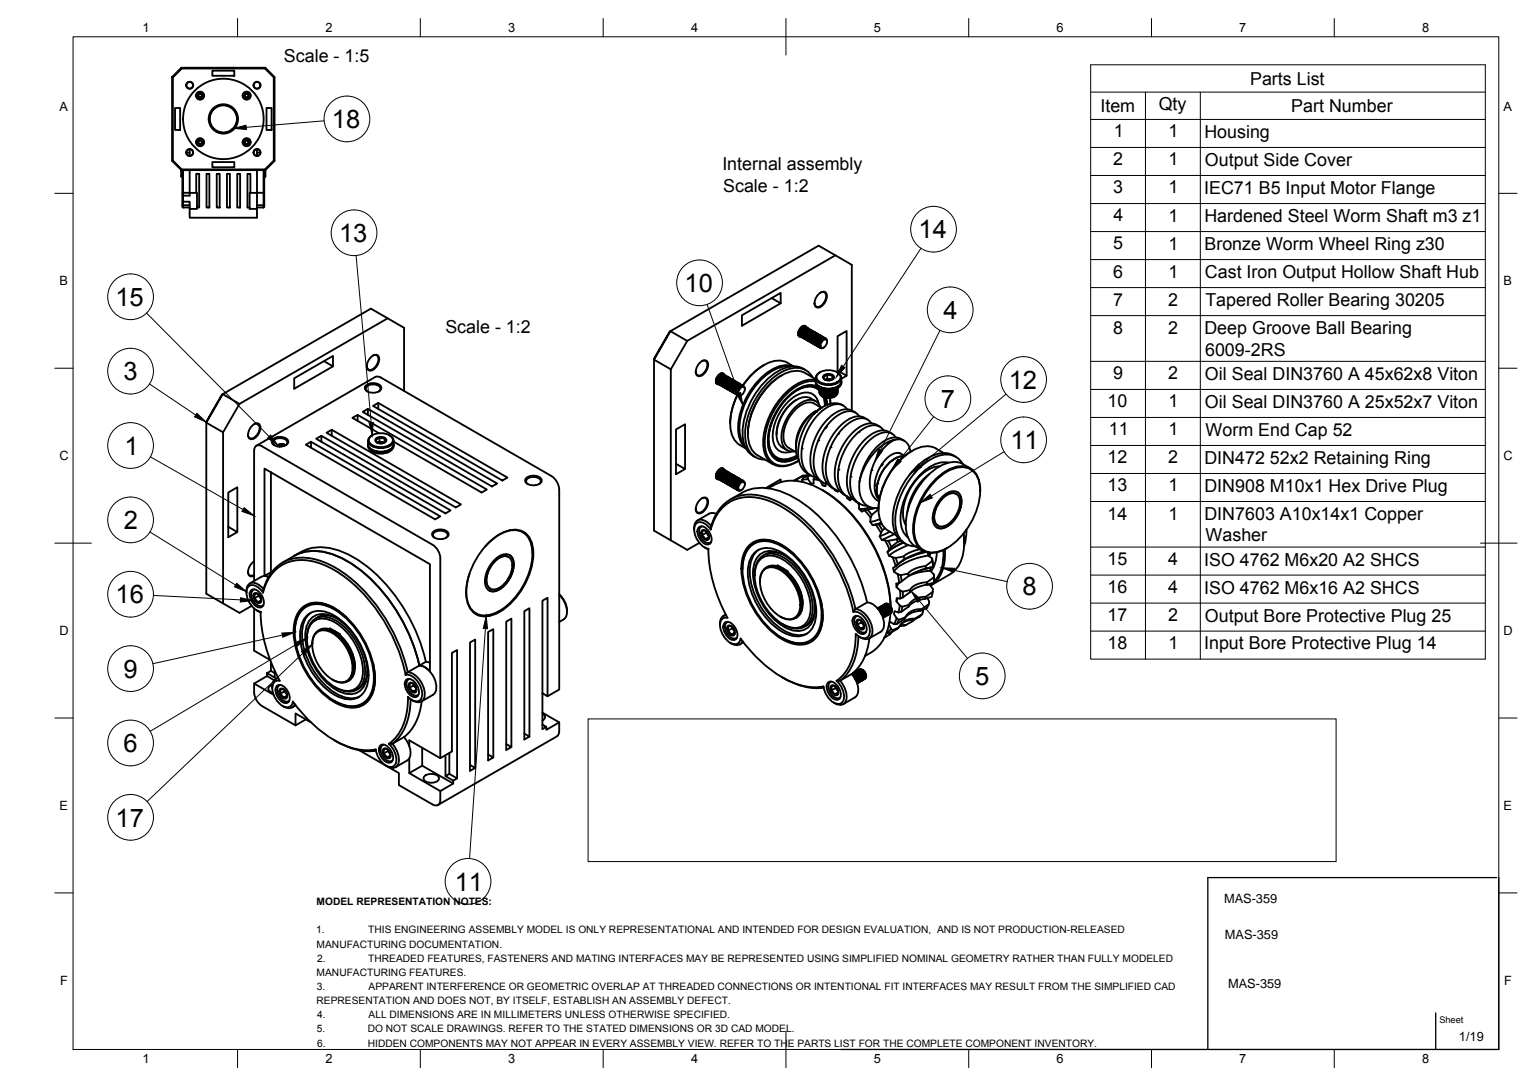
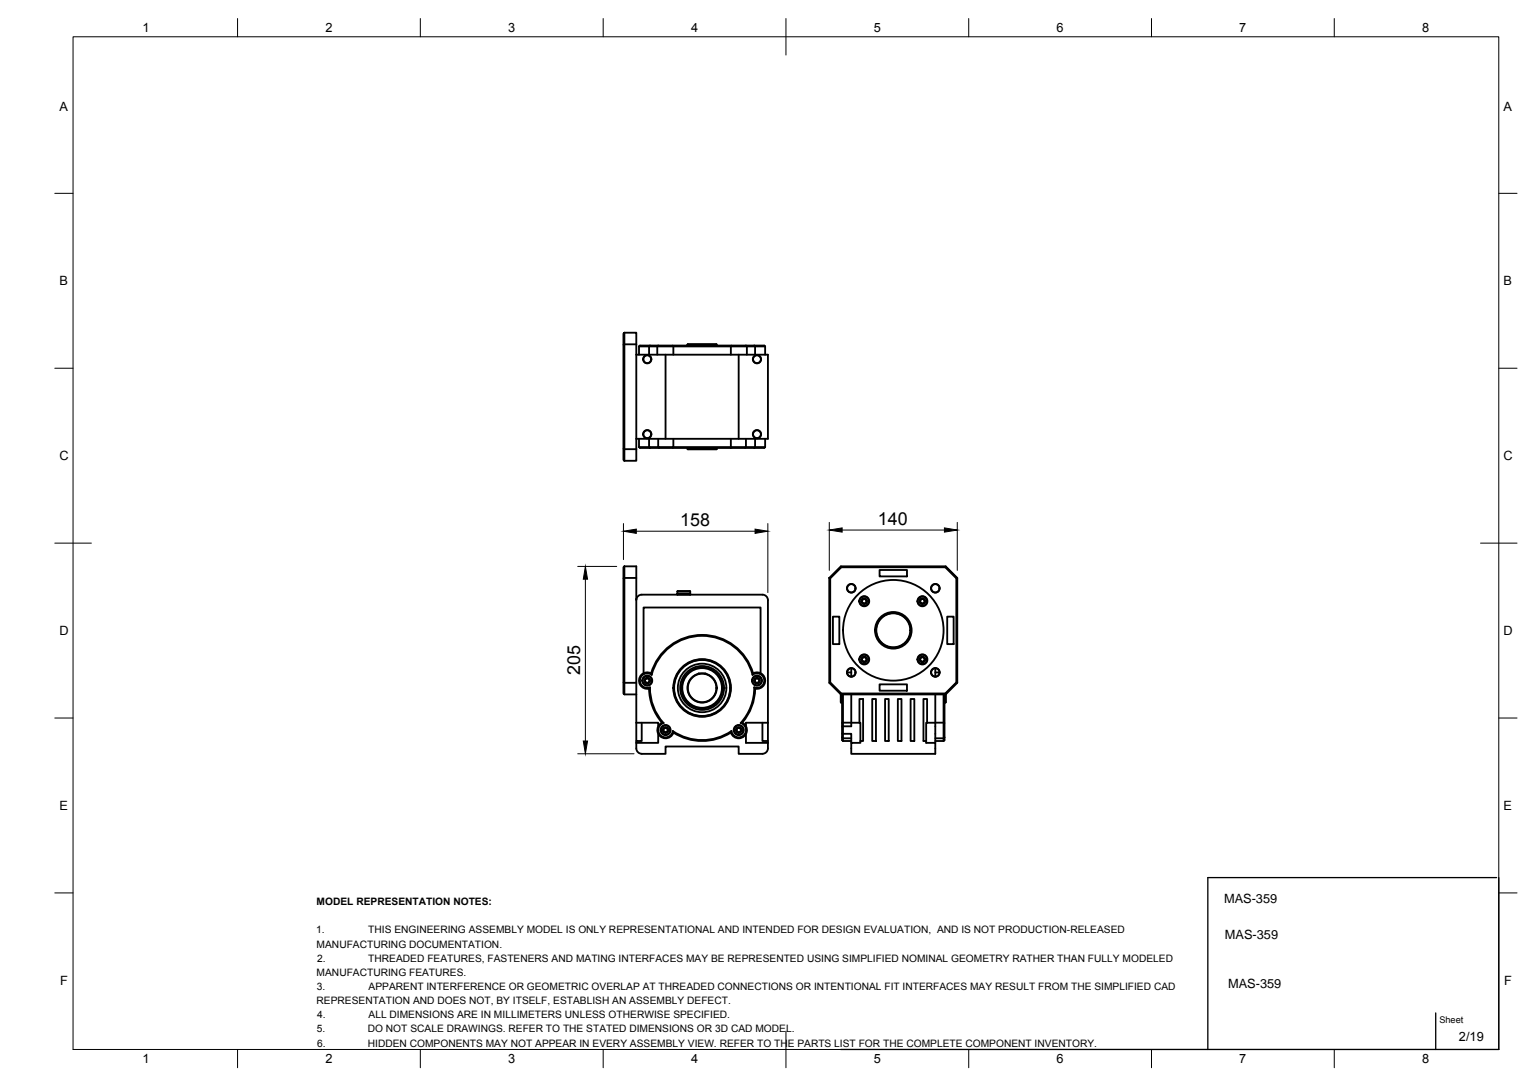
ISO-10303-21;
HEADER;
/* Generated by software containing ST-Developer
 * from STEP Tools, Inc. (www.steptools.com) 
 */

FILE_DESCRIPTION(
/* description */ (''),
/* implementation_level */ '2;1');

FILE_NAME(
/* name */ 'MAS-359',
/* time_stamp */ '2026-10-15T14:25:16-07:00',
/* author */ (''),
/* organization */ (''),
/* preprocessor_version */ 'ST-DEVELOPER v20.2',
/* originating_system */ 'Autodesk Translation Framework v15.15.0.0',
/* authorisation */ '');

FILE_SCHEMA (('AUTOMOTIVE_DESIGN { 1 0 10303 214 3 1 1 }'));
ENDSEC;

DATA;
#10=MECHANICAL_DESIGN_GEOMETRIC_PRESENTATION_REPRESENTATION('',(#323,#324,
#325,#326,#327,#328,#329,#330,#331,#332,#333,#334,#335,#336,#337,#338,#339,
#340),#86429);
#11=ITEM_DEFINED_TRANSFORMATION($,$,#15831,#17257);
#12=ITEM_DEFINED_TRANSFORMATION($,$,#16203,#17258);
#13=ITEM_DEFINED_TRANSFORMATION($,$,#16305,#17259);
#14=ITEM_DEFINED_TRANSFORMATION($,$,#16419,#17260);
#15=ITEM_DEFINED_TRANSFORMATION($,$,#16477,#17261);
#16=ITEM_DEFINED_TRANSFORMATION($,$,#16819,#17262);
#17=ITEM_DEFINED_TRANSFORMATION($,$,#16985,#17263);
#18=ITEM_DEFINED_TRANSFORMATION($,$,#17028,#17264);
#19=ITEM_DEFINED_TRANSFORMATION($,$,#17061,#17265);
#20=ITEM_DEFINED_TRANSFORMATION($,$,#16859,#17266);
#21=ITEM_DEFINED_TRANSFORMATION($,$,#16882,#17267);
#22=ITEM_DEFINED_TRANSFORMATION($,$,#17084,#17268);
#23=ITEM_DEFINED_TRANSFORMATION($,$,#16902,#17269);
#24=ITEM_DEFINED_TRANSFORMATION($,$,#16948,#17270);
#25=ITEM_DEFINED_TRANSFORMATION($,$,#17121,#17271);
#26=ITEM_DEFINED_TRANSFORMATION($,$,#17181,#17272);
#27=ITEM_DEFINED_TRANSFORMATION($,$,#17237,#17273);
#28=ITEM_DEFINED_TRANSFORMATION($,$,#16965,#17274);
#29=ITEM_DEFINED_TRANSFORMATION($,$,#16985,#17275);
#30=ITEM_DEFINED_TRANSFORMATION($,$,#17028,#17276);
#31=ITEM_DEFINED_TRANSFORMATION($,$,#17061,#17277);
#32=ITEM_DEFINED_TRANSFORMATION($,$,#17084,#17278);
#33=ITEM_DEFINED_TRANSFORMATION($,$,#17121,#17279);
#34=ITEM_DEFINED_TRANSFORMATION($,$,#17121,#17280);
#35=ITEM_DEFINED_TRANSFORMATION($,$,#17121,#17281);
#36=ITEM_DEFINED_TRANSFORMATION($,$,#17181,#17282);
#37=ITEM_DEFINED_TRANSFORMATION($,$,#17181,#17283);
#38=ITEM_DEFINED_TRANSFORMATION($,$,#17181,#17284);
#39=ITEM_DEFINED_TRANSFORMATION($,$,#17237,#17285);
#40=(
REPRESENTATION_RELATIONSHIP($,$,#86502,#86501)
REPRESENTATION_RELATIONSHIP_WITH_TRANSFORMATION(#11)
SHAPE_REPRESENTATION_RELATIONSHIP()
);
#41=(
REPRESENTATION_RELATIONSHIP($,$,#86503,#86501)
REPRESENTATION_RELATIONSHIP_WITH_TRANSFORMATION(#12)
SHAPE_REPRESENTATION_RELATIONSHIP()
);
#42=(
REPRESENTATION_RELATIONSHIP($,$,#86504,#86501)
REPRESENTATION_RELATIONSHIP_WITH_TRANSFORMATION(#13)
SHAPE_REPRESENTATION_RELATIONSHIP()
);
#43=(
REPRESENTATION_RELATIONSHIP($,$,#86505,#86501)
REPRESENTATION_RELATIONSHIP_WITH_TRANSFORMATION(#14)
SHAPE_REPRESENTATION_RELATIONSHIP()
);
#44=(
REPRESENTATION_RELATIONSHIP($,$,#86506,#86501)
REPRESENTATION_RELATIONSHIP_WITH_TRANSFORMATION(#15)
SHAPE_REPRESENTATION_RELATIONSHIP()
);
#45=(
REPRESENTATION_RELATIONSHIP($,$,#86507,#86501)
REPRESENTATION_RELATIONSHIP_WITH_TRANSFORMATION(#16)
SHAPE_REPRESENTATION_RELATIONSHIP()
);
#46=(
REPRESENTATION_RELATIONSHIP($,$,#86513,#86501)
REPRESENTATION_RELATIONSHIP_WITH_TRANSFORMATION(#17)
SHAPE_REPRESENTATION_RELATIONSHIP()
);
#47=(
REPRESENTATION_RELATIONSHIP($,$,#86514,#86501)
REPRESENTATION_RELATIONSHIP_WITH_TRANSFORMATION(#18)
SHAPE_REPRESENTATION_RELATIONSHIP()
);
#48=(
REPRESENTATION_RELATIONSHIP($,$,#86515,#86501)
REPRESENTATION_RELATIONSHIP_WITH_TRANSFORMATION(#19)
SHAPE_REPRESENTATION_RELATIONSHIP()
);
#49=(
REPRESENTATION_RELATIONSHIP($,$,#86508,#86501)
REPRESENTATION_RELATIONSHIP_WITH_TRANSFORMATION(#20)
SHAPE_REPRESENTATION_RELATIONSHIP()
);
#50=(
REPRESENTATION_RELATIONSHIP($,$,#86509,#86501)
REPRESENTATION_RELATIONSHIP_WITH_TRANSFORMATION(#21)
SHAPE_REPRESENTATION_RELATIONSHIP()
);
#51=(
REPRESENTATION_RELATIONSHIP($,$,#86516,#86501)
REPRESENTATION_RELATIONSHIP_WITH_TRANSFORMATION(#22)
SHAPE_REPRESENTATION_RELATIONSHIP()
);
#52=(
REPRESENTATION_RELATIONSHIP($,$,#86510,#86501)
REPRESENTATION_RELATIONSHIP_WITH_TRANSFORMATION(#23)
SHAPE_REPRESENTATION_RELATIONSHIP()
);
#53=(
REPRESENTATION_RELATIONSHIP($,$,#86511,#86501)
REPRESENTATION_RELATIONSHIP_WITH_TRANSFORMATION(#24)
SHAPE_REPRESENTATION_RELATIONSHIP()
);
#54=(
REPRESENTATION_RELATIONSHIP($,$,#86517,#86501)
REPRESENTATION_RELATIONSHIP_WITH_TRANSFORMATION(#25)
SHAPE_REPRESENTATION_RELATIONSHIP()
);
#55=(
REPRESENTATION_RELATIONSHIP($,$,#86518,#86501)
REPRESENTATION_RELATIONSHIP_WITH_TRANSFORMATION(#26)
SHAPE_REPRESENTATION_RELATIONSHIP()
);
#56=(
REPRESENTATION_RELATIONSHIP($,$,#86519,#86501)
REPRESENTATION_RELATIONSHIP_WITH_TRANSFORMATION(#27)
SHAPE_REPRESENTATION_RELATIONSHIP()
);
#57=(
REPRESENTATION_RELATIONSHIP($,$,#86512,#86501)
REPRESENTATION_RELATIONSHIP_WITH_TRANSFORMATION(#28)
SHAPE_REPRESENTATION_RELATIONSHIP()
);
#58=(
REPRESENTATION_RELATIONSHIP($,$,#86513,#86501)
REPRESENTATION_RELATIONSHIP_WITH_TRANSFORMATION(#29)
SHAPE_REPRESENTATION_RELATIONSHIP()
);
#59=(
REPRESENTATION_RELATIONSHIP($,$,#86514,#86501)
REPRESENTATION_RELATIONSHIP_WITH_TRANSFORMATION(#30)
SHAPE_REPRESENTATION_RELATIONSHIP()
);
#60=(
REPRESENTATION_RELATIONSHIP($,$,#86515,#86501)
REPRESENTATION_RELATIONSHIP_WITH_TRANSFORMATION(#31)
SHAPE_REPRESENTATION_RELATIONSHIP()
);
#61=(
REPRESENTATION_RELATIONSHIP($,$,#86516,#86501)
REPRESENTATION_RELATIONSHIP_WITH_TRANSFORMATION(#32)
SHAPE_REPRESENTATION_RELATIONSHIP()
);
#62=(
REPRESENTATION_RELATIONSHIP($,$,#86517,#86501)
REPRESENTATION_RELATIONSHIP_WITH_TRANSFORMATION(#33)
SHAPE_REPRESENTATION_RELATIONSHIP()
);
#63=(
REPRESENTATION_RELATIONSHIP($,$,#86517,#86501)
REPRESENTATION_RELATIONSHIP_WITH_TRANSFORMATION(#34)
SHAPE_REPRESENTATION_RELATIONSHIP()
);
#64=(
REPRESENTATION_RELATIONSHIP($,$,#86517,#86501)
REPRESENTATION_RELATIONSHIP_WITH_TRANSFORMATION(#35)
SHAPE_REPRESENTATION_RELATIONSHIP()
);
#65=(
REPRESENTATION_RELATIONSHIP($,$,#86518,#86501)
REPRESENTATION_RELATIONSHIP_WITH_TRANSFORMATION(#36)
SHAPE_REPRESENTATION_RELATIONSHIP()
);
#66=(
REPRESENTATION_RELATIONSHIP($,$,#86518,#86501)
REPRESENTATION_RELATIONSHIP_WITH_TRANSFORMATION(#37)
SHAPE_REPRESENTATION_RELATIONSHIP()
);
#67=(
REPRESENTATION_RELATIONSHIP($,$,#86518,#86501)
REPRESENTATION_RELATIONSHIP_WITH_TRANSFORMATION(#38)
SHAPE_REPRESENTATION_RELATIONSHIP()
);
#68=(
REPRESENTATION_RELATIONSHIP($,$,#86519,#86501)
REPRESENTATION_RELATIONSHIP_WITH_TRANSFORMATION(#39)
SHAPE_REPRESENTATION_RELATIONSHIP()
);
#69=CONTEXT_DEPENDENT_SHAPE_REPRESENTATION(#40,#86472);
#70=CONTEXT_DEPENDENT_SHAPE_REPRESENTATION(#41,#86473);
#71=CONTEXT_DEPENDENT_SHAPE_REPRESENTATION(#42,#86474);
#72=CONTEXT_DEPENDENT_SHAPE_REPRESENTATION(#43,#86475);
#73=CONTEXT_DEPENDENT_SHAPE_REPRESENTATION(#44,#86476);
#74=CONTEXT_DEPENDENT_SHAPE_REPRESENTATION(#45,#86477);
#75=CONTEXT_DEPENDENT_SHAPE_REPRESENTATION(#46,#86478);
#76=CONTEXT_DEPENDENT_SHAPE_REPRESENTATION(#47,#86479);
#77=CONTEXT_DEPENDENT_SHAPE_REPRESENTATION(#48,#86480);
#78=CONTEXT_DEPENDENT_SHAPE_REPRESENTATION(#49,#86481);
#79=CONTEXT_DEPENDENT_SHAPE_REPRESENTATION(#50,#86482);
#80=CONTEXT_DEPENDENT_SHAPE_REPRESENTATION(#51,#86483);
#81=CONTEXT_DEPENDENT_SHAPE_REPRESENTATION(#52,#86484);
#82=CONTEXT_DEPENDENT_SHAPE_REPRESENTATION(#53,#86485);
#83=CONTEXT_DEPENDENT_SHAPE_REPRESENTATION(#54,#86486);
#84=CONTEXT_DEPENDENT_SHAPE_REPRESENTATION(#55,#86487);
#85=CONTEXT_DEPENDENT_SHAPE_REPRESENTATION(#56,#86488);
#86=CONTEXT_DEPENDENT_SHAPE_REPRESENTATION(#57,#86489);
#87=CONTEXT_DEPENDENT_SHAPE_REPRESENTATION(#58,#86490);
#88=CONTEXT_DEPENDENT_SHAPE_REPRESENTATION(#59,#86491);
#89=CONTEXT_DEPENDENT_SHAPE_REPRESENTATION(#60,#86492);
#90=CONTEXT_DEPENDENT_SHAPE_REPRESENTATION(#61,#86493);
#91=CONTEXT_DEPENDENT_SHAPE_REPRESENTATION(#62,#86494);
#92=CONTEXT_DEPENDENT_SHAPE_REPRESENTATION(#63,#86495);
#93=CONTEXT_DEPENDENT_SHAPE_REPRESENTATION(#64,#86496);
#94=CONTEXT_DEPENDENT_SHAPE_REPRESENTATION(#65,#86497);
#95=CONTEXT_DEPENDENT_SHAPE_REPRESENTATION(#66,#86498);
#96=CONTEXT_DEPENDENT_SHAPE_REPRESENTATION(#67,#86499);
#97=CONTEXT_DEPENDENT_SHAPE_REPRESENTATION(#68,#86500);
#98=NEXT_ASSEMBLY_USAGE_OCCURRENCE('Housing:1','Housing:1','Housing:1',
#86521,#86522,'Housing:1');
#99=NEXT_ASSEMBLY_USAGE_OCCURRENCE('Output Side Cover:1',
'Output Side Cover:1','Output Side Cover:1',#86521,#86523,
'Output Side Cover:1');
#100=NEXT_ASSEMBLY_USAGE_OCCURRENCE('IEC71 B5 Input Motor Flange:1',
'IEC71 B5 Input Motor Flange:1','IEC71 B5 Input Motor Flange:1',#86521,
#86524,'IEC71 B5 Input Motor Flange:1');
#101=NEXT_ASSEMBLY_USAGE_OCCURRENCE('Hardened Steel Worm Shaft m3 z1:1',
'Hardened Steel Worm Shaft m3 z1:1','Hardened Steel Worm Shaft m3 z1:1',
#86521,#86525,'Hardened Steel Worm Shaft m3 z1:1');
#102=NEXT_ASSEMBLY_USAGE_OCCURRENCE('Bronze Worm Wheel Ring z30:1',
'Bronze Worm Wheel Ring z30:1','Bronze Worm Wheel Ring z30:1',#86521,#86526,
'Bronze Worm Wheel Ring z30:1');
#103=NEXT_ASSEMBLY_USAGE_OCCURRENCE(
'Cast Iron Output Hollow Shaft Hub:1',
'Cast Iron Output Hollow Shaft Hub:1',
'Cast Iron Output Hollow Shaft Hub:1',#86521,#86527,
'Cast Iron Output Hollow Shaft Hub:1');
#104=NEXT_ASSEMBLY_USAGE_OCCURRENCE('Tapered Roller Bearing 30205:1',
'Tapered Roller Bearing 30205:1','Tapered Roller Bearing 30205:1',#86521,
#86533,'Tapered Roller Bearing 30205:1');
#105=NEXT_ASSEMBLY_USAGE_OCCURRENCE(
'Deep Groove Ball Bearing 6009-2RS:1',
'Deep Groove Ball Bearing 6009-2RS:1',
'Deep Groove Ball Bearing 6009-2RS:1',#86521,#86534,
'Deep Groove Ball Bearing 6009-2RS:1');
#106=NEXT_ASSEMBLY_USAGE_OCCURRENCE(
'Oil Seal DIN3760 A 45x62x8 Viton:1',
'Oil Seal DIN3760 A 45x62x8 Viton:1',
'Oil Seal DIN3760 A 45x62x8 Viton:1',#86521,#86535,
'Oil Seal DIN3760 A 45x62x8 Viton:1');
#107=NEXT_ASSEMBLY_USAGE_OCCURRENCE(
'Oil Seal DIN3760 A 25x52x7 Viton:1',
'Oil Seal DIN3760 A 25x52x7 Viton:1',
'Oil Seal DIN3760 A 25x52x7 Viton:1',#86521,#86528,
'Oil Seal DIN3760 A 25x52x7 Viton:1');
#108=NEXT_ASSEMBLY_USAGE_OCCURRENCE('Worm End Cap 52:1',
'Worm End Cap 52:1','Worm End Cap 52:1',#86521,#86529,
'Worm End Cap 52:1');
#109=NEXT_ASSEMBLY_USAGE_OCCURRENCE('DIN472 52x2 Retaining Ring:1',
'DIN472 52x2 Retaining Ring:1','DIN472 52x2 Retaining Ring:1',#86521,#86536,
'DIN472 52x2 Retaining Ring:1');
#110=NEXT_ASSEMBLY_USAGE_OCCURRENCE('DIN908 M10x1 Hex Drive Plug:1',
'DIN908 M10x1 Hex Drive Plug:1','DIN908 M10x1 Hex Drive Plug:1',#86521,
#86530,'DIN908 M10x1 Hex Drive Plug:1');
#111=NEXT_ASSEMBLY_USAGE_OCCURRENCE('DIN7603 A10x14x1 Copper Washer:1',
'DIN7603 A10x14x1 Copper Washer:1','DIN7603 A10x14x1 Copper Washer:1',#86521,
#86531,'DIN7603 A10x14x1 Copper Washer:1');
#112=NEXT_ASSEMBLY_USAGE_OCCURRENCE('ISO 4762 M6x20 A2 SHCS:1',
'ISO 4762 M6x20 A2 SHCS:1','ISO 4762 M6x20 A2 SHCS:1',#86521,#86537,
'ISO 4762 M6x20 A2 SHCS:1');
#113=NEXT_ASSEMBLY_USAGE_OCCURRENCE('ISO 4762 M6x16 A2 SHCS:1',
'ISO 4762 M6x16 A2 SHCS:1','ISO 4762 M6x16 A2 SHCS:1',#86521,#86538,
'ISO 4762 M6x16 A2 SHCS:1');
#114=NEXT_ASSEMBLY_USAGE_OCCURRENCE('Output Bore Protective Plug 25:1',
'Output Bore Protective Plug 25:1','Output Bore Protective Plug 25:1',#86521,
#86539,'Output Bore Protective Plug 25:1');
#115=NEXT_ASSEMBLY_USAGE_OCCURRENCE('Input Bore Protective Plug 14:1',
'Input Bore Protective Plug 14:1','Input Bore Protective Plug 14:1',#86521,
#86532,'Input Bore Protective Plug 14:1');
#116=NEXT_ASSEMBLY_USAGE_OCCURRENCE('Tapered Roller Bearing 30205:2',
'Tapered Roller Bearing 30205:2','Tapered Roller Bearing 30205:2',#86521,
#86533,'Tapered Roller Bearing 30205:2');
#117=NEXT_ASSEMBLY_USAGE_OCCURRENCE(
'Deep Groove Ball Bearing 6009-2RS:2',
'Deep Groove Ball Bearing 6009-2RS:2',
'Deep Groove Ball Bearing 6009-2RS:2',#86521,#86534,
'Deep Groove Ball Bearing 6009-2RS:2');
#118=NEXT_ASSEMBLY_USAGE_OCCURRENCE(
'Oil Seal DIN3760 A 45x62x8 Viton:2',
'Oil Seal DIN3760 A 45x62x8 Viton:2',
'Oil Seal DIN3760 A 45x62x8 Viton:2',#86521,#86535,
'Oil Seal DIN3760 A 45x62x8 Viton:2');
#119=NEXT_ASSEMBLY_USAGE_OCCURRENCE('DIN472 52x2 Retaining Ring:2',
'DIN472 52x2 Retaining Ring:2','DIN472 52x2 Retaining Ring:2',#86521,#86536,
'DIN472 52x2 Retaining Ring:2');
#120=NEXT_ASSEMBLY_USAGE_OCCURRENCE('ISO 4762 M6x20 A2 SHCS:2',
'ISO 4762 M6x20 A2 SHCS:2','ISO 4762 M6x20 A2 SHCS:2',#86521,#86537,
'ISO 4762 M6x20 A2 SHCS:2');
#121=NEXT_ASSEMBLY_USAGE_OCCURRENCE('ISO 4762 M6x20 A2 SHCS:3',
'ISO 4762 M6x20 A2 SHCS:3','ISO 4762 M6x20 A2 SHCS:3',#86521,#86537,
'ISO 4762 M6x20 A2 SHCS:3');
#122=NEXT_ASSEMBLY_USAGE_OCCURRENCE('ISO 4762 M6x20 A2 SHCS:4',
'ISO 4762 M6x20 A2 SHCS:4','ISO 4762 M6x20 A2 SHCS:4',#86521,#86537,
'ISO 4762 M6x20 A2 SHCS:4');
#123=NEXT_ASSEMBLY_USAGE_OCCURRENCE('ISO 4762 M6x16 A2 SHCS:2',
'ISO 4762 M6x16 A2 SHCS:2','ISO 4762 M6x16 A2 SHCS:2',#86521,#86538,
'ISO 4762 M6x16 A2 SHCS:2');
#124=NEXT_ASSEMBLY_USAGE_OCCURRENCE('ISO 4762 M6x16 A2 SHCS:3',
'ISO 4762 M6x16 A2 SHCS:3','ISO 4762 M6x16 A2 SHCS:3',#86521,#86538,
'ISO 4762 M6x16 A2 SHCS:3');
#125=NEXT_ASSEMBLY_USAGE_OCCURRENCE('ISO 4762 M6x16 A2 SHCS:4',
'ISO 4762 M6x16 A2 SHCS:4','ISO 4762 M6x16 A2 SHCS:4',#86521,#86538,
'ISO 4762 M6x16 A2 SHCS:4');
#126=NEXT_ASSEMBLY_USAGE_OCCURRENCE('Output Bore Protective Plug 25:2',
'Output Bore Protective Plug 25:2','Output Bore Protective Plug 25:2',#86521,
#86539,'Output Bore Protective Plug 25:2');
#127=TOROIDAL_SURFACE('',#16553,6.3,1.5);
#128=TOROIDAL_SURFACE('',#16562,6.3,1.5);
#129=TOROIDAL_SURFACE('',#16571,6.3,1.5);
#130=TOROIDAL_SURFACE('',#16580,6.3,1.5);
#131=TOROIDAL_SURFACE('',#16589,6.3,1.5);
#132=TOROIDAL_SURFACE('',#16598,6.3,1.5);
#133=TOROIDAL_SURFACE('',#16607,6.3,1.5);
#134=TOROIDAL_SURFACE('',#16616,6.3,1.5);
#135=TOROIDAL_SURFACE('',#16625,6.3,1.5);
#136=TOROIDAL_SURFACE('',#16634,6.3,1.5);
#137=TOROIDAL_SURFACE('',#16643,6.3,1.5);
#138=TOROIDAL_SURFACE('',#16652,6.3,1.5);
#139=TOROIDAL_SURFACE('',#16661,6.3,1.5);
#140=TOROIDAL_SURFACE('',#16670,6.3,1.5);
#141=TOROIDAL_SURFACE('',#16679,6.3,1.5);
#142=TOROIDAL_SURFACE('',#16688,6.3,1.5);
#143=TOROIDAL_SURFACE('',#16697,6.3,1.5);
#144=TOROIDAL_SURFACE('',#16706,6.3,1.5);
#145=TOROIDAL_SURFACE('',#16715,6.3,1.5);
#146=TOROIDAL_SURFACE('',#16724,6.3,1.5);
#147=TOROIDAL_SURFACE('',#16733,6.3,1.5);
#148=TOROIDAL_SURFACE('',#16742,6.3,1.5);
#149=TOROIDAL_SURFACE('',#16751,6.3,1.5);
#150=TOROIDAL_SURFACE('',#16760,6.3,1.5);
#151=TOROIDAL_SURFACE('',#16769,6.3,1.5);
#152=TOROIDAL_SURFACE('',#16778,6.3,1.5);
#153=TOROIDAL_SURFACE('',#16787,6.3,1.5);
#154=TOROIDAL_SURFACE('',#16798,6.3,1.5);
#155=TOROIDAL_SURFACE('',#16811,6.3,1.5);
#156=TOROIDAL_SURFACE('',#16817,6.3,1.5);
#157=TOROIDAL_SURFACE('',#17154,0.3342,0.04);
#158=TOROIDAL_SURFACE('',#17170,0.44,0.06);
#159=TOROIDAL_SURFACE('',#17210,0.3342,0.04);
#160=TOROIDAL_SURFACE('',#17226,0.44,0.06);
#161=B_SPLINE_SURFACE_WITH_KNOTS('',3,3,((#24275,#24276,#24277,#24278,#24279,
#24280,#24281,#24282,#24283,#24284,#24285,#24286,#24287,#24288,#24289,#24290,
#24291,#24292,#24293,#24294,#24295,#24296,#24297,#24298,#24299,#24300,#24301,
#24302,#24303,#24304,#24305,#24306,#24307,#24308,#24309,#24310,#24311,#24312,
#24313,#24314,#24315,#24316,#24317,#24318,#24319,#24320,#24321,#24322,#24323,
#24324,#24325,#24326,#24327,#24328,#24329,#24330,#24331,#24332,#24333,#24334,
#24335,#24336,#24337,#24338,#24339,#24340,#24341,#24342,#24343,#24344,#24345,
#24346,#24347,#24348,#24349,#24350,#24351,#24352,#24353,#24354,#24355,#24356,
#24357,#24358,#24359,#24360,#24361,#24362,#24363,#24364,#24365,#24366,#24367,
#24368,#24369,#24370,#24371,#24372,#24373,#24374,#24375,#24376,#24377,#24378,
#24379,#24380,#24381,#24382,#24383,#24384,#24385,#24386,#24387,#24388,#24389,
#24390,#24391,#24392,#24393,#24394,#24395,#24396,#24397,#24398,#24399,#24400,
#24401,#24402,#24403,#24404,#24405,#24406,#24407,#24408,#24409,#24410,#24411,
#24412,#24413,#24414,#24415,#24416,#24417),(#24418,#24419,#24420,#24421,
#24422,#24423,#24424,#24425,#24426,#24427,#24428,#24429,#24430,#24431,#24432,
#24433,#24434,#24435,#24436,#24437,#24438,#24439,#24440,#24441,#24442,#24443,
#24444,#24445,#24446,#24447,#24448,#24449,#24450,#24451,#24452,#24453,#24454,
#24455,#24456,#24457,#24458,#24459,#24460,#24461,#24462,#24463,#24464,#24465,
#24466,#24467,#24468,#24469,#24470,#24471,#24472,#24473,#24474,#24475,#24476,
#24477,#24478,#24479,#24480,#24481,#24482,#24483,#24484,#24485,#24486,#24487,
#24488,#24489,#24490,#24491,#24492,#24493,#24494,#24495,#24496,#24497,#24498,
#24499,#24500,#24501,#24502,#24503,#24504,#24505,#24506,#24507,#24508,#24509,
#24510,#24511,#24512,#24513,#24514,#24515,#24516,#24517,#24518,#24519,#24520,
#24521,#24522,#24523,#24524,#24525,#24526,#24527,#24528,#24529,#24530,#24531,
#24532,#24533,#24534,#24535,#24536,#24537,#24538,#24539,#24540,#24541,#24542,
#24543,#24544,#24545,#24546,#24547,#24548,#24549,#24550,#24551,#24552,#24553,
#24554,#24555,#24556,#24557,#24558,#24559,#24560),(#24561,#24562,#24563,
#24564,#24565,#24566,#24567,#24568,#24569,#24570,#24571,#24572,#24573,#24574,
#24575,#24576,#24577,#24578,#24579,#24580,#24581,#24582,#24583,#24584,#24585,
#24586,#24587,#24588,#24589,#24590,#24591,#24592,#24593,#24594,#24595,#24596,
#24597,#24598,#24599,#24600,#24601,#24602,#24603,#24604,#24605,#24606,#24607,
#24608,#24609,#24610,#24611,#24612,#24613,#24614,#24615,#24616,#24617,#24618,
#24619,#24620,#24621,#24622,#24623,#24624,#24625,#24626,#24627,#24628,#24629,
#24630,#24631,#24632,#24633,#24634,#24635,#24636,#24637,#24638,#24639,#24640,
#24641,#24642,#24643,#24644,#24645,#24646,#24647,#24648,#24649,#24650,#24651,
#24652,#24653,#24654,#24655,#24656,#24657,#24658,#24659,#24660,#24661,#24662,
#24663,#24664,#24665,#24666,#24667,#24668,#24669,#24670,#24671,#24672,#24673,
#24674,#24675,#24676,#24677,#24678,#24679,#24680,#24681,#24682,#24683,#24684,
#24685,#24686,#24687,#24688,#24689,#24690,#24691,#24692,#24693,#24694,#24695,
#24696,#24697,#24698,#24699,#24700,#24701,#24702,#24703),(#24704,#24705,
#24706,#24707,#24708,#24709,#24710,#24711,#24712,#24713,#24714,#24715,#24716,
#24717,#24718,#24719,#24720,#24721,#24722,#24723,#24724,#24725,#24726,#24727,
#24728,#24729,#24730,#24731,#24732,#24733,#24734,#24735,#24736,#24737,#24738,
#24739,#24740,#24741,#24742,#24743,#24744,#24745,#24746,#24747,#24748,#24749,
#24750,#24751,#24752,#24753,#24754,#24755,#24756,#24757,#24758,#24759,#24760,
#24761,#24762,#24763,#24764,#24765,#24766,#24767,#24768,#24769,#24770,#24771,
#24772,#24773,#24774,#24775,#24776,#24777,#24778,#24779,#24780,#24781,#24782,
#24783,#24784,#24785,#24786,#24787,#24788,#24789,#24790,#24791,#24792,#24793,
#24794,#24795,#24796,#24797,#24798,#24799,#24800,#24801,#24802,#24803,#24804,
#24805,#24806,#24807,#24808,#24809,#24810,#24811,#24812,#24813,#24814,#24815,
#24816,#24817,#24818,#24819,#24820,#24821,#24822,#24823,#24824,#24825,#24826,
#24827,#24828,#24829,#24830,#24831,#24832,#24833,#24834,#24835,#24836,#24837,
#24838,#24839,#24840,#24841,#24842,#24843,#24844,#24845,#24846)),
 .UNSPECIFIED.,.F.,.F.,.F.,(4,4),(4,1,1,1,2,1,1,1,1,1,1,1,1,1,2,1,1,1,1,
2,1,1,1,1,2,1,1,2,2,1,1,1,1,1,1,2,1,2,1,1,1,2,1,1,1,2,1,1,1,2,1,1,1,2,1,
1,1,2,1,1,1,2,1,1,1,2,1,1,1,1,1,2,1,1,1,1,1,1,2,2,1,1,2,1,1,1,1,2,1,1,1,
1,2,1,1,1,1,1,1,1,1,1,2,1,1,1,1,1,2,2,1,1,1,1,1,1,4),(-7.42398645807014E-6,
0.252864181465206),(0.121233664526765,0.122596153817018,0.123197115362701,
0.123397435877929,0.124999999999751,0.135817307706478,0.146634615413206,
0.15745192309109,0.168269230768974,0.177884615384371,0.187499999999768,
0.199519230740103,0.206730769230503,0.210336538446854,0.211538461538235,
0.213942307720923,0.218749999970821,0.228365384586246,0.237980769201671,
0.249999999999808,0.25841346152381,0.266826923047812,0.281250000028623,
0.289663461552636,0.298076923076649,0.312499999999747,0.31971153849016,
0.326923076922846,0.33653846153821,0.338942307720942,0.340144230783416,
0.343749999970879,0.353365384586257,0.358173076951719,0.362980769201619,
0.365384615384414,0.370192307692066,0.37499999999969,0.389423076922836,
0.397836538475728,0.406250000028619,0.413461538461298,0.420673076893946,
0.425480769259405,0.427884615384363,0.432692307692057,0.433894230783419,
0.43509615387478,0.437499999999749,0.442307692307468,0.455528846139201,
0.468749999970934,0.483173076951685,0.49999999999975,0.516826923047797,
0.531250000028611,0.544471153860329,0.557692307692047,0.562499999999739,
0.563701923062234,0.564903846124729,0.567307692307427,0.569711538490167,
0.574519230740095,0.579326923105555,0.586538461538202,0.593749999970866,
0.602163461523769,0.610576923076672,0.624999999999777,0.629807692307439,
0.634615384615125,0.637019230797861,0.641826923047781,0.646634615413246,
0.656250000028622,0.659855769216081,0.661057692278563,0.663461538461287,
0.673076923076666,0.680288461509321,0.687499999999755,0.701923076922838,
0.710336538446858,0.718749999970878,0.733173076951697,0.741586538475723,
0.749999999999749,0.762019230797881,0.771634615413259,0.781250000028636,
0.786057692278561,0.788461538461294,0.78966346155265,0.793269230768981,
0.800480769259399,0.812499999999748,0.822115384615134,0.83173076923052,
0.842548076908385,0.853365384586251,0.864182692292999,0.874999999999748,
0.876602564121565,0.876802884636793,0.877403846182474,0.879807692307444,
0.882211538432407,0.884615384615134,0.894230769230516,0.895432692321882,
0.906250000028634,0.915865384644013,0.926682692321841,0.937499999999668,
0.949519230731432,0.955682525542283),.UNSPECIFIED.);
#162=B_SPLINE_SURFACE_WITH_KNOTS('',3,3,((#25484,#25485,#25486,#25487,#25488,
#25489,#25490,#25491,#25492,#25493,#25494,#25495,#25496,#25497,#25498,#25499,
#25500,#25501,#25502,#25503,#25504,#25505,#25506,#25507,#25508,#25509,#25510,
#25511,#25512,#25513,#25514,#25515,#25516,#25517,#25518,#25519,#25520,#25521,
#25522,#25523,#25524,#25525,#25526,#25527,#25528,#25529,#25530,#25531,#25532,
#25533,#25534,#25535,#25536,#25537,#25538,#25539,#25540,#25541,#25542,#25543,
#25544,#25545,#25546,#25547,#25548,#25549,#25550,#25551,#25552,#25553,#25554,
#25555,#25556,#25557,#25558,#25559,#25560,#25561,#25562,#25563,#25564,#25565,
#25566,#25567,#25568,#25569,#25570,#25571,#25572,#25573,#25574,#25575,#25576,
#25577,#25578,#25579,#25580,#25581,#25582,#25583,#25584,#25585,#25586,#25587,
#25588,#25589,#25590,#25591,#25592,#25593,#25594,#25595,#25596,#25597,#25598,
#25599,#25600,#25601,#25602,#25603,#25604,#25605,#25606,#25607,#25608,#25609,
#25610,#25611,#25612,#25613,#25614,#25615,#25616,#25617,#25618,#25619,#25620,
#25621,#25622,#25623,#25624,#25625,#25626,#25627,#25628,#25629,#25630,#25631,
#25632,#25633,#25634,#25635,#25636,#25637,#25638,#25639,#25640,#25641,#25642,
#25643,#25644,#25645,#25646),(#25647,#25648,#25649,#25650,#25651,#25652,
#25653,#25654,#25655,#25656,#25657,#25658,#25659,#25660,#25661,#25662,#25663,
#25664,#25665,#25666,#25667,#25668,#25669,#25670,#25671,#25672,#25673,#25674,
#25675,#25676,#25677,#25678,#25679,#25680,#25681,#25682,#25683,#25684,#25685,
#25686,#25687,#25688,#25689,#25690,#25691,#25692,#25693,#25694,#25695,#25696,
#25697,#25698,#25699,#25700,#25701,#25702,#25703,#25704,#25705,#25706,#25707,
#25708,#25709,#25710,#25711,#25712,#25713,#25714,#25715,#25716,#25717,#25718,
#25719,#25720,#25721,#25722,#25723,#25724,#25725,#25726,#25727,#25728,#25729,
#25730,#25731,#25732,#25733,#25734,#25735,#25736,#25737,#25738,#25739,#25740,
#25741,#25742,#25743,#25744,#25745,#25746,#25747,#25748,#25749,#25750,#25751,
#25752,#25753,#25754,#25755,#25756,#25757,#25758,#25759,#25760,#25761,#25762,
#25763,#25764,#25765,#25766,#25767,#25768,#25769,#25770,#25771,#25772,#25773,
#25774,#25775,#25776,#25777,#25778,#25779,#25780,#25781,#25782,#25783,#25784,
#25785,#25786,#25787,#25788,#25789,#25790,#25791,#25792,#25793,#25794,#25795,
#25796,#25797,#25798,#25799,#25800,#25801,#25802,#25803,#25804,#25805,#25806,
#25807,#25808,#25809),(#25810,#25811,#25812,#25813,#25814,#25815,#25816,
#25817,#25818,#25819,#25820,#25821,#25822,#25823,#25824,#25825,#25826,#25827,
#25828,#25829,#25830,#25831,#25832,#25833,#25834,#25835,#25836,#25837,#25838,
#25839,#25840,#25841,#25842,#25843,#25844,#25845,#25846,#25847,#25848,#25849,
#25850,#25851,#25852,#25853,#25854,#25855,#25856,#25857,#25858,#25859,#25860,
#25861,#25862,#25863,#25864,#25865,#25866,#25867,#25868,#25869,#25870,#25871,
#25872,#25873,#25874,#25875,#25876,#25877,#25878,#25879,#25880,#25881,#25882,
#25883,#25884,#25885,#25886,#25887,#25888,#25889,#25890,#25891,#25892,#25893,
#25894,#25895,#25896,#25897,#25898,#25899,#25900,#25901,#25902,#25903,#25904,
#25905,#25906,#25907,#25908,#25909,#25910,#25911,#25912,#25913,#25914,#25915,
#25916,#25917,#25918,#25919,#25920,#25921,#25922,#25923,#25924,#25925,#25926,
#25927,#25928,#25929,#25930,#25931,#25932,#25933,#25934,#25935,#25936,#25937,
#25938,#25939,#25940,#25941,#25942,#25943,#25944,#25945,#25946,#25947,#25948,
#25949,#25950,#25951,#25952,#25953,#25954,#25955,#25956,#25957,#25958,#25959,
#25960,#25961,#25962,#25963,#25964,#25965,#25966,#25967,#25968,#25969,#25970,
#25971,#25972),(#25973,#25974,#25975,#25976,#25977,#25978,#25979,#25980,
#25981,#25982,#25983,#25984,#25985,#25986,#25987,#25988,#25989,#25990,#25991,
#25992,#25993,#25994,#25995,#25996,#25997,#25998,#25999,#26000,#26001,#26002,
#26003,#26004,#26005,#26006,#26007,#26008,#26009,#26010,#26011,#26012,#26013,
#26014,#26015,#26016,#26017,#26018,#26019,#26020,#26021,#26022,#26023,#26024,
#26025,#26026,#26027,#26028,#26029,#26030,#26031,#26032,#26033,#26034,#26035,
#26036,#26037,#26038,#26039,#26040,#26041,#26042,#26043,#26044,#26045,#26046,
#26047,#26048,#26049,#26050,#26051,#26052,#26053,#26054,#26055,#26056,#26057,
#26058,#26059,#26060,#26061,#26062,#26063,#26064,#26065,#26066,#26067,#26068,
#26069,#26070,#26071,#26072,#26073,#26074,#26075,#26076,#26077,#26078,#26079,
#26080,#26081,#26082,#26083,#26084,#26085,#26086,#26087,#26088,#26089,#26090,
#26091,#26092,#26093,#26094,#26095,#26096,#26097,#26098,#26099,#26100,#26101,
#26102,#26103,#26104,#26105,#26106,#26107,#26108,#26109,#26110,#26111,#26112,
#26113,#26114,#26115,#26116,#26117,#26118,#26119,#26120,#26121,#26122,#26123,
#26124,#26125,#26126,#26127,#26128,#26129,#26130,#26131,#26132,#26133,#26134,
#26135)),.UNSPECIFIED.,.F.,.F.,.F.,(4,4),(4,1,1,1,1,1,1,1,1,1,1,2,2,1,1,
1,1,1,2,1,1,1,1,1,1,1,1,1,2,1,1,1,1,2,1,1,1,1,2,1,1,2,2,1,1,1,1,1,1,2,1,
2,1,1,1,2,1,1,1,2,1,1,1,2,1,1,1,2,1,1,1,2,1,1,1,2,1,1,1,2,1,1,1,2,1,2,1,
1,1,1,1,1,2,2,1,1,2,1,1,1,1,2,1,1,1,1,2,1,1,1,1,1,1,1,1,1,2,1,1,1,1,1,2,
2,1,1,1,1,1,1,1,1,1,4),(0.0100803267684296,0.756239113823487),(-3.07676242782602E-5,
0.00841344965183915,0.0168268993036783,0.0312500013956658,0.0408653845261411,
0.0504807692681131,0.062499999999838,0.0733173076776515,0.0841346153554649,
0.0937499999708451,0.104567307677615,0.105769230768995,0.115384615384363,
0.117788461567088,0.120192307692056,0.122596153817018,0.123197115362701,
0.123397435877929,0.124999999999751,0.135817307706478,0.146634615413206,
0.15745192309109,0.168269230768974,0.177884615384371,0.187499999999768,
0.199519230740103,0.206730769230503,0.210336538446854,0.211538461538235,
0.213942307720923,0.218749999970821,0.228365384586246,0.237980769201671,
0.249999999999808,0.25841346152381,0.266826923047812,0.281250000028623,
0.289663461552636,0.298076923076649,0.312499999999747,0.31971153849016,
0.326923076922846,0.33653846153821,0.338942307720942,0.340144230783416,
0.343749999970879,0.353365384586257,0.358173076951719,0.362980769201619,
0.365384615384414,0.370192307692066,0.37499999999969,0.389423076922836,
0.397836538475728,0.406250000028619,0.413461538461298,0.420673076893946,
0.425480769259405,0.427884615384363,0.432692307692057,0.433894230783419,
0.43509615387478,0.437499999999749,0.442307692307468,0.455528846139201,
0.468749999970934,0.483173076951685,0.49999999999975,0.516826923047797,
0.531250000028611,0.544471153860329,0.557692307692047,0.562499999999739,
0.563701923062234,0.564903846124729,0.567307692307427,0.569711538490167,
0.574519230740095,0.579326923105555,0.586538461538202,0.593749999970866,
0.602163461523769,0.610576923076672,0.624999999999777,0.629807692307439,
0.634615384615125,0.637019230797861,0.641826923047781,0.646634615413246,
0.656250000028622,0.659855769216081,0.661057692278563,0.663461538461287,
0.673076923076666,0.680288461509321,0.687499999999755,0.701923076922838,
0.710336538446858,0.718749999970878,0.733173076951697,0.741586538475723,
0.749999999999749,0.762019230797881,0.771634615413259,0.781250000028636,
0.786057692278561,0.788461538461294,0.78966346155265,0.793269230768981,
0.800480769259399,0.812499999999748,0.822115384615134,0.83173076923052,
0.842548076908385,0.853365384586251,0.864182692292999,0.874999999999748,
0.876602564121565,0.876802884636793,0.877403846182474,0.879807692307444,
0.882211538432407,0.884615384615134,0.894230769230516,0.895432692321882,
0.906250000028634,0.915865384644013,0.926682692321841,0.937499999999668,
0.949519230731432,0.95913461547336,0.968749998603834,0.983173100695849,
0.985231553658313),.UNSPECIFIED.);
#163=B_SPLINE_SURFACE_WITH_KNOTS('',3,3,((#26138,#26139,#26140,#26141,#26142,
#26143,#26144,#26145,#26146,#26147,#26148,#26149,#26150,#26151,#26152,#26153,
#26154,#26155,#26156,#26157,#26158,#26159,#26160,#26161,#26162,#26163,#26164,
#26165,#26166,#26167,#26168,#26169,#26170,#26171,#26172,#26173,#26174,#26175,
#26176,#26177,#26178,#26179,#26180,#26181,#26182,#26183,#26184,#26185,#26186,
#26187,#26188,#26189,#26190,#26191,#26192,#26193,#26194,#26195,#26196,#26197,
#26198,#26199,#26200,#26201,#26202,#26203,#26204,#26205,#26206,#26207,#26208,
#26209,#26210,#26211,#26212,#26213,#26214,#26215,#26216,#26217,#26218,#26219,
#26220,#26221,#26222,#26223,#26224,#26225,#26226,#26227,#26228,#26229,#26230,
#26231,#26232,#26233,#26234,#26235,#26236,#26237,#26238,#26239,#26240,#26241,
#26242,#26243,#26244,#26245,#26246,#26247,#26248,#26249,#26250,#26251,#26252,
#26253,#26254,#26255,#26256,#26257,#26258,#26259,#26260,#26261,#26262,#26263,
#26264,#26265,#26266,#26267,#26268,#26269,#26270,#26271,#26272,#26273,#26274,
#26275,#26276,#26277,#26278,#26279,#26280,#26281,#26282,#26283,#26284,#26285,
#26286,#26287,#26288,#26289,#26290,#26291,#26292,#26293),(#26294,#26295,
#26296,#26297,#26298,#26299,#26300,#26301,#26302,#26303,#26304,#26305,#26306,
#26307,#26308,#26309,#26310,#26311,#26312,#26313,#26314,#26315,#26316,#26317,
#26318,#26319,#26320,#26321,#26322,#26323,#26324,#26325,#26326,#26327,#26328,
#26329,#26330,#26331,#26332,#26333,#26334,#26335,#26336,#26337,#26338,#26339,
#26340,#26341,#26342,#26343,#26344,#26345,#26346,#26347,#26348,#26349,#26350,
#26351,#26352,#26353,#26354,#26355,#26356,#26357,#26358,#26359,#26360,#26361,
#26362,#26363,#26364,#26365,#26366,#26367,#26368,#26369,#26370,#26371,#26372,
#26373,#26374,#26375,#26376,#26377,#26378,#26379,#26380,#26381,#26382,#26383,
#26384,#26385,#26386,#26387,#26388,#26389,#26390,#26391,#26392,#26393,#26394,
#26395,#26396,#26397,#26398,#26399,#26400,#26401,#26402,#26403,#26404,#26405,
#26406,#26407,#26408,#26409,#26410,#26411,#26412,#26413,#26414,#26415,#26416,
#26417,#26418,#26419,#26420,#26421,#26422,#26423,#26424,#26425,#26426,#26427,
#26428,#26429,#26430,#26431,#26432,#26433,#26434,#26435,#26436,#26437,#26438,
#26439,#26440,#26441,#26442,#26443,#26444,#26445,#26446,#26447,#26448,#26449),
(#26450,#26451,#26452,#26453,#26454,#26455,#26456,#26457,#26458,#26459,
#26460,#26461,#26462,#26463,#26464,#26465,#26466,#26467,#26468,#26469,#26470,
#26471,#26472,#26473,#26474,#26475,#26476,#26477,#26478,#26479,#26480,#26481,
#26482,#26483,#26484,#26485,#26486,#26487,#26488,#26489,#26490,#26491,#26492,
#26493,#26494,#26495,#26496,#26497,#26498,#26499,#26500,#26501,#26502,#26503,
#26504,#26505,#26506,#26507,#26508,#26509,#26510,#26511,#26512,#26513,#26514,
#26515,#26516,#26517,#26518,#26519,#26520,#26521,#26522,#26523,#26524,#26525,
#26526,#26527,#26528,#26529,#26530,#26531,#26532,#26533,#26534,#26535,#26536,
#26537,#26538,#26539,#26540,#26541,#26542,#26543,#26544,#26545,#26546,#26547,
#26548,#26549,#26550,#26551,#26552,#26553,#26554,#26555,#26556,#26557,#26558,
#26559,#26560,#26561,#26562,#26563,#26564,#26565,#26566,#26567,#26568,#26569,
#26570,#26571,#26572,#26573,#26574,#26575,#26576,#26577,#26578,#26579,#26580,
#26581,#26582,#26583,#26584,#26585,#26586,#26587,#26588,#26589,#26590,#26591,
#26592,#26593,#26594,#26595,#26596,#26597,#26598,#26599,#26600,#26601,#26602,
#26603,#26604,#26605),(#26606,#26607,#26608,#26609,#26610,#26611,#26612,
#26613,#26614,#26615,#26616,#26617,#26618,#26619,#26620,#26621,#26622,#26623,
#26624,#26625,#26626,#26627,#26628,#26629,#26630,#26631,#26632,#26633,#26634,
#26635,#26636,#26637,#26638,#26639,#26640,#26641,#26642,#26643,#26644,#26645,
#26646,#26647,#26648,#26649,#26650,#26651,#26652,#26653,#26654,#26655,#26656,
#26657,#26658,#26659,#26660,#26661,#26662,#26663,#26664,#26665,#26666,#26667,
#26668,#26669,#26670,#26671,#26672,#26673,#26674,#26675,#26676,#26677,#26678,
#26679,#26680,#26681,#26682,#26683,#26684,#26685,#26686,#26687,#26688,#26689,
#26690,#26691,#26692,#26693,#26694,#26695,#26696,#26697,#26698,#26699,#26700,
#26701,#26702,#26703,#26704,#26705,#26706,#26707,#26708,#26709,#26710,#26711,
#26712,#26713,#26714,#26715,#26716,#26717,#26718,#26719,#26720,#26721,#26722,
#26723,#26724,#26725,#26726,#26727,#26728,#26729,#26730,#26731,#26732,#26733,
#26734,#26735,#26736,#26737,#26738,#26739,#26740,#26741,#26742,#26743,#26744,
#26745,#26746,#26747,#26748,#26749,#26750,#26751,#26752,#26753,#26754,#26755,
#26756,#26757,#26758,#26759,#26760,#26761)),.UNSPECIFIED.,.F.,.F.,.F.,(4,
4),(4,1,1,2,2,1,1,1,1,1,2,1,1,1,1,1,1,1,1,1,2,1,1,1,1,2,1,1,1,1,2,1,1,2,
2,1,1,1,1,1,1,2,1,2,1,1,1,2,1,1,1,2,1,1,1,2,1,1,1,2,1,1,1,2,1,1,1,2,1,1,
1,2,1,1,1,2,1,2,1,1,1,1,1,1,2,2,1,1,2,1,1,1,1,2,1,1,1,1,2,1,1,1,1,1,1,1,
1,1,2,1,1,1,1,1,2,2,1,1,1,1,1,1,1,1,1,1,4),(-0.000390275080997305,0.745485974455544),
(0.0915777109701609,0.0937499999708451,0.104567307677615,0.105769230768995,
0.115384615384363,0.117788461567088,0.120192307692056,0.122596153817018,
0.123197115362701,0.123397435877929,0.124999999999751,0.135817307706478,
0.146634615413206,0.15745192309109,0.168269230768974,0.177884615384371,
0.187499999999768,0.199519230740103,0.206730769230503,0.210336538446854,
0.211538461538235,0.213942307720923,0.218749999970821,0.228365384586246,
0.237980769201671,0.249999999999808,0.25841346152381,0.266826923047812,
0.281250000028623,0.289663461552636,0.298076923076649,0.312499999999747,
0.31971153849016,0.326923076922846,0.33653846153821,0.338942307720942,0.340144230783416,
0.343749999970879,0.353365384586257,0.358173076951719,0.362980769201619,
0.365384615384414,0.370192307692066,0.37499999999969,0.389423076922836,
0.397836538475728,0.406250000028619,0.413461538461298,0.420673076893946,
0.425480769259405,0.427884615384363,0.432692307692057,0.433894230783419,
0.43509615387478,0.437499999999749,0.442307692307468,0.455528846139201,
0.468749999970934,0.483173076951685,0.49999999999975,0.516826923047797,
0.531250000028611,0.544471153860329,0.557692307692047,0.562499999999739,
0.563701923062234,0.564903846124729,0.567307692307427,0.569711538490167,
0.574519230740095,0.579326923105555,0.586538461538202,0.593749999970866,
0.602163461523769,0.610576923076672,0.624999999999777,0.629807692307439,
0.634615384615125,0.637019230797861,0.641826923047781,0.646634615413246,
0.656250000028622,0.659855769216081,0.661057692278563,0.663461538461287,
0.673076923076666,0.680288461509321,0.687499999999755,0.701923076922838,
0.710336538446858,0.718749999970878,0.733173076951697,0.741586538475723,
0.749999999999749,0.762019230797881,0.771634615413259,0.781250000028636,
0.786057692278561,0.788461538461294,0.78966346155265,0.793269230768981,
0.800480769259399,0.812499999999748,0.822115384615134,0.83173076923052,
0.842548076908385,0.853365384586251,0.864182692292999,0.874999999999748,
0.876602564121565,0.876802884636793,0.877403846182474,0.879807692307444,
0.882211538432407,0.884615384615134,0.894230769230516,0.895432692321882,
0.906250000028634,0.915865384644013,0.926682692321841,0.937499999999668,
0.949519230731432,0.95913461547336,0.968749998603834,0.983173100695849,
0.991586550347924,1.0000372584433),.UNSPECIFIED.);
#164=B_SPLINE_SURFACE_WITH_KNOTS('',3,3,((#29446,#29447,#29448,#29449,#29450,
#29451,#29452,#29453,#29454,#29455,#29456,#29457,#29458,#29459),(#29460,
#29461,#29462,#29463,#29464,#29465,#29466,#29467,#29468,#29469,#29470,#29471,
#29472,#29473),(#29474,#29475,#29476,#29477,#29478,#29479,#29480,#29481,
#29482,#29483,#29484,#29485,#29486,#29487),(#29488,#29489,#29490,#29491,
#29492,#29493,#29494,#29495,#29496,#29497,#29498,#29499,#29500,#29501),
(#29502,#29503,#29504,#29505,#29506,#29507,#29508,#29509,#29510,#29511,
#29512,#29513,#29514,#29515),(#29516,#29517,#29518,#29519,#29520,#29521,
#29522,#29523,#29524,#29525,#29526,#29527,#29528,#29529),(#29530,#29531,
#29532,#29533,#29534,#29535,#29536,#29537,#29538,#29539,#29540,#29541,#29542,
#29543),(#29544,#29545,#29546,#29547,#29548,#29549,#29550,#29551,#29552,
#29553,#29554,#29555,#29556,#29557),(#29558,#29559,#29560,#29561,#29562,
#29563,#29564,#29565,#29566,#29567,#29568,#29569,#29570,#29571),(#29572,
#29573,#29574,#29575,#29576,#29577,#29578,#29579,#29580,#29581,#29582,#29583,
#29584,#29585),(#29586,#29587,#29588,#29589,#29590,#29591,#29592,#29593,
#29594,#29595,#29596,#29597,#29598,#29599),(#29600,#29601,#29602,#29603,
#29604,#29605,#29606,#29607,#29608,#29609,#29610,#29611,#29612,#29613),
(#29614,#29615,#29616,#29617,#29618,#29619,#29620,#29621,#29622,#29623,
#29624,#29625,#29626,#29627),(#29628,#29629,#29630,#29631,#29632,#29633,
#29634,#29635,#29636,#29637,#29638,#29639,#29640,#29641),(#29642,#29643,
#29644,#29645,#29646,#29647,#29648,#29649,#29650,#29651,#29652,#29653,#29654,
#29655),(#29656,#29657,#29658,#29659,#29660,#29661,#29662,#29663,#29664,
#29665,#29666,#29667,#29668,#29669),(#29670,#29671,#29672,#29673,#29674,
#29675,#29676,#29677,#29678,#29679,#29680,#29681,#29682,#29683),(#29684,
#29685,#29686,#29687,#29688,#29689,#29690,#29691,#29692,#29693,#29694,#29695,
#29696,#29697),(#29698,#29699,#29700,#29701,#29702,#29703,#29704,#29705,
#29706,#29707,#29708,#29709,#29710,#29711),(#29712,#29713,#29714,#29715,
#29716,#29717,#29718,#29719,#29720,#29721,#29722,#29723,#29724,#29725),
(#29726,#29727,#29728,#29729,#29730,#29731,#29732,#29733,#29734,#29735,
#29736,#29737,#29738,#29739),(#29740,#29741,#29742,#29743,#29744,#29745,
#29746,#29747,#29748,#29749,#29750,#29751,#29752,#29753),(#29754,#29755,
#29756,#29757,#29758,#29759,#29760,#29761,#29762,#29763,#29764,#29765,#29766,
#29767),(#29768,#29769,#29770,#29771,#29772,#29773,#29774,#29775,#29776,
#29777,#29778,#29779,#29780,#29781),(#29782,#29783,#29784,#29785,#29786,
#29787,#29788,#29789,#29790,#29791,#29792,#29793,#29794,#29795),(#29796,
#29797,#29798,#29799,#29800,#29801,#29802,#29803,#29804,#29805,#29806,#29807,
#29808,#29809),(#29810,#29811,#29812,#29813,#29814,#29815,#29816,#29817,
#29818,#29819,#29820,#29821,#29822,#29823),(#29824,#29825,#29826,#29827,
#29828,#29829,#29830,#29831,#29832,#29833,#29834,#29835,#29836,#29837),
(#29838,#29839,#29840,#29841,#29842,#29843,#29844,#29845,#29846,#29847,
#29848,#29849,#29850,#29851),(#29852,#29853,#29854,#29855,#29856,#29857,
#29858,#29859,#29860,#29861,#29862,#29863,#29864,#29865),(#29866,#29867,
#29868,#29869,#29870,#29871,#29872,#29873,#29874,#29875,#29876,#29877,#29878,
#29879),(#29880,#29881,#29882,#29883,#29884,#29885,#29886,#29887,#29888,
#29889,#29890,#29891,#29892,#29893),(#29894,#29895,#29896,#29897,#29898,
#29899,#29900,#29901,#29902,#29903,#29904,#29905,#29906,#29907),(#29908,
#29909,#29910,#29911,#29912,#29913,#29914,#29915,#29916,#29917,#29918,#29919,
#29920,#29921)),.UNSPECIFIED.,.F.,.F.,.F.,(4,1,1,1,1,1,1,1,1,1,1,1,1,1,
1,1,1,1,1,1,1,1,1,1,1,1,1,1,1,1,1,4),(4,2,2,2,2,2,4),(0.0331549352864052,
0.102215297051662,0.171275658816919,0.172354726969501,0.173433795122083,
0.174512863274665,0.175591931427247,0.179908204037576,0.188540749258233,
0.19717329447889,0.205805839699547,0.223070930140861,0.240336020582176,
0.274866201464804,0.309396382347432,0.378456744112689,0.412986924995318,
0.447517105877946,0.482047286760574,0.516577467643203,0.551107648525831,
0.568372738967145,0.585637829408459,0.654698191173716,0.723758552938973,
0.79281891470423,0.827349095586858,0.861879276469487,0.896409457352115,
0.930939638234743,0.948204728676057,1.),(0.0377143719370964,0.167070624995476,
0.336553194126115,0.499999999999991,0.663446805873868,0.832929375004528,
0.962285628058762),.UNSPECIFIED.);
#165=B_SPLINE_SURFACE_WITH_KNOTS('',3,3,((#29982,#29983,#29984,#29985,#29986,
#29987,#29988,#29989,#29990,#29991,#29992,#29993,#29994,#29995),(#29996,
#29997,#29998,#29999,#30000,#30001,#30002,#30003,#30004,#30005,#30006,#30007,
#30008,#30009),(#30010,#30011,#30012,#30013,#30014,#30015,#30016,#30017,
#30018,#30019,#30020,#30021,#30022,#30023),(#30024,#30025,#30026,#30027,
#30028,#30029,#30030,#30031,#30032,#30033,#30034,#30035,#30036,#30037)),
 .UNSPECIFIED.,.F.,.F.,.F.,(4,4),(4,2,2,2,2,2,4),(0.,1.),(0.0377143719414207,
0.167070624995476,0.336553194126115,0.499999999999991,0.663446805873868,
0.832929375004528,0.962285628058582),.UNSPECIFIED.);
#166=B_SPLINE_SURFACE_WITH_KNOTS('',3,3,((#30052,#30053,#30054,#30055,#30056,
#30057,#30058,#30059,#30060,#30061,#30062,#30063,#30064,#30065),(#30066,
#30067,#30068,#30069,#30070,#30071,#30072,#30073,#30074,#30075,#30076,#30077,
#30078,#30079),(#30080,#30081,#30082,#30083,#30084,#30085,#30086,#30087,
#30088,#30089,#30090,#30091,#30092,#30093),(#30094,#30095,#30096,#30097,
#30098,#30099,#30100,#30101,#30102,#30103,#30104,#30105,#30106,#30107),
(#30108,#30109,#30110,#30111,#30112,#30113,#30114,#30115,#30116,#30117,
#30118,#30119,#30120,#30121),(#30122,#30123,#30124,#30125,#30126,#30127,
#30128,#30129,#30130,#30131,#30132,#30133,#30134,#30135),(#30136,#30137,
#30138,#30139,#30140,#30141,#30142,#30143,#30144,#30145,#30146,#30147,#30148,
#30149),(#30150,#30151,#30152,#30153,#30154,#30155,#30156,#30157,#30158,
#30159,#30160,#30161,#30162,#30163),(#30164,#30165,#30166,#30167,#30168,
#30169,#30170,#30171,#30172,#30173,#30174,#30175,#30176,#30177),(#30178,
#30179,#30180,#30181,#30182,#30183,#30184,#30185,#30186,#30187,#30188,#30189,
#30190,#30191),(#30192,#30193,#30194,#30195,#30196,#30197,#30198,#30199,
#30200,#30201,#30202,#30203,#30204,#30205),(#30206,#30207,#30208,#30209,
#30210,#30211,#30212,#30213,#30214,#30215,#30216,#30217,#30218,#30219),
(#30220,#30221,#30222,#30223,#30224,#30225,#30226,#30227,#30228,#30229,
#30230,#30231,#30232,#30233),(#30234,#30235,#30236,#30237,#30238,#30239,
#30240,#30241,#30242,#30243,#30244,#30245,#30246,#30247),(#30248,#30249,
#30250,#30251,#30252,#30253,#30254,#30255,#30256,#30257,#30258,#30259,#30260,
#30261),(#30262,#30263,#30264,#30265,#30266,#30267,#30268,#30269,#30270,
#30271,#30272,#30273,#30274,#30275),(#30276,#30277,#30278,#30279,#30280,
#30281,#30282,#30283,#30284,#30285,#30286,#30287,#30288,#30289),(#30290,
#30291,#30292,#30293,#30294,#30295,#30296,#30297,#30298,#30299,#30300,#30301,
#30302,#30303),(#30304,#30305,#30306,#30307,#30308,#30309,#30310,#30311,
#30312,#30313,#30314,#30315,#30316,#30317),(#30318,#30319,#30320,#30321,
#30322,#30323,#30324,#30325,#30326,#30327,#30328,#30329,#30330,#30331),
(#30332,#30333,#30334,#30335,#30336,#30337,#30338,#30339,#30340,#30341,
#30342,#30343,#30344,#30345),(#30346,#30347,#30348,#30349,#30350,#30351,
#30352,#30353,#30354,#30355,#30356,#30357,#30358,#30359),(#30360,#30361,
#30362,#30363,#30364,#30365,#30366,#30367,#30368,#30369,#30370,#30371,#30372,
#30373),(#30374,#30375,#30376,#30377,#30378,#30379,#30380,#30381,#30382,
#30383,#30384,#30385,#30386,#30387),(#30388,#30389,#30390,#30391,#30392,
#30393,#30394,#30395,#30396,#30397,#30398,#30399,#30400,#30401),(#30402,
#30403,#30404,#30405,#30406,#30407,#30408,#30409,#30410,#30411,#30412,#30413,
#30414,#30415),(#30416,#30417,#30418,#30419,#30420,#30421,#30422,#30423,
#30424,#30425,#30426,#30427,#30428,#30429),(#30430,#30431,#30432,#30433,
#30434,#30435,#30436,#30437,#30438,#30439,#30440,#30441,#30442,#30443),
(#30444,#30445,#30446,#30447,#30448,#30449,#30450,#30451,#30452,#30453,
#30454,#30455,#30456,#30457),(#30458,#30459,#30460,#30461,#30462,#30463,
#30464,#30465,#30466,#30467,#30468,#30469,#30470,#30471),(#30472,#30473,
#30474,#30475,#30476,#30477,#30478,#30479,#30480,#30481,#30482,#30483,#30484,
#30485),(#30486,#30487,#30488,#30489,#30490,#30491,#30492,#30493,#30494,
#30495,#30496,#30497,#30498,#30499),(#30500,#30501,#30502,#30503,#30504,
#30505,#30506,#30507,#30508,#30509,#30510,#30511,#30512,#30513),(#30514,
#30515,#30516,#30517,#30518,#30519,#30520,#30521,#30522,#30523,#30524,#30525,
#30526,#30527),(#30528,#30529,#30530,#30531,#30532,#30533,#30534,#30535,
#30536,#30537,#30538,#30539,#30540,#30541),(#30542,#30543,#30544,#30545,
#30546,#30547,#30548,#30549,#30550,#30551,#30552,#30553,#30554,#30555),
(#30556,#30557,#30558,#30559,#30560,#30561,#30562,#30563,#30564,#30565,
#30566,#30567,#30568,#30569)),.UNSPECIFIED.,.F.,.F.,.F.,(4,1,1,1,1,1,1,
1,1,1,1,1,1,1,1,1,1,1,1,1,1,1,1,1,1,1,1,1,1,1,1,1,1,1,4),(4,2,2,2,2,2,4),
(0.,0.0517952713240545,0.069060361765406,0.103590542648109,0.138120723530812,
0.146753268751488,0.155385813972164,0.189915994854866,0.276241447061624,
0.34530180882703,0.379831989709733,0.414362170592436,0.448892351475139,
0.46615744191649,0.483422532357842,0.552482894123248,0.587013075005951,
0.621543255888654,0.69060361765406,0.759663979419466,0.776929069860817,
0.794194160302169,0.802826705522845,0.81145925074352,0.815775523353858,
0.820091795964196,0.822249932269365,0.824408068574534,0.826566204879703,
0.827645273032287,0.82818480710858,0.828724341184872,0.897784702950278,
0.932314883832981,0.966845064715684),(0.037714371941,0.167070624995476,
0.336553194126115,0.499999999999991,0.663446805873868,0.832929375004528,
0.962285628058665),.UNSPECIFIED.);
#167=B_SPLINE_SURFACE_WITH_KNOTS('',3,3,((#30669,#30670,#30671,#30672,#30673,
#30674,#30675,#30676,#30677,#30678,#30679,#30680,#30681,#30682),(#30683,
#30684,#30685,#30686,#30687,#30688,#30689,#30690,#30691,#30692,#30693,#30694,
#30695,#30696),(#30697,#30698,#30699,#30700,#30701,#30702,#30703,#30704,
#30705,#30706,#30707,#30708,#30709,#30710),(#30711,#30712,#30713,#30714,
#30715,#30716,#30717,#30718,#30719,#30720,#30721,#30722,#30723,#30724),
(#30725,#30726,#30727,#30728,#30729,#30730,#30731,#30732,#30733,#30734,
#30735,#30736,#30737,#30738),(#30739,#30740,#30741,#30742,#30743,#30744,
#30745,#30746,#30747,#30748,#30749,#30750,#30751,#30752),(#30753,#30754,
#30755,#30756,#30757,#30758,#30759,#30760,#30761,#30762,#30763,#30764,#30765,
#30766),(#30767,#30768,#30769,#30770,#30771,#30772,#30773,#30774,#30775,
#30776,#30777,#30778,#30779,#30780),(#30781,#30782,#30783,#30784,#30785,
#30786,#30787,#30788,#30789,#30790,#30791,#30792,#30793,#30794),(#30795,
#30796,#30797,#30798,#30799,#30800,#30801,#30802,#30803,#30804,#30805,#30806,
#30807,#30808),(#30809,#30810,#30811,#30812,#30813,#30814,#30815,#30816,
#30817,#30818,#30819,#30820,#30821,#30822),(#30823,#30824,#30825,#30826,
#30827,#30828,#30829,#30830,#30831,#30832,#30833,#30834,#30835,#30836),
(#30837,#30838,#30839,#30840,#30841,#30842,#30843,#30844,#30845,#30846,
#30847,#30848,#30849,#30850),(#30851,#30852,#30853,#30854,#30855,#30856,
#30857,#30858,#30859,#30860,#30861,#30862,#30863,#30864),(#30865,#30866,
#30867,#30868,#30869,#30870,#30871,#30872,#30873,#30874,#30875,#30876,#30877,
#30878),(#30879,#30880,#30881,#30882,#30883,#30884,#30885,#30886,#30887,
#30888,#30889,#30890,#30891,#30892),(#30893,#30894,#30895,#30896,#30897,
#30898,#30899,#30900,#30901,#30902,#30903,#30904,#30905,#30906),(#30907,
#30908,#30909,#30910,#30911,#30912,#30913,#30914,#30915,#30916,#30917,#30918,
#30919,#30920),(#30921,#30922,#30923,#30924,#30925,#30926,#30927,#30928,
#30929,#30930,#30931,#30932,#30933,#30934),(#30935,#30936,#30937,#30938,
#30939,#30940,#30941,#30942,#30943,#30944,#30945,#30946,#30947,#30948),
(#30949,#30950,#30951,#30952,#30953,#30954,#30955,#30956,#30957,#30958,
#30959,#30960,#30961,#30962),(#30963,#30964,#30965,#30966,#30967,#30968,
#30969,#30970,#30971,#30972,#30973,#30974,#30975,#30976),(#30977,#30978,
#30979,#30980,#30981,#30982,#30983,#30984,#30985,#30986,#30987,#30988,#30989,
#30990),(#30991,#30992,#30993,#30994,#30995,#30996,#30997,#30998,#30999,
#31000,#31001,#31002,#31003,#31004),(#31005,#31006,#31007,#31008,#31009,
#31010,#31011,#31012,#31013,#31014,#31015,#31016,#31017,#31018),(#31019,
#31020,#31021,#31022,#31023,#31024,#31025,#31026,#31027,#31028,#31029,#31030,
#31031,#31032),(#31033,#31034,#31035,#31036,#31037,#31038,#31039,#31040,
#31041,#31042,#31043,#31044,#31045,#31046),(#31047,#31048,#31049,#31050,
#31051,#31052,#31053,#31054,#31055,#31056,#31057,#31058,#31059,#31060),
(#31061,#31062,#31063,#31064,#31065,#31066,#31067,#31068,#31069,#31070,
#31071,#31072,#31073,#31074),(#31075,#31076,#31077,#31078,#31079,#31080,
#31081,#31082,#31083,#31084,#31085,#31086,#31087,#31088),(#31089,#31090,
#31091,#31092,#31093,#31094,#31095,#31096,#31097,#31098,#31099,#31100,#31101,
#31102),(#31103,#31104,#31105,#31106,#31107,#31108,#31109,#31110,#31111,
#31112,#31113,#31114,#31115,#31116),(#31117,#31118,#31119,#31120,#31121,
#31122,#31123,#31124,#31125,#31126,#31127,#31128,#31129,#31130),(#31131,
#31132,#31133,#31134,#31135,#31136,#31137,#31138,#31139,#31140,#31141,#31142,
#31143,#31144),(#31145,#31146,#31147,#31148,#31149,#31150,#31151,#31152,
#31153,#31154,#31155,#31156,#31157,#31158),(#31159,#31160,#31161,#31162,
#31163,#31164,#31165,#31166,#31167,#31168,#31169,#31170,#31171,#31172)),
 .UNSPECIFIED.,.F.,.F.,.F.,(4,1,1,1,1,1,1,1,1,1,1,1,1,1,1,1,1,1,1,1,1,1,
1,1,1,1,1,1,1,1,1,1,1,4),(4,2,2,2,2,2,4),(0.033154935286399,0.0676851161690276,
0.102215297051656,0.171275658816913,0.172354726969496,0.173433795122078,
0.17451286327466,0.175591931427242,0.179908204037571,0.188540749258228,
0.197173294478885,0.205805839699542,0.223070930140856,0.240336020582171,
0.274866201464799,0.309396382347428,0.378456744112685,0.412986924995314,
0.447517105877942,0.482047286760571,0.5165774676432,0.551107648525828,0.568372738967142,
0.585637829408457,0.654698191173714,0.706493462497657,0.723758552938971,
0.792818914704228,0.827349095586857,0.861879276469486,0.896409457352114,
0.930939638234743,0.948204728676057,1.),(0.0377143719407808,0.167070624995476,
0.336553194126115,0.499999999999991,0.663446805873868,0.832929375004528,
0.962285628059334),.UNSPECIFIED.);
#168=B_SPLINE_SURFACE_WITH_KNOTS('',3,3,((#31237,#31238,#31239,#31240,#31241,
#31242,#31243,#31244,#31245,#31246,#31247,#31248,#31249,#31250),(#31251,
#31252,#31253,#31254,#31255,#31256,#31257,#31258,#31259,#31260,#31261,#31262,
#31263,#31264),(#31265,#31266,#31267,#31268,#31269,#31270,#31271,#31272,
#31273,#31274,#31275,#31276,#31277,#31278),(#31279,#31280,#31281,#31282,
#31283,#31284,#31285,#31286,#31287,#31288,#31289,#31290,#31291,#31292)),
 .UNSPECIFIED.,.F.,.F.,.F.,(4,4),(4,2,2,2,2,2,4),(0.,1.),(0.0377143719414207,
0.167070624995476,0.336553194126115,0.499999999999991,0.663446805873868,
0.832929375004528,0.962285628058582),.UNSPECIFIED.);
#169=B_SPLINE_SURFACE_WITH_KNOTS('',3,3,((#31307,#31308,#31309,#31310,#31311,
#31312,#31313,#31314,#31315,#31316,#31317,#31318,#31319,#31320),(#31321,
#31322,#31323,#31324,#31325,#31326,#31327,#31328,#31329,#31330,#31331,#31332,
#31333,#31334),(#31335,#31336,#31337,#31338,#31339,#31340,#31341,#31342,
#31343,#31344,#31345,#31346,#31347,#31348),(#31349,#31350,#31351,#31352,
#31353,#31354,#31355,#31356,#31357,#31358,#31359,#31360,#31361,#31362),
(#31363,#31364,#31365,#31366,#31367,#31368,#31369,#31370,#31371,#31372,
#31373,#31374,#31375,#31376),(#31377,#31378,#31379,#31380,#31381,#31382,
#31383,#31384,#31385,#31386,#31387,#31388,#31389,#31390),(#31391,#31392,
#31393,#31394,#31395,#31396,#31397,#31398,#31399,#31400,#31401,#31402,#31403,
#31404),(#31405,#31406,#31407,#31408,#31409,#31410,#31411,#31412,#31413,
#31414,#31415,#31416,#31417,#31418),(#31419,#31420,#31421,#31422,#31423,
#31424,#31425,#31426,#31427,#31428,#31429,#31430,#31431,#31432),(#31433,
#31434,#31435,#31436,#31437,#31438,#31439,#31440,#31441,#31442,#31443,#31444,
#31445,#31446),(#31447,#31448,#31449,#31450,#31451,#31452,#31453,#31454,
#31455,#31456,#31457,#31458,#31459,#31460),(#31461,#31462,#31463,#31464,
#31465,#31466,#31467,#31468,#31469,#31470,#31471,#31472,#31473,#31474),
(#31475,#31476,#31477,#31478,#31479,#31480,#31481,#31482,#31483,#31484,
#31485,#31486,#31487,#31488),(#31489,#31490,#31491,#31492,#31493,#31494,
#31495,#31496,#31497,#31498,#31499,#31500,#31501,#31502),(#31503,#31504,
#31505,#31506,#31507,#31508,#31509,#31510,#31511,#31512,#31513,#31514,#31515,
#31516),(#31517,#31518,#31519,#31520,#31521,#31522,#31523,#31524,#31525,
#31526,#31527,#31528,#31529,#31530),(#31531,#31532,#31533,#31534,#31535,
#31536,#31537,#31538,#31539,#31540,#31541,#31542,#31543,#31544),(#31545,
#31546,#31547,#31548,#31549,#31550,#31551,#31552,#31553,#31554,#31555,#31556,
#31557,#31558),(#31559,#31560,#31561,#31562,#31563,#31564,#31565,#31566,
#31567,#31568,#31569,#31570,#31571,#31572),(#31573,#31574,#31575,#31576,
#31577,#31578,#31579,#31580,#31581,#31582,#31583,#31584,#31585,#31586),
(#31587,#31588,#31589,#31590,#31591,#31592,#31593,#31594,#31595,#31596,
#31597,#31598,#31599,#31600),(#31601,#31602,#31603,#31604,#31605,#31606,
#31607,#31608,#31609,#31610,#31611,#31612,#31613,#31614),(#31615,#31616,
#31617,#31618,#31619,#31620,#31621,#31622,#31623,#31624,#31625,#31626,#31627,
#31628),(#31629,#31630,#31631,#31632,#31633,#31634,#31635,#31636,#31637,
#31638,#31639,#31640,#31641,#31642),(#31643,#31644,#31645,#31646,#31647,
#31648,#31649,#31650,#31651,#31652,#31653,#31654,#31655,#31656),(#31657,
#31658,#31659,#31660,#31661,#31662,#31663,#31664,#31665,#31666,#31667,#31668,
#31669,#31670),(#31671,#31672,#31673,#31674,#31675,#31676,#31677,#31678,
#31679,#31680,#31681,#31682,#31683,#31684),(#31685,#31686,#31687,#31688,
#31689,#31690,#31691,#31692,#31693,#31694,#31695,#31696,#31697,#31698),
(#31699,#31700,#31701,#31702,#31703,#31704,#31705,#31706,#31707,#31708,
#31709,#31710,#31711,#31712),(#31713,#31714,#31715,#31716,#31717,#31718,
#31719,#31720,#31721,#31722,#31723,#31724,#31725,#31726),(#31727,#31728,
#31729,#31730,#31731,#31732,#31733,#31734,#31735,#31736,#31737,#31738,#31739,
#31740),(#31741,#31742,#31743,#31744,#31745,#31746,#31747,#31748,#31749,
#31750,#31751,#31752,#31753,#31754),(#31755,#31756,#31757,#31758,#31759,
#31760,#31761,#31762,#31763,#31764,#31765,#31766,#31767,#31768),(#31769,
#31770,#31771,#31772,#31773,#31774,#31775,#31776,#31777,#31778,#31779,#31780,
#31781,#31782),(#31783,#31784,#31785,#31786,#31787,#31788,#31789,#31790,
#31791,#31792,#31793,#31794,#31795,#31796),(#31797,#31798,#31799,#31800,
#31801,#31802,#31803,#31804,#31805,#31806,#31807,#31808,#31809,#31810),
(#31811,#31812,#31813,#31814,#31815,#31816,#31817,#31818,#31819,#31820,
#31821,#31822,#31823,#31824),(#31825,#31826,#31827,#31828,#31829,#31830,
#31831,#31832,#31833,#31834,#31835,#31836,#31837,#31838),(#31839,#31840,
#31841,#31842,#31843,#31844,#31845,#31846,#31847,#31848,#31849,#31850,#31851,
#31852),(#31853,#31854,#31855,#31856,#31857,#31858,#31859,#31860,#31861,
#31862,#31863,#31864,#31865,#31866),(#31867,#31868,#31869,#31870,#31871,
#31872,#31873,#31874,#31875,#31876,#31877,#31878,#31879,#31880)),
 .UNSPECIFIED.,.F.,.F.,.F.,(4,1,1,1,1,1,1,1,1,1,1,1,1,1,1,1,1,1,1,1,1,1,
1,1,1,1,1,1,1,1,1,1,1,1,1,1,1,1,4),(4,2,2,2,2,2,4),(0.,0.0517952713240545,
0.069060361765406,0.103590542648109,0.138120723530812,0.155385813972164,
0.172650904413515,0.207181085296218,0.276241447061624,0.34530180882703,
0.379831989709733,0.414362170592436,0.448892351475139,0.483422532357842,
0.552482894123248,0.5697479845646,0.621543255888654,0.638808346330006,0.69060361765406,
0.707868708095412,0.716501253316088,0.725133798536763,0.759663979419467,
0.768296524640142,0.776929069860818,0.79419416030217,0.802826705522845,
0.811459250743521,0.820091795964197,0.824408068574535,0.825487136727119,
0.826566204879704,0.827645273032288,0.82818480710858,0.828454574146726,
0.828724341184873,0.897784702950279,0.932314883832982,0.966845064715685),
(0.0377143719412118,0.167070624995476,0.336553194126115,0.499999999999991,
0.663446805873868,0.832929375004528,0.962285628060063),.UNSPECIFIED.);
#170=B_SPLINE_SURFACE_WITH_KNOTS('',3,3,((#31940,#31941,#31942,#31943,#31944,
#31945,#31946,#31947,#31948,#31949,#31950,#31951,#31952,#31953),(#31954,
#31955,#31956,#31957,#31958,#31959,#31960,#31961,#31962,#31963,#31964,#31965,
#31966,#31967),(#31968,#31969,#31970,#31971,#31972,#31973,#31974,#31975,
#31976,#31977,#31978,#31979,#31980,#31981),(#31982,#31983,#31984,#31985,
#31986,#31987,#31988,#31989,#31990,#31991,#31992,#31993,#31994,#31995),
(#31996,#31997,#31998,#31999,#32000,#32001,#32002,#32003,#32004,#32005,
#32006,#32007,#32008,#32009),(#32010,#32011,#32012,#32013,#32014,#32015,
#32016,#32017,#32018,#32019,#32020,#32021,#32022,#32023),(#32024,#32025,
#32026,#32027,#32028,#32029,#32030,#32031,#32032,#32033,#32034,#32035,#32036,
#32037),(#32038,#32039,#32040,#32041,#32042,#32043,#32044,#32045,#32046,
#32047,#32048,#32049,#32050,#32051),(#32052,#32053,#32054,#32055,#32056,
#32057,#32058,#32059,#32060,#32061,#32062,#32063,#32064,#32065),(#32066,
#32067,#32068,#32069,#32070,#32071,#32072,#32073,#32074,#32075,#32076,#32077,
#32078,#32079),(#32080,#32081,#32082,#32083,#32084,#32085,#32086,#32087,
#32088,#32089,#32090,#32091,#32092,#32093),(#32094,#32095,#32096,#32097,
#32098,#32099,#32100,#32101,#32102,#32103,#32104,#32105,#32106,#32107),
(#32108,#32109,#32110,#32111,#32112,#32113,#32114,#32115,#32116,#32117,
#32118,#32119,#32120,#32121),(#32122,#32123,#32124,#32125,#32126,#32127,
#32128,#32129,#32130,#32131,#32132,#32133,#32134,#32135),(#32136,#32137,
#32138,#32139,#32140,#32141,#32142,#32143,#32144,#32145,#32146,#32147,#32148,
#32149),(#32150,#32151,#32152,#32153,#32154,#32155,#32156,#32157,#32158,
#32159,#32160,#32161,#32162,#32163),(#32164,#32165,#32166,#32167,#32168,
#32169,#32170,#32171,#32172,#32173,#32174,#32175,#32176,#32177),(#32178,
#32179,#32180,#32181,#32182,#32183,#32184,#32185,#32186,#32187,#32188,#32189,
#32190,#32191),(#32192,#32193,#32194,#32195,#32196,#32197,#32198,#32199,
#32200,#32201,#32202,#32203,#32204,#32205),(#32206,#32207,#32208,#32209,
#32210,#32211,#32212,#32213,#32214,#32215,#32216,#32217,#32218,#32219),
(#32220,#32221,#32222,#32223,#32224,#32225,#32226,#32227,#32228,#32229,
#32230,#32231,#32232,#32233),(#32234,#32235,#32236,#32237,#32238,#32239,
#32240,#32241,#32242,#32243,#32244,#32245,#32246,#32247),(#32248,#32249,
#32250,#32251,#32252,#32253,#32254,#32255,#32256,#32257,#32258,#32259,#32260,
#32261),(#32262,#32263,#32264,#32265,#32266,#32267,#32268,#32269,#32270,
#32271,#32272,#32273,#32274,#32275),(#32276,#32277,#32278,#32279,#32280,
#32281,#32282,#32283,#32284,#32285,#32286,#32287,#32288,#32289),(#32290,
#32291,#32292,#32293,#32294,#32295,#32296,#32297,#32298,#32299,#32300,#32301,
#32302,#32303),(#32304,#32305,#32306,#32307,#32308,#32309,#32310,#32311,
#32312,#32313,#32314,#32315,#32316,#32317),(#32318,#32319,#32320,#32321,
#32322,#32323,#32324,#32325,#32326,#32327,#32328,#32329,#32330,#32331),
(#32332,#32333,#32334,#32335,#32336,#32337,#32338,#32339,#32340,#32341,
#32342,#32343,#32344,#32345),(#32346,#32347,#32348,#32349,#32350,#32351,
#32352,#32353,#32354,#32355,#32356,#32357,#32358,#32359),(#32360,#32361,
#32362,#32363,#32364,#32365,#32366,#32367,#32368,#32369,#32370,#32371,#32372,
#32373),(#32374,#32375,#32376,#32377,#32378,#32379,#32380,#32381,#32382,
#32383,#32384,#32385,#32386,#32387),(#32388,#32389,#32390,#32391,#32392,
#32393,#32394,#32395,#32396,#32397,#32398,#32399,#32400,#32401),(#32402,
#32403,#32404,#32405,#32406,#32407,#32408,#32409,#32410,#32411,#32412,#32413,
#32414,#32415),(#32416,#32417,#32418,#32419,#32420,#32421,#32422,#32423,
#32424,#32425,#32426,#32427,#32428,#32429),(#32430,#32431,#32432,#32433,
#32434,#32435,#32436,#32437,#32438,#32439,#32440,#32441,#32442,#32443),
(#32444,#32445,#32446,#32447,#32448,#32449,#32450,#32451,#32452,#32453,
#32454,#32455,#32456,#32457)),.UNSPECIFIED.,.F.,.F.,.F.,(4,1,1,1,1,1,1,
1,1,1,1,1,1,1,1,1,1,1,1,1,1,1,1,1,1,1,1,1,1,1,1,1,1,1,4),(4,2,2,2,2,2,4),
(0.0331549352864065,0.0676851161690348,0.102215297051663,0.17127565881692,
0.171815192893211,0.172354726969502,0.172894261045793,0.173433795122084,
0.175591931427248,0.179908204037577,0.184224476647905,0.188540749258234,
0.205805839699548,0.223070930140862,0.240336020582177,0.274866201464805,
0.309396382347433,0.37845674411269,0.412986924995318,0.447517105877947,
0.482047286760575,0.516577467643203,0.551107648525831,0.568372738967146,
0.58563782940846,0.654698191173717,0.706493462497659,0.723758552938973,
0.79281891470423,0.827349095586858,0.861879276469487,0.896409457352115,
0.930939638234743,0.948204728676057,1.),(0.0377143719413302,0.167070624995476,
0.336553194126115,0.499999999999991,0.663446805873868,0.832929375004528,
0.962285628059334),.UNSPECIFIED.);
#171=B_SPLINE_SURFACE_WITH_KNOTS('',3,3,((#32522,#32523,#32524,#32525,#32526,
#32527,#32528,#32529,#32530,#32531,#32532,#32533,#32534,#32535),(#32536,
#32537,#32538,#32539,#32540,#32541,#32542,#32543,#32544,#32545,#32546,#32547,
#32548,#32549),(#32550,#32551,#32552,#32553,#32554,#32555,#32556,#32557,
#32558,#32559,#32560,#32561,#32562,#32563),(#32564,#32565,#32566,#32567,
#32568,#32569,#32570,#32571,#32572,#32573,#32574,#32575,#32576,#32577)),
 .UNSPECIFIED.,.F.,.F.,.F.,(4,4),(4,2,2,2,2,2,4),(0.,1.),(0.0377143719414212,
0.167070624995476,0.336553194126115,0.499999999999991,0.663446805873868,
0.832929375004528,0.962285628058582),.UNSPECIFIED.);
#172=B_SPLINE_SURFACE_WITH_KNOTS('',3,3,((#32592,#32593,#32594,#32595,#32596,
#32597,#32598,#32599,#32600,#32601,#32602,#32603,#32604,#32605),(#32606,
#32607,#32608,#32609,#32610,#32611,#32612,#32613,#32614,#32615,#32616,#32617,
#32618,#32619),(#32620,#32621,#32622,#32623,#32624,#32625,#32626,#32627,
#32628,#32629,#32630,#32631,#32632,#32633),(#32634,#32635,#32636,#32637,
#32638,#32639,#32640,#32641,#32642,#32643,#32644,#32645,#32646,#32647),
(#32648,#32649,#32650,#32651,#32652,#32653,#32654,#32655,#32656,#32657,
#32658,#32659,#32660,#32661),(#32662,#32663,#32664,#32665,#32666,#32667,
#32668,#32669,#32670,#32671,#32672,#32673,#32674,#32675),(#32676,#32677,
#32678,#32679,#32680,#32681,#32682,#32683,#32684,#32685,#32686,#32687,#32688,
#32689),(#32690,#32691,#32692,#32693,#32694,#32695,#32696,#32697,#32698,
#32699,#32700,#32701,#32702,#32703),(#32704,#32705,#32706,#32707,#32708,
#32709,#32710,#32711,#32712,#32713,#32714,#32715,#32716,#32717),(#32718,
#32719,#32720,#32721,#32722,#32723,#32724,#32725,#32726,#32727,#32728,#32729,
#32730,#32731),(#32732,#32733,#32734,#32735,#32736,#32737,#32738,#32739,
#32740,#32741,#32742,#32743,#32744,#32745),(#32746,#32747,#32748,#32749,
#32750,#32751,#32752,#32753,#32754,#32755,#32756,#32757,#32758,#32759),
(#32760,#32761,#32762,#32763,#32764,#32765,#32766,#32767,#32768,#32769,
#32770,#32771,#32772,#32773),(#32774,#32775,#32776,#32777,#32778,#32779,
#32780,#32781,#32782,#32783,#32784,#32785,#32786,#32787),(#32788,#32789,
#32790,#32791,#32792,#32793,#32794,#32795,#32796,#32797,#32798,#32799,#32800,
#32801),(#32802,#32803,#32804,#32805,#32806,#32807,#32808,#32809,#32810,
#32811,#32812,#32813,#32814,#32815),(#32816,#32817,#32818,#32819,#32820,
#32821,#32822,#32823,#32824,#32825,#32826,#32827,#32828,#32829),(#32830,
#32831,#32832,#32833,#32834,#32835,#32836,#32837,#32838,#32839,#32840,#32841,
#32842,#32843),(#32844,#32845,#32846,#32847,#32848,#32849,#32850,#32851,
#32852,#32853,#32854,#32855,#32856,#32857),(#32858,#32859,#32860,#32861,
#32862,#32863,#32864,#32865,#32866,#32867,#32868,#32869,#32870,#32871),
(#32872,#32873,#32874,#32875,#32876,#32877,#32878,#32879,#32880,#32881,
#32882,#32883,#32884,#32885),(#32886,#32887,#32888,#32889,#32890,#32891,
#32892,#32893,#32894,#32895,#32896,#32897,#32898,#32899),(#32900,#32901,
#32902,#32903,#32904,#32905,#32906,#32907,#32908,#32909,#32910,#32911,#32912,
#32913),(#32914,#32915,#32916,#32917,#32918,#32919,#32920,#32921,#32922,
#32923,#32924,#32925,#32926,#32927),(#32928,#32929,#32930,#32931,#32932,
#32933,#32934,#32935,#32936,#32937,#32938,#32939,#32940,#32941),(#32942,
#32943,#32944,#32945,#32946,#32947,#32948,#32949,#32950,#32951,#32952,#32953,
#32954,#32955),(#32956,#32957,#32958,#32959,#32960,#32961,#32962,#32963,
#32964,#32965,#32966,#32967,#32968,#32969),(#32970,#32971,#32972,#32973,
#32974,#32975,#32976,#32977,#32978,#32979,#32980,#32981,#32982,#32983),
(#32984,#32985,#32986,#32987,#32988,#32989,#32990,#32991,#32992,#32993,
#32994,#32995,#32996,#32997),(#32998,#32999,#33000,#33001,#33002,#33003,
#33004,#33005,#33006,#33007,#33008,#33009,#33010,#33011),(#33012,#33013,
#33014,#33015,#33016,#33017,#33018,#33019,#33020,#33021,#33022,#33023,#33024,
#33025),(#33026,#33027,#33028,#33029,#33030,#33031,#33032,#33033,#33034,
#33035,#33036,#33037,#33038,#33039),(#33040,#33041,#33042,#33043,#33044,
#33045,#33046,#33047,#33048,#33049,#33050,#33051,#33052,#33053),(#33054,
#33055,#33056,#33057,#33058,#33059,#33060,#33061,#33062,#33063,#33064,#33065,
#33066,#33067),(#33068,#33069,#33070,#33071,#33072,#33073,#33074,#33075,
#33076,#33077,#33078,#33079,#33080,#33081),(#33082,#33083,#33084,#33085,
#33086,#33087,#33088,#33089,#33090,#33091,#33092,#33093,#33094,#33095),
(#33096,#33097,#33098,#33099,#33100,#33101,#33102,#33103,#33104,#33105,
#33106,#33107,#33108,#33109),(#33110,#33111,#33112,#33113,#33114,#33115,
#33116,#33117,#33118,#33119,#33120,#33121,#33122,#33123),(#33124,#33125,
#33126,#33127,#33128,#33129,#33130,#33131,#33132,#33133,#33134,#33135,#33136,
#33137),(#33138,#33139,#33140,#33141,#33142,#33143,#33144,#33145,#33146,
#33147,#33148,#33149,#33150,#33151),(#33152,#33153,#33154,#33155,#33156,
#33157,#33158,#33159,#33160,#33161,#33162,#33163,#33164,#33165),(#33166,
#33167,#33168,#33169,#33170,#33171,#33172,#33173,#33174,#33175,#33176,#33177,
#33178,#33179),(#33180,#33181,#33182,#33183,#33184,#33185,#33186,#33187,
#33188,#33189,#33190,#33191,#33192,#33193),(#33194,#33195,#33196,#33197,
#33198,#33199,#33200,#33201,#33202,#33203,#33204,#33205,#33206,#33207),
(#33208,#33209,#33210,#33211,#33212,#33213,#33214,#33215,#33216,#33217,
#33218,#33219,#33220,#33221),(#33222,#33223,#33224,#33225,#33226,#33227,
#33228,#33229,#33230,#33231,#33232,#33233,#33234,#33235),(#33236,#33237,
#33238,#33239,#33240,#33241,#33242,#33243,#33244,#33245,#33246,#33247,#33248,
#33249)),.UNSPECIFIED.,.F.,.F.,.F.,(4,1,1,1,1,1,1,1,1,1,1,1,1,1,1,1,1,1,
1,1,1,1,1,1,1,1,1,1,1,1,1,1,1,1,1,1,1,1,1,1,1,1,1,1,4),(4,2,2,2,2,2,4),
(0.,0.0517952713240546,0.0690603617654062,0.103590542648109,0.138120723530812,
0.155385813972164,0.172650904413515,0.207181085296219,0.276241447061625,
0.345301808827031,0.379831989709734,0.414362170592437,0.422994715813113,
0.431627261033789,0.44889235147514,0.466157441916492,0.483422532357843,
0.552482894123249,0.621543255888656,0.656073436771359,0.690603617654062,
0.699236162874738,0.707868708095413,0.725133798536765,0.759663979419468,
0.77692906986082,0.785561615081495,0.789877887691833,0.794194160302171,
0.802826705522847,0.811459250743523,0.81577552335386,0.820091795964198,
0.824408068574536,0.826566204879705,0.827105738955997,0.82764527303229,
0.828184807108582,0.828454574146728,0.828589457665801,0.828724341184874,
0.880519612508929,0.89778470295028,0.932314883832983,0.966845064715687),
(0.0377143719413724,0.167070624995476,0.336553194126115,0.499999999999991,
0.663446805873868,0.832929375004528,0.96228562805881),.UNSPECIFIED.);
#173=B_SPLINE_SURFACE_WITH_KNOTS('',3,3,((#33305,#33306,#33307,#33308,#33309,
#33310,#33311,#33312,#33313,#33314,#33315,#33316,#33317,#33318),(#33319,
#33320,#33321,#33322,#33323,#33324,#33325,#33326,#33327,#33328,#33329,#33330,
#33331,#33332),(#33333,#33334,#33335,#33336,#33337,#33338,#33339,#33340,
#33341,#33342,#33343,#33344,#33345,#33346),(#33347,#33348,#33349,#33350,
#33351,#33352,#33353,#33354,#33355,#33356,#33357,#33358,#33359,#33360),
(#33361,#33362,#33363,#33364,#33365,#33366,#33367,#33368,#33369,#33370,
#33371,#33372,#33373,#33374),(#33375,#33376,#33377,#33378,#33379,#33380,
#33381,#33382,#33383,#33384,#33385,#33386,#33387,#33388),(#33389,#33390,
#33391,#33392,#33393,#33394,#33395,#33396,#33397,#33398,#33399,#33400,#33401,
#33402),(#33403,#33404,#33405,#33406,#33407,#33408,#33409,#33410,#33411,
#33412,#33413,#33414,#33415,#33416),(#33417,#33418,#33419,#33420,#33421,
#33422,#33423,#33424,#33425,#33426,#33427,#33428,#33429,#33430),(#33431,
#33432,#33433,#33434,#33435,#33436,#33437,#33438,#33439,#33440,#33441,#33442,
#33443,#33444),(#33445,#33446,#33447,#33448,#33449,#33450,#33451,#33452,
#33453,#33454,#33455,#33456,#33457,#33458),(#33459,#33460,#33461,#33462,
#33463,#33464,#33465,#33466,#33467,#33468,#33469,#33470,#33471,#33472),
(#33473,#33474,#33475,#33476,#33477,#33478,#33479,#33480,#33481,#33482,
#33483,#33484,#33485,#33486),(#33487,#33488,#33489,#33490,#33491,#33492,
#33493,#33494,#33495,#33496,#33497,#33498,#33499,#33500),(#33501,#33502,
#33503,#33504,#33505,#33506,#33507,#33508,#33509,#33510,#33511,#33512,#33513,
#33514),(#33515,#33516,#33517,#33518,#33519,#33520,#33521,#33522,#33523,
#33524,#33525,#33526,#33527,#33528),(#33529,#33530,#33531,#33532,#33533,
#33534,#33535,#33536,#33537,#33538,#33539,#33540,#33541,#33542),(#33543,
#33544,#33545,#33546,#33547,#33548,#33549,#33550,#33551,#33552,#33553,#33554,
#33555,#33556),(#33557,#33558,#33559,#33560,#33561,#33562,#33563,#33564,
#33565,#33566,#33567,#33568,#33569,#33570),(#33571,#33572,#33573,#33574,
#33575,#33576,#33577,#33578,#33579,#33580,#33581,#33582,#33583,#33584),
(#33585,#33586,#33587,#33588,#33589,#33590,#33591,#33592,#33593,#33594,
#33595,#33596,#33597,#33598),(#33599,#33600,#33601,#33602,#33603,#33604,
#33605,#33606,#33607,#33608,#33609,#33610,#33611,#33612),(#33613,#33614,
#33615,#33616,#33617,#33618,#33619,#33620,#33621,#33622,#33623,#33624,#33625,
#33626),(#33627,#33628,#33629,#33630,#33631,#33632,#33633,#33634,#33635,
#33636,#33637,#33638,#33639,#33640),(#33641,#33642,#33643,#33644,#33645,
#33646,#33647,#33648,#33649,#33650,#33651,#33652,#33653,#33654),(#33655,
#33656,#33657,#33658,#33659,#33660,#33661,#33662,#33663,#33664,#33665,#33666,
#33667,#33668),(#33669,#33670,#33671,#33672,#33673,#33674,#33675,#33676,
#33677,#33678,#33679,#33680,#33681,#33682),(#33683,#33684,#33685,#33686,
#33687,#33688,#33689,#33690,#33691,#33692,#33693,#33694,#33695,#33696),
(#33697,#33698,#33699,#33700,#33701,#33702,#33703,#33704,#33705,#33706,
#33707,#33708,#33709,#33710),(#33711,#33712,#33713,#33714,#33715,#33716,
#33717,#33718,#33719,#33720,#33721,#33722,#33723,#33724),(#33725,#33726,
#33727,#33728,#33729,#33730,#33731,#33732,#33733,#33734,#33735,#33736,#33737,
#33738),(#33739,#33740,#33741,#33742,#33743,#33744,#33745,#33746,#33747,
#33748,#33749,#33750,#33751,#33752),(#33753,#33754,#33755,#33756,#33757,
#33758,#33759,#33760,#33761,#33762,#33763,#33764,#33765,#33766),(#33767,
#33768,#33769,#33770,#33771,#33772,#33773,#33774,#33775,#33776,#33777,#33778,
#33779,#33780),(#33781,#33782,#33783,#33784,#33785,#33786,#33787,#33788,
#33789,#33790,#33791,#33792,#33793,#33794),(#33795,#33796,#33797,#33798,
#33799,#33800,#33801,#33802,#33803,#33804,#33805,#33806,#33807,#33808),
(#33809,#33810,#33811,#33812,#33813,#33814,#33815,#33816,#33817,#33818,
#33819,#33820,#33821,#33822),(#33823,#33824,#33825,#33826,#33827,#33828,
#33829,#33830,#33831,#33832,#33833,#33834,#33835,#33836),(#33837,#33838,
#33839,#33840,#33841,#33842,#33843,#33844,#33845,#33846,#33847,#33848,#33849,
#33850),(#33851,#33852,#33853,#33854,#33855,#33856,#33857,#33858,#33859,
#33860,#33861,#33862,#33863,#33864)),.UNSPECIFIED.,.F.,.F.,.F.,(4,1,1,1,
1,1,1,1,1,1,1,1,1,1,1,1,1,1,1,1,1,1,1,1,1,1,1,1,1,1,1,1,1,1,1,1,1,4),(4,
2,2,2,2,2,4),(0.0331549352864051,0.102215297051662,0.171275658816919,0.171545425855064,
0.17181519289321,0.172354726969501,0.173433795122083,0.174512863274665,
0.175591931427247,0.179908204037576,0.184224476647904,0.186382612953069,
0.188540749258233,0.19717329447889,0.205805839699547,0.214438384920204,
0.223070930140861,0.22738720275119,0.231703475361518,0.240336020582175,
0.309396382347432,0.343926563230061,0.378456744112689,0.447517105877946,
0.482047286760574,0.499312377201888,0.507944922422545,0.512261195032874,
0.516577467643203,0.585637829408459,0.723758552938973,0.79281891470423,
0.827349095586858,0.861879276469486,0.896409457352115,0.930939638234743,
0.948204728676057,1.),(0.0377143719413517,0.167070624995476,0.336553194126115,
0.499999999999991,0.663446805873868,0.832929375004528,0.96228562805941),
 .UNSPECIFIED.);
#174=B_SPLINE_SURFACE_WITH_KNOTS('',3,3,((#33923,#33924,#33925,#33926,#33927,
#33928,#33929,#33930,#33931,#33932,#33933,#33934,#33935,#33936),(#33937,
#33938,#33939,#33940,#33941,#33942,#33943,#33944,#33945,#33946,#33947,#33948,
#33949,#33950),(#33951,#33952,#33953,#33954,#33955,#33956,#33957,#33958,
#33959,#33960,#33961,#33962,#33963,#33964),(#33965,#33966,#33967,#33968,
#33969,#33970,#33971,#33972,#33973,#33974,#33975,#33976,#33977,#33978)),
 .UNSPECIFIED.,.F.,.F.,.F.,(4,4),(4,2,2,2,2,2,4),(0.,1.),(0.0377143719414209,
0.167070624995476,0.336553194126115,0.499999999999991,0.663446805873868,
0.832929375004528,0.962285628058582),.UNSPECIFIED.);
#175=B_SPLINE_SURFACE_WITH_KNOTS('',3,3,((#33993,#33994,#33995,#33996,#33997,
#33998,#33999,#34000,#34001,#34002,#34003,#34004,#34005,#34006),(#34007,
#34008,#34009,#34010,#34011,#34012,#34013,#34014,#34015,#34016,#34017,#34018,
#34019,#34020),(#34021,#34022,#34023,#34024,#34025,#34026,#34027,#34028,
#34029,#34030,#34031,#34032,#34033,#34034),(#34035,#34036,#34037,#34038,
#34039,#34040,#34041,#34042,#34043,#34044,#34045,#34046,#34047,#34048),
(#34049,#34050,#34051,#34052,#34053,#34054,#34055,#34056,#34057,#34058,
#34059,#34060,#34061,#34062),(#34063,#34064,#34065,#34066,#34067,#34068,
#34069,#34070,#34071,#34072,#34073,#34074,#34075,#34076),(#34077,#34078,
#34079,#34080,#34081,#34082,#34083,#34084,#34085,#34086,#34087,#34088,#34089,
#34090),(#34091,#34092,#34093,#34094,#34095,#34096,#34097,#34098,#34099,
#34100,#34101,#34102,#34103,#34104),(#34105,#34106,#34107,#34108,#34109,
#34110,#34111,#34112,#34113,#34114,#34115,#34116,#34117,#34118),(#34119,
#34120,#34121,#34122,#34123,#34124,#34125,#34126,#34127,#34128,#34129,#34130,
#34131,#34132),(#34133,#34134,#34135,#34136,#34137,#34138,#34139,#34140,
#34141,#34142,#34143,#34144,#34145,#34146),(#34147,#34148,#34149,#34150,
#34151,#34152,#34153,#34154,#34155,#34156,#34157,#34158,#34159,#34160),
(#34161,#34162,#34163,#34164,#34165,#34166,#34167,#34168,#34169,#34170,
#34171,#34172,#34173,#34174),(#34175,#34176,#34177,#34178,#34179,#34180,
#34181,#34182,#34183,#34184,#34185,#34186,#34187,#34188),(#34189,#34190,
#34191,#34192,#34193,#34194,#34195,#34196,#34197,#34198,#34199,#34200,#34201,
#34202),(#34203,#34204,#34205,#34206,#34207,#34208,#34209,#34210,#34211,
#34212,#34213,#34214,#34215,#34216),(#34217,#34218,#34219,#34220,#34221,
#34222,#34223,#34224,#34225,#34226,#34227,#34228,#34229,#34230),(#34231,
#34232,#34233,#34234,#34235,#34236,#34237,#34238,#34239,#34240,#34241,#34242,
#34243,#34244),(#34245,#34246,#34247,#34248,#34249,#34250,#34251,#34252,
#34253,#34254,#34255,#34256,#34257,#34258),(#34259,#34260,#34261,#34262,
#34263,#34264,#34265,#34266,#34267,#34268,#34269,#34270,#34271,#34272),
(#34273,#34274,#34275,#34276,#34277,#34278,#34279,#34280,#34281,#34282,
#34283,#34284,#34285,#34286),(#34287,#34288,#34289,#34290,#34291,#34292,
#34293,#34294,#34295,#34296,#34297,#34298,#34299,#34300),(#34301,#34302,
#34303,#34304,#34305,#34306,#34307,#34308,#34309,#34310,#34311,#34312,#34313,
#34314),(#34315,#34316,#34317,#34318,#34319,#34320,#34321,#34322,#34323,
#34324,#34325,#34326,#34327,#34328),(#34329,#34330,#34331,#34332,#34333,
#34334,#34335,#34336,#34337,#34338,#34339,#34340,#34341,#34342),(#34343,
#34344,#34345,#34346,#34347,#34348,#34349,#34350,#34351,#34352,#34353,#34354,
#34355,#34356),(#34357,#34358,#34359,#34360,#34361,#34362,#34363,#34364,
#34365,#34366,#34367,#34368,#34369,#34370),(#34371,#34372,#34373,#34374,
#34375,#34376,#34377,#34378,#34379,#34380,#34381,#34382,#34383,#34384),
(#34385,#34386,#34387,#34388,#34389,#34390,#34391,#34392,#34393,#34394,
#34395,#34396,#34397,#34398),(#34399,#34400,#34401,#34402,#34403,#34404,
#34405,#34406,#34407,#34408,#34409,#34410,#34411,#34412),(#34413,#34414,
#34415,#34416,#34417,#34418,#34419,#34420,#34421,#34422,#34423,#34424,#34425,
#34426),(#34427,#34428,#34429,#34430,#34431,#34432,#34433,#34434,#34435,
#34436,#34437,#34438,#34439,#34440)),.UNSPECIFIED.,.F.,.F.,.F.,(4,1,1,1,
1,1,1,1,1,1,1,1,1,1,1,1,1,1,1,1,1,1,1,1,1,1,1,1,1,4),(4,2,2,2,2,2,4),(0.,
0.0517952713240544,0.0690603617654059,0.103590542648109,0.138120723530812,
0.155385813972163,0.189915994854866,0.276241447061624,0.310771627944327,
0.345301808827029,0.379831989709732,0.397097080151084,0.40572962537176,
0.414362170592435,0.483422532357841,0.552482894123247,0.621543255888653,
0.64744089155068,0.690603617654059,0.725133798536762,0.759663979419465,
0.776929069860816,0.794194160302168,0.811459250743519,0.820091795964195,
0.824408068574533,0.826566204879702,0.828724341184871,0.897784702950277,
0.966845064715683),(0.0377143719413786,0.167070624995476,0.336553194126115,
0.499999999999991,0.663446805873868,0.832929375004528,0.96228562805878),
 .UNSPECIFIED.);
#176=B_SPLINE_SURFACE_WITH_KNOTS('',3,3,((#34496,#34497,#34498,#34499,#34500,
#34501,#34502,#34503,#34504,#34505,#34506,#34507,#34508,#34509),(#34510,
#34511,#34512,#34513,#34514,#34515,#34516,#34517,#34518,#34519,#34520,#34521,
#34522,#34523),(#34524,#34525,#34526,#34527,#34528,#34529,#34530,#34531,
#34532,#34533,#34534,#34535,#34536,#34537),(#34538,#34539,#34540,#34541,
#34542,#34543,#34544,#34545,#34546,#34547,#34548,#34549,#34550,#34551),
(#34552,#34553,#34554,#34555,#34556,#34557,#34558,#34559,#34560,#34561,
#34562,#34563,#34564,#34565),(#34566,#34567,#34568,#34569,#34570,#34571,
#34572,#34573,#34574,#34575,#34576,#34577,#34578,#34579),(#34580,#34581,
#34582,#34583,#34584,#34585,#34586,#34587,#34588,#34589,#34590,#34591,#34592,
#34593),(#34594,#34595,#34596,#34597,#34598,#34599,#34600,#34601,#34602,
#34603,#34604,#34605,#34606,#34607),(#34608,#34609,#34610,#34611,#34612,
#34613,#34614,#34615,#34616,#34617,#34618,#34619,#34620,#34621),(#34622,
#34623,#34624,#34625,#34626,#34627,#34628,#34629,#34630,#34631,#34632,#34633,
#34634,#34635),(#34636,#34637,#34638,#34639,#34640,#34641,#34642,#34643,
#34644,#34645,#34646,#34647,#34648,#34649),(#34650,#34651,#34652,#34653,
#34654,#34655,#34656,#34657,#34658,#34659,#34660,#34661,#34662,#34663),
(#34664,#34665,#34666,#34667,#34668,#34669,#34670,#34671,#34672,#34673,
#34674,#34675,#34676,#34677),(#34678,#34679,#34680,#34681,#34682,#34683,
#34684,#34685,#34686,#34687,#34688,#34689,#34690,#34691),(#34692,#34693,
#34694,#34695,#34696,#34697,#34698,#34699,#34700,#34701,#34702,#34703,#34704,
#34705),(#34706,#34707,#34708,#34709,#34710,#34711,#34712,#34713,#34714,
#34715,#34716,#34717,#34718,#34719),(#34720,#34721,#34722,#34723,#34724,
#34725,#34726,#34727,#34728,#34729,#34730,#34731,#34732,#34733),(#34734,
#34735,#34736,#34737,#34738,#34739,#34740,#34741,#34742,#34743,#34744,#34745,
#34746,#34747),(#34748,#34749,#34750,#34751,#34752,#34753,#34754,#34755,
#34756,#34757,#34758,#34759,#34760,#34761),(#34762,#34763,#34764,#34765,
#34766,#34767,#34768,#34769,#34770,#34771,#34772,#34773,#34774,#34775),
(#34776,#34777,#34778,#34779,#34780,#34781,#34782,#34783,#34784,#34785,
#34786,#34787,#34788,#34789),(#34790,#34791,#34792,#34793,#34794,#34795,
#34796,#34797,#34798,#34799,#34800,#34801,#34802,#34803),(#34804,#34805,
#34806,#34807,#34808,#34809,#34810,#34811,#34812,#34813,#34814,#34815,#34816,
#34817),(#34818,#34819,#34820,#34821,#34822,#34823,#34824,#34825,#34826,
#34827,#34828,#34829,#34830,#34831),(#34832,#34833,#34834,#34835,#34836,
#34837,#34838,#34839,#34840,#34841,#34842,#34843,#34844,#34845),(#34846,
#34847,#34848,#34849,#34850,#34851,#34852,#34853,#34854,#34855,#34856,#34857,
#34858,#34859),(#34860,#34861,#34862,#34863,#34864,#34865,#34866,#34867,
#34868,#34869,#34870,#34871,#34872,#34873),(#34874,#34875,#34876,#34877,
#34878,#34879,#34880,#34881,#34882,#34883,#34884,#34885,#34886,#34887),
(#34888,#34889,#34890,#34891,#34892,#34893,#34894,#34895,#34896,#34897,
#34898,#34899,#34900,#34901),(#34902,#34903,#34904,#34905,#34906,#34907,
#34908,#34909,#34910,#34911,#34912,#34913,#34914,#34915),(#34916,#34917,
#34918,#34919,#34920,#34921,#34922,#34923,#34924,#34925,#34926,#34927,#34928,
#34929),(#34930,#34931,#34932,#34933,#34934,#34935,#34936,#34937,#34938,
#34939,#34940,#34941,#34942,#34943),(#34944,#34945,#34946,#34947,#34948,
#34949,#34950,#34951,#34952,#34953,#34954,#34955,#34956,#34957),(#34958,
#34959,#34960,#34961,#34962,#34963,#34964,#34965,#34966,#34967,#34968,#34969,
#34970,#34971),(#34972,#34973,#34974,#34975,#34976,#34977,#34978,#34979,
#34980,#34981,#34982,#34983,#34984,#34985),(#34986,#34987,#34988,#34989,
#34990,#34991,#34992,#34993,#34994,#34995,#34996,#34997,#34998,#34999),
(#35000,#35001,#35002,#35003,#35004,#35005,#35006,#35007,#35008,#35009,
#35010,#35011,#35012,#35013),(#35014,#35015,#35016,#35017,#35018,#35019,
#35020,#35021,#35022,#35023,#35024,#35025,#35026,#35027),(#35028,#35029,
#35030,#35031,#35032,#35033,#35034,#35035,#35036,#35037,#35038,#35039,#35040,
#35041),(#35042,#35043,#35044,#35045,#35046,#35047,#35048,#35049,#35050,
#35051,#35052,#35053,#35054,#35055),(#35056,#35057,#35058,#35059,#35060,
#35061,#35062,#35063,#35064,#35065,#35066,#35067,#35068,#35069),(#35070,
#35071,#35072,#35073,#35074,#35075,#35076,#35077,#35078,#35079,#35080,#35081,
#35082,#35083),(#35084,#35085,#35086,#35087,#35088,#35089,#35090,#35091,
#35092,#35093,#35094,#35095,#35096,#35097),(#35098,#35099,#35100,#35101,
#35102,#35103,#35104,#35105,#35106,#35107,#35108,#35109,#35110,#35111),
(#35112,#35113,#35114,#35115,#35116,#35117,#35118,#35119,#35120,#35121,
#35122,#35123,#35124,#35125),(#35126,#35127,#35128,#35129,#35130,#35131,
#35132,#35133,#35134,#35135,#35136,#35137,#35138,#35139),(#35140,#35141,
#35142,#35143,#35144,#35145,#35146,#35147,#35148,#35149,#35150,#35151,#35152,
#35153)),.UNSPECIFIED.,.F.,.F.,.F.,(4,1,1,1,1,1,1,1,1,1,1,1,1,1,1,1,1,1,
1,1,1,1,1,1,1,1,1,1,1,1,1,1,1,1,1,1,1,1,1,1,1,1,1,1,4),(4,2,2,2,2,2,4),
(0.0331549352864063,0.0676851161690347,0.102215297051663,0.136745477934291,
0.17127565881692,0.171545425855065,0.171815192893211,0.172084959931356,
0.172354726969502,0.173433795122084,0.175591931427248,0.177750067732413,
0.179908204037577,0.184224476647905,0.188540749258234,0.205805839699548,
0.223070930140862,0.227387202751191,0.231703475361519,0.240336020582176,
0.274866201464805,0.292131291906119,0.309396382347433,0.343926563230061,
0.37845674411269,0.412986924995318,0.430252015436632,0.447517105877946,
0.516577467643203,0.551107648525831,0.58563782940846,0.620168010291088,
0.654698191173717,0.671963281615031,0.723758552938973,0.79281891470423,
0.827349095586858,0.844614186028172,0.853246731248829,0.861879276469487,
0.896409457352115,0.930939638234743,0.948204728676057,0.965469819117372,
1.),(0.0377143719413899,0.167070624995476,0.336553194126115,0.499999999999991,
0.663446805873868,0.832929375004528,0.96228562805941),.UNSPECIFIED.);
#177=B_SPLINE_SURFACE_WITH_KNOTS('',3,3,((#35212,#35213,#35214,#35215,#35216,
#35217,#35218,#35219,#35220,#35221,#35222,#35223,#35224,#35225),(#35226,
#35227,#35228,#35229,#35230,#35231,#35232,#35233,#35234,#35235,#35236,#35237,
#35238,#35239),(#35240,#35241,#35242,#35243,#35244,#35245,#35246,#35247,
#35248,#35249,#35250,#35251,#35252,#35253),(#35254,#35255,#35256,#35257,
#35258,#35259,#35260,#35261,#35262,#35263,#35264,#35265,#35266,#35267)),
 .UNSPECIFIED.,.F.,.F.,.F.,(4,4),(4,2,2,2,2,2,4),(0.,1.),(0.0377143719414212,
0.167070624995476,0.336553194126115,0.499999999999991,0.663446805873868,
0.832929375004528,0.962285628058582),.UNSPECIFIED.);
#178=B_SPLINE_SURFACE_WITH_KNOTS('',3,3,((#35282,#35283,#35284,#35285,#35286,
#35287,#35288,#35289,#35290,#35291,#35292,#35293,#35294,#35295),(#35296,
#35297,#35298,#35299,#35300,#35301,#35302,#35303,#35304,#35305,#35306,#35307,
#35308,#35309),(#35310,#35311,#35312,#35313,#35314,#35315,#35316,#35317,
#35318,#35319,#35320,#35321,#35322,#35323),(#35324,#35325,#35326,#35327,
#35328,#35329,#35330,#35331,#35332,#35333,#35334,#35335,#35336,#35337),
(#35338,#35339,#35340,#35341,#35342,#35343,#35344,#35345,#35346,#35347,
#35348,#35349,#35350,#35351),(#35352,#35353,#35354,#35355,#35356,#35357,
#35358,#35359,#35360,#35361,#35362,#35363,#35364,#35365),(#35366,#35367,
#35368,#35369,#35370,#35371,#35372,#35373,#35374,#35375,#35376,#35377,#35378,
#35379),(#35380,#35381,#35382,#35383,#35384,#35385,#35386,#35387,#35388,
#35389,#35390,#35391,#35392,#35393),(#35394,#35395,#35396,#35397,#35398,
#35399,#35400,#35401,#35402,#35403,#35404,#35405,#35406,#35407),(#35408,
#35409,#35410,#35411,#35412,#35413,#35414,#35415,#35416,#35417,#35418,#35419,
#35420,#35421),(#35422,#35423,#35424,#35425,#35426,#35427,#35428,#35429,
#35430,#35431,#35432,#35433,#35434,#35435),(#35436,#35437,#35438,#35439,
#35440,#35441,#35442,#35443,#35444,#35445,#35446,#35447,#35448,#35449),
(#35450,#35451,#35452,#35453,#35454,#35455,#35456,#35457,#35458,#35459,
#35460,#35461,#35462,#35463),(#35464,#35465,#35466,#35467,#35468,#35469,
#35470,#35471,#35472,#35473,#35474,#35475,#35476,#35477),(#35478,#35479,
#35480,#35481,#35482,#35483,#35484,#35485,#35486,#35487,#35488,#35489,#35490,
#35491),(#35492,#35493,#35494,#35495,#35496,#35497,#35498,#35499,#35500,
#35501,#35502,#35503,#35504,#35505),(#35506,#35507,#35508,#35509,#35510,
#35511,#35512,#35513,#35514,#35515,#35516,#35517,#35518,#35519),(#35520,
#35521,#35522,#35523,#35524,#35525,#35526,#35527,#35528,#35529,#35530,#35531,
#35532,#35533),(#35534,#35535,#35536,#35537,#35538,#35539,#35540,#35541,
#35542,#35543,#35544,#35545,#35546,#35547),(#35548,#35549,#35550,#35551,
#35552,#35553,#35554,#35555,#35556,#35557,#35558,#35559,#35560,#35561),
(#35562,#35563,#35564,#35565,#35566,#35567,#35568,#35569,#35570,#35571,
#35572,#35573,#35574,#35575),(#35576,#35577,#35578,#35579,#35580,#35581,
#35582,#35583,#35584,#35585,#35586,#35587,#35588,#35589),(#35590,#35591,
#35592,#35593,#35594,#35595,#35596,#35597,#35598,#35599,#35600,#35601,#35602,
#35603),(#35604,#35605,#35606,#35607,#35608,#35609,#35610,#35611,#35612,
#35613,#35614,#35615,#35616,#35617),(#35618,#35619,#35620,#35621,#35622,
#35623,#35624,#35625,#35626,#35627,#35628,#35629,#35630,#35631),(#35632,
#35633,#35634,#35635,#35636,#35637,#35638,#35639,#35640,#35641,#35642,#35643,
#35644,#35645),(#35646,#35647,#35648,#35649,#35650,#35651,#35652,#35653,
#35654,#35655,#35656,#35657,#35658,#35659),(#35660,#35661,#35662,#35663,
#35664,#35665,#35666,#35667,#35668,#35669,#35670,#35671,#35672,#35673),
(#35674,#35675,#35676,#35677,#35678,#35679,#35680,#35681,#35682,#35683,
#35684,#35685,#35686,#35687),(#35688,#35689,#35690,#35691,#35692,#35693,
#35694,#35695,#35696,#35697,#35698,#35699,#35700,#35701),(#35702,#35703,
#35704,#35705,#35706,#35707,#35708,#35709,#35710,#35711,#35712,#35713,#35714,
#35715),(#35716,#35717,#35718,#35719,#35720,#35721,#35722,#35723,#35724,
#35725,#35726,#35727,#35728,#35729)),.UNSPECIFIED.,.F.,.F.,.F.,(4,1,1,1,
1,1,1,1,1,1,1,1,1,1,1,1,1,1,1,1,1,1,1,1,1,1,1,1,1,4),(4,2,2,2,2,2,4),(0.,
0.0517952713240546,0.0690603617654061,0.103590542648109,0.138120723530812,
0.155385813972164,0.189915994854867,0.276241447061625,0.310771627944328,
0.345301808827031,0.379831989709734,0.397097080151085,0.405729625371761,
0.414362170592437,0.483422532357843,0.552482894123249,0.621543255888655,
0.647440891550682,0.690603617654061,0.725133798536764,0.759663979419467,
0.776929069860819,0.79419416030217,0.811459250743522,0.820091795964198,
0.824408068574536,0.826566204879705,0.828724341184873,0.89778470295028,
0.966845064715686),(0.0377143719408444,0.167070624995476,0.336553194126115,
0.499999999999991,0.663446805873868,0.832929375004528,0.962285628060942),
 .UNSPECIFIED.);
#179=B_SPLINE_SURFACE_WITH_KNOTS('',3,3,((#35785,#35786,#35787,#35788,#35789,
#35790,#35791,#35792,#35793,#35794,#35795,#35796,#35797,#35798),(#35799,
#35800,#35801,#35802,#35803,#35804,#35805,#35806,#35807,#35808,#35809,#35810,
#35811,#35812),(#35813,#35814,#35815,#35816,#35817,#35818,#35819,#35820,
#35821,#35822,#35823,#35824,#35825,#35826),(#35827,#35828,#35829,#35830,
#35831,#35832,#35833,#35834,#35835,#35836,#35837,#35838,#35839,#35840),
(#35841,#35842,#35843,#35844,#35845,#35846,#35847,#35848,#35849,#35850,
#35851,#35852,#35853,#35854),(#35855,#35856,#35857,#35858,#35859,#35860,
#35861,#35862,#35863,#35864,#35865,#35866,#35867,#35868),(#35869,#35870,
#35871,#35872,#35873,#35874,#35875,#35876,#35877,#35878,#35879,#35880,#35881,
#35882),(#35883,#35884,#35885,#35886,#35887,#35888,#35889,#35890,#35891,
#35892,#35893,#35894,#35895,#35896),(#35897,#35898,#35899,#35900,#35901,
#35902,#35903,#35904,#35905,#35906,#35907,#35908,#35909,#35910),(#35911,
#35912,#35913,#35914,#35915,#35916,#35917,#35918,#35919,#35920,#35921,#35922,
#35923,#35924),(#35925,#35926,#35927,#35928,#35929,#35930,#35931,#35932,
#35933,#35934,#35935,#35936,#35937,#35938),(#35939,#35940,#35941,#35942,
#35943,#35944,#35945,#35946,#35947,#35948,#35949,#35950,#35951,#35952),
(#35953,#35954,#35955,#35956,#35957,#35958,#35959,#35960,#35961,#35962,
#35963,#35964,#35965,#35966),(#35967,#35968,#35969,#35970,#35971,#35972,
#35973,#35974,#35975,#35976,#35977,#35978,#35979,#35980),(#35981,#35982,
#35983,#35984,#35985,#35986,#35987,#35988,#35989,#35990,#35991,#35992,#35993,
#35994),(#35995,#35996,#35997,#35998,#35999,#36000,#36001,#36002,#36003,
#36004,#36005,#36006,#36007,#36008),(#36009,#36010,#36011,#36012,#36013,
#36014,#36015,#36016,#36017,#36018,#36019,#36020,#36021,#36022),(#36023,
#36024,#36025,#36026,#36027,#36028,#36029,#36030,#36031,#36032,#36033,#36034,
#36035,#36036),(#36037,#36038,#36039,#36040,#36041,#36042,#36043,#36044,
#36045,#36046,#36047,#36048,#36049,#36050),(#36051,#36052,#36053,#36054,
#36055,#36056,#36057,#36058,#36059,#36060,#36061,#36062,#36063,#36064),
(#36065,#36066,#36067,#36068,#36069,#36070,#36071,#36072,#36073,#36074,
#36075,#36076,#36077,#36078),(#36079,#36080,#36081,#36082,#36083,#36084,
#36085,#36086,#36087,#36088,#36089,#36090,#36091,#36092),(#36093,#36094,
#36095,#36096,#36097,#36098,#36099,#36100,#36101,#36102,#36103,#36104,#36105,
#36106),(#36107,#36108,#36109,#36110,#36111,#36112,#36113,#36114,#36115,
#36116,#36117,#36118,#36119,#36120),(#36121,#36122,#36123,#36124,#36125,
#36126,#36127,#36128,#36129,#36130,#36131,#36132,#36133,#36134),(#36135,
#36136,#36137,#36138,#36139,#36140,#36141,#36142,#36143,#36144,#36145,#36146,
#36147,#36148),(#36149,#36150,#36151,#36152,#36153,#36154,#36155,#36156,
#36157,#36158,#36159,#36160,#36161,#36162),(#36163,#36164,#36165,#36166,
#36167,#36168,#36169,#36170,#36171,#36172,#36173,#36174,#36175,#36176),
(#36177,#36178,#36179,#36180,#36181,#36182,#36183,#36184,#36185,#36186,
#36187,#36188,#36189,#36190),(#36191,#36192,#36193,#36194,#36195,#36196,
#36197,#36198,#36199,#36200,#36201,#36202,#36203,#36204),(#36205,#36206,
#36207,#36208,#36209,#36210,#36211,#36212,#36213,#36214,#36215,#36216,#36217,
#36218),(#36219,#36220,#36221,#36222,#36223,#36224,#36225,#36226,#36227,
#36228,#36229,#36230,#36231,#36232),(#36233,#36234,#36235,#36236,#36237,
#36238,#36239,#36240,#36241,#36242,#36243,#36244,#36245,#36246),(#36247,
#36248,#36249,#36250,#36251,#36252,#36253,#36254,#36255,#36256,#36257,#36258,
#36259,#36260)),.UNSPECIFIED.,.F.,.F.,.F.,(4,1,1,1,1,1,1,1,1,1,1,1,1,1,
1,1,1,1,1,1,1,1,1,1,1,1,1,1,1,1,1,4),(4,2,2,2,2,2,4),(0.0331549352864075,
0.102215297051664,0.171275658816921,0.172354726969503,0.173433795122085,
0.174512863274667,0.175591931427249,0.179908204037578,0.188540749258235,
0.201489567089221,0.205805839699549,0.223070930140863,0.240336020582177,
0.274866201464806,0.309396382347434,0.378456744112691,0.412986924995319,
0.447517105877947,0.482047286760576,0.516577467643204,0.551107648525832,
0.568372738967146,0.58563782940846,0.654698191173717,0.723758552938974,
0.79281891470423,0.827349095586859,0.861879276469487,0.896409457352115,
0.930939638234743,0.948204728676058,1.),(0.0377143719407316,0.167070624995476,
0.336553194126115,0.499999999999991,0.663446805873868,0.832929375004528,
0.962285628058715),.UNSPECIFIED.);
#180=B_SPLINE_SURFACE_WITH_KNOTS('',3,3,((#36323,#36324,#36325,#36326,#36327,
#36328,#36329,#36330,#36331,#36332,#36333,#36334,#36335,#36336),(#36337,
#36338,#36339,#36340,#36341,#36342,#36343,#36344,#36345,#36346,#36347,#36348,
#36349,#36350),(#36351,#36352,#36353,#36354,#36355,#36356,#36357,#36358,
#36359,#36360,#36361,#36362,#36363,#36364),(#36365,#36366,#36367,#36368,
#36369,#36370,#36371,#36372,#36373,#36374,#36375,#36376,#36377,#36378)),
 .UNSPECIFIED.,.F.,.F.,.F.,(4,4),(4,2,2,2,2,2,4),(0.,1.),(0.0377143719414212,
0.167070624995476,0.336553194126115,0.499999999999991,0.663446805873868,
0.832929375004528,0.962285628058582),.UNSPECIFIED.);
#181=B_SPLINE_SURFACE_WITH_KNOTS('',3,3,((#36393,#36394,#36395,#36396,#36397,
#36398,#36399,#36400,#36401,#36402,#36403,#36404,#36405,#36406),(#36407,
#36408,#36409,#36410,#36411,#36412,#36413,#36414,#36415,#36416,#36417,#36418,
#36419,#36420),(#36421,#36422,#36423,#36424,#36425,#36426,#36427,#36428,
#36429,#36430,#36431,#36432,#36433,#36434),(#36435,#36436,#36437,#36438,
#36439,#36440,#36441,#36442,#36443,#36444,#36445,#36446,#36447,#36448),
(#36449,#36450,#36451,#36452,#36453,#36454,#36455,#36456,#36457,#36458,
#36459,#36460,#36461,#36462),(#36463,#36464,#36465,#36466,#36467,#36468,
#36469,#36470,#36471,#36472,#36473,#36474,#36475,#36476),(#36477,#36478,
#36479,#36480,#36481,#36482,#36483,#36484,#36485,#36486,#36487,#36488,#36489,
#36490),(#36491,#36492,#36493,#36494,#36495,#36496,#36497,#36498,#36499,
#36500,#36501,#36502,#36503,#36504),(#36505,#36506,#36507,#36508,#36509,
#36510,#36511,#36512,#36513,#36514,#36515,#36516,#36517,#36518),(#36519,
#36520,#36521,#36522,#36523,#36524,#36525,#36526,#36527,#36528,#36529,#36530,
#36531,#36532),(#36533,#36534,#36535,#36536,#36537,#36538,#36539,#36540,
#36541,#36542,#36543,#36544,#36545,#36546),(#36547,#36548,#36549,#36550,
#36551,#36552,#36553,#36554,#36555,#36556,#36557,#36558,#36559,#36560),
(#36561,#36562,#36563,#36564,#36565,#36566,#36567,#36568,#36569,#36570,
#36571,#36572,#36573,#36574),(#36575,#36576,#36577,#36578,#36579,#36580,
#36581,#36582,#36583,#36584,#36585,#36586,#36587,#36588),(#36589,#36590,
#36591,#36592,#36593,#36594,#36595,#36596,#36597,#36598,#36599,#36600,#36601,
#36602),(#36603,#36604,#36605,#36606,#36607,#36608,#36609,#36610,#36611,
#36612,#36613,#36614,#36615,#36616),(#36617,#36618,#36619,#36620,#36621,
#36622,#36623,#36624,#36625,#36626,#36627,#36628,#36629,#36630),(#36631,
#36632,#36633,#36634,#36635,#36636,#36637,#36638,#36639,#36640,#36641,#36642,
#36643,#36644),(#36645,#36646,#36647,#36648,#36649,#36650,#36651,#36652,
#36653,#36654,#36655,#36656,#36657,#36658),(#36659,#36660,#36661,#36662,
#36663,#36664,#36665,#36666,#36667,#36668,#36669,#36670,#36671,#36672),
(#36673,#36674,#36675,#36676,#36677,#36678,#36679,#36680,#36681,#36682,
#36683,#36684,#36685,#36686),(#36687,#36688,#36689,#36690,#36691,#36692,
#36693,#36694,#36695,#36696,#36697,#36698,#36699,#36700),(#36701,#36702,
#36703,#36704,#36705,#36706,#36707,#36708,#36709,#36710,#36711,#36712,#36713,
#36714),(#36715,#36716,#36717,#36718,#36719,#36720,#36721,#36722,#36723,
#36724,#36725,#36726,#36727,#36728),(#36729,#36730,#36731,#36732,#36733,
#36734,#36735,#36736,#36737,#36738,#36739,#36740,#36741,#36742),(#36743,
#36744,#36745,#36746,#36747,#36748,#36749,#36750,#36751,#36752,#36753,#36754,
#36755,#36756),(#36757,#36758,#36759,#36760,#36761,#36762,#36763,#36764,
#36765,#36766,#36767,#36768,#36769,#36770),(#36771,#36772,#36773,#36774,
#36775,#36776,#36777,#36778,#36779,#36780,#36781,#36782,#36783,#36784),
(#36785,#36786,#36787,#36788,#36789,#36790,#36791,#36792,#36793,#36794,
#36795,#36796,#36797,#36798),(#36799,#36800,#36801,#36802,#36803,#36804,
#36805,#36806,#36807,#36808,#36809,#36810,#36811,#36812),(#36813,#36814,
#36815,#36816,#36817,#36818,#36819,#36820,#36821,#36822,#36823,#36824,#36825,
#36826),(#36827,#36828,#36829,#36830,#36831,#36832,#36833,#36834,#36835,
#36836,#36837,#36838,#36839,#36840),(#36841,#36842,#36843,#36844,#36845,
#36846,#36847,#36848,#36849,#36850,#36851,#36852,#36853,#36854),(#36855,
#36856,#36857,#36858,#36859,#36860,#36861,#36862,#36863,#36864,#36865,#36866,
#36867,#36868),(#36869,#36870,#36871,#36872,#36873,#36874,#36875,#36876,
#36877,#36878,#36879,#36880,#36881,#36882),(#36883,#36884,#36885,#36886,
#36887,#36888,#36889,#36890,#36891,#36892,#36893,#36894,#36895,#36896),
(#36897,#36898,#36899,#36900,#36901,#36902,#36903,#36904,#36905,#36906,
#36907,#36908,#36909,#36910),(#36911,#36912,#36913,#36914,#36915,#36916,
#36917,#36918,#36919,#36920,#36921,#36922,#36923,#36924),(#36925,#36926,
#36927,#36928,#36929,#36930,#36931,#36932,#36933,#36934,#36935,#36936,#36937,
#36938),(#36939,#36940,#36941,#36942,#36943,#36944,#36945,#36946,#36947,
#36948,#36949,#36950,#36951,#36952),(#36953,#36954,#36955,#36956,#36957,
#36958,#36959,#36960,#36961,#36962,#36963,#36964,#36965,#36966),(#36967,
#36968,#36969,#36970,#36971,#36972,#36973,#36974,#36975,#36976,#36977,#36978,
#36979,#36980),(#36981,#36982,#36983,#36984,#36985,#36986,#36987,#36988,
#36989,#36990,#36991,#36992,#36993,#36994),(#36995,#36996,#36997,#36998,
#36999,#37000,#37001,#37002,#37003,#37004,#37005,#37006,#37007,#37008)),
 .UNSPECIFIED.,.F.,.F.,.F.,(4,1,1,1,1,1,1,1,1,1,1,1,1,1,1,1,1,1,1,1,1,1,
1,1,1,1,1,1,1,1,1,1,1,1,1,1,1,1,1,1,1,4),(4,2,2,2,2,2,4),(0.,0.0345301808827031,
0.0517952713240546,0.0690603617654061,0.103590542648109,0.138120723530812,
0.155385813972164,0.172650904413515,0.207181085296218,0.276241447061624,
0.345301808827031,0.379831989709734,0.414362170592437,0.44889235147514,
0.483422532357843,0.552482894123249,0.5697479845646,0.587013075005952,0.621543255888655,
0.656073436771358,0.690603617654061,0.725133798536764,0.759663979419467,
0.763980252029805,0.768296524640143,0.770454660945312,0.776929069860819,
0.79419416030217,0.811459250743522,0.813617387048691,0.815775523353859,
0.820091795964197,0.824408068574535,0.82548713672712,0.826566204879704,
0.827645273032289,0.828184807108581,0.828454574146727,0.828724341184873,
0.897784702950279,0.932314883832982,0.966845064715685),(0.0377143719397814,
0.167070624995476,0.336553194126115,0.499999999999991,0.663446805873868,
0.832929375004528,0.962285628059059),.UNSPECIFIED.);
#182=B_SPLINE_SURFACE_WITH_KNOTS('',3,3,((#37068,#37069,#37070,#37071,#37072,
#37073,#37074,#37075,#37076,#37077,#37078,#37079,#37080,#37081),(#37082,
#37083,#37084,#37085,#37086,#37087,#37088,#37089,#37090,#37091,#37092,#37093,
#37094,#37095),(#37096,#37097,#37098,#37099,#37100,#37101,#37102,#37103,
#37104,#37105,#37106,#37107,#37108,#37109),(#37110,#37111,#37112,#37113,
#37114,#37115,#37116,#37117,#37118,#37119,#37120,#37121,#37122,#37123),
(#37124,#37125,#37126,#37127,#37128,#37129,#37130,#37131,#37132,#37133,
#37134,#37135,#37136,#37137),(#37138,#37139,#37140,#37141,#37142,#37143,
#37144,#37145,#37146,#37147,#37148,#37149,#37150,#37151),(#37152,#37153,
#37154,#37155,#37156,#37157,#37158,#37159,#37160,#37161,#37162,#37163,#37164,
#37165),(#37166,#37167,#37168,#37169,#37170,#37171,#37172,#37173,#37174,
#37175,#37176,#37177,#37178,#37179),(#37180,#37181,#37182,#37183,#37184,
#37185,#37186,#37187,#37188,#37189,#37190,#37191,#37192,#37193),(#37194,
#37195,#37196,#37197,#37198,#37199,#37200,#37201,#37202,#37203,#37204,#37205,
#37206,#37207),(#37208,#37209,#37210,#37211,#37212,#37213,#37214,#37215,
#37216,#37217,#37218,#37219,#37220,#37221),(#37222,#37223,#37224,#37225,
#37226,#37227,#37228,#37229,#37230,#37231,#37232,#37233,#37234,#37235),
(#37236,#37237,#37238,#37239,#37240,#37241,#37242,#37243,#37244,#37245,
#37246,#37247,#37248,#37249),(#37250,#37251,#37252,#37253,#37254,#37255,
#37256,#37257,#37258,#37259,#37260,#37261,#37262,#37263),(#37264,#37265,
#37266,#37267,#37268,#37269,#37270,#37271,#37272,#37273,#37274,#37275,#37276,
#37277),(#37278,#37279,#37280,#37281,#37282,#37283,#37284,#37285,#37286,
#37287,#37288,#37289,#37290,#37291),(#37292,#37293,#37294,#37295,#37296,
#37297,#37298,#37299,#37300,#37301,#37302,#37303,#37304,#37305),(#37306,
#37307,#37308,#37309,#37310,#37311,#37312,#37313,#37314,#37315,#37316,#37317,
#37318,#37319),(#37320,#37321,#37322,#37323,#37324,#37325,#37326,#37327,
#37328,#37329,#37330,#37331,#37332,#37333),(#37334,#37335,#37336,#37337,
#37338,#37339,#37340,#37341,#37342,#37343,#37344,#37345,#37346,#37347),
(#37348,#37349,#37350,#37351,#37352,#37353,#37354,#37355,#37356,#37357,
#37358,#37359,#37360,#37361),(#37362,#37363,#37364,#37365,#37366,#37367,
#37368,#37369,#37370,#37371,#37372,#37373,#37374,#37375),(#37376,#37377,
#37378,#37379,#37380,#37381,#37382,#37383,#37384,#37385,#37386,#37387,#37388,
#37389),(#37390,#37391,#37392,#37393,#37394,#37395,#37396,#37397,#37398,
#37399,#37400,#37401,#37402,#37403),(#37404,#37405,#37406,#37407,#37408,
#37409,#37410,#37411,#37412,#37413,#37414,#37415,#37416,#37417),(#37418,
#37419,#37420,#37421,#37422,#37423,#37424,#37425,#37426,#37427,#37428,#37429,
#37430,#37431),(#37432,#37433,#37434,#37435,#37436,#37437,#37438,#37439,
#37440,#37441,#37442,#37443,#37444,#37445),(#37446,#37447,#37448,#37449,
#37450,#37451,#37452,#37453,#37454,#37455,#37456,#37457,#37458,#37459),
(#37460,#37461,#37462,#37463,#37464,#37465,#37466,#37467,#37468,#37469,
#37470,#37471,#37472,#37473),(#37474,#37475,#37476,#37477,#37478,#37479,
#37480,#37481,#37482,#37483,#37484,#37485,#37486,#37487),(#37488,#37489,
#37490,#37491,#37492,#37493,#37494,#37495,#37496,#37497,#37498,#37499,#37500,
#37501),(#37502,#37503,#37504,#37505,#37506,#37507,#37508,#37509,#37510,
#37511,#37512,#37513,#37514,#37515),(#37516,#37517,#37518,#37519,#37520,
#37521,#37522,#37523,#37524,#37525,#37526,#37527,#37528,#37529)),
 .UNSPECIFIED.,.F.,.F.,.F.,(4,1,1,1,1,1,1,1,1,1,1,1,1,1,1,1,1,1,1,1,1,1,
1,1,1,1,1,1,1,1,4),(4,2,2,2,2,2,4),(0.0331549352864083,0.102215297051665,
0.171275658816921,0.172354726969503,0.173433795122086,0.174512863274668,
0.17559193142725,0.179908204037578,0.188540749258235,0.20580583969955,0.223070930140864,
0.231703475361521,0.240336020582178,0.309396382347434,0.378456744112691,
0.412986924995319,0.447517105877948,0.482047286760576,0.516577467643204,
0.551107648525832,0.568372738967146,0.585637829408461,0.654698191173717,
0.723758552938974,0.79281891470423,0.827349095586859,0.861879276469487,
0.896409457352115,0.930939638234743,0.948204728676058,1.),(0.0377143719413654,
0.167070624995476,0.336553194126115,0.499999999999991,0.663446805873868,
0.832929375004528,0.962285628058767),.UNSPECIFIED.);
#183=B_SPLINE_SURFACE_WITH_KNOTS('',3,3,((#37588,#37589,#37590,#37591,#37592,
#37593,#37594,#37595,#37596,#37597,#37598,#37599,#37600,#37601),(#37602,
#37603,#37604,#37605,#37606,#37607,#37608,#37609,#37610,#37611,#37612,#37613,
#37614,#37615),(#37616,#37617,#37618,#37619,#37620,#37621,#37622,#37623,
#37624,#37625,#37626,#37627,#37628,#37629),(#37630,#37631,#37632,#37633,
#37634,#37635,#37636,#37637,#37638,#37639,#37640,#37641,#37642,#37643)),
 .UNSPECIFIED.,.F.,.F.,.F.,(4,4),(4,2,2,2,2,2,4),(0.,1.),(0.037714371941421,
0.167070624995476,0.336553194126115,0.499999999999991,0.663446805873868,
0.832929375004528,0.962285628058582),.UNSPECIFIED.);
#184=B_SPLINE_SURFACE_WITH_KNOTS('',3,3,((#37658,#37659,#37660,#37661,#37662,
#37663,#37664,#37665,#37666,#37667,#37668,#37669,#37670,#37671),(#37672,
#37673,#37674,#37675,#37676,#37677,#37678,#37679,#37680,#37681,#37682,#37683,
#37684,#37685),(#37686,#37687,#37688,#37689,#37690,#37691,#37692,#37693,
#37694,#37695,#37696,#37697,#37698,#37699),(#37700,#37701,#37702,#37703,
#37704,#37705,#37706,#37707,#37708,#37709,#37710,#37711,#37712,#37713),
(#37714,#37715,#37716,#37717,#37718,#37719,#37720,#37721,#37722,#37723,
#37724,#37725,#37726,#37727),(#37728,#37729,#37730,#37731,#37732,#37733,
#37734,#37735,#37736,#37737,#37738,#37739,#37740,#37741),(#37742,#37743,
#37744,#37745,#37746,#37747,#37748,#37749,#37750,#37751,#37752,#37753,#37754,
#37755),(#37756,#37757,#37758,#37759,#37760,#37761,#37762,#37763,#37764,
#37765,#37766,#37767,#37768,#37769),(#37770,#37771,#37772,#37773,#37774,
#37775,#37776,#37777,#37778,#37779,#37780,#37781,#37782,#37783),(#37784,
#37785,#37786,#37787,#37788,#37789,#37790,#37791,#37792,#37793,#37794,#37795,
#37796,#37797),(#37798,#37799,#37800,#37801,#37802,#37803,#37804,#37805,
#37806,#37807,#37808,#37809,#37810,#37811),(#37812,#37813,#37814,#37815,
#37816,#37817,#37818,#37819,#37820,#37821,#37822,#37823,#37824,#37825),
(#37826,#37827,#37828,#37829,#37830,#37831,#37832,#37833,#37834,#37835,
#37836,#37837,#37838,#37839),(#37840,#37841,#37842,#37843,#37844,#37845,
#37846,#37847,#37848,#37849,#37850,#37851,#37852,#37853),(#37854,#37855,
#37856,#37857,#37858,#37859,#37860,#37861,#37862,#37863,#37864,#37865,#37866,
#37867),(#37868,#37869,#37870,#37871,#37872,#37873,#37874,#37875,#37876,
#37877,#37878,#37879,#37880,#37881),(#37882,#37883,#37884,#37885,#37886,
#37887,#37888,#37889,#37890,#37891,#37892,#37893,#37894,#37895),(#37896,
#37897,#37898,#37899,#37900,#37901,#37902,#37903,#37904,#37905,#37906,#37907,
#37908,#37909),(#37910,#37911,#37912,#37913,#37914,#37915,#37916,#37917,
#37918,#37919,#37920,#37921,#37922,#37923),(#37924,#37925,#37926,#37927,
#37928,#37929,#37930,#37931,#37932,#37933,#37934,#37935,#37936,#37937),
(#37938,#37939,#37940,#37941,#37942,#37943,#37944,#37945,#37946,#37947,
#37948,#37949,#37950,#37951),(#37952,#37953,#37954,#37955,#37956,#37957,
#37958,#37959,#37960,#37961,#37962,#37963,#37964,#37965),(#37966,#37967,
#37968,#37969,#37970,#37971,#37972,#37973,#37974,#37975,#37976,#37977,#37978,
#37979),(#37980,#37981,#37982,#37983,#37984,#37985,#37986,#37987,#37988,
#37989,#37990,#37991,#37992,#37993),(#37994,#37995,#37996,#37997,#37998,
#37999,#38000,#38001,#38002,#38003,#38004,#38005,#38006,#38007),(#38008,
#38009,#38010,#38011,#38012,#38013,#38014,#38015,#38016,#38017,#38018,#38019,
#38020,#38021),(#38022,#38023,#38024,#38025,#38026,#38027,#38028,#38029,
#38030,#38031,#38032,#38033,#38034,#38035),(#38036,#38037,#38038,#38039,
#38040,#38041,#38042,#38043,#38044,#38045,#38046,#38047,#38048,#38049),
(#38050,#38051,#38052,#38053,#38054,#38055,#38056,#38057,#38058,#38059,
#38060,#38061,#38062,#38063),(#38064,#38065,#38066,#38067,#38068,#38069,
#38070,#38071,#38072,#38073,#38074,#38075,#38076,#38077),(#38078,#38079,
#38080,#38081,#38082,#38083,#38084,#38085,#38086,#38087,#38088,#38089,#38090,
#38091),(#38092,#38093,#38094,#38095,#38096,#38097,#38098,#38099,#38100,
#38101,#38102,#38103,#38104,#38105),(#38106,#38107,#38108,#38109,#38110,
#38111,#38112,#38113,#38114,#38115,#38116,#38117,#38118,#38119)),
 .UNSPECIFIED.,.F.,.F.,.F.,(4,1,1,1,1,1,1,1,1,1,1,1,1,1,1,1,1,1,1,1,1,1,
1,1,1,1,1,1,1,1,4),(4,2,2,2,2,2,4),(0.,0.0517952713240546,0.0690603617654061,
0.103590542648109,0.138120723530812,0.155385813972164,0.172650904413515,
0.207181085296218,0.276241447061625,0.414362170592437,0.422994715813113,
0.431627261033788,0.44889235147514,0.474789987137167,0.483422532357843,
0.552482894123249,0.604278165447304,0.621543255888655,0.690603617654061,
0.725133798536764,0.759663979419467,0.776929069860819,0.79419416030217,
0.811459250743522,0.820091795964198,0.824408068574536,0.826566204879705,
0.827645273032289,0.828724341184873,0.89778470295028,0.966845064715686),
(0.0377143719413095,0.167070624995476,0.336553194126115,0.499999999999991,
0.663446805873868,0.832929375004528,0.962285628059314),.UNSPECIFIED.);
#185=B_SPLINE_SURFACE_WITH_KNOTS('',3,3,((#38171,#38172,#38173,#38174,#38175,
#38176,#38177,#38178,#38179,#38180,#38181,#38182,#38183,#38184),(#38185,
#38186,#38187,#38188,#38189,#38190,#38191,#38192,#38193,#38194,#38195,#38196,
#38197,#38198),(#38199,#38200,#38201,#38202,#38203,#38204,#38205,#38206,
#38207,#38208,#38209,#38210,#38211,#38212),(#38213,#38214,#38215,#38216,
#38217,#38218,#38219,#38220,#38221,#38222,#38223,#38224,#38225,#38226),
(#38227,#38228,#38229,#38230,#38231,#38232,#38233,#38234,#38235,#38236,
#38237,#38238,#38239,#38240),(#38241,#38242,#38243,#38244,#38245,#38246,
#38247,#38248,#38249,#38250,#38251,#38252,#38253,#38254),(#38255,#38256,
#38257,#38258,#38259,#38260,#38261,#38262,#38263,#38264,#38265,#38266,#38267,
#38268),(#38269,#38270,#38271,#38272,#38273,#38274,#38275,#38276,#38277,
#38278,#38279,#38280,#38281,#38282),(#38283,#38284,#38285,#38286,#38287,
#38288,#38289,#38290,#38291,#38292,#38293,#38294,#38295,#38296),(#38297,
#38298,#38299,#38300,#38301,#38302,#38303,#38304,#38305,#38306,#38307,#38308,
#38309,#38310),(#38311,#38312,#38313,#38314,#38315,#38316,#38317,#38318,
#38319,#38320,#38321,#38322,#38323,#38324),(#38325,#38326,#38327,#38328,
#38329,#38330,#38331,#38332,#38333,#38334,#38335,#38336,#38337,#38338),
(#38339,#38340,#38341,#38342,#38343,#38344,#38345,#38346,#38347,#38348,
#38349,#38350,#38351,#38352),(#38353,#38354,#38355,#38356,#38357,#38358,
#38359,#38360,#38361,#38362,#38363,#38364,#38365,#38366),(#38367,#38368,
#38369,#38370,#38371,#38372,#38373,#38374,#38375,#38376,#38377,#38378,#38379,
#38380),(#38381,#38382,#38383,#38384,#38385,#38386,#38387,#38388,#38389,
#38390,#38391,#38392,#38393,#38394),(#38395,#38396,#38397,#38398,#38399,
#38400,#38401,#38402,#38403,#38404,#38405,#38406,#38407,#38408),(#38409,
#38410,#38411,#38412,#38413,#38414,#38415,#38416,#38417,#38418,#38419,#38420,
#38421,#38422),(#38423,#38424,#38425,#38426,#38427,#38428,#38429,#38430,
#38431,#38432,#38433,#38434,#38435,#38436),(#38437,#38438,#38439,#38440,
#38441,#38442,#38443,#38444,#38445,#38446,#38447,#38448,#38449,#38450),
(#38451,#38452,#38453,#38454,#38455,#38456,#38457,#38458,#38459,#38460,
#38461,#38462,#38463,#38464),(#38465,#38466,#38467,#38468,#38469,#38470,
#38471,#38472,#38473,#38474,#38475,#38476,#38477,#38478),(#38479,#38480,
#38481,#38482,#38483,#38484,#38485,#38486,#38487,#38488,#38489,#38490,#38491,
#38492),(#38493,#38494,#38495,#38496,#38497,#38498,#38499,#38500,#38501,
#38502,#38503,#38504,#38505,#38506),(#38507,#38508,#38509,#38510,#38511,
#38512,#38513,#38514,#38515,#38516,#38517,#38518,#38519,#38520),(#38521,
#38522,#38523,#38524,#38525,#38526,#38527,#38528,#38529,#38530,#38531,#38532,
#38533,#38534),(#38535,#38536,#38537,#38538,#38539,#38540,#38541,#38542,
#38543,#38544,#38545,#38546,#38547,#38548),(#38549,#38550,#38551,#38552,
#38553,#38554,#38555,#38556,#38557,#38558,#38559,#38560,#38561,#38562),
(#38563,#38564,#38565,#38566,#38567,#38568,#38569,#38570,#38571,#38572,
#38573,#38574,#38575,#38576)),.UNSPECIFIED.,.F.,.F.,.F.,(4,1,1,1,1,1,1,
1,1,1,1,1,1,1,1,1,1,1,1,1,1,1,1,1,1,1,4),(4,2,2,2,2,2,4),(0.0331549352864055,
0.102215297051662,0.171275658816919,0.173433795122083,0.175591931427247,
0.179908204037576,0.188540749258233,0.205805839699547,0.240336020582176,
0.274866201464804,0.309396382347432,0.378456744112689,0.412986924995318,
0.447517105877946,0.516577467643203,0.585637829408459,0.602902919849774,
0.620168010291088,0.654698191173716,0.689228372056345,0.723758552938973,
0.810084005145544,0.861879276469486,0.896409457352115,0.930939638234743,
0.948204728676057,1.),(0.0377143719413947,0.167070624995476,0.336553194126115,
0.499999999999991,0.663446805873868,0.832929375004528,0.962285628058718),
 .UNSPECIFIED.);
#186=B_SPLINE_SURFACE_WITH_KNOTS('',3,3,((#38633,#38634,#38635,#38636,#38637,
#38638,#38639,#38640,#38641,#38642,#38643,#38644,#38645,#38646),(#38647,
#38648,#38649,#38650,#38651,#38652,#38653,#38654,#38655,#38656,#38657,#38658,
#38659,#38660),(#38661,#38662,#38663,#38664,#38665,#38666,#38667,#38668,
#38669,#38670,#38671,#38672,#38673,#38674),(#38675,#38676,#38677,#38678,
#38679,#38680,#38681,#38682,#38683,#38684,#38685,#38686,#38687,#38688)),
 .UNSPECIFIED.,.F.,.F.,.F.,(4,4),(4,2,2,2,2,2,4),(0.,1.),(0.0377143719414212,
0.167070624995476,0.336553194126115,0.499999999999991,0.663446805873868,
0.832929375004528,0.962285628058582),.UNSPECIFIED.);
#187=B_SPLINE_SURFACE_WITH_KNOTS('',3,3,((#38703,#38704,#38705,#38706,#38707,
#38708,#38709,#38710,#38711,#38712,#38713,#38714,#38715,#38716),(#38717,
#38718,#38719,#38720,#38721,#38722,#38723,#38724,#38725,#38726,#38727,#38728,
#38729,#38730),(#38731,#38732,#38733,#38734,#38735,#38736,#38737,#38738,
#38739,#38740,#38741,#38742,#38743,#38744),(#38745,#38746,#38747,#38748,
#38749,#38750,#38751,#38752,#38753,#38754,#38755,#38756,#38757,#38758),
(#38759,#38760,#38761,#38762,#38763,#38764,#38765,#38766,#38767,#38768,
#38769,#38770,#38771,#38772),(#38773,#38774,#38775,#38776,#38777,#38778,
#38779,#38780,#38781,#38782,#38783,#38784,#38785,#38786),(#38787,#38788,
#38789,#38790,#38791,#38792,#38793,#38794,#38795,#38796,#38797,#38798,#38799,
#38800),(#38801,#38802,#38803,#38804,#38805,#38806,#38807,#38808,#38809,
#38810,#38811,#38812,#38813,#38814),(#38815,#38816,#38817,#38818,#38819,
#38820,#38821,#38822,#38823,#38824,#38825,#38826,#38827,#38828),(#38829,
#38830,#38831,#38832,#38833,#38834,#38835,#38836,#38837,#38838,#38839,#38840,
#38841,#38842),(#38843,#38844,#38845,#38846,#38847,#38848,#38849,#38850,
#38851,#38852,#38853,#38854,#38855,#38856),(#38857,#38858,#38859,#38860,
#38861,#38862,#38863,#38864,#38865,#38866,#38867,#38868,#38869,#38870),
(#38871,#38872,#38873,#38874,#38875,#38876,#38877,#38878,#38879,#38880,
#38881,#38882,#38883,#38884),(#38885,#38886,#38887,#38888,#38889,#38890,
#38891,#38892,#38893,#38894,#38895,#38896,#38897,#38898),(#38899,#38900,
#38901,#38902,#38903,#38904,#38905,#38906,#38907,#38908,#38909,#38910,#38911,
#38912),(#38913,#38914,#38915,#38916,#38917,#38918,#38919,#38920,#38921,
#38922,#38923,#38924,#38925,#38926),(#38927,#38928,#38929,#38930,#38931,
#38932,#38933,#38934,#38935,#38936,#38937,#38938,#38939,#38940),(#38941,
#38942,#38943,#38944,#38945,#38946,#38947,#38948,#38949,#38950,#38951,#38952,
#38953,#38954),(#38955,#38956,#38957,#38958,#38959,#38960,#38961,#38962,
#38963,#38964,#38965,#38966,#38967,#38968),(#38969,#38970,#38971,#38972,
#38973,#38974,#38975,#38976,#38977,#38978,#38979,#38980,#38981,#38982),
(#38983,#38984,#38985,#38986,#38987,#38988,#38989,#38990,#38991,#38992,
#38993,#38994,#38995,#38996),(#38997,#38998,#38999,#39000,#39001,#39002,
#39003,#39004,#39005,#39006,#39007,#39008,#39009,#39010),(#39011,#39012,
#39013,#39014,#39015,#39016,#39017,#39018,#39019,#39020,#39021,#39022,#39023,
#39024),(#39025,#39026,#39027,#39028,#39029,#39030,#39031,#39032,#39033,
#39034,#39035,#39036,#39037,#39038),(#39039,#39040,#39041,#39042,#39043,
#39044,#39045,#39046,#39047,#39048,#39049,#39050,#39051,#39052),(#39053,
#39054,#39055,#39056,#39057,#39058,#39059,#39060,#39061,#39062,#39063,#39064,
#39065,#39066),(#39067,#39068,#39069,#39070,#39071,#39072,#39073,#39074,
#39075,#39076,#39077,#39078,#39079,#39080),(#39081,#39082,#39083,#39084,
#39085,#39086,#39087,#39088,#39089,#39090,#39091,#39092,#39093,#39094),
(#39095,#39096,#39097,#39098,#39099,#39100,#39101,#39102,#39103,#39104,
#39105,#39106,#39107,#39108),(#39109,#39110,#39111,#39112,#39113,#39114,
#39115,#39116,#39117,#39118,#39119,#39120,#39121,#39122),(#39123,#39124,
#39125,#39126,#39127,#39128,#39129,#39130,#39131,#39132,#39133,#39134,#39135,
#39136),(#39137,#39138,#39139,#39140,#39141,#39142,#39143,#39144,#39145,
#39146,#39147,#39148,#39149,#39150),(#39151,#39152,#39153,#39154,#39155,
#39156,#39157,#39158,#39159,#39160,#39161,#39162,#39163,#39164),(#39165,
#39166,#39167,#39168,#39169,#39170,#39171,#39172,#39173,#39174,#39175,#39176,
#39177,#39178),(#39179,#39180,#39181,#39182,#39183,#39184,#39185,#39186,
#39187,#39188,#39189,#39190,#39191,#39192)),.UNSPECIFIED.,.F.,.F.,.F.,(4,
1,1,1,1,1,1,1,1,1,1,1,1,1,1,1,1,1,1,1,1,1,1,1,1,1,1,1,1,1,1,1,4),(4,2,2,
2,2,2,4),(0.,0.0517952713240544,0.0690603617654059,0.103590542648109,0.138120723530812,
0.155385813972163,0.172650904413515,0.207181085296218,0.276241447061624,
0.34530180882703,0.379831989709732,0.414362170592435,0.431627261033787,
0.448892351475138,0.46615744191649,0.483422532357841,0.552482894123247,
0.58701307500595,0.604278165447302,0.621543255888653,0.656073436771356,
0.690603617654059,0.759663979419465,0.776929069860816,0.794194160302168,
0.811459250743519,0.820091795964195,0.824408068574533,0.826566204879702,
0.827645273032286,0.828724341184871,0.897784702950277,0.966845064715683),
(0.0377143719406538,0.167070624995476,0.336553194126115,0.499999999999991,
0.663446805873868,0.832929375004528,0.96228562805863),.UNSPECIFIED.);
#188=B_SPLINE_SURFACE_WITH_KNOTS('',3,3,((#39248,#39249,#39250,#39251,#39252,
#39253,#39254,#39255,#39256,#39257,#39258,#39259,#39260,#39261),(#39262,
#39263,#39264,#39265,#39266,#39267,#39268,#39269,#39270,#39271,#39272,#39273,
#39274,#39275),(#39276,#39277,#39278,#39279,#39280,#39281,#39282,#39283,
#39284,#39285,#39286,#39287,#39288,#39289),(#39290,#39291,#39292,#39293,
#39294,#39295,#39296,#39297,#39298,#39299,#39300,#39301,#39302,#39303),
(#39304,#39305,#39306,#39307,#39308,#39309,#39310,#39311,#39312,#39313,
#39314,#39315,#39316,#39317),(#39318,#39319,#39320,#39321,#39322,#39323,
#39324,#39325,#39326,#39327,#39328,#39329,#39330,#39331),(#39332,#39333,
#39334,#39335,#39336,#39337,#39338,#39339,#39340,#39341,#39342,#39343,#39344,
#39345),(#39346,#39347,#39348,#39349,#39350,#39351,#39352,#39353,#39354,
#39355,#39356,#39357,#39358,#39359),(#39360,#39361,#39362,#39363,#39364,
#39365,#39366,#39367,#39368,#39369,#39370,#39371,#39372,#39373),(#39374,
#39375,#39376,#39377,#39378,#39379,#39380,#39381,#39382,#39383,#39384,#39385,
#39386,#39387),(#39388,#39389,#39390,#39391,#39392,#39393,#39394,#39395,
#39396,#39397,#39398,#39399,#39400,#39401),(#39402,#39403,#39404,#39405,
#39406,#39407,#39408,#39409,#39410,#39411,#39412,#39413,#39414,#39415),
(#39416,#39417,#39418,#39419,#39420,#39421,#39422,#39423,#39424,#39425,
#39426,#39427,#39428,#39429),(#39430,#39431,#39432,#39433,#39434,#39435,
#39436,#39437,#39438,#39439,#39440,#39441,#39442,#39443),(#39444,#39445,
#39446,#39447,#39448,#39449,#39450,#39451,#39452,#39453,#39454,#39455,#39456,
#39457),(#39458,#39459,#39460,#39461,#39462,#39463,#39464,#39465,#39466,
#39467,#39468,#39469,#39470,#39471),(#39472,#39473,#39474,#39475,#39476,
#39477,#39478,#39479,#39480,#39481,#39482,#39483,#39484,#39485),(#39486,
#39487,#39488,#39489,#39490,#39491,#39492,#39493,#39494,#39495,#39496,#39497,
#39498,#39499),(#39500,#39501,#39502,#39503,#39504,#39505,#39506,#39507,
#39508,#39509,#39510,#39511,#39512,#39513),(#39514,#39515,#39516,#39517,
#39518,#39519,#39520,#39521,#39522,#39523,#39524,#39525,#39526,#39527),
(#39528,#39529,#39530,#39531,#39532,#39533,#39534,#39535,#39536,#39537,
#39538,#39539,#39540,#39541),(#39542,#39543,#39544,#39545,#39546,#39547,
#39548,#39549,#39550,#39551,#39552,#39553,#39554,#39555),(#39556,#39557,
#39558,#39559,#39560,#39561,#39562,#39563,#39564,#39565,#39566,#39567,#39568,
#39569),(#39570,#39571,#39572,#39573,#39574,#39575,#39576,#39577,#39578,
#39579,#39580,#39581,#39582,#39583),(#39584,#39585,#39586,#39587,#39588,
#39589,#39590,#39591,#39592,#39593,#39594,#39595,#39596,#39597),(#39598,
#39599,#39600,#39601,#39602,#39603,#39604,#39605,#39606,#39607,#39608,#39609,
#39610,#39611),(#39612,#39613,#39614,#39615,#39616,#39617,#39618,#39619,
#39620,#39621,#39622,#39623,#39624,#39625),(#39626,#39627,#39628,#39629,
#39630,#39631,#39632,#39633,#39634,#39635,#39636,#39637,#39638,#39639),
(#39640,#39641,#39642,#39643,#39644,#39645,#39646,#39647,#39648,#39649,
#39650,#39651,#39652,#39653),(#39654,#39655,#39656,#39657,#39658,#39659,
#39660,#39661,#39662,#39663,#39664,#39665,#39666,#39667),(#39668,#39669,
#39670,#39671,#39672,#39673,#39674,#39675,#39676,#39677,#39678,#39679,#39680,
#39681),(#39682,#39683,#39684,#39685,#39686,#39687,#39688,#39689,#39690,
#39691,#39692,#39693,#39694,#39695),(#39696,#39697,#39698,#39699,#39700,
#39701,#39702,#39703,#39704,#39705,#39706,#39707,#39708,#39709),(#39710,
#39711,#39712,#39713,#39714,#39715,#39716,#39717,#39718,#39719,#39720,#39721,
#39722,#39723),(#39724,#39725,#39726,#39727,#39728,#39729,#39730,#39731,
#39732,#39733,#39734,#39735,#39736,#39737),(#39738,#39739,#39740,#39741,
#39742,#39743,#39744,#39745,#39746,#39747,#39748,#39749,#39750,#39751)),
 .UNSPECIFIED.,.F.,.F.,.F.,(4,1,1,1,1,1,1,1,1,1,1,1,1,1,1,1,1,1,1,1,1,1,
1,1,1,1,1,1,1,1,1,1,1,4),(4,2,2,2,2,2,4),(0.0331549352864097,0.102215297051666,
0.171275658816923,0.171815192893214,0.172354726969505,0.172894261045796,
0.173433795122087,0.175591931427251,0.177750067732415,0.178829135884997,
0.17990820403758,0.188540749258237,0.205805839699551,0.214438384920208,
0.223070930140865,0.231703475361522,0.240336020582179,0.274866201464807,
0.309396382347435,0.378456744112692,0.41298692499532,0.430252015436634,
0.447517105877948,0.516577467643205,0.585637829408461,0.671963281615032,
0.689228372056346,0.723758552938974,0.810084005145545,0.861879276469487,
0.896409457352115,0.930939638234744,0.948204728676058,1.),(0.0377143719409187,
0.167070624995476,0.336553194126115,0.499999999999991,0.663446805873868,
0.832929375004528,0.962285628058664),.UNSPECIFIED.);
#189=B_SPLINE_SURFACE_WITH_KNOTS('',3,3,((#39812,#39813,#39814,#39815,#39816,
#39817,#39818,#39819,#39820,#39821,#39822,#39823,#39824,#39825),(#39826,
#39827,#39828,#39829,#39830,#39831,#39832,#39833,#39834,#39835,#39836,#39837,
#39838,#39839),(#39840,#39841,#39842,#39843,#39844,#39845,#39846,#39847,
#39848,#39849,#39850,#39851,#39852,#39853),(#39854,#39855,#39856,#39857,
#39858,#39859,#39860,#39861,#39862,#39863,#39864,#39865,#39866,#39867)),
 .UNSPECIFIED.,.F.,.F.,.F.,(4,4),(4,2,2,2,2,2,4),(0.,1.),(0.0377143719414211,
0.167070624995476,0.336553194126115,0.499999999999991,0.663446805873868,
0.832929375004528,0.962285628058582),.UNSPECIFIED.);
#190=B_SPLINE_SURFACE_WITH_KNOTS('',3,3,((#39882,#39883,#39884,#39885,#39886,
#39887,#39888,#39889,#39890,#39891,#39892,#39893,#39894,#39895),(#39896,
#39897,#39898,#39899,#39900,#39901,#39902,#39903,#39904,#39905,#39906,#39907,
#39908,#39909),(#39910,#39911,#39912,#39913,#39914,#39915,#39916,#39917,
#39918,#39919,#39920,#39921,#39922,#39923),(#39924,#39925,#39926,#39927,
#39928,#39929,#39930,#39931,#39932,#39933,#39934,#39935,#39936,#39937),
(#39938,#39939,#39940,#39941,#39942,#39943,#39944,#39945,#39946,#39947,
#39948,#39949,#39950,#39951),(#39952,#39953,#39954,#39955,#39956,#39957,
#39958,#39959,#39960,#39961,#39962,#39963,#39964,#39965),(#39966,#39967,
#39968,#39969,#39970,#39971,#39972,#39973,#39974,#39975,#39976,#39977,#39978,
#39979),(#39980,#39981,#39982,#39983,#39984,#39985,#39986,#39987,#39988,
#39989,#39990,#39991,#39992,#39993),(#39994,#39995,#39996,#39997,#39998,
#39999,#40000,#40001,#40002,#40003,#40004,#40005,#40006,#40007),(#40008,
#40009,#40010,#40011,#40012,#40013,#40014,#40015,#40016,#40017,#40018,#40019,
#40020,#40021),(#40022,#40023,#40024,#40025,#40026,#40027,#40028,#40029,
#40030,#40031,#40032,#40033,#40034,#40035),(#40036,#40037,#40038,#40039,
#40040,#40041,#40042,#40043,#40044,#40045,#40046,#40047,#40048,#40049),
(#40050,#40051,#40052,#40053,#40054,#40055,#40056,#40057,#40058,#40059,
#40060,#40061,#40062,#40063),(#40064,#40065,#40066,#40067,#40068,#40069,
#40070,#40071,#40072,#40073,#40074,#40075,#40076,#40077),(#40078,#40079,
#40080,#40081,#40082,#40083,#40084,#40085,#40086,#40087,#40088,#40089,#40090,
#40091),(#40092,#40093,#40094,#40095,#40096,#40097,#40098,#40099,#40100,
#40101,#40102,#40103,#40104,#40105),(#40106,#40107,#40108,#40109,#40110,
#40111,#40112,#40113,#40114,#40115,#40116,#40117,#40118,#40119),(#40120,
#40121,#40122,#40123,#40124,#40125,#40126,#40127,#40128,#40129,#40130,#40131,
#40132,#40133),(#40134,#40135,#40136,#40137,#40138,#40139,#40140,#40141,
#40142,#40143,#40144,#40145,#40146,#40147),(#40148,#40149,#40150,#40151,
#40152,#40153,#40154,#40155,#40156,#40157,#40158,#40159,#40160,#40161),
(#40162,#40163,#40164,#40165,#40166,#40167,#40168,#40169,#40170,#40171,
#40172,#40173,#40174,#40175),(#40176,#40177,#40178,#40179,#40180,#40181,
#40182,#40183,#40184,#40185,#40186,#40187,#40188,#40189),(#40190,#40191,
#40192,#40193,#40194,#40195,#40196,#40197,#40198,#40199,#40200,#40201,#40202,
#40203),(#40204,#40205,#40206,#40207,#40208,#40209,#40210,#40211,#40212,
#40213,#40214,#40215,#40216,#40217),(#40218,#40219,#40220,#40221,#40222,
#40223,#40224,#40225,#40226,#40227,#40228,#40229,#40230,#40231),(#40232,
#40233,#40234,#40235,#40236,#40237,#40238,#40239,#40240,#40241,#40242,#40243,
#40244,#40245),(#40246,#40247,#40248,#40249,#40250,#40251,#40252,#40253,
#40254,#40255,#40256,#40257,#40258,#40259),(#40260,#40261,#40262,#40263,
#40264,#40265,#40266,#40267,#40268,#40269,#40270,#40271,#40272,#40273),
(#40274,#40275,#40276,#40277,#40278,#40279,#40280,#40281,#40282,#40283,
#40284,#40285,#40286,#40287),(#40288,#40289,#40290,#40291,#40292,#40293,
#40294,#40295,#40296,#40297,#40298,#40299,#40300,#40301),(#40302,#40303,
#40304,#40305,#40306,#40307,#40308,#40309,#40310,#40311,#40312,#40313,#40314,
#40315),(#40316,#40317,#40318,#40319,#40320,#40321,#40322,#40323,#40324,
#40325,#40326,#40327,#40328,#40329),(#40330,#40331,#40332,#40333,#40334,
#40335,#40336,#40337,#40338,#40339,#40340,#40341,#40342,#40343),(#40344,
#40345,#40346,#40347,#40348,#40349,#40350,#40351,#40352,#40353,#40354,#40355,
#40356,#40357),(#40358,#40359,#40360,#40361,#40362,#40363,#40364,#40365,
#40366,#40367,#40368,#40369,#40370,#40371),(#40372,#40373,#40374,#40375,
#40376,#40377,#40378,#40379,#40380,#40381,#40382,#40383,#40384,#40385),
(#40386,#40387,#40388,#40389,#40390,#40391,#40392,#40393,#40394,#40395,
#40396,#40397,#40398,#40399),(#40400,#40401,#40402,#40403,#40404,#40405,
#40406,#40407,#40408,#40409,#40410,#40411,#40412,#40413),(#40414,#40415,
#40416,#40417,#40418,#40419,#40420,#40421,#40422,#40423,#40424,#40425,#40426,
#40427),(#40428,#40429,#40430,#40431,#40432,#40433,#40434,#40435,#40436,
#40437,#40438,#40439,#40440,#40441)),.UNSPECIFIED.,.F.,.F.,.F.,(4,1,1,1,
1,1,1,1,1,1,1,1,1,1,1,1,1,1,1,1,1,1,1,1,1,1,1,1,1,1,1,1,1,1,1,1,1,4),(4,
2,2,2,2,2,4),(0.,0.0517952713240544,0.0690603617654059,0.0863254522067574,
0.103590542648109,0.138120723530812,0.155385813972163,0.189915994854866,
0.207181085296218,0.276241447061624,0.345301808827029,0.379831989709732,
0.414362170592435,0.448892351475138,0.500687622799193,0.552482894123247,
0.569747984564599,0.621543255888653,0.638808346330004,0.690603617654059,
0.725133798536762,0.742398888978113,0.759663979419465,0.776929069860816,
0.794194160302168,0.798510432912505,0.802826705522843,0.811459250743519,
0.820091795964195,0.822249932269364,0.824408068574533,0.826566204879702,
0.827645273032286,0.828184807108578,0.828724341184871,0.897784702950276,
0.932314883832979,0.966845064715682),(0.0377143719385139,0.167070624995476,
0.336553194126115,0.499999999999991,0.663446805873868,0.832929375004528,
0.962285628061),.UNSPECIFIED.);
#191=B_SPLINE_SURFACE_WITH_KNOTS('',3,3,((#40497,#40498,#40499,#40500,#40501,
#40502,#40503,#40504,#40505,#40506,#40507,#40508,#40509,#40510),(#40511,
#40512,#40513,#40514,#40515,#40516,#40517,#40518,#40519,#40520,#40521,#40522,
#40523,#40524),(#40525,#40526,#40527,#40528,#40529,#40530,#40531,#40532,
#40533,#40534,#40535,#40536,#40537,#40538),(#40539,#40540,#40541,#40542,
#40543,#40544,#40545,#40546,#40547,#40548,#40549,#40550,#40551,#40552),
(#40553,#40554,#40555,#40556,#40557,#40558,#40559,#40560,#40561,#40562,
#40563,#40564,#40565,#40566),(#40567,#40568,#40569,#40570,#40571,#40572,
#40573,#40574,#40575,#40576,#40577,#40578,#40579,#40580),(#40581,#40582,
#40583,#40584,#40585,#40586,#40587,#40588,#40589,#40590,#40591,#40592,#40593,
#40594),(#40595,#40596,#40597,#40598,#40599,#40600,#40601,#40602,#40603,
#40604,#40605,#40606,#40607,#40608),(#40609,#40610,#40611,#40612,#40613,
#40614,#40615,#40616,#40617,#40618,#40619,#40620,#40621,#40622),(#40623,
#40624,#40625,#40626,#40627,#40628,#40629,#40630,#40631,#40632,#40633,#40634,
#40635,#40636),(#40637,#40638,#40639,#40640,#40641,#40642,#40643,#40644,
#40645,#40646,#40647,#40648,#40649,#40650),(#40651,#40652,#40653,#40654,
#40655,#40656,#40657,#40658,#40659,#40660,#40661,#40662,#40663,#40664),
(#40665,#40666,#40667,#40668,#40669,#40670,#40671,#40672,#40673,#40674,
#40675,#40676,#40677,#40678),(#40679,#40680,#40681,#40682,#40683,#40684,
#40685,#40686,#40687,#40688,#40689,#40690,#40691,#40692),(#40693,#40694,
#40695,#40696,#40697,#40698,#40699,#40700,#40701,#40702,#40703,#40704,#40705,
#40706),(#40707,#40708,#40709,#40710,#40711,#40712,#40713,#40714,#40715,
#40716,#40717,#40718,#40719,#40720),(#40721,#40722,#40723,#40724,#40725,
#40726,#40727,#40728,#40729,#40730,#40731,#40732,#40733,#40734),(#40735,
#40736,#40737,#40738,#40739,#40740,#40741,#40742,#40743,#40744,#40745,#40746,
#40747,#40748),(#40749,#40750,#40751,#40752,#40753,#40754,#40755,#40756,
#40757,#40758,#40759,#40760,#40761,#40762),(#40763,#40764,#40765,#40766,
#40767,#40768,#40769,#40770,#40771,#40772,#40773,#40774,#40775,#40776),
(#40777,#40778,#40779,#40780,#40781,#40782,#40783,#40784,#40785,#40786,
#40787,#40788,#40789,#40790),(#40791,#40792,#40793,#40794,#40795,#40796,
#40797,#40798,#40799,#40800,#40801,#40802,#40803,#40804),(#40805,#40806,
#40807,#40808,#40809,#40810,#40811,#40812,#40813,#40814,#40815,#40816,#40817,
#40818),(#40819,#40820,#40821,#40822,#40823,#40824,#40825,#40826,#40827,
#40828,#40829,#40830,#40831,#40832),(#40833,#40834,#40835,#40836,#40837,
#40838,#40839,#40840,#40841,#40842,#40843,#40844,#40845,#40846),(#40847,
#40848,#40849,#40850,#40851,#40852,#40853,#40854,#40855,#40856,#40857,#40858,
#40859,#40860),(#40861,#40862,#40863,#40864,#40865,#40866,#40867,#40868,
#40869,#40870,#40871,#40872,#40873,#40874),(#40875,#40876,#40877,#40878,
#40879,#40880,#40881,#40882,#40883,#40884,#40885,#40886,#40887,#40888),
(#40889,#40890,#40891,#40892,#40893,#40894,#40895,#40896,#40897,#40898,
#40899,#40900,#40901,#40902)),.UNSPECIFIED.,.F.,.F.,.F.,(4,1,1,1,1,1,1,
1,1,1,1,1,1,1,1,1,1,1,1,1,1,1,1,1,1,1,4),(4,2,2,2,2,2,4),(0.0331549352864072,
0.102215297051664,0.17127565881692,0.173433795122085,0.175591931427249,
0.179908204037578,0.188540749258235,0.205805839699549,0.240336020582177,
0.274866201464805,0.309396382347434,0.37845674411269,0.412986924995319,
0.447517105877947,0.516577467643204,0.58563782940846,0.602902919849775,
0.620168010291089,0.654698191173717,0.689228372056345,0.723758552938974,
0.810084005145544,0.861879276469487,0.896409457352115,0.930939638234743,
0.948204728676058,1.),(0.0377143719409187,0.167070624995476,0.336553194126115,
0.499999999999991,0.663446805873868,0.832929375004528,0.962285628058774),
 .UNSPECIFIED.);
#192=B_SPLINE_SURFACE_WITH_KNOTS('',3,3,((#40959,#40960,#40961,#40962,#40963,
#40964,#40965,#40966,#40967,#40968,#40969,#40970,#40971,#40972),(#40973,
#40974,#40975,#40976,#40977,#40978,#40979,#40980,#40981,#40982,#40983,#40984,
#40985,#40986),(#40987,#40988,#40989,#40990,#40991,#40992,#40993,#40994,
#40995,#40996,#40997,#40998,#40999,#41000),(#41001,#41002,#41003,#41004,
#41005,#41006,#41007,#41008,#41009,#41010,#41011,#41012,#41013,#41014)),
 .UNSPECIFIED.,.F.,.F.,.F.,(4,4),(4,2,2,2,2,2,4),(0.,1.),(0.0377143719414211,
0.167070624995476,0.336553194126115,0.499999999999991,0.663446805873868,
0.832929375004528,0.962285628058582),.UNSPECIFIED.);
#193=B_SPLINE_SURFACE_WITH_KNOTS('',3,3,((#41029,#41030,#41031,#41032,#41033,
#41034,#41035,#41036,#41037,#41038,#41039,#41040,#41041,#41042),(#41043,
#41044,#41045,#41046,#41047,#41048,#41049,#41050,#41051,#41052,#41053,#41054,
#41055,#41056),(#41057,#41058,#41059,#41060,#41061,#41062,#41063,#41064,
#41065,#41066,#41067,#41068,#41069,#41070),(#41071,#41072,#41073,#41074,
#41075,#41076,#41077,#41078,#41079,#41080,#41081,#41082,#41083,#41084),
(#41085,#41086,#41087,#41088,#41089,#41090,#41091,#41092,#41093,#41094,
#41095,#41096,#41097,#41098),(#41099,#41100,#41101,#41102,#41103,#41104,
#41105,#41106,#41107,#41108,#41109,#41110,#41111,#41112),(#41113,#41114,
#41115,#41116,#41117,#41118,#41119,#41120,#41121,#41122,#41123,#41124,#41125,
#41126),(#41127,#41128,#41129,#41130,#41131,#41132,#41133,#41134,#41135,
#41136,#41137,#41138,#41139,#41140),(#41141,#41142,#41143,#41144,#41145,
#41146,#41147,#41148,#41149,#41150,#41151,#41152,#41153,#41154),(#41155,
#41156,#41157,#41158,#41159,#41160,#41161,#41162,#41163,#41164,#41165,#41166,
#41167,#41168),(#41169,#41170,#41171,#41172,#41173,#41174,#41175,#41176,
#41177,#41178,#41179,#41180,#41181,#41182),(#41183,#41184,#41185,#41186,
#41187,#41188,#41189,#41190,#41191,#41192,#41193,#41194,#41195,#41196),
(#41197,#41198,#41199,#41200,#41201,#41202,#41203,#41204,#41205,#41206,
#41207,#41208,#41209,#41210),(#41211,#41212,#41213,#41214,#41215,#41216,
#41217,#41218,#41219,#41220,#41221,#41222,#41223,#41224),(#41225,#41226,
#41227,#41228,#41229,#41230,#41231,#41232,#41233,#41234,#41235,#41236,#41237,
#41238),(#41239,#41240,#41241,#41242,#41243,#41244,#41245,#41246,#41247,
#41248,#41249,#41250,#41251,#41252),(#41253,#41254,#41255,#41256,#41257,
#41258,#41259,#41260,#41261,#41262,#41263,#41264,#41265,#41266),(#41267,
#41268,#41269,#41270,#41271,#41272,#41273,#41274,#41275,#41276,#41277,#41278,
#41279,#41280),(#41281,#41282,#41283,#41284,#41285,#41286,#41287,#41288,
#41289,#41290,#41291,#41292,#41293,#41294),(#41295,#41296,#41297,#41298,
#41299,#41300,#41301,#41302,#41303,#41304,#41305,#41306,#41307,#41308),
(#41309,#41310,#41311,#41312,#41313,#41314,#41315,#41316,#41317,#41318,
#41319,#41320,#41321,#41322),(#41323,#41324,#41325,#41326,#41327,#41328,
#41329,#41330,#41331,#41332,#41333,#41334,#41335,#41336),(#41337,#41338,
#41339,#41340,#41341,#41342,#41343,#41344,#41345,#41346,#41347,#41348,#41349,
#41350),(#41351,#41352,#41353,#41354,#41355,#41356,#41357,#41358,#41359,
#41360,#41361,#41362,#41363,#41364),(#41365,#41366,#41367,#41368,#41369,
#41370,#41371,#41372,#41373,#41374,#41375,#41376,#41377,#41378),(#41379,
#41380,#41381,#41382,#41383,#41384,#41385,#41386,#41387,#41388,#41389,#41390,
#41391,#41392),(#41393,#41394,#41395,#41396,#41397,#41398,#41399,#41400,
#41401,#41402,#41403,#41404,#41405,#41406),(#41407,#41408,#41409,#41410,
#41411,#41412,#41413,#41414,#41415,#41416,#41417,#41418,#41419,#41420),
(#41421,#41422,#41423,#41424,#41425,#41426,#41427,#41428,#41429,#41430,
#41431,#41432,#41433,#41434),(#41435,#41436,#41437,#41438,#41439,#41440,
#41441,#41442,#41443,#41444,#41445,#41446,#41447,#41448),(#41449,#41450,
#41451,#41452,#41453,#41454,#41455,#41456,#41457,#41458,#41459,#41460,#41461,
#41462),(#41463,#41464,#41465,#41466,#41467,#41468,#41469,#41470,#41471,
#41472,#41473,#41474,#41475,#41476),(#41477,#41478,#41479,#41480,#41481,
#41482,#41483,#41484,#41485,#41486,#41487,#41488,#41489,#41490),(#41491,
#41492,#41493,#41494,#41495,#41496,#41497,#41498,#41499,#41500,#41501,#41502,
#41503,#41504),(#41505,#41506,#41507,#41508,#41509,#41510,#41511,#41512,
#41513,#41514,#41515,#41516,#41517,#41518),(#41519,#41520,#41521,#41522,
#41523,#41524,#41525,#41526,#41527,#41528,#41529,#41530,#41531,#41532),
(#41533,#41534,#41535,#41536,#41537,#41538,#41539,#41540,#41541,#41542,
#41543,#41544,#41545,#41546)),.UNSPECIFIED.,.F.,.F.,.F.,(4,1,1,1,1,1,1,
1,1,1,1,1,1,1,1,1,1,1,1,1,1,1,1,1,1,1,1,1,1,1,1,1,1,1,4),(4,2,2,2,2,2,4),
(0.,0.034530180882703,0.0517952713240545,0.0690603617654059,0.103590542648109,
0.138120723530812,0.155385813972163,0.189915994854866,0.207181085296218,
0.276241447061624,0.34530180882703,0.379831989709733,0.414362170592436,
0.448892351475139,0.483422532357842,0.552482894123247,0.621543255888653,
0.656073436771356,0.690603617654059,0.725133798536762,0.759663979419465,
0.776929069860817,0.785561615081493,0.794194160302168,0.81145925074352,
0.815775523353858,0.820091795964196,0.824408068574533,0.826566204879702,
0.827645273032287,0.828724341184871,0.880519612508926,0.897784702950277,
0.93231488383298,0.966845064715683),(0.0377143719413868,0.167070624995476,
0.336553194126115,0.499999999999991,0.663446805873868,0.832929375004528,
0.962285628060268),.UNSPECIFIED.);
#194=B_SPLINE_SURFACE_WITH_KNOTS('',3,3,((#41598,#41599,#41600,#41601,#41602,
#41603,#41604,#41605,#41606,#41607,#41608,#41609,#41610,#41611),(#41612,
#41613,#41614,#41615,#41616,#41617,#41618,#41619,#41620,#41621,#41622,#41623,
#41624,#41625),(#41626,#41627,#41628,#41629,#41630,#41631,#41632,#41633,
#41634,#41635,#41636,#41637,#41638,#41639),(#41640,#41641,#41642,#41643,
#41644,#41645,#41646,#41647,#41648,#41649,#41650,#41651,#41652,#41653),
(#41654,#41655,#41656,#41657,#41658,#41659,#41660,#41661,#41662,#41663,
#41664,#41665,#41666,#41667),(#41668,#41669,#41670,#41671,#41672,#41673,
#41674,#41675,#41676,#41677,#41678,#41679,#41680,#41681),(#41682,#41683,
#41684,#41685,#41686,#41687,#41688,#41689,#41690,#41691,#41692,#41693,#41694,
#41695),(#41696,#41697,#41698,#41699,#41700,#41701,#41702,#41703,#41704,
#41705,#41706,#41707,#41708,#41709),(#41710,#41711,#41712,#41713,#41714,
#41715,#41716,#41717,#41718,#41719,#41720,#41721,#41722,#41723),(#41724,
#41725,#41726,#41727,#41728,#41729,#41730,#41731,#41732,#41733,#41734,#41735,
#41736,#41737),(#41738,#41739,#41740,#41741,#41742,#41743,#41744,#41745,
#41746,#41747,#41748,#41749,#41750,#41751),(#41752,#41753,#41754,#41755,
#41756,#41757,#41758,#41759,#41760,#41761,#41762,#41763,#41764,#41765),
(#41766,#41767,#41768,#41769,#41770,#41771,#41772,#41773,#41774,#41775,
#41776,#41777,#41778,#41779),(#41780,#41781,#41782,#41783,#41784,#41785,
#41786,#41787,#41788,#41789,#41790,#41791,#41792,#41793),(#41794,#41795,
#41796,#41797,#41798,#41799,#41800,#41801,#41802,#41803,#41804,#41805,#41806,
#41807),(#41808,#41809,#41810,#41811,#41812,#41813,#41814,#41815,#41816,
#41817,#41818,#41819,#41820,#41821),(#41822,#41823,#41824,#41825,#41826,
#41827,#41828,#41829,#41830,#41831,#41832,#41833,#41834,#41835),(#41836,
#41837,#41838,#41839,#41840,#41841,#41842,#41843,#41844,#41845,#41846,#41847,
#41848,#41849),(#41850,#41851,#41852,#41853,#41854,#41855,#41856,#41857,
#41858,#41859,#41860,#41861,#41862,#41863),(#41864,#41865,#41866,#41867,
#41868,#41869,#41870,#41871,#41872,#41873,#41874,#41875,#41876,#41877),
(#41878,#41879,#41880,#41881,#41882,#41883,#41884,#41885,#41886,#41887,
#41888,#41889,#41890,#41891),(#41892,#41893,#41894,#41895,#41896,#41897,
#41898,#41899,#41900,#41901,#41902,#41903,#41904,#41905),(#41906,#41907,
#41908,#41909,#41910,#41911,#41912,#41913,#41914,#41915,#41916,#41917,#41918,
#41919),(#41920,#41921,#41922,#41923,#41924,#41925,#41926,#41927,#41928,
#41929,#41930,#41931,#41932,#41933),(#41934,#41935,#41936,#41937,#41938,
#41939,#41940,#41941,#41942,#41943,#41944,#41945,#41946,#41947),(#41948,
#41949,#41950,#41951,#41952,#41953,#41954,#41955,#41956,#41957,#41958,#41959,
#41960,#41961),(#41962,#41963,#41964,#41965,#41966,#41967,#41968,#41969,
#41970,#41971,#41972,#41973,#41974,#41975),(#41976,#41977,#41978,#41979,
#41980,#41981,#41982,#41983,#41984,#41985,#41986,#41987,#41988,#41989),
(#41990,#41991,#41992,#41993,#41994,#41995,#41996,#41997,#41998,#41999,
#42000,#42001,#42002,#42003),(#42004,#42005,#42006,#42007,#42008,#42009,
#42010,#42011,#42012,#42013,#42014,#42015,#42016,#42017)),.UNSPECIFIED.,
 .F.,.F.,.F.,(4,1,1,1,1,1,1,1,1,1,1,1,1,1,1,1,1,1,1,1,1,1,1,1,1,1,1,4),
(4,2,2,2,2,2,4),(0.0331549352864093,0.102215297051666,0.171275658816922,
0.173433795122087,0.175591931427251,0.179908204037579,0.188540749258236,
0.20580583969955,0.214438384920208,0.223070930140865,0.240336020582179,
0.309396382347435,0.395721834554006,0.447517105877948,0.482047286760576,
0.49931237720189,0.516577467643205,0.551107648525833,0.585637829408461,
0.620168010291089,0.723758552938974,0.79281891470423,0.827349095586859,
0.861879276469487,0.896409457352115,0.930939638234743,0.948204728676058,
1.),(0.0377143719413723,0.167070624995476,0.336553194126115,0.499999999999991,
0.663446805873868,0.832929375004528,0.96228562805941),.UNSPECIFIED.);
#195=B_SPLINE_SURFACE_WITH_KNOTS('',3,3,((#42074,#42075,#42076,#42077,#42078,
#42079,#42080,#42081,#42082,#42083,#42084,#42085,#42086,#42087),(#42088,
#42089,#42090,#42091,#42092,#42093,#42094,#42095,#42096,#42097,#42098,#42099,
#42100,#42101),(#42102,#42103,#42104,#42105,#42106,#42107,#42108,#42109,
#42110,#42111,#42112,#42113,#42114,#42115),(#42116,#42117,#42118,#42119,
#42120,#42121,#42122,#42123,#42124,#42125,#42126,#42127,#42128,#42129)),
 .UNSPECIFIED.,.F.,.F.,.F.,(4,4),(4,2,2,2,2,2,4),(0.,1.),(0.0377143719414211,
0.167070624995476,0.336553194126115,0.499999999999991,0.663446805873868,
0.832929375004528,0.962285628058582),.UNSPECIFIED.);
#196=B_SPLINE_SURFACE_WITH_KNOTS('',3,3,((#42144,#42145,#42146,#42147,#42148,
#42149,#42150,#42151,#42152,#42153,#42154,#42155,#42156,#42157),(#42158,
#42159,#42160,#42161,#42162,#42163,#42164,#42165,#42166,#42167,#42168,#42169,
#42170,#42171),(#42172,#42173,#42174,#42175,#42176,#42177,#42178,#42179,
#42180,#42181,#42182,#42183,#42184,#42185),(#42186,#42187,#42188,#42189,
#42190,#42191,#42192,#42193,#42194,#42195,#42196,#42197,#42198,#42199),
(#42200,#42201,#42202,#42203,#42204,#42205,#42206,#42207,#42208,#42209,
#42210,#42211,#42212,#42213),(#42214,#42215,#42216,#42217,#42218,#42219,
#42220,#42221,#42222,#42223,#42224,#42225,#42226,#42227),(#42228,#42229,
#42230,#42231,#42232,#42233,#42234,#42235,#42236,#42237,#42238,#42239,#42240,
#42241),(#42242,#42243,#42244,#42245,#42246,#42247,#42248,#42249,#42250,
#42251,#42252,#42253,#42254,#42255),(#42256,#42257,#42258,#42259,#42260,
#42261,#42262,#42263,#42264,#42265,#42266,#42267,#42268,#42269),(#42270,
#42271,#42272,#42273,#42274,#42275,#42276,#42277,#42278,#42279,#42280,#42281,
#42282,#42283),(#42284,#42285,#42286,#42287,#42288,#42289,#42290,#42291,
#42292,#42293,#42294,#42295,#42296,#42297),(#42298,#42299,#42300,#42301,
#42302,#42303,#42304,#42305,#42306,#42307,#42308,#42309,#42310,#42311),
(#42312,#42313,#42314,#42315,#42316,#42317,#42318,#42319,#42320,#42321,
#42322,#42323,#42324,#42325),(#42326,#42327,#42328,#42329,#42330,#42331,
#42332,#42333,#42334,#42335,#42336,#42337,#42338,#42339),(#42340,#42341,
#42342,#42343,#42344,#42345,#42346,#42347,#42348,#42349,#42350,#42351,#42352,
#42353),(#42354,#42355,#42356,#42357,#42358,#42359,#42360,#42361,#42362,
#42363,#42364,#42365,#42366,#42367),(#42368,#42369,#42370,#42371,#42372,
#42373,#42374,#42375,#42376,#42377,#42378,#42379,#42380,#42381),(#42382,
#42383,#42384,#42385,#42386,#42387,#42388,#42389,#42390,#42391,#42392,#42393,
#42394,#42395),(#42396,#42397,#42398,#42399,#42400,#42401,#42402,#42403,
#42404,#42405,#42406,#42407,#42408,#42409),(#42410,#42411,#42412,#42413,
#42414,#42415,#42416,#42417,#42418,#42419,#42420,#42421,#42422,#42423),
(#42424,#42425,#42426,#42427,#42428,#42429,#42430,#42431,#42432,#42433,
#42434,#42435,#42436,#42437),(#42438,#42439,#42440,#42441,#42442,#42443,
#42444,#42445,#42446,#42447,#42448,#42449,#42450,#42451),(#42452,#42453,
#42454,#42455,#42456,#42457,#42458,#42459,#42460,#42461,#42462,#42463,#42464,
#42465),(#42466,#42467,#42468,#42469,#42470,#42471,#42472,#42473,#42474,
#42475,#42476,#42477,#42478,#42479),(#42480,#42481,#42482,#42483,#42484,
#42485,#42486,#42487,#42488,#42489,#42490,#42491,#42492,#42493),(#42494,
#42495,#42496,#42497,#42498,#42499,#42500,#42501,#42502,#42503,#42504,#42505,
#42506,#42507)),.UNSPECIFIED.,.F.,.F.,.F.,(4,1,1,1,1,1,1,1,1,1,1,1,1,1,
1,1,1,1,1,1,1,1,1,4),(4,2,2,2,2,2,4),(0.,0.0517952713240544,0.0690603617654059,
0.103590542648109,0.138120723530812,0.189915994854866,0.276241447061623,
0.310771627944326,0.414362170592435,0.431627261033787,0.483422532357841,
0.552482894123247,0.621543255888653,0.690603617654059,0.759663979419464,
0.776929069860816,0.794194160302167,0.811459250743519,0.820091795964194,
0.824408068574532,0.826566204879701,0.82872434118487,0.897784702950276,
0.966845064715682),(0.0377143719391271,0.167070624995476,0.336553194126115,
0.499999999999991,0.663446805873868,0.832929375004528,0.962285628058624),
 .UNSPECIFIED.);
#197=B_SPLINE_SURFACE_WITH_KNOTS('',3,3,((#42559,#42560,#42561,#42562,#42563,
#42564,#42565,#42566,#42567,#42568,#42569,#42570,#42571,#42572),(#42573,
#42574,#42575,#42576,#42577,#42578,#42579,#42580,#42581,#42582,#42583,#42584,
#42585,#42586),(#42587,#42588,#42589,#42590,#42591,#42592,#42593,#42594,
#42595,#42596,#42597,#42598,#42599,#42600),(#42601,#42602,#42603,#42604,
#42605,#42606,#42607,#42608,#42609,#42610,#42611,#42612,#42613,#42614),
(#42615,#42616,#42617,#42618,#42619,#42620,#42621,#42622,#42623,#42624,
#42625,#42626,#42627,#42628),(#42629,#42630,#42631,#42632,#42633,#42634,
#42635,#42636,#42637,#42638,#42639,#42640,#42641,#42642),(#42643,#42644,
#42645,#42646,#42647,#42648,#42649,#42650,#42651,#42652,#42653,#42654,#42655,
#42656),(#42657,#42658,#42659,#42660,#42661,#42662,#42663,#42664,#42665,
#42666,#42667,#42668,#42669,#42670),(#42671,#42672,#42673,#42674,#42675,
#42676,#42677,#42678,#42679,#42680,#42681,#42682,#42683,#42684),(#42685,
#42686,#42687,#42688,#42689,#42690,#42691,#42692,#42693,#42694,#42695,#42696,
#42697,#42698),(#42699,#42700,#42701,#42702,#42703,#42704,#42705,#42706,
#42707,#42708,#42709,#42710,#42711,#42712),(#42713,#42714,#42715,#42716,
#42717,#42718,#42719,#42720,#42721,#42722,#42723,#42724,#42725,#42726),
(#42727,#42728,#42729,#42730,#42731,#42732,#42733,#42734,#42735,#42736,
#42737,#42738,#42739,#42740),(#42741,#42742,#42743,#42744,#42745,#42746,
#42747,#42748,#42749,#42750,#42751,#42752,#42753,#42754),(#42755,#42756,
#42757,#42758,#42759,#42760,#42761,#42762,#42763,#42764,#42765,#42766,#42767,
#42768),(#42769,#42770,#42771,#42772,#42773,#42774,#42775,#42776,#42777,
#42778,#42779,#42780,#42781,#42782),(#42783,#42784,#42785,#42786,#42787,
#42788,#42789,#42790,#42791,#42792,#42793,#42794,#42795,#42796),(#42797,
#42798,#42799,#42800,#42801,#42802,#42803,#42804,#42805,#42806,#42807,#42808,
#42809,#42810),(#42811,#42812,#42813,#42814,#42815,#42816,#42817,#42818,
#42819,#42820,#42821,#42822,#42823,#42824),(#42825,#42826,#42827,#42828,
#42829,#42830,#42831,#42832,#42833,#42834,#42835,#42836,#42837,#42838),
(#42839,#42840,#42841,#42842,#42843,#42844,#42845,#42846,#42847,#42848,
#42849,#42850,#42851,#42852),(#42853,#42854,#42855,#42856,#42857,#42858,
#42859,#42860,#42861,#42862,#42863,#42864,#42865,#42866),(#42867,#42868,
#42869,#42870,#42871,#42872,#42873,#42874,#42875,#42876,#42877,#42878,#42879,
#42880),(#42881,#42882,#42883,#42884,#42885,#42886,#42887,#42888,#42889,
#42890,#42891,#42892,#42893,#42894),(#42895,#42896,#42897,#42898,#42899,
#42900,#42901,#42902,#42903,#42904,#42905,#42906,#42907,#42908),(#42909,
#42910,#42911,#42912,#42913,#42914,#42915,#42916,#42917,#42918,#42919,#42920,
#42921,#42922),(#42923,#42924,#42925,#42926,#42927,#42928,#42929,#42930,
#42931,#42932,#42933,#42934,#42935,#42936),(#42937,#42938,#42939,#42940,
#42941,#42942,#42943,#42944,#42945,#42946,#42947,#42948,#42949,#42950),
(#42951,#42952,#42953,#42954,#42955,#42956,#42957,#42958,#42959,#42960,
#42961,#42962,#42963,#42964),(#42965,#42966,#42967,#42968,#42969,#42970,
#42971,#42972,#42973,#42974,#42975,#42976,#42977,#42978)),.UNSPECIFIED.,
 .F.,.F.,.F.,(4,1,1,1,1,1,1,1,1,1,1,1,1,1,1,1,1,1,1,1,1,1,1,1,1,1,1,4),
(4,2,2,2,2,2,4),(0.0331549352864094,0.102215297051666,0.171275658816922,
0.173433795122087,0.175591931427251,0.179908204037579,0.188540749258236,
0.205805839699551,0.223070930140865,0.240336020582179,0.274866201464807,
0.309396382347435,0.378456744112692,0.41298692499532,0.447517105877948,
0.482047286760576,0.516577467643205,0.551107648525833,0.568372738967147,
0.585637829408461,0.689228372056346,0.723758552938974,0.810084005145545,
0.861879276469487,0.896409457352115,0.930939638234743,0.948204728676058,
1.),(0.0377143719413819,0.167070624995476,0.336553194126115,0.499999999999991,
0.663446805873868,0.832929375004528,0.962285628058676),.UNSPECIFIED.);
#198=B_SPLINE_SURFACE_WITH_KNOTS('',3,3,((#43039,#43040,#43041,#43042,#43043,
#43044,#43045,#43046,#43047,#43048,#43049,#43050,#43051,#43052),(#43053,
#43054,#43055,#43056,#43057,#43058,#43059,#43060,#43061,#43062,#43063,#43064,
#43065,#43066),(#43067,#43068,#43069,#43070,#43071,#43072,#43073,#43074,
#43075,#43076,#43077,#43078,#43079,#43080),(#43081,#43082,#43083,#43084,
#43085,#43086,#43087,#43088,#43089,#43090,#43091,#43092,#43093,#43094)),
 .UNSPECIFIED.,.F.,.F.,.F.,(4,4),(4,2,2,2,2,2,4),(0.,1.),(0.0377143719414212,
0.167070624995476,0.336553194126115,0.499999999999991,0.663446805873868,
0.832929375004528,0.962285628058582),.UNSPECIFIED.);
#199=B_SPLINE_SURFACE_WITH_KNOTS('',3,3,((#43109,#43110,#43111,#43112,#43113,
#43114,#43115,#43116,#43117,#43118,#43119,#43120,#43121,#43122),(#43123,
#43124,#43125,#43126,#43127,#43128,#43129,#43130,#43131,#43132,#43133,#43134,
#43135,#43136),(#43137,#43138,#43139,#43140,#43141,#43142,#43143,#43144,
#43145,#43146,#43147,#43148,#43149,#43150),(#43151,#43152,#43153,#43154,
#43155,#43156,#43157,#43158,#43159,#43160,#43161,#43162,#43163,#43164),
(#43165,#43166,#43167,#43168,#43169,#43170,#43171,#43172,#43173,#43174,
#43175,#43176,#43177,#43178),(#43179,#43180,#43181,#43182,#43183,#43184,
#43185,#43186,#43187,#43188,#43189,#43190,#43191,#43192),(#43193,#43194,
#43195,#43196,#43197,#43198,#43199,#43200,#43201,#43202,#43203,#43204,#43205,
#43206),(#43207,#43208,#43209,#43210,#43211,#43212,#43213,#43214,#43215,
#43216,#43217,#43218,#43219,#43220),(#43221,#43222,#43223,#43224,#43225,
#43226,#43227,#43228,#43229,#43230,#43231,#43232,#43233,#43234),(#43235,
#43236,#43237,#43238,#43239,#43240,#43241,#43242,#43243,#43244,#43245,#43246,
#43247,#43248),(#43249,#43250,#43251,#43252,#43253,#43254,#43255,#43256,
#43257,#43258,#43259,#43260,#43261,#43262),(#43263,#43264,#43265,#43266,
#43267,#43268,#43269,#43270,#43271,#43272,#43273,#43274,#43275,#43276),
(#43277,#43278,#43279,#43280,#43281,#43282,#43283,#43284,#43285,#43286,
#43287,#43288,#43289,#43290),(#43291,#43292,#43293,#43294,#43295,#43296,
#43297,#43298,#43299,#43300,#43301,#43302,#43303,#43304),(#43305,#43306,
#43307,#43308,#43309,#43310,#43311,#43312,#43313,#43314,#43315,#43316,#43317,
#43318),(#43319,#43320,#43321,#43322,#43323,#43324,#43325,#43326,#43327,
#43328,#43329,#43330,#43331,#43332),(#43333,#43334,#43335,#43336,#43337,
#43338,#43339,#43340,#43341,#43342,#43343,#43344,#43345,#43346),(#43347,
#43348,#43349,#43350,#43351,#43352,#43353,#43354,#43355,#43356,#43357,#43358,
#43359,#43360),(#43361,#43362,#43363,#43364,#43365,#43366,#43367,#43368,
#43369,#43370,#43371,#43372,#43373,#43374),(#43375,#43376,#43377,#43378,
#43379,#43380,#43381,#43382,#43383,#43384,#43385,#43386,#43387,#43388),
(#43389,#43390,#43391,#43392,#43393,#43394,#43395,#43396,#43397,#43398,
#43399,#43400,#43401,#43402),(#43403,#43404,#43405,#43406,#43407,#43408,
#43409,#43410,#43411,#43412,#43413,#43414,#43415,#43416),(#43417,#43418,
#43419,#43420,#43421,#43422,#43423,#43424,#43425,#43426,#43427,#43428,#43429,
#43430),(#43431,#43432,#43433,#43434,#43435,#43436,#43437,#43438,#43439,
#43440,#43441,#43442,#43443,#43444),(#43445,#43446,#43447,#43448,#43449,
#43450,#43451,#43452,#43453,#43454,#43455,#43456,#43457,#43458),(#43459,
#43460,#43461,#43462,#43463,#43464,#43465,#43466,#43467,#43468,#43469,#43470,
#43471,#43472),(#43473,#43474,#43475,#43476,#43477,#43478,#43479,#43480,
#43481,#43482,#43483,#43484,#43485,#43486),(#43487,#43488,#43489,#43490,
#43491,#43492,#43493,#43494,#43495,#43496,#43497,#43498,#43499,#43500),
(#43501,#43502,#43503,#43504,#43505,#43506,#43507,#43508,#43509,#43510,
#43511,#43512,#43513,#43514),(#43515,#43516,#43517,#43518,#43519,#43520,
#43521,#43522,#43523,#43524,#43525,#43526,#43527,#43528),(#43529,#43530,
#43531,#43532,#43533,#43534,#43535,#43536,#43537,#43538,#43539,#43540,#43541,
#43542)),.UNSPECIFIED.,.F.,.F.,.F.,(4,1,1,1,1,1,1,1,1,1,1,1,1,1,1,1,1,1,
1,1,1,1,1,1,1,1,1,1,4),(4,2,2,2,2,2,4),(0.,0.0517952713240544,0.0690603617654058,
0.103590542648109,0.138120723530812,0.155385813972163,0.189915994854866,
0.276241447061623,0.345301808827029,0.397097080151083,0.414362170592435,
0.448892351475138,0.552482894123247,0.621543255888652,0.690603617654058,
0.725133798536761,0.759663979419464,0.76829652464014,0.776929069860816,
0.794194160302167,0.811459250743518,0.815775523353856,0.820091795964194,
0.824408068574532,0.826566204879701,0.827645273032285,0.82872434118487,
0.897784702950276,0.966845064715681),(0.037714371940714,0.167070624995476,
0.336553194126115,0.499999999999991,0.663446805873868,0.832929375004528,
0.962285628059076),.UNSPECIFIED.);
#200=B_SPLINE_SURFACE_WITH_KNOTS('',3,3,((#43594,#43595,#43596,#43597,#43598,
#43599,#43600,#43601,#43602,#43603,#43604,#43605,#43606,#43607),(#43608,
#43609,#43610,#43611,#43612,#43613,#43614,#43615,#43616,#43617,#43618,#43619,
#43620,#43621),(#43622,#43623,#43624,#43625,#43626,#43627,#43628,#43629,
#43630,#43631,#43632,#43633,#43634,#43635),(#43636,#43637,#43638,#43639,
#43640,#43641,#43642,#43643,#43644,#43645,#43646,#43647,#43648,#43649),
(#43650,#43651,#43652,#43653,#43654,#43655,#43656,#43657,#43658,#43659,
#43660,#43661,#43662,#43663),(#43664,#43665,#43666,#43667,#43668,#43669,
#43670,#43671,#43672,#43673,#43674,#43675,#43676,#43677),(#43678,#43679,
#43680,#43681,#43682,#43683,#43684,#43685,#43686,#43687,#43688,#43689,#43690,
#43691),(#43692,#43693,#43694,#43695,#43696,#43697,#43698,#43699,#43700,
#43701,#43702,#43703,#43704,#43705),(#43706,#43707,#43708,#43709,#43710,
#43711,#43712,#43713,#43714,#43715,#43716,#43717,#43718,#43719),(#43720,
#43721,#43722,#43723,#43724,#43725,#43726,#43727,#43728,#43729,#43730,#43731,
#43732,#43733),(#43734,#43735,#43736,#43737,#43738,#43739,#43740,#43741,
#43742,#43743,#43744,#43745,#43746,#43747),(#43748,#43749,#43750,#43751,
#43752,#43753,#43754,#43755,#43756,#43757,#43758,#43759,#43760,#43761),
(#43762,#43763,#43764,#43765,#43766,#43767,#43768,#43769,#43770,#43771,
#43772,#43773,#43774,#43775),(#43776,#43777,#43778,#43779,#43780,#43781,
#43782,#43783,#43784,#43785,#43786,#43787,#43788,#43789),(#43790,#43791,
#43792,#43793,#43794,#43795,#43796,#43797,#43798,#43799,#43800,#43801,#43802,
#43803),(#43804,#43805,#43806,#43807,#43808,#43809,#43810,#43811,#43812,
#43813,#43814,#43815,#43816,#43817),(#43818,#43819,#43820,#43821,#43822,
#43823,#43824,#43825,#43826,#43827,#43828,#43829,#43830,#43831),(#43832,
#43833,#43834,#43835,#43836,#43837,#43838,#43839,#43840,#43841,#43842,#43843,
#43844,#43845),(#43846,#43847,#43848,#43849,#43850,#43851,#43852,#43853,
#43854,#43855,#43856,#43857,#43858,#43859),(#43860,#43861,#43862,#43863,
#43864,#43865,#43866,#43867,#43868,#43869,#43870,#43871,#43872,#43873),
(#43874,#43875,#43876,#43877,#43878,#43879,#43880,#43881,#43882,#43883,
#43884,#43885,#43886,#43887),(#43888,#43889,#43890,#43891,#43892,#43893,
#43894,#43895,#43896,#43897,#43898,#43899,#43900,#43901),(#43902,#43903,
#43904,#43905,#43906,#43907,#43908,#43909,#43910,#43911,#43912,#43913,#43914,
#43915),(#43916,#43917,#43918,#43919,#43920,#43921,#43922,#43923,#43924,
#43925,#43926,#43927,#43928,#43929),(#43930,#43931,#43932,#43933,#43934,
#43935,#43936,#43937,#43938,#43939,#43940,#43941,#43942,#43943),(#43944,
#43945,#43946,#43947,#43948,#43949,#43950,#43951,#43952,#43953,#43954,#43955,
#43956,#43957),(#43958,#43959,#43960,#43961,#43962,#43963,#43964,#43965,
#43966,#43967,#43968,#43969,#43970,#43971),(#43972,#43973,#43974,#43975,
#43976,#43977,#43978,#43979,#43980,#43981,#43982,#43983,#43984,#43985),
(#43986,#43987,#43988,#43989,#43990,#43991,#43992,#43993,#43994,#43995,
#43996,#43997,#43998,#43999),(#44000,#44001,#44002,#44003,#44004,#44005,
#44006,#44007,#44008,#44009,#44010,#44011,#44012,#44013),(#44014,#44015,
#44016,#44017,#44018,#44019,#44020,#44021,#44022,#44023,#44024,#44025,#44026,
#44027)),.UNSPECIFIED.,.F.,.F.,.F.,(4,1,1,1,1,1,1,1,1,1,1,1,1,1,1,1,1,1,
1,1,1,1,1,1,1,1,1,1,4),(4,2,2,2,2,2,4),(0.0331549352864062,0.102215297051663,
0.136745477934291,0.17127565881692,0.173433795122084,0.175591931427248,
0.179908204037577,0.188540749258234,0.197173294478891,0.205805839699548,
0.223070930140862,0.240336020582176,0.274866201464805,0.309396382347433,
0.37845674411269,0.412986924995318,0.430252015436632,0.447517105877946,
0.516577467643203,0.58563782940846,0.654698191173716,0.689228372056345,
0.723758552938973,0.827349095586858,0.861879276469486,0.896409457352115,
0.930939638234743,0.948204728676057,1.),(0.0377143719407421,0.167070624995476,
0.336553194126115,0.499999999999991,0.663446805873868,0.832929375004528,
0.962285628059324),.UNSPECIFIED.);
#201=B_SPLINE_SURFACE_WITH_KNOTS('',3,3,((#44088,#44089,#44090,#44091,#44092,
#44093,#44094,#44095,#44096,#44097,#44098,#44099,#44100,#44101),(#44102,
#44103,#44104,#44105,#44106,#44107,#44108,#44109,#44110,#44111,#44112,#44113,
#44114,#44115),(#44116,#44117,#44118,#44119,#44120,#44121,#44122,#44123,
#44124,#44125,#44126,#44127,#44128,#44129),(#44130,#44131,#44132,#44133,
#44134,#44135,#44136,#44137,#44138,#44139,#44140,#44141,#44142,#44143)),
 .UNSPECIFIED.,.F.,.F.,.F.,(4,4),(4,2,2,2,2,2,4),(0.,1.),(0.0377143719414212,
0.167070624995476,0.336553194126115,0.499999999999991,0.663446805873868,
0.832929375004528,0.962285628058582),.UNSPECIFIED.);
#202=B_SPLINE_SURFACE_WITH_KNOTS('',3,3,((#44158,#44159,#44160,#44161,#44162,
#44163,#44164,#44165,#44166,#44167,#44168,#44169,#44170,#44171),(#44172,
#44173,#44174,#44175,#44176,#44177,#44178,#44179,#44180,#44181,#44182,#44183,
#44184,#44185),(#44186,#44187,#44188,#44189,#44190,#44191,#44192,#44193,
#44194,#44195,#44196,#44197,#44198,#44199),(#44200,#44201,#44202,#44203,
#44204,#44205,#44206,#44207,#44208,#44209,#44210,#44211,#44212,#44213),
(#44214,#44215,#44216,#44217,#44218,#44219,#44220,#44221,#44222,#44223,
#44224,#44225,#44226,#44227),(#44228,#44229,#44230,#44231,#44232,#44233,
#44234,#44235,#44236,#44237,#44238,#44239,#44240,#44241),(#44242,#44243,
#44244,#44245,#44246,#44247,#44248,#44249,#44250,#44251,#44252,#44253,#44254,
#44255),(#44256,#44257,#44258,#44259,#44260,#44261,#44262,#44263,#44264,
#44265,#44266,#44267,#44268,#44269),(#44270,#44271,#44272,#44273,#44274,
#44275,#44276,#44277,#44278,#44279,#44280,#44281,#44282,#44283),(#44284,
#44285,#44286,#44287,#44288,#44289,#44290,#44291,#44292,#44293,#44294,#44295,
#44296,#44297),(#44298,#44299,#44300,#44301,#44302,#44303,#44304,#44305,
#44306,#44307,#44308,#44309,#44310,#44311),(#44312,#44313,#44314,#44315,
#44316,#44317,#44318,#44319,#44320,#44321,#44322,#44323,#44324,#44325),
(#44326,#44327,#44328,#44329,#44330,#44331,#44332,#44333,#44334,#44335,
#44336,#44337,#44338,#44339),(#44340,#44341,#44342,#44343,#44344,#44345,
#44346,#44347,#44348,#44349,#44350,#44351,#44352,#44353),(#44354,#44355,
#44356,#44357,#44358,#44359,#44360,#44361,#44362,#44363,#44364,#44365,#44366,
#44367),(#44368,#44369,#44370,#44371,#44372,#44373,#44374,#44375,#44376,
#44377,#44378,#44379,#44380,#44381),(#44382,#44383,#44384,#44385,#44386,
#44387,#44388,#44389,#44390,#44391,#44392,#44393,#44394,#44395),(#44396,
#44397,#44398,#44399,#44400,#44401,#44402,#44403,#44404,#44405,#44406,#44407,
#44408,#44409),(#44410,#44411,#44412,#44413,#44414,#44415,#44416,#44417,
#44418,#44419,#44420,#44421,#44422,#44423),(#44424,#44425,#44426,#44427,
#44428,#44429,#44430,#44431,#44432,#44433,#44434,#44435,#44436,#44437),
(#44438,#44439,#44440,#44441,#44442,#44443,#44444,#44445,#44446,#44447,
#44448,#44449,#44450,#44451),(#44452,#44453,#44454,#44455,#44456,#44457,
#44458,#44459,#44460,#44461,#44462,#44463,#44464,#44465),(#44466,#44467,
#44468,#44469,#44470,#44471,#44472,#44473,#44474,#44475,#44476,#44477,#44478,
#44479),(#44480,#44481,#44482,#44483,#44484,#44485,#44486,#44487,#44488,
#44489,#44490,#44491,#44492,#44493),(#44494,#44495,#44496,#44497,#44498,
#44499,#44500,#44501,#44502,#44503,#44504,#44505,#44506,#44507),(#44508,
#44509,#44510,#44511,#44512,#44513,#44514,#44515,#44516,#44517,#44518,#44519,
#44520,#44521),(#44522,#44523,#44524,#44525,#44526,#44527,#44528,#44529,
#44530,#44531,#44532,#44533,#44534,#44535),(#44536,#44537,#44538,#44539,
#44540,#44541,#44542,#44543,#44544,#44545,#44546,#44547,#44548,#44549),
(#44550,#44551,#44552,#44553,#44554,#44555,#44556,#44557,#44558,#44559,
#44560,#44561,#44562,#44563),(#44564,#44565,#44566,#44567,#44568,#44569,
#44570,#44571,#44572,#44573,#44574,#44575,#44576,#44577),(#44578,#44579,
#44580,#44581,#44582,#44583,#44584,#44585,#44586,#44587,#44588,#44589,#44590,
#44591),(#44592,#44593,#44594,#44595,#44596,#44597,#44598,#44599,#44600,
#44601,#44602,#44603,#44604,#44605),(#44606,#44607,#44608,#44609,#44610,
#44611,#44612,#44613,#44614,#44615,#44616,#44617,#44618,#44619),(#44620,
#44621,#44622,#44623,#44624,#44625,#44626,#44627,#44628,#44629,#44630,#44631,
#44632,#44633),(#44634,#44635,#44636,#44637,#44638,#44639,#44640,#44641,
#44642,#44643,#44644,#44645,#44646,#44647)),.UNSPECIFIED.,.F.,.F.,.F.,(4,
1,1,1,1,1,1,1,1,1,1,1,1,1,1,1,1,1,1,1,1,1,1,1,1,1,1,1,1,1,1,1,4),(4,2,2,
2,2,2,4),(0.,0.0517952713240545,0.069060361765406,0.0863254522067576,0.103590542648109,
0.138120723530812,0.155385813972164,0.189915994854867,0.207181085296218,
0.276241447061624,0.34530180882703,0.379831989709733,0.414362170592436,
0.448892351475139,0.483422532357842,0.517952713240545,0.552482894123248,
0.587013075005951,0.656073436771357,0.69060361765406,0.725133798536763,
0.759663979419467,0.785561615081494,0.79419416030217,0.811459250743521,
0.815775523353859,0.820091795964197,0.824408068574535,0.828724341184873,
0.880519612508927,0.897784702950279,0.932314883832982,0.966845064715685),
(0.0377143719406521,0.167070624995476,0.336553194126115,0.499999999999991,
0.663446805873868,0.832929375004528,0.962285628059093),.UNSPECIFIED.);
#203=B_SPLINE_SURFACE_WITH_KNOTS('',3,3,((#44699,#44700,#44701,#44702,#44703,
#44704,#44705,#44706,#44707,#44708,#44709,#44710,#44711,#44712),(#44713,
#44714,#44715,#44716,#44717,#44718,#44719,#44720,#44721,#44722,#44723,#44724,
#44725,#44726),(#44727,#44728,#44729,#44730,#44731,#44732,#44733,#44734,
#44735,#44736,#44737,#44738,#44739,#44740),(#44741,#44742,#44743,#44744,
#44745,#44746,#44747,#44748,#44749,#44750,#44751,#44752,#44753,#44754),
(#44755,#44756,#44757,#44758,#44759,#44760,#44761,#44762,#44763,#44764,
#44765,#44766,#44767,#44768),(#44769,#44770,#44771,#44772,#44773,#44774,
#44775,#44776,#44777,#44778,#44779,#44780,#44781,#44782),(#44783,#44784,
#44785,#44786,#44787,#44788,#44789,#44790,#44791,#44792,#44793,#44794,#44795,
#44796),(#44797,#44798,#44799,#44800,#44801,#44802,#44803,#44804,#44805,
#44806,#44807,#44808,#44809,#44810),(#44811,#44812,#44813,#44814,#44815,
#44816,#44817,#44818,#44819,#44820,#44821,#44822,#44823,#44824),(#44825,
#44826,#44827,#44828,#44829,#44830,#44831,#44832,#44833,#44834,#44835,#44836,
#44837,#44838),(#44839,#44840,#44841,#44842,#44843,#44844,#44845,#44846,
#44847,#44848,#44849,#44850,#44851,#44852),(#44853,#44854,#44855,#44856,
#44857,#44858,#44859,#44860,#44861,#44862,#44863,#44864,#44865,#44866),
(#44867,#44868,#44869,#44870,#44871,#44872,#44873,#44874,#44875,#44876,
#44877,#44878,#44879,#44880),(#44881,#44882,#44883,#44884,#44885,#44886,
#44887,#44888,#44889,#44890,#44891,#44892,#44893,#44894),(#44895,#44896,
#44897,#44898,#44899,#44900,#44901,#44902,#44903,#44904,#44905,#44906,#44907,
#44908),(#44909,#44910,#44911,#44912,#44913,#44914,#44915,#44916,#44917,
#44918,#44919,#44920,#44921,#44922),(#44923,#44924,#44925,#44926,#44927,
#44928,#44929,#44930,#44931,#44932,#44933,#44934,#44935,#44936),(#44937,
#44938,#44939,#44940,#44941,#44942,#44943,#44944,#44945,#44946,#44947,#44948,
#44949,#44950),(#44951,#44952,#44953,#44954,#44955,#44956,#44957,#44958,
#44959,#44960,#44961,#44962,#44963,#44964),(#44965,#44966,#44967,#44968,
#44969,#44970,#44971,#44972,#44973,#44974,#44975,#44976,#44977,#44978),
(#44979,#44980,#44981,#44982,#44983,#44984,#44985,#44986,#44987,#44988,
#44989,#44990,#44991,#44992),(#44993,#44994,#44995,#44996,#44997,#44998,
#44999,#45000,#45001,#45002,#45003,#45004,#45005,#45006),(#45007,#45008,
#45009,#45010,#45011,#45012,#45013,#45014,#45015,#45016,#45017,#45018,#45019,
#45020),(#45021,#45022,#45023,#45024,#45025,#45026,#45027,#45028,#45029,
#45030,#45031,#45032,#45033,#45034),(#45035,#45036,#45037,#45038,#45039,
#45040,#45041,#45042,#45043,#45044,#45045,#45046,#45047,#45048),(#45049,
#45050,#45051,#45052,#45053,#45054,#45055,#45056,#45057,#45058,#45059,#45060,
#45061,#45062),(#45063,#45064,#45065,#45066,#45067,#45068,#45069,#45070,
#45071,#45072,#45073,#45074,#45075,#45076),(#45077,#45078,#45079,#45080,
#45081,#45082,#45083,#45084,#45085,#45086,#45087,#45088,#45089,#45090)),
 .UNSPECIFIED.,.F.,.F.,.F.,(4,1,1,1,1,1,1,1,1,1,1,1,1,1,1,1,1,1,1,1,1,1,
1,1,1,4),(4,2,2,2,2,2,4),(0.0331549352864051,0.102215297051662,0.171275658816919,
0.175591931427247,0.179908204037576,0.188540749258233,0.205805839699547,
0.223070930140861,0.240336020582175,0.274866201464804,0.309396382347432,
0.378456744112689,0.412986924995317,0.430252015436631,0.447517105877946,
0.516577467643203,0.585637829408459,0.654698191173716,0.689228372056344,
0.723758552938973,0.827349095586858,0.861879276469486,0.896409457352115,
0.930939638234743,0.948204728676057,1.),(0.0377143719409181,0.167070624995476,
0.336553194126115,0.499999999999991,0.663446805873868,0.832929375004528,
0.962285628059611),.UNSPECIFIED.);
#204=B_SPLINE_SURFACE_WITH_KNOTS('',3,3,((#45149,#45150,#45151,#45152,#45153,
#45154,#45155,#45156,#45157,#45158,#45159,#45160,#45161,#45162),(#45163,
#45164,#45165,#45166,#45167,#45168,#45169,#45170,#45171,#45172,#45173,#45174,
#45175,#45176),(#45177,#45178,#45179,#45180,#45181,#45182,#45183,#45184,
#45185,#45186,#45187,#45188,#45189,#45190),(#45191,#45192,#45193,#45194,
#45195,#45196,#45197,#45198,#45199,#45200,#45201,#45202,#45203,#45204)),
 .UNSPECIFIED.,.F.,.F.,.F.,(4,4),(4,2,2,2,2,2,4),(0.,1.),(0.0377143719414212,
0.167070624995476,0.336553194126115,0.499999999999991,0.663446805873868,
0.832929375004528,0.962285628058582),.UNSPECIFIED.);
#205=B_SPLINE_SURFACE_WITH_KNOTS('',3,3,((#45219,#45220,#45221,#45222,#45223,
#45224,#45225,#45226,#45227,#45228,#45229,#45230,#45231,#45232),(#45233,
#45234,#45235,#45236,#45237,#45238,#45239,#45240,#45241,#45242,#45243,#45244,
#45245,#45246),(#45247,#45248,#45249,#45250,#45251,#45252,#45253,#45254,
#45255,#45256,#45257,#45258,#45259,#45260),(#45261,#45262,#45263,#45264,
#45265,#45266,#45267,#45268,#45269,#45270,#45271,#45272,#45273,#45274),
(#45275,#45276,#45277,#45278,#45279,#45280,#45281,#45282,#45283,#45284,
#45285,#45286,#45287,#45288),(#45289,#45290,#45291,#45292,#45293,#45294,
#45295,#45296,#45297,#45298,#45299,#45300,#45301,#45302),(#45303,#45304,
#45305,#45306,#45307,#45308,#45309,#45310,#45311,#45312,#45313,#45314,#45315,
#45316),(#45317,#45318,#45319,#45320,#45321,#45322,#45323,#45324,#45325,
#45326,#45327,#45328,#45329,#45330),(#45331,#45332,#45333,#45334,#45335,
#45336,#45337,#45338,#45339,#45340,#45341,#45342,#45343,#45344),(#45345,
#45346,#45347,#45348,#45349,#45350,#45351,#45352,#45353,#45354,#45355,#45356,
#45357,#45358),(#45359,#45360,#45361,#45362,#45363,#45364,#45365,#45366,
#45367,#45368,#45369,#45370,#45371,#45372),(#45373,#45374,#45375,#45376,
#45377,#45378,#45379,#45380,#45381,#45382,#45383,#45384,#45385,#45386),
(#45387,#45388,#45389,#45390,#45391,#45392,#45393,#45394,#45395,#45396,
#45397,#45398,#45399,#45400),(#45401,#45402,#45403,#45404,#45405,#45406,
#45407,#45408,#45409,#45410,#45411,#45412,#45413,#45414),(#45415,#45416,
#45417,#45418,#45419,#45420,#45421,#45422,#45423,#45424,#45425,#45426,#45427,
#45428),(#45429,#45430,#45431,#45432,#45433,#45434,#45435,#45436,#45437,
#45438,#45439,#45440,#45441,#45442),(#45443,#45444,#45445,#45446,#45447,
#45448,#45449,#45450,#45451,#45452,#45453,#45454,#45455,#45456),(#45457,
#45458,#45459,#45460,#45461,#45462,#45463,#45464,#45465,#45466,#45467,#45468,
#45469,#45470),(#45471,#45472,#45473,#45474,#45475,#45476,#45477,#45478,
#45479,#45480,#45481,#45482,#45483,#45484),(#45485,#45486,#45487,#45488,
#45489,#45490,#45491,#45492,#45493,#45494,#45495,#45496,#45497,#45498),
(#45499,#45500,#45501,#45502,#45503,#45504,#45505,#45506,#45507,#45508,
#45509,#45510,#45511,#45512),(#45513,#45514,#45515,#45516,#45517,#45518,
#45519,#45520,#45521,#45522,#45523,#45524,#45525,#45526),(#45527,#45528,
#45529,#45530,#45531,#45532,#45533,#45534,#45535,#45536,#45537,#45538,#45539,
#45540),(#45541,#45542,#45543,#45544,#45545,#45546,#45547,#45548,#45549,
#45550,#45551,#45552,#45553,#45554),(#45555,#45556,#45557,#45558,#45559,
#45560,#45561,#45562,#45563,#45564,#45565,#45566,#45567,#45568),(#45569,
#45570,#45571,#45572,#45573,#45574,#45575,#45576,#45577,#45578,#45579,#45580,
#45581,#45582)),.UNSPECIFIED.,.F.,.F.,.F.,(4,1,1,1,1,1,1,1,1,1,1,1,1,1,
1,1,1,1,1,1,1,1,1,4),(4,2,2,2,2,2,4),(0.,0.0517952713240545,0.0690603617654061,
0.103590542648109,0.138120723530812,0.155385813972164,0.276241447061624,
0.310771627944327,0.34530180882703,0.414362170592436,0.483422532357842,
0.535217803681897,0.552482894123248,0.621543255888655,0.656073436771358,
0.690603617654061,0.725133798536764,0.759663979419467,0.79419416030217,
0.811459250743521,0.820091795964197,0.828724341184873,0.897784702950279,
0.966845064715685),(0.037714371941385,0.167070624995476,0.336553194126115,
0.499999999999991,0.663446805873868,0.832929375004528,0.962285628060415),
 .UNSPECIFIED.);
#206=B_SPLINE_SURFACE_WITH_KNOTS('',3,3,((#45642,#45643,#45644,#45645,#45646,
#45647,#45648,#45649,#45650,#45651,#45652,#45653,#45654,#45655),(#45656,
#45657,#45658,#45659,#45660,#45661,#45662,#45663,#45664,#45665,#45666,#45667,
#45668,#45669),(#45670,#45671,#45672,#45673,#45674,#45675,#45676,#45677,
#45678,#45679,#45680,#45681,#45682,#45683),(#45684,#45685,#45686,#45687,
#45688,#45689,#45690,#45691,#45692,#45693,#45694,#45695,#45696,#45697),
(#45698,#45699,#45700,#45701,#45702,#45703,#45704,#45705,#45706,#45707,
#45708,#45709,#45710,#45711),(#45712,#45713,#45714,#45715,#45716,#45717,
#45718,#45719,#45720,#45721,#45722,#45723,#45724,#45725),(#45726,#45727,
#45728,#45729,#45730,#45731,#45732,#45733,#45734,#45735,#45736,#45737,#45738,
#45739),(#45740,#45741,#45742,#45743,#45744,#45745,#45746,#45747,#45748,
#45749,#45750,#45751,#45752,#45753),(#45754,#45755,#45756,#45757,#45758,
#45759,#45760,#45761,#45762,#45763,#45764,#45765,#45766,#45767),(#45768,
#45769,#45770,#45771,#45772,#45773,#45774,#45775,#45776,#45777,#45778,#45779,
#45780,#45781),(#45782,#45783,#45784,#45785,#45786,#45787,#45788,#45789,
#45790,#45791,#45792,#45793,#45794,#45795),(#45796,#45797,#45798,#45799,
#45800,#45801,#45802,#45803,#45804,#45805,#45806,#45807,#45808,#45809),
(#45810,#45811,#45812,#45813,#45814,#45815,#45816,#45817,#45818,#45819,
#45820,#45821,#45822,#45823),(#45824,#45825,#45826,#45827,#45828,#45829,
#45830,#45831,#45832,#45833,#45834,#45835,#45836,#45837),(#45838,#45839,
#45840,#45841,#45842,#45843,#45844,#45845,#45846,#45847,#45848,#45849,#45850,
#45851),(#45852,#45853,#45854,#45855,#45856,#45857,#45858,#45859,#45860,
#45861,#45862,#45863,#45864,#45865),(#45866,#45867,#45868,#45869,#45870,
#45871,#45872,#45873,#45874,#45875,#45876,#45877,#45878,#45879),(#45880,
#45881,#45882,#45883,#45884,#45885,#45886,#45887,#45888,#45889,#45890,#45891,
#45892,#45893),(#45894,#45895,#45896,#45897,#45898,#45899,#45900,#45901,
#45902,#45903,#45904,#45905,#45906,#45907),(#45908,#45909,#45910,#45911,
#45912,#45913,#45914,#45915,#45916,#45917,#45918,#45919,#45920,#45921),
(#45922,#45923,#45924,#45925,#45926,#45927,#45928,#45929,#45930,#45931,
#45932,#45933,#45934,#45935),(#45936,#45937,#45938,#45939,#45940,#45941,
#45942,#45943,#45944,#45945,#45946,#45947,#45948,#45949),(#45950,#45951,
#45952,#45953,#45954,#45955,#45956,#45957,#45958,#45959,#45960,#45961,#45962,
#45963),(#45964,#45965,#45966,#45967,#45968,#45969,#45970,#45971,#45972,
#45973,#45974,#45975,#45976,#45977),(#45978,#45979,#45980,#45981,#45982,
#45983,#45984,#45985,#45986,#45987,#45988,#45989,#45990,#45991),(#45992,
#45993,#45994,#45995,#45996,#45997,#45998,#45999,#46000,#46001,#46002,#46003,
#46004,#46005)),.UNSPECIFIED.,.F.,.F.,.F.,(4,1,1,1,1,1,1,1,1,1,1,1,1,1,
1,1,1,1,1,1,1,1,1,4),(4,2,2,2,2,2,4),(0.0331549352864075,0.102215297051664,
0.171275658816921,0.175591931427249,0.179908204037578,0.188540749258235,
0.205805839699549,0.223070930140863,0.240336020582177,0.309396382347434,
0.37845674411269,0.412986924995319,0.430252015436633,0.447517105877947,
0.58563782940846,0.620168010291089,0.671963281615031,0.723758552938974,
0.810084005145544,0.861879276469487,0.896409457352115,0.930939638234743,
0.948204728676058,1.),(0.0377143719412197,0.167070624995476,0.336553194126115,
0.499999999999991,0.663446805873868,0.832929375004528,0.962285628058676),
 .UNSPECIFIED.);
#207=B_SPLINE_SURFACE_WITH_KNOTS('',3,3,((#46064,#46065,#46066,#46067,#46068,
#46069,#46070,#46071,#46072,#46073,#46074,#46075,#46076,#46077),(#46078,
#46079,#46080,#46081,#46082,#46083,#46084,#46085,#46086,#46087,#46088,#46089,
#46090,#46091),(#46092,#46093,#46094,#46095,#46096,#46097,#46098,#46099,
#46100,#46101,#46102,#46103,#46104,#46105),(#46106,#46107,#46108,#46109,
#46110,#46111,#46112,#46113,#46114,#46115,#46116,#46117,#46118,#46119)),
 .UNSPECIFIED.,.F.,.F.,.F.,(4,4),(4,2,2,2,2,2,4),(0.,1.),(0.0377143719414212,
0.167070624995476,0.336553194126115,0.499999999999991,0.663446805873868,
0.832929375004528,0.962285628058582),.UNSPECIFIED.);
#208=B_SPLINE_SURFACE_WITH_KNOTS('',3,3,((#46134,#46135,#46136,#46137,#46138,
#46139,#46140,#46141,#46142,#46143,#46144,#46145,#46146,#46147),(#46148,
#46149,#46150,#46151,#46152,#46153,#46154,#46155,#46156,#46157,#46158,#46159,
#46160,#46161),(#46162,#46163,#46164,#46165,#46166,#46167,#46168,#46169,
#46170,#46171,#46172,#46173,#46174,#46175),(#46176,#46177,#46178,#46179,
#46180,#46181,#46182,#46183,#46184,#46185,#46186,#46187,#46188,#46189),
(#46190,#46191,#46192,#46193,#46194,#46195,#46196,#46197,#46198,#46199,
#46200,#46201,#46202,#46203),(#46204,#46205,#46206,#46207,#46208,#46209,
#46210,#46211,#46212,#46213,#46214,#46215,#46216,#46217),(#46218,#46219,
#46220,#46221,#46222,#46223,#46224,#46225,#46226,#46227,#46228,#46229,#46230,
#46231),(#46232,#46233,#46234,#46235,#46236,#46237,#46238,#46239,#46240,
#46241,#46242,#46243,#46244,#46245),(#46246,#46247,#46248,#46249,#46250,
#46251,#46252,#46253,#46254,#46255,#46256,#46257,#46258,#46259),(#46260,
#46261,#46262,#46263,#46264,#46265,#46266,#46267,#46268,#46269,#46270,#46271,
#46272,#46273),(#46274,#46275,#46276,#46277,#46278,#46279,#46280,#46281,
#46282,#46283,#46284,#46285,#46286,#46287),(#46288,#46289,#46290,#46291,
#46292,#46293,#46294,#46295,#46296,#46297,#46298,#46299,#46300,#46301),
(#46302,#46303,#46304,#46305,#46306,#46307,#46308,#46309,#46310,#46311,
#46312,#46313,#46314,#46315),(#46316,#46317,#46318,#46319,#46320,#46321,
#46322,#46323,#46324,#46325,#46326,#46327,#46328,#46329),(#46330,#46331,
#46332,#46333,#46334,#46335,#46336,#46337,#46338,#46339,#46340,#46341,#46342,
#46343),(#46344,#46345,#46346,#46347,#46348,#46349,#46350,#46351,#46352,
#46353,#46354,#46355,#46356,#46357),(#46358,#46359,#46360,#46361,#46362,
#46363,#46364,#46365,#46366,#46367,#46368,#46369,#46370,#46371),(#46372,
#46373,#46374,#46375,#46376,#46377,#46378,#46379,#46380,#46381,#46382,#46383,
#46384,#46385),(#46386,#46387,#46388,#46389,#46390,#46391,#46392,#46393,
#46394,#46395,#46396,#46397,#46398,#46399),(#46400,#46401,#46402,#46403,
#46404,#46405,#46406,#46407,#46408,#46409,#46410,#46411,#46412,#46413),
(#46414,#46415,#46416,#46417,#46418,#46419,#46420,#46421,#46422,#46423,
#46424,#46425,#46426,#46427),(#46428,#46429,#46430,#46431,#46432,#46433,
#46434,#46435,#46436,#46437,#46438,#46439,#46440,#46441),(#46442,#46443,
#46444,#46445,#46446,#46447,#46448,#46449,#46450,#46451,#46452,#46453,#46454,
#46455),(#46456,#46457,#46458,#46459,#46460,#46461,#46462,#46463,#46464,
#46465,#46466,#46467,#46468,#46469),(#46470,#46471,#46472,#46473,#46474,
#46475,#46476,#46477,#46478,#46479,#46480,#46481,#46482,#46483),(#46484,
#46485,#46486,#46487,#46488,#46489,#46490,#46491,#46492,#46493,#46494,#46495,
#46496,#46497),(#46498,#46499,#46500,#46501,#46502,#46503,#46504,#46505,
#46506,#46507,#46508,#46509,#46510,#46511)),.UNSPECIFIED.,.F.,.F.,.F.,(4,
1,1,1,1,1,1,1,1,1,1,1,1,1,1,1,1,1,1,1,1,1,1,1,4),(4,2,2,2,2,2,4),(0.,0.0517952713240545,
0.0690603617654059,0.103590542648109,0.138120723530812,0.155385813972163,
0.189915994854866,0.276241447061624,0.34530180882703,0.379831989709733,
0.414362170592436,0.448892351475139,0.552482894123247,0.621543255888653,
0.690603617654059,0.759663979419465,0.768296524640141,0.776929069860817,
0.794194160302168,0.81145925074352,0.820091795964196,0.828724341184871,
0.897784702950277,0.93231488383298,0.966845064715683),(0.0377143719404219,
0.167070624995476,0.336553194126115,0.499999999999991,0.663446805873868,
0.832929375004528,0.962285628059789),.UNSPECIFIED.);
#209=B_SPLINE_SURFACE_WITH_KNOTS('',3,3,((#46567,#46568,#46569,#46570,#46571,
#46572,#46573,#46574,#46575,#46576,#46577,#46578,#46579,#46580),(#46581,
#46582,#46583,#46584,#46585,#46586,#46587,#46588,#46589,#46590,#46591,#46592,
#46593,#46594),(#46595,#46596,#46597,#46598,#46599,#46600,#46601,#46602,
#46603,#46604,#46605,#46606,#46607,#46608),(#46609,#46610,#46611,#46612,
#46613,#46614,#46615,#46616,#46617,#46618,#46619,#46620,#46621,#46622),
(#46623,#46624,#46625,#46626,#46627,#46628,#46629,#46630,#46631,#46632,
#46633,#46634,#46635,#46636),(#46637,#46638,#46639,#46640,#46641,#46642,
#46643,#46644,#46645,#46646,#46647,#46648,#46649,#46650),(#46651,#46652,
#46653,#46654,#46655,#46656,#46657,#46658,#46659,#46660,#46661,#46662,#46663,
#46664),(#46665,#46666,#46667,#46668,#46669,#46670,#46671,#46672,#46673,
#46674,#46675,#46676,#46677,#46678),(#46679,#46680,#46681,#46682,#46683,
#46684,#46685,#46686,#46687,#46688,#46689,#46690,#46691,#46692),(#46693,
#46694,#46695,#46696,#46697,#46698,#46699,#46700,#46701,#46702,#46703,#46704,
#46705,#46706),(#46707,#46708,#46709,#46710,#46711,#46712,#46713,#46714,
#46715,#46716,#46717,#46718,#46719,#46720),(#46721,#46722,#46723,#46724,
#46725,#46726,#46727,#46728,#46729,#46730,#46731,#46732,#46733,#46734),
(#46735,#46736,#46737,#46738,#46739,#46740,#46741,#46742,#46743,#46744,
#46745,#46746,#46747,#46748),(#46749,#46750,#46751,#46752,#46753,#46754,
#46755,#46756,#46757,#46758,#46759,#46760,#46761,#46762),(#46763,#46764,
#46765,#46766,#46767,#46768,#46769,#46770,#46771,#46772,#46773,#46774,#46775,
#46776),(#46777,#46778,#46779,#46780,#46781,#46782,#46783,#46784,#46785,
#46786,#46787,#46788,#46789,#46790),(#46791,#46792,#46793,#46794,#46795,
#46796,#46797,#46798,#46799,#46800,#46801,#46802,#46803,#46804),(#46805,
#46806,#46807,#46808,#46809,#46810,#46811,#46812,#46813,#46814,#46815,#46816,
#46817,#46818),(#46819,#46820,#46821,#46822,#46823,#46824,#46825,#46826,
#46827,#46828,#46829,#46830,#46831,#46832),(#46833,#46834,#46835,#46836,
#46837,#46838,#46839,#46840,#46841,#46842,#46843,#46844,#46845,#46846),
(#46847,#46848,#46849,#46850,#46851,#46852,#46853,#46854,#46855,#46856,
#46857,#46858,#46859,#46860),(#46861,#46862,#46863,#46864,#46865,#46866,
#46867,#46868,#46869,#46870,#46871,#46872,#46873,#46874),(#46875,#46876,
#46877,#46878,#46879,#46880,#46881,#46882,#46883,#46884,#46885,#46886,#46887,
#46888),(#46889,#46890,#46891,#46892,#46893,#46894,#46895,#46896,#46897,
#46898,#46899,#46900,#46901,#46902),(#46903,#46904,#46905,#46906,#46907,
#46908,#46909,#46910,#46911,#46912,#46913,#46914,#46915,#46916),(#46917,
#46918,#46919,#46920,#46921,#46922,#46923,#46924,#46925,#46926,#46927,#46928,
#46929,#46930),(#46931,#46932,#46933,#46934,#46935,#46936,#46937,#46938,
#46939,#46940,#46941,#46942,#46943,#46944),(#46945,#46946,#46947,#46948,
#46949,#46950,#46951,#46952,#46953,#46954,#46955,#46956,#46957,#46958),
(#46959,#46960,#46961,#46962,#46963,#46964,#46965,#46966,#46967,#46968,
#46969,#46970,#46971,#46972),(#46973,#46974,#46975,#46976,#46977,#46978,
#46979,#46980,#46981,#46982,#46983,#46984,#46985,#46986),(#46987,#46988,
#46989,#46990,#46991,#46992,#46993,#46994,#46995,#46996,#46997,#46998,#46999,
#47000)),.UNSPECIFIED.,.F.,.F.,.F.,(4,1,1,1,1,1,1,1,1,1,1,1,1,1,1,1,1,1,
1,1,1,1,1,1,1,1,1,1,4),(4,2,2,2,2,2,4),(0.0331549352864085,0.0676851161690368,
0.102215297051665,0.119480387492979,0.171275658816922,0.179908204037579,
0.188540749258236,0.197173294478893,0.20580583969955,0.240336020582178,
0.274866201464806,0.309396382347435,0.378456744112691,0.412986924995319,
0.447517105877948,0.482047286760576,0.551107648525832,0.585637829408461,
0.620168010291089,0.654698191173717,0.723758552938974,0.810084005145544,
0.827349095586859,0.844614186028173,0.861879276469487,0.896409457352115,
0.930939638234743,0.948204728676058,1.),(0.0377143719401151,0.167070624995476,
0.336553194126115,0.499999999999991,0.663446805873868,0.832929375004528,
0.962285628058773),.UNSPECIFIED.);
#210=B_SPLINE_SURFACE_WITH_KNOTS('',3,3,((#47059,#47060,#47061,#47062,#47063,
#47064,#47065,#47066,#47067,#47068,#47069,#47070,#47071,#47072),(#47073,
#47074,#47075,#47076,#47077,#47078,#47079,#47080,#47081,#47082,#47083,#47084,
#47085,#47086),(#47087,#47088,#47089,#47090,#47091,#47092,#47093,#47094,
#47095,#47096,#47097,#47098,#47099,#47100),(#47101,#47102,#47103,#47104,
#47105,#47106,#47107,#47108,#47109,#47110,#47111,#47112,#47113,#47114)),
 .UNSPECIFIED.,.F.,.F.,.F.,(4,4),(4,2,2,2,2,2,4),(0.,1.),(0.0377143719414212,
0.167070624995476,0.336553194126115,0.499999999999991,0.663446805873868,
0.832929375004528,0.962285628058582),.UNSPECIFIED.);
#211=B_SPLINE_SURFACE_WITH_KNOTS('',3,3,((#47129,#47130,#47131,#47132,#47133,
#47134,#47135,#47136,#47137,#47138,#47139,#47140,#47141,#47142),(#47143,
#47144,#47145,#47146,#47147,#47148,#47149,#47150,#47151,#47152,#47153,#47154,
#47155,#47156),(#47157,#47158,#47159,#47160,#47161,#47162,#47163,#47164,
#47165,#47166,#47167,#47168,#47169,#47170),(#47171,#47172,#47173,#47174,
#47175,#47176,#47177,#47178,#47179,#47180,#47181,#47182,#47183,#47184),
(#47185,#47186,#47187,#47188,#47189,#47190,#47191,#47192,#47193,#47194,
#47195,#47196,#47197,#47198),(#47199,#47200,#47201,#47202,#47203,#47204,
#47205,#47206,#47207,#47208,#47209,#47210,#47211,#47212),(#47213,#47214,
#47215,#47216,#47217,#47218,#47219,#47220,#47221,#47222,#47223,#47224,#47225,
#47226),(#47227,#47228,#47229,#47230,#47231,#47232,#47233,#47234,#47235,
#47236,#47237,#47238,#47239,#47240),(#47241,#47242,#47243,#47244,#47245,
#47246,#47247,#47248,#47249,#47250,#47251,#47252,#47253,#47254),(#47255,
#47256,#47257,#47258,#47259,#47260,#47261,#47262,#47263,#47264,#47265,#47266,
#47267,#47268),(#47269,#47270,#47271,#47272,#47273,#47274,#47275,#47276,
#47277,#47278,#47279,#47280,#47281,#47282),(#47283,#47284,#47285,#47286,
#47287,#47288,#47289,#47290,#47291,#47292,#47293,#47294,#47295,#47296),
(#47297,#47298,#47299,#47300,#47301,#47302,#47303,#47304,#47305,#47306,
#47307,#47308,#47309,#47310),(#47311,#47312,#47313,#47314,#47315,#47316,
#47317,#47318,#47319,#47320,#47321,#47322,#47323,#47324),(#47325,#47326,
#47327,#47328,#47329,#47330,#47331,#47332,#47333,#47334,#47335,#47336,#47337,
#47338),(#47339,#47340,#47341,#47342,#47343,#47344,#47345,#47346,#47347,
#47348,#47349,#47350,#47351,#47352),(#47353,#47354,#47355,#47356,#47357,
#47358,#47359,#47360,#47361,#47362,#47363,#47364,#47365,#47366),(#47367,
#47368,#47369,#47370,#47371,#47372,#47373,#47374,#47375,#47376,#47377,#47378,
#47379,#47380),(#47381,#47382,#47383,#47384,#47385,#47386,#47387,#47388,
#47389,#47390,#47391,#47392,#47393,#47394),(#47395,#47396,#47397,#47398,
#47399,#47400,#47401,#47402,#47403,#47404,#47405,#47406,#47407,#47408),
(#47409,#47410,#47411,#47412,#47413,#47414,#47415,#47416,#47417,#47418,
#47419,#47420,#47421,#47422),(#47423,#47424,#47425,#47426,#47427,#47428,
#47429,#47430,#47431,#47432,#47433,#47434,#47435,#47436),(#47437,#47438,
#47439,#47440,#47441,#47442,#47443,#47444,#47445,#47446,#47447,#47448,#47449,
#47450),(#47451,#47452,#47453,#47454,#47455,#47456,#47457,#47458,#47459,
#47460,#47461,#47462,#47463,#47464),(#47465,#47466,#47467,#47468,#47469,
#47470,#47471,#47472,#47473,#47474,#47475,#47476,#47477,#47478),(#47479,
#47480,#47481,#47482,#47483,#47484,#47485,#47486,#47487,#47488,#47489,#47490,
#47491,#47492),(#47493,#47494,#47495,#47496,#47497,#47498,#47499,#47500,
#47501,#47502,#47503,#47504,#47505,#47506),(#47507,#47508,#47509,#47510,
#47511,#47512,#47513,#47514,#47515,#47516,#47517,#47518,#47519,#47520),
(#47521,#47522,#47523,#47524,#47525,#47526,#47527,#47528,#47529,#47530,
#47531,#47532,#47533,#47534)),.UNSPECIFIED.,.F.,.F.,.F.,(4,1,1,1,1,1,1,
1,1,1,1,1,1,1,1,1,1,1,1,1,1,1,1,1,1,1,4),(4,2,2,2,2,2,4),(0.,0.0517952713240544,
0.0690603617654059,0.103590542648109,0.138120723530812,0.172650904413515,
0.276241447061623,0.310771627944326,0.345301808827029,0.414362170592435,
0.483422532357841,0.552482894123247,0.569747984564598,0.58701307500595,
0.621543255888653,0.690603617654059,0.725133798536761,0.759663979419464,
0.776929069860816,0.794194160302167,0.811459250743519,0.820091795964194,
0.824408068574532,0.82872434118487,0.897784702950276,0.932314883832979,
0.966845064715682),(0.0377143719394609,0.167070624995476,0.336553194126115,
0.499999999999991,0.663446805873868,0.832929375004528,0.962285628058648),
 .UNSPECIFIED.);
#212=B_SPLINE_SURFACE_WITH_KNOTS('',3,3,((#47592,#47593,#47594,#47595,#47596,
#47597,#47598,#47599,#47600,#47601,#47602,#47603,#47604,#47605),(#47606,
#47607,#47608,#47609,#47610,#47611,#47612,#47613,#47614,#47615,#47616,#47617,
#47618,#47619),(#47620,#47621,#47622,#47623,#47624,#47625,#47626,#47627,
#47628,#47629,#47630,#47631,#47632,#47633),(#47634,#47635,#47636,#47637,
#47638,#47639,#47640,#47641,#47642,#47643,#47644,#47645,#47646,#47647),
(#47648,#47649,#47650,#47651,#47652,#47653,#47654,#47655,#47656,#47657,
#47658,#47659,#47660,#47661),(#47662,#47663,#47664,#47665,#47666,#47667,
#47668,#47669,#47670,#47671,#47672,#47673,#47674,#47675),(#47676,#47677,
#47678,#47679,#47680,#47681,#47682,#47683,#47684,#47685,#47686,#47687,#47688,
#47689),(#47690,#47691,#47692,#47693,#47694,#47695,#47696,#47697,#47698,
#47699,#47700,#47701,#47702,#47703),(#47704,#47705,#47706,#47707,#47708,
#47709,#47710,#47711,#47712,#47713,#47714,#47715,#47716,#47717),(#47718,
#47719,#47720,#47721,#47722,#47723,#47724,#47725,#47726,#47727,#47728,#47729,
#47730,#47731),(#47732,#47733,#47734,#47735,#47736,#47737,#47738,#47739,
#47740,#47741,#47742,#47743,#47744,#47745),(#47746,#47747,#47748,#47749,
#47750,#47751,#47752,#47753,#47754,#47755,#47756,#47757,#47758,#47759),
(#47760,#47761,#47762,#47763,#47764,#47765,#47766,#47767,#47768,#47769,
#47770,#47771,#47772,#47773),(#47774,#47775,#47776,#47777,#47778,#47779,
#47780,#47781,#47782,#47783,#47784,#47785,#47786,#47787),(#47788,#47789,
#47790,#47791,#47792,#47793,#47794,#47795,#47796,#47797,#47798,#47799,#47800,
#47801),(#47802,#47803,#47804,#47805,#47806,#47807,#47808,#47809,#47810,
#47811,#47812,#47813,#47814,#47815),(#47816,#47817,#47818,#47819,#47820,
#47821,#47822,#47823,#47824,#47825,#47826,#47827,#47828,#47829),(#47830,
#47831,#47832,#47833,#47834,#47835,#47836,#47837,#47838,#47839,#47840,#47841,
#47842,#47843),(#47844,#47845,#47846,#47847,#47848,#47849,#47850,#47851,
#47852,#47853,#47854,#47855,#47856,#47857),(#47858,#47859,#47860,#47861,
#47862,#47863,#47864,#47865,#47866,#47867,#47868,#47869,#47870,#47871),
(#47872,#47873,#47874,#47875,#47876,#47877,#47878,#47879,#47880,#47881,
#47882,#47883,#47884,#47885)),.UNSPECIFIED.,.F.,.F.,.F.,(4,1,1,1,1,1,1,
1,1,1,1,1,1,1,1,1,1,1,4),(4,2,2,2,2,2,4),(0.0331549352864064,0.102215297051663,
0.136745477934291,0.240336020582176,0.309396382347433,0.37845674411269,
0.447517105877946,0.551107648525831,0.58563782940846,0.620168010291088,
0.706493462497659,0.723758552938973,0.758288733821602,0.827349095586858,
0.861879276469487,0.896409457352115,0.930939638234743,0.948204728676057,
1.),(0.0377143719408274,0.167070624995476,0.336553194126115,0.499999999999991,
0.663446805873868,0.832929375004528,0.962285628058718),.UNSPECIFIED.);
#213=B_SPLINE_SURFACE_WITH_KNOTS('',3,3,((#47942,#47943,#47944,#47945,#47946,
#47947,#47948,#47949,#47950,#47951,#47952,#47953,#47954,#47955),(#47956,
#47957,#47958,#47959,#47960,#47961,#47962,#47963,#47964,#47965,#47966,#47967,
#47968,#47969),(#47970,#47971,#47972,#47973,#47974,#47975,#47976,#47977,
#47978,#47979,#47980,#47981,#47982,#47983),(#47984,#47985,#47986,#47987,
#47988,#47989,#47990,#47991,#47992,#47993,#47994,#47995,#47996,#47997)),
 .UNSPECIFIED.,.F.,.F.,.F.,(4,4),(4,2,2,2,2,2,4),(0.,1.),(0.0377143719414211,
0.167070624995476,0.336553194126115,0.499999999999991,0.663446805873868,
0.832929375004528,0.962285628058582),.UNSPECIFIED.);
#214=B_SPLINE_SURFACE_WITH_KNOTS('',3,3,((#48012,#48013,#48014,#48015,#48016,
#48017,#48018,#48019,#48020,#48021,#48022,#48023,#48024,#48025),(#48026,
#48027,#48028,#48029,#48030,#48031,#48032,#48033,#48034,#48035,#48036,#48037,
#48038,#48039),(#48040,#48041,#48042,#48043,#48044,#48045,#48046,#48047,
#48048,#48049,#48050,#48051,#48052,#48053),(#48054,#48055,#48056,#48057,
#48058,#48059,#48060,#48061,#48062,#48063,#48064,#48065,#48066,#48067),
(#48068,#48069,#48070,#48071,#48072,#48073,#48074,#48075,#48076,#48077,
#48078,#48079,#48080,#48081),(#48082,#48083,#48084,#48085,#48086,#48087,
#48088,#48089,#48090,#48091,#48092,#48093,#48094,#48095),(#48096,#48097,
#48098,#48099,#48100,#48101,#48102,#48103,#48104,#48105,#48106,#48107,#48108,
#48109),(#48110,#48111,#48112,#48113,#48114,#48115,#48116,#48117,#48118,
#48119,#48120,#48121,#48122,#48123),(#48124,#48125,#48126,#48127,#48128,
#48129,#48130,#48131,#48132,#48133,#48134,#48135,#48136,#48137),(#48138,
#48139,#48140,#48141,#48142,#48143,#48144,#48145,#48146,#48147,#48148,#48149,
#48150,#48151),(#48152,#48153,#48154,#48155,#48156,#48157,#48158,#48159,
#48160,#48161,#48162,#48163,#48164,#48165),(#48166,#48167,#48168,#48169,
#48170,#48171,#48172,#48173,#48174,#48175,#48176,#48177,#48178,#48179),
(#48180,#48181,#48182,#48183,#48184,#48185,#48186,#48187,#48188,#48189,
#48190,#48191,#48192,#48193),(#48194,#48195,#48196,#48197,#48198,#48199,
#48200,#48201,#48202,#48203,#48204,#48205,#48206,#48207),(#48208,#48209,
#48210,#48211,#48212,#48213,#48214,#48215,#48216,#48217,#48218,#48219,#48220,
#48221),(#48222,#48223,#48224,#48225,#48226,#48227,#48228,#48229,#48230,
#48231,#48232,#48233,#48234,#48235),(#48236,#48237,#48238,#48239,#48240,
#48241,#48242,#48243,#48244,#48245,#48246,#48247,#48248,#48249),(#48250,
#48251,#48252,#48253,#48254,#48255,#48256,#48257,#48258,#48259,#48260,#48261,
#48262,#48263),(#48264,#48265,#48266,#48267,#48268,#48269,#48270,#48271,
#48272,#48273,#48274,#48275,#48276,#48277),(#48278,#48279,#48280,#48281,
#48282,#48283,#48284,#48285,#48286,#48287,#48288,#48289,#48290,#48291),
(#48292,#48293,#48294,#48295,#48296,#48297,#48298,#48299,#48300,#48301,
#48302,#48303,#48304,#48305),(#48306,#48307,#48308,#48309,#48310,#48311,
#48312,#48313,#48314,#48315,#48316,#48317,#48318,#48319),(#48320,#48321,
#48322,#48323,#48324,#48325,#48326,#48327,#48328,#48329,#48330,#48331,#48332,
#48333),(#48334,#48335,#48336,#48337,#48338,#48339,#48340,#48341,#48342,
#48343,#48344,#48345,#48346,#48347),(#48348,#48349,#48350,#48351,#48352,
#48353,#48354,#48355,#48356,#48357,#48358,#48359,#48360,#48361),(#48362,
#48363,#48364,#48365,#48366,#48367,#48368,#48369,#48370,#48371,#48372,#48373,
#48374,#48375),(#48376,#48377,#48378,#48379,#48380,#48381,#48382,#48383,
#48384,#48385,#48386,#48387,#48388,#48389),(#48390,#48391,#48392,#48393,
#48394,#48395,#48396,#48397,#48398,#48399,#48400,#48401,#48402,#48403),
(#48404,#48405,#48406,#48407,#48408,#48409,#48410,#48411,#48412,#48413,
#48414,#48415,#48416,#48417),(#48418,#48419,#48420,#48421,#48422,#48423,
#48424,#48425,#48426,#48427,#48428,#48429,#48430,#48431),(#48432,#48433,
#48434,#48435,#48436,#48437,#48438,#48439,#48440,#48441,#48442,#48443,#48444,
#48445),(#48446,#48447,#48448,#48449,#48450,#48451,#48452,#48453,#48454,
#48455,#48456,#48457,#48458,#48459),(#48460,#48461,#48462,#48463,#48464,
#48465,#48466,#48467,#48468,#48469,#48470,#48471,#48472,#48473)),
 .UNSPECIFIED.,.F.,.F.,.F.,(4,1,1,1,1,1,1,1,1,1,1,1,1,1,1,1,1,1,1,1,1,1,
1,1,1,1,1,1,1,1,4),(4,2,2,2,2,2,4),(0.,0.0517952713240545,0.069060361765406,
0.103590542648109,0.138120723530812,0.172650904413515,0.207181085296218,
0.276241447061624,0.34530180882703,0.414362170592436,0.448892351475139,
0.517952713240545,0.552482894123248,0.587013075005951,0.621543255888654,
0.647440891550682,0.69060361765406,0.725133798536763,0.759663979419467,
0.776929069860818,0.79419416030217,0.811459250743521,0.815775523353859,
0.820091795964197,0.824408068574535,0.826566204879704,0.827645273032288,
0.828724341184873,0.897784702950279,0.932314883832982,0.966845064715685),
(0.0377143719414145,0.167070624995476,0.336553194126115,0.499999999999991,
0.663446805873868,0.832929375004528,0.962285628059096),.UNSPECIFIED.);
#215=B_SPLINE_SURFACE_WITH_KNOTS('',3,3,((#48533,#48534,#48535,#48536,#48537,
#48538,#48539,#48540,#48541,#48542,#48543,#48544,#48545,#48546),(#48547,
#48548,#48549,#48550,#48551,#48552,#48553,#48554,#48555,#48556,#48557,#48558,
#48559,#48560),(#48561,#48562,#48563,#48564,#48565,#48566,#48567,#48568,
#48569,#48570,#48571,#48572,#48573,#48574),(#48575,#48576,#48577,#48578,
#48579,#48580,#48581,#48582,#48583,#48584,#48585,#48586,#48587,#48588),
(#48589,#48590,#48591,#48592,#48593,#48594,#48595,#48596,#48597,#48598,
#48599,#48600,#48601,#48602),(#48603,#48604,#48605,#48606,#48607,#48608,
#48609,#48610,#48611,#48612,#48613,#48614,#48615,#48616),(#48617,#48618,
#48619,#48620,#48621,#48622,#48623,#48624,#48625,#48626,#48627,#48628,#48629,
#48630),(#48631,#48632,#48633,#48634,#48635,#48636,#48637,#48638,#48639,
#48640,#48641,#48642,#48643,#48644),(#48645,#48646,#48647,#48648,#48649,
#48650,#48651,#48652,#48653,#48654,#48655,#48656,#48657,#48658),(#48659,
#48660,#48661,#48662,#48663,#48664,#48665,#48666,#48667,#48668,#48669,#48670,
#48671,#48672),(#48673,#48674,#48675,#48676,#48677,#48678,#48679,#48680,
#48681,#48682,#48683,#48684,#48685,#48686),(#48687,#48688,#48689,#48690,
#48691,#48692,#48693,#48694,#48695,#48696,#48697,#48698,#48699,#48700),
(#48701,#48702,#48703,#48704,#48705,#48706,#48707,#48708,#48709,#48710,
#48711,#48712,#48713,#48714),(#48715,#48716,#48717,#48718,#48719,#48720,
#48721,#48722,#48723,#48724,#48725,#48726,#48727,#48728),(#48729,#48730,
#48731,#48732,#48733,#48734,#48735,#48736,#48737,#48738,#48739,#48740,#48741,
#48742),(#48743,#48744,#48745,#48746,#48747,#48748,#48749,#48750,#48751,
#48752,#48753,#48754,#48755,#48756),(#48757,#48758,#48759,#48760,#48761,
#48762,#48763,#48764,#48765,#48766,#48767,#48768,#48769,#48770),(#48771,
#48772,#48773,#48774,#48775,#48776,#48777,#48778,#48779,#48780,#48781,#48782,
#48783,#48784),(#48785,#48786,#48787,#48788,#48789,#48790,#48791,#48792,
#48793,#48794,#48795,#48796,#48797,#48798),(#48799,#48800,#48801,#48802,
#48803,#48804,#48805,#48806,#48807,#48808,#48809,#48810,#48811,#48812),
(#48813,#48814,#48815,#48816,#48817,#48818,#48819,#48820,#48821,#48822,
#48823,#48824,#48825,#48826),(#48827,#48828,#48829,#48830,#48831,#48832,
#48833,#48834,#48835,#48836,#48837,#48838,#48839,#48840),(#48841,#48842,
#48843,#48844,#48845,#48846,#48847,#48848,#48849,#48850,#48851,#48852,#48853,
#48854),(#48855,#48856,#48857,#48858,#48859,#48860,#48861,#48862,#48863,
#48864,#48865,#48866,#48867,#48868),(#48869,#48870,#48871,#48872,#48873,
#48874,#48875,#48876,#48877,#48878,#48879,#48880,#48881,#48882),(#48883,
#48884,#48885,#48886,#48887,#48888,#48889,#48890,#48891,#48892,#48893,#48894,
#48895,#48896),(#48897,#48898,#48899,#48900,#48901,#48902,#48903,#48904,
#48905,#48906,#48907,#48908,#48909,#48910),(#48911,#48912,#48913,#48914,
#48915,#48916,#48917,#48918,#48919,#48920,#48921,#48922,#48923,#48924),
(#48925,#48926,#48927,#48928,#48929,#48930,#48931,#48932,#48933,#48934,
#48935,#48936,#48937,#48938),(#48939,#48940,#48941,#48942,#48943,#48944,
#48945,#48946,#48947,#48948,#48949,#48950,#48951,#48952)),.UNSPECIFIED.,
 .F.,.F.,.F.,(4,1,1,1,1,1,1,1,1,1,1,1,1,1,1,1,1,1,1,1,1,1,1,1,1,1,1,4),
(4,2,2,2,2,2,4),(0.0331549352864089,0.102215297051665,0.171275658816922,
0.173433795122086,0.17559193142725,0.179908204037579,0.188540749258236,
0.20580583969955,0.223070930140864,0.240336020582178,0.274866201464807,
0.309396382347435,0.378456744112691,0.41298692499532,0.447517105877948,
0.482047286760576,0.516577467643204,0.551107648525833,0.568372738967147,
0.585637829408461,0.689228372056346,0.723758552938974,0.810084005145545,
0.861879276469487,0.896409457352115,0.930939638234743,0.948204728676058,
1.),(0.0377143719403939,0.167070624995476,0.336553194126115,0.499999999999991,
0.663446805873868,0.832929375004528,0.962285628059341),.UNSPECIFIED.);
#216=B_SPLINE_SURFACE_WITH_KNOTS('',3,3,((#49013,#49014,#49015,#49016,#49017,
#49018,#49019,#49020,#49021,#49022,#49023,#49024,#49025,#49026),(#49027,
#49028,#49029,#49030,#49031,#49032,#49033,#49034,#49035,#49036,#49037,#49038,
#49039,#49040),(#49041,#49042,#49043,#49044,#49045,#49046,#49047,#49048,
#49049,#49050,#49051,#49052,#49053,#49054),(#49055,#49056,#49057,#49058,
#49059,#49060,#49061,#49062,#49063,#49064,#49065,#49066,#49067,#49068)),
 .UNSPECIFIED.,.F.,.F.,.F.,(4,4),(4,2,2,2,2,2,4),(0.,1.),(0.0377143719414212,
0.167070624995476,0.336553194126115,0.499999999999991,0.663446805873868,
0.832929375004528,0.962285628058582),.UNSPECIFIED.);
#217=B_SPLINE_SURFACE_WITH_KNOTS('',3,3,((#49083,#49084,#49085,#49086,#49087,
#49088,#49089,#49090,#49091,#49092,#49093,#49094,#49095,#49096),(#49097,
#49098,#49099,#49100,#49101,#49102,#49103,#49104,#49105,#49106,#49107,#49108,
#49109,#49110),(#49111,#49112,#49113,#49114,#49115,#49116,#49117,#49118,
#49119,#49120,#49121,#49122,#49123,#49124),(#49125,#49126,#49127,#49128,
#49129,#49130,#49131,#49132,#49133,#49134,#49135,#49136,#49137,#49138),
(#49139,#49140,#49141,#49142,#49143,#49144,#49145,#49146,#49147,#49148,
#49149,#49150,#49151,#49152),(#49153,#49154,#49155,#49156,#49157,#49158,
#49159,#49160,#49161,#49162,#49163,#49164,#49165,#49166),(#49167,#49168,
#49169,#49170,#49171,#49172,#49173,#49174,#49175,#49176,#49177,#49178,#49179,
#49180),(#49181,#49182,#49183,#49184,#49185,#49186,#49187,#49188,#49189,
#49190,#49191,#49192,#49193,#49194),(#49195,#49196,#49197,#49198,#49199,
#49200,#49201,#49202,#49203,#49204,#49205,#49206,#49207,#49208),(#49209,
#49210,#49211,#49212,#49213,#49214,#49215,#49216,#49217,#49218,#49219,#49220,
#49221,#49222),(#49223,#49224,#49225,#49226,#49227,#49228,#49229,#49230,
#49231,#49232,#49233,#49234,#49235,#49236),(#49237,#49238,#49239,#49240,
#49241,#49242,#49243,#49244,#49245,#49246,#49247,#49248,#49249,#49250),
(#49251,#49252,#49253,#49254,#49255,#49256,#49257,#49258,#49259,#49260,
#49261,#49262,#49263,#49264),(#49265,#49266,#49267,#49268,#49269,#49270,
#49271,#49272,#49273,#49274,#49275,#49276,#49277,#49278),(#49279,#49280,
#49281,#49282,#49283,#49284,#49285,#49286,#49287,#49288,#49289,#49290,#49291,
#49292),(#49293,#49294,#49295,#49296,#49297,#49298,#49299,#49300,#49301,
#49302,#49303,#49304,#49305,#49306),(#49307,#49308,#49309,#49310,#49311,
#49312,#49313,#49314,#49315,#49316,#49317,#49318,#49319,#49320),(#49321,
#49322,#49323,#49324,#49325,#49326,#49327,#49328,#49329,#49330,#49331,#49332,
#49333,#49334),(#49335,#49336,#49337,#49338,#49339,#49340,#49341,#49342,
#49343,#49344,#49345,#49346,#49347,#49348),(#49349,#49350,#49351,#49352,
#49353,#49354,#49355,#49356,#49357,#49358,#49359,#49360,#49361,#49362),
(#49363,#49364,#49365,#49366,#49367,#49368,#49369,#49370,#49371,#49372,
#49373,#49374,#49375,#49376),(#49377,#49378,#49379,#49380,#49381,#49382,
#49383,#49384,#49385,#49386,#49387,#49388,#49389,#49390),(#49391,#49392,
#49393,#49394,#49395,#49396,#49397,#49398,#49399,#49400,#49401,#49402,#49403,
#49404),(#49405,#49406,#49407,#49408,#49409,#49410,#49411,#49412,#49413,
#49414,#49415,#49416,#49417,#49418),(#49419,#49420,#49421,#49422,#49423,
#49424,#49425,#49426,#49427,#49428,#49429,#49430,#49431,#49432),(#49433,
#49434,#49435,#49436,#49437,#49438,#49439,#49440,#49441,#49442,#49443,#49444,
#49445,#49446),(#49447,#49448,#49449,#49450,#49451,#49452,#49453,#49454,
#49455,#49456,#49457,#49458,#49459,#49460),(#49461,#49462,#49463,#49464,
#49465,#49466,#49467,#49468,#49469,#49470,#49471,#49472,#49473,#49474),
(#49475,#49476,#49477,#49478,#49479,#49480,#49481,#49482,#49483,#49484,
#49485,#49486,#49487,#49488),(#49489,#49490,#49491,#49492,#49493,#49494,
#49495,#49496,#49497,#49498,#49499,#49500,#49501,#49502),(#49503,#49504,
#49505,#49506,#49507,#49508,#49509,#49510,#49511,#49512,#49513,#49514,#49515,
#49516),(#49517,#49518,#49519,#49520,#49521,#49522,#49523,#49524,#49525,
#49526,#49527,#49528,#49529,#49530)),.UNSPECIFIED.,.F.,.F.,.F.,(4,1,1,1,
1,1,1,1,1,1,1,1,1,1,1,1,1,1,1,1,1,1,1,1,1,1,1,1,1,4),(4,2,2,2,2,2,4),(0.,
0.0517952713240545,0.069060361765406,0.103590542648109,0.138120723530812,
0.172650904413515,0.207181085296218,0.276241447061624,0.34530180882703,
0.414362170592436,0.483422532357842,0.552482894123248,0.561115439343924,
0.5697479845646,0.587013075005951,0.621543255888654,0.69060361765406,0.725133798536763,
0.759663979419466,0.776929069860818,0.794194160302169,0.811459250743521,
0.815775523353859,0.820091795964197,0.824408068574535,0.826566204879703,
0.827645273032288,0.828724341184872,0.897784702950278,0.966845064715684),
(0.037714371939343,0.167070624995476,0.336553194126115,0.499999999999991,
0.663446805873868,0.832929375004528,0.962285628058644),.UNSPECIFIED.);
#218=B_SPLINE_SURFACE_WITH_KNOTS('',3,3,((#49586,#49587,#49588,#49589,#49590,
#49591,#49592,#49593,#49594,#49595,#49596,#49597,#49598,#49599),(#49600,
#49601,#49602,#49603,#49604,#49605,#49606,#49607,#49608,#49609,#49610,#49611,
#49612,#49613),(#49614,#49615,#49616,#49617,#49618,#49619,#49620,#49621,
#49622,#49623,#49624,#49625,#49626,#49627),(#49628,#49629,#49630,#49631,
#49632,#49633,#49634,#49635,#49636,#49637,#49638,#49639,#49640,#49641),
(#49642,#49643,#49644,#49645,#49646,#49647,#49648,#49649,#49650,#49651,
#49652,#49653,#49654,#49655),(#49656,#49657,#49658,#49659,#49660,#49661,
#49662,#49663,#49664,#49665,#49666,#49667,#49668,#49669),(#49670,#49671,
#49672,#49673,#49674,#49675,#49676,#49677,#49678,#49679,#49680,#49681,#49682,
#49683),(#49684,#49685,#49686,#49687,#49688,#49689,#49690,#49691,#49692,
#49693,#49694,#49695,#49696,#49697),(#49698,#49699,#49700,#49701,#49702,
#49703,#49704,#49705,#49706,#49707,#49708,#49709,#49710,#49711),(#49712,
#49713,#49714,#49715,#49716,#49717,#49718,#49719,#49720,#49721,#49722,#49723,
#49724,#49725),(#49726,#49727,#49728,#49729,#49730,#49731,#49732,#49733,
#49734,#49735,#49736,#49737,#49738,#49739),(#49740,#49741,#49742,#49743,
#49744,#49745,#49746,#49747,#49748,#49749,#49750,#49751,#49752,#49753),
(#49754,#49755,#49756,#49757,#49758,#49759,#49760,#49761,#49762,#49763,
#49764,#49765,#49766,#49767),(#49768,#49769,#49770,#49771,#49772,#49773,
#49774,#49775,#49776,#49777,#49778,#49779,#49780,#49781),(#49782,#49783,
#49784,#49785,#49786,#49787,#49788,#49789,#49790,#49791,#49792,#49793,#49794,
#49795),(#49796,#49797,#49798,#49799,#49800,#49801,#49802,#49803,#49804,
#49805,#49806,#49807,#49808,#49809),(#49810,#49811,#49812,#49813,#49814,
#49815,#49816,#49817,#49818,#49819,#49820,#49821,#49822,#49823),(#49824,
#49825,#49826,#49827,#49828,#49829,#49830,#49831,#49832,#49833,#49834,#49835,
#49836,#49837),(#49838,#49839,#49840,#49841,#49842,#49843,#49844,#49845,
#49846,#49847,#49848,#49849,#49850,#49851),(#49852,#49853,#49854,#49855,
#49856,#49857,#49858,#49859,#49860,#49861,#49862,#49863,#49864,#49865),
(#49866,#49867,#49868,#49869,#49870,#49871,#49872,#49873,#49874,#49875,
#49876,#49877,#49878,#49879),(#49880,#49881,#49882,#49883,#49884,#49885,
#49886,#49887,#49888,#49889,#49890,#49891,#49892,#49893),(#49894,#49895,
#49896,#49897,#49898,#49899,#49900,#49901,#49902,#49903,#49904,#49905,#49906,
#49907),(#49908,#49909,#49910,#49911,#49912,#49913,#49914,#49915,#49916,
#49917,#49918,#49919,#49920,#49921),(#49922,#49923,#49924,#49925,#49926,
#49927,#49928,#49929,#49930,#49931,#49932,#49933,#49934,#49935),(#49936,
#49937,#49938,#49939,#49940,#49941,#49942,#49943,#49944,#49945,#49946,#49947,
#49948,#49949),(#49950,#49951,#49952,#49953,#49954,#49955,#49956,#49957,
#49958,#49959,#49960,#49961,#49962,#49963),(#49964,#49965,#49966,#49967,
#49968,#49969,#49970,#49971,#49972,#49973,#49974,#49975,#49976,#49977),
(#49978,#49979,#49980,#49981,#49982,#49983,#49984,#49985,#49986,#49987,
#49988,#49989,#49990,#49991),(#49992,#49993,#49994,#49995,#49996,#49997,
#49998,#49999,#50000,#50001,#50002,#50003,#50004,#50005)),.UNSPECIFIED.,
 .F.,.F.,.F.,(4,1,1,1,1,1,1,1,1,1,1,1,1,1,1,1,1,1,1,1,1,1,1,1,1,1,1,4),
(4,2,2,2,2,2,4),(0.0331549352864079,0.102215297051665,0.171275658816921,
0.173433795122085,0.17559193142725,0.179908204037578,0.188540749258235,
0.205805839699549,0.240336020582178,0.309396382347434,0.378456744112691,
0.412986924995319,0.430252015436633,0.43888456065729,0.443200833267619,
0.447517105877947,0.516577467643204,0.585637829408461,0.620168010291089,
0.723758552938974,0.79281891470423,0.827349095586858,0.861879276469487,
0.896409457352115,0.913674547793429,0.930939638234743,0.948204728676058,
1.00005376760518),(0.0377143719409181,0.167070624995476,0.336553194126115,
0.499999999999991,0.663446805873868,0.832929375004528,0.962339395663765),
 .UNSPECIFIED.);
#219=B_SPLINE_SURFACE_WITH_KNOTS('',3,3,((#50068,#50069,#50070,#50071,#50072,
#50073,#50074,#50075,#50076,#50077,#50078,#50079,#50080,#50081),(#50082,
#50083,#50084,#50085,#50086,#50087,#50088,#50089,#50090,#50091,#50092,#50093,
#50094,#50095),(#50096,#50097,#50098,#50099,#50100,#50101,#50102,#50103,
#50104,#50105,#50106,#50107,#50108,#50109),(#50110,#50111,#50112,#50113,
#50114,#50115,#50116,#50117,#50118,#50119,#50120,#50121,#50122,#50123)),
 .UNSPECIFIED.,.F.,.F.,.F.,(4,4),(4,2,2,2,2,2,4),(0.,1.),(0.0377143719414212,
0.167070624995476,0.336553194126115,0.499999999999991,0.663446805873868,
0.832929375004528,0.962285628058582),.UNSPECIFIED.);
#220=B_SPLINE_SURFACE_WITH_KNOTS('',3,3,((#50138,#50139,#50140,#50141,#50142,
#50143,#50144,#50145,#50146,#50147,#50148,#50149,#50150,#50151),(#50152,
#50153,#50154,#50155,#50156,#50157,#50158,#50159,#50160,#50161,#50162,#50163,
#50164,#50165),(#50166,#50167,#50168,#50169,#50170,#50171,#50172,#50173,
#50174,#50175,#50176,#50177,#50178,#50179),(#50180,#50181,#50182,#50183,
#50184,#50185,#50186,#50187,#50188,#50189,#50190,#50191,#50192,#50193),
(#50194,#50195,#50196,#50197,#50198,#50199,#50200,#50201,#50202,#50203,
#50204,#50205,#50206,#50207),(#50208,#50209,#50210,#50211,#50212,#50213,
#50214,#50215,#50216,#50217,#50218,#50219,#50220,#50221),(#50222,#50223,
#50224,#50225,#50226,#50227,#50228,#50229,#50230,#50231,#50232,#50233,#50234,
#50235),(#50236,#50237,#50238,#50239,#50240,#50241,#50242,#50243,#50244,
#50245,#50246,#50247,#50248,#50249),(#50250,#50251,#50252,#50253,#50254,
#50255,#50256,#50257,#50258,#50259,#50260,#50261,#50262,#50263),(#50264,
#50265,#50266,#50267,#50268,#50269,#50270,#50271,#50272,#50273,#50274,#50275,
#50276,#50277),(#50278,#50279,#50280,#50281,#50282,#50283,#50284,#50285,
#50286,#50287,#50288,#50289,#50290,#50291),(#50292,#50293,#50294,#50295,
#50296,#50297,#50298,#50299,#50300,#50301,#50302,#50303,#50304,#50305),
(#50306,#50307,#50308,#50309,#50310,#50311,#50312,#50313,#50314,#50315,
#50316,#50317,#50318,#50319),(#50320,#50321,#50322,#50323,#50324,#50325,
#50326,#50327,#50328,#50329,#50330,#50331,#50332,#50333),(#50334,#50335,
#50336,#50337,#50338,#50339,#50340,#50341,#50342,#50343,#50344,#50345,#50346,
#50347),(#50348,#50349,#50350,#50351,#50352,#50353,#50354,#50355,#50356,
#50357,#50358,#50359,#50360,#50361),(#50362,#50363,#50364,#50365,#50366,
#50367,#50368,#50369,#50370,#50371,#50372,#50373,#50374,#50375),(#50376,
#50377,#50378,#50379,#50380,#50381,#50382,#50383,#50384,#50385,#50386,#50387,
#50388,#50389),(#50390,#50391,#50392,#50393,#50394,#50395,#50396,#50397,
#50398,#50399,#50400,#50401,#50402,#50403),(#50404,#50405,#50406,#50407,
#50408,#50409,#50410,#50411,#50412,#50413,#50414,#50415,#50416,#50417),
(#50418,#50419,#50420,#50421,#50422,#50423,#50424,#50425,#50426,#50427,
#50428,#50429,#50430,#50431),(#50432,#50433,#50434,#50435,#50436,#50437,
#50438,#50439,#50440,#50441,#50442,#50443,#50444,#50445),(#50446,#50447,
#50448,#50449,#50450,#50451,#50452,#50453,#50454,#50455,#50456,#50457,#50458,
#50459),(#50460,#50461,#50462,#50463,#50464,#50465,#50466,#50467,#50468,
#50469,#50470,#50471,#50472,#50473),(#50474,#50475,#50476,#50477,#50478,
#50479,#50480,#50481,#50482,#50483,#50484,#50485,#50486,#50487),(#50488,
#50489,#50490,#50491,#50492,#50493,#50494,#50495,#50496,#50497,#50498,#50499,
#50500,#50501)),.UNSPECIFIED.,.F.,.F.,.F.,(4,1,1,1,1,1,1,1,1,1,1,1,1,1,
1,1,1,1,1,1,1,1,1,4),(4,2,2,2,2,2,4),(0.,0.0517952713240544,0.0690603617654059,
0.103590542648109,0.138120723530812,0.189915994854866,0.276241447061624,
0.310771627944327,0.414362170592435,0.431627261033787,0.483422532357841,
0.552482894123247,0.621543255888653,0.690603617654059,0.759663979419465,
0.776929069860816,0.794194160302168,0.811459250743519,0.820091795964195,
0.824408068574533,0.826566204879702,0.828724341184871,0.897784702950277,
0.966845064715683),(0.0377143719411898,0.167070624995476,0.336553194126115,
0.499999999999991,0.663446805873868,0.832929375004528,0.962285628059115),
 .UNSPECIFIED.);
#221=B_SPLINE_SURFACE_WITH_KNOTS('',3,3,((#50553,#50554,#50555,#50556,#50557,
#50558,#50559,#50560,#50561,#50562,#50563,#50564,#50565,#50566),(#50567,
#50568,#50569,#50570,#50571,#50572,#50573,#50574,#50575,#50576,#50577,#50578,
#50579,#50580),(#50581,#50582,#50583,#50584,#50585,#50586,#50587,#50588,
#50589,#50590,#50591,#50592,#50593,#50594),(#50595,#50596,#50597,#50598,
#50599,#50600,#50601,#50602,#50603,#50604,#50605,#50606,#50607,#50608),
(#50609,#50610,#50611,#50612,#50613,#50614,#50615,#50616,#50617,#50618,
#50619,#50620,#50621,#50622),(#50623,#50624,#50625,#50626,#50627,#50628,
#50629,#50630,#50631,#50632,#50633,#50634,#50635,#50636),(#50637,#50638,
#50639,#50640,#50641,#50642,#50643,#50644,#50645,#50646,#50647,#50648,#50649,
#50650),(#50651,#50652,#50653,#50654,#50655,#50656,#50657,#50658,#50659,
#50660,#50661,#50662,#50663,#50664),(#50665,#50666,#50667,#50668,#50669,
#50670,#50671,#50672,#50673,#50674,#50675,#50676,#50677,#50678),(#50679,
#50680,#50681,#50682,#50683,#50684,#50685,#50686,#50687,#50688,#50689,#50690,
#50691,#50692),(#50693,#50694,#50695,#50696,#50697,#50698,#50699,#50700,
#50701,#50702,#50703,#50704,#50705,#50706),(#50707,#50708,#50709,#50710,
#50711,#50712,#50713,#50714,#50715,#50716,#50717,#50718,#50719,#50720),
(#50721,#50722,#50723,#50724,#50725,#50726,#50727,#50728,#50729,#50730,
#50731,#50732,#50733,#50734),(#50735,#50736,#50737,#50738,#50739,#50740,
#50741,#50742,#50743,#50744,#50745,#50746,#50747,#50748),(#50749,#50750,
#50751,#50752,#50753,#50754,#50755,#50756,#50757,#50758,#50759,#50760,#50761,
#50762),(#50763,#50764,#50765,#50766,#50767,#50768,#50769,#50770,#50771,
#50772,#50773,#50774,#50775,#50776),(#50777,#50778,#50779,#50780,#50781,
#50782,#50783,#50784,#50785,#50786,#50787,#50788,#50789,#50790),(#50791,
#50792,#50793,#50794,#50795,#50796,#50797,#50798,#50799,#50800,#50801,#50802,
#50803,#50804),(#50805,#50806,#50807,#50808,#50809,#50810,#50811,#50812,
#50813,#50814,#50815,#50816,#50817,#50818),(#50819,#50820,#50821,#50822,
#50823,#50824,#50825,#50826,#50827,#50828,#50829,#50830,#50831,#50832),
(#50833,#50834,#50835,#50836,#50837,#50838,#50839,#50840,#50841,#50842,
#50843,#50844,#50845,#50846),(#50847,#50848,#50849,#50850,#50851,#50852,
#50853,#50854,#50855,#50856,#50857,#50858,#50859,#50860),(#50861,#50862,
#50863,#50864,#50865,#50866,#50867,#50868,#50869,#50870,#50871,#50872,#50873,
#50874),(#50875,#50876,#50877,#50878,#50879,#50880,#50881,#50882,#50883,
#50884,#50885,#50886,#50887,#50888),(#50889,#50890,#50891,#50892,#50893,
#50894,#50895,#50896,#50897,#50898,#50899,#50900,#50901,#50902),(#50903,
#50904,#50905,#50906,#50907,#50908,#50909,#50910,#50911,#50912,#50913,#50914,
#50915,#50916),(#50917,#50918,#50919,#50920,#50921,#50922,#50923,#50924,
#50925,#50926,#50927,#50928,#50929,#50930),(#50931,#50932,#50933,#50934,
#50935,#50936,#50937,#50938,#50939,#50940,#50941,#50942,#50943,#50944)),
 .UNSPECIFIED.,.F.,.F.,.F.,(4,1,1,1,1,1,1,1,1,1,1,1,1,1,1,1,1,1,1,1,1,1,
1,1,1,4),(4,2,2,2,2,2,4),(0.0331549352864085,0.102215297051665,0.171275658816922,
0.17559193142725,0.179908204037579,0.188540749258236,0.20580583969955,0.240336020582178,
0.274866201464806,0.309396382347435,0.378456744112691,0.412986924995319,
0.447517105877948,0.482047286760576,0.516577467643204,0.551107648525832,
0.585637829408461,0.654698191173717,0.723758552938974,0.810084005145544,
0.827349095586859,0.861879276469487,0.896409457352115,0.930939638234743,
0.948204728676058,1.),(0.0377143719408683,0.167070624995476,0.336553194126115,
0.499999999999991,0.663446805873868,0.832929375004528,0.962285628059217),
 .UNSPECIFIED.);
#222=B_SPLINE_SURFACE_WITH_KNOTS('',3,3,((#51003,#51004,#51005,#51006,#51007,
#51008,#51009,#51010,#51011,#51012,#51013,#51014,#51015,#51016),(#51017,
#51018,#51019,#51020,#51021,#51022,#51023,#51024,#51025,#51026,#51027,#51028,
#51029,#51030),(#51031,#51032,#51033,#51034,#51035,#51036,#51037,#51038,
#51039,#51040,#51041,#51042,#51043,#51044),(#51045,#51046,#51047,#51048,
#51049,#51050,#51051,#51052,#51053,#51054,#51055,#51056,#51057,#51058)),
 .UNSPECIFIED.,.F.,.F.,.F.,(4,4),(4,2,2,2,2,2,4),(0.,1.),(0.0377143719414212,
0.167070624995476,0.336553194126115,0.499999999999991,0.663446805873868,
0.832929375004528,0.962285628058582),.UNSPECIFIED.);
#223=B_SPLINE_SURFACE_WITH_KNOTS('',3,3,((#51073,#51074,#51075,#51076,#51077,
#51078,#51079,#51080,#51081,#51082,#51083,#51084,#51085,#51086),(#51087,
#51088,#51089,#51090,#51091,#51092,#51093,#51094,#51095,#51096,#51097,#51098,
#51099,#51100),(#51101,#51102,#51103,#51104,#51105,#51106,#51107,#51108,
#51109,#51110,#51111,#51112,#51113,#51114),(#51115,#51116,#51117,#51118,
#51119,#51120,#51121,#51122,#51123,#51124,#51125,#51126,#51127,#51128),
(#51129,#51130,#51131,#51132,#51133,#51134,#51135,#51136,#51137,#51138,
#51139,#51140,#51141,#51142),(#51143,#51144,#51145,#51146,#51147,#51148,
#51149,#51150,#51151,#51152,#51153,#51154,#51155,#51156),(#51157,#51158,
#51159,#51160,#51161,#51162,#51163,#51164,#51165,#51166,#51167,#51168,#51169,
#51170),(#51171,#51172,#51173,#51174,#51175,#51176,#51177,#51178,#51179,
#51180,#51181,#51182,#51183,#51184),(#51185,#51186,#51187,#51188,#51189,
#51190,#51191,#51192,#51193,#51194,#51195,#51196,#51197,#51198),(#51199,
#51200,#51201,#51202,#51203,#51204,#51205,#51206,#51207,#51208,#51209,#51210,
#51211,#51212),(#51213,#51214,#51215,#51216,#51217,#51218,#51219,#51220,
#51221,#51222,#51223,#51224,#51225,#51226),(#51227,#51228,#51229,#51230,
#51231,#51232,#51233,#51234,#51235,#51236,#51237,#51238,#51239,#51240),
(#51241,#51242,#51243,#51244,#51245,#51246,#51247,#51248,#51249,#51250,
#51251,#51252,#51253,#51254),(#51255,#51256,#51257,#51258,#51259,#51260,
#51261,#51262,#51263,#51264,#51265,#51266,#51267,#51268),(#51269,#51270,
#51271,#51272,#51273,#51274,#51275,#51276,#51277,#51278,#51279,#51280,#51281,
#51282),(#51283,#51284,#51285,#51286,#51287,#51288,#51289,#51290,#51291,
#51292,#51293,#51294,#51295,#51296),(#51297,#51298,#51299,#51300,#51301,
#51302,#51303,#51304,#51305,#51306,#51307,#51308,#51309,#51310),(#51311,
#51312,#51313,#51314,#51315,#51316,#51317,#51318,#51319,#51320,#51321,#51322,
#51323,#51324),(#51325,#51326,#51327,#51328,#51329,#51330,#51331,#51332,
#51333,#51334,#51335,#51336,#51337,#51338),(#51339,#51340,#51341,#51342,
#51343,#51344,#51345,#51346,#51347,#51348,#51349,#51350,#51351,#51352),
(#51353,#51354,#51355,#51356,#51357,#51358,#51359,#51360,#51361,#51362,
#51363,#51364,#51365,#51366),(#51367,#51368,#51369,#51370,#51371,#51372,
#51373,#51374,#51375,#51376,#51377,#51378,#51379,#51380),(#51381,#51382,
#51383,#51384,#51385,#51386,#51387,#51388,#51389,#51390,#51391,#51392,#51393,
#51394),(#51395,#51396,#51397,#51398,#51399,#51400,#51401,#51402,#51403,
#51404,#51405,#51406,#51407,#51408),(#51409,#51410,#51411,#51412,#51413,
#51414,#51415,#51416,#51417,#51418,#51419,#51420,#51421,#51422),(#51423,
#51424,#51425,#51426,#51427,#51428,#51429,#51430,#51431,#51432,#51433,#51434,
#51435,#51436),(#51437,#51438,#51439,#51440,#51441,#51442,#51443,#51444,
#51445,#51446,#51447,#51448,#51449,#51450)),.UNSPECIFIED.,.F.,.F.,.F.,(4,
1,1,1,1,1,1,1,1,1,1,1,1,1,1,1,1,1,1,1,1,1,1,1,4),(4,2,2,2,2,2,4),(0.,0.0517952713240545,
0.069060361765406,0.103590542648109,0.138120723530812,0.172650904413515,
0.207181085296218,0.276241447061624,0.414362170592436,0.431627261033787,
0.483422532357842,0.552482894123248,0.621543255888654,0.69060361765406,
0.759663979419466,0.776929069860817,0.785561615081493,0.794194160302168,
0.81145925074352,0.820091795964196,0.824408068574534,0.826566204879703,
0.828724341184871,0.897784702950277,0.966845064715684),(0.037714371941379,
0.167070624995476,0.336553194126115,0.499999999999991,0.663446805873868,
0.832929375004528,0.962285628059256),.UNSPECIFIED.);
#224=B_SPLINE_SURFACE_WITH_KNOTS('',3,3,((#51502,#51503,#51504,#51505,#51506,
#51507,#51508,#51509,#51510,#51511,#51512,#51513,#51514,#51515),(#51516,
#51517,#51518,#51519,#51520,#51521,#51522,#51523,#51524,#51525,#51526,#51527,
#51528,#51529),(#51530,#51531,#51532,#51533,#51534,#51535,#51536,#51537,
#51538,#51539,#51540,#51541,#51542,#51543),(#51544,#51545,#51546,#51547,
#51548,#51549,#51550,#51551,#51552,#51553,#51554,#51555,#51556,#51557),
(#51558,#51559,#51560,#51561,#51562,#51563,#51564,#51565,#51566,#51567,
#51568,#51569,#51570,#51571),(#51572,#51573,#51574,#51575,#51576,#51577,
#51578,#51579,#51580,#51581,#51582,#51583,#51584,#51585),(#51586,#51587,
#51588,#51589,#51590,#51591,#51592,#51593,#51594,#51595,#51596,#51597,#51598,
#51599),(#51600,#51601,#51602,#51603,#51604,#51605,#51606,#51607,#51608,
#51609,#51610,#51611,#51612,#51613),(#51614,#51615,#51616,#51617,#51618,
#51619,#51620,#51621,#51622,#51623,#51624,#51625,#51626,#51627),(#51628,
#51629,#51630,#51631,#51632,#51633,#51634,#51635,#51636,#51637,#51638,#51639,
#51640,#51641),(#51642,#51643,#51644,#51645,#51646,#51647,#51648,#51649,
#51650,#51651,#51652,#51653,#51654,#51655),(#51656,#51657,#51658,#51659,
#51660,#51661,#51662,#51663,#51664,#51665,#51666,#51667,#51668,#51669),
(#51670,#51671,#51672,#51673,#51674,#51675,#51676,#51677,#51678,#51679,
#51680,#51681,#51682,#51683),(#51684,#51685,#51686,#51687,#51688,#51689,
#51690,#51691,#51692,#51693,#51694,#51695,#51696,#51697),(#51698,#51699,
#51700,#51701,#51702,#51703,#51704,#51705,#51706,#51707,#51708,#51709,#51710,
#51711),(#51712,#51713,#51714,#51715,#51716,#51717,#51718,#51719,#51720,
#51721,#51722,#51723,#51724,#51725),(#51726,#51727,#51728,#51729,#51730,
#51731,#51732,#51733,#51734,#51735,#51736,#51737,#51738,#51739),(#51740,
#51741,#51742,#51743,#51744,#51745,#51746,#51747,#51748,#51749,#51750,#51751,
#51752,#51753),(#51754,#51755,#51756,#51757,#51758,#51759,#51760,#51761,
#51762,#51763,#51764,#51765,#51766,#51767),(#51768,#51769,#51770,#51771,
#51772,#51773,#51774,#51775,#51776,#51777,#51778,#51779,#51780,#51781),
(#51782,#51783,#51784,#51785,#51786,#51787,#51788,#51789,#51790,#51791,
#51792,#51793,#51794,#51795),(#51796,#51797,#51798,#51799,#51800,#51801,
#51802,#51803,#51804,#51805,#51806,#51807,#51808,#51809),(#51810,#51811,
#51812,#51813,#51814,#51815,#51816,#51817,#51818,#51819,#51820,#51821,#51822,
#51823),(#51824,#51825,#51826,#51827,#51828,#51829,#51830,#51831,#51832,
#51833,#51834,#51835,#51836,#51837),(#51838,#51839,#51840,#51841,#51842,
#51843,#51844,#51845,#51846,#51847,#51848,#51849,#51850,#51851),(#51852,
#51853,#51854,#51855,#51856,#51857,#51858,#51859,#51860,#51861,#51862,#51863,
#51864,#51865),(#51866,#51867,#51868,#51869,#51870,#51871,#51872,#51873,
#51874,#51875,#51876,#51877,#51878,#51879),(#51880,#51881,#51882,#51883,
#51884,#51885,#51886,#51887,#51888,#51889,#51890,#51891,#51892,#51893),
(#51894,#51895,#51896,#51897,#51898,#51899,#51900,#51901,#51902,#51903,
#51904,#51905,#51906,#51907),(#51908,#51909,#51910,#51911,#51912,#51913,
#51914,#51915,#51916,#51917,#51918,#51919,#51920,#51921),(#51922,#51923,
#51924,#51925,#51926,#51927,#51928,#51929,#51930,#51931,#51932,#51933,#51934,
#51935),(#51936,#51937,#51938,#51939,#51940,#51941,#51942,#51943,#51944,
#51945,#51946,#51947,#51948,#51949),(#51950,#51951,#51952,#51953,#51954,
#51955,#51956,#51957,#51958,#51959,#51960,#51961,#51962,#51963)),
 .UNSPECIFIED.,.F.,.F.,.F.,(4,1,1,1,1,1,1,1,1,1,1,1,1,1,1,1,1,1,1,1,1,1,
1,1,1,1,1,1,1,1,4),(4,2,2,2,2,2,4),(0.0331549352864046,0.102215297051661,
0.171275658816918,0.1723547269695,0.173433795122083,0.174512863274665,0.175591931427247,
0.179908204037575,0.188540749258232,0.19717329447889,0.201489567089218,
0.205805839699547,0.223070930140861,0.240336020582175,0.274866201464803,
0.309396382347432,0.378456744112689,0.412986924995317,0.430252015436631,
0.447517105877945,0.516577467643202,0.585637829408459,0.654698191173716,
0.689228372056344,0.723758552938973,0.810084005145544,0.861879276469486,
0.896409457352115,0.930939638234743,0.948204728676057,1.),(0.0377143719409187,
0.167070624995476,0.336553194126115,0.499999999999991,0.663446805873868,
0.832929375004528,0.962285628058616),.UNSPECIFIED.);
#225=B_SPLINE_SURFACE_WITH_KNOTS('',3,3,((#52024,#52025,#52026,#52027,#52028,
#52029,#52030,#52031,#52032,#52033,#52034,#52035,#52036,#52037),(#52038,
#52039,#52040,#52041,#52042,#52043,#52044,#52045,#52046,#52047,#52048,#52049,
#52050,#52051),(#52052,#52053,#52054,#52055,#52056,#52057,#52058,#52059,
#52060,#52061,#52062,#52063,#52064,#52065),(#52066,#52067,#52068,#52069,
#52070,#52071,#52072,#52073,#52074,#52075,#52076,#52077,#52078,#52079)),
 .UNSPECIFIED.,.F.,.F.,.F.,(4,4),(4,2,2,2,2,2,4),(0.,1.),(0.0377143719414211,
0.167070624995476,0.336553194126115,0.499999999999991,0.663446805873868,
0.832929375004528,0.962285628058582),.UNSPECIFIED.);
#226=B_SPLINE_SURFACE_WITH_KNOTS('',3,3,((#52094,#52095,#52096,#52097,#52098,
#52099,#52100,#52101,#52102,#52103,#52104,#52105,#52106,#52107),(#52108,
#52109,#52110,#52111,#52112,#52113,#52114,#52115,#52116,#52117,#52118,#52119,
#52120,#52121),(#52122,#52123,#52124,#52125,#52126,#52127,#52128,#52129,
#52130,#52131,#52132,#52133,#52134,#52135),(#52136,#52137,#52138,#52139,
#52140,#52141,#52142,#52143,#52144,#52145,#52146,#52147,#52148,#52149),
(#52150,#52151,#52152,#52153,#52154,#52155,#52156,#52157,#52158,#52159,
#52160,#52161,#52162,#52163),(#52164,#52165,#52166,#52167,#52168,#52169,
#52170,#52171,#52172,#52173,#52174,#52175,#52176,#52177),(#52178,#52179,
#52180,#52181,#52182,#52183,#52184,#52185,#52186,#52187,#52188,#52189,#52190,
#52191),(#52192,#52193,#52194,#52195,#52196,#52197,#52198,#52199,#52200,
#52201,#52202,#52203,#52204,#52205),(#52206,#52207,#52208,#52209,#52210,
#52211,#52212,#52213,#52214,#52215,#52216,#52217,#52218,#52219),(#52220,
#52221,#52222,#52223,#52224,#52225,#52226,#52227,#52228,#52229,#52230,#52231,
#52232,#52233),(#52234,#52235,#52236,#52237,#52238,#52239,#52240,#52241,
#52242,#52243,#52244,#52245,#52246,#52247),(#52248,#52249,#52250,#52251,
#52252,#52253,#52254,#52255,#52256,#52257,#52258,#52259,#52260,#52261),
(#52262,#52263,#52264,#52265,#52266,#52267,#52268,#52269,#52270,#52271,
#52272,#52273,#52274,#52275),(#52276,#52277,#52278,#52279,#52280,#52281,
#52282,#52283,#52284,#52285,#52286,#52287,#52288,#52289),(#52290,#52291,
#52292,#52293,#52294,#52295,#52296,#52297,#52298,#52299,#52300,#52301,#52302,
#52303),(#52304,#52305,#52306,#52307,#52308,#52309,#52310,#52311,#52312,
#52313,#52314,#52315,#52316,#52317),(#52318,#52319,#52320,#52321,#52322,
#52323,#52324,#52325,#52326,#52327,#52328,#52329,#52330,#52331),(#52332,
#52333,#52334,#52335,#52336,#52337,#52338,#52339,#52340,#52341,#52342,#52343,
#52344,#52345),(#52346,#52347,#52348,#52349,#52350,#52351,#52352,#52353,
#52354,#52355,#52356,#52357,#52358,#52359),(#52360,#52361,#52362,#52363,
#52364,#52365,#52366,#52367,#52368,#52369,#52370,#52371,#52372,#52373),
(#52374,#52375,#52376,#52377,#52378,#52379,#52380,#52381,#52382,#52383,
#52384,#52385,#52386,#52387),(#52388,#52389,#52390,#52391,#52392,#52393,
#52394,#52395,#52396,#52397,#52398,#52399,#52400,#52401),(#52402,#52403,
#52404,#52405,#52406,#52407,#52408,#52409,#52410,#52411,#52412,#52413,#52414,
#52415),(#52416,#52417,#52418,#52419,#52420,#52421,#52422,#52423,#52424,
#52425,#52426,#52427,#52428,#52429),(#52430,#52431,#52432,#52433,#52434,
#52435,#52436,#52437,#52438,#52439,#52440,#52441,#52442,#52443),(#52444,
#52445,#52446,#52447,#52448,#52449,#52450,#52451,#52452,#52453,#52454,#52455,
#52456,#52457),(#52458,#52459,#52460,#52461,#52462,#52463,#52464,#52465,
#52466,#52467,#52468,#52469,#52470,#52471),(#52472,#52473,#52474,#52475,
#52476,#52477,#52478,#52479,#52480,#52481,#52482,#52483,#52484,#52485),
(#52486,#52487,#52488,#52489,#52490,#52491,#52492,#52493,#52494,#52495,
#52496,#52497,#52498,#52499),(#52500,#52501,#52502,#52503,#52504,#52505,
#52506,#52507,#52508,#52509,#52510,#52511,#52512,#52513),(#52514,#52515,
#52516,#52517,#52518,#52519,#52520,#52521,#52522,#52523,#52524,#52525,#52526,
#52527),(#52528,#52529,#52530,#52531,#52532,#52533,#52534,#52535,#52536,
#52537,#52538,#52539,#52540,#52541),(#52542,#52543,#52544,#52545,#52546,
#52547,#52548,#52549,#52550,#52551,#52552,#52553,#52554,#52555),(#52556,
#52557,#52558,#52559,#52560,#52561,#52562,#52563,#52564,#52565,#52566,#52567,
#52568,#52569),(#52570,#52571,#52572,#52573,#52574,#52575,#52576,#52577,
#52578,#52579,#52580,#52581,#52582,#52583),(#52584,#52585,#52586,#52587,
#52588,#52589,#52590,#52591,#52592,#52593,#52594,#52595,#52596,#52597),
(#52598,#52599,#52600,#52601,#52602,#52603,#52604,#52605,#52606,#52607,
#52608,#52609,#52610,#52611),(#52612,#52613,#52614,#52615,#52616,#52617,
#52618,#52619,#52620,#52621,#52622,#52623,#52624,#52625),(#52626,#52627,
#52628,#52629,#52630,#52631,#52632,#52633,#52634,#52635,#52636,#52637,#52638,
#52639),(#52640,#52641,#52642,#52643,#52644,#52645,#52646,#52647,#52648,
#52649,#52650,#52651,#52652,#52653),(#52654,#52655,#52656,#52657,#52658,
#52659,#52660,#52661,#52662,#52663,#52664,#52665,#52666,#52667)),
 .UNSPECIFIED.,.F.,.F.,.F.,(4,1,1,1,1,1,1,1,1,1,1,1,1,1,1,1,1,1,1,1,1,1,
1,1,1,1,1,1,1,1,1,1,1,1,1,1,1,1,4),(4,2,2,2,2,2,4),(0.,0.0517952713240546,
0.0690603617654062,0.103590542648109,0.138120723530812,0.172650904413515,
0.207181085296219,0.276241447061625,0.310771627944328,0.345301808827031,
0.414362170592437,0.422994715813113,0.431627261033789,0.44889235147514,
0.483422532357843,0.552482894123249,0.587013075005953,0.595645620226628,
0.621543255888656,0.656073436771359,0.690603617654062,0.725133798536765,
0.759663979419468,0.763980252029806,0.768296524640144,0.77692906986082,
0.794194160302171,0.802826705522847,0.811459250743523,0.820091795964198,
0.824408068574536,0.825487136727121,0.826566204879705,0.82764527303229,
0.828184807108582,0.828454574146728,0.828724341184874,0.89778470295028,
0.966845064715687),(0.0377143719402601,0.167070624995476,0.336553194126115,
0.499999999999991,0.663446805873868,0.832929375004528,0.962285628059988),
 .UNSPECIFIED.);
#227=B_SPLINE_SURFACE_WITH_KNOTS('',3,3,((#52721,#52722,#52723,#52724,#52725,
#52726,#52727,#52728,#52729,#52730,#52731,#52732,#52733,#52734),(#52735,
#52736,#52737,#52738,#52739,#52740,#52741,#52742,#52743,#52744,#52745,#52746,
#52747,#52748),(#52749,#52750,#52751,#52752,#52753,#52754,#52755,#52756,
#52757,#52758,#52759,#52760,#52761,#52762),(#52763,#52764,#52765,#52766,
#52767,#52768,#52769,#52770,#52771,#52772,#52773,#52774,#52775,#52776),
(#52777,#52778,#52779,#52780,#52781,#52782,#52783,#52784,#52785,#52786,
#52787,#52788,#52789,#52790),(#52791,#52792,#52793,#52794,#52795,#52796,
#52797,#52798,#52799,#52800,#52801,#52802,#52803,#52804),(#52805,#52806,
#52807,#52808,#52809,#52810,#52811,#52812,#52813,#52814,#52815,#52816,#52817,
#52818),(#52819,#52820,#52821,#52822,#52823,#52824,#52825,#52826,#52827,
#52828,#52829,#52830,#52831,#52832),(#52833,#52834,#52835,#52836,#52837,
#52838,#52839,#52840,#52841,#52842,#52843,#52844,#52845,#52846),(#52847,
#52848,#52849,#52850,#52851,#52852,#52853,#52854,#52855,#52856,#52857,#52858,
#52859,#52860),(#52861,#52862,#52863,#52864,#52865,#52866,#52867,#52868,
#52869,#52870,#52871,#52872,#52873,#52874),(#52875,#52876,#52877,#52878,
#52879,#52880,#52881,#52882,#52883,#52884,#52885,#52886,#52887,#52888),
(#52889,#52890,#52891,#52892,#52893,#52894,#52895,#52896,#52897,#52898,
#52899,#52900,#52901,#52902),(#52903,#52904,#52905,#52906,#52907,#52908,
#52909,#52910,#52911,#52912,#52913,#52914,#52915,#52916),(#52917,#52918,
#52919,#52920,#52921,#52922,#52923,#52924,#52925,#52926,#52927,#52928,#52929,
#52930),(#52931,#52932,#52933,#52934,#52935,#52936,#52937,#52938,#52939,
#52940,#52941,#52942,#52943,#52944),(#52945,#52946,#52947,#52948,#52949,
#52950,#52951,#52952,#52953,#52954,#52955,#52956,#52957,#52958),(#52959,
#52960,#52961,#52962,#52963,#52964,#52965,#52966,#52967,#52968,#52969,#52970,
#52971,#52972),(#52973,#52974,#52975,#52976,#52977,#52978,#52979,#52980,
#52981,#52982,#52983,#52984,#52985,#52986),(#52987,#52988,#52989,#52990,
#52991,#52992,#52993,#52994,#52995,#52996,#52997,#52998,#52999,#53000),
(#53001,#53002,#53003,#53004,#53005,#53006,#53007,#53008,#53009,#53010,
#53011,#53012,#53013,#53014),(#53015,#53016,#53017,#53018,#53019,#53020,
#53021,#53022,#53023,#53024,#53025,#53026,#53027,#53028),(#53029,#53030,
#53031,#53032,#53033,#53034,#53035,#53036,#53037,#53038,#53039,#53040,#53041,
#53042),(#53043,#53044,#53045,#53046,#53047,#53048,#53049,#53050,#53051,
#53052,#53053,#53054,#53055,#53056),(#53057,#53058,#53059,#53060,#53061,
#53062,#53063,#53064,#53065,#53066,#53067,#53068,#53069,#53070),(#53071,
#53072,#53073,#53074,#53075,#53076,#53077,#53078,#53079,#53080,#53081,#53082,
#53083,#53084),(#53085,#53086,#53087,#53088,#53089,#53090,#53091,#53092,
#53093,#53094,#53095,#53096,#53097,#53098),(#53099,#53100,#53101,#53102,
#53103,#53104,#53105,#53106,#53107,#53108,#53109,#53110,#53111,#53112),
(#53113,#53114,#53115,#53116,#53117,#53118,#53119,#53120,#53121,#53122,
#53123,#53124,#53125,#53126)),.UNSPECIFIED.,.F.,.F.,.F.,(4,1,1,1,1,1,1,
1,1,1,1,1,1,1,1,1,1,1,1,1,1,1,1,1,1,1,4),(4,2,2,2,2,2,4),(0.0331549352864105,
0.102215297051667,0.171275658816923,0.173433795122088,0.175591931427252,
0.17990820403758,0.188540749258237,0.205805839699551,0.24033602058218,0.274866201464808,
0.309396382347436,0.378456744112692,0.412986924995321,0.447517105877949,
0.516577467643205,0.585637829408462,0.602902919849776,0.62016801029109,
0.654698191173718,0.689228372056346,0.723758552938975,0.810084005145545,
0.861879276469487,0.896409457352116,0.930939638234744,0.948204728676058,
1.),(0.0377143719413902,0.167070624995476,0.336553194126115,0.499999999999991,
0.663446805873868,0.832929375004528,0.962285628058762),.UNSPECIFIED.);
#228=B_SPLINE_SURFACE_WITH_KNOTS('',3,3,((#53183,#53184,#53185,#53186,#53187,
#53188,#53189,#53190,#53191,#53192,#53193,#53194,#53195,#53196),(#53197,
#53198,#53199,#53200,#53201,#53202,#53203,#53204,#53205,#53206,#53207,#53208,
#53209,#53210),(#53211,#53212,#53213,#53214,#53215,#53216,#53217,#53218,
#53219,#53220,#53221,#53222,#53223,#53224),(#53225,#53226,#53227,#53228,
#53229,#53230,#53231,#53232,#53233,#53234,#53235,#53236,#53237,#53238)),
 .UNSPECIFIED.,.F.,.F.,.F.,(4,4),(4,2,2,2,2,2,4),(0.,1.),(0.0377143719414212,
0.167070624995476,0.336553194126115,0.499999999999991,0.663446805873868,
0.832929375004528,0.962285628058582),.UNSPECIFIED.);
#229=B_SPLINE_SURFACE_WITH_KNOTS('',3,3,((#53253,#53254,#53255,#53256,#53257,
#53258,#53259,#53260,#53261,#53262,#53263,#53264,#53265,#53266),(#53267,
#53268,#53269,#53270,#53271,#53272,#53273,#53274,#53275,#53276,#53277,#53278,
#53279,#53280),(#53281,#53282,#53283,#53284,#53285,#53286,#53287,#53288,
#53289,#53290,#53291,#53292,#53293,#53294),(#53295,#53296,#53297,#53298,
#53299,#53300,#53301,#53302,#53303,#53304,#53305,#53306,#53307,#53308),
(#53309,#53310,#53311,#53312,#53313,#53314,#53315,#53316,#53317,#53318,
#53319,#53320,#53321,#53322),(#53323,#53324,#53325,#53326,#53327,#53328,
#53329,#53330,#53331,#53332,#53333,#53334,#53335,#53336),(#53337,#53338,
#53339,#53340,#53341,#53342,#53343,#53344,#53345,#53346,#53347,#53348,#53349,
#53350),(#53351,#53352,#53353,#53354,#53355,#53356,#53357,#53358,#53359,
#53360,#53361,#53362,#53363,#53364),(#53365,#53366,#53367,#53368,#53369,
#53370,#53371,#53372,#53373,#53374,#53375,#53376,#53377,#53378),(#53379,
#53380,#53381,#53382,#53383,#53384,#53385,#53386,#53387,#53388,#53389,#53390,
#53391,#53392),(#53393,#53394,#53395,#53396,#53397,#53398,#53399,#53400,
#53401,#53402,#53403,#53404,#53405,#53406),(#53407,#53408,#53409,#53410,
#53411,#53412,#53413,#53414,#53415,#53416,#53417,#53418,#53419,#53420),
(#53421,#53422,#53423,#53424,#53425,#53426,#53427,#53428,#53429,#53430,
#53431,#53432,#53433,#53434),(#53435,#53436,#53437,#53438,#53439,#53440,
#53441,#53442,#53443,#53444,#53445,#53446,#53447,#53448),(#53449,#53450,
#53451,#53452,#53453,#53454,#53455,#53456,#53457,#53458,#53459,#53460,#53461,
#53462),(#53463,#53464,#53465,#53466,#53467,#53468,#53469,#53470,#53471,
#53472,#53473,#53474,#53475,#53476),(#53477,#53478,#53479,#53480,#53481,
#53482,#53483,#53484,#53485,#53486,#53487,#53488,#53489,#53490),(#53491,
#53492,#53493,#53494,#53495,#53496,#53497,#53498,#53499,#53500,#53501,#53502,
#53503,#53504),(#53505,#53506,#53507,#53508,#53509,#53510,#53511,#53512,
#53513,#53514,#53515,#53516,#53517,#53518),(#53519,#53520,#53521,#53522,
#53523,#53524,#53525,#53526,#53527,#53528,#53529,#53530,#53531,#53532),
(#53533,#53534,#53535,#53536,#53537,#53538,#53539,#53540,#53541,#53542,
#53543,#53544,#53545,#53546),(#53547,#53548,#53549,#53550,#53551,#53552,
#53553,#53554,#53555,#53556,#53557,#53558,#53559,#53560),(#53561,#53562,
#53563,#53564,#53565,#53566,#53567,#53568,#53569,#53570,#53571,#53572,#53573,
#53574),(#53575,#53576,#53577,#53578,#53579,#53580,#53581,#53582,#53583,
#53584,#53585,#53586,#53587,#53588),(#53589,#53590,#53591,#53592,#53593,
#53594,#53595,#53596,#53597,#53598,#53599,#53600,#53601,#53602),(#53603,
#53604,#53605,#53606,#53607,#53608,#53609,#53610,#53611,#53612,#53613,#53614,
#53615,#53616),(#53617,#53618,#53619,#53620,#53621,#53622,#53623,#53624,
#53625,#53626,#53627,#53628,#53629,#53630),(#53631,#53632,#53633,#53634,
#53635,#53636,#53637,#53638,#53639,#53640,#53641,#53642,#53643,#53644),
(#53645,#53646,#53647,#53648,#53649,#53650,#53651,#53652,#53653,#53654,
#53655,#53656,#53657,#53658),(#53659,#53660,#53661,#53662,#53663,#53664,
#53665,#53666,#53667,#53668,#53669,#53670,#53671,#53672),(#53673,#53674,
#53675,#53676,#53677,#53678,#53679,#53680,#53681,#53682,#53683,#53684,#53685,
#53686),(#53687,#53688,#53689,#53690,#53691,#53692,#53693,#53694,#53695,
#53696,#53697,#53698,#53699,#53700),(#53701,#53702,#53703,#53704,#53705,
#53706,#53707,#53708,#53709,#53710,#53711,#53712,#53713,#53714)),
 .UNSPECIFIED.,.F.,.F.,.F.,(4,1,1,1,1,1,1,1,1,1,1,1,1,1,1,1,1,1,1,1,1,1,
1,1,1,1,1,1,1,1,4),(4,2,2,2,2,2,4),(0.,0.0517952713240545,0.069060361765406,
0.103590542648109,0.138120723530812,0.172650904413515,0.207181085296218,
0.276241447061624,0.310771627944327,0.414362170592436,0.483422532357842,
0.500687622799194,0.517952713240545,0.552482894123248,0.621543255888654,
0.69060361765406,0.759663979419466,0.776929069860818,0.785561615081493,
0.789877887691831,0.794194160302169,0.802826705522845,0.811459250743521,
0.820091795964196,0.824408068574534,0.826566204879703,0.827645273032288,
0.82818480710858,0.828724341184872,0.897784702950278,0.966845064715684),
(0.0377143719414203,0.167070624995476,0.336553194126115,0.499999999999991,
0.663446805873868,0.832929375004528,0.962285628060272),.UNSPECIFIED.);
#230=B_SPLINE_SURFACE_WITH_KNOTS('',3,3,((#53766,#53767,#53768,#53769,#53770,
#53771,#53772,#53773,#53774,#53775,#53776,#53777,#53778,#53779),(#53780,
#53781,#53782,#53783,#53784,#53785,#53786,#53787,#53788,#53789,#53790,#53791,
#53792,#53793),(#53794,#53795,#53796,#53797,#53798,#53799,#53800,#53801,
#53802,#53803,#53804,#53805,#53806,#53807),(#53808,#53809,#53810,#53811,
#53812,#53813,#53814,#53815,#53816,#53817,#53818,#53819,#53820,#53821),
(#53822,#53823,#53824,#53825,#53826,#53827,#53828,#53829,#53830,#53831,
#53832,#53833,#53834,#53835),(#53836,#53837,#53838,#53839,#53840,#53841,
#53842,#53843,#53844,#53845,#53846,#53847,#53848,#53849),(#53850,#53851,
#53852,#53853,#53854,#53855,#53856,#53857,#53858,#53859,#53860,#53861,#53862,
#53863),(#53864,#53865,#53866,#53867,#53868,#53869,#53870,#53871,#53872,
#53873,#53874,#53875,#53876,#53877),(#53878,#53879,#53880,#53881,#53882,
#53883,#53884,#53885,#53886,#53887,#53888,#53889,#53890,#53891),(#53892,
#53893,#53894,#53895,#53896,#53897,#53898,#53899,#53900,#53901,#53902,#53903,
#53904,#53905),(#53906,#53907,#53908,#53909,#53910,#53911,#53912,#53913,
#53914,#53915,#53916,#53917,#53918,#53919),(#53920,#53921,#53922,#53923,
#53924,#53925,#53926,#53927,#53928,#53929,#53930,#53931,#53932,#53933),
(#53934,#53935,#53936,#53937,#53938,#53939,#53940,#53941,#53942,#53943,
#53944,#53945,#53946,#53947),(#53948,#53949,#53950,#53951,#53952,#53953,
#53954,#53955,#53956,#53957,#53958,#53959,#53960,#53961),(#53962,#53963,
#53964,#53965,#53966,#53967,#53968,#53969,#53970,#53971,#53972,#53973,#53974,
#53975),(#53976,#53977,#53978,#53979,#53980,#53981,#53982,#53983,#53984,
#53985,#53986,#53987,#53988,#53989),(#53990,#53991,#53992,#53993,#53994,
#53995,#53996,#53997,#53998,#53999,#54000,#54001,#54002,#54003),(#54004,
#54005,#54006,#54007,#54008,#54009,#54010,#54011,#54012,#54013,#54014,#54015,
#54016,#54017),(#54018,#54019,#54020,#54021,#54022,#54023,#54024,#54025,
#54026,#54027,#54028,#54029,#54030,#54031),(#54032,#54033,#54034,#54035,
#54036,#54037,#54038,#54039,#54040,#54041,#54042,#54043,#54044,#54045),
(#54046,#54047,#54048,#54049,#54050,#54051,#54052,#54053,#54054,#54055,
#54056,#54057,#54058,#54059),(#54060,#54061,#54062,#54063,#54064,#54065,
#54066,#54067,#54068,#54069,#54070,#54071,#54072,#54073),(#54074,#54075,
#54076,#54077,#54078,#54079,#54080,#54081,#54082,#54083,#54084,#54085,#54086,
#54087),(#54088,#54089,#54090,#54091,#54092,#54093,#54094,#54095,#54096,
#54097,#54098,#54099,#54100,#54101),(#54102,#54103,#54104,#54105,#54106,
#54107,#54108,#54109,#54110,#54111,#54112,#54113,#54114,#54115),(#54116,
#54117,#54118,#54119,#54120,#54121,#54122,#54123,#54124,#54125,#54126,#54127,
#54128,#54129),(#54130,#54131,#54132,#54133,#54134,#54135,#54136,#54137,
#54138,#54139,#54140,#54141,#54142,#54143),(#54144,#54145,#54146,#54147,
#54148,#54149,#54150,#54151,#54152,#54153,#54154,#54155,#54156,#54157),
(#54158,#54159,#54160,#54161,#54162,#54163,#54164,#54165,#54166,#54167,
#54168,#54169,#54170,#54171),(#54172,#54173,#54174,#54175,#54176,#54177,
#54178,#54179,#54180,#54181,#54182,#54183,#54184,#54185),(#54186,#54187,
#54188,#54189,#54190,#54191,#54192,#54193,#54194,#54195,#54196,#54197,#54198,
#54199)),.UNSPECIFIED.,.F.,.F.,.F.,(4,1,1,1,1,1,1,1,1,1,1,1,1,1,1,1,1,1,
1,1,1,1,1,1,1,1,1,1,4),(4,2,2,2,2,2,4),(0.0331549352864077,0.102215297051664,
0.171275658816921,0.173433795122085,0.175591931427249,0.179908204037578,
0.188540749258235,0.205805839699549,0.223070930140863,0.240336020582177,
0.309396382347434,0.378456744112691,0.447517105877947,0.516577467643204,
0.551107648525832,0.58563782940846,0.594270374629118,0.602902919849775,
0.620168010291089,0.654698191173717,0.689228372056345,0.723758552938974,
0.810084005145544,0.844614186028173,0.861879276469487,0.896409457352115,
0.930939638234743,0.948204728676058,1.),(0.0377143719414061,0.167070624995476,
0.336553194126115,0.499999999999991,0.663446805873868,0.832929375004528,
0.962285628058718),.UNSPECIFIED.);
#231=B_SPLINE_SURFACE_WITH_KNOTS('',3,3,((#54256,#54257,#54258,#54259,#54260,
#54261,#54262,#54263,#54264,#54265,#54266,#54267,#54268,#54269),(#54270,
#54271,#54272,#54273,#54274,#54275,#54276,#54277,#54278,#54279,#54280,#54281,
#54282,#54283),(#54284,#54285,#54286,#54287,#54288,#54289,#54290,#54291,
#54292,#54293,#54294,#54295,#54296,#54297),(#54298,#54299,#54300,#54301,
#54302,#54303,#54304,#54305,#54306,#54307,#54308,#54309,#54310,#54311)),
 .UNSPECIFIED.,.F.,.F.,.F.,(4,4),(4,2,2,2,2,2,4),(0.,1.),(0.0377143719414212,
0.167070624995476,0.336553194126115,0.499999999999991,0.663446805873868,
0.832929375004528,0.962285628058582),.UNSPECIFIED.);
#232=B_SPLINE_SURFACE_WITH_KNOTS('',3,3,((#54326,#54327,#54328,#54329,#54330,
#54331,#54332,#54333,#54334,#54335,#54336,#54337,#54338,#54339),(#54340,
#54341,#54342,#54343,#54344,#54345,#54346,#54347,#54348,#54349,#54350,#54351,
#54352,#54353),(#54354,#54355,#54356,#54357,#54358,#54359,#54360,#54361,
#54362,#54363,#54364,#54365,#54366,#54367),(#54368,#54369,#54370,#54371,
#54372,#54373,#54374,#54375,#54376,#54377,#54378,#54379,#54380,#54381),
(#54382,#54383,#54384,#54385,#54386,#54387,#54388,#54389,#54390,#54391,
#54392,#54393,#54394,#54395),(#54396,#54397,#54398,#54399,#54400,#54401,
#54402,#54403,#54404,#54405,#54406,#54407,#54408,#54409),(#54410,#54411,
#54412,#54413,#54414,#54415,#54416,#54417,#54418,#54419,#54420,#54421,#54422,
#54423),(#54424,#54425,#54426,#54427,#54428,#54429,#54430,#54431,#54432,
#54433,#54434,#54435,#54436,#54437),(#54438,#54439,#54440,#54441,#54442,
#54443,#54444,#54445,#54446,#54447,#54448,#54449,#54450,#54451),(#54452,
#54453,#54454,#54455,#54456,#54457,#54458,#54459,#54460,#54461,#54462,#54463,
#54464,#54465),(#54466,#54467,#54468,#54469,#54470,#54471,#54472,#54473,
#54474,#54475,#54476,#54477,#54478,#54479),(#54480,#54481,#54482,#54483,
#54484,#54485,#54486,#54487,#54488,#54489,#54490,#54491,#54492,#54493),
(#54494,#54495,#54496,#54497,#54498,#54499,#54500,#54501,#54502,#54503,
#54504,#54505,#54506,#54507),(#54508,#54509,#54510,#54511,#54512,#54513,
#54514,#54515,#54516,#54517,#54518,#54519,#54520,#54521),(#54522,#54523,
#54524,#54525,#54526,#54527,#54528,#54529,#54530,#54531,#54532,#54533,#54534,
#54535),(#54536,#54537,#54538,#54539,#54540,#54541,#54542,#54543,#54544,
#54545,#54546,#54547,#54548,#54549),(#54550,#54551,#54552,#54553,#54554,
#54555,#54556,#54557,#54558,#54559,#54560,#54561,#54562,#54563),(#54564,
#54565,#54566,#54567,#54568,#54569,#54570,#54571,#54572,#54573,#54574,#54575,
#54576,#54577),(#54578,#54579,#54580,#54581,#54582,#54583,#54584,#54585,
#54586,#54587,#54588,#54589,#54590,#54591),(#54592,#54593,#54594,#54595,
#54596,#54597,#54598,#54599,#54600,#54601,#54602,#54603,#54604,#54605),
(#54606,#54607,#54608,#54609,#54610,#54611,#54612,#54613,#54614,#54615,
#54616,#54617,#54618,#54619),(#54620,#54621,#54622,#54623,#54624,#54625,
#54626,#54627,#54628,#54629,#54630,#54631,#54632,#54633),(#54634,#54635,
#54636,#54637,#54638,#54639,#54640,#54641,#54642,#54643,#54644,#54645,#54646,
#54647),(#54648,#54649,#54650,#54651,#54652,#54653,#54654,#54655,#54656,
#54657,#54658,#54659,#54660,#54661),(#54662,#54663,#54664,#54665,#54666,
#54667,#54668,#54669,#54670,#54671,#54672,#54673,#54674,#54675),(#54676,
#54677,#54678,#54679,#54680,#54681,#54682,#54683,#54684,#54685,#54686,#54687,
#54688,#54689),(#54690,#54691,#54692,#54693,#54694,#54695,#54696,#54697,
#54698,#54699,#54700,#54701,#54702,#54703),(#54704,#54705,#54706,#54707,
#54708,#54709,#54710,#54711,#54712,#54713,#54714,#54715,#54716,#54717),
(#54718,#54719,#54720,#54721,#54722,#54723,#54724,#54725,#54726,#54727,
#54728,#54729,#54730,#54731),(#54732,#54733,#54734,#54735,#54736,#54737,
#54738,#54739,#54740,#54741,#54742,#54743,#54744,#54745),(#54746,#54747,
#54748,#54749,#54750,#54751,#54752,#54753,#54754,#54755,#54756,#54757,#54758,
#54759)),.UNSPECIFIED.,.F.,.F.,.F.,(4,1,1,1,1,1,1,1,1,1,1,1,1,1,1,1,1,1,
1,1,1,1,1,1,1,1,1,1,4),(4,2,2,2,2,2,4),(0.,0.0517952713240543,0.0690603617654058,
0.103590542648109,0.138120723530812,0.155385813972163,0.189915994854866,
0.276241447061623,0.345301808827029,0.414362170592435,0.431627261033786,
0.448892351475138,0.48342253235784,0.517952713240543,0.552482894123246,
0.587013075005949,0.621543255888652,0.690603617654058,0.699236162874733,
0.725133798536761,0.759663979419464,0.794194160302166,0.811459250743518,
0.820091795964194,0.824408068574531,0.8265662048797,0.828724341184869,0.897784702950275,
0.966845064715681),(0.0377143719405064,0.167070624995476,0.336553194126115,
0.499999999999991,0.663446805873868,0.832929375004528,0.962285628058607),
 .UNSPECIFIED.);
#233=B_SPLINE_SURFACE_WITH_KNOTS('',3,3,((#54817,#54818,#54819,#54820,#54821,
#54822,#54823,#54824,#54825,#54826,#54827,#54828,#54829,#54830),(#54831,
#54832,#54833,#54834,#54835,#54836,#54837,#54838,#54839,#54840,#54841,#54842,
#54843,#54844),(#54845,#54846,#54847,#54848,#54849,#54850,#54851,#54852,
#54853,#54854,#54855,#54856,#54857,#54858),(#54859,#54860,#54861,#54862,
#54863,#54864,#54865,#54866,#54867,#54868,#54869,#54870,#54871,#54872),
(#54873,#54874,#54875,#54876,#54877,#54878,#54879,#54880,#54881,#54882,
#54883,#54884,#54885,#54886),(#54887,#54888,#54889,#54890,#54891,#54892,
#54893,#54894,#54895,#54896,#54897,#54898,#54899,#54900),(#54901,#54902,
#54903,#54904,#54905,#54906,#54907,#54908,#54909,#54910,#54911,#54912,#54913,
#54914),(#54915,#54916,#54917,#54918,#54919,#54920,#54921,#54922,#54923,
#54924,#54925,#54926,#54927,#54928),(#54929,#54930,#54931,#54932,#54933,
#54934,#54935,#54936,#54937,#54938,#54939,#54940,#54941,#54942),(#54943,
#54944,#54945,#54946,#54947,#54948,#54949,#54950,#54951,#54952,#54953,#54954,
#54955,#54956),(#54957,#54958,#54959,#54960,#54961,#54962,#54963,#54964,
#54965,#54966,#54967,#54968,#54969,#54970),(#54971,#54972,#54973,#54974,
#54975,#54976,#54977,#54978,#54979,#54980,#54981,#54982,#54983,#54984),
(#54985,#54986,#54987,#54988,#54989,#54990,#54991,#54992,#54993,#54994,
#54995,#54996,#54997,#54998),(#54999,#55000,#55001,#55002,#55003,#55004,
#55005,#55006,#55007,#55008,#55009,#55010,#55011,#55012),(#55013,#55014,
#55015,#55016,#55017,#55018,#55019,#55020,#55021,#55022,#55023,#55024,#55025,
#55026),(#55027,#55028,#55029,#55030,#55031,#55032,#55033,#55034,#55035,
#55036,#55037,#55038,#55039,#55040),(#55041,#55042,#55043,#55044,#55045,
#55046,#55047,#55048,#55049,#55050,#55051,#55052,#55053,#55054),(#55055,
#55056,#55057,#55058,#55059,#55060,#55061,#55062,#55063,#55064,#55065,#55066,
#55067,#55068),(#55069,#55070,#55071,#55072,#55073,#55074,#55075,#55076,
#55077,#55078,#55079,#55080,#55081,#55082),(#55083,#55084,#55085,#55086,
#55087,#55088,#55089,#55090,#55091,#55092,#55093,#55094,#55095,#55096),
(#55097,#55098,#55099,#55100,#55101,#55102,#55103,#55104,#55105,#55106,
#55107,#55108,#55109,#55110),(#55111,#55112,#55113,#55114,#55115,#55116,
#55117,#55118,#55119,#55120,#55121,#55122,#55123,#55124),(#55125,#55126,
#55127,#55128,#55129,#55130,#55131,#55132,#55133,#55134,#55135,#55136,#55137,
#55138),(#55139,#55140,#55141,#55142,#55143,#55144,#55145,#55146,#55147,
#55148,#55149,#55150,#55151,#55152),(#55153,#55154,#55155,#55156,#55157,
#55158,#55159,#55160,#55161,#55162,#55163,#55164,#55165,#55166),(#55167,
#55168,#55169,#55170,#55171,#55172,#55173,#55174,#55175,#55176,#55177,#55178,
#55179,#55180),(#55181,#55182,#55183,#55184,#55185,#55186,#55187,#55188,
#55189,#55190,#55191,#55192,#55193,#55194),(#55195,#55196,#55197,#55198,
#55199,#55200,#55201,#55202,#55203,#55204,#55205,#55206,#55207,#55208),
(#55209,#55210,#55211,#55212,#55213,#55214,#55215,#55216,#55217,#55218,
#55219,#55220,#55221,#55222),(#55223,#55224,#55225,#55226,#55227,#55228,
#55229,#55230,#55231,#55232,#55233,#55234,#55235,#55236),(#55237,#55238,
#55239,#55240,#55241,#55242,#55243,#55244,#55245,#55246,#55247,#55248,#55249,
#55250),(#55251,#55252,#55253,#55254,#55255,#55256,#55257,#55258,#55259,
#55260,#55261,#55262,#55263,#55264),(#55265,#55266,#55267,#55268,#55269,
#55270,#55271,#55272,#55273,#55274,#55275,#55276,#55277,#55278)),
 .UNSPECIFIED.,.F.,.F.,.F.,(4,1,1,1,1,1,1,1,1,1,1,1,1,1,1,1,1,1,1,1,1,1,
1,1,1,1,1,1,1,1,4),(4,2,2,2,2,2,4),(0.0331549352864095,0.102215297051666,
0.171275658816922,0.172354726969505,0.173433795122087,0.175591931427251,
0.179908204037579,0.188540749258237,0.205805839699551,0.223070930140865,
0.240336020582179,0.274866201464807,0.309396382347435,0.378456744112692,
0.395721834554006,0.447517105877948,0.516577467643205,0.525210012863862,
0.551107648525833,0.568372738967147,0.577005284187804,0.585637829408461,
0.723758552938974,0.79281891470423,0.827349095586859,0.844614186028173,
0.861879276469487,0.896409457352115,0.930939638234743,0.948204728676058,
1.),(0.0377143719411004,0.167070624995476,0.336553194126115,0.499999999999991,
0.663446805873868,0.832929375004528,0.962285628058762),.UNSPECIFIED.);
#234=B_SPLINE_SURFACE_WITH_KNOTS('',3,3,((#55335,#55336,#55337,#55338,#55339,
#55340,#55341,#55342,#55343,#55344,#55345,#55346,#55347,#55348),(#55349,
#55350,#55351,#55352,#55353,#55354,#55355,#55356,#55357,#55358,#55359,#55360,
#55361,#55362),(#55363,#55364,#55365,#55366,#55367,#55368,#55369,#55370,
#55371,#55372,#55373,#55374,#55375,#55376),(#55377,#55378,#55379,#55380,
#55381,#55382,#55383,#55384,#55385,#55386,#55387,#55388,#55389,#55390)),
 .UNSPECIFIED.,.F.,.F.,.F.,(4,4),(4,2,2,2,2,2,4),(0.,1.),(0.0377143719414212,
0.167070624995476,0.336553194126115,0.499999999999991,0.663446805873868,
0.832929375004528,0.962285628058582),.UNSPECIFIED.);
#235=B_SPLINE_SURFACE_WITH_KNOTS('',3,3,((#55405,#55406,#55407,#55408,#55409,
#55410,#55411,#55412,#55413,#55414,#55415,#55416,#55417,#55418),(#55419,
#55420,#55421,#55422,#55423,#55424,#55425,#55426,#55427,#55428,#55429,#55430,
#55431,#55432),(#55433,#55434,#55435,#55436,#55437,#55438,#55439,#55440,
#55441,#55442,#55443,#55444,#55445,#55446),(#55447,#55448,#55449,#55450,
#55451,#55452,#55453,#55454,#55455,#55456,#55457,#55458,#55459,#55460),
(#55461,#55462,#55463,#55464,#55465,#55466,#55467,#55468,#55469,#55470,
#55471,#55472,#55473,#55474),(#55475,#55476,#55477,#55478,#55479,#55480,
#55481,#55482,#55483,#55484,#55485,#55486,#55487,#55488),(#55489,#55490,
#55491,#55492,#55493,#55494,#55495,#55496,#55497,#55498,#55499,#55500,#55501,
#55502),(#55503,#55504,#55505,#55506,#55507,#55508,#55509,#55510,#55511,
#55512,#55513,#55514,#55515,#55516),(#55517,#55518,#55519,#55520,#55521,
#55522,#55523,#55524,#55525,#55526,#55527,#55528,#55529,#55530),(#55531,
#55532,#55533,#55534,#55535,#55536,#55537,#55538,#55539,#55540,#55541,#55542,
#55543,#55544),(#55545,#55546,#55547,#55548,#55549,#55550,#55551,#55552,
#55553,#55554,#55555,#55556,#55557,#55558),(#55559,#55560,#55561,#55562,
#55563,#55564,#55565,#55566,#55567,#55568,#55569,#55570,#55571,#55572),
(#55573,#55574,#55575,#55576,#55577,#55578,#55579,#55580,#55581,#55582,
#55583,#55584,#55585,#55586),(#55587,#55588,#55589,#55590,#55591,#55592,
#55593,#55594,#55595,#55596,#55597,#55598,#55599,#55600),(#55601,#55602,
#55603,#55604,#55605,#55606,#55607,#55608,#55609,#55610,#55611,#55612,#55613,
#55614),(#55615,#55616,#55617,#55618,#55619,#55620,#55621,#55622,#55623,
#55624,#55625,#55626,#55627,#55628),(#55629,#55630,#55631,#55632,#55633,
#55634,#55635,#55636,#55637,#55638,#55639,#55640,#55641,#55642),(#55643,
#55644,#55645,#55646,#55647,#55648,#55649,#55650,#55651,#55652,#55653,#55654,
#55655,#55656),(#55657,#55658,#55659,#55660,#55661,#55662,#55663,#55664,
#55665,#55666,#55667,#55668,#55669,#55670),(#55671,#55672,#55673,#55674,
#55675,#55676,#55677,#55678,#55679,#55680,#55681,#55682,#55683,#55684),
(#55685,#55686,#55687,#55688,#55689,#55690,#55691,#55692,#55693,#55694,
#55695,#55696,#55697,#55698),(#55699,#55700,#55701,#55702,#55703,#55704,
#55705,#55706,#55707,#55708,#55709,#55710,#55711,#55712),(#55713,#55714,
#55715,#55716,#55717,#55718,#55719,#55720,#55721,#55722,#55723,#55724,#55725,
#55726),(#55727,#55728,#55729,#55730,#55731,#55732,#55733,#55734,#55735,
#55736,#55737,#55738,#55739,#55740),(#55741,#55742,#55743,#55744,#55745,
#55746,#55747,#55748,#55749,#55750,#55751,#55752,#55753,#55754),(#55755,
#55756,#55757,#55758,#55759,#55760,#55761,#55762,#55763,#55764,#55765,#55766,
#55767,#55768),(#55769,#55770,#55771,#55772,#55773,#55774,#55775,#55776,
#55777,#55778,#55779,#55780,#55781,#55782),(#55783,#55784,#55785,#55786,
#55787,#55788,#55789,#55790,#55791,#55792,#55793,#55794,#55795,#55796),
(#55797,#55798,#55799,#55800,#55801,#55802,#55803,#55804,#55805,#55806,
#55807,#55808,#55809,#55810),(#55811,#55812,#55813,#55814,#55815,#55816,
#55817,#55818,#55819,#55820,#55821,#55822,#55823,#55824),(#55825,#55826,
#55827,#55828,#55829,#55830,#55831,#55832,#55833,#55834,#55835,#55836,#55837,
#55838)),.UNSPECIFIED.,.F.,.F.,.F.,(4,1,1,1,1,1,1,1,1,1,1,1,1,1,1,1,1,1,
1,1,1,1,1,1,1,1,1,1,4),(4,2,2,2,2,2,4),(0.,0.0517952713240543,0.0690603617654058,
0.103590542648109,0.138120723530812,0.155385813972163,0.189915994854866,
0.276241447061623,0.345301808827029,0.414362170592435,0.431627261033786,
0.448892351475138,0.48342253235784,0.517952713240543,0.552482894123246,
0.587013075005949,0.621543255888652,0.690603617654058,0.699236162874733,
0.725133798536761,0.759663979419464,0.794194160302166,0.811459250743518,
0.820091795964194,0.824408068574531,0.8265662048797,0.828724341184869,0.897784702950275,
0.966845064715681),(0.0377143719395592,0.167070624995476,0.336553194126115,
0.499999999999991,0.663446805873868,0.832929375004528,0.962285628060022),
 .UNSPECIFIED.);
#236=B_SPLINE_SURFACE_WITH_KNOTS('',3,3,((#55896,#55897,#55898,#55899,#55900,
#55901,#55902,#55903,#55904,#55905,#55906,#55907,#55908,#55909),(#55910,
#55911,#55912,#55913,#55914,#55915,#55916,#55917,#55918,#55919,#55920,#55921,
#55922,#55923),(#55924,#55925,#55926,#55927,#55928,#55929,#55930,#55931,
#55932,#55933,#55934,#55935,#55936,#55937),(#55938,#55939,#55940,#55941,
#55942,#55943,#55944,#55945,#55946,#55947,#55948,#55949,#55950,#55951),
(#55952,#55953,#55954,#55955,#55956,#55957,#55958,#55959,#55960,#55961,
#55962,#55963,#55964,#55965),(#55966,#55967,#55968,#55969,#55970,#55971,
#55972,#55973,#55974,#55975,#55976,#55977,#55978,#55979),(#55980,#55981,
#55982,#55983,#55984,#55985,#55986,#55987,#55988,#55989,#55990,#55991,#55992,
#55993),(#55994,#55995,#55996,#55997,#55998,#55999,#56000,#56001,#56002,
#56003,#56004,#56005,#56006,#56007),(#56008,#56009,#56010,#56011,#56012,
#56013,#56014,#56015,#56016,#56017,#56018,#56019,#56020,#56021),(#56022,
#56023,#56024,#56025,#56026,#56027,#56028,#56029,#56030,#56031,#56032,#56033,
#56034,#56035),(#56036,#56037,#56038,#56039,#56040,#56041,#56042,#56043,
#56044,#56045,#56046,#56047,#56048,#56049),(#56050,#56051,#56052,#56053,
#56054,#56055,#56056,#56057,#56058,#56059,#56060,#56061,#56062,#56063),
(#56064,#56065,#56066,#56067,#56068,#56069,#56070,#56071,#56072,#56073,
#56074,#56075,#56076,#56077),(#56078,#56079,#56080,#56081,#56082,#56083,
#56084,#56085,#56086,#56087,#56088,#56089,#56090,#56091),(#56092,#56093,
#56094,#56095,#56096,#56097,#56098,#56099,#56100,#56101,#56102,#56103,#56104,
#56105),(#56106,#56107,#56108,#56109,#56110,#56111,#56112,#56113,#56114,
#56115,#56116,#56117,#56118,#56119),(#56120,#56121,#56122,#56123,#56124,
#56125,#56126,#56127,#56128,#56129,#56130,#56131,#56132,#56133),(#56134,
#56135,#56136,#56137,#56138,#56139,#56140,#56141,#56142,#56143,#56144,#56145,
#56146,#56147),(#56148,#56149,#56150,#56151,#56152,#56153,#56154,#56155,
#56156,#56157,#56158,#56159,#56160,#56161),(#56162,#56163,#56164,#56165,
#56166,#56167,#56168,#56169,#56170,#56171,#56172,#56173,#56174,#56175),
(#56176,#56177,#56178,#56179,#56180,#56181,#56182,#56183,#56184,#56185,
#56186,#56187,#56188,#56189),(#56190,#56191,#56192,#56193,#56194,#56195,
#56196,#56197,#56198,#56199,#56200,#56201,#56202,#56203),(#56204,#56205,
#56206,#56207,#56208,#56209,#56210,#56211,#56212,#56213,#56214,#56215,#56216,
#56217),(#56218,#56219,#56220,#56221,#56222,#56223,#56224,#56225,#56226,
#56227,#56228,#56229,#56230,#56231),(#56232,#56233,#56234,#56235,#56236,
#56237,#56238,#56239,#56240,#56241,#56242,#56243,#56244,#56245),(#56246,
#56247,#56248,#56249,#56250,#56251,#56252,#56253,#56254,#56255,#56256,#56257,
#56258,#56259),(#56260,#56261,#56262,#56263,#56264,#56265,#56266,#56267,
#56268,#56269,#56270,#56271,#56272,#56273),(#56274,#56275,#56276,#56277,
#56278,#56279,#56280,#56281,#56282,#56283,#56284,#56285,#56286,#56287),
(#56288,#56289,#56290,#56291,#56292,#56293,#56294,#56295,#56296,#56297,
#56298,#56299,#56300,#56301),(#56302,#56303,#56304,#56305,#56306,#56307,
#56308,#56309,#56310,#56311,#56312,#56313,#56314,#56315),(#56316,#56317,
#56318,#56319,#56320,#56321,#56322,#56323,#56324,#56325,#56326,#56327,#56328,
#56329),(#56330,#56331,#56332,#56333,#56334,#56335,#56336,#56337,#56338,
#56339,#56340,#56341,#56342,#56343),(#56344,#56345,#56346,#56347,#56348,
#56349,#56350,#56351,#56352,#56353,#56354,#56355,#56356,#56357),(#56358,
#56359,#56360,#56361,#56362,#56363,#56364,#56365,#56366,#56367,#56368,#56369,
#56370,#56371),(#56372,#56373,#56374,#56375,#56376,#56377,#56378,#56379,
#56380,#56381,#56382,#56383,#56384,#56385),(#56386,#56387,#56388,#56389,
#56390,#56391,#56392,#56393,#56394,#56395,#56396,#56397,#56398,#56399),
(#56400,#56401,#56402,#56403,#56404,#56405,#56406,#56407,#56408,#56409,
#56410,#56411,#56412,#56413),(#56414,#56415,#56416,#56417,#56418,#56419,
#56420,#56421,#56422,#56423,#56424,#56425,#56426,#56427),(#56428,#56429,
#56430,#56431,#56432,#56433,#56434,#56435,#56436,#56437,#56438,#56439,#56440,
#56441),(#56442,#56443,#56444,#56445,#56446,#56447,#56448,#56449,#56450,
#56451,#56452,#56453,#56454,#56455),(#56456,#56457,#56458,#56459,#56460,
#56461,#56462,#56463,#56464,#56465,#56466,#56467,#56468,#56469),(#56470,
#56471,#56472,#56473,#56474,#56475,#56476,#56477,#56478,#56479,#56480,#56481,
#56482,#56483),(#56484,#56485,#56486,#56487,#56488,#56489,#56490,#56491,
#56492,#56493,#56494,#56495,#56496,#56497)),.UNSPECIFIED.,.F.,.F.,.F.,(4,
1,1,1,1,1,1,1,1,1,1,1,1,1,1,1,1,1,1,1,1,1,1,1,1,1,1,1,1,1,1,1,1,1,1,1,1,
1,1,1,4),(4,2,2,2,2,2,4),(0.0331549352864066,0.067685116169035,0.102215297051663,
0.136745477934292,0.17127565881692,0.171815192893211,0.172354726969502,
0.173433795122084,0.175591931427249,0.179908204037577,0.184224476647906,
0.188540749258234,0.205805839699548,0.214438384920205,0.240336020582177,
0.274866201464805,0.309396382347433,0.37845674411269,0.412986924995318,
0.430252015436632,0.43888456065729,0.443200833267618,0.445358969572782,
0.446438037725365,0.447517105877947,0.482047286760575,0.516577467643203,
0.551107648525832,0.58563782940846,0.620168010291088,0.654698191173717,
0.689228372056345,0.723758552938973,0.79281891470423,0.827349095586858,
0.844614186028173,0.861879276469487,0.896409457352115,0.930939638234743,
0.948204728676058,1.),(0.0377143719407316,0.167070624995476,0.336553194126115,
0.499999999999991,0.663446805873868,0.832929375004528,0.962285628060079),
 .UNSPECIFIED.);
#237=B_SPLINE_SURFACE_WITH_KNOTS('',3,3,((#56560,#56561,#56562,#56563,#56564,
#56565,#56566,#56567,#56568,#56569,#56570,#56571,#56572,#56573),(#56574,
#56575,#56576,#56577,#56578,#56579,#56580,#56581,#56582,#56583,#56584,#56585,
#56586,#56587),(#56588,#56589,#56590,#56591,#56592,#56593,#56594,#56595,
#56596,#56597,#56598,#56599,#56600,#56601),(#56602,#56603,#56604,#56605,
#56606,#56607,#56608,#56609,#56610,#56611,#56612,#56613,#56614,#56615)),
 .UNSPECIFIED.,.F.,.F.,.F.,(4,4),(4,2,2,2,2,2,4),(0.,1.),(0.0377143719414212,
0.167070624995476,0.336553194126115,0.499999999999991,0.663446805873868,
0.832929375004528,0.962285628058582),.UNSPECIFIED.);
#238=B_SPLINE_SURFACE_WITH_KNOTS('',3,3,((#56630,#56631,#56632,#56633,#56634,
#56635,#56636,#56637,#56638,#56639,#56640,#56641,#56642,#56643),(#56644,
#56645,#56646,#56647,#56648,#56649,#56650,#56651,#56652,#56653,#56654,#56655,
#56656,#56657),(#56658,#56659,#56660,#56661,#56662,#56663,#56664,#56665,
#56666,#56667,#56668,#56669,#56670,#56671),(#56672,#56673,#56674,#56675,
#56676,#56677,#56678,#56679,#56680,#56681,#56682,#56683,#56684,#56685),
(#56686,#56687,#56688,#56689,#56690,#56691,#56692,#56693,#56694,#56695,
#56696,#56697,#56698,#56699),(#56700,#56701,#56702,#56703,#56704,#56705,
#56706,#56707,#56708,#56709,#56710,#56711,#56712,#56713),(#56714,#56715,
#56716,#56717,#56718,#56719,#56720,#56721,#56722,#56723,#56724,#56725,#56726,
#56727),(#56728,#56729,#56730,#56731,#56732,#56733,#56734,#56735,#56736,
#56737,#56738,#56739,#56740,#56741),(#56742,#56743,#56744,#56745,#56746,
#56747,#56748,#56749,#56750,#56751,#56752,#56753,#56754,#56755),(#56756,
#56757,#56758,#56759,#56760,#56761,#56762,#56763,#56764,#56765,#56766,#56767,
#56768,#56769),(#56770,#56771,#56772,#56773,#56774,#56775,#56776,#56777,
#56778,#56779,#56780,#56781,#56782,#56783),(#56784,#56785,#56786,#56787,
#56788,#56789,#56790,#56791,#56792,#56793,#56794,#56795,#56796,#56797),
(#56798,#56799,#56800,#56801,#56802,#56803,#56804,#56805,#56806,#56807,
#56808,#56809,#56810,#56811),(#56812,#56813,#56814,#56815,#56816,#56817,
#56818,#56819,#56820,#56821,#56822,#56823,#56824,#56825),(#56826,#56827,
#56828,#56829,#56830,#56831,#56832,#56833,#56834,#56835,#56836,#56837,#56838,
#56839),(#56840,#56841,#56842,#56843,#56844,#56845,#56846,#56847,#56848,
#56849,#56850,#56851,#56852,#56853),(#56854,#56855,#56856,#56857,#56858,
#56859,#56860,#56861,#56862,#56863,#56864,#56865,#56866,#56867),(#56868,
#56869,#56870,#56871,#56872,#56873,#56874,#56875,#56876,#56877,#56878,#56879,
#56880,#56881),(#56882,#56883,#56884,#56885,#56886,#56887,#56888,#56889,
#56890,#56891,#56892,#56893,#56894,#56895),(#56896,#56897,#56898,#56899,
#56900,#56901,#56902,#56903,#56904,#56905,#56906,#56907,#56908,#56909),
(#56910,#56911,#56912,#56913,#56914,#56915,#56916,#56917,#56918,#56919,
#56920,#56921,#56922,#56923),(#56924,#56925,#56926,#56927,#56928,#56929,
#56930,#56931,#56932,#56933,#56934,#56935,#56936,#56937),(#56938,#56939,
#56940,#56941,#56942,#56943,#56944,#56945,#56946,#56947,#56948,#56949,#56950,
#56951),(#56952,#56953,#56954,#56955,#56956,#56957,#56958,#56959,#56960,
#56961,#56962,#56963,#56964,#56965),(#56966,#56967,#56968,#56969,#56970,
#56971,#56972,#56973,#56974,#56975,#56976,#56977,#56978,#56979),(#56980,
#56981,#56982,#56983,#56984,#56985,#56986,#56987,#56988,#56989,#56990,#56991,
#56992,#56993),(#56994,#56995,#56996,#56997,#56998,#56999,#57000,#57001,
#57002,#57003,#57004,#57005,#57006,#57007),(#57008,#57009,#57010,#57011,
#57012,#57013,#57014,#57015,#57016,#57017,#57018,#57019,#57020,#57021),
(#57022,#57023,#57024,#57025,#57026,#57027,#57028,#57029,#57030,#57031,
#57032,#57033,#57034,#57035),(#57036,#57037,#57038,#57039,#57040,#57041,
#57042,#57043,#57044,#57045,#57046,#57047,#57048,#57049),(#57050,#57051,
#57052,#57053,#57054,#57055,#57056,#57057,#57058,#57059,#57060,#57061,#57062,
#57063),(#57064,#57065,#57066,#57067,#57068,#57069,#57070,#57071,#57072,
#57073,#57074,#57075,#57076,#57077),(#57078,#57079,#57080,#57081,#57082,
#57083,#57084,#57085,#57086,#57087,#57088,#57089,#57090,#57091),(#57092,
#57093,#57094,#57095,#57096,#57097,#57098,#57099,#57100,#57101,#57102,#57103,
#57104,#57105),(#57106,#57107,#57108,#57109,#57110,#57111,#57112,#57113,
#57114,#57115,#57116,#57117,#57118,#57119),(#57120,#57121,#57122,#57123,
#57124,#57125,#57126,#57127,#57128,#57129,#57130,#57131,#57132,#57133),
(#57134,#57135,#57136,#57137,#57138,#57139,#57140,#57141,#57142,#57143,
#57144,#57145,#57146,#57147),(#57148,#57149,#57150,#57151,#57152,#57153,
#57154,#57155,#57156,#57157,#57158,#57159,#57160,#57161),(#57162,#57163,
#57164,#57165,#57166,#57167,#57168,#57169,#57170,#57171,#57172,#57173,#57174,
#57175),(#57176,#57177,#57178,#57179,#57180,#57181,#57182,#57183,#57184,
#57185,#57186,#57187,#57188,#57189)),.UNSPECIFIED.,.F.,.F.,.F.,(4,1,1,1,
1,1,1,1,1,1,1,1,1,1,1,1,1,1,1,1,1,1,1,1,1,1,1,1,1,1,1,1,1,1,1,1,1,4),(4,
2,2,2,2,2,4),(0.,0.0517952713240546,0.0690603617654061,0.103590542648109,
0.138120723530812,0.172650904413515,0.207181085296218,0.276241447061624,
0.414362170592437,0.483422532357843,0.48773880496818,0.492055077578518,
0.500687622799194,0.517952713240546,0.552482894123249,0.621543255888655,
0.638808346330006,0.690603617654061,0.759663979419467,0.768296524640143,
0.772612797250481,0.776929069860818,0.785561615081494,0.79419416030217,
0.802826705522846,0.811459250743522,0.81361738704869,0.815775523353859,
0.820091795964197,0.824408068574535,0.82548713672712,0.826566204879704,
0.827645273032289,0.828184807108581,0.828454574146727,0.828724341184873,
0.897784702950279,0.966845064715685),(0.0377143719407368,0.167070624995476,
0.336553194126115,0.499999999999991,0.663446805873868,0.832929375004528,
0.96228562805882),.UNSPECIFIED.);
#239=B_SPLINE_SURFACE_WITH_KNOTS('',3,3,((#57243,#57244,#57245,#57246,#57247,
#57248,#57249,#57250,#57251,#57252,#57253,#57254,#57255,#57256),(#57257,
#57258,#57259,#57260,#57261,#57262,#57263,#57264,#57265,#57266,#57267,#57268,
#57269,#57270),(#57271,#57272,#57273,#57274,#57275,#57276,#57277,#57278,
#57279,#57280,#57281,#57282,#57283,#57284),(#57285,#57286,#57287,#57288,
#57289,#57290,#57291,#57292,#57293,#57294,#57295,#57296,#57297,#57298),
(#57299,#57300,#57301,#57302,#57303,#57304,#57305,#57306,#57307,#57308,
#57309,#57310,#57311,#57312),(#57313,#57314,#57315,#57316,#57317,#57318,
#57319,#57320,#57321,#57322,#57323,#57324,#57325,#57326),(#57327,#57328,
#57329,#57330,#57331,#57332,#57333,#57334,#57335,#57336,#57337,#57338,#57339,
#57340),(#57341,#57342,#57343,#57344,#57345,#57346,#57347,#57348,#57349,
#57350,#57351,#57352,#57353,#57354),(#57355,#57356,#57357,#57358,#57359,
#57360,#57361,#57362,#57363,#57364,#57365,#57366,#57367,#57368),(#57369,
#57370,#57371,#57372,#57373,#57374,#57375,#57376,#57377,#57378,#57379,#57380,
#57381,#57382),(#57383,#57384,#57385,#57386,#57387,#57388,#57389,#57390,
#57391,#57392,#57393,#57394,#57395,#57396),(#57397,#57398,#57399,#57400,
#57401,#57402,#57403,#57404,#57405,#57406,#57407,#57408,#57409,#57410),
(#57411,#57412,#57413,#57414,#57415,#57416,#57417,#57418,#57419,#57420,
#57421,#57422,#57423,#57424),(#57425,#57426,#57427,#57428,#57429,#57430,
#57431,#57432,#57433,#57434,#57435,#57436,#57437,#57438),(#57439,#57440,
#57441,#57442,#57443,#57444,#57445,#57446,#57447,#57448,#57449,#57450,#57451,
#57452),(#57453,#57454,#57455,#57456,#57457,#57458,#57459,#57460,#57461,
#57462,#57463,#57464,#57465,#57466),(#57467,#57468,#57469,#57470,#57471,
#57472,#57473,#57474,#57475,#57476,#57477,#57478,#57479,#57480),(#57481,
#57482,#57483,#57484,#57485,#57486,#57487,#57488,#57489,#57490,#57491,#57492,
#57493,#57494),(#57495,#57496,#57497,#57498,#57499,#57500,#57501,#57502,
#57503,#57504,#57505,#57506,#57507,#57508),(#57509,#57510,#57511,#57512,
#57513,#57514,#57515,#57516,#57517,#57518,#57519,#57520,#57521,#57522),
(#57523,#57524,#57525,#57526,#57527,#57528,#57529,#57530,#57531,#57532,
#57533,#57534,#57535,#57536),(#57537,#57538,#57539,#57540,#57541,#57542,
#57543,#57544,#57545,#57546,#57547,#57548,#57549,#57550),(#57551,#57552,
#57553,#57554,#57555,#57556,#57557,#57558,#57559,#57560,#57561,#57562,#57563,
#57564),(#57565,#57566,#57567,#57568,#57569,#57570,#57571,#57572,#57573,
#57574,#57575,#57576,#57577,#57578),(#57579,#57580,#57581,#57582,#57583,
#57584,#57585,#57586,#57587,#57588,#57589,#57590,#57591,#57592),(#57593,
#57594,#57595,#57596,#57597,#57598,#57599,#57600,#57601,#57602,#57603,#57604,
#57605,#57606),(#57607,#57608,#57609,#57610,#57611,#57612,#57613,#57614,
#57615,#57616,#57617,#57618,#57619,#57620),(#57621,#57622,#57623,#57624,
#57625,#57626,#57627,#57628,#57629,#57630,#57631,#57632,#57633,#57634),
(#57635,#57636,#57637,#57638,#57639,#57640,#57641,#57642,#57643,#57644,
#57645,#57646,#57647,#57648),(#57649,#57650,#57651,#57652,#57653,#57654,
#57655,#57656,#57657,#57658,#57659,#57660,#57661,#57662),(#57663,#57664,
#57665,#57666,#57667,#57668,#57669,#57670,#57671,#57672,#57673,#57674,#57675,
#57676),(#57677,#57678,#57679,#57680,#57681,#57682,#57683,#57684,#57685,
#57686,#57687,#57688,#57689,#57690),(#57691,#57692,#57693,#57694,#57695,
#57696,#57697,#57698,#57699,#57700,#57701,#57702,#57703,#57704),(#57705,
#57706,#57707,#57708,#57709,#57710,#57711,#57712,#57713,#57714,#57715,#57716,
#57717,#57718),(#57719,#57720,#57721,#57722,#57723,#57724,#57725,#57726,
#57727,#57728,#57729,#57730,#57731,#57732),(#57733,#57734,#57735,#57736,
#57737,#57738,#57739,#57740,#57741,#57742,#57743,#57744,#57745,#57746)),
 .UNSPECIFIED.,.F.,.F.,.F.,(4,1,1,1,1,1,1,1,1,1,1,1,1,1,1,1,1,1,1,1,1,1,
1,1,1,1,1,1,1,1,1,1,1,4),(4,2,2,2,2,2,4),(0.0331549352864083,0.0676851161690366,
0.102215297051665,0.171275658816921,0.172354726969504,0.173433795122086,
0.174512863274668,0.17559193142725,0.179908204037579,0.188540749258236,
0.197173294478893,0.20580583969955,0.223070930140864,0.240336020582178,
0.274866201464806,0.309396382347435,0.378456744112691,0.412986924995319,
0.447517105877948,0.482047286760576,0.516577467643204,0.551107648525832,
0.568372738967147,0.585637829408461,0.654698191173717,0.70649346249766,
0.723758552938974,0.79281891470423,0.827349095586859,0.861879276469487,
0.896409457352115,0.930939638234743,0.948204728676058,1.),(0.037714371941404,
0.167070624995476,0.336553194126115,0.499999999999991,0.663446805873868,
0.832929375004528,0.962285628059334),.UNSPECIFIED.);
#240=B_SPLINE_SURFACE_WITH_KNOTS('',3,3,((#57811,#57812,#57813,#57814,#57815,
#57816,#57817,#57818,#57819,#57820,#57821,#57822,#57823,#57824),(#57825,
#57826,#57827,#57828,#57829,#57830,#57831,#57832,#57833,#57834,#57835,#57836,
#57837,#57838),(#57839,#57840,#57841,#57842,#57843,#57844,#57845,#57846,
#57847,#57848,#57849,#57850,#57851,#57852),(#57853,#57854,#57855,#57856,
#57857,#57858,#57859,#57860,#57861,#57862,#57863,#57864,#57865,#57866)),
 .UNSPECIFIED.,.F.,.F.,.F.,(4,4),(4,2,2,2,2,2,4),(0.,1.),(0.0377143719414212,
0.167070624995476,0.336553194126115,0.499999999999991,0.663446805873868,
0.832929375004528,0.962285628058582),.UNSPECIFIED.);
#241=B_SPLINE_SURFACE_WITH_KNOTS('',3,3,((#57881,#57882,#57883,#57884,#57885,
#57886,#57887,#57888,#57889,#57890,#57891,#57892,#57893,#57894),(#57895,
#57896,#57897,#57898,#57899,#57900,#57901,#57902,#57903,#57904,#57905,#57906,
#57907,#57908),(#57909,#57910,#57911,#57912,#57913,#57914,#57915,#57916,
#57917,#57918,#57919,#57920,#57921,#57922),(#57923,#57924,#57925,#57926,
#57927,#57928,#57929,#57930,#57931,#57932,#57933,#57934,#57935,#57936),
(#57937,#57938,#57939,#57940,#57941,#57942,#57943,#57944,#57945,#57946,
#57947,#57948,#57949,#57950),(#57951,#57952,#57953,#57954,#57955,#57956,
#57957,#57958,#57959,#57960,#57961,#57962,#57963,#57964),(#57965,#57966,
#57967,#57968,#57969,#57970,#57971,#57972,#57973,#57974,#57975,#57976,#57977,
#57978),(#57979,#57980,#57981,#57982,#57983,#57984,#57985,#57986,#57987,
#57988,#57989,#57990,#57991,#57992),(#57993,#57994,#57995,#57996,#57997,
#57998,#57999,#58000,#58001,#58002,#58003,#58004,#58005,#58006),(#58007,
#58008,#58009,#58010,#58011,#58012,#58013,#58014,#58015,#58016,#58017,#58018,
#58019,#58020),(#58021,#58022,#58023,#58024,#58025,#58026,#58027,#58028,
#58029,#58030,#58031,#58032,#58033,#58034),(#58035,#58036,#58037,#58038,
#58039,#58040,#58041,#58042,#58043,#58044,#58045,#58046,#58047,#58048),
(#58049,#58050,#58051,#58052,#58053,#58054,#58055,#58056,#58057,#58058,
#58059,#58060,#58061,#58062),(#58063,#58064,#58065,#58066,#58067,#58068,
#58069,#58070,#58071,#58072,#58073,#58074,#58075,#58076),(#58077,#58078,
#58079,#58080,#58081,#58082,#58083,#58084,#58085,#58086,#58087,#58088,#58089,
#58090),(#58091,#58092,#58093,#58094,#58095,#58096,#58097,#58098,#58099,
#58100,#58101,#58102,#58103,#58104),(#58105,#58106,#58107,#58108,#58109,
#58110,#58111,#58112,#58113,#58114,#58115,#58116,#58117,#58118),(#58119,
#58120,#58121,#58122,#58123,#58124,#58125,#58126,#58127,#58128,#58129,#58130,
#58131,#58132),(#58133,#58134,#58135,#58136,#58137,#58138,#58139,#58140,
#58141,#58142,#58143,#58144,#58145,#58146),(#58147,#58148,#58149,#58150,
#58151,#58152,#58153,#58154,#58155,#58156,#58157,#58158,#58159,#58160),
(#58161,#58162,#58163,#58164,#58165,#58166,#58167,#58168,#58169,#58170,
#58171,#58172,#58173,#58174),(#58175,#58176,#58177,#58178,#58179,#58180,
#58181,#58182,#58183,#58184,#58185,#58186,#58187,#58188),(#58189,#58190,
#58191,#58192,#58193,#58194,#58195,#58196,#58197,#58198,#58199,#58200,#58201,
#58202),(#58203,#58204,#58205,#58206,#58207,#58208,#58209,#58210,#58211,
#58212,#58213,#58214,#58215,#58216),(#58217,#58218,#58219,#58220,#58221,
#58222,#58223,#58224,#58225,#58226,#58227,#58228,#58229,#58230),(#58231,
#58232,#58233,#58234,#58235,#58236,#58237,#58238,#58239,#58240,#58241,#58242,
#58243,#58244)),.UNSPECIFIED.,.F.,.F.,.F.,(4,1,1,1,1,1,1,1,1,1,1,1,1,1,
1,1,1,1,1,1,1,1,1,4),(4,2,2,2,2,2,4),(0.,0.0517952713240544,0.0690603617654058,
0.103590542648109,0.138120723530812,0.189915994854866,0.24171126617892,
0.276241447061623,0.310771627944326,0.345301808827029,0.379831989709732,
0.414362170592435,0.448892351475138,0.483422532357841,0.552482894123247,
0.587013075005949,0.690603617654058,0.759663979419464,0.76829652464014,
0.776929069860816,0.794194160302167,0.863254522067573,0.897784702950276,
0.966845064715682),(0.0377143719413297,0.167070624995476,0.336553194126115,
0.499999999999991,0.663446805873868,0.832929375004528,0.962285628058621),
 .UNSPECIFIED.);
#242=B_SPLINE_SURFACE_WITH_KNOTS('',3,3,((#58300,#58301,#58302,#58303,#58304,
#58305,#58306,#58307,#58308,#58309,#58310,#58311,#58312,#58313),(#58314,
#58315,#58316,#58317,#58318,#58319,#58320,#58321,#58322,#58323,#58324,#58325,
#58326,#58327),(#58328,#58329,#58330,#58331,#58332,#58333,#58334,#58335,
#58336,#58337,#58338,#58339,#58340,#58341),(#58342,#58343,#58344,#58345,
#58346,#58347,#58348,#58349,#58350,#58351,#58352,#58353,#58354,#58355),
(#58356,#58357,#58358,#58359,#58360,#58361,#58362,#58363,#58364,#58365,
#58366,#58367,#58368,#58369),(#58370,#58371,#58372,#58373,#58374,#58375,
#58376,#58377,#58378,#58379,#58380,#58381,#58382,#58383),(#58384,#58385,
#58386,#58387,#58388,#58389,#58390,#58391,#58392,#58393,#58394,#58395,#58396,
#58397),(#58398,#58399,#58400,#58401,#58402,#58403,#58404,#58405,#58406,
#58407,#58408,#58409,#58410,#58411),(#58412,#58413,#58414,#58415,#58416,
#58417,#58418,#58419,#58420,#58421,#58422,#58423,#58424,#58425),(#58426,
#58427,#58428,#58429,#58430,#58431,#58432,#58433,#58434,#58435,#58436,#58437,
#58438,#58439),(#58440,#58441,#58442,#58443,#58444,#58445,#58446,#58447,
#58448,#58449,#58450,#58451,#58452,#58453),(#58454,#58455,#58456,#58457,
#58458,#58459,#58460,#58461,#58462,#58463,#58464,#58465,#58466,#58467),
(#58468,#58469,#58470,#58471,#58472,#58473,#58474,#58475,#58476,#58477,
#58478,#58479,#58480,#58481),(#58482,#58483,#58484,#58485,#58486,#58487,
#58488,#58489,#58490,#58491,#58492,#58493,#58494,#58495),(#58496,#58497,
#58498,#58499,#58500,#58501,#58502,#58503,#58504,#58505,#58506,#58507,#58508,
#58509),(#58510,#58511,#58512,#58513,#58514,#58515,#58516,#58517,#58518,
#58519,#58520,#58521,#58522,#58523),(#58524,#58525,#58526,#58527,#58528,
#58529,#58530,#58531,#58532,#58533,#58534,#58535,#58536,#58537),(#58538,
#58539,#58540,#58541,#58542,#58543,#58544,#58545,#58546,#58547,#58548,#58549,
#58550,#58551),(#58552,#58553,#58554,#58555,#58556,#58557,#58558,#58559,
#58560,#58561,#58562,#58563,#58564,#58565),(#58566,#58567,#58568,#58569,
#58570,#58571,#58572,#58573,#58574,#58575,#58576,#58577,#58578,#58579),
(#58580,#58581,#58582,#58583,#58584,#58585,#58586,#58587,#58588,#58589,
#58590,#58591,#58592,#58593),(#58594,#58595,#58596,#58597,#58598,#58599,
#58600,#58601,#58602,#58603,#58604,#58605,#58606,#58607),(#58608,#58609,
#58610,#58611,#58612,#58613,#58614,#58615,#58616,#58617,#58618,#58619,#58620,
#58621),(#58622,#58623,#58624,#58625,#58626,#58627,#58628,#58629,#58630,
#58631,#58632,#58633,#58634,#58635),(#58636,#58637,#58638,#58639,#58640,
#58641,#58642,#58643,#58644,#58645,#58646,#58647,#58648,#58649),(#58650,
#58651,#58652,#58653,#58654,#58655,#58656,#58657,#58658,#58659,#58660,#58661,
#58662,#58663),(#58664,#58665,#58666,#58667,#58668,#58669,#58670,#58671,
#58672,#58673,#58674,#58675,#58676,#58677),(#58678,#58679,#58680,#58681,
#58682,#58683,#58684,#58685,#58686,#58687,#58688,#58689,#58690,#58691),
(#58692,#58693,#58694,#58695,#58696,#58697,#58698,#58699,#58700,#58701,
#58702,#58703,#58704,#58705),(#58706,#58707,#58708,#58709,#58710,#58711,
#58712,#58713,#58714,#58715,#58716,#58717,#58718,#58719),(#58720,#58721,
#58722,#58723,#58724,#58725,#58726,#58727,#58728,#58729,#58730,#58731,#58732,
#58733),(#58734,#58735,#58736,#58737,#58738,#58739,#58740,#58741,#58742,
#58743,#58744,#58745,#58746,#58747),(#58748,#58749,#58750,#58751,#58752,
#58753,#58754,#58755,#58756,#58757,#58758,#58759,#58760,#58761),(#58762,
#58763,#58764,#58765,#58766,#58767,#58768,#58769,#58770,#58771,#58772,#58773,
#58774,#58775),(#58776,#58777,#58778,#58779,#58780,#58781,#58782,#58783,
#58784,#58785,#58786,#58787,#58788,#58789),(#58790,#58791,#58792,#58793,
#58794,#58795,#58796,#58797,#58798,#58799,#58800,#58801,#58802,#58803)),
 .UNSPECIFIED.,.F.,.F.,.F.,(4,1,1,1,1,1,1,1,1,1,1,1,1,1,1,1,1,1,1,1,1,1,
1,1,1,1,1,1,1,1,1,1,1,4),(4,2,2,2,2,2,4),(0.0331549352864083,0.0676851161690366,
0.102215297051665,0.171275658816921,0.172354726969504,0.173433795122086,
0.174512863274668,0.17559193142725,0.179908204037578,0.188540749258236,
0.197173294478893,0.20580583969955,0.223070930140864,0.240336020582178,
0.274866201464806,0.309396382347434,0.378456744112691,0.412986924995319,
0.447517105877948,0.482047286760576,0.516577467643204,0.551107648525832,
0.568372738967146,0.585637829408461,0.654698191173717,0.70649346249766,
0.723758552938974,0.79281891470423,0.827349095586859,0.861879276469487,
0.896409457352115,0.930939638234743,0.948204728676058,1.),(0.0377143719412435,
0.167070624995476,0.336553194126115,0.499999999999991,0.663446805873868,
0.832929375004528,0.962285628059578),.UNSPECIFIED.);
#243=B_SPLINE_SURFACE_WITH_KNOTS('',3,3,((#58868,#58869,#58870,#58871,#58872,
#58873,#58874,#58875,#58876,#58877,#58878,#58879,#58880,#58881),(#58882,
#58883,#58884,#58885,#58886,#58887,#58888,#58889,#58890,#58891,#58892,#58893,
#58894,#58895),(#58896,#58897,#58898,#58899,#58900,#58901,#58902,#58903,
#58904,#58905,#58906,#58907,#58908,#58909),(#58910,#58911,#58912,#58913,
#58914,#58915,#58916,#58917,#58918,#58919,#58920,#58921,#58922,#58923)),
 .UNSPECIFIED.,.F.,.F.,.F.,(4,4),(4,2,2,2,2,2,4),(0.,1.),(0.037714371941421,
0.167070624995476,0.336553194126115,0.499999999999991,0.663446805873868,
0.832929375004528,0.962285628058582),.UNSPECIFIED.);
#244=B_SPLINE_SURFACE_WITH_KNOTS('',3,3,((#58938,#58939,#58940,#58941,#58942,
#58943,#58944,#58945,#58946,#58947,#58948,#58949,#58950,#58951),(#58952,
#58953,#58954,#58955,#58956,#58957,#58958,#58959,#58960,#58961,#58962,#58963,
#58964,#58965),(#58966,#58967,#58968,#58969,#58970,#58971,#58972,#58973,
#58974,#58975,#58976,#58977,#58978,#58979),(#58980,#58981,#58982,#58983,
#58984,#58985,#58986,#58987,#58988,#58989,#58990,#58991,#58992,#58993),
(#58994,#58995,#58996,#58997,#58998,#58999,#59000,#59001,#59002,#59003,
#59004,#59005,#59006,#59007),(#59008,#59009,#59010,#59011,#59012,#59013,
#59014,#59015,#59016,#59017,#59018,#59019,#59020,#59021),(#59022,#59023,
#59024,#59025,#59026,#59027,#59028,#59029,#59030,#59031,#59032,#59033,#59034,
#59035),(#59036,#59037,#59038,#59039,#59040,#59041,#59042,#59043,#59044,
#59045,#59046,#59047,#59048,#59049),(#59050,#59051,#59052,#59053,#59054,
#59055,#59056,#59057,#59058,#59059,#59060,#59061,#59062,#59063),(#59064,
#59065,#59066,#59067,#59068,#59069,#59070,#59071,#59072,#59073,#59074,#59075,
#59076,#59077),(#59078,#59079,#59080,#59081,#59082,#59083,#59084,#59085,
#59086,#59087,#59088,#59089,#59090,#59091),(#59092,#59093,#59094,#59095,
#59096,#59097,#59098,#59099,#59100,#59101,#59102,#59103,#59104,#59105),
(#59106,#59107,#59108,#59109,#59110,#59111,#59112,#59113,#59114,#59115,
#59116,#59117,#59118,#59119),(#59120,#59121,#59122,#59123,#59124,#59125,
#59126,#59127,#59128,#59129,#59130,#59131,#59132,#59133),(#59134,#59135,
#59136,#59137,#59138,#59139,#59140,#59141,#59142,#59143,#59144,#59145,#59146,
#59147),(#59148,#59149,#59150,#59151,#59152,#59153,#59154,#59155,#59156,
#59157,#59158,#59159,#59160,#59161),(#59162,#59163,#59164,#59165,#59166,
#59167,#59168,#59169,#59170,#59171,#59172,#59173,#59174,#59175),(#59176,
#59177,#59178,#59179,#59180,#59181,#59182,#59183,#59184,#59185,#59186,#59187,
#59188,#59189),(#59190,#59191,#59192,#59193,#59194,#59195,#59196,#59197,
#59198,#59199,#59200,#59201,#59202,#59203),(#59204,#59205,#59206,#59207,
#59208,#59209,#59210,#59211,#59212,#59213,#59214,#59215,#59216,#59217),
(#59218,#59219,#59220,#59221,#59222,#59223,#59224,#59225,#59226,#59227,
#59228,#59229,#59230,#59231),(#59232,#59233,#59234,#59235,#59236,#59237,
#59238,#59239,#59240,#59241,#59242,#59243,#59244,#59245),(#59246,#59247,
#59248,#59249,#59250,#59251,#59252,#59253,#59254,#59255,#59256,#59257,#59258,
#59259),(#59260,#59261,#59262,#59263,#59264,#59265,#59266,#59267,#59268,
#59269,#59270,#59271,#59272,#59273),(#59274,#59275,#59276,#59277,#59278,
#59279,#59280,#59281,#59282,#59283,#59284,#59285,#59286,#59287),(#59288,
#59289,#59290,#59291,#59292,#59293,#59294,#59295,#59296,#59297,#59298,#59299,
#59300,#59301),(#59302,#59303,#59304,#59305,#59306,#59307,#59308,#59309,
#59310,#59311,#59312,#59313,#59314,#59315),(#59316,#59317,#59318,#59319,
#59320,#59321,#59322,#59323,#59324,#59325,#59326,#59327,#59328,#59329),
(#59330,#59331,#59332,#59333,#59334,#59335,#59336,#59337,#59338,#59339,
#59340,#59341,#59342,#59343),(#59344,#59345,#59346,#59347,#59348,#59349,
#59350,#59351,#59352,#59353,#59354,#59355,#59356,#59357),(#59358,#59359,
#59360,#59361,#59362,#59363,#59364,#59365,#59366,#59367,#59368,#59369,#59370,
#59371),(#59372,#59373,#59374,#59375,#59376,#59377,#59378,#59379,#59380,
#59381,#59382,#59383,#59384,#59385),(#59386,#59387,#59388,#59389,#59390,
#59391,#59392,#59393,#59394,#59395,#59396,#59397,#59398,#59399),(#59400,
#59401,#59402,#59403,#59404,#59405,#59406,#59407,#59408,#59409,#59410,#59411,
#59412,#59413),(#59414,#59415,#59416,#59417,#59418,#59419,#59420,#59421,
#59422,#59423,#59424,#59425,#59426,#59427),(#59428,#59429,#59430,#59431,
#59432,#59433,#59434,#59435,#59436,#59437,#59438,#59439,#59440,#59441),
(#59442,#59443,#59444,#59445,#59446,#59447,#59448,#59449,#59450,#59451,
#59452,#59453,#59454,#59455),(#59456,#59457,#59458,#59459,#59460,#59461,
#59462,#59463,#59464,#59465,#59466,#59467,#59468,#59469),(#59470,#59471,
#59472,#59473,#59474,#59475,#59476,#59477,#59478,#59479,#59480,#59481,#59482,
#59483),(#59484,#59485,#59486,#59487,#59488,#59489,#59490,#59491,#59492,
#59493,#59494,#59495,#59496,#59497),(#59498,#59499,#59500,#59501,#59502,
#59503,#59504,#59505,#59506,#59507,#59508,#59509,#59510,#59511),(#59512,
#59513,#59514,#59515,#59516,#59517,#59518,#59519,#59520,#59521,#59522,#59523,
#59524,#59525),(#59526,#59527,#59528,#59529,#59530,#59531,#59532,#59533,
#59534,#59535,#59536,#59537,#59538,#59539),(#59540,#59541,#59542,#59543,
#59544,#59545,#59546,#59547,#59548,#59549,#59550,#59551,#59552,#59553),
(#59554,#59555,#59556,#59557,#59558,#59559,#59560,#59561,#59562,#59563,
#59564,#59565,#59566,#59567),(#59568,#59569,#59570,#59571,#59572,#59573,
#59574,#59575,#59576,#59577,#59578,#59579,#59580,#59581),(#59582,#59583,
#59584,#59585,#59586,#59587,#59588,#59589,#59590,#59591,#59592,#59593,#59594,
#59595)),.UNSPECIFIED.,.F.,.F.,.F.,(4,1,1,1,1,1,1,1,1,1,1,1,1,1,1,1,1,1,
1,1,1,1,1,1,1,1,1,1,1,1,1,1,1,1,1,1,1,1,1,1,1,1,1,1,4),(4,2,2,2,2,2,4),
(0.,0.0517952713240546,0.0690603617654062,0.103590542648109,0.138120723530812,
0.155385813972164,0.172650904413515,0.207181085296219,0.276241447061625,
0.345301808827031,0.379831989709734,0.414362170592437,0.422994715813113,
0.431627261033789,0.44889235147514,0.466157441916492,0.483422532357843,
0.55248289412325,0.621543255888656,0.656073436771359,0.690603617654062,
0.699236162874738,0.707868708095414,0.725133798536765,0.759663979419468,
0.763980252029806,0.768296524640144,0.77692906986082,0.785561615081495,
0.794194160302171,0.802826705522847,0.811459250743523,0.820091795964199,
0.822249932269367,0.823329000421952,0.824408068574537,0.826566204879705,
0.82764527303229,0.827915040070436,0.828184807108582,0.828454574146728,
0.828724341184874,0.897784702950281,0.932314883832984,0.966845064715687),
(0.0377143719413837,0.167070624995476,0.336553194126115,0.499999999999991,
0.663446805873868,0.832929375004528,0.962285628058658),.UNSPECIFIED.);
#245=B_SPLINE_SURFACE_WITH_KNOTS('',3,3,((#59653,#59654,#59655,#59656,#59657,
#59658,#59659,#59660,#59661,#59662,#59663,#59664,#59665,#59666),(#59667,
#59668,#59669,#59670,#59671,#59672,#59673,#59674,#59675,#59676,#59677,#59678,
#59679,#59680),(#59681,#59682,#59683,#59684,#59685,#59686,#59687,#59688,
#59689,#59690,#59691,#59692,#59693,#59694),(#59695,#59696,#59697,#59698,
#59699,#59700,#59701,#59702,#59703,#59704,#59705,#59706,#59707,#59708),
(#59709,#59710,#59711,#59712,#59713,#59714,#59715,#59716,#59717,#59718,
#59719,#59720,#59721,#59722),(#59723,#59724,#59725,#59726,#59727,#59728,
#59729,#59730,#59731,#59732,#59733,#59734,#59735,#59736),(#59737,#59738,
#59739,#59740,#59741,#59742,#59743,#59744,#59745,#59746,#59747,#59748,#59749,
#59750),(#59751,#59752,#59753,#59754,#59755,#59756,#59757,#59758,#59759,
#59760,#59761,#59762,#59763,#59764),(#59765,#59766,#59767,#59768,#59769,
#59770,#59771,#59772,#59773,#59774,#59775,#59776,#59777,#59778),(#59779,
#59780,#59781,#59782,#59783,#59784,#59785,#59786,#59787,#59788,#59789,#59790,
#59791,#59792),(#59793,#59794,#59795,#59796,#59797,#59798,#59799,#59800,
#59801,#59802,#59803,#59804,#59805,#59806),(#59807,#59808,#59809,#59810,
#59811,#59812,#59813,#59814,#59815,#59816,#59817,#59818,#59819,#59820),
(#59821,#59822,#59823,#59824,#59825,#59826,#59827,#59828,#59829,#59830,
#59831,#59832,#59833,#59834),(#59835,#59836,#59837,#59838,#59839,#59840,
#59841,#59842,#59843,#59844,#59845,#59846,#59847,#59848),(#59849,#59850,
#59851,#59852,#59853,#59854,#59855,#59856,#59857,#59858,#59859,#59860,#59861,
#59862),(#59863,#59864,#59865,#59866,#59867,#59868,#59869,#59870,#59871,
#59872,#59873,#59874,#59875,#59876),(#59877,#59878,#59879,#59880,#59881,
#59882,#59883,#59884,#59885,#59886,#59887,#59888,#59889,#59890),(#59891,
#59892,#59893,#59894,#59895,#59896,#59897,#59898,#59899,#59900,#59901,#59902,
#59903,#59904),(#59905,#59906,#59907,#59908,#59909,#59910,#59911,#59912,
#59913,#59914,#59915,#59916,#59917,#59918),(#59919,#59920,#59921,#59922,
#59923,#59924,#59925,#59926,#59927,#59928,#59929,#59930,#59931,#59932),
(#59933,#59934,#59935,#59936,#59937,#59938,#59939,#59940,#59941,#59942,
#59943,#59944,#59945,#59946),(#59947,#59948,#59949,#59950,#59951,#59952,
#59953,#59954,#59955,#59956,#59957,#59958,#59959,#59960),(#59961,#59962,
#59963,#59964,#59965,#59966,#59967,#59968,#59969,#59970,#59971,#59972,#59973,
#59974),(#59975,#59976,#59977,#59978,#59979,#59980,#59981,#59982,#59983,
#59984,#59985,#59986,#59987,#59988),(#59989,#59990,#59991,#59992,#59993,
#59994,#59995,#59996,#59997,#59998,#59999,#60000,#60001,#60002),(#60003,
#60004,#60005,#60006,#60007,#60008,#60009,#60010,#60011,#60012,#60013,#60014,
#60015,#60016),(#60017,#60018,#60019,#60020,#60021,#60022,#60023,#60024,
#60025,#60026,#60027,#60028,#60029,#60030),(#60031,#60032,#60033,#60034,
#60035,#60036,#60037,#60038,#60039,#60040,#60041,#60042,#60043,#60044),
(#60045,#60046,#60047,#60048,#60049,#60050,#60051,#60052,#60053,#60054,
#60055,#60056,#60057,#60058),(#60059,#60060,#60061,#60062,#60063,#60064,
#60065,#60066,#60067,#60068,#60069,#60070,#60071,#60072),(#60073,#60074,
#60075,#60076,#60077,#60078,#60079,#60080,#60081,#60082,#60083,#60084,#60085,
#60086),(#60087,#60088,#60089,#60090,#60091,#60092,#60093,#60094,#60095,
#60096,#60097,#60098,#60099,#60100),(#60101,#60102,#60103,#60104,#60105,
#60106,#60107,#60108,#60109,#60110,#60111,#60112,#60113,#60114),(#60115,
#60116,#60117,#60118,#60119,#60120,#60121,#60122,#60123,#60124,#60125,#60126,
#60127,#60128),(#60129,#60130,#60131,#60132,#60133,#60134,#60135,#60136,
#60137,#60138,#60139,#60140,#60141,#60142),(#60143,#60144,#60145,#60146,
#60147,#60148,#60149,#60150,#60151,#60152,#60153,#60154,#60155,#60156),
(#60157,#60158,#60159,#60160,#60161,#60162,#60163,#60164,#60165,#60166,
#60167,#60168,#60169,#60170),(#60171,#60172,#60173,#60174,#60175,#60176,
#60177,#60178,#60179,#60180,#60181,#60182,#60183,#60184),(#60185,#60186,
#60187,#60188,#60189,#60190,#60191,#60192,#60193,#60194,#60195,#60196,#60197,
#60198),(#60199,#60200,#60201,#60202,#60203,#60204,#60205,#60206,#60207,
#60208,#60209,#60210,#60211,#60212)),.UNSPECIFIED.,.F.,.F.,.F.,(4,1,1,1,
1,1,1,1,1,1,1,1,1,1,1,1,1,1,1,1,1,1,1,1,1,1,1,1,1,1,1,1,1,1,1,1,1,4),(4,
2,2,2,2,2,4),(0.0331549352864082,0.102215297051665,0.171275658816921,0.171815192893212,
0.172354726969503,0.172894261045795,0.173433795122086,0.17559193142725,
0.179908204037578,0.182066340342743,0.184224476647907,0.188540749258235,
0.197173294478893,0.201489567089221,0.20580583969955,0.214438384920207,
0.223070930140864,0.227387202751192,0.231703475361521,0.240336020582178,
0.309396382347434,0.361191653671377,0.378456744112691,0.447517105877948,
0.482047286760576,0.49931237720189,0.507944922422547,0.512261195032876,
0.516577467643204,0.585637829408461,0.723758552938974,0.79281891470423,
0.827349095586859,0.861879276469487,0.896409457352115,0.930939638234743,
0.948204728676058,1.),(0.0377143719407819,0.167070624995476,0.336553194126115,
0.499999999999991,0.663446805873868,0.832929375004528,0.962285628058724),
 .UNSPECIFIED.);
#246=B_SPLINE_SURFACE_WITH_KNOTS('',3,3,((#60271,#60272,#60273,#60274,#60275,
#60276,#60277,#60278,#60279,#60280,#60281,#60282,#60283,#60284),(#60285,
#60286,#60287,#60288,#60289,#60290,#60291,#60292,#60293,#60294,#60295,#60296,
#60297,#60298),(#60299,#60300,#60301,#60302,#60303,#60304,#60305,#60306,
#60307,#60308,#60309,#60310,#60311,#60312),(#60313,#60314,#60315,#60316,
#60317,#60318,#60319,#60320,#60321,#60322,#60323,#60324,#60325,#60326)),
 .UNSPECIFIED.,.F.,.F.,.F.,(4,4),(4,2,2,2,2,2,4),(0.,1.),(0.0377143719414212,
0.167070624995476,0.336553194126115,0.499999999999991,0.663446805873868,
0.832929375004528,0.962285628058582),.UNSPECIFIED.);
#247=B_SPLINE_SURFACE_WITH_KNOTS('',3,3,((#60341,#60342,#60343,#60344,#60345,
#60346,#60347,#60348,#60349,#60350,#60351,#60352,#60353,#60354),(#60355,
#60356,#60357,#60358,#60359,#60360,#60361,#60362,#60363,#60364,#60365,#60366,
#60367,#60368),(#60369,#60370,#60371,#60372,#60373,#60374,#60375,#60376,
#60377,#60378,#60379,#60380,#60381,#60382),(#60383,#60384,#60385,#60386,
#60387,#60388,#60389,#60390,#60391,#60392,#60393,#60394,#60395,#60396),
(#60397,#60398,#60399,#60400,#60401,#60402,#60403,#60404,#60405,#60406,
#60407,#60408,#60409,#60410),(#60411,#60412,#60413,#60414,#60415,#60416,
#60417,#60418,#60419,#60420,#60421,#60422,#60423,#60424),(#60425,#60426,
#60427,#60428,#60429,#60430,#60431,#60432,#60433,#60434,#60435,#60436,#60437,
#60438),(#60439,#60440,#60441,#60442,#60443,#60444,#60445,#60446,#60447,
#60448,#60449,#60450,#60451,#60452),(#60453,#60454,#60455,#60456,#60457,
#60458,#60459,#60460,#60461,#60462,#60463,#60464,#60465,#60466),(#60467,
#60468,#60469,#60470,#60471,#60472,#60473,#60474,#60475,#60476,#60477,#60478,
#60479,#60480),(#60481,#60482,#60483,#60484,#60485,#60486,#60487,#60488,
#60489,#60490,#60491,#60492,#60493,#60494),(#60495,#60496,#60497,#60498,
#60499,#60500,#60501,#60502,#60503,#60504,#60505,#60506,#60507,#60508),
(#60509,#60510,#60511,#60512,#60513,#60514,#60515,#60516,#60517,#60518,
#60519,#60520,#60521,#60522),(#60523,#60524,#60525,#60526,#60527,#60528,
#60529,#60530,#60531,#60532,#60533,#60534,#60535,#60536),(#60537,#60538,
#60539,#60540,#60541,#60542,#60543,#60544,#60545,#60546,#60547,#60548,#60549,
#60550),(#60551,#60552,#60553,#60554,#60555,#60556,#60557,#60558,#60559,
#60560,#60561,#60562,#60563,#60564),(#60565,#60566,#60567,#60568,#60569,
#60570,#60571,#60572,#60573,#60574,#60575,#60576,#60577,#60578),(#60579,
#60580,#60581,#60582,#60583,#60584,#60585,#60586,#60587,#60588,#60589,#60590,
#60591,#60592),(#60593,#60594,#60595,#60596,#60597,#60598,#60599,#60600,
#60601,#60602,#60603,#60604,#60605,#60606),(#60607,#60608,#60609,#60610,
#60611,#60612,#60613,#60614,#60615,#60616,#60617,#60618,#60619,#60620),
(#60621,#60622,#60623,#60624,#60625,#60626,#60627,#60628,#60629,#60630,
#60631,#60632,#60633,#60634),(#60635,#60636,#60637,#60638,#60639,#60640,
#60641,#60642,#60643,#60644,#60645,#60646,#60647,#60648),(#60649,#60650,
#60651,#60652,#60653,#60654,#60655,#60656,#60657,#60658,#60659,#60660,#60661,
#60662),(#60663,#60664,#60665,#60666,#60667,#60668,#60669,#60670,#60671,
#60672,#60673,#60674,#60675,#60676),(#60677,#60678,#60679,#60680,#60681,
#60682,#60683,#60684,#60685,#60686,#60687,#60688,#60689,#60690),(#60691,
#60692,#60693,#60694,#60695,#60696,#60697,#60698,#60699,#60700,#60701,#60702,
#60703,#60704)),.UNSPECIFIED.,.F.,.F.,.F.,(4,1,1,1,1,1,1,1,1,1,1,1,1,1,
1,1,1,1,1,1,1,1,1,4),(4,2,2,2,2,2,4),(0.,0.0517952713240545,0.069060361765406,
0.103590542648109,0.138120723530812,0.189915994854866,0.241711266178921,
0.276241447061624,0.310771627944327,0.34530180882703,0.362566899268381,
0.379831989709733,0.414362170592436,0.552482894123248,0.587013075005951,
0.621543255888654,0.69060361765406,0.759663979419466,0.768296524640142,
0.776929069860817,0.794194160302169,0.863254522067575,0.897784702950278,
0.966845064715684),(0.0377143719414028,0.167070624995476,0.336553194126115,
0.499999999999991,0.663446805873868,0.832929375004528,0.962285628059076),
 .UNSPECIFIED.);
#248=B_SPLINE_SURFACE_WITH_KNOTS('',3,3,((#60773,#60774,#60775,#60776,#60777,
#60778,#60779,#60780,#60781,#60782,#60783,#60784,#60785,#60786),(#60787,
#60788,#60789,#60790,#60791,#60792,#60793,#60794,#60795,#60796,#60797,#60798,
#60799,#60800),(#60801,#60802,#60803,#60804,#60805,#60806,#60807,#60808,
#60809,#60810,#60811,#60812,#60813,#60814),(#60815,#60816,#60817,#60818,
#60819,#60820,#60821,#60822,#60823,#60824,#60825,#60826,#60827,#60828),
(#60829,#60830,#60831,#60832,#60833,#60834,#60835,#60836,#60837,#60838,
#60839,#60840,#60841,#60842),(#60843,#60844,#60845,#60846,#60847,#60848,
#60849,#60850,#60851,#60852,#60853,#60854,#60855,#60856),(#60857,#60858,
#60859,#60860,#60861,#60862,#60863,#60864,#60865,#60866,#60867,#60868,#60869,
#60870),(#60871,#60872,#60873,#60874,#60875,#60876,#60877,#60878,#60879,
#60880,#60881,#60882,#60883,#60884),(#60885,#60886,#60887,#60888,#60889,
#60890,#60891,#60892,#60893,#60894,#60895,#60896,#60897,#60898),(#60899,
#60900,#60901,#60902,#60903,#60904,#60905,#60906,#60907,#60908,#60909,#60910,
#60911,#60912),(#60913,#60914,#60915,#60916,#60917,#60918,#60919,#60920,
#60921,#60922,#60923,#60924,#60925,#60926),(#60927,#60928,#60929,#60930,
#60931,#60932,#60933,#60934,#60935,#60936,#60937,#60938,#60939,#60940),
(#60941,#60942,#60943,#60944,#60945,#60946,#60947,#60948,#60949,#60950,
#60951,#60952,#60953,#60954),(#60955,#60956,#60957,#60958,#60959,#60960,
#60961,#60962,#60963,#60964,#60965,#60966,#60967,#60968),(#60969,#60970,
#60971,#60972,#60973,#60974,#60975,#60976,#60977,#60978,#60979,#60980,#60981,
#60982),(#60983,#60984,#60985,#60986,#60987,#60988,#60989,#60990,#60991,
#60992,#60993,#60994,#60995,#60996),(#60997,#60998,#60999,#61000,#61001,
#61002,#61003,#61004,#61005,#61006,#61007,#61008,#61009,#61010),(#61011,
#61012,#61013,#61014,#61015,#61016,#61017,#61018,#61019,#61020,#61021,#61022,
#61023,#61024),(#61025,#61026,#61027,#61028,#61029,#61030,#61031,#61032,
#61033,#61034,#61035,#61036,#61037,#61038),(#61039,#61040,#61041,#61042,
#61043,#61044,#61045,#61046,#61047,#61048,#61049,#61050,#61051,#61052),
(#61053,#61054,#61055,#61056,#61057,#61058,#61059,#61060,#61061,#61062,
#61063,#61064,#61065,#61066),(#61067,#61068,#61069,#61070,#61071,#61072,
#61073,#61074,#61075,#61076,#61077,#61078,#61079,#61080),(#61081,#61082,
#61083,#61084,#61085,#61086,#61087,#61088,#61089,#61090,#61091,#61092,#61093,
#61094),(#61095,#61096,#61097,#61098,#61099,#61100,#61101,#61102,#61103,
#61104,#61105,#61106,#61107,#61108),(#61109,#61110,#61111,#61112,#61113,
#61114,#61115,#61116,#61117,#61118,#61119,#61120,#61121,#61122),(#61123,
#61124,#61125,#61126,#61127,#61128,#61129,#61130,#61131,#61132,#61133,#61134,
#61135,#61136),(#61137,#61138,#61139,#61140,#61141,#61142,#61143,#61144,
#61145,#61146,#61147,#61148,#61149,#61150),(#61151,#61152,#61153,#61154,
#61155,#61156,#61157,#61158,#61159,#61160,#61161,#61162,#61163,#61164),
(#61165,#61166,#61167,#61168,#61169,#61170,#61171,#61172,#61173,#61174,
#61175,#61176,#61177,#61178),(#61179,#61180,#61181,#61182,#61183,#61184,
#61185,#61186,#61187,#61188,#61189,#61190,#61191,#61192),(#61193,#61194,
#61195,#61196,#61197,#61198,#61199,#61200,#61201,#61202,#61203,#61204,#61205,
#61206),(#61207,#61208,#61209,#61210,#61211,#61212,#61213,#61214,#61215,
#61216,#61217,#61218,#61219,#61220),(#61221,#61222,#61223,#61224,#61225,
#61226,#61227,#61228,#61229,#61230,#61231,#61232,#61233,#61234),(#61235,
#61236,#61237,#61238,#61239,#61240,#61241,#61242,#61243,#61244,#61245,#61246,
#61247,#61248),(#61249,#61250,#61251,#61252,#61253,#61254,#61255,#61256,
#61257,#61258,#61259,#61260,#61261,#61262),(#61263,#61264,#61265,#61266,
#61267,#61268,#61269,#61270,#61271,#61272,#61273,#61274,#61275,#61276)),
 .UNSPECIFIED.,.F.,.F.,.F.,(4,1,1,1,1,1,1,1,1,1,1,1,1,1,1,1,1,1,1,1,1,1,
1,1,1,1,1,1,1,1,1,1,1,4),(4,2,2,2,2,2,4),(0.0331549352864088,0.102215297051665,
0.171275658816922,0.171815192893213,0.172354726969504,0.172894261045795,
0.173433795122086,0.17559193142725,0.179908204037579,0.182066340342743,
0.188540749258236,0.197173294478893,0.20580583969955,0.214438384920207,
0.223070930140864,0.240336020582178,0.274866201464807,0.292131291906121,
0.309396382347435,0.378456744112691,0.41298692499532,0.430252015436634,
0.447517105877948,0.516577467643204,0.585637829408461,0.654698191173717,
0.689228372056346,0.723758552938974,0.810084005145544,0.861879276469487,
0.896409457352115,0.930939638234743,0.948204728676058,1.),(0.0377143719413782,
0.167070624995476,0.336553194126115,0.499999999999991,0.663446805873868,
0.832929375004528,0.962285628059578),.UNSPECIFIED.);
#249=B_SPLINE_SURFACE_WITH_KNOTS('',3,3,((#61328,#61329,#61330,#61331,#61332,
#61333,#61334,#61335,#61336,#61337,#61338,#61339,#61340,#61341),(#61342,
#61343,#61344,#61345,#61346,#61347,#61348,#61349,#61350,#61351,#61352,#61353,
#61354,#61355),(#61356,#61357,#61358,#61359,#61360,#61361,#61362,#61363,
#61364,#61365,#61366,#61367,#61368,#61369),(#61370,#61371,#61372,#61373,
#61374,#61375,#61376,#61377,#61378,#61379,#61380,#61381,#61382,#61383)),
 .UNSPECIFIED.,.F.,.F.,.F.,(4,4),(4,2,2,2,2,2,4),(0.,1.),(0.037714371941421,
0.167070624995476,0.336553194126115,0.499999999999991,0.663446805873868,
0.832929375004528,0.962285628058582),.UNSPECIFIED.);
#250=B_SPLINE_SURFACE_WITH_KNOTS('',3,3,((#61398,#61399,#61400,#61401,#61402,
#61403,#61404,#61405,#61406,#61407,#61408,#61409,#61410,#61411),(#61412,
#61413,#61414,#61415,#61416,#61417,#61418,#61419,#61420,#61421,#61422,#61423,
#61424,#61425),(#61426,#61427,#61428,#61429,#61430,#61431,#61432,#61433,
#61434,#61435,#61436,#61437,#61438,#61439),(#61440,#61441,#61442,#61443,
#61444,#61445,#61446,#61447,#61448,#61449,#61450,#61451,#61452,#61453),
(#61454,#61455,#61456,#61457,#61458,#61459,#61460,#61461,#61462,#61463,
#61464,#61465,#61466,#61467),(#61468,#61469,#61470,#61471,#61472,#61473,
#61474,#61475,#61476,#61477,#61478,#61479,#61480,#61481),(#61482,#61483,
#61484,#61485,#61486,#61487,#61488,#61489,#61490,#61491,#61492,#61493,#61494,
#61495),(#61496,#61497,#61498,#61499,#61500,#61501,#61502,#61503,#61504,
#61505,#61506,#61507,#61508,#61509),(#61510,#61511,#61512,#61513,#61514,
#61515,#61516,#61517,#61518,#61519,#61520,#61521,#61522,#61523),(#61524,
#61525,#61526,#61527,#61528,#61529,#61530,#61531,#61532,#61533,#61534,#61535,
#61536,#61537),(#61538,#61539,#61540,#61541,#61542,#61543,#61544,#61545,
#61546,#61547,#61548,#61549,#61550,#61551),(#61552,#61553,#61554,#61555,
#61556,#61557,#61558,#61559,#61560,#61561,#61562,#61563,#61564,#61565),
(#61566,#61567,#61568,#61569,#61570,#61571,#61572,#61573,#61574,#61575,
#61576,#61577,#61578,#61579),(#61580,#61581,#61582,#61583,#61584,#61585,
#61586,#61587,#61588,#61589,#61590,#61591,#61592,#61593),(#61594,#61595,
#61596,#61597,#61598,#61599,#61600,#61601,#61602,#61603,#61604,#61605,#61606,
#61607),(#61608,#61609,#61610,#61611,#61612,#61613,#61614,#61615,#61616,
#61617,#61618,#61619,#61620,#61621),(#61622,#61623,#61624,#61625,#61626,
#61627,#61628,#61629,#61630,#61631,#61632,#61633,#61634,#61635),(#61636,
#61637,#61638,#61639,#61640,#61641,#61642,#61643,#61644,#61645,#61646,#61647,
#61648,#61649),(#61650,#61651,#61652,#61653,#61654,#61655,#61656,#61657,
#61658,#61659,#61660,#61661,#61662,#61663),(#61664,#61665,#61666,#61667,
#61668,#61669,#61670,#61671,#61672,#61673,#61674,#61675,#61676,#61677),
(#61678,#61679,#61680,#61681,#61682,#61683,#61684,#61685,#61686,#61687,
#61688,#61689,#61690,#61691),(#61692,#61693,#61694,#61695,#61696,#61697,
#61698,#61699,#61700,#61701,#61702,#61703,#61704,#61705),(#61706,#61707,
#61708,#61709,#61710,#61711,#61712,#61713,#61714,#61715,#61716,#61717,#61718,
#61719),(#61720,#61721,#61722,#61723,#61724,#61725,#61726,#61727,#61728,
#61729,#61730,#61731,#61732,#61733),(#61734,#61735,#61736,#61737,#61738,
#61739,#61740,#61741,#61742,#61743,#61744,#61745,#61746,#61747),(#61748,
#61749,#61750,#61751,#61752,#61753,#61754,#61755,#61756,#61757,#61758,#61759,
#61760,#61761),(#61762,#61763,#61764,#61765,#61766,#61767,#61768,#61769,
#61770,#61771,#61772,#61773,#61774,#61775),(#61776,#61777,#61778,#61779,
#61780,#61781,#61782,#61783,#61784,#61785,#61786,#61787,#61788,#61789),
(#61790,#61791,#61792,#61793,#61794,#61795,#61796,#61797,#61798,#61799,
#61800,#61801,#61802,#61803),(#61804,#61805,#61806,#61807,#61808,#61809,
#61810,#61811,#61812,#61813,#61814,#61815,#61816,#61817),(#61818,#61819,
#61820,#61821,#61822,#61823,#61824,#61825,#61826,#61827,#61828,#61829,#61830,
#61831),(#61832,#61833,#61834,#61835,#61836,#61837,#61838,#61839,#61840,
#61841,#61842,#61843,#61844,#61845),(#61846,#61847,#61848,#61849,#61850,
#61851,#61852,#61853,#61854,#61855,#61856,#61857,#61858,#61859),(#61860,
#61861,#61862,#61863,#61864,#61865,#61866,#61867,#61868,#61869,#61870,#61871,
#61872,#61873),(#61874,#61875,#61876,#61877,#61878,#61879,#61880,#61881,
#61882,#61883,#61884,#61885,#61886,#61887),(#61888,#61889,#61890,#61891,
#61892,#61893,#61894,#61895,#61896,#61897,#61898,#61899,#61900,#61901),
(#61902,#61903,#61904,#61905,#61906,#61907,#61908,#61909,#61910,#61911,
#61912,#61913,#61914,#61915),(#61916,#61917,#61918,#61919,#61920,#61921,
#61922,#61923,#61924,#61925,#61926,#61927,#61928,#61929),(#61930,#61931,
#61932,#61933,#61934,#61935,#61936,#61937,#61938,#61939,#61940,#61941,#61942,
#61943),(#61944,#61945,#61946,#61947,#61948,#61949,#61950,#61951,#61952,
#61953,#61954,#61955,#61956,#61957),(#61958,#61959,#61960,#61961,#61962,
#61963,#61964,#61965,#61966,#61967,#61968,#61969,#61970,#61971),(#61972,
#61973,#61974,#61975,#61976,#61977,#61978,#61979,#61980,#61981,#61982,#61983,
#61984,#61985),(#61986,#61987,#61988,#61989,#61990,#61991,#61992,#61993,
#61994,#61995,#61996,#61997,#61998,#61999),(#62000,#62001,#62002,#62003,
#62004,#62005,#62006,#62007,#62008,#62009,#62010,#62011,#62012,#62013),
(#62014,#62015,#62016,#62017,#62018,#62019,#62020,#62021,#62022,#62023,
#62024,#62025,#62026,#62027),(#62028,#62029,#62030,#62031,#62032,#62033,
#62034,#62035,#62036,#62037,#62038,#62039,#62040,#62041)),.UNSPECIFIED.,
 .F.,.F.,.F.,(4,1,1,1,1,1,1,1,1,1,1,1,1,1,1,1,1,1,1,1,1,1,1,1,1,1,1,1,1,
1,1,1,1,1,1,1,1,1,1,1,1,1,1,4),(4,2,2,2,2,2,4),(0.,0.034530180882703,0.0517952713240545,
0.069060361765406,0.103590542648109,0.138120723530812,0.146753268751488,
0.155385813972164,0.172650904413515,0.207181085296218,0.276241447061624,
0.310771627944327,0.34530180882703,0.379831989709733,0.414362170592436,
0.448892351475139,0.483422532357842,0.500687622799194,0.552482894123248,
0.5697479845646,0.621543255888654,0.656073436771357,0.69060361765406,0.707868708095412,
0.716501253316088,0.725133798536763,0.759663979419467,0.776929069860818,
0.785561615081494,0.79419416030217,0.802826705522845,0.811459250743521,
0.820091795964197,0.824408068574535,0.825487136727119,0.826566204879704,
0.827645273032288,0.82818480710858,0.828454574146726,0.828724341184873,
0.863254522067576,0.897784702950279,0.932314883832982,0.966845064715685),
(0.0377143719413179,0.167070624995476,0.336553194126115,0.499999999999991,
0.663446805873868,0.832929375004528,0.962285628060395),.UNSPECIFIED.);
#251=B_SPLINE_SURFACE_WITH_KNOTS('',3,3,((#62109,#62110,#62111,#62112,#62113,
#62114,#62115,#62116,#62117,#62118,#62119,#62120,#62121,#62122),(#62123,
#62124,#62125,#62126,#62127,#62128,#62129,#62130,#62131,#62132,#62133,#62134,
#62135,#62136),(#62137,#62138,#62139,#62140,#62141,#62142,#62143,#62144,
#62145,#62146,#62147,#62148,#62149,#62150),(#62151,#62152,#62153,#62154,
#62155,#62156,#62157,#62158,#62159,#62160,#62161,#62162,#62163,#62164),
(#62165,#62166,#62167,#62168,#62169,#62170,#62171,#62172,#62173,#62174,
#62175,#62176,#62177,#62178),(#62179,#62180,#62181,#62182,#62183,#62184,
#62185,#62186,#62187,#62188,#62189,#62190,#62191,#62192),(#62193,#62194,
#62195,#62196,#62197,#62198,#62199,#62200,#62201,#62202,#62203,#62204,#62205,
#62206),(#62207,#62208,#62209,#62210,#62211,#62212,#62213,#62214,#62215,
#62216,#62217,#62218,#62219,#62220),(#62221,#62222,#62223,#62224,#62225,
#62226,#62227,#62228,#62229,#62230,#62231,#62232,#62233,#62234),(#62235,
#62236,#62237,#62238,#62239,#62240,#62241,#62242,#62243,#62244,#62245,#62246,
#62247,#62248),(#62249,#62250,#62251,#62252,#62253,#62254,#62255,#62256,
#62257,#62258,#62259,#62260,#62261,#62262),(#62263,#62264,#62265,#62266,
#62267,#62268,#62269,#62270,#62271,#62272,#62273,#62274,#62275,#62276),
(#62277,#62278,#62279,#62280,#62281,#62282,#62283,#62284,#62285,#62286,
#62287,#62288,#62289,#62290),(#62291,#62292,#62293,#62294,#62295,#62296,
#62297,#62298,#62299,#62300,#62301,#62302,#62303,#62304),(#62305,#62306,
#62307,#62308,#62309,#62310,#62311,#62312,#62313,#62314,#62315,#62316,#62317,
#62318),(#62319,#62320,#62321,#62322,#62323,#62324,#62325,#62326,#62327,
#62328,#62329,#62330,#62331,#62332),(#62333,#62334,#62335,#62336,#62337,
#62338,#62339,#62340,#62341,#62342,#62343,#62344,#62345,#62346),(#62347,
#62348,#62349,#62350,#62351,#62352,#62353,#62354,#62355,#62356,#62357,#62358,
#62359,#62360),(#62361,#62362,#62363,#62364,#62365,#62366,#62367,#62368,
#62369,#62370,#62371,#62372,#62373,#62374),(#62375,#62376,#62377,#62378,
#62379,#62380,#62381,#62382,#62383,#62384,#62385,#62386,#62387,#62388),
(#62389,#62390,#62391,#62392,#62393,#62394,#62395,#62396,#62397,#62398,
#62399,#62400,#62401,#62402),(#62403,#62404,#62405,#62406,#62407,#62408,
#62409,#62410,#62411,#62412,#62413,#62414,#62415,#62416),(#62417,#62418,
#62419,#62420,#62421,#62422,#62423,#62424,#62425,#62426,#62427,#62428,#62429,
#62430),(#62431,#62432,#62433,#62434,#62435,#62436,#62437,#62438,#62439,
#62440,#62441,#62442,#62443,#62444),(#62445,#62446,#62447,#62448,#62449,
#62450,#62451,#62452,#62453,#62454,#62455,#62456,#62457,#62458),(#62459,
#62460,#62461,#62462,#62463,#62464,#62465,#62466,#62467,#62468,#62469,#62470,
#62471,#62472),(#62473,#62474,#62475,#62476,#62477,#62478,#62479,#62480,
#62481,#62482,#62483,#62484,#62485,#62486),(#62487,#62488,#62489,#62490,
#62491,#62492,#62493,#62494,#62495,#62496,#62497,#62498,#62499,#62500),
(#62501,#62502,#62503,#62504,#62505,#62506,#62507,#62508,#62509,#62510,
#62511,#62512,#62513,#62514),(#62515,#62516,#62517,#62518,#62519,#62520,
#62521,#62522,#62523,#62524,#62525,#62526,#62527,#62528)),.UNSPECIFIED.,
 .F.,.F.,.F.,(4,1,1,1,1,1,1,1,1,1,1,1,1,1,1,1,1,1,1,1,1,1,1,1,1,1,1,4),
(4,2,2,2,2,2,4),(0.0331549352864031,0.10221529705166,0.171275658816917,
0.173433795122081,0.175591931427245,0.179908204037574,0.188540749258231,
0.205805839699545,0.214438384920203,0.22307093014086,0.240336020582174,
0.309396382347431,0.395721834554002,0.447517105877945,0.482047286760573,
0.499312377201887,0.516577467643202,0.55110764852583,0.585637829408458,
0.620168010291087,0.723758552938972,0.792818914704229,0.827349095586858,
0.861879276469486,0.896409457352115,0.930939638234743,0.948204728676057,
1.),(0.0377143719413312,0.167070624995476,0.336553194126115,0.499999999999991,
0.663446805873868,0.832929375004528,0.962285628058676),.UNSPECIFIED.);
#252=B_SPLINE_SURFACE_WITH_KNOTS('',3,3,((#62573,#62574,#62575,#62576,#62577,
#62578,#62579,#62580,#62581,#62582,#62583,#62584,#62585,#62586),(#62587,
#62588,#62589,#62590,#62591,#62592,#62593,#62594,#62595,#62596,#62597,#62598,
#62599,#62600),(#62601,#62602,#62603,#62604,#62605,#62606,#62607,#62608,
#62609,#62610,#62611,#62612,#62613,#62614),(#62615,#62616,#62617,#62618,
#62619,#62620,#62621,#62622,#62623,#62624,#62625,#62626,#62627,#62628)),
 .UNSPECIFIED.,.F.,.F.,.F.,(4,4),(4,2,2,2,2,2,4),(0.,1.),(0.037714371941421,
0.167070624995476,0.336553194126115,0.499999999999991,0.663446805873868,
0.832929375004528,0.962285628058582),.UNSPECIFIED.);
#253=B_SPLINE_SURFACE_WITH_KNOTS('',3,3,((#62643,#62644,#62645,#62646,#62647,
#62648,#62649,#62650,#62651,#62652,#62653,#62654,#62655,#62656),(#62657,
#62658,#62659,#62660,#62661,#62662,#62663,#62664,#62665,#62666,#62667,#62668,
#62669,#62670),(#62671,#62672,#62673,#62674,#62675,#62676,#62677,#62678,
#62679,#62680,#62681,#62682,#62683,#62684),(#62685,#62686,#62687,#62688,
#62689,#62690,#62691,#62692,#62693,#62694,#62695,#62696,#62697,#62698),
(#62699,#62700,#62701,#62702,#62703,#62704,#62705,#62706,#62707,#62708,
#62709,#62710,#62711,#62712),(#62713,#62714,#62715,#62716,#62717,#62718,
#62719,#62720,#62721,#62722,#62723,#62724,#62725,#62726),(#62727,#62728,
#62729,#62730,#62731,#62732,#62733,#62734,#62735,#62736,#62737,#62738,#62739,
#62740),(#62741,#62742,#62743,#62744,#62745,#62746,#62747,#62748,#62749,
#62750,#62751,#62752,#62753,#62754),(#62755,#62756,#62757,#62758,#62759,
#62760,#62761,#62762,#62763,#62764,#62765,#62766,#62767,#62768),(#62769,
#62770,#62771,#62772,#62773,#62774,#62775,#62776,#62777,#62778,#62779,#62780,
#62781,#62782),(#62783,#62784,#62785,#62786,#62787,#62788,#62789,#62790,
#62791,#62792,#62793,#62794,#62795,#62796),(#62797,#62798,#62799,#62800,
#62801,#62802,#62803,#62804,#62805,#62806,#62807,#62808,#62809,#62810),
(#62811,#62812,#62813,#62814,#62815,#62816,#62817,#62818,#62819,#62820,
#62821,#62822,#62823,#62824),(#62825,#62826,#62827,#62828,#62829,#62830,
#62831,#62832,#62833,#62834,#62835,#62836,#62837,#62838),(#62839,#62840,
#62841,#62842,#62843,#62844,#62845,#62846,#62847,#62848,#62849,#62850,#62851,
#62852),(#62853,#62854,#62855,#62856,#62857,#62858,#62859,#62860,#62861,
#62862,#62863,#62864,#62865,#62866),(#62867,#62868,#62869,#62870,#62871,
#62872,#62873,#62874,#62875,#62876,#62877,#62878,#62879,#62880),(#62881,
#62882,#62883,#62884,#62885,#62886,#62887,#62888,#62889,#62890,#62891,#62892,
#62893,#62894),(#62895,#62896,#62897,#62898,#62899,#62900,#62901,#62902,
#62903,#62904,#62905,#62906,#62907,#62908),(#62909,#62910,#62911,#62912,
#62913,#62914,#62915,#62916,#62917,#62918,#62919,#62920,#62921,#62922),
(#62923,#62924,#62925,#62926,#62927,#62928,#62929,#62930,#62931,#62932,
#62933,#62934,#62935,#62936),(#62937,#62938,#62939,#62940,#62941,#62942,
#62943,#62944,#62945,#62946,#62947,#62948,#62949,#62950),(#62951,#62952,
#62953,#62954,#62955,#62956,#62957,#62958,#62959,#62960,#62961,#62962,#62963,
#62964),(#62965,#62966,#62967,#62968,#62969,#62970,#62971,#62972,#62973,
#62974,#62975,#62976,#62977,#62978),(#62979,#62980,#62981,#62982,#62983,
#62984,#62985,#62986,#62987,#62988,#62989,#62990,#62991,#62992),(#62993,
#62994,#62995,#62996,#62997,#62998,#62999,#63000,#63001,#63002,#63003,#63004,
#63005,#63006),(#63007,#63008,#63009,#63010,#63011,#63012,#63013,#63014,
#63015,#63016,#63017,#63018,#63019,#63020),(#63021,#63022,#63023,#63024,
#63025,#63026,#63027,#63028,#63029,#63030,#63031,#63032,#63033,#63034),
(#63035,#63036,#63037,#63038,#63039,#63040,#63041,#63042,#63043,#63044,
#63045,#63046,#63047,#63048),(#63049,#63050,#63051,#63052,#63053,#63054,
#63055,#63056,#63057,#63058,#63059,#63060,#63061,#63062),(#63063,#63064,
#63065,#63066,#63067,#63068,#63069,#63070,#63071,#63072,#63073,#63074,#63075,
#63076)),.UNSPECIFIED.,.F.,.F.,.F.,(4,1,1,1,1,1,1,1,1,1,1,1,1,1,1,1,1,1,
1,1,1,1,1,1,1,1,1,1,4),(4,2,2,2,2,2,4),(0.,0.0517952713240546,0.0690603617654061,
0.103590542648109,0.138120723530812,0.155385813972164,0.189915994854867,
0.276241447061624,0.34530180882703,0.414362170592436,0.431627261033788,
0.448892351475139,0.483422532357842,0.517952713240545,0.552482894123249,
0.587013075005952,0.621543255888655,0.690603617654061,0.699236162874737,
0.725133798536764,0.759663979419467,0.79419416030217,0.811459250743521,
0.820091795964197,0.824408068574535,0.826566204879704,0.828724341184873,
0.897784702950279,0.966845064715685),(0.0377143719404219,0.167070624995476,
0.336553194126115,0.499999999999991,0.663446805873868,0.832929375004528,
0.962285628061492),.UNSPECIFIED.);
#254=B_SPLINE_SURFACE_WITH_KNOTS('',3,3,((#65570,#65571,#65572,#65573,#65574,
#65575,#65576,#65577,#65578,#65579,#65580,#65581,#65582,#65583,#65584,#65585,
#65586,#65587,#65588,#65589,#65590,#65591,#65592,#65593,#65594,#65595,#65596,
#65597,#65598,#65599,#65600,#65601,#65602,#65603,#65604,#65605,#65606,#65607,
#65608,#65609,#65610,#65611,#65612,#65613,#65614,#65615),(#65616,#65617,
#65618,#65619,#65620,#65621,#65622,#65623,#65624,#65625,#65626,#65627,#65628,
#65629,#65630,#65631,#65632,#65633,#65634,#65635,#65636,#65637,#65638,#65639,
#65640,#65641,#65642,#65643,#65644,#65645,#65646,#65647,#65648,#65649,#65650,
#65651,#65652,#65653,#65654,#65655,#65656,#65657,#65658,#65659,#65660,#65661),
(#65662,#65663,#65664,#65665,#65666,#65667,#65668,#65669,#65670,#65671,
#65672,#65673,#65674,#65675,#65676,#65677,#65678,#65679,#65680,#65681,#65682,
#65683,#65684,#65685,#65686,#65687,#65688,#65689,#65690,#65691,#65692,#65693,
#65694,#65695,#65696,#65697,#65698,#65699,#65700,#65701,#65702,#65703,#65704,
#65705,#65706,#65707),(#65708,#65709,#65710,#65711,#65712,#65713,#65714,
#65715,#65716,#65717,#65718,#65719,#65720,#65721,#65722,#65723,#65724,#65725,
#65726,#65727,#65728,#65729,#65730,#65731,#65732,#65733,#65734,#65735,#65736,
#65737,#65738,#65739,#65740,#65741,#65742,#65743,#65744,#65745,#65746,#65747,
#65748,#65749,#65750,#65751,#65752,#65753)),.UNSPECIFIED.,.F.,.F.,.F.,(4,
4),(4,1,1,1,1,1,1,1,1,1,1,1,1,1,1,1,1,1,1,1,1,1,1,1,1,1,1,1,1,1,1,1,1,1,
1,1,1,1,1,1,1,1,1,4),(-0.00074044236405861,0.066233565701187),(8.3083844520832,
8.80545257887392,9.30252070566464,10.2966569592461,11.2907932128275,12.284929466409,
13.2790657199904,14.2732019735718,15.2673382271533,16.2614744807347,17.2556107343161,
18.2497469878976,19.243883241479,20.2380194950604,21.2321557486419,22.2262920022233,
23.2204282558048,24.2145645093862,25.2087007629676,26.2028370165491,27.1969732701305,
28.1911095237119,29.1852457772934,30.1793820308748,31.1735182844562,32.1676545380377,
33.1617907916191,34.1559270452005,35.150063298782,36.1441995523634,37.1383358059449,
38.1324720595263,39.1266083131077,40.1207445666892,41.1148808202706,42.109017073852,
43.1031533274335,44.0972895810149,45.0914258345964,46.0855620881778,47.0796983417592,
48.0738345953407,48.5709027221314,49.0687112912862),.UNSPECIFIED.);
#255=B_SPLINE_SURFACE_WITH_KNOTS('',3,3,((#65959,#65960,#65961,#65962,#65963,
#65964,#65965,#65966,#65967,#65968,#65969,#65970,#65971,#65972,#65973,#65974,
#65975,#65976,#65977,#65978,#65979,#65980,#65981,#65982,#65983,#65984,#65985,
#65986,#65987,#65988,#65989,#65990,#65991,#65992,#65993,#65994,#65995,#65996,
#65997,#65998,#65999,#66000,#66001,#66002,#66003,#66004),(#66005,#66006,
#66007,#66008,#66009,#66010,#66011,#66012,#66013,#66014,#66015,#66016,#66017,
#66018,#66019,#66020,#66021,#66022,#66023,#66024,#66025,#66026,#66027,#66028,
#66029,#66030,#66031,#66032,#66033,#66034,#66035,#66036,#66037,#66038,#66039,
#66040,#66041,#66042,#66043,#66044,#66045,#66046,#66047,#66048,#66049,#66050),
(#66051,#66052,#66053,#66054,#66055,#66056,#66057,#66058,#66059,#66060,
#66061,#66062,#66063,#66064,#66065,#66066,#66067,#66068,#66069,#66070,#66071,
#66072,#66073,#66074,#66075,#66076,#66077,#66078,#66079,#66080,#66081,#66082,
#66083,#66084,#66085,#66086,#66087,#66088,#66089,#66090,#66091,#66092,#66093,
#66094,#66095,#66096),(#66097,#66098,#66099,#66100,#66101,#66102,#66103,
#66104,#66105,#66106,#66107,#66108,#66109,#66110,#66111,#66112,#66113,#66114,
#66115,#66116,#66117,#66118,#66119,#66120,#66121,#66122,#66123,#66124,#66125,
#66126,#66127,#66128,#66129,#66130,#66131,#66132,#66133,#66134,#66135,#66136,
#66137,#66138,#66139,#66140,#66141,#66142)),.UNSPECIFIED.,.F.,.F.,.F.,(4,
4),(4,1,1,1,1,1,1,1,1,1,1,1,1,1,1,1,1,1,1,1,1,1,1,1,1,1,1,1,1,1,1,1,1,1,
1,1,1,1,1,1,1,1,1,4),(-0.000415672852192788,0.0663202636511997),(11.6148054166941,
12.112100974609,12.6091691013998,13.6033053549812,14.5974416085626,15.5915778621441,
16.5857141157255,17.5798503693069,18.5739866228884,19.5681228764698,20.5622591300512,
21.5563953836327,22.5505316372141,23.5446678907956,24.538804144377,25.5329403979584,
26.5270766515399,27.5212129051213,28.5153491587027,29.5094854122842,30.5036216658656,
31.497757919447,32.4918941730285,33.4860304266099,34.4801666801914,35.4743029337728,
36.4684391873542,37.4625754409357,38.4567116945171,39.4508479480985,40.44498420168,
41.4391204552614,42.4332567088428,43.4273929624243,44.4215292160057,45.4156654695872,
46.4098017231686,47.40393797675,48.3980742303315,49.3922104839129,50.3863467374943,
51.3804829910758,51.8775511178665,52.3746192446572),.UNSPECIFIED.);
#256=B_SPLINE_SURFACE_WITH_KNOTS('',3,3,((#76225,#76226,#76227,#76228,#76229,
#76230,#76231,#76232,#76233,#76234,#76235,#76236,#76237,#76238,#76239,#76240,
#76241,#76242,#76243,#76244,#76245,#76246,#76247,#76248,#76249,#76250,#76251,
#76252,#76253,#76254,#76255,#76256,#76257,#76258,#76259,#76260,#76261,#76262,
#76263,#76264,#76265,#76266,#76267,#76268,#76269,#76270,#76271,#76272,#76273,
#76274,#76275,#76276,#76277,#76278,#76279,#76280,#76281,#76282,#76283,#76284,
#76285,#76286,#76287,#76288,#76289,#76290,#76291,#76292,#76293,#76294,#76295,
#76296,#76297,#76298,#76299,#76300,#76301,#76302,#76303,#76304,#76305,#76306,
#76307,#76308,#76309,#76310,#76311,#76312,#76313,#76314,#76315,#76316,#76317,
#76318,#76319,#76320,#76321,#76322,#76323,#76324,#76325,#76326,#76327,#76328,
#76329,#76330,#76331,#76332,#76333,#76334,#76335,#76336,#76337,#76338,#76339,
#76340,#76341,#76342,#76343,#76344,#76345,#76346,#76347,#76348,#76349,#76350),
(#76351,#76352,#76353,#76354,#76355,#76356,#76357,#76358,#76359,#76360,
#76361,#76362,#76363,#76364,#76365,#76366,#76367,#76368,#76369,#76370,#76371,
#76372,#76373,#76374,#76375,#76376,#76377,#76378,#76379,#76380,#76381,#76382,
#76383,#76384,#76385,#76386,#76387,#76388,#76389,#76390,#76391,#76392,#76393,
#76394,#76395,#76396,#76397,#76398,#76399,#76400,#76401,#76402,#76403,#76404,
#76405,#76406,#76407,#76408,#76409,#76410,#76411,#76412,#76413,#76414,#76415,
#76416,#76417,#76418,#76419,#76420,#76421,#76422,#76423,#76424,#76425,#76426,
#76427,#76428,#76429,#76430,#76431,#76432,#76433,#76434,#76435,#76436,#76437,
#76438,#76439,#76440,#76441,#76442,#76443,#76444,#76445,#76446,#76447,#76448,
#76449,#76450,#76451,#76452,#76453,#76454,#76455,#76456,#76457,#76458,#76459,
#76460,#76461,#76462,#76463,#76464,#76465,#76466,#76467,#76468,#76469,#76470,
#76471,#76472,#76473,#76474,#76475,#76476),(#76477,#76478,#76479,#76480,
#76481,#76482,#76483,#76484,#76485,#76486,#76487,#76488,#76489,#76490,#76491,
#76492,#76493,#76494,#76495,#76496,#76497,#76498,#76499,#76500,#76501,#76502,
#76503,#76504,#76505,#76506,#76507,#76508,#76509,#76510,#76511,#76512,#76513,
#76514,#76515,#76516,#76517,#76518,#76519,#76520,#76521,#76522,#76523,#76524,
#76525,#76526,#76527,#76528,#76529,#76530,#76531,#76532,#76533,#76534,#76535,
#76536,#76537,#76538,#76539,#76540,#76541,#76542,#76543,#76544,#76545,#76546,
#76547,#76548,#76549,#76550,#76551,#76552,#76553,#76554,#76555,#76556,#76557,
#76558,#76559,#76560,#76561,#76562,#76563,#76564,#76565,#76566,#76567,#76568,
#76569,#76570,#76571,#76572,#76573,#76574,#76575,#76576,#76577,#76578,#76579,
#76580,#76581,#76582,#76583,#76584,#76585,#76586,#76587,#76588,#76589,#76590,
#76591,#76592,#76593,#76594,#76595,#76596,#76597,#76598,#76599,#76600,#76601,
#76602),(#76603,#76604,#76605,#76606,#76607,#76608,#76609,#76610,#76611,
#76612,#76613,#76614,#76615,#76616,#76617,#76618,#76619,#76620,#76621,#76622,
#76623,#76624,#76625,#76626,#76627,#76628,#76629,#76630,#76631,#76632,#76633,
#76634,#76635,#76636,#76637,#76638,#76639,#76640,#76641,#76642,#76643,#76644,
#76645,#76646,#76647,#76648,#76649,#76650,#76651,#76652,#76653,#76654,#76655,
#76656,#76657,#76658,#76659,#76660,#76661,#76662,#76663,#76664,#76665,#76666,
#76667,#76668,#76669,#76670,#76671,#76672,#76673,#76674,#76675,#76676,#76677,
#76678,#76679,#76680,#76681,#76682,#76683,#76684,#76685,#76686,#76687,#76688,
#76689,#76690,#76691,#76692,#76693,#76694,#76695,#76696,#76697,#76698,#76699,
#76700,#76701,#76702,#76703,#76704,#76705,#76706,#76707,#76708,#76709,#76710,
#76711,#76712,#76713,#76714,#76715,#76716,#76717,#76718,#76719,#76720,#76721,
#76722,#76723,#76724,#76725,#76726,#76727,#76728)),.UNSPECIFIED.,.F.,.F.,
 .F.,(4,4),(4,1,1,1,1,1,1,1,1,1,1,1,1,1,1,1,1,1,1,1,1,1,1,1,1,1,1,1,1,1,
1,1,1,1,1,1,1,1,1,1,1,1,1,1,1,1,1,1,1,1,1,1,1,1,1,1,1,1,1,1,1,1,1,1,1,1,
1,1,1,1,1,1,1,1,1,1,1,1,1,1,1,1,1,1,1,1,1,1,1,1,1,1,1,1,1,1,1,1,1,1,1,1,
1,1,1,1,1,1,1,1,1,1,1,1,1,1,1,1,1,1,1,1,1,4),(-0.000489095128896854,0.0662888134554226),
(8.30725886192223,9.30549431301254,10.303511073624,11.3015278342355,12.299544594847,
13.2975613554585,14.29557811607,15.2935948766815,16.291611637293,17.2896283979046,
18.287645158516,19.2856619191276,20.2836786797391,21.2816954403506,22.2797122009621,
23.2777289615736,24.2757457221851,25.2737624827966,26.2717792434081,27.2697960040196,
28.2678127646311,29.2658295252426,30.2638462858541,31.2618630464656,32.2598798070771,
33.2578965676886,34.2559133283001,35.2539300889116,36.2519468495231,37.2499636101346,
38.2479803707461,39.2459971313576,40.2440138919691,41.2420306525806,42.2400474131921,
43.2380641738036,44.2360809344151,45.2340976950266,46.2321144556381,47.2301312162496,
48.2281479768611,49.2261647374726,50.2241814980841,51.2221982586956,52.2202150193071,
53.2182317799186,54.2162485405301,55.2142653011416,56.2122820617531,57.2102988223646,
58.2083155829761,59.2063323435876,60.2043491041991,61.2023658648106,62.2003826254221,
63.1983993860336,64.1964161466451,65.1944329072566,66.1924496678681,67.1904664284796,
68.1884831890911,69.1864999497026,70.1845167103141,71.1825334709256,72.1805502315371,
73.1785669921486,74.1765837527601,75.1746005133716,76.1726172739831,77.1706340345946,
78.1686507952061,79.1666675558176,80.1646843164291,81.1627010770406,82.1607178376521,
83.1587345982636,84.1567513588751,85.1547681194866,86.1527848800981,87.1508016407096,
88.1488184013211,89.1468351619326,90.1448519225441,91.1428686831556,92.1408854437671,
93.1389022043786,94.1369189649901,95.1349357256016,96.1329524862131,97.1309692468246,
98.1289860074361,99.1270027680476,100.125019528659,101.123036289271,102.121053049882,
103.119069810494,104.117086571105,105.115103331717,106.113120092328,107.11113685294,
108.109153613551,109.107170374163,110.105187134774,111.103203895386,112.101220655997,
113.099237416609,114.09725417722,115.095270937832,116.093287698443,117.091304459055,
118.089321219666,119.087337980278,120.085354740889,121.083371501501,122.081388262112,
123.079405022724,124.077421783335,125.075438543947,126.073455304558,127.07147206517,
128.069488825781,129.067505586393,130.065522347004,131.064028202745),
 .UNSPECIFIED.);
#257=B_SPLINE_SURFACE_WITH_KNOTS('',3,3,((#76851,#76852,#76853,#76854,#76855,
#76856,#76857,#76858,#76859,#76860,#76861,#76862,#76863,#76864,#76865,#76866,
#76867,#76868,#76869,#76870,#76871,#76872,#76873,#76874,#76875,#76876,#76877,
#76878,#76879,#76880,#76881,#76882,#76883,#76884,#76885,#76886,#76887,#76888,
#76889,#76890,#76891,#76892,#76893,#76894,#76895,#76896,#76897,#76898,#76899,
#76900,#76901,#76902,#76903,#76904,#76905,#76906,#76907,#76908,#76909,#76910,
#76911,#76912,#76913,#76914,#76915,#76916,#76917,#76918,#76919,#76920,#76921,
#76922,#76923,#76924,#76925,#76926,#76927,#76928,#76929,#76930,#76931,#76932,
#76933,#76934,#76935,#76936,#76937,#76938,#76939,#76940,#76941,#76942,#76943,
#76944,#76945,#76946,#76947,#76948,#76949,#76950,#76951,#76952,#76953,#76954,
#76955,#76956,#76957,#76958,#76959,#76960,#76961,#76962,#76963,#76964,#76965,
#76966,#76967,#76968,#76969,#76970,#76971,#76972,#76973,#76974,#76975,#76976),
(#76977,#76978,#76979,#76980,#76981,#76982,#76983,#76984,#76985,#76986,
#76987,#76988,#76989,#76990,#76991,#76992,#76993,#76994,#76995,#76996,#76997,
#76998,#76999,#77000,#77001,#77002,#77003,#77004,#77005,#77006,#77007,#77008,
#77009,#77010,#77011,#77012,#77013,#77014,#77015,#77016,#77017,#77018,#77019,
#77020,#77021,#77022,#77023,#77024,#77025,#77026,#77027,#77028,#77029,#77030,
#77031,#77032,#77033,#77034,#77035,#77036,#77037,#77038,#77039,#77040,#77041,
#77042,#77043,#77044,#77045,#77046,#77047,#77048,#77049,#77050,#77051,#77052,
#77053,#77054,#77055,#77056,#77057,#77058,#77059,#77060,#77061,#77062,#77063,
#77064,#77065,#77066,#77067,#77068,#77069,#77070,#77071,#77072,#77073,#77074,
#77075,#77076,#77077,#77078,#77079,#77080,#77081,#77082,#77083,#77084,#77085,
#77086,#77087,#77088,#77089,#77090,#77091,#77092,#77093,#77094,#77095,#77096,
#77097,#77098,#77099,#77100,#77101,#77102),(#77103,#77104,#77105,#77106,
#77107,#77108,#77109,#77110,#77111,#77112,#77113,#77114,#77115,#77116,#77117,
#77118,#77119,#77120,#77121,#77122,#77123,#77124,#77125,#77126,#77127,#77128,
#77129,#77130,#77131,#77132,#77133,#77134,#77135,#77136,#77137,#77138,#77139,
#77140,#77141,#77142,#77143,#77144,#77145,#77146,#77147,#77148,#77149,#77150,
#77151,#77152,#77153,#77154,#77155,#77156,#77157,#77158,#77159,#77160,#77161,
#77162,#77163,#77164,#77165,#77166,#77167,#77168,#77169,#77170,#77171,#77172,
#77173,#77174,#77175,#77176,#77177,#77178,#77179,#77180,#77181,#77182,#77183,
#77184,#77185,#77186,#77187,#77188,#77189,#77190,#77191,#77192,#77193,#77194,
#77195,#77196,#77197,#77198,#77199,#77200,#77201,#77202,#77203,#77204,#77205,
#77206,#77207,#77208,#77209,#77210,#77211,#77212,#77213,#77214,#77215,#77216,
#77217,#77218,#77219,#77220,#77221,#77222,#77223,#77224,#77225,#77226,#77227,
#77228),(#77229,#77230,#77231,#77232,#77233,#77234,#77235,#77236,#77237,
#77238,#77239,#77240,#77241,#77242,#77243,#77244,#77245,#77246,#77247,#77248,
#77249,#77250,#77251,#77252,#77253,#77254,#77255,#77256,#77257,#77258,#77259,
#77260,#77261,#77262,#77263,#77264,#77265,#77266,#77267,#77268,#77269,#77270,
#77271,#77272,#77273,#77274,#77275,#77276,#77277,#77278,#77279,#77280,#77281,
#77282,#77283,#77284,#77285,#77286,#77287,#77288,#77289,#77290,#77291,#77292,
#77293,#77294,#77295,#77296,#77297,#77298,#77299,#77300,#77301,#77302,#77303,
#77304,#77305,#77306,#77307,#77308,#77309,#77310,#77311,#77312,#77313,#77314,
#77315,#77316,#77317,#77318,#77319,#77320,#77321,#77322,#77323,#77324,#77325,
#77326,#77327,#77328,#77329,#77330,#77331,#77332,#77333,#77334,#77335,#77336,
#77337,#77338,#77339,#77340,#77341,#77342,#77343,#77344,#77345,#77346,#77347,
#77348,#77349,#77350,#77351,#77352,#77353,#77354)),.UNSPECIFIED.,.F.,.F.,
 .F.,(4,4),(4,1,1,1,1,1,1,1,1,1,1,1,1,1,1,1,1,1,1,1,1,1,1,1,1,1,1,1,1,1,
1,1,1,1,1,1,1,1,1,1,1,1,1,1,1,1,1,1,1,1,1,1,1,1,1,1,1,1,1,1,1,1,1,1,1,1,
1,1,1,1,1,1,1,1,1,1,1,1,1,1,1,1,1,1,1,1,1,1,1,1,1,1,1,1,1,1,1,1,1,1,1,1,
1,1,1,1,1,1,1,1,1,1,1,1,1,1,1,1,1,1,1,1,1,4),(-0.000418746624015696,0.0663359285465069),
(11.6145437174728,12.6130496084297,13.6110663690412,14.6090831296527,15.6070998902642,
16.6051166508757,17.6031334114872,18.6011501720987,19.5991669327102,20.5971836933217,
21.5952004539332,22.5932172145448,23.5912339751562,24.5892507357678,25.5872674963793,
26.5852842569908,27.5833010176023,28.5813177782138,29.5793345388253,30.5773512994368,
31.5753680600483,32.5733848206598,33.5714015812713,34.5694183418828,35.5674351024943,
36.5654518631058,37.5634686237173,38.5614853843288,39.5595021449403,40.5575189055518,
41.5555356661633,42.5535524267748,43.5515691873863,44.5495859479978,45.5476027086093,
46.5456194692208,47.5436362298323,48.5416529904438,49.5396697510553,50.5376865116668,
51.5357032722783,52.5337200328898,53.5317367935013,54.5297535541128,55.5277703147243,
56.5257870753358,57.5238038359473,58.5218205965588,59.5198373571703,60.5178541177818,
61.5158708783933,62.5138876390048,63.5119043996163,64.5099211602278,65.5079379208393,
66.5059546814508,67.5039714420623,68.5019882026738,69.5000049632853,70.4980217238968,
71.4960384845083,72.4940552451198,73.4920720057313,74.4900887663428,75.4881055269543,
76.4861222875658,77.4841390481773,78.4821558087888,79.4801725694003,80.4781893300118,
81.4762060906233,82.4742228512348,83.4722396118463,84.4702563724578,85.4682731330693,
86.4662898936808,87.4643066542923,88.4623234149038,89.4603401755153,90.4583569361268,
91.4563736967383,92.4543904573498,93.4524072179613,94.4504239785728,95.4484407391843,
96.4464574997958,97.4444742604073,98.4424910210188,99.4405077816303,100.438524542242,
101.436541302853,102.434558063465,103.432574824076,104.430591584688,105.428608345299,
106.426625105911,107.424641866522,108.422658627134,109.420675387745,110.418692148357,
111.416708908968,112.41472566958,113.412742430191,114.410759190803,115.408775951414,
116.406792712026,117.404809472637,118.402826233249,119.40084299386,120.398859754472,
121.396876515083,122.394893275695,123.392910036306,124.390926796918,125.388943557529,
126.386960318141,127.384977078752,128.382993839364,129.381010599975,130.379027360587,
131.377044121198,132.37506088181,133.373077642421,134.371094403033),
 .UNSPECIFIED.);
#258=B_SPLINE_SURFACE_WITH_KNOTS('',3,3,((#85302,#85303,#85304,#85305,#85306,
#85307,#85308,#85309,#85310,#85311,#85312,#85313,#85314,#85315,#85316,#85317,
#85318,#85319,#85320,#85321,#85322,#85323,#85324,#85325,#85326,#85327,#85328,
#85329,#85330,#85331,#85332,#85333,#85334,#85335,#85336,#85337,#85338,#85339,
#85340,#85341,#85342,#85343,#85344,#85345,#85346,#85347,#85348,#85349,#85350,
#85351,#85352,#85353,#85354,#85355,#85356,#85357,#85358,#85359,#85360,#85361,
#85362,#85363,#85364,#85365,#85366,#85367,#85368,#85369,#85370,#85371,#85372,
#85373,#85374,#85375,#85376,#85377,#85378,#85379,#85380,#85381,#85382,#85383,
#85384,#85385,#85386,#85387,#85388,#85389,#85390,#85391,#85392,#85393,#85394,
#85395,#85396,#85397,#85398,#85399,#85400,#85401,#85402),(#85403,#85404,
#85405,#85406,#85407,#85408,#85409,#85410,#85411,#85412,#85413,#85414,#85415,
#85416,#85417,#85418,#85419,#85420,#85421,#85422,#85423,#85424,#85425,#85426,
#85427,#85428,#85429,#85430,#85431,#85432,#85433,#85434,#85435,#85436,#85437,
#85438,#85439,#85440,#85441,#85442,#85443,#85444,#85445,#85446,#85447,#85448,
#85449,#85450,#85451,#85452,#85453,#85454,#85455,#85456,#85457,#85458,#85459,
#85460,#85461,#85462,#85463,#85464,#85465,#85466,#85467,#85468,#85469,#85470,
#85471,#85472,#85473,#85474,#85475,#85476,#85477,#85478,#85479,#85480,#85481,
#85482,#85483,#85484,#85485,#85486,#85487,#85488,#85489,#85490,#85491,#85492,
#85493,#85494,#85495,#85496,#85497,#85498,#85499,#85500,#85501,#85502,#85503),
(#85504,#85505,#85506,#85507,#85508,#85509,#85510,#85511,#85512,#85513,
#85514,#85515,#85516,#85517,#85518,#85519,#85520,#85521,#85522,#85523,#85524,
#85525,#85526,#85527,#85528,#85529,#85530,#85531,#85532,#85533,#85534,#85535,
#85536,#85537,#85538,#85539,#85540,#85541,#85542,#85543,#85544,#85545,#85546,
#85547,#85548,#85549,#85550,#85551,#85552,#85553,#85554,#85555,#85556,#85557,
#85558,#85559,#85560,#85561,#85562,#85563,#85564,#85565,#85566,#85567,#85568,
#85569,#85570,#85571,#85572,#85573,#85574,#85575,#85576,#85577,#85578,#85579,
#85580,#85581,#85582,#85583,#85584,#85585,#85586,#85587,#85588,#85589,#85590,
#85591,#85592,#85593,#85594,#85595,#85596,#85597,#85598,#85599,#85600,#85601,
#85602,#85603,#85604),(#85605,#85606,#85607,#85608,#85609,#85610,#85611,
#85612,#85613,#85614,#85615,#85616,#85617,#85618,#85619,#85620,#85621,#85622,
#85623,#85624,#85625,#85626,#85627,#85628,#85629,#85630,#85631,#85632,#85633,
#85634,#85635,#85636,#85637,#85638,#85639,#85640,#85641,#85642,#85643,#85644,
#85645,#85646,#85647,#85648,#85649,#85650,#85651,#85652,#85653,#85654,#85655,
#85656,#85657,#85658,#85659,#85660,#85661,#85662,#85663,#85664,#85665,#85666,
#85667,#85668,#85669,#85670,#85671,#85672,#85673,#85674,#85675,#85676,#85677,
#85678,#85679,#85680,#85681,#85682,#85683,#85684,#85685,#85686,#85687,#85688,
#85689,#85690,#85691,#85692,#85693,#85694,#85695,#85696,#85697,#85698,#85699,
#85700,#85701,#85702,#85703,#85704,#85705)),.UNSPECIFIED.,.F.,.F.,.F.,(4,
4),(4,1,1,1,1,1,1,1,1,1,1,1,1,1,1,1,1,1,1,1,1,1,1,1,1,1,1,1,1,1,1,1,1,1,
1,1,1,1,1,1,1,1,1,1,1,1,1,1,1,1,1,1,1,1,1,1,1,1,1,1,1,1,1,1,1,1,1,1,1,1,
1,1,1,1,1,1,1,1,1,1,1,1,1,1,1,1,1,1,1,1,1,1,1,1,1,1,1,1,4),(-0.000485376732247951,
0.0662851291984278),(8.30747755240103,9.30363388226323,10.2997902121254,
11.2959465419876,12.2921028718499,13.2882592017121,14.2844155315743,15.2805718614365,
16.2767281912987,17.2728845211609,18.2690408510231,19.2651971808853,20.2613535107475,
21.2575098406097,22.2536661704719,23.2498225003341,24.2459788301963,25.2421351600585,
26.2382914899207,27.234447819783,28.2306041496452,29.2267604795074,30.2229168093696,
31.2190731392318,32.215229469094,33.2113857989562,34.2075421288184,35.2036984586806,
36.1998547885428,37.196011118405,38.1921674482672,39.1883237781294,40.1844801079916,
41.1806364378539,42.1767927677161,43.1729490975783,44.1691054274405,45.1652617573027,
46.1614180871649,47.1575744170271,48.1537307468893,49.1498870767515,50.1460434066137,
51.1421997364759,52.1383560663381,53.1345123962003,54.1306687260625,55.1268250559247,
56.122981385787,57.1191377156492,58.1152940455114,59.1114503753736,60.1076067052358,
61.103763035098,62.0999193649602,63.0960756948224,64.0922320246846,65.0883883545468,
66.084544684409,67.0807010142712,68.0768573441334,69.0730136739956,70.0691700038579,
71.0653263337201,72.0614826635823,73.0576389934445,74.0537953233067,75.0499516531689,
76.0461079830311,77.0422643128933,78.0384206427555,79.0345769726177,80.0307333024799,
81.0268896323421,82.0230459622043,83.0192022920665,84.0153586219288,85.011514951791,
86.0076712816532,87.0038276115154,87.9999839413776,88.9961402712398,89.992296601102,
90.9884529309642,91.9846092608264,92.9807655906886,93.9769219205508,94.973078250413,
95.9692345802752,96.9653909101374,97.9615472399996,98.9577035698618,99.9538598997241,
100.950016229586,101.946172559448,102.942328889311,103.938485219173,104.934641549035,
105.931283255629),.UNSPECIFIED.);
#259=B_SPLINE_SURFACE_WITH_KNOTS('',3,3,((#85831,#85832,#85833,#85834,#85835,
#85836,#85837,#85838,#85839,#85840,#85841,#85842,#85843,#85844,#85845,#85846,
#85847,#85848,#85849,#85850,#85851,#85852,#85853,#85854,#85855,#85856,#85857,
#85858,#85859,#85860,#85861,#85862,#85863,#85864,#85865,#85866,#85867,#85868,
#85869,#85870,#85871,#85872,#85873,#85874,#85875,#85876,#85877,#85878,#85879,
#85880,#85881,#85882,#85883,#85884,#85885,#85886,#85887,#85888,#85889,#85890,
#85891,#85892,#85893,#85894,#85895,#85896,#85897,#85898,#85899,#85900,#85901,
#85902,#85903,#85904,#85905,#85906,#85907,#85908,#85909,#85910,#85911,#85912,
#85913,#85914,#85915,#85916,#85917,#85918,#85919,#85920,#85921,#85922,#85923,
#85924,#85925,#85926,#85927,#85928,#85929,#85930,#85931),(#85932,#85933,
#85934,#85935,#85936,#85937,#85938,#85939,#85940,#85941,#85942,#85943,#85944,
#85945,#85946,#85947,#85948,#85949,#85950,#85951,#85952,#85953,#85954,#85955,
#85956,#85957,#85958,#85959,#85960,#85961,#85962,#85963,#85964,#85965,#85966,
#85967,#85968,#85969,#85970,#85971,#85972,#85973,#85974,#85975,#85976,#85977,
#85978,#85979,#85980,#85981,#85982,#85983,#85984,#85985,#85986,#85987,#85988,
#85989,#85990,#85991,#85992,#85993,#85994,#85995,#85996,#85997,#85998,#85999,
#86000,#86001,#86002,#86003,#86004,#86005,#86006,#86007,#86008,#86009,#86010,
#86011,#86012,#86013,#86014,#86015,#86016,#86017,#86018,#86019,#86020,#86021,
#86022,#86023,#86024,#86025,#86026,#86027,#86028,#86029,#86030,#86031,#86032),
(#86033,#86034,#86035,#86036,#86037,#86038,#86039,#86040,#86041,#86042,
#86043,#86044,#86045,#86046,#86047,#86048,#86049,#86050,#86051,#86052,#86053,
#86054,#86055,#86056,#86057,#86058,#86059,#86060,#86061,#86062,#86063,#86064,
#86065,#86066,#86067,#86068,#86069,#86070,#86071,#86072,#86073,#86074,#86075,
#86076,#86077,#86078,#86079,#86080,#86081,#86082,#86083,#86084,#86085,#86086,
#86087,#86088,#86089,#86090,#86091,#86092,#86093,#86094,#86095,#86096,#86097,
#86098,#86099,#86100,#86101,#86102,#86103,#86104,#86105,#86106,#86107,#86108,
#86109,#86110,#86111,#86112,#86113,#86114,#86115,#86116,#86117,#86118,#86119,
#86120,#86121,#86122,#86123,#86124,#86125,#86126,#86127,#86128,#86129,#86130,
#86131,#86132,#86133),(#86134,#86135,#86136,#86137,#86138,#86139,#86140,
#86141,#86142,#86143,#86144,#86145,#86146,#86147,#86148,#86149,#86150,#86151,
#86152,#86153,#86154,#86155,#86156,#86157,#86158,#86159,#86160,#86161,#86162,
#86163,#86164,#86165,#86166,#86167,#86168,#86169,#86170,#86171,#86172,#86173,
#86174,#86175,#86176,#86177,#86178,#86179,#86180,#86181,#86182,#86183,#86184,
#86185,#86186,#86187,#86188,#86189,#86190,#86191,#86192,#86193,#86194,#86195,
#86196,#86197,#86198,#86199,#86200,#86201,#86202,#86203,#86204,#86205,#86206,
#86207,#86208,#86209,#86210,#86211,#86212,#86213,#86214,#86215,#86216,#86217,
#86218,#86219,#86220,#86221,#86222,#86223,#86224,#86225,#86226,#86227,#86228,
#86229,#86230,#86231,#86232,#86233,#86234)),.UNSPECIFIED.,.F.,.F.,.F.,(4,
4),(4,1,1,1,1,1,1,1,1,1,1,1,1,1,1,1,1,1,1,1,1,1,1,1,1,1,1,1,1,1,1,1,1,1,
1,1,1,1,1,1,1,1,1,1,1,1,1,1,1,1,1,1,1,1,1,1,1,1,1,1,1,1,1,1,1,1,1,1,1,1,
1,1,1,1,1,1,1,1,1,1,1,1,1,1,1,1,1,1,1,1,1,1,1,1,1,1,1,1,4),(-0.000418551673040404,
0.0663322186430087),(11.6145474273763,12.6111891776804,13.6073455075426,
14.6035018374048,15.5996581672671,16.5958144971293,17.5919708269915,18.5881271568537,
19.5842834867159,20.5804398165781,21.5765961464403,22.5727524763025,23.5689088061647,
24.5650651360269,25.5612214658891,26.5573777957513,27.5535341256135,28.5496904554757,
29.545846785338,30.5420031152002,31.5381594450624,32.5343157749246,33.5304721047868,
34.526628434649,35.5227847645112,36.5189410943734,37.5150974242356,38.5112537540978,
39.50741008396,40.5035664138222,41.4997227436844,42.4958790735466,43.4920354034089,
44.4881917332711,45.4843480631333,46.4805043929955,47.4766607228577,48.4728170527199,
49.4689733825821,50.4651297124443,51.4612860423065,52.4574423721687,53.4535987020309,
54.4497550318931,55.4459113617553,56.4420676916176,57.4382240214798,58.434380351342,
59.4305366812042,60.4266930110664,61.4228493409286,62.4190056707908,63.415162000653,
64.4113183305152,65.4074746603774,66.4036309902396,67.3997873201018,68.395943649964,
69.3920999798262,70.3882563096884,71.3844126395506,72.3805689694129,73.3767252992751,
74.3728816291373,75.3690379589995,76.3651942888617,77.3613506187239,78.3575069485861,
79.3536632784483,80.3498196083105,81.3459759381727,82.3421322680349,83.3382885978971,
84.3344449277593,85.3306012576216,86.3267575874838,87.322913917346,88.3190702472082,
89.3152265770704,90.3113829069326,91.3075392367948,92.303695566657,93.2998518965192,
94.2960082263814,95.2921645562436,96.2883208861058,97.284477215968,98.2806335458303,
99.2767898756925,100.272946205555,101.269102535417,102.265258865279,103.261415195141,
104.257571525003,105.253727854866,106.249884184728,107.24604051459,108.242196844452,
109.238353174315),.UNSPECIFIED.);
#260=(
BOUNDED_CURVE()
B_SPLINE_CURVE(2,(#23943,#23944,#23945),.UNSPECIFIED.,.F.,.F.)
B_SPLINE_CURVE_WITH_KNOTS((3,3),(0.,0.0438796975155138),.UNSPECIFIED.)
CURVE()
GEOMETRIC_REPRESENTATION_ITEM()
RATIONAL_B_SPLINE_CURVE((1.,1.00025082231383,1.))
REPRESENTATION_ITEM('')
);
#261=(
BOUNDED_CURVE()
B_SPLINE_CURVE(2,(#23957,#23958,#23959),.UNSPECIFIED.,.F.,.F.)
B_SPLINE_CURVE_WITH_KNOTS((3,3),(0.,0.0438796975155138),.UNSPECIFIED.)
CURVE()
GEOMETRIC_REPRESENTATION_ITEM()
RATIONAL_B_SPLINE_CURVE((1.,1.00025082231383,1.))
REPRESENTATION_ITEM('')
);
#262=(
BOUNDED_CURVE()
B_SPLINE_CURVE(2,(#63092,#63093,#63094),.UNSPECIFIED.,.F.,.F.)
B_SPLINE_CURVE_WITH_KNOTS((3,3),(0.,0.145078131153909),.UNSPECIFIED.)
CURVE()
GEOMETRIC_REPRESENTATION_ITEM()
RATIONAL_B_SPLINE_CURVE((1.,1.00081813630177,1.))
REPRESENTATION_ITEM('')
);
#263=(
BOUNDED_CURVE()
B_SPLINE_CURVE(2,(#63097,#63098,#63099),.UNSPECIFIED.,.F.,.F.)
B_SPLINE_CURVE_WITH_KNOTS((3,3),(0.,0.145078131153909),.UNSPECIFIED.)
CURVE()
GEOMETRIC_REPRESENTATION_ITEM()
RATIONAL_B_SPLINE_CURVE((1.,1.00081813630177,1.))
REPRESENTATION_ITEM('')
);
#264=(
BOUNDED_CURVE()
B_SPLINE_CURVE(2,(#63110,#63111,#63112),.UNSPECIFIED.,.F.,.F.)
B_SPLINE_CURVE_WITH_KNOTS((3,3),(0.,0.145078131153909),.UNSPECIFIED.)
CURVE()
GEOMETRIC_REPRESENTATION_ITEM()
RATIONAL_B_SPLINE_CURVE((1.,1.00081813630177,1.))
REPRESENTATION_ITEM('')
);
#265=(
BOUNDED_CURVE()
B_SPLINE_CURVE(2,(#63116,#63117,#63118),.UNSPECIFIED.,.F.,.F.)
B_SPLINE_CURVE_WITH_KNOTS((3,3),(0.,0.145078131153909),.UNSPECIFIED.)
CURVE()
GEOMETRIC_REPRESENTATION_ITEM()
RATIONAL_B_SPLINE_CURVE((1.,1.00081813630177,1.))
REPRESENTATION_ITEM('')
);
#266=(
BOUNDED_CURVE()
B_SPLINE_CURVE(2,(#66219,#66220,#66221),.UNSPECIFIED.,.F.,.F.)
B_SPLINE_CURVE_WITH_KNOTS((3,3),(-0.639366558443437,-0.433164349146202),
 .UNSPECIFIED.)
CURVE()
GEOMETRIC_REPRESENTATION_ITEM()
RATIONAL_B_SPLINE_CURVE((1.35866716012837,1.4637604307034,1.4637604307034))
REPRESENTATION_ITEM('')
);
#267=(
BOUNDED_CURVE()
B_SPLINE_CURVE(2,(#66223,#66224,#66225),.UNSPECIFIED.,.F.,.F.)
B_SPLINE_CURVE_WITH_KNOTS((3,3),(0.0319010196424348,0.336489692457453),
 .UNSPECIFIED.)
CURVE()
GEOMETRIC_REPRESENTATION_ITEM()
RATIONAL_B_SPLINE_CURVE((1.03712812921102,1.19757240916823,1.03712812921102))
REPRESENTATION_ITEM('')
);
#268=(
BOUNDED_CURVE()
B_SPLINE_CURVE(2,(#66227,#66228,#66229),.UNSPECIFIED.,.F.,.F.)
B_SPLINE_CURVE_WITH_KNOTS((3,3),(0.0319010196424347,0.336489692457453),
 .UNSPECIFIED.)
CURVE()
GEOMETRIC_REPRESENTATION_ITEM()
RATIONAL_B_SPLINE_CURVE((1.03712812921102,1.19757240916823,1.03712812921102))
REPRESENTATION_ITEM('')
);
#269=(
BOUNDED_CURVE()
B_SPLINE_CURVE(2,(#66231,#66232,#66233),.UNSPECIFIED.,.F.,.F.)
B_SPLINE_CURVE_WITH_KNOTS((3,3),(0.0319010196424348,0.336489692457453),
 .UNSPECIFIED.)
CURVE()
GEOMETRIC_REPRESENTATION_ITEM()
RATIONAL_B_SPLINE_CURVE((1.03712812921102,1.19757240916823,1.03712812921102))
REPRESENTATION_ITEM('')
);
#270=(
BOUNDED_CURVE()
B_SPLINE_CURVE(2,(#66235,#66236,#66237),.UNSPECIFIED.,.F.,.F.)
B_SPLINE_CURVE_WITH_KNOTS((3,3),(0.0319010196424349,0.336489692457453),
 .UNSPECIFIED.)
CURVE()
GEOMETRIC_REPRESENTATION_ITEM()
RATIONAL_B_SPLINE_CURVE((1.03712812921102,1.19757240916823,1.03712812921102))
REPRESENTATION_ITEM('')
);
#271=(
BOUNDED_CURVE()
B_SPLINE_CURVE(2,(#66239,#66240,#66241),.UNSPECIFIED.,.F.,.F.)
B_SPLINE_CURVE_WITH_KNOTS((3,3),(0.0319010196424347,0.336489692457453),
 .UNSPECIFIED.)
CURVE()
GEOMETRIC_REPRESENTATION_ITEM()
RATIONAL_B_SPLINE_CURVE((1.03712812921102,1.19757240916823,1.03712812921102))
REPRESENTATION_ITEM('')
);
#272=(
BOUNDED_CURVE()
B_SPLINE_CURVE(2,(#66242,#66243,#66244),.UNSPECIFIED.,.F.,.F.)
B_SPLINE_CURVE_WITH_KNOTS((3,3),(-0.433164349146202,-0.226962139848967),
 .UNSPECIFIED.)
CURVE()
GEOMETRIC_REPRESENTATION_ITEM()
RATIONAL_B_SPLINE_CURVE((1.4637604307034,1.4637604307034,1.35866716012837))
REPRESENTATION_ITEM('')
);
#273=(
BOUNDED_CURVE()
B_SPLINE_CURVE(2,(#77369,#77370,#77371),.UNSPECIFIED.,.F.,.F.)
B_SPLINE_CURVE_WITH_KNOTS((3,3),(-0.639366558443436,-0.433164349146202),
 .UNSPECIFIED.)
CURVE()
GEOMETRIC_REPRESENTATION_ITEM()
RATIONAL_B_SPLINE_CURVE((1.35866716012837,1.4637604307034,1.4637604307034))
REPRESENTATION_ITEM('')
);
#274=(
BOUNDED_CURVE()
B_SPLINE_CURVE(2,(#77373,#77374,#77375),.UNSPECIFIED.,.F.,.F.)
B_SPLINE_CURVE_WITH_KNOTS((3,3),(0.0319010196424347,0.336489692457453),
 .UNSPECIFIED.)
CURVE()
GEOMETRIC_REPRESENTATION_ITEM()
RATIONAL_B_SPLINE_CURVE((1.03712812921102,1.19757240916823,1.03712812921102))
REPRESENTATION_ITEM('')
);
#275=(
BOUNDED_CURVE()
B_SPLINE_CURVE(2,(#77377,#77378,#77379),.UNSPECIFIED.,.F.,.F.)
B_SPLINE_CURVE_WITH_KNOTS((3,3),(0.0319010196424348,0.336489692457454),
 .UNSPECIFIED.)
CURVE()
GEOMETRIC_REPRESENTATION_ITEM()
RATIONAL_B_SPLINE_CURVE((1.03712812921102,1.19757240916823,1.03712812921102))
REPRESENTATION_ITEM('')
);
#276=(
BOUNDED_CURVE()
B_SPLINE_CURVE(2,(#77381,#77382,#77383),.UNSPECIFIED.,.F.,.F.)
B_SPLINE_CURVE_WITH_KNOTS((3,3),(0.031901019642435,0.336489692457454),
 .UNSPECIFIED.)
CURVE()
GEOMETRIC_REPRESENTATION_ITEM()
RATIONAL_B_SPLINE_CURVE((1.03712812921102,1.19757240916823,1.03712812921102))
REPRESENTATION_ITEM('')
);
#277=(
BOUNDED_CURVE()
B_SPLINE_CURVE(2,(#77385,#77386,#77387),.UNSPECIFIED.,.F.,.F.)
B_SPLINE_CURVE_WITH_KNOTS((3,3),(0.0319010196424349,0.336489692457453),
 .UNSPECIFIED.)
CURVE()
GEOMETRIC_REPRESENTATION_ITEM()
RATIONAL_B_SPLINE_CURVE((1.03712812921102,1.19757240916823,1.03712812921102))
REPRESENTATION_ITEM('')
);
#278=(
BOUNDED_CURVE()
B_SPLINE_CURVE(2,(#77389,#77390,#77391),.UNSPECIFIED.,.F.,.F.)
B_SPLINE_CURVE_WITH_KNOTS((3,3),(0.0319010196424348,0.336489692457453),
 .UNSPECIFIED.)
CURVE()
GEOMETRIC_REPRESENTATION_ITEM()
RATIONAL_B_SPLINE_CURVE((1.03712812921102,1.19757240916823,1.03712812921102))
REPRESENTATION_ITEM('')
);
#279=(
BOUNDED_CURVE()
B_SPLINE_CURVE(2,(#77392,#77393,#77394),.UNSPECIFIED.,.F.,.F.)
B_SPLINE_CURVE_WITH_KNOTS((3,3),(-0.433164349146202,-0.226962139848967),
 .UNSPECIFIED.)
CURVE()
GEOMETRIC_REPRESENTATION_ITEM()
RATIONAL_B_SPLINE_CURVE((1.4637604307034,1.4637604307034,1.35866716012837))
REPRESENTATION_ITEM('')
);
#280=(
BOUNDED_CURVE()
B_SPLINE_CURVE(2,(#86249,#86250,#86251),.UNSPECIFIED.,.F.,.F.)
B_SPLINE_CURVE_WITH_KNOTS((3,3),(-0.639366558443436,-0.433164349146202),
 .UNSPECIFIED.)
CURVE()
GEOMETRIC_REPRESENTATION_ITEM()
RATIONAL_B_SPLINE_CURVE((1.35866716012837,1.4637604307034,1.4637604307034))
REPRESENTATION_ITEM('')
);
#281=(
BOUNDED_CURVE()
B_SPLINE_CURVE(2,(#86253,#86254,#86255),.UNSPECIFIED.,.F.,.F.)
B_SPLINE_CURVE_WITH_KNOTS((3,3),(0.0319010196424347,0.336489692457453),
 .UNSPECIFIED.)
CURVE()
GEOMETRIC_REPRESENTATION_ITEM()
RATIONAL_B_SPLINE_CURVE((1.03712812921102,1.19757240916823,1.03712812921102))
REPRESENTATION_ITEM('')
);
#282=(
BOUNDED_CURVE()
B_SPLINE_CURVE(2,(#86257,#86258,#86259),.UNSPECIFIED.,.F.,.F.)
B_SPLINE_CURVE_WITH_KNOTS((3,3),(0.0319010196424348,0.336489692457454),
 .UNSPECIFIED.)
CURVE()
GEOMETRIC_REPRESENTATION_ITEM()
RATIONAL_B_SPLINE_CURVE((1.03712812921102,1.19757240916823,1.03712812921102))
REPRESENTATION_ITEM('')
);
#283=(
BOUNDED_CURVE()
B_SPLINE_CURVE(2,(#86261,#86262,#86263),.UNSPECIFIED.,.F.,.F.)
B_SPLINE_CURVE_WITH_KNOTS((3,3),(0.031901019642435,0.336489692457454),
 .UNSPECIFIED.)
CURVE()
GEOMETRIC_REPRESENTATION_ITEM()
RATIONAL_B_SPLINE_CURVE((1.03712812921102,1.19757240916823,1.03712812921102))
REPRESENTATION_ITEM('')
);
#284=(
BOUNDED_CURVE()
B_SPLINE_CURVE(2,(#86265,#86266,#86267),.UNSPECIFIED.,.F.,.F.)
B_SPLINE_CURVE_WITH_KNOTS((3,3),(0.0319010196424349,0.336489692457453),
 .UNSPECIFIED.)
CURVE()
GEOMETRIC_REPRESENTATION_ITEM()
RATIONAL_B_SPLINE_CURVE((1.03712812921102,1.19757240916823,1.03712812921102))
REPRESENTATION_ITEM('')
);
#285=(
BOUNDED_CURVE()
B_SPLINE_CURVE(2,(#86269,#86270,#86271),.UNSPECIFIED.,.F.,.F.)
B_SPLINE_CURVE_WITH_KNOTS((3,3),(0.0319010196424348,0.336489692457453),
 .UNSPECIFIED.)
CURVE()
GEOMETRIC_REPRESENTATION_ITEM()
RATIONAL_B_SPLINE_CURVE((1.03712812921102,1.19757240916823,1.03712812921102))
REPRESENTATION_ITEM('')
);
#286=(
BOUNDED_CURVE()
B_SPLINE_CURVE(2,(#86272,#86273,#86274),.UNSPECIFIED.,.F.,.F.)
B_SPLINE_CURVE_WITH_KNOTS((3,3),(-0.433164349146202,-0.226962139848967),
 .UNSPECIFIED.)
CURVE()
GEOMETRIC_REPRESENTATION_ITEM()
RATIONAL_B_SPLINE_CURVE((1.4637604307034,1.4637604307034,1.35866716012837))
REPRESENTATION_ITEM('')
);
#287=SHAPE_REPRESENTATION_RELATIONSHIP('SRR','None',#86502,#305);
#288=SHAPE_REPRESENTATION_RELATIONSHIP('SRR','None',#86503,#306);
#289=SHAPE_REPRESENTATION_RELATIONSHIP('SRR','None',#86504,#307);
#290=SHAPE_REPRESENTATION_RELATIONSHIP('SRR','None',#86505,#308);
#291=SHAPE_REPRESENTATION_RELATIONSHIP('SRR','None',#86506,#309);
#292=SHAPE_REPRESENTATION_RELATIONSHIP('SRR','None',#86507,#310);
#293=SHAPE_REPRESENTATION_RELATIONSHIP('SRR','None',#86508,#311);
#294=SHAPE_REPRESENTATION_RELATIONSHIP('SRR','None',#86509,#312);
#295=SHAPE_REPRESENTATION_RELATIONSHIP('SRR','None',#86510,#313);
#296=SHAPE_REPRESENTATION_RELATIONSHIP('SRR','None',#86511,#314);
#297=SHAPE_REPRESENTATION_RELATIONSHIP('SRR','None',#86512,#315);
#298=SHAPE_REPRESENTATION_RELATIONSHIP('SRR','None',#86513,#316);
#299=SHAPE_REPRESENTATION_RELATIONSHIP('SRR','None',#86514,#317);
#300=SHAPE_REPRESENTATION_RELATIONSHIP('SRR','None',#86515,#318);
#301=SHAPE_REPRESENTATION_RELATIONSHIP('SRR','None',#86516,#319);
#302=SHAPE_REPRESENTATION_RELATIONSHIP('SRR','None',#86517,#320);
#303=SHAPE_REPRESENTATION_RELATIONSHIP('SRR','None',#86518,#321);
#304=SHAPE_REPRESENTATION_RELATIONSHIP('SRR','None',#86519,#322);
#305=ADVANCED_BREP_SHAPE_REPRESENTATION('',(#341),#86411);
#306=ADVANCED_BREP_SHAPE_REPRESENTATION('',(#342),#86412);
#307=ADVANCED_BREP_SHAPE_REPRESENTATION('',(#343),#86413);
#308=ADVANCED_BREP_SHAPE_REPRESENTATION('',(#344),#86414);
#309=ADVANCED_BREP_SHAPE_REPRESENTATION('',(#345),#86415);
#310=ADVANCED_BREP_SHAPE_REPRESENTATION('',(#346),#86416);
#311=ADVANCED_BREP_SHAPE_REPRESENTATION('',(#347),#86417);
#312=ADVANCED_BREP_SHAPE_REPRESENTATION('',(#348),#86418);
#313=ADVANCED_BREP_SHAPE_REPRESENTATION('',(#349),#86419);
#314=ADVANCED_BREP_SHAPE_REPRESENTATION('',(#350),#86420);
#315=ADVANCED_BREP_SHAPE_REPRESENTATION('',(#351),#86421);
#316=ADVANCED_BREP_SHAPE_REPRESENTATION('',(#352),#86422);
#317=ADVANCED_BREP_SHAPE_REPRESENTATION('',(#353),#86423);
#318=ADVANCED_BREP_SHAPE_REPRESENTATION('',(#354),#86424);
#319=ADVANCED_BREP_SHAPE_REPRESENTATION('',(#355),#86425);
#320=ADVANCED_BREP_SHAPE_REPRESENTATION('',(#356),#86426);
#321=ADVANCED_BREP_SHAPE_REPRESENTATION('',(#357),#86427);
#322=ADVANCED_BREP_SHAPE_REPRESENTATION('',(#358),#86428);
#323=STYLED_ITEM('',(#86601),#341);
#324=STYLED_ITEM('',(#86602),#342);
#325=STYLED_ITEM('',(#86603),#343);
#326=STYLED_ITEM('',(#86604),#344);
#327=STYLED_ITEM('',(#86605),#345);
#328=STYLED_ITEM('',(#86606),#346);
#329=STYLED_ITEM('',(#86607),#347);
#330=STYLED_ITEM('',(#86608),#348);
#331=STYLED_ITEM('',(#86609),#349);
#332=STYLED_ITEM('',(#86610),#350);
#333=STYLED_ITEM('',(#86611),#351);
#334=STYLED_ITEM('',(#86612),#352);
#335=STYLED_ITEM('',(#86613),#353);
#336=STYLED_ITEM('',(#86614),#354);
#337=STYLED_ITEM('',(#86615),#355);
#338=STYLED_ITEM('',(#86616),#356);
#339=STYLED_ITEM('',(#86617),#357);
#340=STYLED_ITEM('',(#86611),#358);
#341=MANIFOLD_SOLID_BREP('Body1',#15613);
#342=MANIFOLD_SOLID_BREP('Body1',#15614);
#343=MANIFOLD_SOLID_BREP('Body1',#15615);
#344=MANIFOLD_SOLID_BREP('Body1',#15616);
#345=MANIFOLD_SOLID_BREP('Body1',#15617);
#346=MANIFOLD_SOLID_BREP('Body1',#15618);
#347=MANIFOLD_SOLID_BREP('Body1',#15619);
#348=MANIFOLD_SOLID_BREP('Body1',#15620);
#349=MANIFOLD_SOLID_BREP('Body1',#15621);
#350=MANIFOLD_SOLID_BREP('Body1',#15622);
#351=MANIFOLD_SOLID_BREP('Body1',#15623);
#352=MANIFOLD_SOLID_BREP('Body1',#15624);
#353=MANIFOLD_SOLID_BREP('Body1',#15625);
#354=MANIFOLD_SOLID_BREP('Body1',#15626);
#355=MANIFOLD_SOLID_BREP('Body1',#15627);
#356=MANIFOLD_SOLID_BREP('Body1',#15628);
#357=MANIFOLD_SOLID_BREP('Body1',#15629);
#358=MANIFOLD_SOLID_BREP('Body1',#15630);
#359=ELLIPSE('',#15940,151.19389506818,3.23363209990621);
#360=ELLIPSE('',#15943,151.194075359537,3.2336340714008);
#361=ELLIPSE('',#15952,151.194380471967,3.23363740533001);
#362=ELLIPSE('',#15955,151.194647853758,3.23364033017112);
#363=B_SPLINE_CURVE_WITH_KNOTS('',3,(#21563,#21564,#21565,#21566),
 .UNSPECIFIED.,.F.,.F.,(4,4),(-0.201492965018242,0.),.UNSPECIFIED.);
#364=B_SPLINE_CURVE_WITH_KNOTS('',3,(#21569,#21570,#21571,#21572),
 .UNSPECIFIED.,.F.,.F.,(4,4),(-0.195594022319034,0.),.UNSPECIFIED.);
#365=B_SPLINE_CURVE_WITH_KNOTS('',3,(#21589,#21590,#21591,#21592),
 .UNSPECIFIED.,.F.,.F.,(4,4),(-0.201492965018205,0.),.UNSPECIFIED.);
#366=B_SPLINE_CURVE_WITH_KNOTS('',3,(#21598,#21599,#21600,#21601),
 .UNSPECIFIED.,.F.,.F.,(4,4),(-0.201492965018185,0.),.UNSPECIFIED.);
#367=B_SPLINE_CURVE_WITH_KNOTS('',3,(#21620,#21621,#21622,#21623),
 .UNSPECIFIED.,.F.,.F.,(4,4),(-0.201492965018191,0.),.UNSPECIFIED.);
#368=B_SPLINE_CURVE_WITH_KNOTS('',3,(#21629,#21630,#21631,#21632),
 .UNSPECIFIED.,.F.,.F.,(4,4),(-0.195594022319061,0.),.UNSPECIFIED.);
#369=B_SPLINE_CURVE_WITH_KNOTS('',3,(#21638,#21639,#21640,#21641),
 .UNSPECIFIED.,.F.,.F.,(4,4),(-0.195594022319045,0.),.UNSPECIFIED.);
#370=B_SPLINE_CURVE_WITH_KNOTS('',3,(#21647,#21648,#21649,#21650),
 .UNSPECIFIED.,.F.,.F.,(4,4),(-0.195594022319043,0.),.UNSPECIFIED.);
#371=B_SPLINE_CURVE_WITH_KNOTS('',3,(#21681,#21682,#21683,#21684,#21685,
#21686,#21687,#21688,#21689,#21690),.UNSPECIFIED.,.F.,.F.,(4,2,2,2,4),(-3.05436467918173,
-2.86345905577985,-2.67255343237797,-2.48166347088213,-2.2907735093863),
 .UNSPECIFIED.);
#372=B_SPLINE_CURVE_WITH_KNOTS('',3,(#21691,#21692,#21693,#21694,#21695,
#21696,#21697,#21698,#21699,#21700,#21701,#21702,#21703,#21704,#21705,#21706,
#21707,#21708,#21709,#21710,#21711,#21712,#21713,#21714,#21715,#21716),
 .UNSPECIFIED.,.F.,.F.,(4,2,2,2,2,2,2,2,2,2,2,2,4),(-2.2907735093863,-2.09988354789047,
-1.90899358639463,-1.71808796299275,-1.52718233959087,-1.33627671618898,
-1.1453710927871,-0.954481131291268,-0.763591169795433,-0.572701208299599,
-0.381811246803764,-0.190905623401882,0.),.UNSPECIFIED.);
#373=B_SPLINE_CURVE_WITH_KNOTS('',3,(#21733,#21734,#21735,#21736,#21737,
#21738,#21739,#21740,#21741,#21742,#21743,#21744,#21745,#21746),
 .UNSPECIFIED.,.F.,.F.,(4,2,2,2,2,2,4),(-1.32169585665546,-1.18688181797703,
-1.0520677792986,-0.988183485413416,-0.924299191528231,-0.792573559927981,
-0.660847928327731),.UNSPECIFIED.);
#374=B_SPLINE_CURVE_WITH_KNOTS('',3,(#21748,#21749,#21750,#21751,#21752,
#21753,#21754,#21755,#21756,#21757,#21758,#21759,#21760,#21761),
 .UNSPECIFIED.,.F.,.F.,(4,2,2,2,2,2,4),(0.660847928327731,0.792573559927981,
0.924299191528231,0.988183485413416,1.0520677792986,1.18688181797703,1.32169585665546),
 .UNSPECIFIED.);
#375=B_SPLINE_CURVE_WITH_KNOTS('',3,(#21765,#21766,#21767,#21768,#21769,
#21770,#21771,#21772,#21773,#21774,#21775,#21776,#21777,#21778,#21779,#21780,
#21781,#21782,#21783,#21784,#21785,#21786,#21787,#21788,#21789,#21790,#21791),
 .UNSPECIFIED.,.F.,.F.,(4,2,2,2,2,2,3,2,2,2,2,2,4),(-0.660847928327731,
-0.529122296727481,-0.39739666512723,-0.333512371242046,-0.269628077356861,
-0.134814038678431,0.,0.13481403867843,0.269628077356861,0.333512371242045,
0.39739666512723,0.52912229672748,0.660847928327731),.UNSPECIFIED.);
#376=B_SPLINE_CURVE_WITH_KNOTS('',3,(#21798,#21799,#21800,#21801,#21802,
#21803,#21804,#21805,#21806,#21807),.UNSPECIFIED.,.F.,.F.,(4,2,2,2,4),(0.858794530961258,
0.902694826940309,1.07577532936191,1.25459835745813,1.29336839957273),
 .UNSPECIFIED.);
#377=B_SPLINE_CURVE_WITH_KNOTS('',3,(#21893,#21894,#21895,#21896,#21897,
#21898,#21899,#21900,#21901,#21902,#21903,#21904,#21905,#21906,#21907,#21908,
#21909,#21910,#21911,#21912,#21913,#21914,#21915,#21916,#21917,#21918),
 .UNSPECIFIED.,.F.,.F.,(4,2,2,2,2,2,2,2,2,2,2,2,4),(-1.32169585665546,-1.18688181797703,
-1.0520677792986,-0.988183485413416,-0.924299191528231,-0.792573559927981,
-0.660847928327731,-0.529122296727481,-0.39739666512723,-0.333512371242046,
-0.269628077356861,-0.134814038678431,0.),.UNSPECIFIED.);
#378=B_SPLINE_CURVE_WITH_KNOTS('',3,(#21919,#21920,#21921,#21922,#21923,
#21924,#21925,#21926,#21927,#21928,#21929,#21930,#21931,#21932,#21933,#21934,
#21935,#21936,#21937,#21938,#21939,#21940,#21941,#21942,#21943,#21944),
 .UNSPECIFIED.,.F.,.F.,(4,2,2,2,2,2,2,2,2,2,2,2,4),(0.,0.13481403867843,
0.269628077356861,0.333512371242045,0.39739666512723,0.52912229672748,0.660847928327731,
0.792573559927981,0.924299191528231,0.988183485413416,1.0520677792986,1.18688181797703,
1.32169585665546),.UNSPECIFIED.);
#379=B_SPLINE_CURVE_WITH_KNOTS('',3,(#21947,#21948,#21949,#21950,#21951,
#21952,#21953,#21954,#21955,#21956),.UNSPECIFIED.,.F.,.F.,(4,2,2,2,4),(0.877716942395265,
0.916486984509874,1.09531001260609,1.26839051502769,1.31229081100675),
 .UNSPECIFIED.);
#380=B_SPLINE_CURVE_WITH_KNOTS('',3,(#21958,#21959,#21960,#21961,#21962,
#21963,#21964,#21965,#21966,#21967,#21968,#21969,#21970,#21971,#21972,#21973,
#21974,#21975,#21976,#21977,#21978,#21979,#21980),.UNSPECIFIED.,.F.,.F.,
(4,2,2,2,2,3,2,2,2,2,4),(1.51638402057123,1.52276019461865,1.58643945940805,
1.65011872419746,1.7823849294906,1.91465113478373,2.04691734007687,2.17918354537001,
2.24286281015941,2.30654207494882,2.31291824899624),.UNSPECIFIED.);
#381=B_SPLINE_CURVE_WITH_KNOTS('',3,(#21981,#21982,#21983,#21984,#21985,
#21986,#21987,#21988,#21989,#21990,#21991,#21992,#21993,#21994,#21995,#21996,
#21997,#21998,#21999,#22000,#22001,#22002,#22003),.UNSPECIFIED.,.F.,.F.,
(4,2,2,2,2,3,2,2,2,2,4),(1.51638402057122,1.52276019461865,1.58643945940805,
1.65011872419746,1.7823849294906,1.91465113478373,2.04691734007687,2.17918354537001,
2.24286281015942,2.30654207494882,2.31291824899624),.UNSPECIFIED.);
#382=B_SPLINE_CURVE_WITH_KNOTS('',3,(#22016,#22017,#22018,#22019,#22020,
#22021,#22022,#22023,#22024,#22025),.UNSPECIFIED.,.F.,.F.,(4,2,2,2,4),(0.877716942395273,
0.916486984509874,1.09531001260609,1.26839051502769,1.31229081100674),
 .UNSPECIFIED.);
#383=B_SPLINE_CURVE_WITH_KNOTS('',3,(#22028,#22029,#22030,#22031,#22032,
#22033,#22034,#22035,#22036,#22037),.UNSPECIFIED.,.F.,.F.,(4,2,2,2,4),(0.858794530961249,
0.902694826940311,1.07577532936191,1.25459835745813,1.29336839957274),
 .UNSPECIFIED.);
#384=B_SPLINE_CURVE_WITH_KNOTS('',3,(#22453,#22454,#22455,#22456,#22457,
#22458,#22459,#22460,#22461,#22462,#22463,#22464,#22465,#22466,#22467,#22468,
#22469,#22470),.UNSPECIFIED.,.F.,.F.,(4,2,2,2,2,2,2,2,4),(-9.41073061373359,
-8.52189532994956,-7.63306004616553,-6.7442247623815,-5.85538947859747,
-5.5678834356648,-5.28037739273213,-4.99287134979946,-4.70536530686679),
 .UNSPECIFIED.);
#385=B_SPLINE_CURVE_WITH_KNOTS('',3,(#22472,#22473,#22474,#22475,#22476,
#22477,#22478,#22479,#22480,#22481,#22482,#22483,#22484,#22485,#22486,#22487,
#22488,#22489),.UNSPECIFIED.,.F.,.F.,(4,2,2,2,2,2,2,2,4),(4.70536530686679,
4.99287134979946,5.28037739273213,5.5678834356648,5.85538947859747,6.7442247623815,
7.63306004616553,8.52189532994956,9.41073061373359),.UNSPECIFIED.);
#386=B_SPLINE_CURVE_WITH_KNOTS('',3,(#22493,#22494,#22495,#22496,#22497,
#22498,#22499,#22500,#22501,#22502,#22503,#22504,#22505,#22506,#22507,#22508,
#22509,#22510,#22511,#22512,#22513,#22514,#22515,#22516,#22517,#22518,#22519,
#22520,#22521,#22522,#22523,#22524,#22525,#22526,#22527),.UNSPECIFIED.,
 .F.,.F.,(4,2,2,2,2,2,2,2,3,2,2,2,2,2,2,2,4),(-4.70536530686679,-4.41785926393413,
-4.13035322100146,-3.84284717806879,-3.55534113513612,-2.66650585135209,
-1.77767056756806,-0.888835283784031,0.,0.888835283784029,1.77767056756806,
2.66650585135209,3.55534113513612,3.84284717806879,4.13035322100146,4.41785926393413,
4.70536530686679),.UNSPECIFIED.);
#387=B_SPLINE_CURVE_WITH_KNOTS('',3,(#22589,#22590,#22591,#22592),
 .UNSPECIFIED.,.F.,.F.,(4,4),(-0.195594022319082,0.),.UNSPECIFIED.);
#388=B_SPLINE_CURVE_WITH_KNOTS('',3,(#22595,#22596,#22597,#22598),
 .UNSPECIFIED.,.F.,.F.,(4,4),(-0.195594022319045,0.),.UNSPECIFIED.);
#389=B_SPLINE_CURVE_WITH_KNOTS('',3,(#22603,#22604,#22605,#22606),
 .UNSPECIFIED.,.F.,.F.,(4,4),(-0.195594022319034,0.),.UNSPECIFIED.);
#390=B_SPLINE_CURVE_WITH_KNOTS('',3,(#22612,#22613,#22614,#22615),
 .UNSPECIFIED.,.F.,.F.,(4,4),(-0.201492965018152,0.),.UNSPECIFIED.);
#391=B_SPLINE_CURVE_WITH_KNOTS('',3,(#22621,#22622,#22623,#22624),
 .UNSPECIFIED.,.F.,.F.,(4,4),(-0.201492965018184,0.),.UNSPECIFIED.);
#392=B_SPLINE_CURVE_WITH_KNOTS('',3,(#22630,#22631,#22632,#22633),
 .UNSPECIFIED.,.F.,.F.,(4,4),(-0.201492965018239,0.),.UNSPECIFIED.);
#393=B_SPLINE_CURVE_WITH_KNOTS('',3,(#22640,#22641,#22642,#22643),
 .UNSPECIFIED.,.F.,.F.,(4,4),(-0.201492965018198,0.),.UNSPECIFIED.);
#394=B_SPLINE_CURVE_WITH_KNOTS('',3,(#22649,#22650,#22651,#22652),
 .UNSPECIFIED.,.F.,.F.,(4,4),(-0.195594022319061,0.),.UNSPECIFIED.);
#395=B_SPLINE_CURVE_WITH_KNOTS('',3,(#23127,#23128,#23129,#23130,#23131,
#23132,#23133,#23134,#23135,#23136,#23137,#23138,#23139,#23140,#23141,#23142,
#23143,#23144,#23145,#23146,#23147,#23148,#23149,#23150,#23151,#23152,#23153,
#23154,#23155,#23156,#23157,#23158,#23159,#23160,#23161,#23162,#23163,#23164,
#23165,#23166,#23167,#23168,#23169,#23170,#23171,#23172,#23173,#23174,#23175,
#23176,#23177,#23178,#23179,#23180,#23181,#23182,#23183,#23184,#23185,#23186,
#23187,#23188),.UNSPECIFIED.,.F.,.F.,(4,2,2,2,2,2,2,2,2,2,2,2,2,2,2,2,2,
2,2,2,2,2,2,2,2,2,2,2,2,2,4),(48.3095209509747,48.3438126061204,48.481226208238,
48.7564115875427,48.8943879405152,49.1670882523347,49.4057479328213,49.5435390452519,
49.8157502041263,50.086596913725,50.3608603822337,50.907937332897,51.1838264118632,
51.4592719418958,52.0080440963282,52.2810596578922,52.4186420978999,52.6942356980283,
53.2414178320407,53.3792880152578,53.6599840542201,53.9346199725026,54.4787854744381,
54.7497288191555,55.0208858330499,55.5745224561154,55.8470714557858,56.2861992300559,
56.5144008207168,56.6298096390493,56.7452388041896),.UNSPECIFIED.);
#396=B_SPLINE_CURVE_WITH_KNOTS('',3,(#23193,#23194,#23195,#23196,#23197,
#23198),.UNSPECIFIED.,.F.,.F.,(4,2,4),(0.000824378371301782,0.307333000414166,
0.426549198415677),.UNSPECIFIED.);
#397=B_SPLINE_CURVE_WITH_KNOTS('',3,(#23203,#23204,#23205,#23206,#23207,
#23208,#23209,#23210,#23211,#23212,#23213,#23214,#23215,#23216,#23217,#23218,
#23219,#23220,#23221,#23222,#23223,#23224,#23225,#23226,#23227,#23228,#23229,
#23230,#23231,#23232,#23233,#23234,#23235,#23236,#23237,#23238,#23239,#23240,
#23241,#23242,#23243,#23244,#23245,#23246,#23247,#23248,#23249,#23250,#23251,
#23252,#23253,#23254,#23255,#23256,#23257,#23258),.UNSPECIFIED.,.F.,.F.,
(4,2,2,2,2,2,2,2,2,2,2,2,2,2,2,2,2,2,2,2,2,2,2,2,2,2,2,4),(39.4473895294157,
39.6410372250372,40.0957750453416,40.3654377525067,40.6583563356197,40.9344854155672,
41.4872248887745,41.755996746073,42.1841163903161,42.557814705178,42.8338667979832,
43.1095103949903,43.6634534770776,43.9349491227225,44.2067442703658,44.4807550283175,
44.7532491351571,45.0271301508351,45.3010640927362,45.5768720367176,46.1309839511959,
46.5611880266105,46.8321636906455,47.0750044321246,47.350424720883,47.6223526303686,
47.8963704741162,48.3095209509747),.UNSPECIFIED.);
#398=B_SPLINE_CURVE_WITH_KNOTS('',3,(#23259,#23260,#23261,#23262,#23263,
#23264,#23265,#23266,#23267,#23268,#23269,#23270,#23271,#23272,#23273,#23274,
#23275,#23276,#23277,#23278,#23279,#23280,#23281,#23282,#23283,#23284,#23285,
#23286,#23287,#23288,#23289,#23290,#23291,#23292,#23293,#23294,#23295,#23296,
#23297,#23298,#23299,#23300,#23301,#23302,#23303,#23304,#23305,#23306,#23307,
#23308,#23309,#23310,#23311,#23312,#23313,#23314,#23315,#23316,#23317,#23318),
 .UNSPECIFIED.,.F.,.F.,(4,2,2,2,2,2,2,2,2,2,2,2,2,2,2,2,2,2,2,2,2,2,2,2,
2,2,2,2,2,4),(0.426549198415677,0.614191706618979,1.01002600072371,1.48582906984535,
1.73759812188067,2.01062010057207,2.56389527135009,2.83633022706529,3.1081672480776,
3.64857217350429,3.78620389269443,4.34106360761934,4.61723684328365,4.89201771080173,
5.16743328258393,5.44296844699991,5.58036719526417,6.12790418811079,6.4032185522103,
6.67910469076678,6.95504464088112,7.2275421020416,7.36514240490451,7.83280211438953,
7.97052980987632,8.45937656117122,8.59709328117351,9.08556481291611,9.22324652695596,
9.28838277977079),.UNSPECIFIED.);
#399=B_SPLINE_CURVE_WITH_KNOTS('',3,(#23323,#23324,#23325,#23326,#23327,
#23328,#23329,#23330,#23331,#23332,#23333,#23334,#23335,#23336,#23337,#23338,
#23339,#23340,#23341,#23342,#23343,#23344,#23345,#23346,#23347,#23348,#23349,
#23350,#23351,#23352,#23353,#23354,#23355,#23356,#23357,#23358,#23359,#23360,
#23361,#23362,#23363,#23364,#23365,#23366,#23367,#23368,#23369,#23370,#23371,
#23372,#23373,#23374,#23375,#23376,#23377,#23378,#23379,#23380,#23381,#23382,
#23383,#23384,#23385,#23386,#23387,#23388,#23389,#23390),.UNSPECIFIED.,
 .F.,.F.,(4,2,2,2,2,2,2,2,2,2,2,2,2,2,2,2,2,2,2,2,2,2,2,2,2,2,2,2,2,2,2,
2,2,4),(30.5866212966661,30.6469362186711,31.0261209213079,31.2978607379824,
31.7939621385182,32.0654867500116,32.2460223109104,32.7976124523937,32.9354482217323,
33.0733378306324,33.2112285916035,33.3491078585792,33.6242471271187,33.7619713364408,
34.0361140014156,34.1738247544983,34.4478069684183,34.7232900527495,35.2770415980905,
35.5501868477252,35.7887137967358,36.3430806261292,36.6190105141371,36.8949931496492,
37.1708524034991,37.4465777704499,37.5844613566104,37.8577982383939,37.9952584033865,
38.2699550429054,38.5435740429261,38.8173456070261,39.0912255075645,39.4473895294157),
 .UNSPECIFIED.);
#400=B_SPLINE_CURVE_WITH_KNOTS('',3,(#23391,#23392,#23393,#23394,#23395,
#23396,#23397,#23398,#23399,#23400,#23401,#23402,#23403,#23404,#23405,#23406,
#23407,#23408,#23409,#23410,#23411,#23412,#23413,#23414,#23415,#23416,#23417,
#23418,#23419,#23420,#23421,#23422,#23423,#23424,#23425,#23426,#23427,#23428,
#23429,#23430,#23431,#23432,#23433,#23434,#23435,#23436,#23437,#23438,#23439,
#23440,#23441,#23442,#23443,#23444,#23445,#23446,#23447,#23448),
 .UNSPECIFIED.,.F.,.F.,(4,2,2,2,2,2,2,2,2,2,2,2,2,2,2,2,2,2,2,2,2,2,2,2,
2,2,2,2,4),(9.28838277977079,9.69957849302504,9.97380096579599,10.2462470500306,
10.3838569093476,10.8129824883417,10.9507459110335,11.5141586961433,11.7884642076982,
12.0640566356795,12.3397813255604,12.614174112575,12.8892030655763,13.1614192721906,
13.2991037273397,13.5746845444855,14.1259124003885,14.2636924951075,14.8151556448298,
15.0915097232107,15.3718497780372,15.9274951705087,16.0651506906214,16.6104057666243,
16.8859839527044,17.2493313174359,17.5200638539738,18.0608178392373,18.1514671267416),
 .UNSPECIFIED.);
#401=B_SPLINE_CURVE_WITH_KNOTS('',3,(#23453,#23454,#23455,#23456,#23457,
#23458,#23459,#23460,#23461,#23462,#23463,#23464,#23465,#23466,#23467,#23468,
#23469,#23470,#23471,#23472,#23473,#23474,#23475,#23476,#23477,#23478,#23479,
#23480,#23481,#23482,#23483,#23484,#23485,#23486,#23487,#23488,#23489,#23490,
#23491,#23492,#23493,#23494,#23495,#23496,#23497,#23498,#23499,#23500,#23501,
#23502,#23503,#23504,#23505,#23506,#23507,#23508,#23509,#23510,#23511,#23512,
#23513,#23514,#23515,#23516,#23517,#23518,#23519,#23520),.UNSPECIFIED.,
 .F.,.F.,(4,2,2,2,2,2,2,2,2,2,2,2,2,2,2,2,2,2,2,2,2,2,2,2,2,2,2,2,2,2,2,
2,2,4),(21.7281508769804,21.859292462676,22.1347421134665,22.4138620953436,
22.6872284752932,22.9632671779943,23.1008811145477,23.3736294193785,23.6486966165464,
23.7864302925312,24.0619441755822,24.199625648023,24.3374800874459,24.6134095278544,
24.7512635221148,25.0272402972866,25.1650661303055,25.3026888072312,25.5774460693942,
25.8508320352646,26.2838985525551,26.5551310298002,26.9440332751233,27.2126940433332,
27.7565528573337,28.0278344389847,28.3724041446136,28.708047633284,28.9733600116614,
29.2041603109075,29.5653567879662,29.8366592676533,30.3783623722413,30.5866212966661),
 .UNSPECIFIED.);
#402=B_SPLINE_CURVE_WITH_KNOTS('',3,(#23521,#23522,#23523,#23524,#23525,
#23526,#23527,#23528,#23529,#23530,#23531,#23532,#23533,#23534,#23535,#23536,
#23537,#23538,#23539,#23540,#23541,#23542,#23543,#23544,#23545,#23546,#23547,
#23548,#23549,#23550,#23551,#23552,#23553,#23554,#23555,#23556,#23557,#23558,
#23559,#23560,#23561,#23562,#23563,#23564,#23565,#23566,#23567,#23568,#23569,
#23570,#23571,#23572,#23573,#23574,#23575,#23576,#23577,#23578,#23579,#23580,
#23581,#23582,#23583,#23584,#23585,#23586,#23587,#23588),.UNSPECIFIED.,
 .F.,.F.,(4,2,2,2,2,2,2,2,2,2,2,2,2,2,2,2,2,2,2,2,2,2,2,2,2,2,2,2,2,2,2,
2,2,4),(18.1514671267416,18.3359725867351,18.8879297461098,19.1636965767125,
19.3013917945595,19.8552808656922,20.1308659781475,20.4060615379671,20.6818851569234,
20.9577875123256,21.2337405314606,21.5081460257525,21.6197260439793,22.172500653785,
22.3102732515512,22.8627418433339,23.138149633494,23.4111694467411,23.5489071631255,
23.8222381557675,23.9599828842976,24.2346751933028,24.3725314687067,24.5103462088827,
24.6482043889914,24.785933581394,24.9238088698136,25.4775940615791,25.6160547495808,
25.8909936109743,26.1614289065469,26.7114543958306,26.9823357781454,27.0126062280082),
 .UNSPECIFIED.);
#403=B_SPLINE_CURVE_WITH_KNOTS('',3,(#23593,#23594,#23595,#23596,#23597,
#23598,#23599,#23600,#23601,#23602,#23603,#23604,#23605,#23606,#23607,#23608,
#23609,#23610,#23611,#23612,#23613,#23614,#23615,#23616,#23617,#23618,#23619,
#23620,#23621,#23622,#23623,#23624,#23625,#23626,#23627,#23628,#23629,#23630,
#23631,#23632,#23633,#23634,#23635,#23636,#23637,#23638,#23639,#23640,#23641,
#23642,#23643,#23644,#23645,#23646,#23647,#23648,#23649,#23650,#23651,#23652,
#23653,#23654),.UNSPECIFIED.,.F.,.F.,(4,2,2,2,2,2,2,2,2,2,2,2,2,2,2,2,2,
2,2,2,2,2,2,2,2,2,2,2,2,2,4),(12.8673372881869,13.1045912480947,13.3784206922435,
13.6508493140918,13.9224251719806,14.4747733220309,14.7502018033826,15.0261882292162,
15.2867204870524,15.7143806877064,16.1397500990148,16.4122973490567,16.9672169387799,
17.2033227276788,17.4726908823725,18.037876335385,18.3124420816258,18.8598305789335,
18.9974121921246,19.2729763606579,19.5488031042003,19.8228552663192,20.097625942618,
20.3704230665631,20.6463274234226,20.9217341125824,21.0596243445807,21.3351615072599,
21.4724476291603,21.721963084712,21.7281508769804),.UNSPECIFIED.);
#404=B_SPLINE_CURVE_WITH_KNOTS('',3,(#23655,#23656,#23657,#23658,#23659,
#23660,#23661,#23662,#23663,#23664,#23665,#23666,#23667,#23668,#23669,#23670,
#23671,#23672,#23673,#23674,#23675,#23676,#23677,#23678,#23679,#23680,#23681,
#23682,#23683,#23684,#23685,#23686,#23687,#23688,#23689,#23690,#23691,#23692,
#23693,#23694,#23695,#23696,#23697,#23698,#23699,#23700,#23701,#23702,#23703,
#23704,#23705,#23706,#23707,#23708,#23709,#23710,#23711,#23712,#23713,#23714,
#23715,#23716,#23717,#23718),.UNSPECIFIED.,.F.,.F.,(4,2,2,2,2,2,2,2,2,2,
2,2,2,2,2,2,2,2,2,2,2,2,2,2,2,2,2,2,2,2,2,4),(27.0126062280082,27.3028829986553,
27.8351272737622,28.0388596861804,28.4737664649467,28.7408417219884,28.9998149350992,
29.2355762469122,29.4192788621494,29.6954983810387,30.0670604013279,30.6244762789582,
30.9498794660956,31.4902800694265,31.763897147745,32.0371486886421,32.3104751893334,
32.4482035971803,32.72417276819,32.8620543008062,32.9999247087657,33.2758973613899,
33.5518702088626,33.8273566843513,33.9652030027378,34.240225672795,34.5140108716027,
34.6516577003026,34.9275167223425,35.2011094137945,35.6443705723813,35.8725192426511),
 .UNSPECIFIED.);
#405=B_SPLINE_CURVE_WITH_KNOTS('',3,(#23723,#23724,#23725,#23726,#23727,
#23728,#23729,#23730,#23731,#23732,#23733,#23734,#23735,#23736,#23737,#23738,
#23739,#23740,#23741,#23742,#23743,#23744,#23745,#23746,#23747,#23748,#23749,
#23750,#23751,#23752,#23753,#23754,#23755,#23756,#23757,#23758,#23759,#23760,
#23761,#23762,#23763,#23764,#23765,#23766,#23767,#23768,#23769,#23770,#23771,
#23772,#23773,#23774,#23775,#23776,#23777,#23778,#23779,#23780,#23781,#23782,
#23783,#23784),.UNSPECIFIED.,.F.,.F.,(4,2,2,2,2,2,2,2,2,2,2,2,2,2,2,2,2,
2,2,2,2,2,2,2,2,2,2,2,2,2,4),(4.00579666373733,4.22413930375615,4.36190267992724,
4.91034098288094,5.18600966471709,5.32349953457887,5.59632872461622,6.14663667970456,
6.42222459948757,6.69804980819117,7.2474319093848,7.38486184776289,7.83922119968481,
7.97688389264115,8.52926536854384,8.80482269152215,9.08530248842244,9.22296907620534,
9.71155236699991,9.98575858600692,10.2588795271958,10.5345327905916,10.7699146367297,
11.0408326712101,11.5939442609587,11.8696146241601,12.1455514363969,12.2834279870469,
12.5577920931176,12.8314615618714,12.8673372881869),.UNSPECIFIED.);
#406=B_SPLINE_CURVE_WITH_KNOTS('',3,(#23785,#23786,#23787,#23788,#23789,
#23790,#23791,#23792,#23793,#23794,#23795,#23796,#23797,#23798,#23799,#23800,
#23801,#23802,#23803,#23804,#23805,#23806,#23807,#23808,#23809,#23810,#23811,
#23812,#23813,#23814,#23815,#23816,#23817,#23818,#23819,#23820,#23821,#23822,
#23823,#23824,#23825,#23826,#23827,#23828,#23829,#23830,#23831,#23832,#23833,
#23834,#23835,#23836,#23837,#23838,#23839,#23840,#23841,#23842),
 .UNSPECIFIED.,.F.,.F.,(4,2,2,2,2,2,2,2,2,2,2,2,2,2,2,2,2,2,2,2,2,2,2,2,
2,2,2,2,4),(35.8725192426511,35.9151842174268,36.09983440795,36.3742808891897,
36.5122035519266,36.6501205150463,36.9260423900668,37.2019237953068,37.4769431036303,
37.7524677979035,38.3063620750602,38.4441238522539,38.7198610588383,39.2714120779741,
39.5465499155902,40.1111820373952,40.3816152785012,40.6708302493013,40.946855041263,
41.4986518734995,41.7690904826401,42.2242805568422,42.5186658754165,42.7949816988295,
43.3460251568471,43.6210829792625,43.8937594718918,44.3327289395869,44.7369456500769),
 .UNSPECIFIED.);
#407=B_SPLINE_CURVE_WITH_KNOTS('',3,(#23845,#23846,#23847,#23848,#23849,
#23850,#23851,#23852,#23853,#23854,#23855,#23856,#23857,#23858,#23859,#23860,
#23861,#23862,#23863,#23864,#23865,#23866,#23867,#23868,#23869,#23870,#23871,
#23872,#23873,#23874,#23875,#23876,#23877,#23878,#23879,#23880,#23881,#23882,
#23883,#23884,#23885,#23886,#23887,#23888,#23889,#23890,#23891,#23892,#23893,
#23894,#23895,#23896,#23897,#23898,#23899,#23900,#23901,#23902),
 .UNSPECIFIED.,.F.,.F.,(4,2,2,2,2,2,2,2,2,2,2,2,2,2,2,2,2,2,2,2,2,2,2,2,
2,2,2,2,4),(44.7369456500769,44.8867742748783,45.0245971947796,45.2985652981441,
45.5743906456427,46.1283912454116,46.5570552926755,46.8287680120469,47.0682425531597,
47.3440177136997,47.6178066999295,47.8923482402771,48.1645791411325,48.3023652432245,
48.574971680631,48.8464001383451,49.1209239039586,49.3951619578507,49.5330723902179,
49.8059417425042,50.0766678420903,50.3516170304178,50.9023268700414,51.1781921554573,
51.453978195975,51.8867436693424,52.1031849749825,52.2112916210837,52.3187924201233),
 .UNSPECIFIED.);
#408=B_SPLINE_CURVE_WITH_KNOTS('',3,(#23907,#23908,#23909,#23910,#23911,
#23912,#23913,#23914,#23915,#23916,#23917,#23918,#23919,#23920,#23921,#23922,
#23923,#23924,#23925,#23926,#23927,#23928,#23929,#23930,#23931,#23932),
 .UNSPECIFIED.,.F.,.F.,(4,2,2,2,2,2,2,2,2,2,2,2,4),(0.000824364847128334,
0.279789559980365,0.559133666621795,1.03110720678431,1.40797268178914,1.75551901563212,
2.02774233750806,2.58176080895605,2.85228694703896,3.12295036047126,3.66872486797347,
3.9434825123866,4.00579666373733),.UNSPECIFIED.);
#409=B_SPLINE_CURVE_WITH_KNOTS('',3,(#23985,#23986,#23987,#23988,#23989,
#23990,#23991,#23992,#23993,#23994,#23995,#23996,#23997,#23998,#23999,#24000,
#24001,#24002,#24003,#24004,#24005,#24006,#24007,#24008,#24009,#24010),
 .UNSPECIFIED.,.F.,.F.,(4,2,2,2,2,2,2,2,2,2,2,2,4),(9.99999998997544E-7,
0.277509193145354,0.559562005090733,1.13595993001213,1.45422004501248,2.10759695469075,
2.43887984940046,3.11114962502898,3.45649386180175,3.80276810060717,4.51975710851416,
5.24677359279633,5.41878430004213),.UNSPECIFIED.);
#410=B_SPLINE_CURVE_WITH_KNOTS('',3,(#24013,#24014,#24015,#24016,#24017,
#24018,#24019,#24020,#24021,#24022,#24023,#24024,#24025,#24026,#24027,#24028,
#24029,#24030,#24031,#24032,#24033,#24034,#24035,#24036,#24037,#24038,#24039,
#24040,#24041,#24042,#24043,#24044,#24045,#24046,#24047,#24048,#24049,#24050,
#24051,#24052,#24053,#24054,#24055,#24056,#24057,#24058,#24059,#24060,#24061,
#24062,#24063,#24064,#24065,#24066,#24067,#24068,#24069,#24070,#24071,#24072,
#24073,#24074,#24075,#24076,#24077,#24078,#24079,#24080,#24081,#24082,#24083,
#24084,#24085,#24086,#24087,#24088,#24089,#24090,#24091,#24092,#24093,#24094,
#24095,#24096,#24097,#24098,#24099,#24100,#24101,#24102,#24103,#24104,#24105,
#24106,#24107,#24108,#24109,#24110,#24111,#24112,#24113,#24114,#24115,#24116,
#24117,#24118),.UNSPECIFIED.,.F.,.F.,(4,3,3,3,3,3,3,3,3,3,3,3,3,3,3,3,3,
3,3,3,3,3,3,3,3,3,3,3,3,3,3,3,3,3,3,4),(-5.14602986437962,-4.9124571768068,
-4.71371046276571,-4.54086707520652,-4.32250456683061,-4.10713809464024,
-3.95554536139003,-3.82420547225028,-3.61585834214411,-3.41052234213242,
-3.20824947806771,-3.00469258194512,-2.97873918630968,-2.77502713067335,
-2.57493296082448,-2.49620314801143,-2.29768232080681,-2.17849548023144,
-2.06364564461087,-2.04936478423458,-2.00662821804358,-1.83737350397171,
-1.81938711170177,-1.67044184854484,-1.50530496693403,-1.31867939695959,
-1.17777177287489,-0.994244625335878,-0.867823569922663,-0.790542128771154,
-0.608686868523352,-0.571323537610721,-0.394394587266291,-0.220420986284586,
-0.120990393829573,-0.00018052822953134),.UNSPECIFIED.);
#411=B_SPLINE_CURVE_WITH_KNOTS('',3,(#24120,#24121,#24122,#24123,#24124,
#24125,#24126,#24127,#24128,#24129,#24130,#24131,#24132,#24133,#24134,#24135,
#24136,#24137,#24138,#24139,#24140,#24141,#24142,#24143,#24144,#24145,#24146,
#24147,#24148,#24149,#24150,#24151,#24152,#24153,#24154,#24155,#24156,#24157,
#24158,#24159,#24160,#24161,#24162,#24163,#24164,#24165,#24166,#24167,#24168,
#24169,#24170,#24171,#24172,#24173,#24174,#24175,#24176,#24177,#24178,#24179,
#24180,#24181,#24182,#24183),.UNSPECIFIED.,.F.,.F.,(4,3,3,3,3,3,3,3,3,3,
3,3,3,3,3,3,3,3,3,3,3,4),(-3.54929782707136,-3.43298875244871,-3.38136321121889,
-3.36415083557511,-3.22642372778473,-3.00517870020166,-2.77298587052083,
-2.54081959100311,-2.46105968243433,-2.29735828955663,-2.06510807290758,
-1.83230960956431,-1.64070659226555,-1.40756763421874,-1.36661117934383,
-1.133848457372,-0.90127112443142,-0.820353364661033,-0.587108315483886,
-0.435770693368578,-0.202446776608828,-1.64264001317083E-5),
 .UNSPECIFIED.);
#412=B_SPLINE_CURVE_WITH_KNOTS('',3,(#24184,#24185,#24186,#24187,#24188,
#24189,#24190,#24191,#24192,#24193,#24194,#24195,#24196,#24197,#24198,#24199,
#24200,#24201,#24202,#24203),.UNSPECIFIED.,.F.,.F.,(4,2,2,2,2,2,2,2,2,4),
(5.41878430004213,5.612905067052,5.98508461978949,6.35542810705476,6.73497483683354,
7.11388681821555,7.89769154966654,8.16903003314377,8.58256664643331,8.99852632498306),
 .UNSPECIFIED.);
#413=B_SPLINE_CURVE_WITH_KNOTS('',3,(#24207,#24208,#24209,#24210,#24211,
#24212,#24213,#24214,#24215,#24216,#24217,#24218,#24219,#24220,#24221,#24222,
#24223,#24224,#24225,#24226,#24227,#24228,#24229,#24230,#24231,#24232),
 .UNSPECIFIED.,.F.,.F.,(4,2,2,2,2,2,2,2,2,2,2,2,4),(2.24906504782965E-5,
0.571634272981765,1.12074908741776,1.48125473010532,1.85616076048785,2.58661322797785,
2.93330821431849,3.27144832173647,3.91512369926488,4.53192872349113,4.84787148574749,
5.00150736838493,5.15431373386902),.UNSPECIFIED.);
#414=B_SPLINE_CURVE_WITH_KNOTS('',3,(#24234,#24235,#24236,#24237,#24238,
#24239,#24240,#24241,#24242,#24243,#24244,#24245,#24246,#24247),
 .UNSPECIFIED.,.F.,.F.,(4,2,2,2,2,2,4),(0.,0.474678646281976,0.942829047193473,
1.51670727039287,1.90291538542257,2.09764827213206,2.29412506652137),
 .UNSPECIFIED.);
#415=B_SPLINE_CURVE_WITH_KNOTS('',3,(#24249,#24250,#24251,#24252,#24253,
#24254,#24255,#24256,#24257,#24258,#24259,#24260,#24261,#24262,#24263,#24264,
#24265,#24266),.UNSPECIFIED.,.F.,.F.,(4,2,2,2,2,2,2,2,4),(0.,0.350415922095155,
0.706087820863965,1.42957591857985,1.81390106464849,2.61485609197721,3.11237077026773,
3.36521279740499,3.6186598959626),.UNSPECIFIED.);
#416=B_SPLINE_CURVE_WITH_KNOTS('',3,(#24847,#24848,#24849,#24850,#24851,
#24852,#24853,#24854,#24855,#24856,#24857,#24858,#24859,#24860,#24861,#24862,
#24863,#24864,#24865,#24866,#24867,#24868,#24869,#24870,#24871,#24872,#24873,
#24874,#24875,#24876,#24877,#24878,#24879,#24880,#24881,#24882,#24883,#24884,
#24885,#24886,#24887,#24888,#24889,#24890,#24891,#24892,#24893,#24894,#24895,
#24896,#24897,#24898,#24899,#24900,#24901,#24902,#24903,#24904,#24905,#24906,
#24907,#24908,#24909,#24910,#24911,#24912,#24913,#24914,#24915,#24916,#24917,
#24918,#24919,#24920,#24921,#24922,#24923,#24924,#24925,#24926,#24927,#24928,
#24929,#24930,#24931,#24932,#24933,#24934,#24935,#24936,#24937,#24938,#24939,
#24940,#24941,#24942,#24943,#24944,#24945,#24946,#24947,#24948,#24949,#24950,
#24951,#24952,#24953,#24954,#24955,#24956,#24957,#24958,#24959,#24960,#24961,
#24962,#24963,#24964,#24965,#24966,#24967,#24968,#24969,#24970,#24971,#24972,
#24973,#24974,#24975,#24976,#24977,#24978,#24979,#24980,#24981),
 .UNSPECIFIED.,.F.,.F.,(4,1,1,1,1,1,1,2,1,1,1,1,2,1,1,1,1,2,1,1,2,2,1,1,
1,1,1,1,2,1,2,1,1,1,2,1,1,1,2,1,1,1,2,1,1,1,2,1,1,1,2,1,1,1,2,1,1,1,2,1,
1,1,1,1,2,1,1,1,1,1,1,2,2,1,1,2,1,1,1,1,2,1,1,1,1,2,1,1,1,1,1,1,1,1,1,2,
1,1,1,1,1,2,2,1,1,1,1,1,1,4),(0.162516398693048,0.168269230768974,0.177884615384371,
0.187499999999768,0.199519230740103,0.206730769230503,0.210336538446854,
0.211538461538235,0.213942307720923,0.218749999970821,0.228365384586246,
0.237980769201671,0.249999999999808,0.25841346152381,0.266826923047812,
0.281250000028623,0.289663461552636,0.298076923076649,0.312499999999747,
0.31971153849016,0.326923076922846,0.33653846153821,0.338942307720942,0.340144230783416,
0.343749999970879,0.353365384586257,0.358173076951719,0.362980769201619,
0.365384615384414,0.370192307692066,0.37499999999969,0.389423076922836,
0.397836538475728,0.406250000028619,0.413461538461298,0.420673076893946,
0.425480769259405,0.427884615384363,0.432692307692057,0.433894230783419,
0.43509615387478,0.437499999999749,0.442307692307468,0.455528846139201,
0.468749999970934,0.483173076951685,0.49999999999975,0.516826923047797,
0.531250000028611,0.544471153860329,0.557692307692047,0.562499999999739,
0.563701923062234,0.564903846124729,0.567307692307427,0.569711538490167,
0.574519230740095,0.579326923105555,0.586538461538202,0.593749999970866,
0.602163461523769,0.610576923076672,0.624999999999777,0.629807692307439,
0.634615384615125,0.637019230797861,0.641826923047781,0.646634615413246,
0.656250000028622,0.659855769216081,0.661057692278563,0.663461538461287,
0.673076923076666,0.680288461509321,0.687499999999755,0.701923076922838,
0.710336538446858,0.718749999970878,0.733173076951697,0.741586538475723,
0.749999999999749,0.762019230797881,0.771634615413259,0.781250000028636,
0.786057692278561,0.788461538461294,0.78966346155265,0.793269230768981,
0.800480769259399,0.812499999999748,0.822115384615134,0.83173076923052,
0.842548076908385,0.853365384586251,0.864182692292999,0.874999999999748,
0.876602564121565,0.876802884636793,0.877403846182474,0.879807692307444,
0.882211538432407,0.884615384615134,0.894230769230516,0.895432692321882,
0.906250000028634,0.915865384644013,0.926682692321841,0.937499999999668,
0.949519230731432,0.955682525542283),.UNSPECIFIED.);
#417=B_SPLINE_CURVE_WITH_KNOTS('',3,(#24982,#24983,#24984,#24985,#24986,
#24987,#24988,#24989,#24990,#24991,#24992,#24993,#24994,#24995,#24996,#24997,
#24998,#24999,#25000,#25001,#25002,#25003,#25004,#25005,#25006,#25007,#25008,
#25009,#25010,#25011,#25012,#25013,#25014,#25015,#25016,#25017,#25018,#25019,
#25020,#25021,#25022,#25023,#25024,#25025,#25026,#25027,#25028,#25029,#25030,
#25031,#25032,#25033,#25034,#25035,#25036,#25037,#25038,#25039,#25040,#25041,
#25042,#25043,#25044,#25045,#25046,#25047,#25048,#25049,#25050,#25051,#25052,
#25053,#25054,#25055,#25056,#25057,#25058,#25059,#25060,#25061,#25062,#25063,
#25064,#25065,#25066,#25067,#25068,#25069,#25070,#25071,#25072,#25073,#25074,
#25075,#25076,#25077,#25078,#25079,#25080,#25081,#25082,#25083,#25084,#25085,
#25086,#25087,#25088,#25089,#25090,#25091,#25092,#25093,#25094,#25095,#25096,
#25097,#25098,#25099,#25100,#25101,#25102,#25103,#25104,#25105,#25106,#25107,
#25108,#25109,#25110,#25111,#25112,#25113,#25114,#25115,#25116,#25117,#25118,
#25119,#25120,#25121,#25122,#25123,#25124,#25125,#25126,#25127,#25128,#25129,
#25130,#25131,#25132,#25133,#25134,#25135,#25136,#25137,#25138,#25139,#25140,
#25141,#25142,#25143,#25144,#25145,#25146,#25147,#25148,#25149,#25150,#25151,
#25152,#25153,#25154,#25155,#25156,#25157,#25158,#25159,#25160,#25161,#25162,
#25163,#25164,#25165,#25166,#25167,#25168,#25169,#25170,#25171,#25172,#25173,
#25174,#25175,#25176,#25177,#25178,#25179,#25180,#25181,#25182,#25183,#25184,
#25185,#25186,#25187,#25188,#25189,#25190,#25191,#25192,#25193,#25194,#25195,
#25196,#25197,#25198,#25199,#25200,#25201,#25202,#25203,#25204,#25205,#25206,
#25207,#25208,#25209,#25210,#25211,#25212,#25213,#25214,#25215,#25216,#25217,
#25218,#25219,#25220,#25221,#25222,#25223,#25224,#25225,#25226,#25227,#25228,
#25229,#25230,#25231,#25232,#25233,#25234,#25235,#25236,#25237,#25238,#25239,
#25240,#25241,#25242,#25243,#25244,#25245,#25246,#25247,#25248,#25249,#25250,
#25251,#25252,#25253,#25254,#25255,#25256,#25257,#25258,#25259,#25260,#25261,
#25262,#25263,#25264,#25265,#25266,#25267,#25268,#25269,#25270,#25271,#25272,
#25273,#25274,#25275,#25276,#25277,#25278,#25279,#25280,#25281,#25282,#25283,
#25284,#25285,#25286,#25287,#25288,#25289,#25290,#25291,#25292,#25293,#25294,
#25295,#25296,#25297,#25298,#25299,#25300,#25301,#25302,#25303,#25304,#25305,
#25306,#25307,#25308,#25309,#25310,#25311,#25312,#25313,#25314,#25315,#25316,
#25317,#25318,#25319,#25320,#25321,#25322,#25323,#25324,#25325,#25326,#25327,
#25328,#25329,#25330,#25331,#25332,#25333,#25334,#25335,#25336,#25337,#25338,
#25339,#25340,#25341,#25342,#25343,#25344,#25345,#25346,#25347,#25348,#25349,
#25350,#25351,#25352,#25353,#25354,#25355,#25356,#25357,#25358,#25359,#25360,
#25361,#25362,#25363,#25364,#25365,#25366,#25367,#25368,#25369,#25370,#25371,
#25372,#25373,#25374,#25375,#25376,#25377,#25378,#25379,#25380,#25381,#25382,
#25383,#25384,#25385,#25386,#25387,#25388,#25389,#25390,#25391,#25392,#25393,
#25394,#25395,#25396,#25397,#25398,#25399,#25400,#25401,#25402,#25403,#25404,
#25405,#25406,#25407,#25408,#25409,#25410,#25411,#25412,#25413,#25414,#25415,
#25416,#25417,#25418,#25419,#25420,#25421,#25422,#25423,#25424,#25425,#25426,
#25427,#25428,#25429,#25430,#25431,#25432,#25433,#25434,#25435,#25436,#25437,
#25438,#25439,#25440,#25441,#25442,#25443,#25444,#25445,#25446,#25447,#25448,
#25449,#25450,#25451,#25452,#25453,#25454,#25455,#25456,#25457,#25458,#25459,
#25460,#25461,#25462,#25463,#25464,#25465,#25466,#25467,#25468,#25469,#25470,
#25471,#25472,#25473,#25474,#25475,#25476,#25477,#25478,#25479,#25480,#25481,
#25482,#25483),.UNSPECIFIED.,.F.,.F.,(4,3,3,3,3,3,3,3,3,3,3,3,3,3,3,3,3,
3,3,3,3,3,3,3,3,3,3,3,3,3,3,3,3,3,3,3,3,3,3,3,3,3,3,3,3,3,3,3,3,3,3,3,3,
3,3,3,3,3,3,3,3,3,3,3,3,3,3,3,3,3,3,3,3,3,3,3,3,3,3,3,3,3,3,3,3,3,3,3,3,
3,3,3,3,3,3,3,3,3,3,3,3,3,3,3,3,3,3,3,3,3,3,3,3,3,3,3,3,3,3,3,3,3,3,3,3,
3,3,3,3,3,3,3,3,3,3,3,3,3,3,3,3,3,3,3,3,3,3,3,3,3,3,3,3,3,3,3,3,3,3,3,3,
3,3,3,3,3,3,4),(0.121241235866819,0.122596333952119,0.123197306239647,0.123397630454117,
0.125000220490707,0.135817558564196,0.146634821242987,0.157452054343042,
0.16826930039866,0.177884615384371,0.177884648357071,0.187499999999768,
0.199519216306826,0.199519230740103,0.206730748861056,0.206730769230503,
0.210336516868093,0.210336538446854,0.211538439269354,0.211538461538235,
0.213942284455432,0.213942307720923,0.21874997552603,0.218749999970821,
0.22836536738934,0.228365384586246,0.237980769201671,0.250000006012719,
0.25841346152381,0.266826923047812,0.281250000028623,0.289663461552636,
0.298076913590586,0.312499999999747,0.31971153849016,0.326923094679332,
0.336538484588579,0.338942331282927,0.340144254583534,0.343750023825251,
0.35336540594336,0.358173095018189,0.362980782487174,0.365384626334338,
0.370192307692066,0.374999999391061,0.389423076922836,0.389423093033542,
0.397836575504186,0.406250058688912,0.413461607848517,0.420673152098523,
0.42548084303445,0.427884687070039,0.432692372895138,0.433894293991556,
0.435096214869763,0.43750005599482,0.442307736943911,0.455528868281594,
0.46875003733348,0.483173076951685,0.483173116205438,0.499999999838053,
0.51682688352103,0.516826923047797,0.531249962424686,0.531250000028611,
0.544471131109026,0.544471153860329,0.557692260171344,0.557692307692047,
0.562499939446951,0.562499999999739,0.563701859758352,0.563701923062234,
0.564903780248029,0.564903846124729,0.567307621420288,0.567307692307427,
0.569711463075703,0.569711538490167,0.574519148795765,0.574519230740095,
0.579326835836925,0.579326923105555,0.586538355389812,0.586538461538202,
0.593163510583565,0.593749999970866,0.593750080688083,0.600519790385705,
0.602163221950243,0.602163461523769,0.60896006288304,0.610576923076672,
0.61057724928789,0.617292450591262,0.623876825081465,0.624999612585041,
0.624999999999777,0.628545774026805,0.629807692307439,0.629808266711979,
0.63322388056985,0.634615284988846,0.634615384615125,0.637019175058555,
0.637019230797861,0.641826862941149,0.641826923047781,0.646634549684172,
0.646634615413246,0.656249954446322,0.656250000028622,0.659855725068628,
0.659855769216081,0.661057648907858,0.661057692278563,0.663461496685113,
0.663461538461287,0.673076896175284,0.673076923076666,0.680288447579257,
0.680288461509321,0.687499999999755,0.701923087601902,0.710336548577926,
0.718749999970878,0.733173076951697,0.741586538475723,0.749999993068343,
0.762019230797881,0.771634615413259,0.771634627337508,0.781250017474292,
0.786057708639458,0.788461554153435,0.789663476774355,0.79326924518666,
0.800480769259399,0.812499999999748,0.822115384615134,0.831730763372892,
0.842548076908385,0.853365384586251,0.864182692292999,0.874999982515718,
0.874999999999748,0.87660254418179,0.876602564121565,0.876802864442705,
0.876802884636793,0.877403825127061,0.877403846182474,0.879807666207773,
0.879807692307444,0.882211507161395,0.882211538432407,0.884615347276649,
0.884615384615134,0.894230680447608,0.894230769230516,0.895432604252924,
0.895432692321882,0.906249829255419,0.906250000028634,0.914406074621021),
 .UNSPECIFIED.);
#418=B_SPLINE_CURVE_WITH_KNOTS('',3,(#26828,#26829,#26830,#26831,#26832,
#26833,#26834,#26835,#26836,#26837,#26838,#26839,#26840,#26841,#26842,#26843,
#26844,#26845,#26846),.UNSPECIFIED.,.F.,.F.,(4,1,1,1,1,1,1,1,1,1,1,1,1,
1,1,1,4),(0.,0.0325793930090435,0.0434391906787246,0.0651587860180869,0.0868783813574492,
0.0923082801922898,0.0977381790271304,0.119457774366493,0.173756762714898,
0.217195953393623,0.238915548732985,0.260635144072348,0.28235473941171,
0.293214537081391,0.304074334751072,0.347513525429797,0.350797960844041),
 .UNSPECIFIED.);
#419=B_SPLINE_CURVE_WITH_KNOTS('',3,(#26850,#26851,#26852,#26853,#26854,
#26855,#26856,#26857,#26858,#26859,#26860,#26861,#26862,#26863,#26864,#26865,
#26866,#26867,#26868),.UNSPECIFIED.,.F.,.F.,(4,1,1,1,1,1,1,1,1,1,1,1,1,
1,1,1,4),(0.351264129075342,0.354255847547048,0.372150346521233,0.390044845495419,
0.407939344469604,0.416886593956697,0.42583384344379,0.46162284139216,0.488464589853438,
0.497411839340531,0.533200837288902,0.551095336263087,0.568989835237273,
0.586884334211458,0.604778833185643,0.613726082672736,0.640567831134014),
 .UNSPECIFIED.);
#420=B_SPLINE_CURVE_WITH_KNOTS('',3,(#26872,#26873,#26874,#26875,#26876,
#26877,#26878,#26879,#26880,#26881,#26882,#26883,#26884,#26885,#26886,#26887,
#26888,#26889),.UNSPECIFIED.,.F.,.F.,(4,1,1,1,1,1,1,1,1,1,1,1,1,1,1,4),
(0.,0.0325793930343183,0.0434391907124244,0.0651587860686366,0.0868783814248488,
0.0977381791029549,0.108597976781061,0.130317572137273,0.173756762849698,
0.217195953562122,0.238915548918334,0.260635144274546,0.282354739630759,
0.304074334986971,0.347513525699395,0.350847233099761),.UNSPECIFIED.);
#421=B_SPLINE_CURVE_WITH_KNOTS('',3,(#26893,#26894,#26895,#26896,#26897,
#26898,#26899,#26900,#26901,#26902,#26903,#26904,#26905,#26906,#26907,#26908,
#26909,#26910,#26911),.UNSPECIFIED.,.F.,.F.,(4,1,1,1,1,1,1,1,1,1,1,1,1,
1,1,1,4),(0.351264249492161,0.354255847579901,0.372150346750411,0.39004484592092,
0.40793934509143,0.416886594676685,0.42583384426194,0.46162284260296,0.488464591358724,
0.497411840943979,0.533200839284999,0.551095338455509,0.568989837626019,
0.586884336796529,0.604778835967039,0.613726085552294,0.640567834308058),
 .UNSPECIFIED.);
#422=B_SPLINE_CURVE_WITH_KNOTS('',3,(#26915,#26916,#26917,#26918,#26919,
#26920,#26921,#26922,#26923,#26924,#26925,#26926,#26927,#26928,#26929,#26930,
#26931,#26932,#26933,#26934,#26935),.UNSPECIFIED.,.F.,.F.,(4,1,1,1,1,1,
1,1,1,1,1,1,1,1,1,1,1,1,4),(0.,0.0325793930168542,0.0434391906891389,0.0651587860337083,
0.0868783813782778,0.0977381790505625,0.108597976722847,0.130317572067417,
0.173756762756556,0.217195953445694,0.238915548790264,0.260635144134833,
0.266065042970976,0.271494941807118,0.282354739479403,0.293214537151688,
0.304074334823972,0.347513525513111,0.350819403961439),.UNSPECIFIED.);
#423=B_SPLINE_CURVE_WITH_KNOTS('',3,(#26939,#26940,#26941,#26942,#26943,
#26944,#26945,#26946,#26947,#26948,#26949,#26950,#26951,#26952,#26953,#26954,
#26955,#26956),.UNSPECIFIED.,.F.,.F.,(4,1,1,1,1,1,1,1,1,1,1,1,1,1,1,4),
(0.351261425313741,0.35425584743808,0.372150345761052,0.381097594922539,
0.385571219503282,0.387808031793653,0.390044844084025,0.425833840729969,
0.497411834021859,0.533200830667804,0.551095328990776,0.568989827313749,
0.586884325636721,0.604778823959693,0.61372607312118,0.640567820605638),
 .UNSPECIFIED.);
#424=B_SPLINE_CURVE_WITH_KNOTS('',3,(#26960,#26961,#26962,#26963,#26964,
#26965,#26966,#26967,#26968,#26969,#26970,#26971,#26972,#26973,#26974,#26975,
#26976,#26977,#26978),.UNSPECIFIED.,.F.,.F.,(4,1,1,1,1,1,1,1,1,1,1,1,1,
1,1,1,4),(0.,0.0325793930229512,0.0434391906972683,0.0651587860459025,0.0868783813945366,
0.0977381790688537,0.119457774417488,0.173756762789073,0.195476358137707,
0.217195953486341,0.238915548834976,0.249775346509293,0.255205245346451,
0.26063514418361,0.304074334880878,0.347513525578146,0.350819878802366),
 .UNSPECIFIED.);
#425=B_SPLINE_CURVE_WITH_KNOTS('',3,(#26982,#26983,#26984,#26985,#26986,
#26987,#26988,#26989,#26990,#26991,#26992,#26993,#26994,#26995,#26996,#26997,
#26998,#26999,#27000,#27001,#27002),.UNSPECIFIED.,.F.,.F.,(4,1,1,1,1,1,
1,1,1,1,1,1,1,1,1,1,1,1,4),(0.351261425313739,0.354255847492041,0.390044844782951,
0.407939343428406,0.42583384207386,0.443728340719315,0.46162283936477,0.470570088687497,
0.497411836655679,0.533200833946589,0.551095332592044,0.560042581914771,
0.564516206576135,0.568989831237498,0.586884329882953,0.604778828528408,
0.613726077851135,0.622673327173863,0.640567825819317),.UNSPECIFIED.);
#426=B_SPLINE_CURVE_WITH_KNOTS('',3,(#27006,#27007,#27008,#27009,#27010,
#27011,#27012,#27013,#27014,#27015,#27016,#27017,#27018,#27019,#27020,#27021,
#27022,#27023,#27024),.UNSPECIFIED.,.F.,.F.,(4,1,1,1,1,1,1,1,1,1,1,1,1,
1,1,1,4),(0.,0.032579393007947,0.0434391906772627,0.065158786015894,0.0868783813545254,
0.0977381790238411,0.119457774362472,0.173756762709051,0.195476358047682,
0.217195953386313,0.238915548724945,0.24977534639426,0.255205245228918,
0.260635144063576,0.304074334740839,0.347513525418102,0.350819155150611),
 .UNSPECIFIED.);
#427=B_SPLINE_CURVE_WITH_KNOTS('',3,(#27028,#27029,#27030,#27031,#27032,
#27033,#27034,#27035,#27036,#27037,#27038,#27039,#27040,#27041,#27042,#27043,
#27044,#27045),.UNSPECIFIED.,.F.,.F.,(4,1,1,1,1,1,1,1,1,1,1,1,1,1,1,4),
(0.351261425313739,0.35425584787858,0.372150348833954,0.390044849789328,
0.407939350744702,0.416886601222389,0.425833851700076,0.461622853610824,
0.497411855521572,0.53320085743232,0.551095358387694,0.568989859343068,
0.586884360298442,0.604778861253817,0.613726111731503,0.640567863164564),
 .UNSPECIFIED.);
#428=B_SPLINE_CURVE_WITH_KNOTS('',3,(#27049,#27050,#27051,#27052,#27053,
#27054,#27055,#27056,#27057,#27058,#27059,#27060,#27061,#27062,#27063,#27064,
#27065,#27066,#27067),.UNSPECIFIED.,.F.,.F.,(4,1,1,1,1,1,1,1,1,1,1,1,1,
1,1,1,4),(0.,0.0218558225633788,0.0327837338450682,0.0437116451267576,0.0655674676901365,
0.0874232902535153,0.0983512015352047,0.109279112816894,0.131134935380273,
0.174846580507031,0.218558225633788,0.240414048197167,0.262269870760546,
0.284125693323925,0.305981515887303,0.349693161014061,0.353045062814117),
 .UNSPECIFIED.);
#429=B_SPLINE_CURVE_WITH_KNOTS('',3,(#27071,#27072,#27073,#27074,#27075,
#27076,#27077,#27078,#27079,#27080,#27081,#27082,#27083,#27084,#27085,#27086,
#27087,#27088),.UNSPECIFIED.,.F.,.F.,(4,1,1,1,1,1,1,1,1,1,1,1,1,1,1,4),
(0.134726986384039,0.138033894591262,0.157795792183236,0.177557689775211,
0.197319587367185,0.207200536163172,0.21708148495916,0.256605280143108,
0.296129075327057,0.335652870511006,0.35541476810298,0.375176665694955,
0.394938563286929,0.414700460878903,0.424581409674891,0.454224256062852),
 .UNSPECIFIED.);
#430=B_SPLINE_CURVE_WITH_KNOTS('',3,(#27092,#27093,#27094,#27095,#27096,
#27097,#27098,#27099,#27100,#27101,#27102,#27103,#27104,#27105,#27106,#27107,
#27108,#27109,#27110),.UNSPECIFIED.,.F.,.F.,(4,1,1,1,1,1,1,1,1,1,1,1,1,
1,1,1,4),(0.,0.032572548443813,0.0434300645917507,0.065145096887626,0.0868601291835013,
0.097717645331439,0.108575161479377,0.130290193775252,0.173720258367003,
0.260580387550504,0.266009145624473,0.271437903698442,0.282295419846379,
0.298581694068286,0.304010452142255,0.347440516734005,0.350748646683325),
 .UNSPECIFIED.);
#431=B_SPLINE_CURVE_WITH_KNOTS('',3,(#27114,#27115,#27116,#27117,#27118,
#27119,#27120,#27121,#27122,#27123,#27124,#27125,#27126,#27127,#27128,#27129,
#27130),.UNSPECIFIED.,.F.,.F.,(4,1,1,1,1,1,1,1,1,1,1,1,1,1,4),(0.0574324344854207,
0.0593504322920632,0.0822759013466683,0.105201370401273,0.110932737664925,
0.116664104928576,0.128126839455878,0.139589573983181,0.151052308510483,
0.17970914482874,0.196903246619694,0.208365981146996,0.219828715674299,
0.22556008293795,0.242754184728904),.UNSPECIFIED.);
#432=B_SPLINE_CURVE_WITH_KNOTS('',3,(#27134,#27135,#27136,#27137,#27138,
#27139,#27140,#27141,#27142,#27143,#27144,#27145,#27146,#27147,#27148,#27149,
#27150,#27151,#27152,#27153),.UNSPECIFIED.,.F.,.F.,(4,1,1,1,1,1,1,1,1,1,
1,1,1,1,1,1,1,4),(0.,0.0325789546137133,0.0434386061516177,0.0651579092274265,
0.0868772123032354,0.0977368638411398,0.108596515379044,0.130315818454853,
0.173754424606471,0.217193030758089,0.238912333833897,0.260631636909706,
0.271491288447611,0.282350939985515,0.29321059152342,0.304070243061324,
0.347508849212942,0.350821898751245),.UNSPECIFIED.);
#433=B_SPLINE_CURVE_WITH_KNOTS('',3,(#27157,#27158,#27159,#27160,#27161,
#27162,#27163,#27164,#27165,#27166,#27167,#27168,#27169,#27170,#27171),
 .UNSPECIFIED.,.F.,.F.,(4,1,1,1,1,1,1,1,1,1,1,1,4),(0.351261425313739,0.354255847717629,
0.390044847704719,0.425833847691809,0.470570097675672,0.479517347672445,
0.49741184766599,0.542148097649853,0.568989847640171,0.586884347633716,
0.604778847627261,0.613726097624034,0.640567847614352),.UNSPECIFIED.);
#434=B_SPLINE_CURVE_WITH_KNOTS('',3,(#27175,#27176,#27177,#27178,#27179,
#27180,#27181,#27182,#27183,#27184,#27185,#27186,#27187,#27188,#27189,#27190,
#27191,#27192,#27193),.UNSPECIFIED.,.F.,.F.,(4,1,1,1,1,1,1,1,1,1,1,1,1,
1,1,1,4),(0.,0.0325793930141872,0.043439190685583,0.0542989883569787,0.0651587860283745,
0.086878381371166,0.0977381790425617,0.119457774385353,0.130317572056749,
0.173756762742332,0.217195953427915,0.238915548770706,0.260635144113498,
0.282354739456289,0.314934132470477,0.347513525484664,0.350848293700851),
 .UNSPECIFIED.);
#435=B_SPLINE_CURVE_WITH_KNOTS('',3,(#27197,#27198,#27199,#27200,#27201,
#27202,#27203,#27204,#27205,#27206,#27207,#27208,#27209,#27210,#27211,#27212,
#27213),.UNSPECIFIED.,.F.,.F.,(4,1,1,1,1,1,1,1,1,1,1,1,1,1,4),(0.351261530740907,
0.354255847382348,0.390044843362201,0.425833839342054,0.434781088337017,
0.44372833733198,0.461622835321907,0.479517333311833,0.49741183130176,0.542148076276576,
0.568989823261466,0.586884321251392,0.604778819241319,0.613726068236282,
0.640567815221172),.UNSPECIFIED.);
#436=B_SPLINE_CURVE_WITH_KNOTS('',3,(#27217,#27218,#27219,#27220,#27221,
#27222,#27223,#27224,#27225,#27226,#27227,#27228,#27229,#27230,#27231,#27232,
#27233,#27234,#27235),.UNSPECIFIED.,.F.,.F.,(4,1,1,1,1,1,1,1,1,1,1,1,1,
1,1,1,4),(0.,0.021719595347394,0.032579393021091,0.043439190694788,0.065158786042182,
0.0868783813895759,0.0977381790632729,0.119457774410667,0.130317572084364,
0.173756762779152,0.21719595347394,0.238915548821334,0.260635144168728,
0.282354739516122,0.304074334863516,0.347513525558304,0.350824050932044),
 .UNSPECIFIED.);
#437=B_SPLINE_CURVE_WITH_KNOTS('',3,(#27239,#27240,#27241,#27242,#27243,
#27244,#27245,#27246,#27247,#27248,#27249,#27250,#27251,#27252,#27253,#27254,
#27255,#27256),.UNSPECIFIED.,.F.,.F.,(4,1,1,1,1,1,1,1,1,1,1,1,1,1,1,4),
(0.351271479446867,0.354255847276431,0.3721503446334,0.381097593311884,
0.390044841990369,0.407939339347338,0.425833836704307,0.443728334061276,
0.497411826132183,0.533200820846121,0.55109531820309,0.568989815560059,
0.586884312917028,0.604778810273997,0.613726058952482,0.640567804987935),
 .UNSPECIFIED.);
#438=B_SPLINE_CURVE_WITH_KNOTS('',3,(#27260,#27261,#27262,#27263,#27264,
#27265,#27266,#27267,#27268,#27269,#27270,#27271,#27272,#27273,#27274),
 .UNSPECIFIED.,.F.,.F.,(4,1,1,1,1,1,1,1,1,1,1,1,4),(0.,0.0325793930123882,
0.0434391906831843,0.0651587860247764,0.0868783813663685,0.119457774378757,
0.173756762732737,0.195476358074329,0.260635144099105,0.271494941769902,
0.30407433478229,0.347513525465474,0.350791036601536),.UNSPECIFIED.);
#439=B_SPLINE_CURVE_WITH_KNOTS('',3,(#27278,#27279,#27280,#27281,#27282,
#27283,#27284,#27285,#27286,#27287,#27288,#27289,#27290,#27291,#27292,#27293,
#27294),.UNSPECIFIED.,.F.,.F.,(4,1,1,1,1,1,1,1,1,1,1,1,1,1,4),(0.351261728605554,
0.354255847725072,0.37215034776309,0.390044847801108,0.407939347839126,
0.416886597858135,0.425833847877144,0.479517347991197,0.497411848029215,
0.542148098124259,0.568989848181286,0.586884348219304,0.604778848257322,
0.613726098276331,0.640567848333357),.UNSPECIFIED.);
#440=B_SPLINE_CURVE_WITH_KNOTS('',3,(#27298,#27299,#27300,#27301,#27302,
#27303,#27304,#27305,#27306,#27307,#27308,#27309,#27310,#27311,#27312,#27313),
 .UNSPECIFIED.,.F.,.F.,(4,1,1,1,1,1,1,1,1,1,1,1,1,4),(0.,0.0325793930249551,
0.0434391906999401,0.0651587860499102,0.0868783813998803,0.0977381790748653,
0.119457774424835,0.173756762799761,0.217195953499701,0.249775346524656,
0.260635144199641,0.282354739549611,0.347513525599521,0.350789741290272),
 .UNSPECIFIED.);
#441=B_SPLINE_CURVE_WITH_KNOTS('',3,(#27317,#27318,#27319,#27320,#27321,
#27322,#27323,#27324,#27325,#27326,#27327,#27328,#27329,#27330,#27331),
 .UNSPECIFIED.,.F.,.F.,(4,1,1,1,1,1,1,1,1,1,1,1,4),(0.351261425313738,0.35425584759651,
0.390044846136022,0.425833844675534,0.461622843215046,0.479517342484802,
0.497411841754558,0.551095339563825,0.568989838833581,0.586884338103337,
0.604778837373093,0.613726087007971,0.640567835912605),.UNSPECIFIED.);
#442=B_SPLINE_CURVE_WITH_KNOTS('',3,(#27335,#27336,#27337,#27338,#27339,
#27340,#27341,#27342,#27343,#27344,#27345,#27346,#27347,#27348,#27349,#27350,
#27351,#27352,#27353,#27354),.UNSPECIFIED.,.F.,.F.,(4,1,1,1,1,1,1,1,1,1,
1,1,1,1,1,1,1,4),(0.,0.0325793930116233,0.0434391906821644,0.0542989883527054,
0.0651587860232465,0.0868783813643287,0.0977381790348698,0.119457774375952,
0.130317572046493,0.173756762728657,0.217195953410822,0.238915548751904,
0.260635144092986,0.282354739434068,0.30407433477515,0.325793930116233,
0.347513525457315,0.350813372103892),.UNSPECIFIED.);
#443=B_SPLINE_CURVE_WITH_KNOTS('',3,(#27358,#27359,#27360,#27361,#27362,
#27363,#27364,#27365,#27366,#27367,#27368,#27369,#27370,#27371,#27372),
 .UNSPECIFIED.,.F.,.F.,(4,1,1,1,1,1,1,1,1,1,1,1,4),(0.351261425313738,0.354255847421228,
0.390044843865796,0.425833840310363,0.461622836754931,0.479517334977215,
0.497411833199498,0.55109532786635,0.568989826088633,0.586884324310917,
0.604778822533201,0.613726071644343,0.640567818977768),.UNSPECIFIED.);
#444=B_SPLINE_CURVE_WITH_KNOTS('',3,(#27376,#27377,#27378,#27379,#27380,
#27381,#27382,#27383,#27384,#27385,#27386,#27387,#27388,#27389,#27390,#27391),
 .UNSPECIFIED.,.F.,.F.,(4,1,1,1,1,1,1,1,1,1,1,1,1,4),(0.,0.0325793097402814,
0.0434390796537085,0.0651586194805627,0.086878159307417,0.0977379292208441,
0.173756318614834,0.195475858441688,0.217195398268542,0.260634477922251,
0.304073557575959,0.336652867316241,0.347512637229668,0.350798526118062),
 .UNSPECIFIED.);
#445=B_SPLINE_CURVE_WITH_KNOTS('',3,(#27395,#27396,#27397,#27398,#27399,
#27400,#27401,#27402,#27403,#27404,#27405,#27406,#27407,#27408),
 .UNSPECIFIED.,.F.,.F.,(4,1,1,1,1,1,1,1,1,1,1,4),(0.0931972916890651,0.0981391683195413,
0.216268676323884,0.24580105332497,0.290099618826599,0.334398184328228,
0.408229126830942,0.452527692332571,0.482060069333657,0.511592446334743,
0.526358634835285,0.570657200336914),.UNSPECIFIED.);
#446=B_SPLINE_CURVE_WITH_KNOTS('',3,(#27412,#27413,#27414,#27415,#27416,
#27417,#27418,#27419,#27420,#27421,#27422,#27423,#27424,#27425,#27426,#27427),
 .UNSPECIFIED.,.F.,.F.,(4,1,1,1,1,1,1,1,1,1,1,1,1,4),(0.,0.0368941921573239,
0.0491922562097653,0.0737883843146479,0.0983845124195305,0.110682576471972,
0.135278704576854,0.196769024839061,0.245961281048826,0.270557409153709,
0.295153537258592,0.319749665363474,0.393538049678122,0.397251142174947),
 .UNSPECIFIED.);
#447=B_SPLINE_CURVE_WITH_KNOTS('',3,(#27431,#27432,#27433,#27434,#27435,
#27436,#27437,#27438,#27439,#27440,#27441,#27442,#27443,#27444,#27445,#27446,
#27447,#27448),.UNSPECIFIED.,.F.,.F.,(4,1,1,1,1,1,1,1,1,1,1,1,1,1,1,4),
(0.136741791121389,0.139904182663315,0.158819432388561,0.196649931839055,
0.215565181564302,0.234480431289549,0.253395681014796,0.291226180465289,
0.338514304778406,0.34797192964103,0.357429554503653,0.366887179366277,
0.385802429091524,0.404717678816771,0.414175303679394,0.442548178267264),
 .UNSPECIFIED.);
#448=B_SPLINE_CURVE_WITH_KNOTS('',3,(#27452,#27453,#27454,#27455,#27456,
#27457,#27458,#27459,#27460,#27461,#27462,#27463,#27464,#27465,#27466),
 .UNSPECIFIED.,.F.,.F.,(4,1,1,1,1,1,1,1,1,1,1,1,4),(0.,0.0325793930125535,
0.0434391906834047,0.0651587860251071,0.0868783813668094,0.108597976708512,
0.173756762733619,0.195476358075321,0.217195953417024,0.260635144100428,
0.304074334783833,0.347513525467238,0.350846174826461),.UNSPECIFIED.);
#449=B_SPLINE_CURVE_WITH_KNOTS('',3,(#27470,#27471,#27472,#27473,#27474,
#27475,#27476,#27477,#27478,#27479,#27480,#27481,#27482,#27483,#27484,#27485),
 .UNSPECIFIED.,.F.,.F.,(4,1,1,1,1,1,1,1,1,1,1,1,1,4),(0.351271301501517,
0.354255847707038,0.407939347497804,0.425833847428059,0.443728347358315,
0.488464597183953,0.497411847149081,0.515306347079336,0.551095346939847,
0.568989846870102,0.586884346800358,0.604778846730613,0.613726096695741,
0.640567846591124),.UNSPECIFIED.);
#450=B_SPLINE_CURVE_WITH_KNOTS('',3,(#27489,#27490,#27491,#27492,#27493,
#27494,#27495,#27496,#27497,#27498,#27499,#27500,#27501,#27502,#27503,#27504),
 .UNSPECIFIED.,.F.,.F.,(4,1,1,1,1,1,1,1,1,1,1,1,1,4),(0.,0.0325793930317906,
0.0434391907090541,0.0651587860635812,0.0868783814181082,0.108597976772635,
0.130317572127162,0.173756762836216,0.217195953545271,0.260635144254325,
0.282354739608852,0.325793930317906,0.347513525672433,0.350848293890421),
 .UNSPECIFIED.);
#451=B_SPLINE_CURVE_WITH_KNOTS('',3,(#27508,#27509,#27510,#27511,#27512,
#27513,#27514,#27515,#27516,#27517,#27518,#27519,#27520,#27521,#27522,#27523,
#27524),.UNSPECIFIED.,.F.,.F.,(4,1,1,1,1,1,1,1,1,1,1,1,1,1,4),(0.351261678797134,
0.35425584762492,0.372150347064446,0.390044846503972,0.407939345943498,
0.416886595663261,0.425833845383024,0.479517343701602,0.497411843141128,
0.542148091739942,0.568989840899231,0.586884340338757,0.604778839778283,
0.613726089498046,0.640567838657335),.UNSPECIFIED.);
#452=B_SPLINE_CURVE_WITH_KNOTS('',3,(#27528,#27529,#27530,#27531,#27532,
#27533,#27534,#27535,#27536,#27537,#27538,#27539,#27540,#27541,#27542),
 .UNSPECIFIED.,.F.,.F.,(4,1,1,1,1,1,1,1,1,1,1,1,4),(0.,0.0325793930157896,
0.0434391906877195,0.0651587860315793,0.086878381375439,0.108597976719299,
0.130317572063159,0.173756762750878,0.217195953438598,0.260635144126317,
0.304074334814037,0.347513525501756,0.350842474191291),.UNSPECIFIED.);
#453=B_SPLINE_CURVE_WITH_KNOTS('',3,(#27546,#27547,#27548,#27549,#27550,
#27551,#27552,#27553,#27554,#27555,#27556,#27557,#27558,#27559,#27560,#27561,
#27562,#27563,#27564,#27565,#27566,#27567,#27568,#27569,#27570,#27571,#27572,
#27573,#27574,#27575,#27576,#27577,#27578,#27579,#27580,#27581,#27582,#27583,
#27584,#27585),.UNSPECIFIED.,.F.,.F.,(4,3,3,3,3,3,3,3,3,3,3,3,3,4),(0.000100343318888589,
0.00211700710578998,0.0116301296248504,0.0176438447776065,0.0203218262442056,
0.0279911126768708,0.0341353720887311,0.0378914478697084,0.0416646752176139,
0.045727158280587,0.0481343714586611,0.0509000843805532,0.0542503351447326,
0.0813895718295443),.UNSPECIFIED.);
#454=B_SPLINE_CURVE_WITH_KNOTS('',3,(#27589,#27590,#27591,#27592,#27593,
#27594,#27595,#27596,#27597,#27598,#27599,#27600,#27601,#27602,#27603),
 .UNSPECIFIED.,.F.,.F.,(4,1,1,1,1,1,1,1,1,1,1,1,4),(0.,0.0325793930236318,
0.0434391906981757,0.0651587860472636,0.0868783813963514,0.119457774419983,
0.173756762792703,0.195476358141791,0.260635144189054,0.271494941863598,
0.30407433488723,0.347513525585406,0.350787783602951),.UNSPECIFIED.);
#455=B_SPLINE_CURVE_WITH_KNOTS('',3,(#27607,#27608,#27609,#27610,#27611,
#27612,#27613,#27614,#27615,#27616,#27617,#27618,#27619,#27620,#27621,#27622,
#27623),.UNSPECIFIED.,.F.,.F.,(4,1,1,1,1,1,1,1,1,1,1,1,1,1,4),(0.351273472241782,
0.354255847802748,0.372150348304963,0.390044848807178,0.407939349309393,
0.425833849811608,0.461622850816039,0.497411851820469,0.542148103076006,
0.551095353327114,0.568989853829329,0.586884354331544,0.604778854833759,
0.613726105084867,0.64056785583819),.UNSPECIFIED.);
#456=B_SPLINE_CURVE_WITH_KNOTS('',3,(#27627,#27628,#27629,#27630,#27631,
#27632,#27633,#27634,#27635,#27636,#27637,#27638,#27639,#27640,#27641),
 .UNSPECIFIED.,.F.,.F.,(4,1,1,1,1,1,1,1,1,1,1,1,4),(0.,0.032579393022239,
0.0434391906963187,0.065158786044478,0.0868783813926374,0.108597976740797,
0.130317572088956,0.173756762785275,0.260635144177912,0.271494941851992,
0.304074334874231,0.347513525570549,0.350823140362429),.UNSPECIFIED.);
#457=B_SPLINE_CURVE_WITH_KNOTS('',3,(#27645,#27646,#27647,#27648,#27649,
#27650,#27651,#27652,#27653,#27654,#27655,#27656,#27657,#27658,#27659),
 .UNSPECIFIED.,.F.,.F.,(4,1,1,1,1,1,1,1,1,1,1,1,4),(0.351261425313741,0.35425584764769,
0.390044846798899,0.425833845950108,0.461622845101317,0.479517344676922,
0.497411844252526,0.542148093191537,0.568989842554944,0.586884342130548,
0.604778841706153,0.613726091493955,0.640567840857362),.UNSPECIFIED.);
#458=B_SPLINE_CURVE_WITH_KNOTS('',3,(#27663,#27664,#27665,#27666,#27667,
#27668,#27669,#27670,#27671,#27672,#27673,#27674,#27675,#27676,#27677,#27678,
#27679,#27680,#27681),.UNSPECIFIED.,.F.,.F.,(4,1,1,1,1,1,1,1,1,1,1,1,1,
1,1,1,4),(0.,0.0327837338451708,0.0437116451268944,0.0655674676903416,0.0874232902537888,
0.109279112817236,0.131134935380683,0.174846580507578,0.196702403071025,
0.218558225634472,0.262269870761366,0.267733826402228,0.27319778204309,
0.284125693324814,0.305981515888261,0.349693161015155,0.35304098170316),
 .UNSPECIFIED.);
#459=B_SPLINE_CURVE_WITH_KNOTS('',3,(#27685,#27686,#27687,#27688,#27689,
#27690,#27691,#27692,#27693,#27694,#27695,#27696,#27697,#27698,#27699,#27700,
#27701),.UNSPECIFIED.,.F.,.F.,(4,1,1,1,1,1,1,1,1,1,1,1,1,1,4),(0.134727030764327,
0.138033894591211,0.177557689775802,0.217081484960394,0.226962433756542,
0.23684338255269,0.256605280144986,0.276367177737282,0.296129075329578,
0.345533819310318,0.375176665698762,0.394938563291058,0.414700460883354,
0.424581409679502,0.454224256067946),.UNSPECIFIED.);
#460=B_SPLINE_CURVE_WITH_KNOTS('',3,(#27705,#27706,#27707,#27708,#27709,
#27710,#27711,#27712),.UNSPECIFIED.,.F.,.F.,(4,2,2,4),(0.,0.0512135387342888,
0.087237825725378,0.157821777158906),.UNSPECIFIED.);
#461=B_SPLINE_CURVE_WITH_KNOTS('',3,(#27716,#27717,#27718,#27719,#27720,
#27721,#27722,#27723,#27724,#27725,#27726,#27727,#27728,#27729,#27730,#27731,
#27732,#27733,#27734,#27735),.UNSPECIFIED.,.F.,.F.,(4,1,1,1,1,1,1,1,1,1,
1,1,1,1,1,1,1,4),(0.0574322859850518,0.0593504322657392,0.0822759010057599,
0.0937386353757703,0.105201369745781,0.108067053338283,0.110932736930786,
0.116664104115791,0.128126838485801,0.139589572855812,0.151052307225822,
0.179709143150848,0.191171877520858,0.196903244705864,0.208365979075874,
0.219828713445884,0.22556008063089,0.242754182185905),.UNSPECIFIED.);
#462=B_SPLINE_CURVE_WITH_KNOTS('',3,(#27739,#27740,#27741,#27742,#27743,
#27744,#27745,#27746,#27747,#27748,#27749,#27750,#27751,#27752,#27753,#27754,
#27755,#27756),.UNSPECIFIED.,.F.,.F.,(4,1,1,1,1,1,1,1,1,1,1,1,1,1,1,4),
(0.,0.0325789545997274,0.0434386061329699,0.0651579091994548,0.0868772122659398,
0.0977368637991822,0.119456166865667,0.17375442453188,0.217193030664849,
0.260631636797819,0.271491288331062,0.282350939864304,0.304070242930789,
0.325789545997274,0.347508849063759,0.350802705344221),.UNSPECIFIED.);
#463=B_SPLINE_CURVE_WITH_KNOTS('',3,(#27760,#27761,#27762,#27763,#27764,
#27765,#27766,#27767,#27768,#27769,#27770,#27771,#27772,#27773,#27774,#27775,
#27776,#27777,#27778),.UNSPECIFIED.,.F.,.F.,(4,1,1,1,1,1,1,1,1,1,1,1,1,
1,1,1,4),(0.351274828846267,0.354255848623625,0.39004485943905,0.394518485790978,
0.407939364846763,0.416886617550619,0.421360243902547,0.425833870254475,
0.497411891885325,0.53320090270075,0.551095408108462,0.560042660812319,
0.568989913516175,0.586884418923887,0.6047789243316,0.613726177035456,0.640567935147025),
 .UNSPECIFIED.);
#464=B_SPLINE_CURVE_WITH_KNOTS('',3,(#27782,#27783,#27784,#27785,#27786,
#27787,#27788,#27789,#27790,#27791,#27792,#27793,#27794,#27795,#27796,#27797,
#27798,#27799),.UNSPECIFIED.,.F.,.F.,(4,1,1,1,1,1,1,1,1,1,1,1,1,1,1,4),
(0.,0.0325793930123313,0.0434391906831083,0.0651587860246625,0.0868783813662167,
0.0977381790369938,0.119457774378548,0.173756762732433,0.217195953415542,
0.26063514409865,0.271494941769427,0.282354739440204,0.304074334781758,
0.325793930123313,0.347513525464867,0.350806496344244),.UNSPECIFIED.);
#465=B_SPLINE_CURVE_WITH_KNOTS('',3,(#27803,#27804,#27805,#27806,#27807,
#27808,#27809,#27810,#27811,#27812,#27813,#27814,#27815,#27816,#27817,#27818,
#27819,#27820,#27821,#27822,#27823,#27824,#27825),.UNSPECIFIED.,.F.,.F.,
(4,2,2,1,1,1,1,1,1,1,1,1,1,1,1,1,1,1,4),(0.351271261271763,0.353137441377921,
0.354255847573797,0.372150346707808,0.390044845841819,0.407939344975829,
0.42583384410984,0.443728343243851,0.461622842377862,0.479517341511873,
0.497411840645883,0.533200838913905,0.551095338047916,0.560042587614921,
0.568989837181927,0.586884336315937,0.604778835449948,0.613726085016954,
0.64056783371797),.UNSPECIFIED.);
#466=B_SPLINE_CURVE_WITH_KNOTS('',3,(#27829,#27830,#27831,#27832,#27833,
#27834,#27835,#27836,#27837,#27838,#27839,#27840,#27841,#27842,#27843,#27844,
#27845,#27846),.UNSPECIFIED.,.F.,.F.,(4,1,1,1,1,1,1,1,1,1,1,1,1,1,1,4),
(0.,0.0325793930260695,0.0434391907014261,0.0651587860521391,0.0868783814028521,
0.108597976753565,0.130317572104278,0.173756762805704,0.260635144208556,
0.304074334909982,0.306789284328822,0.309504233747661,0.314934132585339,
0.325793930260696,0.347513525611409,0.350836093641256),.UNSPECIFIED.);
#467=B_SPLINE_CURVE_WITH_KNOTS('',3,(#27850,#27851,#27852,#27853,#27854,
#27855,#27856,#27857,#27858,#27859,#27860,#27861,#27862,#27863,#27864,#27865,
#27866,#27867,#27868),.UNSPECIFIED.,.F.,.F.,(4,1,1,1,1,1,1,1,1,1,1,1,1,
1,1,1,4),(0.351264100247147,0.354255847560549,0.372150346615404,0.390044845670259,
0.407939344725115,0.416886594252542,0.42583384377997,0.461622841889681,
0.488464590471964,0.497411839999392,0.533200838109102,0.551095337163958,
0.568989836218813,0.586884335273668,0.604778834328524,0.613726083855951,
0.640567832438234),.UNSPECIFIED.);
#468=B_SPLINE_CURVE_WITH_KNOTS('',3,(#27872,#27873,#27874,#27875,#27876,
#27877,#27878,#27879,#27880,#27881,#27882,#27883,#27884,#27885,#27886,#27887,
#27888,#27889),.UNSPECIFIED.,.F.,.F.,(4,1,1,1,1,1,1,1,1,1,1,1,1,1,1,4),
(0.,0.0325793930079354,0.0434391906772472,0.0651587860158707,0.0868783813544943,
0.11945777436243,0.152037167370365,0.173756762708989,0.195476358047612,
0.217195953386236,0.238915548724859,0.260635144063483,0.282354739402107,
0.30407433474073,0.347513525417977,0.350816322009827),.UNSPECIFIED.);
#469=B_SPLINE_CURVE_WITH_KNOTS('',3,(#27893,#27894,#27895,#27896,#27897,
#27898,#27899,#27900,#27901,#27902,#27903,#27904,#27905,#27906,#27907,#27908,
#27909,#27910,#27911),.UNSPECIFIED.,.F.,.F.,(4,1,1,1,1,1,1,1,1,1,1,1,1,
1,1,1,4),(0.351263876883672,0.354255847479606,0.372150346050742,0.390044844621878,
0.407939343193014,0.416886592478582,0.42583384176415,0.461622838906422,
0.488464586763126,0.497411836048694,0.533200833190966,0.551095331762102,
0.568989830333238,0.586884328904374,0.60477882747551,0.613726076761078,
0.640567824617782),.UNSPECIFIED.);
#470=B_SPLINE_CURVE_WITH_KNOTS('',3,(#27915,#27916,#27917,#27918,#27919,
#27920,#27921,#27922,#27923,#27924,#27925,#27926,#27927,#27928,#27929,#27930,
#27931,#27932,#27933,#27934,#27935),.UNSPECIFIED.,.F.,.F.,(4,1,1,1,1,1,
1,1,1,1,1,1,1,1,1,1,1,1,4),(0.,0.0325793930226444,0.0434391906968592,0.0651587860452888,
0.0868783813937184,0.0977381790679332,0.108597976742148,0.130317572090578,
0.173756762787437,0.217195953484296,0.238915548832726,0.260635144181155,
0.266065043018263,0.27149494185537,0.282354739529585,0.2932145372038,0.304074334878014,
0.347513525574874,0.350818340766546),.UNSPECIFIED.);
#471=B_SPLINE_CURVE_WITH_KNOTS('',3,(#27939,#27940,#27941,#27942,#27943,
#27944,#27945,#27946,#27947,#27948,#27949,#27950,#27951,#27952,#27953,#27954,
#27955,#27956),.UNSPECIFIED.,.F.,.F.,(4,1,1,1,1,1,1,1,1,1,1,1,1,1,1,4),
(0.351261425313741,0.354255848056333,0.372150350073952,0.381097601082762,
0.385571226587167,0.38780803933937,0.390044852091572,0.425833856126811,
0.49741186419729,0.533200868232529,0.551095370250149,0.568989872267768,
0.586884374285388,0.604778876303007,0.613726127311817,0.640567880338247),
 .UNSPECIFIED.);
#472=B_SPLINE_CURVE_WITH_KNOTS('',3,(#27960,#27961,#27962,#27963,#27964,
#27965,#27966,#27967,#27968,#27969,#27970,#27971,#27972,#27973,#27974,#27975,
#27976),.UNSPECIFIED.,.F.,.F.,(4,1,1,1,1,1,1,1,1,1,1,1,1,1,4),(0.,0.0325793930148059,
0.0434391906864078,0.0651587860296118,0.0868783813728157,0.119457774387622,
0.152037167402427,0.173756762745631,0.195476358088835,0.217195953432039,
0.228055751103641,0.238915548775243,0.260635144118447,0.347513525491263,
0.35080304454135),.UNSPECIFIED.);
#473=B_SPLINE_CURVE_WITH_KNOTS('',3,(#27980,#27981,#27982,#27983,#27984,
#27985,#27986,#27987,#27988,#27989,#27990,#27991,#27992,#27993,#27994),
 .UNSPECIFIED.,.F.,.F.,(4,1,1,1,1,1,1,1,1,1,1,1,4),(0.35126142531374,0.354255847892618,
0.390044849971179,0.42583385204974,0.4616228541283,0.479517355167581,0.497411856206861,
0.542148108805062,0.568989860363982,0.586884361403262,0.604778862442543,
0.613726112962183,0.640567864521103),.UNSPECIFIED.);
#474=B_SPLINE_CURVE_WITH_KNOTS('',3,(#27998,#27999,#28000,#28001,#28002,
#28003,#28004,#28005,#28006,#28007,#28008,#28009,#28010,#28011,#28012,#28013,
#28014,#28015,#28016,#28017,#28018,#28019),.UNSPECIFIED.,.F.,.F.,(4,1,1,
1,1,1,1,1,1,1,1,1,1,1,1,1,1,1,1,4),(0.,0.0217195398190078,0.0325793097285116,
0.0434390796380155,0.0651586194570233,0.086878159276031,0.092308044230783,
0.0977379291855349,0.108597699095039,0.130317238914047,0.173756318552062,
0.19547585837107,0.217195398190078,0.238914938009085,0.260634477828093,
0.282354017647101,0.304073557466109,0.314933327375612,0.347512637104124,
0.350829886386395),.UNSPECIFIED.);
#475=B_SPLINE_CURVE_WITH_KNOTS('',3,(#28023,#28024,#28025,#28026,#28027,
#28028,#28029,#28030,#28031,#28032,#28033,#28034,#28035,#28036,#28037,#28038,
#28039,#28040),.UNSPECIFIED.,.F.,.F.,(4,1,1,1,1,1,1,1,1,1,1,1,1,1,1,4),
(0.0932056818412186,0.0981391682442792,0.127671545353425,0.142437733907998,
0.15720392246257,0.186736299571716,0.216268676680861,0.245801053790007,
0.334398185117444,0.393462939335735,0.42299531644488,0.452527693554026,
0.482060070663172,0.511592447772317,0.52635863632689,0.570657201990608),
 .UNSPECIFIED.);
#476=B_SPLINE_CURVE_WITH_KNOTS('',3,(#28044,#28045,#28046,#28047,#28048,
#28049),.UNSPECIFIED.,.F.,.F.,(4,2,4),(0.,0.0601601681445252,0.0880292330372518),
 .UNSPECIFIED.);
#477=B_SPLINE_CURVE_WITH_KNOTS('',3,(#28053,#28054,#28055,#28056,#28057,
#28058,#28059,#28060,#28061,#28062,#28063,#28064,#28065,#28066,#28067,#28068,
#28069,#28070,#28071,#28072,#28073,#28074,#28075,#28076,#28077,#28078,#28079,
#28080,#28081,#28082,#28083,#28084,#28085,#28086,#28087,#28088,#28089,#28090,
#28091,#28092,#28093,#28094,#28095,#28096,#28097,#28098,#28099,#28100,#28101,
#28102,#28103,#28104,#28105,#28106,#28107,#28108,#28109,#28110),
 .UNSPECIFIED.,.F.,.F.,(4,3,3,3,3,3,3,3,3,3,3,3,3,3,3,3,3,3,3,4),(6.08712730435348E-5,
0.00275844945283138,0.0137381870738885,0.0225620476034396,0.0312714732191953,
0.0362576288629832,0.0423533777643801,0.0549063154363092,0.0674592531082383,
0.0925651284520965,0.142776879139813,0.255475301627304,0.367738092144255,
0.372730032656669,0.391490074030401,0.400744250952332,0.409965101196975,
0.421939848038402,0.429790402970525,0.485968151358161),.UNSPECIFIED.);
#478=B_SPLINE_CURVE_WITH_KNOTS('',3,(#28119,#28120,#28121,#28122,#28123,
#28124,#28125,#28126),.UNSPECIFIED.,.F.,.F.,(4,2,2,4),(6.11743783436508E-5,
0.191849769363527,0.239938446755784,0.283419085994991),.UNSPECIFIED.);
#479=B_SPLINE_CURVE_WITH_KNOTS('',3,(#28130,#28131,#28132,#28133,#28134,
#28135,#28136,#28137,#28138,#28139,#28140,#28141,#28142,#28143,#28144,#28145,
#28146,#28147),.UNSPECIFIED.,.F.,.F.,(4,1,1,1,1,1,1,1,1,1,1,1,1,1,1,4),
(0.,0.0325750462990963,0.0434333950654617,0.0651500925981926,0.0868667901309233,
0.108583487663654,0.130300185196385,0.173733580261847,0.217166975327308,
0.26060037039277,0.271458719159135,0.282317067925501,0.304033765458232,
0.325750462990963,0.347467160523693,0.350763145419038),.UNSPECIFIED.);
#480=B_SPLINE_CURVE_WITH_KNOTS('',3,(#28151,#28152,#28153,#28154,#28155,
#28156,#28157,#28158,#28159,#28160,#28161,#28162,#28163,#28164,#28165,#28166,
#28167,#28168),.UNSPECIFIED.,.F.,.F.,(4,1,1,1,1,1,1,1,1,1,1,1,1,1,1,4),
(0.0932058072533814,0.096518162942361,0.116363502645051,0.136208842347741,
0.156054182050431,0.165976851901776,0.175899521753121,0.215590201158501,
0.255280880563881,0.304894229820606,0.324739569523297,0.334662239374642,
0.354507579077332,0.374352918780022,0.384275588631367,0.414043598185402),
 .UNSPECIFIED.);
#481=B_SPLINE_CURVE_WITH_KNOTS('',3,(#28172,#28173,#28174,#28175,#28176,
#28177,#28178,#28179,#28180,#28181,#28182,#28183,#28184,#28185,#28186,#28187,
#28188,#28189),.UNSPECIFIED.,.F.,.F.,(4,1,1,1,1,1,1,1,1,1,1,1,1,1,1,4),
(0.,0.0325788513745152,0.0434384684993537,0.0651577027490305,0.0868769369987073,
0.108596171248384,0.130315405498061,0.173753873997415,0.238911576746445,
0.260630810996122,0.282350045245799,0.304069279495476,0.314928896620314,
0.325788513745152,0.347507747994829,0.350794257840603),.UNSPECIFIED.);
#482=B_SPLINE_CURVE_WITH_KNOTS('',3,(#28193,#28194,#28195,#28196,#28197,
#28198,#28199,#28200,#28201,#28202,#28203,#28204,#28205,#28206,#28207,#28208,
#28209,#28210,#28211,#28212,#28213,#28214,#28215,#28216,#28217,#28218,#28219,
#28220,#28221,#28222,#28223,#28224,#28225,#28226,#28227,#28228,#28229,#28230,
#28231,#28232,#28233,#28234,#28235,#28236,#28237,#28238,#28239,#28240,#28241,
#28242,#28243,#28244,#28245,#28246,#28247,#28248,#28249,#28250),
 .UNSPECIFIED.,.F.,.F.,(4,3,3,3,3,3,3,3,3,3,3,3,3,3,3,3,3,3,3,4),(2.64881849881361E-5,
0.00307223750536735,0.028642489643384,0.0367669288755048,0.0524286784203567,
0.0679644484217536,0.0833030784739446,0.0990034397740617,0.115012342116765,
0.132014384921338,0.171542385361576,0.19885726229201,0.214932531301613,
0.22333513626821,0.232015923980944,0.270309223346912,0.31550125331855,0.341731569313757,
0.371362864081148,0.439678803039698),.UNSPECIFIED.);
#483=B_SPLINE_CURVE_WITH_KNOTS('',3,(#28254,#28255,#28256,#28257,#28258,
#28259,#28260,#28261,#28262,#28263,#28264,#28265,#28266,#28267,#28268),
 .UNSPECIFIED.,.F.,.F.,(4,1,1,1,1,1,1,1,1,1,1,1,4),(0.,0.0325813112900846,
0.0434417483867794,0.0651626225801691,0.0868834967735589,0.119464808063643,
0.173766993547118,0.195487867740507,0.217208741933897,0.260650490320676,
0.304092238707456,0.347533987094235,0.350847240140668),.UNSPECIFIED.);
#484=B_SPLINE_CURVE_WITH_KNOTS('',3,(#28272,#28273,#28274,#28275,#28276,
#28277),.UNSPECIFIED.,.F.,.F.,(4,2,4),(8.14301014391022E-5,0.196579653373709,
0.311490292475107),.UNSPECIFIED.);
#485=B_SPLINE_CURVE_WITH_KNOTS('',3,(#28281,#28282,#28283,#28284,#28285,
#28286,#28287,#28288,#28289,#28290,#28291,#28292,#28293,#28294,#28295,#28296,
#28297,#28298),.UNSPECIFIED.,.F.,.F.,(4,1,1,1,1,1,1,1,1,1,1,1,1,1,1,4),
(0.,0.0325813113329355,0.0434417484439139,0.0651626226658709,0.0868834968878278,
0.108604371109785,0.130325245331742,0.173766993775656,0.260650490663484,
0.304092239107397,0.306807348385142,0.309522457662887,0.314952676218376,
0.325813113329354,0.347533987551311,0.350857049542678),.UNSPECIFIED.);
#486=B_SPLINE_CURVE_WITH_KNOTS('',3,(#28302,#28303,#28304,#28305,#28306,
#28307,#28308,#28309,#28310,#28311,#28312,#28313,#28314,#28315,#28316,#28317,
#28318,#28319,#28320,#28321,#28322,#28323,#28324,#28325,#28326,#28327,#28328,
#28329,#28330,#28331,#28332,#28333,#28334,#28335,#28336,#28337,#28338,#28339,
#28340,#28341,#28342,#28343,#28344,#28345,#28346,#28347,#28348,#28349,#28350,
#28351,#28352,#28353,#28354,#28355,#28356),.UNSPECIFIED.,.F.,.F.,(4,3,3,
3,3,3,3,3,3,3,3,3,3,3,3,3,3,3,4),(2.11964464360651E-5,0.00307933761122651,
0.0395949433846797,0.0486546450384591,0.0576974609832352,0.0668894095700696,
0.071471610540102,0.0760053733416042,0.0940997687264147,0.112217019766355,
0.148197822286634,0.184121554894769,0.202078226650051,0.211018420941679,
0.219896800832225,0.23983820976113,0.2677172728698,0.278184634008653,0.312492015504387),
 .UNSPECIFIED.);
#487=B_SPLINE_CURVE_WITH_KNOTS('',3,(#28360,#28361,#28362,#28363,#28364,
#28365,#28366,#28367,#28368,#28369,#28370,#28371,#28372,#28373,#28374,#28375,
#28376,#28377,#28378),.UNSPECIFIED.,.F.,.F.,(4,1,1,1,1,1,1,1,1,1,1,1,1,
1,1,1,4),(0.,0.0325813112891162,0.0434417483854882,0.0651626225782322,0.0868834967709763,
0.10860437096372,0.130325245156464,0.173766993541953,0.184627430638325,
0.217208741927441,0.260650490312929,0.271510927409301,0.282371364505673,
0.304092238698417,0.325813112891161,0.347533987083905,0.35082133726808),
 .UNSPECIFIED.);
#488=B_SPLINE_CURVE_WITH_KNOTS('',3,(#28382,#28383,#28384,#28385,#28386,
#28387),.UNSPECIFIED.,.F.,.F.,(4,2,4),(0.000173516420610335,0.167723093051734,
0.254522511958816),.UNSPECIFIED.);
#489=B_SPLINE_CURVE_WITH_KNOTS('',3,(#28391,#28392,#28393,#28394,#28395,
#28396,#28397,#28398,#28399,#28400,#28401,#28402,#28403,#28404,#28405,#28406,
#28407,#28408,#28409),.UNSPECIFIED.,.F.,.F.,(4,1,1,1,1,1,1,1,1,1,1,1,1,
1,1,1,4),(0.,0.0325813113093916,0.0434417484125221,0.0651626226187831,0.0868834968250442,
0.108604371031305,0.130325245237566,0.173766993650088,0.184627430753219,
0.21720874206261,0.260650490475133,0.271510927578263,0.282371364681394,
0.304092238887655,0.325813113093916,0.347533987300177,0.350820075515927),
 .UNSPECIFIED.);
#490=B_SPLINE_CURVE_WITH_KNOTS('',3,(#28413,#28414,#28415,#28416,#28417,
#28418),.UNSPECIFIED.,.F.,.F.,(4,2,4),(0.,0.264764622084999,0.482894632601792),
 .UNSPECIFIED.);
#491=B_SPLINE_CURVE_WITH_KNOTS('',3,(#28422,#28423,#28424,#28425,#28426,
#28427,#28428,#28429,#28430,#28431,#28432,#28433,#28434,#28435,#28436,#28437,
#28438,#28439,#28440,#28441,#28442,#28443,#28444),.UNSPECIFIED.,.F.,.F.,
(4,1,1,1,1,1,1,1,1,1,1,1,1,1,1,1,1,1,1,1,4),(0.,0.0325813113021046,0.0434417484028061,
0.0651626226042092,0.0868834968056123,0.0977439339063137,0.108604371007015,
0.130325245208418,0.173766993611225,0.195487867812628,0.217208742014031,
0.238929616215434,0.260650490416837,0.28237136461824,0.304092238819643,
0.325813113021046,0.347533987222449,0.348212764541243,0.348891541860037,
0.350249096497625,0.35080830738772),.UNSPECIFIED.);
#492=B_SPLINE_CURVE_WITH_KNOTS('',3,(#28448,#28449,#28450,#28451,#28452,
#28453,#28454,#28455,#28456,#28457,#28458,#28459,#28460,#28461,#28462,#28463,
#28464,#28465,#28466,#28467,#28468,#28469,#28470,#28471,#28472,#28473,#28474,
#28475,#28476,#28477,#28478,#28479,#28480,#28481,#28482,#28483,#28484,#28485,
#28486,#28487,#28488,#28489,#28490,#28491,#28492,#28493),.UNSPECIFIED.,
 .F.,.F.,(4,3,3,3,3,3,3,3,3,3,3,3,3,3,3,4),(2.29325682757538E-5,0.00307497248475355,
0.0214432536953726,0.0402954758924377,0.0593096938468517,0.0691626711428028,
0.0790635228724472,0.120294907072033,0.165515885024277,0.233611439622154,
0.268825942121262,0.290245409680214,0.354810754057985,0.445312525809899,
0.479839949490667,0.594280619733159),.UNSPECIFIED.);
#493=B_SPLINE_CURVE_WITH_KNOTS('',3,(#28497,#28498,#28499,#28500,#28501,
#28502,#28503,#28504,#28505,#28506,#28507,#28508,#28509,#28510,#28511,#28512,
#28513,#28514,#28515),.UNSPECIFIED.,.F.,.F.,(4,1,1,1,1,1,1,1,1,1,1,1,1,
1,1,1,4),(0.,0.0325811093290978,0.0434414791054637,0.0651622186581956,0.0868829582109275,
0.0977433279872934,0.108603697763659,0.130324437316391,0.173765916421855,
0.260648874632782,0.266079059520965,0.271509244409148,0.282369614185514,
0.298660168850063,0.304090353738246,0.34753183284371,0.35083845041488),
 .UNSPECIFIED.);
#494=B_SPLINE_CURVE_WITH_KNOTS('',3,(#28519,#28520,#28521,#28522,#28523,
#28524,#28525,#28526,#28527,#28528,#28529,#28530,#28531,#28532,#28533,#28534,
#28535,#28536),.UNSPECIFIED.,.F.,.F.,(4,1,1,1,1,1,1,1,1,1,1,1,1,1,1,4),
(0.134735529536501,0.138033894591027,0.157795792185277,0.177557689779527,
0.197319587373778,0.207200536170903,0.217081484968028,0.256605280156529,
0.29612907534503,0.345533819330656,0.365295716924906,0.375176665722032,
0.394938563316282,0.414700460910532,0.424581409707658,0.454224256099033),
 .UNSPECIFIED.);
#495=B_SPLINE_CURVE_WITH_KNOTS('',3,(#28540,#28541,#28542,#28543,#28544,
#28545,#28546,#28547,#28548,#28549,#28550,#28551,#28552,#28553,#28554,#28555,
#28556,#28557,#28558,#28559),.UNSPECIFIED.,.F.,.F.,(4,1,1,1,1,1,1,1,1,1,
1,1,1,1,1,1,1,4),(0.,0.0325779980296814,0.0434373307062418,0.0651559960593628,
0.0868746614124837,0.0977339940890442,0.119452659442165,0.173749322824967,
0.195467988178088,0.217186653531209,0.23890531888433,0.249764651560891,
0.255194317899171,0.260623984237451,0.282342649590572,0.304061314943693,
0.347498645649935,0.350792283140098),.UNSPECIFIED.);
#496=B_SPLINE_CURVE_WITH_KNOTS('',3,(#28563,#28564,#28565,#28566,#28567,
#28568,#28569,#28570,#28571,#28572,#28573,#28574,#28575,#28576,#28577,#28578,
#28579),.UNSPECIFIED.,.F.,.F.,(4,1,1,1,1,1,1,1,1,1,1,1,1,1,4),(0.0574322859849621,
0.0593504322721664,0.0708131666834375,0.0765445338890731,0.0822759010947087,
0.105201369917251,0.139589573151064,0.151052307562335,0.173977776384878,
0.185440510796149,0.19690324520742,0.208365979618691,0.219828714029962,
0.225560081235598,0.242754182852504),.UNSPECIFIED.);
#497=B_SPLINE_CURVE_WITH_KNOTS('',3,(#28583,#28584,#28585,#28586,#28587,
#28588,#28589,#28590,#28591,#28592,#28593,#28594,#28595,#28596,#28597,#28598,
#28599),.UNSPECIFIED.,.F.,.F.,(4,1,1,1,1,1,1,1,1,1,1,1,1,1,4),(0.,0.0325780266935636,
0.0434373689247514,0.0651560533871272,0.086874737849503,0.119452764543067,
0.173749475699006,0.195468160161382,0.217186844623757,0.238905529086133,
0.249764871317321,0.260624213548509,0.30406158247326,0.347498951398012,
0.35078480449443),.UNSPECIFIED.);
#498=B_SPLINE_CURVE_WITH_KNOTS('',3,(#28603,#28604,#28605,#28606,#28607,
#28608,#28609,#28610),.UNSPECIFIED.,.F.,.F.,(4,2,2,4),(0.000125698572975419,
0.227792182462144,0.286179225344766,0.357965061381181),.UNSPECIFIED.);
#499=B_SPLINE_CURVE_WITH_KNOTS('',3,(#28614,#28615,#28616,#28617,#28618,
#28619,#28620,#28621,#28622,#28623,#28624,#28625,#28626,#28627,#28628),
 .UNSPECIFIED.,.F.,.F.,(4,1,1,1,1,1,1,1,1,1,1,1,4),(0.,0.032581311307726,
0.0434417484103013,0.065162622615452,0.0868834968206025,0.119464808128328,
0.173766993641205,0.195487867846356,0.217208742051506,0.260650490461807,
0.304092238872109,0.34753398728241,0.350846347076693),.UNSPECIFIED.);
#500=B_SPLINE_CURVE_WITH_KNOTS('',3,(#28632,#28633,#28634,#28635,#28636,
#28637),.UNSPECIFIED.,.F.,.F.,(4,2,4),(6.30123959129944E-5,0.28662538597019,
0.558744736279564),.UNSPECIFIED.);
#501=B_SPLINE_CURVE_WITH_KNOTS('',3,(#28641,#28642,#28643,#28644,#28645,
#28646,#28647,#28648,#28649,#28650,#28651,#28652,#28653,#28654,#28655,#28656,
#28657),.UNSPECIFIED.,.F.,.F.,(4,1,1,1,1,1,1,1,1,1,1,1,1,1,4),(0.,0.0325813112990995,
0.0434417483987993,0.065162622598199,0.0868834967975986,0.108604370996998,
0.119464808096698,0.173766993595197,0.217208741993997,0.260650490392796,
0.282371364592195,0.304092238791595,0.325813112990995,0.347533987190394,
0.350818585035077),.UNSPECIFIED.);
#502=B_SPLINE_CURVE_WITH_KNOTS('',3,(#28661,#28662,#28663,#28664,#28665,
#28666),.UNSPECIFIED.,.F.,.F.,(4,2,4),(8.10097431310763E-5,0.0939376681945024,
0.135055213019345),.UNSPECIFIED.);
#503=B_SPLINE_CURVE_WITH_KNOTS('',3,(#28670,#28671,#28672,#28673,#28674,
#28675,#28676,#28677,#28678,#28679,#28680,#28681,#28682,#28683,#28684,#28685,
#28686),.UNSPECIFIED.,.F.,.F.,(4,1,1,1,1,1,1,1,1,1,1,1,2,4),(0.,0.0325813113113254,
0.0434417484151006,0.0543021855188758,0.0651626226226509,0.0868834968302012,
0.108604371037751,0.130325245245302,0.173766993660402,0.238929616283053,
0.260650490490603,0.304092238905704,0.347533987320804,0.350868951891457),
 .UNSPECIFIED.);
#504=B_SPLINE_CURVE_WITH_KNOTS('',3,(#28690,#28691,#28692,#28693,#28694,
#28695),.UNSPECIFIED.,.F.,.F.,(4,2,4),(9.94409432394449E-5,0.227746038346159,
0.389493151962301),.UNSPECIFIED.);
#505=B_SPLINE_CURVE_WITH_KNOTS('',3,(#28699,#28700,#28701,#28702,#28703,
#28704,#28705,#28706,#28707,#28708,#28709,#28710,#28711,#28712,#28713,#28714,
#28715),.UNSPECIFIED.,.F.,.F.,(4,1,1,1,1,1,1,1,1,1,1,1,1,1,4),(0.,0.0325813113011869,
0.0434417484015825,0.0651626226023737,0.0868834968031649,0.119464808104352,
0.17376699360633,0.195487867807121,0.260650490409495,0.27151092750989,0.282371364610286,
0.304092238811077,0.325813113011869,0.34753398721266,0.350822431972601),
 .UNSPECIFIED.);
#506=B_SPLINE_CURVE_WITH_KNOTS('',3,(#28719,#28720,#28721,#28722,#28723,
#28724),.UNSPECIFIED.,.F.,.F.,(4,2,4),(5.13423395914222E-5,0.227662696235558,
0.386226851134491),.UNSPECIFIED.);
#507=B_SPLINE_CURVE_WITH_KNOTS('',3,(#28728,#28729,#28730,#28731,#28732,
#28733,#28734,#28735,#28736,#28737,#28738,#28739,#28740,#28741,#28742,#28743),
 .UNSPECIFIED.,.F.,.F.,(4,1,1,1,1,1,1,1,1,1,1,1,1,4),(0.,0.0325813113000667,
0.0434417484000888,0.0651626226001333,0.0868834968001777,0.108604371000222,
0.152046119400311,0.173766993600355,0.184627430700377,0.238929616200488,
0.260650490400533,0.282371364600577,0.347533987200711,0.35081085871336),
 .UNSPECIFIED.);
#508=B_SPLINE_CURVE_WITH_KNOTS('',3,(#28747,#28748,#28749,#28750,#28751,
#28752,#28753,#28754,#28755,#28756,#28757,#28758,#28759,#28760,#28761,#28762,
#28763,#28764,#28765,#28766,#28767,#28768,#28769,#28770,#28771,#28772,#28773,
#28774,#28775,#28776,#28777,#28778,#28779,#28780,#28781,#28782,#28783),
 .UNSPECIFIED.,.F.,.F.,(4,3,3,3,3,3,3,3,3,3,3,3,4),(0.000120425573379091,
0.00317624209811181,0.034923100327543,0.0622117780158951,0.0875829757712474,
0.0998257630783663,0.112050473037524,0.149386931156097,0.162459268273195,
0.176536957109724,0.194439588055033,0.206018741387147,0.264230255678867),
 .UNSPECIFIED.);
#509=B_SPLINE_CURVE_WITH_KNOTS('',3,(#28787,#28788,#28789,#28790,#28791,
#28792,#28793,#28794,#28795,#28796,#28797,#28798,#28799,#28800,#28801,#28802,
#28803,#28804),.UNSPECIFIED.,.F.,.F.,(4,1,1,1,1,1,1,1,1,1,1,1,1,1,1,4),
(0.,0.0325751931318221,0.0434335908424294,0.0651503862636442,0.0868671816848588,
0.0977255793954661,0.108583977106074,0.119442374816681,0.173734363369718,
0.217167954212147,0.238884749633362,0.260601545054576,0.282318340475791,
0.325751931318221,0.347468726739435,0.350792906271863),.UNSPECIFIED.);
#510=B_SPLINE_CURVE_WITH_KNOTS('',3,(#28808,#28809,#28810,#28811,#28812,
#28813,#28814,#28815,#28816,#28817),.UNSPECIFIED.,.F.,.F.,(4,2,2,2,4),(2.68015753038539E-5,
0.146332244518046,0.219070648592723,0.270822325009499,0.340813208551893),
 .UNSPECIFIED.);
#511=B_SPLINE_CURVE_WITH_KNOTS('',3,(#28821,#28822,#28823,#28824,#28825,
#28826,#28827,#28828,#28829,#28830,#28831,#28832,#28833,#28834),
 .UNSPECIFIED.,.F.,.F.,(4,1,1,1,1,1,1,1,1,1,1,4),(0.,0.0325788513687624,
0.0434384684916831,0.0651577027375248,0.0868769369833663,0.119455788352129,
0.173753873966733,0.206332725335495,0.238911576704257,0.260630810950099,
0.347507747933465,0.35083610433132),.UNSPECIFIED.);
#512=B_SPLINE_CURVE_WITH_KNOTS('',3,(#28838,#28839,#28840,#28841,#28842,
#28843),.UNSPECIFIED.,.F.,.F.,(4,2,4),(4.81243928056727E-5,0.094951878313684,
0.175392450319733),.UNSPECIFIED.);
#513=B_SPLINE_CURVE_WITH_KNOTS('',3,(#28847,#28848,#28849,#28850,#28851,
#28852,#28853,#28854,#28855,#28856,#28857,#28858,#28859,#28860,#28861),
 .UNSPECIFIED.,.F.,.F.,(4,1,1,1,1,1,1,1,1,1,1,1,4),(0.,0.0325813112935661,
0.0434417483914214,0.0651626225871322,0.0868834967828429,0.108604370978554,
0.173766993565686,0.195487867761397,0.217208741957107,0.260650490348529,
0.30409223873995,0.347533987131372,0.350868951700208),.UNSPECIFIED.);
#514=B_SPLINE_CURVE_WITH_KNOTS('',3,(#28865,#28866,#28867,#28868,#28869,
#28870,#28871,#28872,#28873,#28874,#28875,#28876,#28877,#28878,#28879,#28880,
#28881,#28882,#28883,#28884,#28885,#28886,#28887,#28888,#28889,#28890,#28891,
#28892,#28893,#28894,#28895,#28896,#28897,#28898,#28899,#28900,#28901,#28902,
#28903,#28904,#28905,#28906,#28907,#28908,#28909,#28910,#28911,#28912,#28913,
#28914,#28915,#28916),.UNSPECIFIED.,.F.,.F.,(4,3,3,3,3,3,3,3,3,3,3,3,3,
3,3,3,3,4),(2.08975011247579E-5,0.00308607105095766,0.0215396517126696,
0.0405802381433016,0.0599061205553268,0.0800477842295079,0.100708814480148,
0.122385505337789,0.169065775168934,0.2240388208304,0.240016854106345,0.276817460735969,
0.299181834597421,0.36391927474236,0.406482599347405,0.447325093929158,
0.482679027142275,0.593863693098499),.UNSPECIFIED.);
#515=B_SPLINE_CURVE_WITH_KNOTS('',3,(#28920,#28921,#28922,#28923,#28924,
#28925,#28926,#28927,#28928,#28929,#28930,#28931,#28932,#28933,#28934),
 .UNSPECIFIED.,.F.,.F.,(4,1,1,1,1,1,1,1,1,1,1,1,4),(0.,0.0325813113014245,
0.0434417484018993,0.065162622602849,0.0868834968037986,0.108604371004748,
0.173766993607597,0.195487867808547,0.217208742009496,0.260650490411396,
0.304092238813295,0.347533987215194,0.350868415382151),.UNSPECIFIED.);
#516=B_SPLINE_CURVE_WITH_KNOTS('',3,(#28938,#28939,#28940,#28941,#28942,
#28943,#28944,#28945,#28946,#28947,#28948,#28949,#28950,#28951,#28952,#28953,
#28954,#28955,#28956,#28957,#28958,#28959,#28960,#28961,#28962,#28963,#28964,
#28965,#28966,#28967,#28968,#28969,#28970,#28971,#28972,#28973,#28974,#28975,
#28976,#28977),.UNSPECIFIED.,.F.,.F.,(4,3,3,3,3,3,3,3,3,3,3,3,3,4),(1.8132500310452E-5,
0.00304106400815239,0.0495323610481579,0.0633408111336385,0.0700209626369159,
0.0898911299380531,0.116220295863278,0.151110195365111,0.166467059445078,
0.17462226984871,0.194444744111124,0.224081832239665,0.235151757120569,
0.271406539154298),.UNSPECIFIED.);
#517=B_SPLINE_CURVE_WITH_KNOTS('',3,(#28981,#28982,#28983,#28984,#28985,
#28986,#28987,#28988,#28989,#28990,#28991,#28992,#28993,#28994,#28995,#28996,
#28997),.UNSPECIFIED.,.F.,.F.,(4,1,1,1,1,1,1,1,1,1,1,1,1,1,4),(0.,0.0325813113088777,
0.0434417484118369,0.0651626226177552,0.0868834968236736,0.119464808132551,
0.173766993647347,0.195487867853266,0.260650490471021,0.27151092757398,
0.282371364676939,0.304092238882858,0.325813113088776,0.347533987294695,
0.350822723223362),.UNSPECIFIED.);
#518=B_SPLINE_CURVE_WITH_KNOTS('',3,(#29001,#29002,#29003,#29004,#29005,
#29006),.UNSPECIFIED.,.F.,.F.,(4,2,4),(7.69577465685739E-5,0.0940098568691888,
0.135160714322205),.UNSPECIFIED.);
#519=B_SPLINE_CURVE_WITH_KNOTS('',3,(#29010,#29011,#29012,#29013,#29014,
#29015,#29016,#29017,#29018,#29019,#29020,#29021,#29022,#29023,#29024,#29025,
#29026,#29027),.UNSPECIFIED.,.F.,.F.,(4,1,1,1,1,1,1,1,1,1,1,1,1,1,1,4),
(0.,0.0325813113041659,0.0434417484055545,0.0651626226083318,0.086883496811109,
0.108604371013886,0.130325245216663,0.173766993622218,0.23892961623055,
0.260650490433327,0.282371364636104,0.304092238838881,0.31495267594027,
0.325813113041659,0.347533987244436,0.350814109544273),.UNSPECIFIED.);
#520=B_SPLINE_CURVE_WITH_KNOTS('',3,(#29031,#29032,#29033,#29034,#29035,
#29036,#29037,#29038),.UNSPECIFIED.,.F.,.F.,(4,2,2,4),(3.31139120221695E-5,
0.227629525449843,0.255364348773956,0.28456350304073),.UNSPECIFIED.);
#521=B_SPLINE_CURVE_WITH_KNOTS('',3,(#29042,#29043,#29044,#29045,#29046,
#29047,#29048,#29049,#29050,#29051,#29052,#29053,#29054,#29055,#29056,#29057,
#29058),.UNSPECIFIED.,.F.,.F.,(4,1,1,1,1,1,1,1,1,1,1,1,1,1,4),(0.,0.0325813112927442,
0.0434417483903256,0.0651626225854883,0.0868834967806511,0.119464808073395,
0.173766993561302,0.195487867756465,0.217208741951628,0.23892961614679,
0.249790053244372,0.260650490341953,0.304092238732279,0.347533987122604,
0.350819280994235),.UNSPECIFIED.);
#522=B_SPLINE_CURVE_WITH_KNOTS('',3,(#29062,#29063,#29064,#29065,#29066,
#29067,#29068,#29069),.UNSPECIFIED.,.F.,.F.,(4,2,2,4),(8.75783588774737E-5,
0.227723333688707,0.267086083002731,0.303951261502786),.UNSPECIFIED.);
#523=B_SPLINE_CURVE_WITH_KNOTS('',3,(#29073,#29074,#29075,#29076,#29077,
#29078,#29079,#29080,#29081,#29082,#29083,#29084,#29085,#29086,#29087),
 .UNSPECIFIED.,.F.,.F.,(4,1,1,1,1,1,1,1,1,1,1,1,4),(0.,0.0325811092953062,
0.0434414790604082,0.0651622185906124,0.0868829581208164,0.119464067416123,
0.173765916241633,0.195486655771837,0.206347025536939,0.260648874362449,
0.304090353422858,0.347531832483266,0.350844600598755),.UNSPECIFIED.);
#524=B_SPLINE_CURVE_WITH_KNOTS('',3,(#29091,#29092,#29093,#29094,#29095,
#29096,#29097,#29098),.UNSPECIFIED.,.F.,.F.,(4,2,2,4),(2.27200726371039E-5,
0.231955136446205,0.488819014410125,1.2898502229429),.UNSPECIFIED.);
#525=B_SPLINE_CURVE_WITH_KNOTS('',3,(#29102,#29103,#29104,#29105,#29106,
#29107,#29108,#29109,#29110,#29111,#29112,#29113,#29114,#29115,#29116,#29117,
#29118),.UNSPECIFIED.,.F.,.F.,(4,1,1,1,1,1,1,1,1,1,1,1,1,1,4),(0.,0.0325779980334532,
0.043437330711271,0.0651559960669065,0.0868746614225421,0.119452659455995,
0.173749322845084,0.19546798820072,0.217186653556355,0.238905318911991,
0.249764651589808,0.260623984267626,0.304061314978897,0.347498645690168,
0.350781901481053),.UNSPECIFIED.);
#526=B_SPLINE_CURVE_WITH_KNOTS('',3,(#29122,#29123,#29124,#29125,#29126,
#29127,#29128,#29129,#29130,#29131,#29132,#29133,#29134,#29135,#29136,#29137,
#29138,#29139,#29140,#29141,#29142,#29143,#29144,#29145,#29146,#29147,#29148,
#29149,#29150,#29151,#29152,#29153,#29154,#29155,#29156,#29157,#29158,#29159,
#29160,#29161,#29162,#29163,#29164,#29165,#29166,#29167,#29168,#29169,#29170),
 .UNSPECIFIED.,.F.,.F.,(4,3,3,3,3,3,3,3,3,3,3,3,3,3,3,3,4),(1.37553095906785E-6,
0.00304386864164244,0.0381582824207633,0.0424078913534377,0.0550000496558162,
0.0634874491076403,0.0677090991850859,0.0718883344512816,0.139202166901755,
0.175799272796621,0.200576190294692,0.220626076332347,0.243429823456619,
0.289644318509875,0.337908382119408,0.363805344557365,0.456456048950493),
 .UNSPECIFIED.);
#527=B_SPLINE_CURVE_WITH_KNOTS('',3,(#29174,#29175,#29176,#29177,#29178,
#29179,#29180,#29181,#29182,#29183,#29184,#29185,#29186,#29187,#29188,#29189,
#29190,#29191),.UNSPECIFIED.,.F.,.F.,(4,1,1,1,1,1,1,1,1,1,1,1,1,1,1,4),
(0.,0.0325780266754328,0.043437368900577,0.0651560533508656,0.0868747378011541,
0.108593422251443,0.130312106701731,0.173749475602308,0.217186844502885,
0.260624213403462,0.271483555628607,0.282342897853751,0.304061582304039,
0.325780266754328,0.347498951204616,0.350807062835108),.UNSPECIFIED.);
#528=B_SPLINE_CURVE_WITH_KNOTS('',3,(#29195,#29196,#29197,#29198,#29199,
#29200,#29201,#29202,#29203,#29204,#29205,#29206,#29207,#29208,#29209,#29210,
#29211,#29212,#29213,#29214,#29215,#29216,#29217,#29218,#29219,#29220,#29221,
#29222,#29223,#29224,#29225,#29226,#29227,#29228,#29229,#29230,#29231,#29232,
#29233,#29234,#29235,#29236,#29237,#29238,#29239,#29240,#29241,#29242,#29243),
 .UNSPECIFIED.,.F.,.F.,(4,3,3,3,3,3,3,3,3,3,3,3,3,3,3,3,4),(0.,0.00302406508941641,
0.0395522621603711,0.057705333245643,0.0759815108224394,0.0940426303547463,
0.112199213405293,0.148158415042036,0.184110455163659,0.202070811707743,
0.211010109764078,0.219889141985247,0.237220260655798,0.25240704224699,
0.259630849810946,0.267667276481433,0.284994839229281),.UNSPECIFIED.);
#529=B_SPLINE_CURVE_WITH_KNOTS('',3,(#29247,#29248,#29249,#29250,#29251,
#29252,#29253,#29254,#29255,#29256,#29257,#29258,#29259,#29260,#29261,#29262,
#29263,#29264),.UNSPECIFIED.,.F.,.F.,(4,1,1,1,1,1,1,1,1,1,1,1,1,1,1,4),
(0.,0.0325813113104041,0.0434417484138721,0.0651626226208082,0.0868834968277442,
0.10860437103468,0.130325245241616,0.173766993655489,0.217208742069361,
0.260650490483233,0.271510927586701,0.282371364690169,0.304092238897105,
0.325813113104041,0.347533987310977,0.350830458492577),.UNSPECIFIED.);
#530=B_SPLINE_CURVE_WITH_KNOTS('',3,(#29268,#29269,#29270,#29271,#29272,
#29273,#29274,#29275),.UNSPECIFIED.,.F.,.F.,(4,2,2,4),(5.39325034638232E-5,
0.227672425891551,0.267374517425262,0.303028644711899),.UNSPECIFIED.);
#531=B_SPLINE_CURVE_WITH_KNOTS('',3,(#29279,#29280,#29281,#29282,#29283,
#29284,#29285,#29286,#29287,#29288,#29289,#29290,#29291,#29292,#29293,#29294,
#29295,#29296,#29297,#29298,#29299),.UNSPECIFIED.,.F.,.F.,(4,1,1,1,1,1,
1,1,1,1,1,1,1,1,1,1,1,1,4),(0.,0.0217208741937073,0.0325813112905609,0.0434417483874145,
0.0651626225811218,0.086883496774829,0.0923137153232559,0.0977439338716826,
0.108604370968536,0.130325245162244,0.173766993549658,0.206348304840219,
0.217208741937072,0.23892961613078,0.260650490324487,0.282371364518194,
0.304092238711901,0.347533987099316,0.350868951667842),.UNSPECIFIED.);
#532=B_SPLINE_CURVE_WITH_KNOTS('',3,(#29303,#29304,#29305,#29306,#29307,
#29308,#29309,#29310),.UNSPECIFIED.,.F.,.F.,(4,2,2,4),(5.31032778941324E-5,
0.227671003125575,0.267370133098792,0.303019957630964),.UNSPECIFIED.);
#533=B_SPLINE_CURVE_WITH_KNOTS('',3,(#29314,#29315,#29316,#29317,#29318,
#29319,#29320,#29321,#29322,#29323,#29324,#29325,#29326,#29327,#29328,#29329,
#29330,#29331),.UNSPECIFIED.,.F.,.F.,(4,1,1,1,1,1,1,1,1,1,1,1,1,1,1,4),
(0.,0.0325813112956053,0.0434417483941404,0.0651626225912106,0.0868834967882808,
0.108604370985351,0.130325245182421,0.173766993576562,0.260650490364843,
0.304092238758983,0.306807348033617,0.309522457308251,0.314952675857518,
0.325813112956053,0.347533987153123,0.350847650043364),.UNSPECIFIED.);
#534=B_SPLINE_CURVE_WITH_KNOTS('',3,(#29335,#29336,#29337,#29338,#29339,
#29340,#29341,#29342,#29343,#29344,#29345,#29346,#29347,#29348,#29349,#29350,
#29351,#29352,#29353,#29354,#29355,#29356,#29357,#29358,#29359,#29360,#29361,
#29362,#29363,#29364,#29365,#29366,#29367,#29368,#29369,#29370,#29371,#29372,
#29373,#29374,#29375,#29376,#29377,#29378,#29379,#29380,#29381,#29382,#29383,
#29384,#29385,#29386,#29387,#29388,#29389),.UNSPECIFIED.,.F.,.F.,(4,3,3,
3,3,3,3,3,3,3,3,3,3,3,3,3,3,3,4),(1.69664194135058E-5,0.00307114277356412,
0.039585456561102,0.0486449755101495,0.0576877261582512,0.066879541498318,
0.0714617073426762,0.0759954470654279,0.0940893974202715,0.112206315525557,
0.148186601031976,0.184109848624511,0.20206634187012,0.211006462456386,
0.219884740867183,0.239823962825612,0.267679208993222,0.27814146155332,
0.312441926852791),.UNSPECIFIED.);
#535=B_SPLINE_CURVE_WITH_KNOTS('',3,(#29393,#29394,#29395,#29396,#29397,
#29398,#29399,#29400,#29401,#29402,#29403,#29404,#29405,#29406,#29407,#29408,
#29409,#29410,#29411),.UNSPECIFIED.,.F.,.F.,(4,1,1,1,1,1,1,1,1,1,1,1,1,
1,1,1,4),(0.,0.0325813112998826,0.0434417483998435,0.0651626225997652,0.0868834967996869,
0.108604370999609,0.13032524519953,0.173766993599374,0.184627430699335,
0.217208741999217,0.260650490399061,0.271510927499021,0.282371364598982,
0.304092238798904,0.325813112998826,0.347533987198747,0.350820570359218),
 .UNSPECIFIED.);
#536=B_SPLINE_CURVE_WITH_KNOTS('',3,(#29415,#29416,#29417,#29418,#29419,
#29420,#29421,#29422),.UNSPECIFIED.,.F.,.F.,(4,2,2,4),(0.,0.227561771076043,
0.271281179207273,0.310769966142806),.UNSPECIFIED.);
#537=B_SPLINE_CURVE_WITH_KNOTS('',3,(#29426,#29427,#29428,#29429,#29430,
#29431,#29432,#29433,#29434,#29435,#29436,#29437,#29438,#29439,#29440,#29441,
#29442,#29443,#29444),.UNSPECIFIED.,.F.,.F.,(4,1,1,1,1,1,1,1,1,1,1,1,1,
1,1,1,4),(0.,0.0325813112989154,0.0434417483985538,0.0651626225978307,0.0868834967971076,
0.108604370996385,0.130325245195661,0.173766993594215,0.184627430693854,
0.217208741992769,0.260650490391323,0.271510927490961,0.2823713645906,0.304092238789877,
0.325813112989153,0.34753398718843,0.350819913879885),.UNSPECIFIED.);
#538=B_SPLINE_CURVE_WITH_KNOTS('',3,(#29922,#29923,#29924,#29925,#29926,
#29927,#29928,#29929,#29930,#29931,#29932,#29933,#29934,#29935),
 .UNSPECIFIED.,.F.,.F.,(4,2,2,2,2,2,4),(0.0377143719414213,0.167070624995476,
0.336553194126115,0.499999999999991,0.663446805873868,0.832929375004528,
0.962285628058582),.UNSPECIFIED.);
#539=B_SPLINE_CURVE_WITH_KNOTS('',3,(#29937,#29938,#29939,#29940,#29941,
#29942,#29943,#29944,#29945,#29946),.UNSPECIFIED.,.F.,.F.,(4,2,2,2,4),(6.02998356774229E-5,
0.0827092794731852,0.124915109661161,0.159012423184403,0.16290738863864),
 .UNSPECIFIED.);
#540=B_SPLINE_CURVE_WITH_KNOTS('',3,(#29948,#29949,#29950,#29951,#29952,
#29953),.UNSPECIFIED.,.F.,.F.,(4,2,4),(1.00681757910309E-6,0.198376055662081,
0.616164391347873),.UNSPECIFIED.);
#541=B_SPLINE_CURVE_WITH_KNOTS('',3,(#29955,#29956,#29957,#29958,#29959,
#29960,#29961,#29962,#29963,#29964,#29965,#29966,#29967,#29968),
 .UNSPECIFIED.,.F.,.F.,(4,2,2,2,2,2,4),(-1.3697495952833,-1.10023259323731,
-0.875123171455467,-0.683367626235548,-0.492293828139748,-0.265579528785075,
-1.00032822303378E-6),.UNSPECIFIED.);
#542=B_SPLINE_CURVE_WITH_KNOTS('',3,(#29970,#29971,#29972,#29973,#29974,
#29975),.UNSPECIFIED.,.F.,.F.,(4,2,4),(2.07957879669281E-5,0.198544173877694,
0.338081838894613),.UNSPECIFIED.);
#543=B_SPLINE_CURVE_WITH_KNOTS('',3,(#29976,#29977,#29978,#29979,#29980,
#29981),.UNSPECIFIED.,.F.,.F.,(4,2,4),(7.3985770635887E-13,0.0834659910448719,
0.124630945443496),.UNSPECIFIED.);
#544=B_SPLINE_CURVE_WITH_KNOTS('',3,(#30038,#30039,#30040,#30041,#30042,
#30043,#30044,#30045,#30046,#30047,#30048,#30049,#30050,#30051),
 .UNSPECIFIED.,.F.,.F.,(4,2,2,2,2,2,4),(0.0377143719414213,0.167070624995476,
0.336553194126115,0.499999999999991,0.663446805873868,0.832929375004528,
0.962285628058582),.UNSPECIFIED.);
#545=B_SPLINE_CURVE_WITH_KNOTS('',3,(#30571,#30572,#30573,#30574,#30575,
#30576),.UNSPECIFIED.,.F.,.F.,(4,2,4),(2.29474227301907E-5,0.0820321645242487,
0.127086402594844),.UNSPECIFIED.);
#546=B_SPLINE_CURVE_WITH_KNOTS('',3,(#30578,#30579,#30580,#30581,#30582,
#30583,#30584,#30585,#30586,#30587),.UNSPECIFIED.,.F.,.F.,(4,2,2,2,4),(1.0015711071698E-6,
0.191278795792421,0.38757373555012,0.491221092732434,0.551410070798975),
 .UNSPECIFIED.);
#547=B_SPLINE_CURVE_WITH_KNOTS('',3,(#30589,#30590,#30591,#30592,#30593,
#30594,#30595,#30596,#30597,#30598,#30599,#30600,#30601,#30602),
 .UNSPECIFIED.,.F.,.F.,(4,2,2,2,2,2,4),(-1.35492578021256,-1.08827021184037,
-0.865791397536503,-0.676241847501408,-0.487357773086443,-0.263174151541431,
-1.00020091572966E-6),.UNSPECIFIED.);
#548=B_SPLINE_CURVE_WITH_KNOTS('',3,(#30604,#30605,#30606,#30607,#30608,
#30609),.UNSPECIFIED.,.F.,.F.,(4,2,4),(0.000114833391804824,0.165073300431955,
0.25614615827788),.UNSPECIFIED.);
#549=B_SPLINE_CURVE_WITH_KNOTS('',3,(#30610,#30611,#30612,#30613,#30614,
#30615),.UNSPECIFIED.,.F.,.F.,(4,2,4),(2.21353696645175E-12,0.0812321189495927,
0.187083951430582),.UNSPECIFIED.);
#550=B_SPLINE_CURVE_WITH_KNOTS('',3,(#30619,#30620,#30621,#30622,#30623,
#30624),.UNSPECIFIED.,.F.,.F.,(4,2,4),(2.9238385461313E-5,0.103447066749674,
0.163628142816379),.UNSPECIFIED.);
#551=B_SPLINE_CURVE_WITH_KNOTS('',3,(#30628,#30629,#30630,#30631,#30632,
#30633,#30634,#30635),.UNSPECIFIED.,.F.,.F.,(4,2,2,4),(1.0058637232954E-6,
0.195653995077043,0.273235261095345,0.534959287266804),.UNSPECIFIED.);
#552=B_SPLINE_CURVE_WITH_KNOTS('',3,(#30639,#30640,#30641,#30642,#30643,
#30644,#30645,#30646,#30647,#30648,#30649,#30650,#30651,#30652),
 .UNSPECIFIED.,.F.,.F.,(4,2,2,2,2,2,4),(-1.36676454451703,-1.09824091081614,
-0.873519748019839,-0.682131120567347,-0.491400640516798,-0.264972088549723,
-1.00035032482767E-6),.UNSPECIFIED.);
#553=B_SPLINE_CURVE_WITH_KNOTS('',3,(#30656,#30657,#30658,#30659,#30660,
#30661),.UNSPECIFIED.,.F.,.F.,(4,2,4),(0.000130181004474716,0.209368508323579,
0.347593165933443),.UNSPECIFIED.);
#554=B_SPLINE_CURVE_WITH_KNOTS('',3,(#30663,#30664,#30665,#30666,#30667,
#30668),.UNSPECIFIED.,.F.,.F.,(4,2,4),(4.22281107869509E-12,0.0949552245569479,
0.178548392329359),.UNSPECIFIED.);
#555=B_SPLINE_CURVE_WITH_KNOTS('',3,(#31173,#31174,#31175,#31176,#31177,
#31178,#31179,#31180,#31181,#31182,#31183,#31184,#31185,#31186),
 .UNSPECIFIED.,.F.,.F.,(4,2,2,2,2,2,4),(0.0377143719414213,0.167070624995476,
0.336553194126115,0.499999999999991,0.663446805873868,0.832929375004528,
0.962285628058582),.UNSPECIFIED.);
#556=B_SPLINE_CURVE_WITH_KNOTS('',3,(#31188,#31189,#31190,#31191,#31192,
#31193,#31194,#31195,#31196,#31197),.UNSPECIFIED.,.F.,.F.,(4,2,2,2,4),(6.27818039135639E-5,
0.082188319328403,0.124361031846954,0.160510990515046,0.165279378877141),
 .UNSPECIFIED.);
#557=B_SPLINE_CURVE_WITH_KNOTS('',3,(#31199,#31200,#31201,#31202,#31203,
#31204,#31205,#31206,#31207,#31208),.UNSPECIFIED.,.F.,.F.,(4,2,2,2,4),(1.00120787235036E-6,
0.178106589831891,0.361003049087605,0.458246244320469,0.518090207569899),
 .UNSPECIFIED.);
#558=B_SPLINE_CURVE_WITH_KNOTS('',3,(#31210,#31211,#31212,#31213,#31214,
#31215,#31216,#31217,#31218,#31219,#31220,#31221,#31222,#31223),
 .UNSPECIFIED.,.F.,.F.,(4,2,2,2,2,2,4),(-1.35451776762616,-1.08791731812649,
-0.865511022534625,-0.676038029847498,-0.48722621698279,-0.263105347394021,
-1.00024492573328E-6),.UNSPECIFIED.);
#559=B_SPLINE_CURVE_WITH_KNOTS('',3,(#31225,#31226,#31227,#31228,#31229,
#31230),.UNSPECIFIED.,.F.,.F.,(4,2,4),(5.14867016416543E-5,0.195132654327356,
0.330523874257241),.UNSPECIFIED.);
#560=B_SPLINE_CURVE_WITH_KNOTS('',3,(#31231,#31232,#31233,#31234,#31235,
#31236),.UNSPECIFIED.,.F.,.F.,(4,2,4),(2.74483044490136E-12,0.0801886121002409,
0.134391643166566),.UNSPECIFIED.);
#561=B_SPLINE_CURVE_WITH_KNOTS('',3,(#31293,#31294,#31295,#31296,#31297,
#31298,#31299,#31300,#31301,#31302,#31303,#31304,#31305,#31306),
 .UNSPECIFIED.,.F.,.F.,(4,2,2,2,2,2,4),(0.0377143719414213,0.167070624995476,
0.336553194126115,0.499999999999991,0.663446805873868,0.832929375004528,
0.962285628058582),.UNSPECIFIED.);
#562=B_SPLINE_CURVE_WITH_KNOTS('',3,(#31882,#31883,#31884,#31885,#31886,
#31887),.UNSPECIFIED.,.F.,.F.,(4,2,4),(3.83144405905161E-5,0.0820775777658897,
0.163588942869382),.UNSPECIFIED.);
#563=B_SPLINE_CURVE_WITH_KNOTS('',3,(#31889,#31890,#31891,#31892,#31893,
#31894,#31895,#31896,#31897,#31898),.UNSPECIFIED.,.F.,.F.,(4,2,2,2,4),(1.00111834067745E-6,
0.176745823297941,0.356256554433591,0.450695302353019,0.510467153062589),
 .UNSPECIFIED.);
#564=B_SPLINE_CURVE_WITH_KNOTS('',3,(#31900,#31901,#31902,#31903,#31904,
#31905,#31906,#31907,#31908,#31909,#31910,#31911,#31912,#31913),
 .UNSPECIFIED.,.F.,.F.,(4,2,2,2,2,2,4),(-1.35467512487212,-1.08805555198913,
-0.865672785184554,-0.676085696250677,-0.487155925003567,-0.26302937099976,
-1.00022677660484E-6),.UNSPECIFIED.);
#565=B_SPLINE_CURVE_WITH_KNOTS('',3,(#31915,#31916,#31917,#31918,#31919,
#31920),.UNSPECIFIED.,.F.,.F.,(4,2,4),(7.5428832328408E-5,0.105663039185365,
0.180626596448931),.UNSPECIFIED.);
#566=B_SPLINE_CURVE_WITH_KNOTS('',3,(#31921,#31922,#31923,#31924,#31925,
#31926,#31927,#31928,#31929,#31930),.UNSPECIFIED.,.F.,.F.,(4,2,2,2,4),(0.,
0.0810373126568711,0.0959717664713932,0.101312246402759,0.103448648415402),
 .UNSPECIFIED.);
#567=B_SPLINE_CURVE_WITH_KNOTS('',3,(#32458,#32459,#32460,#32461,#32462,
#32463,#32464,#32465,#32466,#32467,#32468,#32469,#32470,#32471),
 .UNSPECIFIED.,.F.,.F.,(4,2,2,2,2,2,4),(0.0377143719414213,0.167070624995476,
0.336553194126115,0.499999999999991,0.663446805873868,0.832929375004528,
0.962285628058582),.UNSPECIFIED.);
#568=B_SPLINE_CURVE_WITH_KNOTS('',3,(#32473,#32474,#32475,#32476,#32477,
#32478,#32479,#32480,#32481,#32482),.UNSPECIFIED.,.F.,.F.,(4,2,2,2,4),(6.00642358182352E-5,
0.0821817544261252,0.124362812830404,0.160530644634858,0.165303570917889),
 .UNSPECIFIED.);
#569=B_SPLINE_CURVE_WITH_KNOTS('',3,(#32484,#32485,#32486,#32487,#32488,
#32489,#32490,#32491,#32492,#32493),.UNSPECIFIED.,.F.,.F.,(4,2,2,2,4),(1.0012084904056E-6,
0.178254736450577,0.361162889837382,0.457988221849768,0.519343329924884),
 .UNSPECIFIED.);
#570=B_SPLINE_CURVE_WITH_KNOTS('',3,(#32495,#32496,#32497,#32498,#32499,
#32500,#32501,#32502,#32503,#32504,#32505,#32506,#32507,#32508),
 .UNSPECIFIED.,.F.,.F.,(4,2,2,2,2,2,4),(-1.35452989588837,-1.08792747113547,
-0.865519548823138,-0.676043361721358,-0.487228090638011,-0.263104534485106,
-1.00024503859763E-6),.UNSPECIFIED.);
#571=B_SPLINE_CURVE_WITH_KNOTS('',3,(#32510,#32511,#32512,#32513,#32514,
#32515),.UNSPECIFIED.,.F.,.F.,(4,2,4),(4.84470832014495E-5,0.182163199855647,
0.304984269132144),.UNSPECIFIED.);
#572=B_SPLINE_CURVE_WITH_KNOTS('',3,(#32516,#32517,#32518,#32519,#32520,
#32521),.UNSPECIFIED.,.F.,.F.,(4,2,4),(3.76146522406052E-12,0.0801875735797784,
0.135807623237589),.UNSPECIFIED.);
#573=B_SPLINE_CURVE_WITH_KNOTS('',3,(#32578,#32579,#32580,#32581,#32582,
#32583,#32584,#32585,#32586,#32587,#32588,#32589,#32590,#32591),
 .UNSPECIFIED.,.F.,.F.,(4,2,2,2,2,2,4),(0.0377143719414213,0.167070624995476,
0.336553194126115,0.499999999999991,0.663446805873868,0.832929375004528,
0.962285628058582),.UNSPECIFIED.);
#574=B_SPLINE_CURVE_WITH_KNOTS('',3,(#33251,#33252,#33253,#33254,#33255,
#33256),.UNSPECIFIED.,.F.,.F.,(4,2,4),(5.09831611999352E-6,0.0820253557161963,
0.163612440508287),.UNSPECIFIED.);
#575=B_SPLINE_CURVE_WITH_KNOTS('',3,(#33258,#33259,#33260,#33261,#33262,
#33263),.UNSPECIFIED.,.F.,.F.,(4,2,4),(1.00115786546793E-6,0.203270398076333,
0.655123139928109),.UNSPECIFIED.);
#576=B_SPLINE_CURVE_WITH_KNOTS('',3,(#33265,#33266,#33267,#33268,#33269,
#33270,#33271,#33272,#33273,#33274,#33275,#33276,#33277,#33278),
 .UNSPECIFIED.,.F.,.F.,(4,2,2,2,2,2,4),(-1.35341451706435,-1.08670028936229,
-0.86441625397775,-0.675525209241787,-0.487228648686942,-0.263116926873662,
-1.00023452885085E-6),.UNSPECIFIED.);
#577=B_SPLINE_CURVE_WITH_KNOTS('',3,(#33280,#33281,#33282,#33283,#33284,
#33285),.UNSPECIFIED.,.F.,.F.,(4,2,4),(8.06566033118487E-5,0.235791800547026,
0.430083034163372),.UNSPECIFIED.);
#578=B_SPLINE_CURVE_WITH_KNOTS('',3,(#33286,#33287,#33288,#33289,#33290,
#33291,#33292,#33293,#33294,#33295),.UNSPECIFIED.,.F.,.F.,(4,2,2,2,4),(0.,
0.0811226560809443,0.105916017129699,0.119512712641936,0.124075141076686),
 .UNSPECIFIED.);
#579=B_SPLINE_CURVE_WITH_KNOTS('',3,(#33865,#33866,#33867,#33868,#33869,
#33870,#33871,#33872,#33873,#33874,#33875,#33876,#33877,#33878),
 .UNSPECIFIED.,.F.,.F.,(4,2,2,2,2,2,4),(0.0377143719414213,0.167070624995476,
0.336553194126115,0.499999999999991,0.663446805873868,0.832929375004528,
0.962285628058582),.UNSPECIFIED.);
#580=B_SPLINE_CURVE_WITH_KNOTS('',3,(#33880,#33881,#33882,#33883,#33884,
#33885,#33886,#33887),.UNSPECIFIED.,.F.,.F.,(4,2,2,4),(3.90292133962738E-5,
0.0821103706390817,0.159792128481933,0.163589006475625),.UNSPECIFIED.);
#581=B_SPLINE_CURVE_WITH_KNOTS('',3,(#33889,#33890,#33891,#33892,#33893,
#33894),.UNSPECIFIED.,.F.,.F.,(4,2,4),(1.00679590137882E-6,0.198428655308229,
0.616220686425556),.UNSPECIFIED.);
#582=B_SPLINE_CURVE_WITH_KNOTS('',3,(#33896,#33897,#33898,#33899,#33900,
#33901,#33902,#33903,#33904,#33905,#33906,#33907,#33908,#33909),
 .UNSPECIFIED.,.F.,.F.,(4,2,2,2,2,2,4),(-1.36946436726572,-1.09993796007104,
-0.87483524085704,-0.683080422126019,-0.492004958736434,-0.265277755647832,
-1.00032716612113E-6),.UNSPECIFIED.);
#583=B_SPLINE_CURVE_WITH_KNOTS('',3,(#33911,#33912,#33913,#33914,#33915,
#33916),.UNSPECIFIED.,.F.,.F.,(4,2,4),(5.26674620364727E-6,0.201391218966152,
0.343250429838191),.UNSPECIFIED.);
#584=B_SPLINE_CURVE_WITH_KNOTS('',3,(#33917,#33918,#33919,#33920,#33921,
#33922),.UNSPECIFIED.,.F.,.F.,(4,2,4),(5.79777279590719E-12,0.0800737732076016,
0.153868907149876),.UNSPECIFIED.);
#585=B_SPLINE_CURVE_WITH_KNOTS('',3,(#33979,#33980,#33981,#33982,#33983,
#33984,#33985,#33986,#33987,#33988,#33989,#33990,#33991,#33992),
 .UNSPECIFIED.,.F.,.F.,(4,2,2,2,2,2,4),(0.0377143719414213,0.167070624995476,
0.336553194126115,0.499999999999991,0.663446805873868,0.832929375004528,
0.962285628058582),.UNSPECIFIED.);
#586=B_SPLINE_CURVE_WITH_KNOTS('',3,(#34442,#34443,#34444,#34445,#34446,
#34447,#34448,#34449),.UNSPECIFIED.,.F.,.F.,(4,2,2,4),(6.73894020493833E-6,
0.0820391933763412,0.122258941274579,0.165103583903822),.UNSPECIFIED.);
#587=B_SPLINE_CURVE_WITH_KNOTS('',3,(#34451,#34452,#34453,#34454,#34455,
#34456),.UNSPECIFIED.,.F.,.F.,(4,2,4),(1.00575280131252E-6,0.196998295881173,
0.611676358684534),.UNSPECIFIED.);
#588=B_SPLINE_CURVE_WITH_KNOTS('',3,(#34458,#34459,#34460,#34461,#34462,
#34463,#34464,#34465,#34466,#34467,#34468,#34469,#34470,#34471),
 .UNSPECIFIED.,.F.,.F.,(4,2,2,2,2,2,4),(-1.36653537100014,-1.09810186112548,
-0.873434408555324,-0.682043594538526,-0.49131851038635,-0.264945371797465,
-1.00034356989698E-6),.UNSPECIFIED.);
#589=B_SPLINE_CURVE_WITH_KNOTS('',3,(#34473,#34474,#34475,#34476,#34477,
#34478),.UNSPECIFIED.,.F.,.F.,(4,2,4),(8.77479325007996E-5,0.221380284319995,
0.382793527514749),.UNSPECIFIED.);
#590=B_SPLINE_CURVE_WITH_KNOTS('',3,(#34479,#34480,#34481,#34482,#34483,
#34484,#34485,#34486),.UNSPECIFIED.,.F.,.F.,(4,2,2,4),(2.39130355285181E-13,
0.0351374765588485,0.0713576360411048,0.114209460841156),.UNSPECIFIED.);
#591=B_SPLINE_CURVE_WITH_KNOTS('',3,(#35154,#35155,#35156,#35157,#35158,
#35159,#35160,#35161,#35162,#35163,#35164,#35165,#35166,#35167),
 .UNSPECIFIED.,.F.,.F.,(4,2,2,2,2,2,4),(0.0377143719414213,0.167070624995476,
0.336553194126115,0.499999999999991,0.663446805873868,0.832929375004528,
0.962285628058582),.UNSPECIFIED.);
#592=B_SPLINE_CURVE_WITH_KNOTS('',3,(#35169,#35170,#35171,#35172,#35173,
#35174),.UNSPECIFIED.,.F.,.F.,(4,2,4),(1.24525365641064E-5,0.0820262168893432,
0.163512197605749),.UNSPECIFIED.);
#593=B_SPLINE_CURVE_WITH_KNOTS('',3,(#35176,#35177,#35178,#35179,#35180,
#35181),.UNSPECIFIED.,.F.,.F.,(4,2,4),(1.00040793070525E-6,0.173262947876778,
0.559558397335178),.UNSPECIFIED.);
#594=B_SPLINE_CURVE_WITH_KNOTS('',3,(#35183,#35184,#35185,#35186,#35187,
#35188,#35189,#35190,#35191,#35192,#35193,#35194,#35195,#35196),
 .UNSPECIFIED.,.F.,.F.,(4,2,2,2,2,2,4),(-1.35063028345454,-1.08468537305046,
-0.862939535319615,-0.674245622212526,-0.486174128017263,-0.262647316233601,
-1.00009146822194E-6),.UNSPECIFIED.);
#595=B_SPLINE_CURVE_WITH_KNOTS('',3,(#35198,#35199,#35200,#35201,#35202,
#35203),.UNSPECIFIED.,.F.,.F.,(4,2,4),(1.936890280024E-5,0.202772428402345,
0.388563110243199),.UNSPECIFIED.);
#596=B_SPLINE_CURVE_WITH_KNOTS('',3,(#35204,#35205,#35206,#35207,#35208,
#35209,#35210,#35211),.UNSPECIFIED.,.F.,.F.,(4,2,2,4),(0.,0.00386300464665212,
0.0800231995509174,0.130453162506101),.UNSPECIFIED.);
#597=B_SPLINE_CURVE_WITH_KNOTS('',3,(#35268,#35269,#35270,#35271,#35272,
#35273,#35274,#35275,#35276,#35277,#35278,#35279,#35280,#35281),
 .UNSPECIFIED.,.F.,.F.,(4,2,2,2,2,2,4),(0.0377143719414213,0.167070624995476,
0.336553194126115,0.499999999999991,0.663446805873868,0.832929375004528,
0.962285628058582),.UNSPECIFIED.);
#598=B_SPLINE_CURVE_WITH_KNOTS('',3,(#35731,#35732,#35733,#35734,#35735,
#35736,#35737,#35738),.UNSPECIFIED.,.F.,.F.,(4,2,2,4),(6.90400899849116E-6,
0.0820395128145215,0.122259153116005,0.165101582267905),.UNSPECIFIED.);
#599=B_SPLINE_CURVE_WITH_KNOTS('',3,(#35740,#35741,#35742,#35743,#35744,
#35745),.UNSPECIFIED.,.F.,.F.,(4,2,4),(1.00575513369814E-6,0.196994699755262,
0.611609770297254),.UNSPECIFIED.);
#600=B_SPLINE_CURVE_WITH_KNOTS('',3,(#35747,#35748,#35749,#35750,#35751,
#35752,#35753,#35754,#35755,#35756,#35757,#35758,#35759,#35760),
 .UNSPECIFIED.,.F.,.F.,(4,2,2,2,2,2,4),(-1.36653731681659,-1.09810214381664,
-0.873434196730641,-0.682044304096007,-0.49132017893128,-0.264946970986512,
-1.00034369628633E-6),.UNSPECIFIED.);
#601=B_SPLINE_CURVE_WITH_KNOTS('',3,(#35762,#35763,#35764,#35765,#35766,
#35767),.UNSPECIFIED.,.F.,.F.,(4,2,4),(8.89329850189062E-5,0.221868589758904,
0.38383585754025),.UNSPECIFIED.);
#602=B_SPLINE_CURVE_WITH_KNOTS('',3,(#35768,#35769,#35770,#35771,#35772,
#35773,#35774,#35775),.UNSPECIFIED.,.F.,.F.,(4,2,2,4),(2.40826726029524E-12,
0.0351391314154969,0.0713608565247239,0.114146477814614),.UNSPECIFIED.);
#603=B_SPLINE_CURVE_WITH_KNOTS('',3,(#36261,#36262,#36263,#36264,#36265,
#36266,#36267,#36268,#36269,#36270,#36271,#36272,#36273,#36274),
 .UNSPECIFIED.,.F.,.F.,(4,2,2,2,2,2,4),(0.0377143719414213,0.167070624995476,
0.336553194126115,0.499999999999991,0.663446805873868,0.832929375004528,
0.962285628058582),.UNSPECIFIED.);
#604=B_SPLINE_CURVE_WITH_KNOTS('',3,(#36276,#36277,#36278,#36279,#36280,
#36281,#36282,#36283,#36284,#36285,#36286,#36287),.UNSPECIFIED.,.F.,.F.,
(4,2,2,2,2,4),(6.06953724766298E-5,0.0723177934624636,0.142586707446175,
0.189383971247134,0.229663834041465,0.234960972274723),.UNSPECIFIED.);
#605=B_SPLINE_CURVE_WITH_KNOTS('',3,(#36289,#36290,#36291,#36292,#36293,
#36294),.UNSPECIFIED.,.F.,.F.,(4,2,4),(1.00681844603221E-6,0.198376306856705,
0.616167083390173),.UNSPECIFIED.);
#606=B_SPLINE_CURVE_WITH_KNOTS('',3,(#36296,#36297,#36298,#36299,#36300,
#36301,#36302,#36303,#36304,#36305,#36306,#36307,#36308,#36309),
 .UNSPECIFIED.,.F.,.F.,(4,2,2,2,2,2,4),(-1.36975063911396,-1.10023328664463,
-0.875123658513123,-0.683368107151748,-0.492294313860235,-0.26558001556176,
-1.0003282794275E-6),.UNSPECIFIED.);
#607=B_SPLINE_CURVE_WITH_KNOTS('',3,(#36311,#36312,#36313,#36314,#36315,
#36316),.UNSPECIFIED.,.F.,.F.,(4,2,4),(2.03029926476926E-5,0.199101046105406,
0.339123960645439),.UNSPECIFIED.);
#608=B_SPLINE_CURVE_WITH_KNOTS('',3,(#36317,#36318,#36319,#36320,#36321,
#36322),.UNSPECIFIED.,.F.,.F.,(4,2,4),(0.,0.0801741784244009,0.133244087202315),
 .UNSPECIFIED.);
#609=B_SPLINE_CURVE_WITH_KNOTS('',3,(#36379,#36380,#36381,#36382,#36383,
#36384,#36385,#36386,#36387,#36388,#36389,#36390,#36391,#36392),
 .UNSPECIFIED.,.F.,.F.,(4,2,2,2,2,2,4),(0.0377143719414213,0.167070624995476,
0.336553194126115,0.499999999999991,0.663446805873868,0.832929375004528,
0.962285628058582),.UNSPECIFIED.);
#610=B_SPLINE_CURVE_WITH_KNOTS('',3,(#37010,#37011,#37012,#37013,#37014,
#37015,#37016,#37017),.UNSPECIFIED.,.F.,.F.,(4,2,2,4),(2.12328689868991E-5,
0.0820465025813729,0.0975804088568552,0.0980854119622017),.UNSPECIFIED.);
#611=B_SPLINE_CURVE_WITH_KNOTS('',3,(#37019,#37020,#37021,#37022,#37023,
#37024,#37025,#37026,#37027,#37028),.UNSPECIFIED.,.F.,.F.,(4,2,2,2,4),(1.00120754304711E-6,
0.180563424164471,0.364157287903267,0.442097033926019,0.497873685697995),
 .UNSPECIFIED.);
#612=B_SPLINE_CURVE_WITH_KNOTS('',3,(#37030,#37031,#37032,#37033,#37034,
#37035,#37036,#37037,#37038,#37039,#37040,#37041,#37042,#37043),
 .UNSPECIFIED.,.F.,.F.,(4,2,2,2,2,2,4),(-1.35482880152986,-1.08819875332802,
-0.865789686987352,-0.676162724939522,-0.487193738484184,-0.263042222431825,
-1.00024482310964E-6),.UNSPECIFIED.);
#613=B_SPLINE_CURVE_WITH_KNOTS('',3,(#37045,#37046,#37047,#37048,#37049,
#37050),.UNSPECIFIED.,.F.,.F.,(4,2,4),(4.92544827602823E-5,0.177705442380597,
0.325738385748943),.UNSPECIFIED.);
#614=B_SPLINE_CURVE_WITH_KNOTS('',3,(#37051,#37052,#37053,#37054,#37055,
#37056,#37057,#37058),.UNSPECIFIED.,.F.,.F.,(4,2,2,4),(0.,0.00483273455720385,
0.0810988666945897,0.131043136461057),.UNSPECIFIED.);
#615=B_SPLINE_CURVE_WITH_KNOTS('',3,(#37530,#37531,#37532,#37533,#37534,
#37535,#37536,#37537,#37538,#37539,#37540,#37541,#37542,#37543),
 .UNSPECIFIED.,.F.,.F.,(4,2,2,2,2,2,4),(0.0377143719414213,0.167070624995476,
0.336553194126115,0.499999999999991,0.663446805873868,0.832929375004528,
0.962285628058582),.UNSPECIFIED.);
#616=B_SPLINE_CURVE_WITH_KNOTS('',3,(#37545,#37546,#37547,#37548,#37549,
#37550,#37551,#37552),.UNSPECIFIED.,.F.,.F.,(4,2,2,4),(5.42376165162044E-5,
0.0821643460301592,0.213267550478571,0.227565828155254),.UNSPECIFIED.);
#617=B_SPLINE_CURVE_WITH_KNOTS('',3,(#37554,#37555,#37556,#37557,#37558,
#37559),.UNSPECIFIED.,.F.,.F.,(4,2,4),(1.00681606646651E-6,0.198408681306464,
0.616468624198531),.UNSPECIFIED.);
#618=B_SPLINE_CURVE_WITH_KNOTS('',3,(#37561,#37562,#37563,#37564,#37565,
#37566,#37567,#37568,#37569,#37570,#37571,#37572,#37573,#37574),
 .UNSPECIFIED.,.F.,.F.,(4,2,2,2,2,2,4),(-1.36977192354957,-1.10024954678324,
-0.875138273537566,-0.68337946038512,-0.492301827559948,-0.265581063709854,
-1.00032816558492E-6),.UNSPECIFIED.);
#619=B_SPLINE_CURVE_WITH_KNOTS('',3,(#37576,#37577,#37578,#37579,#37580,
#37581),.UNSPECIFIED.,.F.,.F.,(4,2,4),(5.21624935227409E-6,0.197869989680169,
0.3367373897978),.UNSPECIFIED.);
#620=B_SPLINE_CURVE_WITH_KNOTS('',3,(#37582,#37583,#37584,#37585,#37586,
#37587),.UNSPECIFIED.,.F.,.F.,(4,2,4),(1.02764932528255E-12,0.0801413076023557,
0.194331925601292),.UNSPECIFIED.);
#621=B_SPLINE_CURVE_WITH_KNOTS('',3,(#37644,#37645,#37646,#37647,#37648,
#37649,#37650,#37651,#37652,#37653,#37654,#37655,#37656,#37657),
 .UNSPECIFIED.,.F.,.F.,(4,2,2,2,2,2,4),(0.0377143719414213,0.167070624995476,
0.336553194126115,0.499999999999991,0.663446805873868,0.832929375004528,
0.962285628058582),.UNSPECIFIED.);
#622=B_SPLINE_CURVE_WITH_KNOTS('',3,(#38121,#38122,#38123,#38124,#38125,
#38126),.UNSPECIFIED.,.F.,.F.,(4,2,4),(1.3375296468513E-5,0.118849802950364,
0.770735236720951),.UNSPECIFIED.);
#623=B_SPLINE_CURVE_WITH_KNOTS('',3,(#38128,#38129,#38130,#38131,#38132,
#38133),.UNSPECIFIED.,.F.,.F.,(4,2,4),(1.00583908498562E-6,0.197083724989951,
0.612585872513722),.UNSPECIFIED.);
#624=B_SPLINE_CURVE_WITH_KNOTS('',3,(#38135,#38136,#38137,#38138,#38139,
#38140,#38141,#38142,#38143,#38144,#38145,#38146,#38147,#38148),
 .UNSPECIFIED.,.F.,.F.,(4,2,2,2,2,2,4),(-1.36677954016887,-1.09825974558988,
-0.873545667521562,-0.682153185342683,-0.491418884621818,-0.264981806425049,
-1.00034871381864E-6),.UNSPECIFIED.);
#625=B_SPLINE_CURVE_WITH_KNOTS('',3,(#38150,#38151,#38152,#38153,#38154,
#38155),.UNSPECIFIED.,.F.,.F.,(4,2,4),(2.0131697178417E-5,0.188528940513233,
0.322027145962636),.UNSPECIFIED.);
#626=B_SPLINE_CURVE_WITH_KNOTS('',3,(#38156,#38157,#38158,#38159,#38160,
#38161),.UNSPECIFIED.,.F.,.F.,(4,2,4),(5.18698018589852E-13,0.0829527696225184,
0.126881817845898),.UNSPECIFIED.);
#627=B_SPLINE_CURVE_WITH_KNOTS('',3,(#38577,#38578,#38579,#38580,#38581,
#38582,#38583,#38584,#38585,#38586,#38587,#38588,#38589,#38590),
 .UNSPECIFIED.,.F.,.F.,(4,2,2,2,2,2,4),(0.0377143719414213,0.167070624995476,
0.336553194126115,0.499999999999991,0.663446805873868,0.832929375004528,
0.962285628058582),.UNSPECIFIED.);
#628=B_SPLINE_CURVE_WITH_KNOTS('',3,(#38592,#38593,#38594,#38595,#38596,
#38597),.UNSPECIFIED.,.F.,.F.,(4,2,4),(3.25283738680958E-5,0.0575600610182617,
0.119710480217137),.UNSPECIFIED.);
#629=B_SPLINE_CURVE_WITH_KNOTS('',3,(#38599,#38600,#38601,#38602,#38603,
#38604),.UNSPECIFIED.,.F.,.F.,(4,2,4),(1.00574980111111E-6,0.196438860777099,
0.615936660954388),.UNSPECIFIED.);
#630=B_SPLINE_CURVE_WITH_KNOTS('',3,(#38606,#38607,#38608,#38609,#38610,
#38611,#38612,#38613,#38614,#38615,#38616,#38617,#38618,#38619),
 .UNSPECIFIED.,.F.,.F.,(4,2,2,2,2,2,4),(-1.36646497173156,-1.09803036534575,
-0.873371570921259,-0.682007908066334,-0.491310112387284,-0.264951815991902,
-1.00034338197123E-6),.UNSPECIFIED.);
#631=B_SPLINE_CURVE_WITH_KNOTS('',3,(#38621,#38622,#38623,#38624,#38625,
#38626),.UNSPECIFIED.,.F.,.F.,(4,2,4),(8.95077426275264E-5,0.213418487477568,
0.347676401385313),.UNSPECIFIED.);
#632=B_SPLINE_CURVE_WITH_KNOTS('',3,(#38627,#38628,#38629,#38630,#38631,
#38632),.UNSPECIFIED.,.F.,.F.,(4,2,4),(5.71589455049436E-13,0.0829410743851074,
0.160131049736526),.UNSPECIFIED.);
#633=B_SPLINE_CURVE_WITH_KNOTS('',3,(#38689,#38690,#38691,#38692,#38693,
#38694,#38695,#38696,#38697,#38698,#38699,#38700,#38701,#38702),
 .UNSPECIFIED.,.F.,.F.,(4,2,2,2,2,2,4),(0.0377143719414213,0.167070624995476,
0.336553194126115,0.499999999999991,0.663446805873868,0.832929375004528,
0.962285628058582),.UNSPECIFIED.);
#634=B_SPLINE_CURVE_WITH_KNOTS('',3,(#39194,#39195,#39196,#39197,#39198,
#39199,#39200,#39201),.UNSPECIFIED.,.F.,.F.,(4,2,2,4),(5.63653703654061E-6,
0.0819976592555741,0.0994840943119498,0.110621668417563),.UNSPECIFIED.);
#635=B_SPLINE_CURVE_WITH_KNOTS('',3,(#39203,#39204,#39205,#39206,#39207,
#39208),.UNSPECIFIED.,.F.,.F.,(4,2,4),(1.00578674459647E-6,0.196744693440733,
0.608070001195422),.UNSPECIFIED.);
#636=B_SPLINE_CURVE_WITH_KNOTS('',3,(#39210,#39211,#39212,#39213,#39214,
#39215,#39216,#39217,#39218,#39219,#39220,#39221,#39222,#39223),
 .UNSPECIFIED.,.F.,.F.,(4,2,2,2,2,2,4),(-1.36654018190171,-1.09811194514787,
-0.873433001188821,-0.682044964262726,-0.491323861095133,-0.264952627419438,
-1.00034558310118E-6),.UNSPECIFIED.);
#637=B_SPLINE_CURVE_WITH_KNOTS('',3,(#39225,#39226,#39227,#39228,#39229,
#39230),.UNSPECIFIED.,.F.,.F.,(4,2,4),(7.36982883605742E-6,0.21182056227566,
0.362967551660399),.UNSPECIFIED.);
#638=B_SPLINE_CURVE_WITH_KNOTS('',3,(#39231,#39232,#39233,#39234,#39235,
#39236,#39237,#39238),.UNSPECIFIED.,.F.,.F.,(4,2,2,4),(3.36762946852576E-12,
0.0811207756408513,0.121444988164551,0.192000399014979),.UNSPECIFIED.);
#639=B_SPLINE_CURVE_WITH_KNOTS('',3,(#39752,#39753,#39754,#39755,#39756,
#39757,#39758,#39759,#39760,#39761,#39762,#39763,#39764,#39765),
 .UNSPECIFIED.,.F.,.F.,(4,2,2,2,2,2,4),(0.0377143719414213,0.167070624995476,
0.336553194126115,0.499999999999991,0.663446805873868,0.832929375004528,
0.962285628058582),.UNSPECIFIED.);
#640=B_SPLINE_CURVE_WITH_KNOTS('',3,(#39767,#39768,#39769,#39770,#39771,
#39772,#39773,#39774),.UNSPECIFIED.,.F.,.F.,(4,2,2,4),(6.08478568690021E-5,
0.0749500177471191,0.137874692765321,0.214092945323678),.UNSPECIFIED.);
#641=B_SPLINE_CURVE_WITH_KNOTS('',3,(#39776,#39777,#39778,#39779,#39780,
#39781),.UNSPECIFIED.,.F.,.F.,(4,2,4),(1.00674948340903E-6,0.19860241559806,
0.616969018247203),.UNSPECIFIED.);
#642=B_SPLINE_CURVE_WITH_KNOTS('',3,(#39783,#39784,#39785,#39786,#39787,
#39788,#39789,#39790,#39791,#39792,#39793,#39794,#39795,#39796),
 .UNSPECIFIED.,.F.,.F.,(4,2,2,2,2,2,4),(-1.36942885849635,-1.09990630423119,
-0.874813906835148,-0.683066677551954,-0.491998067801788,-0.265271812378102,
-1.00032494267263E-6),.UNSPECIFIED.);
#643=B_SPLINE_CURVE_WITH_KNOTS('',3,(#39798,#39799,#39800,#39801,#39802,
#39803),.UNSPECIFIED.,.F.,.F.,(4,2,4),(2.26430690219157E-5,0.201402499858342,
0.343296266574079),.UNSPECIFIED.);
#644=B_SPLINE_CURVE_WITH_KNOTS('',3,(#39804,#39805,#39806,#39807,#39808,
#39809,#39810,#39811),.UNSPECIFIED.,.F.,.F.,(4,2,2,4),(1.74684428518018E-12,
0.0522340767156272,0.136645058339451,0.231738878590132),.UNSPECIFIED.);
#645=B_SPLINE_CURVE_WITH_KNOTS('',3,(#39868,#39869,#39870,#39871,#39872,
#39873,#39874,#39875,#39876,#39877,#39878,#39879,#39880,#39881),
 .UNSPECIFIED.,.F.,.F.,(4,2,2,2,2,2,4),(0.0377143719414213,0.167070624995476,
0.336553194126115,0.499999999999991,0.663446805873868,0.832929375004528,
0.962285628058582),.UNSPECIFIED.);
#646=B_SPLINE_CURVE_WITH_KNOTS('',3,(#40443,#40444,#40445,#40446,#40447,
#40448),.UNSPECIFIED.,.F.,.F.,(4,2,4),(3.99306793426499E-5,0.0820843888608893,
0.163582789889144),.UNSPECIFIED.);
#647=B_SPLINE_CURVE_WITH_KNOTS('',3,(#40450,#40451,#40452,#40453,#40454,
#40455,#40456,#40457,#40458,#40459),.UNSPECIFIED.,.F.,.F.,(4,2,2,2,4),(1.001144715258E-6,
0.176544129782838,0.356948476219595,0.452196137824933,0.511488742402409),
 .UNSPECIFIED.);
#648=B_SPLINE_CURVE_WITH_KNOTS('',3,(#40461,#40462,#40463,#40464,#40465,
#40466,#40467,#40468,#40469,#40470,#40471,#40472,#40473,#40474),
 .UNSPECIFIED.,.F.,.F.,(4,2,2,2,2,2,4),(-1.35478963372027,-1.08811184962075,
-0.865669720728692,-0.676143977124964,-0.487271283253805,-0.263087029256964,
-1.00023212990909E-6),.UNSPECIFIED.);
#649=B_SPLINE_CURVE_WITH_KNOTS('',3,(#40476,#40477,#40478,#40479,#40480,
#40481),.UNSPECIFIED.,.F.,.F.,(4,2,4),(6.51111114373825E-5,0.197951050690941,
0.363934107919122),.UNSPECIFIED.);
#650=B_SPLINE_CURVE_WITH_KNOTS('',3,(#40482,#40483,#40484,#40485,#40486,
#40487),.UNSPECIFIED.,.F.,.F.,(4,2,4),(0.,0.0810433266429397,0.145890417857538),
 .UNSPECIFIED.);
#651=B_SPLINE_CURVE_WITH_KNOTS('',3,(#40903,#40904,#40905,#40906,#40907,
#40908,#40909,#40910,#40911,#40912,#40913,#40914,#40915,#40916),
 .UNSPECIFIED.,.F.,.F.,(4,2,2,2,2,2,4),(0.0377143719414213,0.167070624995476,
0.336553194126115,0.499999999999991,0.663446805873868,0.832929375004528,
0.962285628058582),.UNSPECIFIED.);
#652=B_SPLINE_CURVE_WITH_KNOTS('',3,(#40918,#40919,#40920,#40921,#40922,
#40923),.UNSPECIFIED.,.F.,.F.,(4,2,4),(3.20283895616613E-5,0.0586306467901465,
0.121642806585947),.UNSPECIFIED.);
#653=B_SPLINE_CURVE_WITH_KNOTS('',3,(#40925,#40926,#40927,#40928,#40929,
#40930),.UNSPECIFIED.,.F.,.F.,(4,2,4),(1.00574695584138E-6,0.196441563595188,
0.616027525838472),.UNSPECIFIED.);
#654=B_SPLINE_CURVE_WITH_KNOTS('',3,(#40932,#40933,#40934,#40935,#40936,
#40937,#40938,#40939,#40940,#40941,#40942,#40943,#40944,#40945),
 .UNSPECIFIED.,.F.,.F.,(4,2,2,2,2,2,4),(-1.36646292126098,-1.09803107097949,
-0.873372841577203,-0.682007267078294,-0.491307511055257,-0.264949168082375,
-1.00034321282837E-6),.UNSPECIFIED.);
#655=B_SPLINE_CURVE_WITH_KNOTS('',3,(#40947,#40948,#40949,#40950,#40951,
#40952),.UNSPECIFIED.,.F.,.F.,(4,2,4),(8.66234192869361E-5,0.213329487663992,
0.347531973651816),.UNSPECIFIED.);
#656=B_SPLINE_CURVE_WITH_KNOTS('',3,(#40953,#40954,#40955,#40956,#40957,
#40958),.UNSPECIFIED.,.F.,.F.,(4,2,4),(8.38585718100273E-13,0.0801874437919323,
0.160125031278999),.UNSPECIFIED.);
#657=B_SPLINE_CURVE_WITH_KNOTS('',3,(#41015,#41016,#41017,#41018,#41019,
#41020,#41021,#41022,#41023,#41024,#41025,#41026,#41027,#41028),
 .UNSPECIFIED.,.F.,.F.,(4,2,2,2,2,2,4),(0.0377143719414213,0.167070624995476,
0.336553194126115,0.499999999999991,0.663446805873868,0.832929375004528,
0.962285628058582),.UNSPECIFIED.);
#658=B_SPLINE_CURVE_WITH_KNOTS('',3,(#41548,#41549,#41550,#41551,#41552,
#41553),.UNSPECIFIED.,.F.,.F.,(4,2,4),(5.78796480941106E-6,0.0820241632572779,
0.0983326513668803),.UNSPECIFIED.);
#659=B_SPLINE_CURVE_WITH_KNOTS('',3,(#41555,#41556,#41557,#41558,#41559,
#41560),.UNSPECIFIED.,.F.,.F.,(4,2,4),(1.00111011279019E-6,0.20056691109568,
0.646408027829995),.UNSPECIFIED.);
#660=B_SPLINE_CURVE_WITH_KNOTS('',3,(#41562,#41563,#41564,#41565,#41566,
#41567,#41568,#41569,#41570,#41571,#41572,#41573,#41574,#41575),
 .UNSPECIFIED.,.F.,.F.,(4,2,2,2,2,2,4),(-1.35329688927434,-1.08662400245728,
-0.864362407604642,-0.675470253341474,-0.487172784036078,-0.263083584774088,
-1.0002248669823E-6),.UNSPECIFIED.);
#661=B_SPLINE_CURVE_WITH_KNOTS('',3,(#41577,#41578,#41579,#41580,#41581,
#41582),.UNSPECIFIED.,.F.,.F.,(4,2,4),(7.6238807513628E-5,0.428958911085021,
0.98234564450394),.UNSPECIFIED.);
#662=B_SPLINE_CURVE_WITH_KNOTS('',3,(#41583,#41584,#41585,#41586,#41587,
#41588),.UNSPECIFIED.,.F.,.F.,(4,2,4),(2.36314343156334E-13,0.0811159727681617,
0.112753130003149),.UNSPECIFIED.);
#663=B_SPLINE_CURVE_WITH_KNOTS('',3,(#42018,#42019,#42020,#42021,#42022,
#42023,#42024,#42025,#42026,#42027,#42028,#42029,#42030,#42031),
 .UNSPECIFIED.,.F.,.F.,(4,2,2,2,2,2,4),(0.0377143719414213,0.167070624995476,
0.336553194126115,0.499999999999991,0.663446805873868,0.832929375004528,
0.962285628058582),.UNSPECIFIED.);
#664=B_SPLINE_CURVE_WITH_KNOTS('',3,(#42033,#42034,#42035,#42036,#42037,
#42038),.UNSPECIFIED.,.F.,.F.,(4,2,4),(3.17996200538999E-5,0.0821085150301028,
0.156371486023489),.UNSPECIFIED.);
#665=B_SPLINE_CURVE_WITH_KNOTS('',3,(#42040,#42041,#42042,#42043,#42044,
#42045),.UNSPECIFIED.,.F.,.F.,(4,2,4),(1.00587720305493E-6,0.195537009167673,
0.606860770741171),.UNSPECIFIED.);
#666=B_SPLINE_CURVE_WITH_KNOTS('',3,(#42047,#42048,#42049,#42050,#42051,
#42052,#42053,#42054,#42055,#42056,#42057,#42058,#42059,#42060),
 .UNSPECIFIED.,.F.,.F.,(4,2,2,2,2,2,4),(-1.36641479922188,-1.09801466418853,
-0.87334685635933,-0.681977540546231,-0.491275627793233,-0.264940661371275,
-1.00035098939736E-6),.UNSPECIFIED.);
#667=B_SPLINE_CURVE_WITH_KNOTS('',3,(#42062,#42063,#42064,#42065,#42066,
#42067),.UNSPECIFIED.,.F.,.F.,(4,2,4),(8.49732544616001E-5,0.171599040272099,
0.274221646995865),.UNSPECIFIED.);
#668=B_SPLINE_CURVE_WITH_KNOTS('',3,(#42068,#42069,#42070,#42071,#42072,
#42073),.UNSPECIFIED.,.F.,.F.,(4,2,4),(0.,0.0802786247734464,0.181190612654646),
 .UNSPECIFIED.);
#669=B_SPLINE_CURVE_WITH_KNOTS('',3,(#42130,#42131,#42132,#42133,#42134,
#42135,#42136,#42137,#42138,#42139,#42140,#42141,#42142,#42143),
 .UNSPECIFIED.,.F.,.F.,(4,2,2,2,2,2,4),(0.0377143719414213,0.167070624995476,
0.336553194126115,0.499999999999991,0.663446805873868,0.832929375004528,
0.962285628058582),.UNSPECIFIED.);
#670=B_SPLINE_CURVE_WITH_KNOTS('',3,(#42509,#42510,#42511,#42512,#42513,
#42514),.UNSPECIFIED.,.F.,.F.,(4,2,4),(2.77418896662162E-5,0.0821040997741305,
0.185637111823654),.UNSPECIFIED.);
#671=B_SPLINE_CURVE_WITH_KNOTS('',3,(#42516,#42517,#42518,#42519,#42520,
#42521),.UNSPECIFIED.,.F.,.F.,(4,2,4),(1.00575954346815E-6,0.196733751213732,
0.608207148250796),.UNSPECIFIED.);
#672=B_SPLINE_CURVE_WITH_KNOTS('',3,(#42523,#42524,#42525,#42526,#42527,
#42528,#42529,#42530,#42531,#42532,#42533,#42534,#42535,#42536),
 .UNSPECIFIED.,.F.,.F.,(4,2,2,2,2,2,4),(-1.36645102810747,-1.09803162874758,
-0.873371647969155,-0.681999637833079,-0.491294686089601,-0.264941085845053,
-1.00034395944326E-6),.UNSPECIFIED.);
#673=B_SPLINE_CURVE_WITH_KNOTS('',3,(#42538,#42539,#42540,#42541,#42542,
#42543),.UNSPECIFIED.,.F.,.F.,(4,2,4),(4.6534746752922E-5,0.221801216668018,
0.383393535508176),.UNSPECIFIED.);
#674=B_SPLINE_CURVE_WITH_KNOTS('',3,(#42544,#42545,#42546,#42547,#42548,
#42549),.UNSPECIFIED.,.F.,.F.,(4,2,4),(9.75142074189076E-12,0.0812508942657999,
0.181132066940532),.UNSPECIFIED.);
#675=B_SPLINE_CURVE_WITH_KNOTS('',3,(#42979,#42980,#42981,#42982,#42983,
#42984,#42985,#42986,#42987,#42988,#42989,#42990,#42991,#42992),
 .UNSPECIFIED.,.F.,.F.,(4,2,2,2,2,2,4),(0.0377143719414213,0.167070624995476,
0.336553194126115,0.499999999999991,0.663446805873868,0.832929375004528,
0.962285628058582),.UNSPECIFIED.);
#676=B_SPLINE_CURVE_WITH_KNOTS('',3,(#42994,#42995,#42996,#42997,#42998,
#42999,#43000,#43001,#43002,#43003),.UNSPECIFIED.,.F.,.F.,(4,2,2,2,4),(5.42770356477153E-5,
0.082170276446433,0.124430513201584,0.160833130319759,0.165642154100829),
 .UNSPECIFIED.);
#677=B_SPLINE_CURVE_WITH_KNOTS('',3,(#43005,#43006,#43007,#43008,#43009,
#43010),.UNSPECIFIED.,.F.,.F.,(4,2,4),(1.00682002279841E-6,0.198152813321902,
0.615513442370215),.UNSPECIFIED.);
#678=B_SPLINE_CURVE_WITH_KNOTS('',3,(#43012,#43013,#43014,#43015,#43016,
#43017,#43018,#43019,#43020,#43021,#43022,#43023,#43024,#43025),
 .UNSPECIFIED.,.F.,.F.,(4,2,2,2,2,2,4),(-1.36965848181598,-1.10016097342675,
-0.875066628972613,-0.683316003615392,-0.492247655326726,-0.265550093286376,
-1.00032835407965E-6),.UNSPECIFIED.);
#679=B_SPLINE_CURVE_WITH_KNOTS('',3,(#43027,#43028,#43029,#43030,#43031,
#43032),.UNSPECIFIED.,.F.,.F.,(4,2,4),(2.80984943197878E-5,0.207705089179129,
0.35709509524869),.UNSPECIFIED.);
#680=B_SPLINE_CURVE_WITH_KNOTS('',3,(#43033,#43034,#43035,#43036,#43037,
#43038),.UNSPECIFIED.,.F.,.F.,(4,2,4),(2.92897079760619E-13,0.0802239228803233,
0.139498602952362),.UNSPECIFIED.);
#681=B_SPLINE_CURVE_WITH_KNOTS('',3,(#43095,#43096,#43097,#43098,#43099,
#43100,#43101,#43102,#43103,#43104,#43105,#43106,#43107,#43108),
 .UNSPECIFIED.,.F.,.F.,(4,2,2,2,2,2,4),(0.0377143719414213,0.167070624995476,
0.336553194126115,0.499999999999991,0.663446805873868,0.832929375004528,
0.962285628058582),.UNSPECIFIED.);
#682=B_SPLINE_CURVE_WITH_KNOTS('',3,(#43544,#43545,#43546,#43547,#43548,
#43549),.UNSPECIFIED.,.F.,.F.,(4,2,4),(3.61744708263467E-5,0.0820903485190886,
0.151462981409793),.UNSPECIFIED.);
#683=B_SPLINE_CURVE_WITH_KNOTS('',3,(#43551,#43552,#43553,#43554,#43555,
#43556),.UNSPECIFIED.,.F.,.F.,(4,2,4),(1.00682037581877E-6,0.198591576030872,
0.612057308716193),.UNSPECIFIED.);
#684=B_SPLINE_CURVE_WITH_KNOTS('',3,(#43558,#43559,#43560,#43561,#43562,
#43563,#43564,#43565,#43566,#43567,#43568,#43569,#43570,#43571),
 .UNSPECIFIED.,.F.,.F.,(4,2,2,2,2,2,4),(-1.36969550267109,-1.10017893246134,
-0.875088347365155,-0.683338633894847,-0.492266819638581,-0.265550398905338,
-1.00032836821468E-6),.UNSPECIFIED.);
#685=B_SPLINE_CURVE_WITH_KNOTS('',3,(#43573,#43574,#43575,#43576,#43577,
#43578),.UNSPECIFIED.,.F.,.F.,(4,2,4),(3.32639783591171E-5,0.197339009355241,
0.335420963807672),.UNSPECIFIED.);
#686=B_SPLINE_CURVE_WITH_KNOTS('',3,(#43579,#43580,#43581,#43582,#43583,
#43584),.UNSPECIFIED.,.F.,.F.,(4,2,4),(3.15044624714952E-12,0.0812340423540164,
0.130576380927272),.UNSPECIFIED.);
#687=B_SPLINE_CURVE_WITH_KNOTS('',3,(#44028,#44029,#44030,#44031,#44032,
#44033,#44034,#44035,#44036,#44037,#44038,#44039,#44040,#44041),
 .UNSPECIFIED.,.F.,.F.,(4,2,2,2,2,2,4),(0.0377143719414213,0.167070624995476,
0.336553194126115,0.499999999999991,0.663446805873868,0.832929375004528,
0.962285628058582),.UNSPECIFIED.);
#688=B_SPLINE_CURVE_WITH_KNOTS('',3,(#44043,#44044,#44045,#44046,#44047,
#44048,#44049,#44050),.UNSPECIFIED.,.F.,.F.,(4,2,2,4),(7.66815118875742E-6,
0.0719725088285606,0.133933240585685,0.207132823723994),.UNSPECIFIED.);
#689=B_SPLINE_CURVE_WITH_KNOTS('',3,(#44052,#44053,#44054,#44055,#44056,
#44057),.UNSPECIFIED.,.F.,.F.,(4,2,4),(1.00645408089785E-6,0.202058735386919,
0.625169506815927),.UNSPECIFIED.);
#690=B_SPLINE_CURVE_WITH_KNOTS('',3,(#44059,#44060,#44061,#44062,#44063,
#44064,#44065,#44066,#44067,#44068,#44069,#44070,#44071,#44072),
 .UNSPECIFIED.,.F.,.F.,(4,2,2,2,2,2,4),(-1.36982770647676,-1.10026801869593,
-0.875089073772716,-0.683242477348657,-0.492101062955115,-0.265280784052238,
-1.00031248059293E-6),.UNSPECIFIED.);
#691=B_SPLINE_CURVE_WITH_KNOTS('',3,(#44074,#44075,#44076,#44077,#44078,
#44079),.UNSPECIFIED.,.F.,.F.,(4,2,4),(7.21374248179772E-5,0.145937889148844,
0.224935975704918),.UNSPECIFIED.);
#692=B_SPLINE_CURVE_WITH_KNOTS('',3,(#44080,#44081,#44082,#44083,#44084,
#44085,#44086,#44087),.UNSPECIFIED.,.F.,.F.,(4,2,2,4),(0.,0.00388201731530571,
0.0800806715946951,0.130377783514938),.UNSPECIFIED.);
#693=B_SPLINE_CURVE_WITH_KNOTS('',3,(#44144,#44145,#44146,#44147,#44148,
#44149,#44150,#44151,#44152,#44153,#44154,#44155,#44156,#44157),
 .UNSPECIFIED.,.F.,.F.,(4,2,2,2,2,2,4),(0.0377143719414213,0.167070624995476,
0.336553194126115,0.499999999999991,0.663446805873868,0.832929375004528,
0.962285628058582),.UNSPECIFIED.);
#694=B_SPLINE_CURVE_WITH_KNOTS('',3,(#44649,#44650,#44651,#44652,#44653,
#44654),.UNSPECIFIED.,.F.,.F.,(4,2,4),(2.46231051897258E-5,0.0821382968673538,
0.159729243346244),.UNSPECIFIED.);
#695=B_SPLINE_CURVE_WITH_KNOTS('',3,(#44656,#44657,#44658,#44659,#44660,
#44661),.UNSPECIFIED.,.F.,.F.,(4,2,4),(1.00103827732456E-6,0.198279414012427,
0.639031973469237),.UNSPECIFIED.);
#696=B_SPLINE_CURVE_WITH_KNOTS('',3,(#44663,#44664,#44665,#44666,#44667,
#44668,#44669,#44670,#44671,#44672,#44673,#44674,#44675,#44676),
 .UNSPECIFIED.,.F.,.F.,(4,2,2,2,2,2,4),(-1.3530882309929,-1.08643200781697,
-0.864215538893404,-0.67536646667284,-0.487108134126014,-0.263052051794661,
-1.00022350183771E-6),.UNSPECIFIED.);
#697=B_SPLINE_CURVE_WITH_KNOTS('',3,(#44678,#44679,#44680,#44681,#44682,
#44683),.UNSPECIFIED.,.F.,.F.,(4,2,4),(7.89412222038307E-5,0.167932169494167,
0.297563614930367),.UNSPECIFIED.);
#698=B_SPLINE_CURVE_WITH_KNOTS('',3,(#44684,#44685,#44686,#44687,#44688,
#44689),.UNSPECIFIED.,.F.,.F.,(4,2,4),(3.26720990769784E-12,0.110549333290049,
0.163767498068542),.UNSPECIFIED.);
#699=B_SPLINE_CURVE_WITH_KNOTS('',3,(#45091,#45092,#45093,#45094,#45095,
#45096,#45097,#45098,#45099,#45100,#45101,#45102,#45103,#45104),
 .UNSPECIFIED.,.F.,.F.,(4,2,2,2,2,2,4),(0.0377143719414213,0.167070624995476,
0.336553194126115,0.499999999999991,0.663446805873868,0.832929375004528,
0.962285628058582),.UNSPECIFIED.);
#700=B_SPLINE_CURVE_WITH_KNOTS('',3,(#45106,#45107,#45108,#45109,#45110,
#45111),.UNSPECIFIED.,.F.,.F.,(4,2,4),(6.726102877353E-5,0.116989061547652,
0.697184527165448),.UNSPECIFIED.);
#701=B_SPLINE_CURVE_WITH_KNOTS('',3,(#45113,#45114,#45115,#45116,#45117,
#45118),.UNSPECIFIED.,.F.,.F.,(4,2,4),(1.00666090718109E-6,0.198552744294137,
0.618327596429947),.UNSPECIFIED.);
#702=B_SPLINE_CURVE_WITH_KNOTS('',3,(#45120,#45121,#45122,#45123,#45124,
#45125,#45126,#45127,#45128,#45129,#45130,#45131,#45132,#45133),
 .UNSPECIFIED.,.F.,.F.,(4,2,2,2,2,2,4),(-1.36853366463682,-1.09981790730256,
-0.874751340081577,-0.683009325808431,-0.491945339785637,-0.26523823904143,
-1.00032068147704E-6),.UNSPECIFIED.);
#703=B_SPLINE_CURVE_WITH_KNOTS('',3,(#45135,#45136,#45137,#45138,#45139,
#45140),.UNSPECIFIED.,.F.,.F.,(4,2,4),(3.71680310896038E-5,0.188969719403689,
0.318357862923346),.UNSPECIFIED.);
#704=B_SPLINE_CURVE_WITH_KNOTS('',3,(#45141,#45142,#45143,#45144,#45145,
#45146,#45147,#45148),.UNSPECIFIED.,.F.,.F.,(4,2,2,4),(0.,0.00387868763366687,
0.0800762215668998,0.137711267059276),.UNSPECIFIED.);
#705=B_SPLINE_CURVE_WITH_KNOTS('',3,(#45205,#45206,#45207,#45208,#45209,
#45210,#45211,#45212,#45213,#45214,#45215,#45216,#45217,#45218),
 .UNSPECIFIED.,.F.,.F.,(4,2,2,2,2,2,4),(0.0377143719414213,0.167070624995476,
0.336553194126115,0.499999999999991,0.663446805873868,0.832929375004528,
0.962285628058582),.UNSPECIFIED.);
#706=B_SPLINE_CURVE_WITH_KNOTS('',3,(#45584,#45585,#45586,#45587,#45588,
#45589,#45590,#45591),.UNSPECIFIED.,.F.,.F.,(4,2,2,4),(3.86068946090691E-5,
0.0477481584382911,0.113775363683532,0.296176984369277),.UNSPECIFIED.);
#707=B_SPLINE_CURVE_WITH_KNOTS('',3,(#45593,#45594,#45595,#45596,#45597,
#45598,#45599,#45600,#45601,#45602),.UNSPECIFIED.,.F.,.F.,(4,2,2,2,4),(1.00675013885361E-6,
0.198280154256163,0.401801682357639,0.519968319797222,0.606410947309042),
 .UNSPECIFIED.);
#708=B_SPLINE_CURVE_WITH_KNOTS('',3,(#45604,#45605,#45606,#45607,#45608,
#45609,#45610,#45611,#45612,#45613,#45614,#45615,#45616,#45617),
 .UNSPECIFIED.,.F.,.F.,(4,2,2,2,2,2,4),(-1.36923063553463,-1.09976128371409,
-0.874703857588768,-0.68297060694838,-0.49191596635355,-0.265236424101605,
-1.00032497786205E-6),.UNSPECIFIED.);
#709=B_SPLINE_CURVE_WITH_KNOTS('',3,(#45619,#45620,#45621,#45622,#45623,
#45624),.UNSPECIFIED.,.F.,.F.,(4,2,4),(5.24545898662702E-5,0.182499654277947,
0.288993661227474),.UNSPECIFIED.);
#710=B_SPLINE_CURVE_WITH_KNOTS('',3,(#45625,#45626,#45627,#45628,#45629,
#45630,#45631,#45632),.UNSPECIFIED.,.F.,.F.,(4,2,2,4),(1.58568685059277E-13,
0.035377553448089,0.0719723147421016,0.13036658253743),.UNSPECIFIED.);
#711=B_SPLINE_CURVE_WITH_KNOTS('',3,(#46006,#46007,#46008,#46009,#46010,
#46011,#46012,#46013,#46014,#46015,#46016,#46017,#46018,#46019),
 .UNSPECIFIED.,.F.,.F.,(4,2,2,2,2,2,4),(0.0377143719414213,0.167070624995476,
0.336553194126115,0.499999999999991,0.663446805873868,0.832929375004528,
0.962285628058582),.UNSPECIFIED.);
#712=B_SPLINE_CURVE_WITH_KNOTS('',3,(#46021,#46022,#46023,#46024,#46025,
#46026,#46027,#46028),.UNSPECIFIED.,.F.,.F.,(4,2,2,4),(3.69697143127623E-5,
0.053751719227584,0.103579138587863,0.175747470358817),.UNSPECIFIED.);
#713=B_SPLINE_CURVE_WITH_KNOTS('',3,(#46030,#46031,#46032,#46033,#46034,
#46035),.UNSPECIFIED.,.F.,.F.,(4,2,4),(1.0067260897438E-6,0.198302453808835,
0.617617266278844),.UNSPECIFIED.);
#714=B_SPLINE_CURVE_WITH_KNOTS('',3,(#46037,#46038,#46039,#46040,#46041,
#46042,#46043,#46044,#46045,#46046,#46047,#46048,#46049,#46050),
 .UNSPECIFIED.,.F.,.F.,(4,2,2,2,2,2,4),(-1.36856131602685,-1.09983747446031,
-0.874764567364842,-0.683019106044176,-0.491951477912598,-0.265243600779506,
-1.00032381763926E-6),.UNSPECIFIED.);
#715=B_SPLINE_CURVE_WITH_KNOTS('',3,(#46052,#46053,#46054,#46055,#46056,
#46057),.UNSPECIFIED.,.F.,.F.,(4,2,4),(1.01102908296581E-5,0.229050332432197,
0.401317557299931),.UNSPECIFIED.);
#716=B_SPLINE_CURVE_WITH_KNOTS('',3,(#46058,#46059,#46060,#46061,#46062,
#46063),.UNSPECIFIED.,.F.,.F.,(4,2,4),(4.00958579207454E-13,0.0448362547412082,
0.0753294109411124),.UNSPECIFIED.);
#717=B_SPLINE_CURVE_WITH_KNOTS('',3,(#46120,#46121,#46122,#46123,#46124,
#46125,#46126,#46127,#46128,#46129,#46130,#46131,#46132,#46133),
 .UNSPECIFIED.,.F.,.F.,(4,2,2,2,2,2,4),(0.0377143719414213,0.167070624995476,
0.336553194126115,0.499999999999991,0.663446805873868,0.832929375004528,
0.962285628058582),.UNSPECIFIED.);
#718=B_SPLINE_CURVE_WITH_KNOTS('',3,(#46513,#46514,#46515,#46516,#46517,
#46518),.UNSPECIFIED.,.F.,.F.,(4,2,4),(4.34887184794296E-5,0.103480982422226,
0.149574548200566),.UNSPECIFIED.);
#719=B_SPLINE_CURVE_WITH_KNOTS('',3,(#46520,#46521,#46522,#46523,#46524,
#46525,#46526,#46527,#46528,#46529),.UNSPECIFIED.,.F.,.F.,(4,2,2,2,4),(1.00143118243601E-6,
0.180608739286493,0.368729050760223,0.465285214132863,0.552599028244089),
 .UNSPECIFIED.);
#720=B_SPLINE_CURVE_WITH_KNOTS('',3,(#46531,#46532,#46533,#46534,#46535,
#46536,#46537,#46538,#46539,#46540,#46541,#46542,#46543,#46544),
 .UNSPECIFIED.,.F.,.F.,(4,2,2,2,2,2,4),(-1.35524591239,-1.08845925117483,
-0.865940013333757,-0.676355299140697,-0.487422236949836,-0.263156882106951,
-1.00018709657936E-6),.UNSPECIFIED.);
#721=B_SPLINE_CURVE_WITH_KNOTS('',3,(#46546,#46547,#46548,#46549,#46550,
#46551),.UNSPECIFIED.,.F.,.F.,(4,2,4),(2.96547197040926E-5,0.217520565424474,
0.410447896098608),.UNSPECIFIED.);
#722=B_SPLINE_CURVE_WITH_KNOTS('',3,(#46552,#46553,#46554,#46555,#46556,
#46557),.UNSPECIFIED.,.F.,.F.,(4,2,4),(4.22886337875709E-12,0.0851568103986181,
0.190922300311632),.UNSPECIFIED.);
#723=B_SPLINE_CURVE_WITH_KNOTS('',3,(#47001,#47002,#47003,#47004,#47005,
#47006,#47007,#47008,#47009,#47010,#47011,#47012,#47013,#47014),
 .UNSPECIFIED.,.F.,.F.,(4,2,2,2,2,2,4),(0.0377143719414213,0.167070624995476,
0.336553194126115,0.499999999999991,0.663446805873868,0.832929375004528,
0.962285628058582),.UNSPECIFIED.);
#724=B_SPLINE_CURVE_WITH_KNOTS('',3,(#47016,#47017,#47018,#47019,#47020,
#47021),.UNSPECIFIED.,.F.,.F.,(4,2,4),(2.21311227024518E-5,0.059746661158349,
0.130829664938975),.UNSPECIFIED.);
#725=B_SPLINE_CURVE_WITH_KNOTS('',3,(#47023,#47024,#47025,#47026,#47027,
#47028),.UNSPECIFIED.,.F.,.F.,(4,2,4),(1.00115827109886E-6,0.204260590716849,
0.65966839194673),.UNSPECIFIED.);
#726=B_SPLINE_CURVE_WITH_KNOTS('',3,(#47030,#47031,#47032,#47033,#47034,
#47035,#47036,#47037,#47038,#47039,#47040,#47041,#47042,#47043),
 .UNSPECIFIED.,.F.,.F.,(4,2,2,2,2,2,4),(-1.35292348708793,-1.08632729712736,
-0.864134156802677,-0.675300660556552,-0.487063391819361,-0.263053608006327,
-1.00023460417283E-6),.UNSPECIFIED.);
#727=B_SPLINE_CURVE_WITH_KNOTS('',3,(#47045,#47046,#47047,#47048,#47049,
#47050),.UNSPECIFIED.,.F.,.F.,(4,2,4),(0.000113907795243102,0.308169653858189,
0.697441169951114),.UNSPECIFIED.);
#728=B_SPLINE_CURVE_WITH_KNOTS('',3,(#47051,#47052,#47053,#47054,#47055,
#47056,#47057,#47058),.UNSPECIFIED.,.F.,.F.,(4,2,2,4),(8.12439686031872E-13,
0.0801092010493702,0.132357556624391,0.174836143722638),.UNSPECIFIED.);
#729=B_SPLINE_CURVE_WITH_KNOTS('',3,(#47115,#47116,#47117,#47118,#47119,
#47120,#47121,#47122,#47123,#47124,#47125,#47126,#47127,#47128),
 .UNSPECIFIED.,.F.,.F.,(4,2,2,2,2,2,4),(0.0377143719414213,0.167070624995476,
0.336553194126115,0.499999999999991,0.663446805873868,0.832929375004528,
0.962285628058582),.UNSPECIFIED.);
#730=B_SPLINE_CURVE_WITH_KNOTS('',3,(#47536,#47537,#47538,#47539,#47540,
#47541),.UNSPECIFIED.,.F.,.F.,(4,2,4),(6.85948530913353E-5,0.117689713160168,
0.701425347858688),.UNSPECIFIED.);
#731=B_SPLINE_CURVE_WITH_KNOTS('',3,(#47543,#47544,#47545,#47546,#47547,
#47548,#47549,#47550,#47551,#47552),.UNSPECIFIED.,.F.,.F.,(4,2,2,2,4),(1.00112175382184E-6,
0.175138486721777,0.354266046028186,0.450458287458295,0.512798132480794),
 .UNSPECIFIED.);
#732=B_SPLINE_CURVE_WITH_KNOTS('',3,(#47554,#47555,#47556,#47557,#47558,
#47559,#47560,#47561,#47562,#47563,#47564,#47565,#47566,#47567),
 .UNSPECIFIED.,.F.,.F.,(4,2,2,2,2,2,4),(-1.35460666568921,-1.08802411036352,
-0.865653674945032,-0.67605696728004,-0.487118571463883,-0.263006191372635,
-1.00022748703302E-6),.UNSPECIFIED.);
#733=B_SPLINE_CURVE_WITH_KNOTS('',3,(#47569,#47570,#47571,#47572,#47573,
#47574),.UNSPECIFIED.,.F.,.F.,(4,2,4),(2.20616210062517E-5,0.193313035420533,
0.359805614049465),.UNSPECIFIED.);
#734=B_SPLINE_CURVE_WITH_KNOTS('',3,(#47575,#47576,#47577,#47578,#47579,
#47580,#47581,#47582),.UNSPECIFIED.,.F.,.F.,(4,2,2,4),(0.,0.00481423729226705,
0.0811672210679098,0.136469477695337),.UNSPECIFIED.);
#735=B_SPLINE_CURVE_WITH_KNOTS('',3,(#47886,#47887,#47888,#47889,#47890,
#47891,#47892,#47893,#47894,#47895,#47896,#47897,#47898,#47899),
 .UNSPECIFIED.,.F.,.F.,(4,2,2,2,2,2,4),(0.0377143719414213,0.167070624995476,
0.336553194126115,0.499999999999991,0.663446805873868,0.832929375004528,
0.962285628058582),.UNSPECIFIED.);
#736=B_SPLINE_CURVE_WITH_KNOTS('',3,(#47901,#47902,#47903,#47904,#47905,
#47906),.UNSPECIFIED.,.F.,.F.,(4,2,4),(4.33372062421294E-5,0.0872462844676235,
0.169929347173722),.UNSPECIFIED.);
#737=B_SPLINE_CURVE_WITH_KNOTS('',3,(#47908,#47909,#47910,#47911,#47912,
#47913),.UNSPECIFIED.,.F.,.F.,(4,2,4),(1.00509826735353E-6,0.230891419553613,
0.673928064810453),.UNSPECIFIED.);
#738=B_SPLINE_CURVE_WITH_KNOTS('',3,(#47915,#47916,#47917,#47918,#47919,
#47920,#47921,#47922,#47923,#47924,#47925,#47926,#47927,#47928),
 .UNSPECIFIED.,.F.,.F.,(4,2,2,2,2,2,4),(-1.36612196099995,-1.09794402529119,
-0.873297935175745,-0.681853284681958,-0.491110055755908,-0.264840632478997,
-1.00030635918908E-6),.UNSPECIFIED.);
#739=B_SPLINE_CURVE_WITH_KNOTS('',3,(#47930,#47931,#47932,#47933,#47934,
#47935),.UNSPECIFIED.,.F.,.F.,(4,2,4),(5.23876301957788E-5,0.312841131349345,
0.562209482106279),.UNSPECIFIED.);
#740=B_SPLINE_CURVE_WITH_KNOTS('',3,(#47936,#47937,#47938,#47939,#47940,
#47941),.UNSPECIFIED.,.F.,.F.,(4,2,4),(5.79986291934581E-13,0.0801909208299588,
0.203417498476444),.UNSPECIFIED.);
#741=B_SPLINE_CURVE_WITH_KNOTS('',3,(#47998,#47999,#48000,#48001,#48002,
#48003,#48004,#48005,#48006,#48007,#48008,#48009,#48010,#48011),
 .UNSPECIFIED.,.F.,.F.,(4,2,2,2,2,2,4),(0.0377143719414213,0.167070624995476,
0.336553194126115,0.499999999999991,0.663446805873868,0.832929375004528,
0.962285628058582),.UNSPECIFIED.);
#742=B_SPLINE_CURVE_WITH_KNOTS('',3,(#48475,#48476,#48477,#48478,#48479,
#48480,#48481,#48482),.UNSPECIFIED.,.F.,.F.,(4,2,2,4),(1.93377698411972E-5,
0.0820712727478993,0.122296786666274,0.170369462240826),.UNSPECIFIED.);
#743=B_SPLINE_CURVE_WITH_KNOTS('',3,(#48484,#48485,#48486,#48487,#48488,
#48489,#48490,#48491,#48492,#48493),.UNSPECIFIED.,.F.,.F.,(4,2,2,2,4),(1.00118992452698E-6,
0.179077885748985,0.36144549077746,0.457726266756894,0.517260714194413),
 .UNSPECIFIED.);
#744=B_SPLINE_CURVE_WITH_KNOTS('',3,(#48495,#48496,#48497,#48498,#48499,
#48500,#48501,#48502,#48503,#48504,#48505,#48506,#48507,#48508),
 .UNSPECIFIED.,.F.,.F.,(4,2,2,2,2,2,4),(-1.35490487101256,-1.0882371122648,
-0.865819079989883,-0.676189142194246,-0.487214042398886,-0.263045157964749,
-1.00024126735575E-6),.UNSPECIFIED.);
#745=B_SPLINE_CURVE_WITH_KNOTS('',3,(#48510,#48511,#48512,#48513,#48514,
#48515),.UNSPECIFIED.,.F.,.F.,(4,2,4),(8.91007845760208E-5,0.191315852305385,
0.359031481093143),.UNSPECIFIED.);
#746=B_SPLINE_CURVE_WITH_KNOTS('',3,(#48516,#48517,#48518,#48519,#48520,
#48521,#48522,#48523),.UNSPECIFIED.,.F.,.F.,(4,2,2,4),(0.,0.05072995219315,
0.0893288312911254,0.132513385708746),.UNSPECIFIED.);
#747=B_SPLINE_CURVE_WITH_KNOTS('',3,(#48953,#48954,#48955,#48956,#48957,
#48958,#48959,#48960,#48961,#48962,#48963,#48964,#48965,#48966),
 .UNSPECIFIED.,.F.,.F.,(4,2,2,2,2,2,4),(0.0377143719414213,0.167070624995476,
0.336553194126115,0.499999999999991,0.663446805873868,0.832929375004528,
0.962285628058582),.UNSPECIFIED.);
#748=B_SPLINE_CURVE_WITH_KNOTS('',3,(#48968,#48969,#48970,#48971,#48972,
#48973,#48974,#48975,#48976,#48977),.UNSPECIFIED.,.F.,.F.,(4,2,2,2,4),(5.46118981870342E-5,
0.082170984774354,0.124431208907008,0.160831785884752,0.165639953609767),
 .UNSPECIFIED.);
#749=B_SPLINE_CURVE_WITH_KNOTS('',3,(#48979,#48980,#48981,#48982,#48983,
#48984),.UNSPECIFIED.,.F.,.F.,(4,2,4),(1.00682141930218E-6,0.198151473936767,
0.615501668196838),.UNSPECIFIED.);
#750=B_SPLINE_CURVE_WITH_KNOTS('',3,(#48986,#48987,#48988,#48989,#48990,
#48991,#48992,#48993,#48994,#48995,#48996,#48997,#48998,#48999),
 .UNSPECIFIED.,.F.,.F.,(4,2,2,2,2,2,4),(-1.36965940615866,-1.10016160366861,
-0.875066962492997,-0.683316335775481,-0.4922480420488,-0.265550631343516,
-1.00032842355209E-6),.UNSPECIFIED.);
#751=B_SPLINE_CURVE_WITH_KNOTS('',3,(#49001,#49002,#49003,#49004,#49005,
#49006),.UNSPECIFIED.,.F.,.F.,(4,2,4),(2.8517522314608E-5,0.207870471119106,
0.357440650988324),.UNSPECIFIED.);
#752=B_SPLINE_CURVE_WITH_KNOTS('',3,(#49007,#49008,#49009,#49010,#49011,
#49012),.UNSPECIFIED.,.F.,.F.,(4,2,4),(3.11253900974665E-12,0.0802245432637982,
0.139502091510436),.UNSPECIFIED.);
#753=B_SPLINE_CURVE_WITH_KNOTS('',3,(#49069,#49070,#49071,#49072,#49073,
#49074,#49075,#49076,#49077,#49078,#49079,#49080,#49081,#49082),
 .UNSPECIFIED.,.F.,.F.,(4,2,2,2,2,2,4),(0.0377143719414213,0.167070624995476,
0.336553194126115,0.499999999999991,0.663446805873868,0.832929375004528,
0.962285628058582),.UNSPECIFIED.);
#754=B_SPLINE_CURVE_WITH_KNOTS('',3,(#49532,#49533,#49534,#49535,#49536,
#49537,#49538,#49539),.UNSPECIFIED.,.F.,.F.,(4,2,2,4),(5.42863886920242E-5,
0.115927289482269,0.403180122557581,0.690436409009198),.UNSPECIFIED.);
#755=B_SPLINE_CURVE_WITH_KNOTS('',3,(#49541,#49542,#49543,#49544,#49545,
#49546),.UNSPECIFIED.,.F.,.F.,(4,2,4),(1.0067111711105E-6,0.19906795124752,
0.614262232114511),.UNSPECIFIED.);
#756=B_SPLINE_CURVE_WITH_KNOTS('',3,(#49548,#49549,#49550,#49551,#49552,
#49553,#49554,#49555,#49556,#49557,#49558,#49559,#49560,#49561),
 .UNSPECIFIED.,.F.,.F.,(4,2,2,2,2,2,4),(-1.36941174610337,-1.09990067907437,
-0.87481431262687,-0.683060659900653,-0.491984873694128,-0.265259069617268,
-1.00032309670381E-6),.UNSPECIFIED.);
#757=B_SPLINE_CURVE_WITH_KNOTS('',3,(#49563,#49564,#49565,#49566,#49567,
#49568),.UNSPECIFIED.,.F.,.F.,(4,2,4),(6.11026370320298E-5,0.197154855683272,
0.335212309964277),.UNSPECIFIED.);
#758=B_SPLINE_CURVE_WITH_KNOTS('',3,(#49569,#49570,#49571,#49572,#49573,
#49574,#49575,#49576),.UNSPECIFIED.,.F.,.F.,(4,2,2,4),(0.,0.00480921378375552,
0.0810921310518215,0.12941952313067),.UNSPECIFIED.);
#759=B_SPLINE_CURVE_WITH_KNOTS('',3,(#50006,#50007,#50008,#50009,#50010,
#50011,#50012,#50013,#50014,#50015,#50016,#50017,#50018,#50019),
 .UNSPECIFIED.,.F.,.F.,(4,2,2,2,2,2,4),(0.0377143719414213,0.167070624995476,
0.336553194126115,0.499999999999991,0.663446805873868,0.832929375004528,
0.962285628058582),.UNSPECIFIED.);
#760=B_SPLINE_CURVE_WITH_KNOTS('',3,(#50021,#50022,#50023,#50024,#50025,
#50026,#50027,#50028,#50029,#50030),.UNSPECIFIED.,.F.,.F.,(4,2,2,2,4),(4.40252338115954E-5,
0.0593320969994734,0.077891435154,0.0947902856199741,0.0969876170690407),
 .UNSPECIFIED.);
#761=B_SPLINE_CURVE_WITH_KNOTS('',3,(#50032,#50033,#50034,#50035,#50036,
#50037),.UNSPECIFIED.,.F.,.F.,(4,2,4),(1.00575192677772E-6,0.196465123063792,
0.617668689286788),.UNSPECIFIED.);
#762=B_SPLINE_CURVE_WITH_KNOTS('',3,(#50039,#50040,#50041,#50042,#50043,
#50044,#50045,#50046,#50047,#50048,#50049,#50050,#50051,#50052),
 .UNSPECIFIED.,.F.,.F.,(4,2,2,2,2,2,4),(-1.36650845342114,-1.09810261018534,
-0.873436258570306,-0.682032732525366,-0.491294664691022,-0.264928244974586,
-1.00034351039345E-6),.UNSPECIFIED.);
#763=B_SPLINE_CURVE_WITH_KNOTS('',3,(#50054,#50055,#50056,#50057,#50058,
#50059),.UNSPECIFIED.,.F.,.F.,(4,2,4),(1.56372366413953E-5,0.223813981237213,
0.38728646607154),.UNSPECIFIED.);
#764=B_SPLINE_CURVE_WITH_KNOTS('',3,(#50060,#50061,#50062,#50063,#50064,
#50065,#50066,#50067),.UNSPECIFIED.,.F.,.F.,(4,2,2,4),(0.,0.0799523739475497,
0.120850709803476,0.158334330677306),.UNSPECIFIED.);
#765=B_SPLINE_CURVE_WITH_KNOTS('',3,(#50124,#50125,#50126,#50127,#50128,
#50129,#50130,#50131,#50132,#50133,#50134,#50135,#50136,#50137),
 .UNSPECIFIED.,.F.,.F.,(4,2,2,2,2,2,4),(0.0377143719414213,0.167070624995476,
0.336553194126115,0.499999999999991,0.663446805873868,0.832929375004528,
0.962285628058582),.UNSPECIFIED.);
#766=B_SPLINE_CURVE_WITH_KNOTS('',3,(#50503,#50504,#50505,#50506,#50507,
#50508),.UNSPECIFIED.,.F.,.F.,(4,2,4),(2.90735538954063E-5,0.0821068334164978,
0.185641730304597),.UNSPECIFIED.);
#767=B_SPLINE_CURVE_WITH_KNOTS('',3,(#50510,#50511,#50512,#50513,#50514,
#50515),.UNSPECIFIED.,.F.,.F.,(4,2,4),(1.00576589928379E-6,0.196720798610431,
0.607958009277496),.UNSPECIFIED.);
#768=B_SPLINE_CURVE_WITH_KNOTS('',3,(#50517,#50518,#50519,#50520,#50521,
#50522,#50523,#50524,#50525,#50526,#50527,#50528,#50529,#50530),
 .UNSPECIFIED.,.F.,.F.,(4,2,2,2,2,2,4),(-1.36645387087117,-1.09803009009587,
-0.873368980499991,-0.682000111522624,-0.491298508345502,-0.26494563806227,
-1.00034434035875E-6),.UNSPECIFIED.);
#769=B_SPLINE_CURVE_WITH_KNOTS('',3,(#50532,#50533,#50534,#50535,#50536,
#50537),.UNSPECIFIED.,.F.,.F.,(4,2,4),(5.04888740588569E-5,0.222104264584732,
0.384046823394325),.UNSPECIFIED.);
#770=B_SPLINE_CURVE_WITH_KNOTS('',3,(#50538,#50539,#50540,#50541,#50542,
#50543),.UNSPECIFIED.,.F.,.F.,(4,2,4),(0.,0.0812570486202188,0.181154925817027),
 .UNSPECIFIED.);
#771=B_SPLINE_CURVE_WITH_KNOTS('',3,(#50945,#50946,#50947,#50948,#50949,
#50950,#50951,#50952,#50953,#50954,#50955,#50956,#50957,#50958),
 .UNSPECIFIED.,.F.,.F.,(4,2,2,2,2,2,4),(0.0377143719414213,0.167070624995476,
0.336553194126115,0.499999999999991,0.663446805873868,0.832929375004528,
0.962285628058582),.UNSPECIFIED.);
#772=B_SPLINE_CURVE_WITH_KNOTS('',3,(#50960,#50961,#50962,#50963,#50964,
#50965,#50966,#50967),.UNSPECIFIED.,.F.,.F.,(4,2,2,4),(3.17122319223456E-5,
0.0452758658318462,0.104387964404602,0.163687991775634),.UNSPECIFIED.);
#773=B_SPLINE_CURVE_WITH_KNOTS('',3,(#50969,#50970,#50971,#50972,#50973,
#50974),.UNSPECIFIED.,.F.,.F.,(4,2,4),(1.00585128027205E-6,0.196560733785392,
0.622029044934339),.UNSPECIFIED.);
#774=B_SPLINE_CURVE_WITH_KNOTS('',3,(#50976,#50977,#50978,#50979,#50980,
#50981,#50982,#50983,#50984,#50985,#50986,#50987,#50988,#50989),
 .UNSPECIFIED.,.F.,.F.,(4,2,2,2,2,2,4),(-1.36674172606792,-1.09823421639304,
-0.873527156968718,-0.682129646363664,-0.49139025098167,-0.264967864874043,
-1.00034944706873E-6),.UNSPECIFIED.);
#775=B_SPLINE_CURVE_WITH_KNOTS('',3,(#50991,#50992,#50993,#50994,#50995,
#50996),.UNSPECIFIED.,.F.,.F.,(4,2,4),(6.32656345427143E-5,0.163040125320008,
0.265078073811059),.UNSPECIFIED.);
#776=B_SPLINE_CURVE_WITH_KNOTS('',3,(#50997,#50998,#50999,#51000,#51001,
#51002),.UNSPECIFIED.,.F.,.F.,(4,2,4),(2.68743761055743E-12,0.0899508604032875,
0.179627225923839),.UNSPECIFIED.);
#777=B_SPLINE_CURVE_WITH_KNOTS('',3,(#51059,#51060,#51061,#51062,#51063,
#51064,#51065,#51066,#51067,#51068,#51069,#51070,#51071,#51072),
 .UNSPECIFIED.,.F.,.F.,(4,2,2,2,2,2,4),(0.0377143719414213,0.167070624995476,
0.336553194126115,0.499999999999991,0.663446805873868,0.832929375004528,
0.962285628058582),.UNSPECIFIED.);
#778=B_SPLINE_CURVE_WITH_KNOTS('',3,(#51452,#51453,#51454,#51455,#51456,
#51457),.UNSPECIFIED.,.F.,.F.,(4,2,4),(2.02724939215941E-5,0.0820778995171911,
0.183608432352108),.UNSPECIFIED.);
#779=B_SPLINE_CURVE_WITH_KNOTS('',3,(#51459,#51460,#51461,#51462,#51463,
#51464),.UNSPECIFIED.,.F.,.F.,(4,2,4),(1.00573485054331E-6,0.196992912849433,
0.611376509494975),.UNSPECIFIED.);
#780=B_SPLINE_CURVE_WITH_KNOTS('',3,(#51466,#51467,#51468,#51469,#51470,
#51471,#51472,#51473,#51474,#51475,#51476,#51477,#51478,#51479),
 .UNSPECIFIED.,.F.,.F.,(4,2,2,2,2,2,4),(-1.36651508911559,-1.09808854337808,
-0.873419265282326,-0.682038625392179,-0.491323399854143,-0.264952793979431,
-1.00034248505535E-6),.UNSPECIFIED.);
#781=B_SPLINE_CURVE_WITH_KNOTS('',3,(#51481,#51482,#51483,#51484,#51485,
#51486),.UNSPECIFIED.,.F.,.F.,(4,2,4),(1.03339269301046E-5,0.176278240887036,
0.282118520392689),.UNSPECIFIED.);
#782=B_SPLINE_CURVE_WITH_KNOTS('',3,(#51487,#51488,#51489,#51490,#51491,
#51492),.UNSPECIFIED.,.F.,.F.,(4,2,4),(1.94846466985946E-13,0.0811435839467738,
0.185199096592569),.UNSPECIFIED.);
#783=B_SPLINE_CURVE_WITH_KNOTS('',3,(#51964,#51965,#51966,#51967,#51968,
#51969,#51970,#51971,#51972,#51973,#51974,#51975,#51976,#51977),
 .UNSPECIFIED.,.F.,.F.,(4,2,2,2,2,2,4),(0.0377143719414213,0.167070624995476,
0.336553194126115,0.499999999999991,0.663446805873868,0.832929375004528,
0.962285628058582),.UNSPECIFIED.);
#784=B_SPLINE_CURVE_WITH_KNOTS('',3,(#51979,#51980,#51981,#51982,#51983,
#51984,#51985,#51986),.UNSPECIFIED.,.F.,.F.,(4,2,2,4),(7.66048904690143E-5,
0.0724751619057042,0.135157008985432,0.209683518789831),.UNSPECIFIED.);
#785=B_SPLINE_CURVE_WITH_KNOTS('',3,(#51988,#51989,#51990,#51991,#51992,
#51993),.UNSPECIFIED.,.F.,.F.,(4,2,4),(1.00671823419874E-6,0.198656747545274,
0.617231925244798),.UNSPECIFIED.);
#786=B_SPLINE_CURVE_WITH_KNOTS('',3,(#51995,#51996,#51997,#51998,#51999,
#52000,#52001,#52002,#52003,#52004,#52005,#52006,#52007,#52008),
 .UNSPECIFIED.,.F.,.F.,(4,2,2,2,2,2,4),(-1.36939616200995,-1.09987950875221,
-0.874793162387835,-0.683050721286367,-0.491987088351277,-0.265266499330064,
-1.00032344033588E-6),.UNSPECIFIED.);
#787=B_SPLINE_CURVE_WITH_KNOTS('',3,(#52010,#52011,#52012,#52013,#52014,
#52015),.UNSPECIFIED.,.F.,.F.,(4,2,4),(3.08789861800714E-5,0.198559217559626,
0.337824153970451),.UNSPECIFIED.);
#788=B_SPLINE_CURVE_WITH_KNOTS('',3,(#52016,#52017,#52018,#52019,#52020,
#52021,#52022,#52023),.UNSPECIFIED.,.F.,.F.,(4,2,2,4),(4.33668191395318E-13,
0.0554692068429926,0.26010462373677,0.513538194310567),.UNSPECIFIED.);
#789=B_SPLINE_CURVE_WITH_KNOTS('',3,(#52080,#52081,#52082,#52083,#52084,
#52085,#52086,#52087,#52088,#52089,#52090,#52091,#52092,#52093),
 .UNSPECIFIED.,.F.,.F.,(4,2,2,2,2,2,4),(0.0377143719414213,0.167070624995476,
0.336553194126115,0.499999999999991,0.663446805873868,0.832929375004528,
0.962285628058582),.UNSPECIFIED.);
#790=B_SPLINE_CURVE_WITH_KNOTS('',3,(#52669,#52670,#52671,#52672,#52673,
#52674,#52675,#52676),.UNSPECIFIED.,.F.,.F.,(4,2,2,4),(4.0720543721802E-5,
0.082048395609366,0.10384153561188,0.165696528972352),.UNSPECIFIED.);
#791=B_SPLINE_CURVE_WITH_KNOTS('',3,(#52678,#52679,#52680,#52681,#52682,
#52683),.UNSPECIFIED.,.F.,.F.,(4,2,4),(1.00674327113181E-6,0.198975068155899,
0.613393100807198),.UNSPECIFIED.);
#792=B_SPLINE_CURVE_WITH_KNOTS('',3,(#52685,#52686,#52687,#52688,#52689,
#52690,#52691,#52692,#52693,#52694,#52695,#52696,#52697,#52698),
 .UNSPECIFIED.,.F.,.F.,(4,2,2,2,2,2,4),(-1.36945586316978,-1.09992910347376,
-0.874829785599427,-0.683077785823512,-0.492005087217108,-0.265273394907698,
-1.00032464471707E-6),.UNSPECIFIED.);
#793=B_SPLINE_CURVE_WITH_KNOTS('',3,(#52700,#52701,#52702,#52703,#52704,
#52705),.UNSPECIFIED.,.F.,.F.,(4,2,4),(3.77093093284653E-5,0.199023405936395,
0.338855740163895),.UNSPECIFIED.);
#794=B_SPLINE_CURVE_WITH_KNOTS('',3,(#52706,#52707,#52708,#52709,#52710,
#52711),.UNSPECIFIED.,.F.,.F.,(4,2,4),(0.,0.0811055819570389,0.134676521572393),
 .UNSPECIFIED.);
#795=B_SPLINE_CURVE_WITH_KNOTS('',3,(#53127,#53128,#53129,#53130,#53131,
#53132,#53133,#53134,#53135,#53136,#53137,#53138,#53139,#53140),
 .UNSPECIFIED.,.F.,.F.,(4,2,2,2,2,2,4),(0.0377143719414213,0.167070624995476,
0.336553194126115,0.499999999999991,0.663446805873868,0.832929375004528,
0.962285628058582),.UNSPECIFIED.);
#796=B_SPLINE_CURVE_WITH_KNOTS('',3,(#53142,#53143,#53144,#53145,#53146,
#53147),.UNSPECIFIED.,.F.,.F.,(4,2,4),(3.17663181462393E-5,0.0586300965114554,
0.12163893952438),.UNSPECIFIED.);
#797=B_SPLINE_CURVE_WITH_KNOTS('',3,(#53149,#53150,#53151,#53152,#53153,
#53154),.UNSPECIFIED.,.F.,.F.,(4,2,4),(1.00574544958261E-6,0.196442953126253,
0.616075190837725),.UNSPECIFIED.);
#798=B_SPLINE_CURVE_WITH_KNOTS('',3,(#53156,#53157,#53158,#53159,#53160,
#53161,#53162,#53163,#53164,#53165,#53166,#53167,#53168,#53169),
 .UNSPECIFIED.,.F.,.F.,(4,2,2,2,2,2,4),(-1.36646180861503,-1.09803139080332,
-0.873373464214575,-0.682006913510101,-0.491306155279075,-0.26494779063171,
-1.00034312451653E-6),.UNSPECIFIED.);
#799=B_SPLINE_CURVE_WITH_KNOTS('',3,(#53171,#53172,#53173,#53174,#53175,
#53176),.UNSPECIFIED.,.F.,.F.,(4,2,4),(8.51202734725518E-5,0.213282211024296,
0.347455197118523),.UNSPECIFIED.);
#800=B_SPLINE_CURVE_WITH_KNOTS('',3,(#53177,#53178,#53179,#53180,#53181,
#53182),.UNSPECIFIED.,.F.,.F.,(4,2,4),(8.22519357859456E-13,0.0801856487952568,
0.160124211305378),.UNSPECIFIED.);
#801=B_SPLINE_CURVE_WITH_KNOTS('',3,(#53239,#53240,#53241,#53242,#53243,
#53244,#53245,#53246,#53247,#53248,#53249,#53250,#53251,#53252),
 .UNSPECIFIED.,.F.,.F.,(4,2,2,2,2,2,4),(0.0377143719414213,0.167070624995476,
0.336553194126115,0.499999999999991,0.663446805873868,0.832929375004528,
0.962285628058582),.UNSPECIFIED.);
#802=B_SPLINE_CURVE_WITH_KNOTS('',3,(#53716,#53717,#53718,#53719,#53720,
#53721),.UNSPECIFIED.,.F.,.F.,(4,2,4),(2.85042569573143E-5,0.0779704082414512,
0.146157984837617),.UNSPECIFIED.);
#803=B_SPLINE_CURVE_WITH_KNOTS('',3,(#53723,#53724,#53725,#53726,#53727,
#53728),.UNSPECIFIED.,.F.,.F.,(4,2,4),(1.00575001969219E-6,0.196811902994003,
0.607209604097769),.UNSPECIFIED.);
#804=B_SPLINE_CURVE_WITH_KNOTS('',3,(#53730,#53731,#53732,#53733,#53734,
#53735,#53736,#53737,#53738,#53739,#53740,#53741,#53742,#53743),
 .UNSPECIFIED.,.F.,.F.,(4,2,2,2,2,2,4),(-1.36646927232899,-1.09805347703677,
-0.87339045221244,-0.682015194511553,-0.49130486745357,-0.264941327695831,
-1.00034339038765E-6),.UNSPECIFIED.);
#805=B_SPLINE_CURVE_WITH_KNOTS('',3,(#53745,#53746,#53747,#53748,#53749,
#53750),.UNSPECIFIED.,.F.,.F.,(4,2,4),(3.18944872613953E-5,0.201689934389403,
0.342722617046712),.UNSPECIFIED.);
#806=B_SPLINE_CURVE_WITH_KNOTS('',3,(#53751,#53752,#53753,#53754,#53755,
#53756),.UNSPECIFIED.,.F.,.F.,(4,2,4),(7.41583121241415E-13,0.0919471405631882,
0.218813839045918),.UNSPECIFIED.);
#807=B_SPLINE_CURVE_WITH_KNOTS('',3,(#54200,#54201,#54202,#54203,#54204,
#54205,#54206,#54207,#54208,#54209,#54210,#54211,#54212,#54213),
 .UNSPECIFIED.,.F.,.F.,(4,2,2,2,2,2,4),(0.0377143719414213,0.167070624995476,
0.336553194126115,0.499999999999991,0.663446805873868,0.832929375004528,
0.962285628058582),.UNSPECIFIED.);
#808=B_SPLINE_CURVE_WITH_KNOTS('',3,(#54215,#54216,#54217,#54218,#54219,
#54220),.UNSPECIFIED.,.F.,.F.,(4,2,4),(8.27853671649851E-6,0.117348681204103,
0.81803028591539),.UNSPECIFIED.);
#809=B_SPLINE_CURVE_WITH_KNOTS('',3,(#54222,#54223,#54224,#54225,#54226,
#54227),.UNSPECIFIED.,.F.,.F.,(4,2,4),(1.00584838939465E-6,0.196105737182075,
0.613752572300065),.UNSPECIFIED.);
#810=B_SPLINE_CURVE_WITH_KNOTS('',3,(#54229,#54230,#54231,#54232,#54233,
#54234,#54235,#54236,#54237,#54238,#54239,#54240,#54241,#54242),
 .UNSPECIFIED.,.F.,.F.,(4,2,2,2,2,2,4),(-1.36657598676591,-1.09814330805353,
-0.873456182939785,-0.682053794892946,-0.49131998381188,-0.264952672836963,
-1.00034927255395E-6),.UNSPECIFIED.);
#811=B_SPLINE_CURVE_WITH_KNOTS('',3,(#54244,#54245,#54246,#54247,#54248,
#54249),.UNSPECIFIED.,.F.,.F.,(4,2,4),(8.19755470884497E-5,0.23524102296215,
0.412699034637965),.UNSPECIFIED.);
#812=B_SPLINE_CURVE_WITH_KNOTS('',3,(#54250,#54251,#54252,#54253,#54254,
#54255),.UNSPECIFIED.,.F.,.F.,(4,2,4),(5.98025872820168E-13,0.0829465259271522,
0.178737241653031),.UNSPECIFIED.);
#813=B_SPLINE_CURVE_WITH_KNOTS('',3,(#54312,#54313,#54314,#54315,#54316,
#54317,#54318,#54319,#54320,#54321,#54322,#54323,#54324,#54325),
 .UNSPECIFIED.,.F.,.F.,(4,2,2,2,2,2,4),(0.0377143719414213,0.167070624995476,
0.336553194126115,0.499999999999991,0.663446805873868,0.832929375004528,
0.962285628058582),.UNSPECIFIED.);
#814=B_SPLINE_CURVE_WITH_KNOTS('',3,(#54761,#54762,#54763,#54764,#54765,
#54766,#54767,#54768,#54769,#54770),.UNSPECIFIED.,.F.,.F.,(4,2,2,2,4),(2.91083665470649E-5,
0.0448810650389932,0.10235865502192,0.143363070345125,0.176052267827766),
 .UNSPECIFIED.);
#815=B_SPLINE_CURVE_WITH_KNOTS('',3,(#54772,#54773,#54774,#54775,#54776,
#54777),.UNSPECIFIED.,.F.,.F.,(4,2,4),(1.00586691344213E-6,0.197039335069742,
0.614437201408451),.UNSPECIFIED.);
#816=B_SPLINE_CURVE_WITH_KNOTS('',3,(#54779,#54780,#54781,#54782,#54783,
#54784,#54785,#54786,#54787,#54788,#54789,#54790,#54791,#54792),
 .UNSPECIFIED.,.F.,.F.,(4,2,2,2,2,2,4),(-1.36676533760477,-1.09824478324466,
-0.873535367034155,-0.682138570180602,-0.491399555548606,-0.264972297603895,
-1.00035037616401E-6),.UNSPECIFIED.);
#817=B_SPLINE_CURVE_WITH_KNOTS('',3,(#54794,#54795,#54796,#54797,#54798,
#54799),.UNSPECIFIED.,.F.,.F.,(4,2,4),(0.00013096404143776,0.152963582320661,
0.248940965083308),.UNSPECIFIED.);
#818=B_SPLINE_CURVE_WITH_KNOTS('',3,(#54800,#54801,#54802,#54803,#54804,
#54805,#54806,#54807),.UNSPECIFIED.,.F.,.F.,(4,2,2,4),(3.81584992072495E-12,
0.0811754769524944,0.11370948911483,0.136181238711659),.UNSPECIFIED.);
#819=B_SPLINE_CURVE_WITH_KNOTS('',3,(#55279,#55280,#55281,#55282,#55283,
#55284,#55285,#55286,#55287,#55288,#55289,#55290,#55291,#55292),
 .UNSPECIFIED.,.F.,.F.,(4,2,2,2,2,2,4),(0.0377143719414213,0.167070624995476,
0.336553194126115,0.499999999999991,0.663446805873868,0.832929375004528,
0.962285628058582),.UNSPECIFIED.);
#820=B_SPLINE_CURVE_WITH_KNOTS('',3,(#55294,#55295,#55296,#55297,#55298,
#55299),.UNSPECIFIED.,.F.,.F.,(4,2,4),(1.31240404424589E-5,0.118148896618705,
0.705933282625893),.UNSPECIFIED.);
#821=B_SPLINE_CURVE_WITH_KNOTS('',3,(#55301,#55302,#55303,#55304,#55305,
#55306),.UNSPECIFIED.,.F.,.F.,(4,2,4),(1.00584283955035E-6,0.196654732302861,
0.618684486486058),.UNSPECIFIED.);
#822=B_SPLINE_CURVE_WITH_KNOTS('',3,(#55308,#55309,#55310,#55311,#55312,
#55313,#55314,#55315,#55316,#55317,#55318,#55319,#55320,#55321),
 .UNSPECIFIED.,.F.,.F.,(4,2,2,2,2,2,4),(-1.36678617495215,-1.09826185815999,
-0.873545812350535,-0.682155092083844,-0.491422802142017,-0.264985880565712,
-1.00034894152623E-6),.UNSPECIFIED.);
#823=B_SPLINE_CURVE_WITH_KNOTS('',3,(#55323,#55324,#55325,#55326,#55327,
#55328),.UNSPECIFIED.,.F.,.F.,(4,2,4),(1.56558672178928E-5,0.190788483130578,
0.32659926592214),.UNSPECIFIED.);
#824=B_SPLINE_CURVE_WITH_KNOTS('',3,(#55329,#55330,#55331,#55332,#55333,
#55334),.UNSPECIFIED.,.F.,.F.,(4,2,4),(1.03020526869841E-12,0.0800803859593916,
0.135679047359458),.UNSPECIFIED.);
#825=B_SPLINE_CURVE_WITH_KNOTS('',3,(#55391,#55392,#55393,#55394,#55395,
#55396,#55397,#55398,#55399,#55400,#55401,#55402,#55403,#55404),
 .UNSPECIFIED.,.F.,.F.,(4,2,2,2,2,2,4),(0.0377143719414213,0.167070624995476,
0.336553194126115,0.499999999999991,0.663446805873868,0.832929375004528,
0.962285628058582),.UNSPECIFIED.);
#826=B_SPLINE_CURVE_WITH_KNOTS('',3,(#55840,#55841,#55842,#55843,#55844,
#55845,#55846,#55847,#55848,#55849),.UNSPECIFIED.,.F.,.F.,(4,2,2,2,4),(2.95331200204396E-5,
0.0448823812946117,0.10236199038552,0.143361158366412,0.176043615886501),
 .UNSPECIFIED.);
#827=B_SPLINE_CURVE_WITH_KNOTS('',3,(#55851,#55852,#55853,#55854,#55855,
#55856),.UNSPECIFIED.,.F.,.F.,(4,2,4),(1.00586876398164E-6,0.197038889607744,
0.614451442266876),.UNSPECIFIED.);
#828=B_SPLINE_CURVE_WITH_KNOTS('',3,(#55858,#55859,#55860,#55861,#55862,
#55863,#55864,#55865,#55866,#55867,#55868,#55869,#55870,#55871),
 .UNSPECIFIED.,.F.,.F.,(4,2,2,2,2,2,4),(-1.36676752401463,-1.09824522385243,
-0.873535205630291,-0.682139122541776,-0.49140088307381,-0.264973665093558,
-1.00035048783346E-6),.UNSPECIFIED.);
#829=B_SPLINE_CURVE_WITH_KNOTS('',3,(#55873,#55874,#55875,#55876,#55877,
#55878),.UNSPECIFIED.,.F.,.F.,(4,2,4),(0.000132963294187387,0.153060747720903,
0.249120285259133),.UNSPECIFIED.);
#830=B_SPLINE_CURVE_WITH_KNOTS('',3,(#55879,#55880,#55881,#55882,#55883,
#55884,#55885,#55886),.UNSPECIFIED.,.F.,.F.,(4,2,2,4),(7.85771554400852E-12,
0.0811766790944722,0.113710097814863,0.136178725750842),.UNSPECIFIED.);
#831=B_SPLINE_CURVE_WITH_KNOTS('',3,(#56498,#56499,#56500,#56501,#56502,
#56503,#56504,#56505,#56506,#56507,#56508,#56509,#56510,#56511),
 .UNSPECIFIED.,.F.,.F.,(4,2,2,2,2,2,4),(0.0377143719414213,0.167070624995476,
0.336553194126115,0.499999999999991,0.663446805873868,0.832929375004528,
0.962285628058582),.UNSPECIFIED.);
#832=B_SPLINE_CURVE_WITH_KNOTS('',3,(#56513,#56514,#56515,#56516,#56517,
#56518,#56519,#56520,#56521,#56522),.UNSPECIFIED.,.F.,.F.,(4,2,2,2,4),(2.90874908040396E-5,
0.0695369396976002,0.127685025171556,0.192550047820966,0.193204673416467),
 .UNSPECIFIED.);
#833=B_SPLINE_CURVE_WITH_KNOTS('',3,(#56524,#56525,#56526,#56527,#56528,
#56529),.UNSPECIFIED.,.F.,.F.,(4,2,4),(1.00063186540735E-6,0.183871198323765,
0.593831676218595),.UNSPECIFIED.);
#834=B_SPLINE_CURVE_WITH_KNOTS('',3,(#56531,#56532,#56533,#56534,#56535,
#56536,#56537,#56538,#56539,#56540,#56541,#56542,#56543,#56544),
 .UNSPECIFIED.,.F.,.F.,(4,2,2,2,2,2,4),(-1.35138145767626,-1.08533623797411,
-0.863457932782986,-0.67461579591868,-0.48640715531557,-0.262769633851996,
-1.00013603251387E-6),.UNSPECIFIED.);
#835=B_SPLINE_CURVE_WITH_KNOTS('',3,(#56546,#56547,#56548,#56549,#56550,
#56551),.UNSPECIFIED.,.F.,.F.,(4,2,4),(7.67987202833742E-5,0.135045540153931,
0.23216672789008),.UNSPECIFIED.);
#836=B_SPLINE_CURVE_WITH_KNOTS('',3,(#56552,#56553,#56554,#56555,#56556,
#56557,#56558,#56559),.UNSPECIFIED.,.F.,.F.,(4,2,2,4),(5.70631864960257E-12,
0.0385065493161646,0.101661114347598,0.190748080830985),.UNSPECIFIED.);
#837=B_SPLINE_CURVE_WITH_KNOTS('',3,(#56616,#56617,#56618,#56619,#56620,
#56621,#56622,#56623,#56624,#56625,#56626,#56627,#56628,#56629),
 .UNSPECIFIED.,.F.,.F.,(4,2,2,2,2,2,4),(0.0377143719414213,0.167070624995476,
0.336553194126115,0.499999999999991,0.663446805873868,0.832929375004528,
0.962285628058582),.UNSPECIFIED.);
#838=B_SPLINE_CURVE_WITH_KNOTS('',3,(#57191,#57192,#57193,#57194,#57195,
#57196,#57197,#57198),.UNSPECIFIED.,.F.,.F.,(4,2,2,4),(3.73720623976683E-5,
0.0820934034488392,0.159780549935175,0.163589055589674),.UNSPECIFIED.);
#839=B_SPLINE_CURVE_WITH_KNOTS('',3,(#57200,#57201,#57202,#57203,#57204,
#57205),.UNSPECIFIED.,.F.,.F.,(4,2,4),(1.00680487095348E-6,0.198775773316189,
0.612602414802361),.UNSPECIFIED.);
#840=B_SPLINE_CURVE_WITH_KNOTS('',3,(#57207,#57208,#57209,#57210,#57211,
#57212,#57213,#57214,#57215,#57216,#57217,#57218,#57219,#57220),
 .UNSPECIFIED.,.F.,.F.,(4,2,2,2,2,2,4),(-1.36947028433637,-1.09994697149041,
-0.874841168477541,-0.68308329902947,-0.492005354543596,-0.265278186460551,
-1.00032760913201E-6),.UNSPECIFIED.);
#841=B_SPLINE_CURVE_WITH_KNOTS('',3,(#57222,#57223,#57224,#57225,#57226,
#57227),.UNSPECIFIED.,.F.,.F.,(4,2,4),(9.95249900306014E-6,0.201659078077706,
0.343960579336747),.UNSPECIFIED.);
#842=B_SPLINE_CURVE_WITH_KNOTS('',3,(#57228,#57229,#57230,#57231,#57232,
#57233),.UNSPECIFIED.,.F.,.F.,(4,2,4),(0.,0.0810866766827009,0.130143252265822),
 .UNSPECIFIED.);
#843=B_SPLINE_CURVE_WITH_KNOTS('',3,(#57747,#57748,#57749,#57750,#57751,
#57752,#57753,#57754,#57755,#57756,#57757,#57758,#57759,#57760),
 .UNSPECIFIED.,.F.,.F.,(4,2,2,2,2,2,4),(0.0377143719414213,0.167070624995476,
0.336553194126115,0.499999999999991,0.663446805873868,0.832929375004528,
0.962285628058582),.UNSPECIFIED.);
#844=B_SPLINE_CURVE_WITH_KNOTS('',3,(#57762,#57763,#57764,#57765,#57766,
#57767,#57768,#57769,#57770,#57771),.UNSPECIFIED.,.F.,.F.,(4,2,2,2,4),(6.26026778345803E-5,
0.0821879366532444,0.124360696633958,0.160511740289931,0.165280462627525),
 .UNSPECIFIED.);
#845=B_SPLINE_CURVE_WITH_KNOTS('',3,(#57773,#57774,#57775,#57776,#57777,
#57778,#57779,#57780,#57781,#57782),.UNSPECIFIED.,.F.,.F.,(4,2,2,2,4),(1.00120887031484E-6,
0.178144277374141,0.361084123405984,0.458351091752043,0.518212486842599),
 .UNSPECIFIED.);
#846=B_SPLINE_CURVE_WITH_KNOTS('',3,(#57784,#57785,#57786,#57787,#57788,
#57789,#57790,#57791,#57792,#57793,#57794,#57795,#57796,#57797),
 .UNSPECIFIED.,.F.,.F.,(4,2,2,2,2,2,4),(-1.35452120523838,-1.08792026996376,
-0.865513415712065,-0.676039627480199,-0.487227006474019,-0.263105526553072,
-1.00024511471768E-6),.UNSPECIFIED.);
#847=B_SPLINE_CURVE_WITH_KNOTS('',3,(#57799,#57800,#57801,#57802,#57803,
#57804),.UNSPECIFIED.,.F.,.F.,(4,2,4),(5.13023327127914E-5,0.195133577906603,
0.330520359442512),.UNSPECIFIED.);
#848=B_SPLINE_CURVE_WITH_KNOTS('',3,(#57805,#57806,#57807,#57808,#57809,
#57810),.UNSPECIFIED.,.F.,.F.,(4,2,4),(2.7857164981918E-12,0.0801884474066829,
0.134390902567056),.UNSPECIFIED.);
#849=B_SPLINE_CURVE_WITH_KNOTS('',3,(#57867,#57868,#57869,#57870,#57871,
#57872,#57873,#57874,#57875,#57876,#57877,#57878,#57879,#57880),
 .UNSPECIFIED.,.F.,.F.,(4,2,2,2,2,2,4),(0.0377143719414213,0.167070624995476,
0.336553194126115,0.499999999999991,0.663446805873868,0.832929375004528,
0.962285628058582),.UNSPECIFIED.);
#850=B_SPLINE_CURVE_WITH_KNOTS('',3,(#58246,#58247,#58248,#58249,#58250,
#58251,#58252,#58253),.UNSPECIFIED.,.F.,.F.,(4,2,2,4),(4.73120833335754E-5,
0.0422670695525102,0.0810849470856931,0.127252781970067),.UNSPECIFIED.);
#851=B_SPLINE_CURVE_WITH_KNOTS('',3,(#58255,#58256,#58257,#58258,#58259,
#58260),.UNSPECIFIED.,.F.,.F.,(4,2,4),(1.00647499030429E-6,0.200113073863495,
0.595429491994324),.UNSPECIFIED.);
#852=B_SPLINE_CURVE_WITH_KNOTS('',3,(#58262,#58263,#58264,#58265,#58266,
#58267,#58268,#58269,#58270,#58271,#58272,#58273,#58274,#58275),
 .UNSPECIFIED.,.F.,.F.,(4,2,2,2,2,2,4),(-1.36849439771666,-1.09954066052859,
-0.874510163535254,-0.682956346820273,-0.492067229987142,-0.265320521461021,
-1.00031346793631E-6),.UNSPECIFIED.);
#853=B_SPLINE_CURVE_WITH_KNOTS('',3,(#58277,#58278,#58279,#58280,#58281,
#58282),.UNSPECIFIED.,.F.,.F.,(4,2,4),(7.71756783525451E-5,0.307508164573013,
0.565378873758567),.UNSPECIFIED.);
#854=B_SPLINE_CURVE_WITH_KNOTS('',3,(#58283,#58284,#58285,#58286,#58287,
#58288,#58289,#58290),.UNSPECIFIED.,.F.,.F.,(4,2,2,4),(3.89766384540504E-13,
0.0811658080415485,0.130795260681648,0.217612754456687),.UNSPECIFIED.);
#855=B_SPLINE_CURVE_WITH_KNOTS('',3,(#58804,#58805,#58806,#58807,#58808,
#58809,#58810,#58811,#58812,#58813,#58814,#58815,#58816,#58817),
 .UNSPECIFIED.,.F.,.F.,(4,2,2,2,2,2,4),(0.0377143719414213,0.167070624995476,
0.336553194126115,0.499999999999991,0.663446805873868,0.832929375004528,
0.962285628058582),.UNSPECIFIED.);
#856=B_SPLINE_CURVE_WITH_KNOTS('',3,(#58819,#58820,#58821,#58822,#58823,
#58824,#58825,#58826,#58827,#58828),.UNSPECIFIED.,.F.,.F.,(4,2,2,2,4),(6.1190446859549E-5,
0.0821849189214334,0.124358056634849,0.160517624190395,0.165288966829186),
 .UNSPECIFIED.);
#857=B_SPLINE_CURVE_WITH_KNOTS('',3,(#58830,#58831,#58832,#58833,#58834,
#58835,#58836,#58837,#58838,#58839),.UNSPECIFIED.,.F.,.F.,(4,2,2,2,4),(1.00121666513906E-6,
0.178436610588235,0.361713510187113,0.459165212991689,0.519162438061592),
 .UNSPECIFIED.);
#858=B_SPLINE_CURVE_WITH_KNOTS('',3,(#58841,#58842,#58843,#58844,#58845,
#58846,#58847,#58848,#58849,#58850,#58851,#58852,#58853,#58854),
 .UNSPECIFIED.,.F.,.F.,(4,2,2,2,2,2,4),(-1.35454818634146,-1.08794337470072,
-0.865532135918778,-0.676052154638076,-0.487233237434815,-0.26310695574337,
-1.00024670269493E-6),.UNSPECIFIED.);
#859=B_SPLINE_CURVE_WITH_KNOTS('',3,(#58856,#58857,#58858,#58859,#58860,
#58861),.UNSPECIFIED.,.F.,.F.,(4,2,4),(4.98634138348218E-5,0.195141037972379,
0.330493201196748),.UNSPECIFIED.);
#860=B_SPLINE_CURVE_WITH_KNOTS('',3,(#58862,#58863,#58864,#58865,#58866,
#58867),.UNSPECIFIED.,.F.,.F.,(4,2,4),(4.57542679217533E-12,0.0801871578090029,
0.134385019693337),.UNSPECIFIED.);
#861=B_SPLINE_CURVE_WITH_KNOTS('',3,(#58924,#58925,#58926,#58927,#58928,
#58929,#58930,#58931,#58932,#58933,#58934,#58935,#58936,#58937),
 .UNSPECIFIED.,.F.,.F.,(4,2,2,2,2,2,4),(0.0377143719414213,0.167070624995476,
0.336553194126115,0.499999999999991,0.663446805873868,0.832929375004528,
0.962285628058582),.UNSPECIFIED.);
#862=B_SPLINE_CURVE_WITH_KNOTS('',3,(#59597,#59598,#59599,#59600,#59601,
#59602,#59603,#59604),.UNSPECIFIED.,.F.,.F.,(4,2,2,4),(1.07065022399325E-5,
0.0820415500405752,0.124395055584087,0.162715337467435),.UNSPECIFIED.);
#863=B_SPLINE_CURVE_WITH_KNOTS('',3,(#59606,#59607,#59608,#59609,#59610,
#59611,#59612,#59613,#59614,#59615),.UNSPECIFIED.,.F.,.F.,(4,2,2,2,4),(1.00134536322123E-6,
0.18222044597792,0.367842106932836,0.465703496956847,0.525884883424001),
 .UNSPECIFIED.);
#864=B_SPLINE_CURVE_WITH_KNOTS('',3,(#59617,#59618,#59619,#59620,#59621,
#59622,#59623,#59624,#59625,#59626,#59627,#59628,#59629,#59630),
 .UNSPECIFIED.,.F.,.F.,(4,2,2,2,2,2,4),(-1.35506345253935,-1.08840531341759,
-0.865944635772675,-0.676279073046853,-0.487277090549597,-0.263087864621955,
-1.00017583849435E-6),.UNSPECIFIED.);
#865=B_SPLINE_CURVE_WITH_KNOTS('',3,(#59632,#59633,#59634,#59635,#59636,
#59637),.UNSPECIFIED.,.F.,.F.,(4,2,4),(5.3962766046209E-5,0.108969967890436,
0.182584633205874),.UNSPECIFIED.);
#866=B_SPLINE_CURVE_WITH_KNOTS('',3,(#59638,#59639,#59640,#59641,#59642,
#59643),.UNSPECIFIED.,.F.,.F.,(4,2,4),(5.22653476197789E-12,0.0811239424511172,
0.11375725969146),.UNSPECIFIED.);
#867=B_SPLINE_CURVE_WITH_KNOTS('',3,(#60213,#60214,#60215,#60216,#60217,
#60218,#60219,#60220,#60221,#60222,#60223,#60224,#60225,#60226),
 .UNSPECIFIED.,.F.,.F.,(4,2,2,2,2,2,4),(0.0377143719414213,0.167070624995476,
0.336553194126115,0.499999999999991,0.663446805873868,0.832929375004528,
0.962285628058582),.UNSPECIFIED.);
#868=B_SPLINE_CURVE_WITH_KNOTS('',3,(#60228,#60229,#60230,#60231,#60232,
#60233,#60234,#60235),.UNSPECIFIED.,.F.,.F.,(4,2,2,4),(3.79993615621598E-5,
0.0820948071540982,0.159782168454658,0.163590605624764),.UNSPECIFIED.);
#869=B_SPLINE_CURVE_WITH_KNOTS('',3,(#60237,#60238,#60239,#60240,#60241,
#60242),.UNSPECIFIED.,.F.,.F.,(4,2,4),(1.00680304406573E-6,0.198371116469636,
0.616016616729024),.UNSPECIFIED.);
#870=B_SPLINE_CURVE_WITH_KNOTS('',3,(#60244,#60245,#60246,#60247,#60248,
#60249,#60250,#60251,#60252,#60253,#60254,#60255,#60256,#60257),
 .UNSPECIFIED.,.F.,.F.,(4,2,2,2,2,2,4),(-1.36946791051543,-1.09994504179602,
-0.874839555222837,-0.68308307358568,-0.492006341135471,-0.26527826440027,
-1.0003275292482E-6),.UNSPECIFIED.);
#871=B_SPLINE_CURVE_WITH_KNOTS('',3,(#60259,#60260,#60261,#60262,#60263,
#60264),.UNSPECIFIED.,.F.,.F.,(4,2,4),(9.21025416984816E-6,0.201412302234187,
0.34337647011839),.UNSPECIFIED.);
#872=B_SPLINE_CURVE_WITH_KNOTS('',3,(#60265,#60266,#60267,#60268,#60269,
#60270),.UNSPECIFIED.,.F.,.F.,(4,2,4),(1.74012010253697E-12,0.0799694236906792,
0.14961823093418),.UNSPECIFIED.);
#873=B_SPLINE_CURVE_WITH_KNOTS('',3,(#60327,#60328,#60329,#60330,#60331,
#60332,#60333,#60334,#60335,#60336,#60337,#60338,#60339,#60340),
 .UNSPECIFIED.,.F.,.F.,(4,2,2,2,2,2,4),(0.0377143719414213,0.167070624995476,
0.336553194126115,0.499999999999991,0.663446805873868,0.832929375004528,
0.962285628058582),.UNSPECIFIED.);
#874=B_SPLINE_CURVE_WITH_KNOTS('',3,(#60706,#60707,#60708,#60709,#60710,
#60711,#60712,#60713),.UNSPECIFIED.,.F.,.F.,(4,2,2,4),(0.000198665912013773,
0.0423192231855041,0.0819962999928345,0.222796246729331),.UNSPECIFIED.);
#875=B_SPLINE_CURVE_WITH_KNOTS('',3,(#60715,#60716,#60717,#60718,#60719,
#60720),.UNSPECIFIED.,.F.,.F.,(4,2,4),(1.00678242509254E-6,0.199083168651477,
0.591904491004669),.UNSPECIFIED.);
#876=B_SPLINE_CURVE_WITH_KNOTS('',3,(#60722,#60723,#60724,#60725,#60726,
#60727,#60728,#60729,#60730,#60731,#60732,#60733,#60734,#60735),
 .UNSPECIFIED.,.F.,.F.,(4,2,2,2,2,2,4),(-1.36893350864692,-1.09997929470732,
-0.87490648981194,-0.683305966268589,-0.4923773938272,-0.265638162538616,
-1.00032653094444E-6),.UNSPECIFIED.);
#877=B_SPLINE_CURVE_WITH_KNOTS('',3,(#60737,#60738,#60739,#60740,#60741,
#60742),.UNSPECIFIED.,.F.,.F.,(4,2,4),(6.74092780132926E-5,0.30785071191309,
0.598735524338827),.UNSPECIFIED.);
#878=B_SPLINE_CURVE_WITH_KNOTS('',3,(#60743,#60744,#60745,#60746,#60747,
#60748,#60749,#60750),.UNSPECIFIED.,.F.,.F.,(4,2,2,4),(6.87557743431209E-14,
0.0811979885087478,0.125523813671698,0.201873086677692),.UNSPECIFIED.);
#879=B_SPLINE_CURVE_WITH_KNOTS('',3,(#60755,#60756,#60757,#60758,#60759,
#60760,#60761,#60762,#60763,#60764),.UNSPECIFIED.,.F.,.F.,(4,2,2,2,4),(0.,
0.0285072227353245,0.0532892290060001,0.0661103821512685,0.0936902631120297),
 .UNSPECIFIED.);
#880=B_SPLINE_CURVE_WITH_KNOTS('',3,(#61277,#61278,#61279,#61280,#61281,
#61282,#61283,#61284,#61285,#61286,#61287,#61288,#61289,#61290),
 .UNSPECIFIED.,.F.,.F.,(4,2,2,2,2,2,4),(0.0377143719414213,0.167070624995476,
0.336553194126115,0.499999999999991,0.663446805873868,0.832929375004528,
0.962285628058582),.UNSPECIFIED.);
#881=B_SPLINE_CURVE_WITH_KNOTS('',3,(#61292,#61293,#61294,#61295,#61296,
#61297,#61298,#61299),.UNSPECIFIED.,.F.,.F.,(4,2,2,4),(8.2068747900806E-5,
0.0736236603178404,0.133996054723513,0.219980728701435),.UNSPECIFIED.);
#882=B_SPLINE_CURVE_WITH_KNOTS('',3,(#61301,#61302,#61303,#61304,#61305,
#61306),.UNSPECIFIED.,.F.,.F.,(4,2,4),(1.00672590815621E-6,0.199031231385238,
0.613338043951791),.UNSPECIFIED.);
#883=B_SPLINE_CURVE_WITH_KNOTS('',3,(#61308,#61309,#61310,#61311,#61312,
#61313,#61314,#61315,#61316,#61317,#61318,#61319,#61320,#61321),
 .UNSPECIFIED.,.F.,.F.,(4,2,2,2,2,2,4),(-1.36940170500402,-1.09988295614753,
-0.874791882030613,-0.683052425013262,-0.491992883634759,-0.265273198644392,
-1.00032379802467E-6),.UNSPECIFIED.);
#884=B_SPLINE_CURVE_WITH_KNOTS('',3,(#61322,#61323,#61324,#61325,#61326,
#61327),.UNSPECIFIED.,.F.,.F.,(4,2,4),(2.55717115154207E-6,0.198998134710777,
0.338859911257635),.UNSPECIFIED.);
#885=B_SPLINE_CURVE_WITH_KNOTS('',3,(#61384,#61385,#61386,#61387,#61388,
#61389,#61390,#61391,#61392,#61393,#61394,#61395,#61396,#61397),
 .UNSPECIFIED.,.F.,.F.,(4,2,2,2,2,2,4),(0.0377143719414213,0.167070624995476,
0.336553194126115,0.499999999999991,0.663446805873868,0.832929375004528,
0.962285628058582),.UNSPECIFIED.);
#886=B_SPLINE_CURVE_WITH_KNOTS('',3,(#62043,#62044,#62045,#62046,#62047,
#62048),.UNSPECIFIED.,.F.,.F.,(4,2,4),(2.35124835048059E-5,0.0896951576367538,
0.182831089214791),.UNSPECIFIED.);
#887=B_SPLINE_CURVE_WITH_KNOTS('',3,(#62050,#62051,#62052,#62053,#62054,
#62055),.UNSPECIFIED.,.F.,.F.,(4,2,4),(1.00039620620053E-6,0.178978044961171,
0.576833929771009),.UNSPECIFIED.);
#888=B_SPLINE_CURVE_WITH_KNOTS('',3,(#62057,#62058,#62059,#62060,#62061,
#62062,#62063,#62064,#62065,#62066,#62067,#62068,#62069,#62070),
 .UNSPECIFIED.,.F.,.F.,(4,2,2,2,2,2,4),(-1.35020638398027,-1.08443693237292,
-0.862819012108596,-0.674058735997087,-0.48593035055054,-0.262536029678697,
-1.00008876609848E-6),.UNSPECIFIED.);
#889=B_SPLINE_CURVE_WITH_KNOTS('',3,(#62072,#62073,#62074,#62075,#62076,
#62077),.UNSPECIFIED.,.F.,.F.,(4,2,4),(4.60565042976658E-5,0.201020831894536,
0.382076214067163),.UNSPECIFIED.);
#890=B_SPLINE_CURVE_WITH_KNOTS('',3,(#62078,#62079,#62080,#62081,#62082,
#62083),.UNSPECIFIED.,.F.,.F.,(4,2,4),(0.,0.0817717936353896,0.122657946516836),
 .UNSPECIFIED.);
#891=B_SPLINE_CURVE_WITH_KNOTS('',3,(#62086,#62087,#62088,#62089,#62090,
#62091),.UNSPECIFIED.,.F.,.F.,(4,2,4),(4.16219211490419E-13,0.0801522498243031,
0.181100777626267),.UNSPECIFIED.);
#892=B_SPLINE_CURVE_WITH_KNOTS('',3,(#62097,#62098,#62099,#62100,#62101,
#62102),.UNSPECIFIED.,.F.,.F.,(4,2,4),(9.76525933546162E-5,0.171030074764551,
0.274312857421989),.UNSPECIFIED.);
#893=B_SPLINE_CURVE_WITH_KNOTS('',3,(#62529,#62530,#62531,#62532,#62533,
#62534,#62535,#62536,#62537,#62538,#62539,#62540,#62541,#62542),
 .UNSPECIFIED.,.F.,.F.,(4,2,2,2,2,2,4),(0.0377143719414213,0.167070624995476,
0.336553194126115,0.499999999999991,0.663446805873868,0.832929375004528,
0.962285628058582),.UNSPECIFIED.);
#894=B_SPLINE_CURVE_WITH_KNOTS('',3,(#62544,#62545,#62546,#62547,#62548,
#62549),.UNSPECIFIED.,.F.,.F.,(4,2,4),(3.73183726292144E-5,0.103357039408085,
0.159897599535642),.UNSPECIFIED.);
#895=B_SPLINE_CURVE_WITH_KNOTS('',3,(#62551,#62552,#62553,#62554,#62555,
#62556,#62557,#62558),.UNSPECIFIED.,.F.,.F.,(4,2,2,4),(1.00587379666966E-6,
0.192203020379571,0.269152108519518,0.528949682547937),.UNSPECIFIED.);
#896=B_SPLINE_CURVE_WITH_KNOTS('',3,(#62559,#62560,#62561,#62562,#62563,
#62564,#62565,#62566,#62567,#62568,#62569,#62570,#62571,#62572),
 .UNSPECIFIED.,.F.,.F.,(4,2,2,2,2,2,4),(-1.36643940243578,-1.09802651843964,
-0.87334041482261,-0.68198104582902,-0.491290408247465,-0.264952115802241,
-1.00035096156786E-6),.UNSPECIFIED.);
#897=B_SPLINE_CURVE_WITH_KNOTS('',3,(#62629,#62630,#62631,#62632,#62633,
#62634,#62635,#62636,#62637,#62638,#62639,#62640,#62641,#62642),
 .UNSPECIFIED.,.F.,.F.,(4,2,2,2,2,2,4),(0.0377143719414213,0.167070624995476,
0.336553194126115,0.499999999999991,0.663446805873868,0.832929375004528,
0.962285628058582),.UNSPECIFIED.);
#898=B_SPLINE_CURVE_WITH_KNOTS('',3,(#63261,#63262,#63263,#63264,#63265,
#63266,#63267,#63268,#63269,#63270,#63271,#63272,#63273,#63274,#63275,#63276,
#63277,#63278,#63279,#63280,#63281,#63282,#63283,#63284,#63285,#63286,#63287,
#63288,#63289,#63290,#63291,#63292,#63293,#63294,#63295,#63296,#63297,#63298,
#63299,#63300,#63301,#63302,#63303,#63304,#63305,#63306,#63307,#63308,#63309,
#63310,#63311,#63312,#63313,#63314,#63315,#63316,#63317,#63318,#63319,#63320,
#63321,#63322,#63323,#63324,#63325,#63326,#63327,#63328,#63329,#63330,#63331,
#63332,#63333,#63334,#63335,#63336,#63337,#63338,#63339),.UNSPECIFIED.,
 .F.,.F.,(4,3,3,3,3,3,3,3,3,3,3,3,3,3,3,3,3,3,3,3,3,3,3,3,3,3,4),(10.3769577827544,
10.5273598900866,10.6774945443399,10.8308192114618,10.9808890436316,11.1358411282296,
11.2907932128275,11.4445181516619,11.5979719285541,11.7512647292242,11.9046292861554,
12.0580308496751,12.211755396569,12.284929466409,12.4385133838143,12.5918292435621,
12.7449877126714,12.8982250015488,13.0515031898628,13.2051123582851,13.2790657199904,
13.432297699739,13.5852451018772,13.7380996304701,13.8908875290217,14.0438933465584,
14.1577916878073),.UNSPECIFIED.);
#899=B_SPLINE_CURVE_WITH_KNOTS('',3,(#63342,#63343,#63344,#63345,#63346,
#63347,#63348,#63349,#63350,#63351,#63352,#63353,#63354,#63355,#63356,#63357,
#63358,#63359,#63360,#63361,#63362,#63363,#63364,#63365,#63366,#63367,#63368,
#63369,#63370,#63371,#63372,#63373,#63374,#63375,#63376,#63377,#63378,#63379,
#63380,#63381,#63382,#63383,#63384,#63385,#63386,#63387,#63388,#63389,#63390,
#63391,#63392,#63393,#63394,#63395,#63396),.UNSPECIFIED.,.F.,.F.,(4,3,3,
3,3,3,3,3,3,3,3,3,3,3,3,3,3,3,4),(11.6150328478183,11.7926764189461,11.9701488858192,
12.112100974609,12.2661530434337,12.4201862996183,12.5744137841679,12.6091691013998,
12.7645204088578,12.919681016886,13.0747528344925,13.2299786470436,13.3852896170894,
13.5409644760237,13.6033053549812,13.7553480979553,13.9070954748021,14.0586995150233,
14.1583240782391),.UNSPECIFIED.);
#900=B_SPLINE_CURVE_WITH_KNOTS('',3,(#63402,#63403,#63404,#63405,#63406,
#63407,#63408,#63409,#63410,#63411,#63412,#63413,#63414,#63415,#63416,#63417,
#63418,#63419,#63420,#63421,#63422,#63423,#63424,#63425,#63426,#63427,#63428,
#63429,#63430,#63431,#63432,#63433,#63434,#63435,#63436,#63437,#63438,#63439,
#63440,#63441,#63442,#63443,#63444,#63445,#63446,#63447,#63448,#63449,#63450,
#63451,#63452,#63453,#63454,#63455,#63456,#63457,#63458,#63459,#63460,#63461,
#63462,#63463,#63464,#63465,#63466,#63467,#63468,#63469,#63470,#63471,#63472,
#63473,#63474,#63475,#63476,#63477,#63478,#63479,#63480,#63481,#63482,#63483,
#63484,#63485,#63486,#63487,#63488,#63489,#63490,#63491,#63492,#63493,#63494,
#63495,#63496,#63497,#63498,#63499,#63500,#63501,#63502,#63503,#63504),
 .UNSPECIFIED.,.F.,.F.,(4,3,3,3,3,3,3,3,3,3,3,3,3,3,3,3,3,3,3,3,3,3,3,3,
3,3,3,3,3,3,3,3,3,3,4),(15.7079632679489,15.8650809592317,16.0223560154779,
16.180095481684,16.2614744807347,16.414856728946,16.5679648062975,16.7209100993148,
16.8739286197668,17.0269845627285,17.1803695780412,17.2556107343161,17.4090275970834,
17.5621709487349,17.7151520567367,17.8682067844267,18.021299206932,18.1747205540646,
18.2497469878976,18.4031557793674,18.5562910052633,18.7092639603358,18.8623105909142,
19.0153949374731,19.1688083680783,19.243883241479,19.3972872546799,19.5504175546535,
19.703385452925,19.8564268889446,20.0095059553496,20.1629140554059,20.2380194950604,
20.3914408227308,20.4420478592521),.UNSPECIFIED.);
#901=B_SPLINE_CURVE_WITH_KNOTS('',3,(#63505,#63506,#63507,#63508,#63509,
#63510,#63511,#63512,#63513,#63514,#63515,#63516,#63517,#63518,#63519,#63520,
#63521,#63522,#63523,#63524,#63525,#63526,#63527,#63528,#63529,#63530,#63531,
#63532,#63533,#63534,#63535,#63536,#63537,#63538),.UNSPECIFIED.,.F.,.F.,
(4,3,3,3,3,3,3,3,3,3,3,4),(14.1577916878073,14.2732019735718,14.4266654812486,
14.5798559651052,14.7328845330507,14.8859866502668,15.039126483985,15.1925945327221,
15.2673382271533,15.4330590962838,15.5979020456747,15.7079632678343),
 .UNSPECIFIED.);
#902=B_SPLINE_CURVE_WITH_KNOTS('',3,(#63540,#63541,#63542,#63543,#63544,
#63545,#63546,#63547,#63548,#63549,#63550,#63551,#63552,#63553,#63554,#63555,
#63556,#63557,#63558,#63559,#63560,#63561,#63562,#63563,#63564,#63565,#63566,
#63567,#63568,#63569,#63570,#63571,#63572,#63573),.UNSPECIFIED.,.F.,.F.,
(4,3,3,3,3,3,3,3,3,3,3,4),(14.1583240782391,14.3099489598577,14.4619231331325,
14.5974416085626,14.7511673052192,14.9046218555822,15.05791544251,15.2112807951612,
15.3646831606929,15.5184085065351,15.5915778621441,15.707963267949),
 .UNSPECIFIED.);
#903=B_SPLINE_CURVE_WITH_KNOTS('',3,(#63574,#63575,#63576,#63577,#63578,
#63579,#63580,#63581,#63582,#63583,#63584,#63585,#63586,#63587,#63588,#63589,
#63590,#63591,#63592,#63593,#63594,#63595,#63596,#63597,#63598,#63599,#63600,
#63601,#63602,#63603,#63604,#63605,#63606,#63607,#63608,#63609,#63610,#63611,
#63612,#63613,#63614,#63615,#63616,#63617,#63618,#63619,#63620,#63621,#63622,
#63623,#63624,#63625,#63626,#63627,#63628,#63629,#63630,#63631,#63632,#63633,
#63634,#63635,#63636,#63637,#63638,#63639,#63640,#63641,#63642,#63643,#63644,
#63645,#63646,#63647,#63648,#63649,#63650,#63651,#63652,#63653,#63654,#63655,
#63656,#63657,#63658,#63659,#63660,#63661,#63662,#63663,#63664,#63665,#63666,
#63667,#63668,#63669,#63670,#63671,#63672,#63673),.UNSPECIFIED.,.F.,.F.,
(4,3,3,3,3,3,3,3,3,3,3,3,3,3,3,3,3,3,3,3,3,3,3,3,3,3,3,3,3,3,3,3,3,4),(15.7079632680668,
15.8594388736004,16.0106884436182,16.1619521092882,16.3132060736808,16.4647924609641,
16.5857141157255,16.7389389348221,16.8918864719011,17.0446686448837,17.1975220592675,
17.3504115327853,17.5036305542145,17.5798503693069,17.733313923022,17.886504454532,
18.0395330715724,18.1926352394518,18.3457751247938,18.4992432258178,18.5739866228884,
18.7274115805076,18.8805635511898,19.033553772357,19.1866182515782,19.3397208031865,
19.4931527076817,19.5681228764698,19.7215125444031,19.8746204229269,20.0276355842012,
20.1805858124463,20.3337471975624,20.4409723240163),.UNSPECIFIED.);
#904=B_SPLINE_CURVE_WITH_KNOTS('',3,(#63679,#63680,#63681,#63682,#63683,
#63684,#63685,#63686,#63687,#63688,#63689,#63690,#63691,#63692,#63693,#63694,
#63695,#63696,#63697,#63698,#63699,#63700,#63701,#63702,#63703,#63704,#63705,
#63706,#63707,#63708,#63709,#63710,#63711,#63712,#63713,#63714,#63715,#63716,
#63717,#63718,#63719,#63720,#63721,#63722,#63723,#63724,#63725,#63726,#63727,
#63728,#63729,#63730,#63731,#63732,#63733,#63734,#63735,#63736,#63737,#63738,
#63739,#63740,#63741,#63742,#63743,#63744,#63745,#63746,#63747,#63748,#63749,
#63750,#63751,#63752,#63753,#63754,#63755,#63756,#63757,#63758,#63759,#63760,
#63761,#63762,#63763,#63764,#63765,#63766,#63767,#63768,#63769,#63770,#63771,
#63772,#63773,#63774,#63775,#63776,#63777,#63778,#63779,#63780,#63781),
 .UNSPECIFIED.,.F.,.F.,(4,3,3,3,3,3,3,3,3,3,3,3,3,3,3,3,3,3,3,3,3,3,3,3,
3,3,3,3,3,3,3,3,3,3,4),(21.99114857526,22.1939267919493,22.2262920022233,
22.3796989418416,22.5328322331403,22.6858031775158,22.838847706263,22.9919298961389,
23.145341118553,23.2204282558048,23.3738358680276,23.5269698461768,23.6799414893234,
23.8329867265599,23.9860696314175,24.13948156771,24.2145645093862,24.3679718714795,
24.5211055961752,24.6740769833984,24.827121964018,24.9802046115219,25.1336162933461,
25.2087007629676,25.3621080840594,25.5152417657962,25.6682131082504,25.8212580418961,
25.9743406411039,26.127752273332,26.2028370165491,26.3562428141984,26.5093760788686,
26.662367028694,26.7245753429587),.UNSPECIFIED.);
#905=B_SPLINE_CURVE_WITH_KNOTS('',3,(#63782,#63783,#63784,#63785,#63786,
#63787,#63788,#63789,#63790,#63791,#63792,#63793,#63794,#63795,#63796,#63797,
#63798,#63799,#63800,#63801,#63802,#63803,#63804,#63805,#63806,#63807,#63808,
#63809,#63810,#63811,#63812,#63813,#63814,#63815),.UNSPECIFIED.,.F.,.F.,
(4,3,3,3,3,3,3,3,3,3,3,4),(20.4420478592521,20.5951172325546,20.7543768615764,
20.9074258209389,21.0605493555233,21.2139862899396,21.2321557486419,21.3836611788031,
21.5355330278844,21.6866431849307,21.8388958800296,21.9911485751285),
 .UNSPECIFIED.);
#906=B_SPLINE_CURVE_WITH_KNOTS('',3,(#63817,#63818,#63819,#63820,#63821,
#63822,#63823,#63824,#63825,#63826,#63827,#63828,#63829,#63830,#63831,#63832,
#63833,#63834,#63835,#63836,#63837,#63838,#63839,#63840,#63841,#63842,#63843,
#63844,#63845,#63846,#63847,#63848,#63849,#63850),.UNSPECIFIED.,.F.,.F.,
(4,3,3,3,3,3,3,3,3,3,3,4),(20.4409723240163,20.5622591300512,20.7156759866491,
20.8688193321945,21.0218004341724,21.1748551560304,21.3279475728055,21.4813689144523,
21.5563953836327,21.7227148730573,21.8881132512756,21.9911485750061),
 .UNSPECIFIED.);
#907=B_SPLINE_CURVE_WITH_KNOTS('',3,(#63851,#63852,#63853,#63854,#63855,
#63856,#63857,#63858,#63859,#63860,#63861,#63862,#63863,#63864,#63865,#63866,
#63867,#63868,#63869,#63870,#63871,#63872,#63873,#63874,#63875,#63876,#63877,
#63878,#63879,#63880,#63881,#63882,#63883,#63884,#63885,#63886,#63887,#63888,
#63889,#63890,#63891,#63892,#63893,#63894,#63895,#63896,#63897,#63898,#63899,
#63900,#63901,#63902,#63903,#63904,#63905,#63906,#63907,#63908,#63909,#63910,
#63911,#63912,#63913,#63914,#63915,#63916,#63917,#63918,#63919,#63920,#63921,
#63922,#63923,#63924,#63925,#63926,#63927,#63928,#63929,#63930,#63931,#63932,
#63933,#63934,#63935,#63936,#63937,#63938,#63939,#63940,#63941,#63942,#63943,
#63944,#63945,#63946,#63947,#63948,#63949,#63950,#63951,#63952,#63953),
 .UNSPECIFIED.,.F.,.F.,(4,3,3,3,3,3,3,3,3,3,3,3,3,3,3,3,3,3,3,3,3,3,3,3,
3,3,3,3,3,3,3,3,3,3,4),(21.9911485751285,22.1479256648879,22.3048452391874,
22.462221546967,22.5505316372141,22.703935658999,22.8570659677062,23.0100338748324,
23.1630753197854,23.3161543951809,23.469562504177,23.5446678907956,23.6980767887443,
23.8512120717938,24.0041850346144,24.1572315981784,24.3103158349244,24.4637290908905,
24.538804144377,24.6922115651092,24.8453453550659,24.9983168139393,25.1513618750143,
25.3044446081105,25.4578563821735,25.5329403979584,25.6863473392698,25.8394806322957,
25.9924515784266,26.145496108951,26.2985783006192,26.4519895248209,26.5270766515399,
26.6804991039507,26.7252324446079),.UNSPECIFIED.);
#908=B_SPLINE_CURVE_WITH_KNOTS('',3,(#63959,#63960,#63961,#63962,#63963,
#63964,#63965,#63966,#63967,#63968,#63969,#63970,#63971,#63972,#63973,#63974,
#63975,#63976,#63977,#63978,#63979,#63980,#63981,#63982,#63983,#63984,#63985,
#63986,#63987,#63988,#63989,#63990,#63991,#63992,#63993,#63994,#63995,#63996,
#63997,#63998,#63999,#64000,#64001,#64002,#64003,#64004,#64005,#64006,#64007,
#64008,#64009,#64010,#64011,#64012,#64013,#64014,#64015,#64016,#64017,#64018,
#64019,#64020,#64021,#64022,#64023,#64024,#64025,#64026,#64027,#64028,#64029,
#64030,#64031,#64032,#64033,#64034,#64035,#64036,#64037,#64038,#64039,#64040,
#64041,#64042,#64043,#64044,#64045,#64046,#64047,#64048,#64049,#64050,#64051,
#64052,#64053,#64054,#64055,#64056,#64057,#64058),.UNSPECIFIED.,.F.,.F.,
(4,3,3,3,3,3,3,3,3,3,3,3,3,3,3,3,3,3,3,3,3,3,3,3,3,3,3,3,3,3,3,3,3,4),(28.2743338824354,
28.4259808413042,28.5773785225841,28.7293453362614,28.8807048174512,29.0329752973723,
29.1852457772934,29.3386531544532,29.4917868936077,29.644758294636,29.7978032879121,
29.9508859474332,30.104297640095,30.1793820308748,30.3327894432698,30.4859232177876,
30.6388946541924,30.7919396824536,30.9450223767831,31.0984341034409,31.1735182844562,
31.3269256011464,31.480059280071,31.6330306212942,31.7860755560757,31.9391581577712,
32.0925697945182,32.1676545380377,32.3210720983193,32.4742063232938,32.6272330512433,
32.7801943527862,32.9333288292476,33.0072870494089),.UNSPECIFIED.);
#909=B_SPLINE_CURVE_WITH_KNOTS('',3,(#64059,#64060,#64061,#64062,#64063,
#64064,#64065,#64066,#64067,#64068,#64069,#64070,#64071,#64072,#64073,#64074,
#64075,#64076,#64077,#64078,#64079,#64080,#64081,#64082,#64083,#64084,#64085,
#64086,#64087,#64088,#64089,#64090,#64091,#64092),.UNSPECIFIED.,.F.,.F.,
(4,3,3,3,3,3,3,3,3,3,3,4),(26.7245753429587,26.8776236986561,27.0372984843933,
27.1969732701305,27.3503806471368,27.5035143861932,27.6564857871786,27.8095307804943,
27.9626134401022,28.1160251329216,28.1911095237119,28.2743338823081),
 .UNSPECIFIED.);
#910=B_SPLINE_CURVE_WITH_KNOTS('',3,(#64094,#64095,#64096,#64097,#64098,
#64099,#64100,#64101,#64102,#64103,#64104,#64105,#64106,#64107,#64108,#64109,
#64110,#64111,#64112,#64113,#64114,#64115,#64116,#64117,#64118,#64119,#64120,
#64121,#64122,#64123,#64124,#64125,#64126,#64127),.UNSPECIFIED.,.F.,.F.,
(4,3,3,3,3,3,3,3,3,3,3,4),(26.7252324446079,26.8783075285994,27.0390338727299,
27.1920808254545,27.3451994950597,27.498632670491,27.5212129051213,27.672785837319,
27.8241164256345,27.9752896314244,28.1265899278275,28.2743338823081),
 .UNSPECIFIED.);
#911=B_SPLINE_CURVE_WITH_KNOTS('',3,(#64128,#64129,#64130,#64131,#64132,
#64133,#64134,#64135,#64136,#64137,#64138,#64139,#64140,#64141,#64142,#64143,
#64144,#64145,#64146,#64147,#64148,#64149,#64150,#64151,#64152,#64153,#64154,
#64155,#64156,#64157,#64158,#64159,#64160,#64161,#64162,#64163,#64164,#64165,
#64166,#64167,#64168,#64169,#64170,#64171,#64172,#64173,#64174,#64175,#64176,
#64177,#64178,#64179,#64180,#64181,#64182,#64183,#64184,#64185,#64186,#64187,
#64188,#64189,#64190,#64191,#64192,#64193,#64194,#64195,#64196,#64197,#64198,
#64199,#64200,#64201,#64202,#64203,#64204,#64205,#64206,#64207,#64208,#64209,
#64210,#64211,#64212,#64213,#64214,#64215,#64216,#64217,#64218,#64219,#64220,
#64221,#64222,#64223,#64224,#64225,#64226,#64227,#64228,#64229,#64230),
 .UNSPECIFIED.,.F.,.F.,(4,3,3,3,3,3,3,3,3,3,3,3,3,3,3,3,3,3,3,3,3,3,3,3,
3,3,3,3,3,3,3,3,3,3,4),(28.2743338824879,28.4750398536421,28.5153491587027,
28.6687564800878,28.8218901621242,28.9748615048833,29.1279064388382,29.2809890383584,
29.4344006708985,29.5094854122842,29.6628928231069,29.8160265965599,29.9689980324053,
30.1220430608655,30.2751257558269,30.4285374837698,30.5036216658656,30.6570290428525,
30.810162781889,30.9631341828541,31.1161791761489,31.2692618357356,31.4226735285337,
31.497757919447,31.651165282527,31.8042990074916,31.9572703942643,32.1103153733462,
32.2633980186889,32.4168096974117,32.4918941730285,32.6453002476881,32.7984336411736,
32.9514213448994,33.0077784099125),.UNSPECIFIED.);
#912=B_SPLINE_CURVE_WITH_KNOTS('',3,(#64236,#64237,#64238,#64239,#64240,
#64241,#64242,#64243,#64244,#64245,#64246,#64247,#64248,#64249,#64250,#64251,
#64252,#64253,#64254,#64255,#64256,#64257,#64258,#64259,#64260,#64261,#64262,
#64263,#64264,#64265,#64266,#64267,#64268,#64269,#64270,#64271,#64272,#64273,
#64274,#64275,#64276,#64277,#64278,#64279,#64280,#64281,#64282,#64283,#64284,
#64285,#64286,#64287,#64288,#64289,#64290,#64291,#64292,#64293,#64294,#64295,
#64296,#64297,#64298,#64299,#64300,#64301,#64302,#64303,#64304,#64305,#64306,
#64307,#64308,#64309,#64310,#64311,#64312,#64313,#64314,#64315,#64316,#64317,
#64318,#64319,#64320,#64321,#64322,#64323,#64324,#64325,#64326,#64327,#64328,
#64329,#64330,#64331,#64332,#64333,#64334,#64335,#64336,#64337,#64338),
 .UNSPECIFIED.,.F.,.F.,(4,3,3,3,3,3,3,3,3,3,3,3,3,3,3,3,3,3,3,3,3,3,3,3,
3,3,3,3,3,3,3,3,3,3,4),(34.5575191894877,34.7128109395726,34.8681775956844,
35.0239713658574,35.150063298782,35.3034707576981,35.456604572422,35.6095760427116,
35.762621095208,35.915703808308,36.0691155452003,36.1441995523634,36.2976084936062,
36.4507438054633,36.6037167826695,36.7567633389953,36.9098475561584,37.0632607739405,
37.1383358059449,37.291739596941,37.4448697549461,37.5978375910733,37.7508790844318,
37.9039582764099,38.0573666045902,38.1324720595263,38.2858811685694,38.4390165973614,
38.5919896412426,38.745036189863,38.8981203569408,39.0515334615024,39.1266083131077,
39.2800571769567,39.2915821620202),.UNSPECIFIED.);
#913=B_SPLINE_CURVE_WITH_KNOTS('',3,(#64339,#64340,#64341,#64342,#64343,
#64344,#64345,#64346,#64347,#64348,#64349,#64350,#64351,#64352,#64353,#64354,
#64355,#64356,#64357,#64358,#64359,#64360,#64361,#64362,#64363,#64364,#64365,
#64366,#64367,#64368,#64369,#64370,#64371,#64372),.UNSPECIFIED.,.F.,.F.,
(4,3,3,3,3,3,3,3,3,3,3,4),(33.0072870494089,33.1617907916191,33.3151984118971,
33.4683323951928,33.6213040405922,33.77434927575,33.9274321760551,34.0808441040777,
34.1559270452005,34.3257930361133,34.4944769778812,34.5575191893185),
 .UNSPECIFIED.);
#914=B_SPLINE_CURVE_WITH_KNOTS('',3,(#64374,#64375,#64376,#64377,#64378,
#64379,#64380,#64381,#64382,#64383,#64384,#64385,#64386,#64387,#64388,#64389,
#64390,#64391,#64392,#64393,#64394,#64395,#64396,#64397,#64398,#64399,#64400,
#64401,#64402,#64403,#64404,#64405,#64406,#64407,#64408,#64409,#64410),
 .UNSPECIFIED.,.F.,.F.,(4,3,3,3,3,3,3,3,3,3,3,3,4),(33.0077784099125,33.1608257171148,
33.3139472904311,33.4673823924497,33.4860304266099,33.6394378388404,33.7925716131929,
33.9455430494321,34.098588077529,34.2516707716947,34.4050824981922,34.4801666801914,
34.5575191894877),.UNSPECIFIED.);
#915=B_SPLINE_CURVE_WITH_KNOTS('',3,(#64411,#64412,#64413,#64414,#64415,
#64416,#64417,#64418,#64419,#64420,#64421,#64422,#64423,#64424,#64425,#64426,
#64427,#64428,#64429,#64430,#64431,#64432,#64433,#64434,#64435,#64436,#64437,
#64438,#64439,#64440,#64441,#64442,#64443,#64444,#64445,#64446,#64447,#64448,
#64449,#64450,#64451,#64452,#64453,#64454,#64455,#64456,#64457,#64458,#64459,
#64460,#64461,#64462,#64463,#64464,#64465,#64466,#64467,#64468,#64469,#64470,
#64471,#64472,#64473,#64474,#64475,#64476,#64477,#64478,#64479,#64480,#64481,
#64482,#64483,#64484,#64485,#64486,#64487,#64488,#64489,#64490,#64491,#64492,
#64493,#64494,#64495,#64496,#64497,#64498,#64499,#64500,#64501,#64502,#64503,
#64504,#64505,#64506,#64507,#64508,#64509,#64510),.UNSPECIFIED.,.F.,.F.,
(4,3,3,3,3,3,3,3,3,3,3,3,3,3,3,3,3,3,3,3,3,3,3,3,3,3,3,3,3,3,3,3,3,4),(34.5575191896116,
34.7092547626843,34.8607382426211,35.014129415409,35.165569538894,35.3199362363334,
35.4743029337728,35.6277102998244,35.7808440270258,35.9338154153095,36.0868603948273,
36.2399430399945,36.3933547176269,36.4684391873542,36.6218468068268,36.7749807893111,
36.9279524338957,37.0809976682432,37.2340805677396,37.3874924949681,37.4625754409357,
37.6159823503777,37.7691156230423,37.9220865602605,38.0751310990094,38.2282133086885,
38.3816245656092,38.4567116945171,38.610129889132,38.7632643739221,38.916288756662,
39.0692475637796,39.2223732435226,39.2904651979605),.UNSPECIFIED.);
#916=B_SPLINE_CURVE_WITH_KNOTS('',3,(#64516,#64517,#64518,#64519,#64520,
#64521,#64522,#64523,#64524,#64525,#64526,#64527,#64528,#64529,#64530,#64531,
#64532,#64533,#64534,#64535,#64536,#64537,#64538,#64539,#64540,#64541,#64542,
#64543,#64544,#64545,#64546,#64547,#64548,#64549,#64550,#64551,#64552,#64553,
#64554,#64555,#64556,#64557,#64558,#64559,#64560,#64561,#64562,#64563,#64564,
#64565,#64566,#64567,#64568,#64569,#64570,#64571,#64572,#64573,#64574,#64575,
#64576,#64577,#64578,#64579,#64580,#64581,#64582,#64583,#64584,#64585,#64586,
#64587,#64588,#64589,#64590,#64591,#64592,#64593,#64594,#64595,#64596,#64597,
#64598,#64599,#64600,#64601,#64602,#64603,#64604,#64605,#64606,#64607,#64608,
#64609,#64610,#64611,#64612,#64613,#64614,#64615,#64616,#64617,#64618),
 .UNSPECIFIED.,.F.,.F.,(4,3,3,3,3,3,3,3,3,3,3,3,3,3,3,3,3,3,3,3,3,3,3,3,
3,3,3,3,3,3,3,3,3,3,4),(40.840704496861,41.0315513197139,41.1148808202706,
41.2683084070192,41.4214620763041,41.5744530701636,41.727516935667,41.8806180818076,
42.0340473903573,42.109017073852,42.2624807464789,42.4156713357008,42.5686999497321,
42.7218020243238,42.8749417647447,43.0284096440709,43.1031533274335,43.256368374023,
43.4093096679249,43.5620891086826,43.714945049858,43.8678400512264,44.021069118693,
44.0972895810149,44.2508939544776,44.404222874785,44.5573870466767,44.7106190333205,
44.8638856297818,45.0174737708723,45.0914258345964,45.2451470488387,45.3985988150857,
45.5518916188261,45.5743044775645),.UNSPECIFIED.);
#917=B_SPLINE_CURVE_WITH_KNOTS('',3,(#64619,#64620,#64621,#64622,#64623,
#64624,#64625,#64626,#64627,#64628,#64629,#64630,#64631,#64632,#64633,#64634,
#64635,#64636,#64637,#64638,#64639,#64640,#64641,#64642,#64643,#64644,#64645,
#64646,#64647,#64648,#64649,#64650,#64651,#64652),.UNSPECIFIED.,.F.,.F.,
(4,3,3,3,3,3,3,3,3,3,3,4),(39.2915821620202,39.4447095027457,39.5976829127759,
39.7507369759808,39.9038361708233,40.0572607936133,40.1207445666892,40.2727807639225,
40.4245502282633,40.5761563774086,40.7278367229112,40.8407044966673),
 .UNSPECIFIED.);
#918=B_SPLINE_CURVE_WITH_KNOTS('',3,(#64654,#64655,#64656,#64657,#64658,
#64659,#64660,#64661,#64662,#64663,#64664,#64665,#64666,#64667,#64668,#64669,
#64670,#64671,#64672,#64673,#64674,#64675,#64676,#64677,#64678,#64679,#64680,
#64681,#64682,#64683,#64684,#64685,#64686,#64687),.UNSPECIFIED.,.F.,.F.,
(4,3,3,3,3,3,3,3,3,3,3,4),(39.2904651979605,39.4508479480985,39.6042568862644,
39.7573921950086,39.910365169076,40.0634117222608,40.2164959362774,40.3699091509537,
40.44498420168,40.6155411212441,40.7848606623605,40.8407044964945),
 .UNSPECIFIED.);
#919=B_SPLINE_CURVE_WITH_KNOTS('',3,(#64688,#64689,#64690,#64691,#64692,
#64693,#64694,#64695,#64696,#64697,#64698,#64699,#64700,#64701,#64702,#64703,
#64704,#64705,#64706,#64707,#64708,#64709,#64710,#64711,#64712,#64713,#64714,
#64715,#64716,#64717,#64718,#64719,#64720,#64721,#64722,#64723,#64724,#64725,
#64726,#64727,#64728,#64729,#64730,#64731,#64732,#64733,#64734,#64735,#64736,
#64737,#64738,#64739,#64740,#64741,#64742,#64743,#64744,#64745,#64746,#64747,
#64748,#64749,#64750,#64751,#64752,#64753,#64754,#64755,#64756,#64757,#64758,
#64759,#64760,#64761,#64762,#64763,#64764,#64765,#64766,#64767,#64768,#64769,
#64770,#64771,#64772,#64773,#64774,#64775,#64776,#64777,#64778,#64779,#64780,
#64781,#64782,#64783,#64784,#64785,#64786,#64787),.UNSPECIFIED.,.F.,.F.,
(4,3,3,3,3,3,3,3,3,3,3,3,3,3,3,3,3,3,3,3,3,3,3,3,3,3,3,3,3,3,3,3,3,4),(40.8407044966673,
40.9957591292645,41.1508780734467,41.3064201957631,41.4391204552614,41.5925295553931,
41.7456649753238,41.8986380104205,42.0516845504698,42.2047687090867,42.3581818054854,
42.4332567088428,42.5866737227815,42.7398171688485,42.8927983148208,43.0458529960652,
43.1989453239065,43.3523665040073,43.4273929624243,43.5807737407789,43.7338808906567,
43.8868257956909,44.0398447353975,44.19290155861,44.3462881466742,44.4215292160057,
44.5749567504601,44.7281103673692,44.8811013089363,45.0341651228667,45.1872662177759,
45.3406954764042,45.4156654695872,45.5747633669549),.UNSPECIFIED.);
#920=B_SPLINE_CURVE_WITH_KNOTS('',3,(#64791,#64792,#64793,#64794,#64795,
#64796,#64797,#64798,#64799,#64800,#64801,#64802,#64803,#64804,#64805,#64806,
#64807,#64808,#64809,#64810,#64811,#64812,#64813,#64814,#64815,#64816,#64817,
#64818,#64819,#64820,#64821,#64822,#64823,#64824,#64825,#64826,#64827,#64828,
#64829,#64830,#64831,#64832,#64833,#64834,#64835,#64836),.UNSPECIFIED.,
 .F.,.F.,(4,3,3,3,3,3,3,3,3,3,3,3,3,3,3,4),(-4.09293042013064,-3.97654501432575,
-3.82746242150663,-3.67863474659495,-3.5299614831974,-3.38122102744219,
-3.23245410916824,-3.08336698099754,-2.98240876074431,-2.83653578429899,
-2.69091995422318,-2.54545308154322,-2.39991629923551,-2.25433443827349,
-2.10845930416463,-2.06815232264671),.UNSPECIFIED.);
#921=B_SPLINE_CURVE_WITH_KNOTS('',3,(#64840,#64841,#64842,#64843,#64844,
#64845,#64846,#64847,#64848,#64849,#64850,#64851,#64852,#64853,#64854,#64855,
#64856,#64857,#64858,#64859,#64860,#64861,#64862,#64863,#64864),
 .UNSPECIFIED.,.F.,.F.,(4,3,3,3,3,3,3,3,4),(4.32144212904479E-15,0.172314051943978,
0.344469545399341,0.497068126790716,0.646463497421989,0.7958397759613,0.945404528325424,
0.994136253581434,1.11639350868616),.UNSPECIFIED.);
#922=B_SPLINE_CURVE_WITH_KNOTS('',3,(#64866,#64867,#64868,#64869,#64870,
#64871,#64872,#64873,#64874,#64875,#64876,#64877,#64878,#64879,#64880,#64881,
#64882,#64883,#64884,#64885,#64886,#64887,#64888,#64889,#64890,#64891,#64892,
#64893,#64894,#64895,#64896,#64897,#64898,#64899,#64900,#64901,#64902,#64903,
#64904,#64905,#64906,#64907,#64908,#64909,#64910,#64911,#64912,#64913,#64914,
#64915,#64916,#64917,#64918,#64919,#64920,#64921,#64922,#64923,#64924,#64925,
#64926,#64927,#64928,#64929,#64930,#64931,#64932,#64933,#64934,#64935,#64936,
#64937,#64938,#64939,#64940,#64941,#64942,#64943,#64944,#64945,#64946,#64947,
#64948,#64949,#64950,#64951,#64952,#64953,#64954,#64955,#64956,#64957,#64958,
#64959,#64960,#64961,#64962,#64963,#64964,#64965,#64966,#64967,#64968,#64969,
#64970,#64971,#64972,#64973,#64974,#64975,#64976,#64977,#64978,#64979,#64980,
#64981,#64982,#64983,#64984,#64985,#64986,#64987,#64988,#64989,#64990,#64991,
#64992,#64993,#64994,#64995,#64996,#64997,#64998),.UNSPECIFIED.,.F.,.F.,
(4,3,3,3,3,3,3,3,3,3,3,3,3,3,3,3,3,3,3,3,3,3,3,3,3,3,3,3,3,3,3,3,3,3,3,
3,3,3,3,3,3,3,3,3,4),(1.11639350886518,1.26540107529424,1.4142593470189,
1.56320326233909,1.71217655620612,1.8615074690152,1.98827250716287,2.13573320085301,
2.28291060830462,2.42991002969188,2.57695920191632,2.72402208004863,2.87141215415248,
2.98240876074431,3.13149538526514,3.28032540437999,3.42899933538523,3.5777379135382,
3.726501525518,3.87558312345145,3.97654501432575,4.1254948724311,4.27419103796277,
4.4227344671354,4.57134929638097,4.71999277787197,4.86896212241735,4.97068126790718,
5.11928286943791,5.26762208690304,5.41580101787194,5.56404404366028,5.71231106677202,
5.86090261216133,5.96481752148862,6.11365060296603,6.26222531479554,6.41064301553827,
6.55912704817221,6.70763670357741,6.85646952638757,6.95895377507006,7.11967437914505,
7.27955756183248,7.39957853315717),.UNSPECIFIED.);
#923=B_SPLINE_CURVE_WITH_KNOTS('',3,(#65000,#65001,#65002,#65003,#65004,
#65005,#65006,#65007,#65008,#65009),.UNSPECIFIED.,.F.,.F.,(4,1,1,1,1,1,
1,4),(7.39957881586575,7.9530900286515,8.94722628223293,9.94136253581436,
10.9354987893958,11.9296350429772,12.9237712965587,13.6827641230453),
 .UNSPECIFIED.);
#924=B_SPLINE_CURVE_WITH_KNOTS('',3,(#65011,#65012,#65013,#65014,#65015,
#65016,#65017,#65018,#65019,#65020,#65021),.UNSPECIFIED.,.F.,.F.,(4,1,1,
1,1,1,1,1,4),(13.6827641230453,13.9179075501401,14.9120438037215,15.906180057303,
16.9003163108844,17.8944525644659,18.8885888180473,19.8827250716287,19.9659494302249),
 .UNSPECIFIED.);
#925=B_SPLINE_CURVE_WITH_KNOTS('',3,(#65023,#65024,#65025,#65026,#65027,
#65028,#65029,#65030,#65031,#65032),.UNSPECIFIED.,.F.,.F.,(4,1,1,1,1,1,
1,4),(19.9659494302249,20.8768613252102,21.8709975787916,22.865133832373,
23.8592700859545,24.8534063395359,25.8475425931173,26.2491347374045),
 .UNSPECIFIED.);
#926=B_SPLINE_CURVE_WITH_KNOTS('',3,(#65034,#65035,#65036,#65037,#65038,
#65039,#65040,#65041,#65042,#65043),.UNSPECIFIED.,.F.,.F.,(4,1,1,1,1,1,
1,4),(26.2491347374045,26.8416788466988,27.8358151002802,28.8299513538617,
29.8240876074431,30.8182238610245,31.812360114606,32.5323200445841),
 .UNSPECIFIED.);
#927=B_SPLINE_CURVE_WITH_KNOTS('',3,(#65045,#65046,#65047,#65048,#65049,
#65050,#65051,#65052,#65053,#65054,#65055,#65056,#65057,#65058,#65059,#65060,
#65061,#65062,#65063,#65064,#65065,#65066,#65067,#65068,#65069,#65070,#65071,
#65072,#65073,#65074,#65075,#65076,#65077,#65078,#65079,#65080,#65081,#65082,
#65083,#65084,#65085,#65086,#65087,#65088,#65089,#65090,#65091,#65092,#65093,
#65094,#65095,#65096,#65097,#65098,#65099,#65100,#65101,#65102,#65103,#65104,
#65105,#65106,#65107,#65108,#65109,#65110,#65111,#65112,#65113,#65114,#65115,
#65116,#65117,#65118,#65119,#65120,#65121,#65122,#65123,#65124,#65125,#65126,
#65127,#65128,#65129,#65130,#65131,#65132,#65133,#65134,#65135,#65136,#65137,
#65138,#65139,#65140,#65141,#65142,#65143,#65144,#65145,#65146,#65147,#65148,
#65149,#65150,#65151,#65152,#65153,#65154,#65155,#65156,#65157,#65158,#65159,
#65160,#65161,#65162,#65163,#65164,#65165,#65166,#65167,#65168,#65169,#65170,
#65171,#65172,#65173,#65174,#65175,#65176,#65177),.UNSPECIFIED.,.F.,.F.,
(4,3,3,3,3,3,3,3,3,3,3,3,3,3,3,3,3,3,3,3,3,3,3,3,3,3,3,3,3,3,3,3,3,3,3,
3,3,3,3,3,3,3,3,3,4),(32.5323201655523,32.7174086039218,32.8064963681874,
32.9552946125721,33.1038336449076,33.2522149461395,33.4006619248636,33.5491341052137,
33.6979294074392,33.8006326217688,33.9494658632194,34.0980406789765,34.246458427882,
34.3949424236234,34.5434519944777,34.6922846579409,34.7947688753503,34.9433609925112,
35.0916940432564,35.2398701083223,35.3881153077529,35.536387325413,35.6849883028127,
35.7889051289317,35.9378748258775,36.0865838740458,36.235133264314,36.3837435031379,
36.5323764787389,36.681326045038,36.7830413825131,36.9321232017769,37.0809501019115,
37.2296225918539,37.3783622855042,37.5271284470279,37.6762148396121,37.7771776360946,
37.9230522499658,38.0686696788295,38.2141381094229,38.3596761871594,38.5052593174765,
38.6511351639275,38.6910128210415),.UNSPECIFIED.);
#928=B_SPLINE_CURVE_WITH_KNOTS('',3,(#65181,#65182,#65183,#65184,#65185,
#65186,#65187,#65188,#65189,#65190),.UNSPECIFIED.,.F.,.F.,(4,1,1,1,1,1,
1,4),(-40.7595863968389,-40.2625182700482,-39.7654501432575,-38.771313889676,
-37.7771776360946,-36.7830413825131,-35.7889051289317,-35.5088569560286),
 .UNSPECIFIED.);
#929=B_SPLINE_CURVE_WITH_KNOTS('',3,(#65192,#65193,#65194,#65195,#65196,
#65197,#65198,#65199,#65200,#65201),.UNSPECIFIED.,.F.,.F.,(4,1,1,1,1,1,
1,4),(-35.5088569560286,-34.7947688753503,-33.8006326217688,-32.8064963681874,
-31.812360114606,-30.8182238610245,-29.8240876074431,-29.225671648849),
 .UNSPECIFIED.);
#930=B_SPLINE_CURVE_WITH_KNOTS('',3,(#65203,#65204,#65205,#65206,#65207,
#65208,#65209,#65210,#65211,#65212),.UNSPECIFIED.,.F.,.F.,(4,1,1,1,1,1,
1,4),(-29.225671648849,-28.8299513538617,-27.8358151002802,-26.8416788466988,
-25.8475425931173,-24.8534063395359,-23.8592700859545,-22.9424863416694),
 .UNSPECIFIED.);
#931=B_SPLINE_CURVE_WITH_KNOTS('',3,(#65214,#65215,#65216,#65217,#65218,
#65219,#65220,#65221,#65222,#65223,#65224),.UNSPECIFIED.,.F.,.F.,(4,1,1,
1,1,1,1,1,4),(-22.9424863416694,-22.8651338323731,-21.8709975787916,-20.8768613252102,
-19.8827250716287,-18.8885888180473,-17.8944525644659,-16.9003163108844,
-16.6593010344898),.UNSPECIFIED.);
#932=B_SPLINE_CURVE_WITH_KNOTS('',3,(#65226,#65227,#65228,#65229,#65230,
#65231,#65232,#65233,#65234,#65235),.UNSPECIFIED.,.F.,.F.,(4,1,1,1,1,1,
1,4),(-16.6593010344898,-15.906180057303,-14.9120438037215,-13.9179075501401,
-12.9237712965587,-11.9296350429772,-10.9354987893958,-10.3761157273102),
 .UNSPECIFIED.);
#933=B_SPLINE_CURVE_WITH_KNOTS('',3,(#65236,#65237,#65238,#65239,#65240,
#65241,#65242,#65243,#65244,#65245,#65246,#65247,#65248,#65249,#65250,#65251,
#65252,#65253,#65254,#65255,#65256,#65257,#65258,#65259,#65260,#65261,#65262,
#65263,#65264,#65265,#65266,#65267,#65268,#65269,#65270,#65271,#65272,#65273,
#65274,#65275,#65276,#65277,#65278,#65279,#65280,#65281,#65282,#65283,#65284,
#65285,#65286,#65287,#65288,#65289,#65290,#65291,#65292,#65293,#65294,#65295,
#65296,#65297,#65298,#65299,#65300,#65301,#65302,#65303,#65304,#65305,#65306,
#65307,#65308,#65309,#65310,#65311,#65312,#65313,#65314,#65315,#65316,#65317,
#65318,#65319,#65320,#65321,#65322,#65323,#65324,#65325,#65326,#65327,#65328,
#65329,#65330,#65331,#65332,#65333,#65334,#65335,#65336,#65337,#65338,#65339,
#65340,#65341,#65342,#65343,#65344,#65345,#65346,#65347,#65348,#65349,#65350,
#65351,#65352,#65353,#65354,#65355,#65356,#65357,#65358,#65359,#65360,#65361,
#65362,#65363,#65364,#65365,#65366,#65367,#65368),.UNSPECIFIED.,.F.,.F.,
(4,3,3,3,3,3,3,3,3,3,3,3,3,3,3,3,3,3,3,3,3,3,3,3,3,3,3,3,3,3,3,3,3,3,3,
3,3,3,3,3,3,3,3,3,4),(-10.3761154186762,-10.2158546220139,-10.0546622936771,
-9.94136253581437,-9.79257454522795,-9.64404543825574,-9.49567371048497,
-9.34723566986522,-9.1987720858116,-9.04998470033248,-8.94722628223293,
-8.79847343390106,-8.64997952782992,-8.50164295391919,-8.35323959238031,
-8.20481047459631,-8.05605665252681,-7.95309002865149,-7.804291834983,-7.65575285344285,
-7.50737160293488,-7.3589246742507,-7.21045254363333,-7.06165728984481,
-6.95895377507006,-6.81012048303958,-6.66154561725903,-6.51312781903422,
-6.36464377561713,-6.21613415793645,-6.06730144977603,-5.96481752148862,
-5.81622542190058,-5.66789238697528,-5.51971633593897,-5.37147114763442,
-5.22319913949464,-5.07459816886151,-4.97068126790718,-4.82366356325693,
-4.67690419063574,-4.53020116852648,-4.3835521535988,-4.23663812113851,
-4.09293042032931),.UNSPECIFIED.);
#934=B_SPLINE_CURVE_WITH_KNOTS('',3,(#65371,#65372,#65373,#65374,#65375,
#65376,#65377,#65378,#65379,#65380,#65381,#65382,#65383,#65384,#65385,#65386,
#65387,#65388,#65389,#65390,#65391,#65392,#65393,#65394,#65395,#65396,#65397,
#65398,#65399,#65400,#65401,#65402,#65403,#65404),.UNSPECIFIED.,.F.,.F.,
(4,3,3,3,3,3,3,3,3,3,3,4),(45.5747633669549,45.7279460916964,45.8809709137411,
46.0340726659095,46.1872157257738,46.3406852415556,46.4098017231686,46.5617942570585,
46.7135157473756,46.8650726102834,47.0166960136029,47.1238898038469),
 .UNSPECIFIED.);
#935=B_SPLINE_CURVE_WITH_KNOTS('',3,(#65406,#65407,#65408,#65409,#65410,
#65411,#65412,#65413,#65414,#65415,#65416,#65417,#65418,#65419,#65420,#65421,
#65422,#65423,#65424,#65425,#65426,#65427,#65428,#65429,#65430,#65431,#65432,
#65433,#65434,#65435,#65436,#65437,#65438,#65439,#65440,#65441,#65442,#65443,
#65444,#65445,#65446,#65447,#65448,#65449,#65450,#65451,#65452,#65453,#65454,
#65455,#65456,#65457,#65458,#65459,#65460,#65461,#65462,#65463,#65464,#65465,
#65466,#65467,#65468,#65469,#65470,#65471,#65472),.UNSPECIFIED.,.F.,.F.,
(4,3,3,3,3,3,3,3,3,3,3,3,3,3,3,3,3,3,3,3,3,3,4),(47.1238898040689,47.3128509909798,
47.40393797675,47.5575421867538,47.710870940444,47.8640349431444,48.0172667587525,
48.1705331829181,48.3241211524605,48.3980742303315,48.5517950120318,48.7052464258146,
48.8585386455141,49.0119052759824,49.1653104318385,49.3190408342028,49.3922104839129,
49.5426217757813,49.692761485266,49.8462863076115,49.9963515219788,50.1516061483134,
50.306860774648),.UNSPECIFIED.);
#936=B_SPLINE_CURVE_WITH_KNOTS('',3,(#65476,#65477,#65478,#65479,#65480,
#65481,#65482,#65483,#65484,#65485,#65486,#65487,#65488,#65489,#65490,#65491,
#65492,#65493,#65494,#65495,#65496,#65497,#65498,#65499,#65500,#65501,#65502,
#65503,#65504,#65505,#65506,#65507,#65508,#65509,#65510,#65511,#65512,#65513,
#65514,#65515,#65516,#65517,#65518),.UNSPECIFIED.,.F.,.F.,(4,3,3,3,3,3,
3,3,3,3,3,3,3,3,4),(47.1238898040128,47.2782816278034,47.4323697908821,
47.5927359919967,47.7466225144832,47.9005181633557,48.054632188318,48.0738345953407,
48.2280558285865,48.382092629286,48.5360906232682,48.5709027221314,48.7482748367486,
48.9259950495598,49.0679708489221),.UNSPECIFIED.);
#937=B_SPLINE_CURVE_WITH_KNOTS('',3,(#65519,#65520,#65521,#65522,#65523,
#65524,#65525,#65526,#65527,#65528,#65529,#65530,#65531,#65532,#65533,#65534,
#65535,#65536,#65537,#65538,#65539,#65540,#65541,#65542,#65543,#65544,#65545,
#65546,#65547,#65548,#65549,#65550,#65551,#65552,#65553,#65554,#65555),
 .UNSPECIFIED.,.F.,.F.,(4,3,3,3,3,3,3,3,3,3,3,3,4),(45.5743044775645,45.7276698135094,
45.8810880641648,46.0348251362156,46.0855620881778,46.2375386974501,46.3892415635035,
46.5407859647282,46.6924252089547,46.8441117319342,46.9961635381894,47.0796983417592,
47.1238898038469),.UNSPECIFIED.);
#938=B_SPLINE_CURVE_WITH_KNOTS('',3,(#65558,#65559,#65560,#65561),
 .UNSPECIFIED.,.F.,.F.,(4,4),(-0.968477696161942,-0.935071686684093),
 .UNSPECIFIED.);
#939=B_SPLINE_CURVE_WITH_KNOTS('',3,(#65564,#65565,#65566,#65567,#65568,
#65569),.UNSPECIFIED.,.F.,.F.,(4,2,4),(8.52351753051953E-6,0.0223434875386195,
0.0446411083741544),.UNSPECIFIED.);
#940=B_SPLINE_CURVE_WITH_KNOTS('',3,(#65755,#65756,#65757,#65758),
 .UNSPECIFIED.,.F.,.F.,(4,4),(0.,0.000836946426958433),.UNSPECIFIED.);
#941=B_SPLINE_CURVE_WITH_KNOTS('',3,(#65759,#65760,#65761,#65762,#65763,
#65764,#65765,#65766,#65767,#65768,#65769,#65770,#65771,#65772,#65773,#65774,
#65775,#65776,#65777,#65778,#65779,#65780,#65781,#65782,#65783,#65784,#65785,
#65786,#65787,#65788,#65789,#65790,#65791,#65792,#65793,#65794,#65795,#65796,
#65797,#65798,#65799,#65800,#65801,#65802,#65803,#65804,#65805,#65806,#65807,
#65808,#65809,#65810,#65811,#65812,#65813,#65814,#65815,#65816,#65817,#65818,
#65819,#65820,#65821,#65822,#65823,#65824,#65825),.UNSPECIFIED.,.F.,.F.,
(4,3,3,3,3,3,3,3,3,3,3,3,3,3,3,3,3,3,3,3,3,3,4),(0.,0.0393121242914099,
0.117107898720596,0.167166306519262,0.189098627719502,0.208304762061158,
0.258210465370092,0.32305163930505,0.355694799905693,0.380210492454201,
0.409081485034023,0.483065857864488,0.517575161109925,0.554598739699055,
0.575971627854233,0.64977279486791,0.698159307576866,0.728055674524275,
0.746545820285823,0.819560974564155,0.852041521246935,0.875301939868949,
0.922805662986717),.UNSPECIFIED.);
#942=B_SPLINE_CURVE_WITH_KNOTS('',3,(#65826,#65827,#65828,#65829,#65830,
#65831,#65832,#65833,#65834,#65835,#65836,#65837,#65838,#65839,#65840,#65841,
#65842,#65843,#65844,#65845,#65846,#65847,#65848,#65849,#65850,#65851,#65852,
#65853,#65854,#65855,#65856,#65857,#65858,#65859,#65860,#65861,#65862,#65863,
#65864,#65865,#65866,#65867,#65868,#65869,#65870,#65871,#65872,#65873,#65874,
#65875,#65876,#65877,#65878,#65879,#65880,#65881,#65882,#65883,#65884,#65885,
#65886,#65887,#65888,#65889),.UNSPECIFIED.,.F.,.F.,(4,3,3,3,3,3,3,3,3,3,
3,3,3,3,3,3,3,3,3,3,3,4),(-0.968477696161958,-0.93346935475494,-0.87462218483068,
-0.838968787568558,-0.787473146091247,-0.753349378601184,-0.721529105370558,
-0.646900128137883,-0.59677334563425,-0.567483204022971,-0.543548087950493,
-0.480303919736905,-0.421085426012196,-0.392827821972742,-0.362136007930906,
-0.285930318294375,-0.243429944838067,-0.203365840094899,-0.175996194930052,
-0.0982285541899456,-0.0209966080041514,-2.23186798271618E-15),
 .UNSPECIFIED.);
#943=B_SPLINE_CURVE_WITH_KNOTS('',3,(#65895,#65896,#65897,#65898,#65899,
#65900,#65901,#65902,#65903,#65904,#65905,#65906,#65907,#65908,#65909,#65910,
#65911,#65912,#65913,#65914,#65915,#65916,#65917,#65918,#65919,#65920,#65921,
#65922,#65923,#65924,#65925,#65926,#65927,#65928,#65929,#65930,#65931,#65932,
#65933,#65934,#65935,#65936,#65937,#65938,#65939,#65940,#65941,#65942,#65943,
#65944,#65945,#65946,#65947,#65948,#65949,#65950,#65951,#65952,#65953,#65954,
#65955,#65956,#65957,#65958),.UNSPECIFIED.,.F.,.F.,(4,3,3,3,3,3,3,3,3,3,
3,3,3,3,3,3,3,3,3,3,3,4),(-0.953001334118943,-0.926795214108053,-0.867226959656485,
-0.843238497088046,-0.822042260146921,-0.745112575774413,-0.716203876023601,
-0.693609567103274,-0.617312067174212,-0.566983454838404,-0.537479678376499,
-0.514261574452167,-0.450249178495506,-0.393119621046725,-0.34952529407956,
-0.293393258181454,-0.221730948700384,-0.182710666717766,-0.157793989938048,
-0.085628124075386,-0.0150794994075627,-1.37622244676669E-15),
 .UNSPECIFIED.);
#944=B_SPLINE_CURVE_WITH_KNOTS('',3,(#66144,#66145,#66146,#66147),
 .UNSPECIFIED.,.F.,.F.,(4,4),(0.,0.0112420344023245),.UNSPECIFIED.);
#945=B_SPLINE_CURVE_WITH_KNOTS('',3,(#66148,#66149,#66150,#66151),
 .UNSPECIFIED.,.F.,.F.,(4,4),(0.,0.0131288794431488),.UNSPECIFIED.);
#946=B_SPLINE_CURVE_WITH_KNOTS('',3,(#66152,#66153,#66154,#66155,#66156,
#66157,#66158,#66159,#66160,#66161,#66162,#66163,#66164,#66165,#66166,#66167,
#66168,#66169,#66170,#66171,#66172,#66173,#66174,#66175,#66176,#66177,#66178,
#66179,#66180,#66181,#66182,#66183,#66184,#66185,#66186,#66187,#66188,#66189,
#66190,#66191,#66192,#66193,#66194,#66195,#66196,#66197,#66198,#66199,#66200,
#66201,#66202,#66203,#66204,#66205,#66206,#66207,#66208,#66209,#66210,#66211,
#66212,#66213,#66214,#66215),.UNSPECIFIED.,.F.,.F.,(4,3,3,3,3,3,3,3,3,3,
3,3,3,3,3,3,3,3,3,3,3,4),(0.0447297051812948,0.11579384797572,0.169972513625885,
0.195080510370564,0.269055930443271,0.323648223080396,0.345181704722379,
0.365728274421021,0.407621329269858,0.482026226691156,0.487425100991772,
0.524760575111112,0.54632412226274,0.620775662398705,0.672151363956664,
0.703230969871393,0.723527065514623,0.784142853240842,0.821242619777157,
0.858091484337553,0.935825551512836,0.965990216419499),.UNSPECIFIED.);
#947=B_SPLINE_CURVE_WITH_KNOTS('',3,(#66636,#66637,#66638,#66639,#66640,
#66641,#66642,#66643,#66644,#66645,#66646,#66647,#66648,#66649,#66650,#66651,
#66652,#66653,#66654,#66655,#66656,#66657,#66658,#66659,#66660,#66661,#66662,
#66663,#66664,#66665,#66666,#66667,#66668,#66669,#66670,#66671,#66672,#66673,
#66674,#66675,#66676,#66677,#66678,#66679,#66680,#66681,#66682,#66683,#66684,
#66685,#66686,#66687,#66688,#66689,#66690,#66691,#66692,#66693,#66694,#66695,
#66696,#66697,#66698,#66699,#66700,#66701,#66702,#66703,#66704,#66705,#66706,
#66707,#66708,#66709,#66710,#66711),.UNSPECIFIED.,.F.,.F.,(4,3,3,3,3,3,
3,3,3,3,3,3,3,3,3,3,3,3,3,3,3,3,3,3,3,4),(10.3765110117404,10.553450790841,
10.7300519237118,10.9066404614712,11.0832321762531,11.2602038202997,11.3015278342355,
11.4805049057995,11.6591300536428,11.837736646534,12.0163195055085,12.1953225046721,
12.299544594847,12.477964982007,12.6560183737272,12.8340392590285,13.0120277045372,
13.190434319541,13.2975613554585,13.4762752215219,13.6546274568134,13.8329507487056,
14.0112440633789,14.1899534235983,14.29557811607,14.315035395632),
 .UNSPECIFIED.);
#948=B_SPLINE_CURVE_WITH_KNOTS('',3,(#66714,#66715,#66716,#66717,#66718,
#66719,#66720,#66721,#66722,#66723,#66724,#66725,#66726,#66727,#66728,#66729,
#66730,#66731,#66732,#66733,#66734,#66735,#66736,#66737,#66738,#66739,#66740,
#66741,#66742,#66743,#66744,#66745,#66746,#66747,#66748,#66749,#66750,#66751,
#66752,#66753,#66754,#66755,#66756,#66757,#66758,#66759,#66760,#66761,#66762),
 .UNSPECIFIED.,.F.,.F.,(4,3,3,3,3,3,3,3,3,3,3,3,3,3,3,3,4),(11.6150328478182,
11.7979606486813,11.9807538318031,12.1637609224241,12.3468733973939,12.5304979994706,
12.6130496084297,12.7898803693582,12.9663087351348,13.1426740016011,13.3189861820381,
13.4957160141166,13.6110663690412,13.790004086606,13.9685863611197,14.1471565225389,
14.3143732599613),.UNSPECIFIED.);
#949=B_SPLINE_CURVE_WITH_KNOTS('',3,(#66768,#66769,#66770,#66771,#66772,
#66773,#66774,#66775,#66776,#66777,#66778,#66779,#66780,#66781,#66782,#66783,
#66784,#66785,#66786,#66787,#66788,#66789,#66790,#66791,#66792,#66793,#66794,
#66795,#66796,#66797,#66798,#66799,#66800,#66801,#66802,#66803,#66804,#66805,
#66806,#66807,#66808,#66809,#66810,#66811,#66812,#66813,#66814,#66815,#66816,
#66817,#66818,#66819,#66820,#66821,#66822,#66823,#66824,#66825,#66826,#66827,
#66828,#66829,#66830,#66831,#66832,#66833,#66834,#66835,#66836,#66837,#66838,
#66839,#66840,#66841,#66842,#66843,#66844,#66845,#66846,#66847,#66848,#66849,
#66850,#66851,#66852,#66853,#66854,#66855,#66856,#66857,#66858,#66859,#66860,
#66861,#66862,#66863,#66864,#66865,#66866,#66867,#66868,#66869,#66870,#66871,
#66872,#66873,#66874,#66875,#66876,#66877,#66878,#66879,#66880,#66881,#66882,
#66883,#66884,#66885,#66886,#66887,#66888,#66889,#66890,#66891,#66892,#66893,
#66894,#66895,#66896,#66897,#66898,#66899,#66900,#66901,#66902,#66903,#66904,
#66905,#66906,#66907,#66908,#66909,#66910,#66911,#66912,#66913,#66914,#66915,
#66916,#66917,#66918,#66919,#66920,#66921,#66922,#66923,#66924,#66925,#66926,
#66927,#66928,#66929,#66930,#66931,#66932,#66933,#66934,#66935,#66936,#66937,
#66938,#66939,#66940,#66941,#66942,#66943),.UNSPECIFIED.,.F.,.F.,(4,2,2,
2,2,2,2,2,2,2,2,2,2,2,2,2,2,2,2,2,2,2,2,2,2,2,2,2,2,2,2,2,2,2,2,2,2,2,2,
2,2,2,2,2,2,2,2,2,2,2,2,2,2,2,2,2,2,2,2,2,2,2,2,2,2,2,2,2,2,2,2,2,2,2,2,
2,2,2,2,2,2,2,2,2,2,2,2,4),(-1.16393024442893,-1.1221121315859,-1.10881872775493,
-1.09544934716449,-1.09173058973152,-1.08953019556074,-1.08752664172342,
-1.08475168761754,-1.07807017871904,-1.06837433006326,-1.03766271561164,
-0.986967317852749,-0.977454673078762,-0.972924462585128,-0.969395708425164,
-0.965480163368157,-0.958971176180976,-0.932462287603271,-0.898938534238497,
-0.862323864343115,-0.856094385560679,-0.853588717151212,-0.851567613516379,
-0.849448493062549,-0.846097056573953,-0.835079364231314,-0.81540391299286,
-0.803966476133666,-0.749205411550143,-0.739933534931748,-0.735449519421135,
-0.731926722665925,-0.727986733892083,-0.721362440590357,-0.693068305980396,
-0.661126188336577,-0.62498318336144,-0.618724065166356,-0.616213585950999,
-0.614191439698589,-0.612074386397869,-0.608732469713031,-0.597803658723205,
-0.578369392903072,-0.565103910874299,-0.512002169030124,-0.502609093783704,
-0.498101699222849,-0.494575904380125,-0.490648422164753,-0.484083268407897,
-0.456726688401616,-0.424134078931558,-0.387566159612312,-0.38133545021858,
-0.37882929357464,-0.376807817974159,-0.374687075157398,-0.371333009017104,
-0.360304955609168,-0.340603341285605,-0.333711435315054,-0.273565360251425,
-0.264992529056898,-0.260586706715257,-0.257245427320754,-0.253405341354982,
-0.249363595655126,-0.24334388884479,-0.232352183683043,-0.205509402738985,
-0.167177413247694,-0.146863476916789,-0.142705047485694,-0.14038371096495,
-0.138409430867859,-0.135855093702301,-0.130411237430462,-0.123009150411749,
-0.103368057562215,-0.0503645383585366,-0.0314881958645743,-0.02544491739472,
-0.0216335334546739,-0.0182616452424589,-0.0148096369960941,-0.00864602604130215,
-0.00070557473632002),.UNSPECIFIED.);
#950=B_SPLINE_CURVE_WITH_KNOTS('',3,(#66944,#66945,#66946,#66947,#66948,
#66949,#66950,#66951,#66952,#66953,#66954,#66955,#66956,#66957,#66958,#66959,
#66960,#66961,#66962,#66963,#66964,#66965,#66966,#66967,#66968,#66969,#66970,
#66971),.UNSPECIFIED.,.F.,.F.,(4,3,3,3,3,3,3,3,3,4),(14.315035395632,14.4936872514172,
14.6719976991658,14.8502987123366,15.0285878152494,15.2072891407824,15.2935948766815,
15.4900540694702,15.685111908359,15.7079632676251),.UNSPECIFIED.);
#951=B_SPLINE_CURVE_WITH_KNOTS('',3,(#66973,#66974,#66975,#66976,#66977,
#66978,#66979,#66980,#66981,#66982,#66983,#66984,#66985,#66986,#66987,#66988,
#66989,#66990,#66991,#66992,#66993,#66994,#66995,#66996,#66997,#66998,#66999,
#67000),.UNSPECIFIED.,.F.,.F.,(4,3,3,3,3,3,3,3,3,4),(14.3143732599613,14.4932818470659,
14.6090831296527,14.7880601048648,14.9666851520948,15.1452916394554,15.3238743899854,
15.5028772782052,15.6070998902642,15.7079632679489),.UNSPECIFIED.);
#952=B_SPLINE_CURVE_WITH_KNOTS('',3,(#67001,#67002,#67003,#67004,#67005,
#67006,#67007,#67008,#67009,#67010,#67011,#67012,#67013,#67014,#67015,#67016,
#67017,#67018,#67019,#67020,#67021,#67022,#67023,#67024,#67025,#67026,#67027,
#67028,#67029,#67030,#67031,#67032,#67033,#67034,#67035,#67036,#67037,#67038,
#67039,#67040,#67041,#67042,#67043,#67044,#67045,#67046,#67047,#67048,#67049,
#67050,#67051,#67052,#67053,#67054,#67055,#67056,#67057,#67058,#67059,#67060,
#67061,#67062,#67063,#67064,#67065,#67066,#67067,#67068,#67069,#67070,#67071,
#67072,#67073,#67074,#67075,#67076,#67077,#67078,#67079,#67080,#67081,#67082,
#67083,#67084,#67085,#67086,#67087,#67088,#67089,#67090,#67091,#67092,#67093,
#67094,#67095,#67096,#67097,#67098,#67099,#67100,#67101,#67102,#67103,#67104,
#67105,#67106,#67107,#67108,#67109,#67110,#67111,#67112,#67113,#67114,#67115,
#67116,#67117,#67118,#67119,#67120,#67121,#67122,#67123,#67124,#67125,#67126,
#67127,#67128,#67129,#67130,#67131,#67132,#67133,#67134,#67135,#67136,#67137,
#67138,#67139,#67140,#67141,#67142,#67143,#67144,#67145,#67146,#67147,#67148,
#67149,#67150,#67151,#67152,#67153,#67154,#67155,#67156,#67157,#67158,#67159,
#67160,#67161,#67162),.UNSPECIFIED.,.F.,.F.,(4,2,2,2,2,2,2,2,2,2,2,2,2,
2,2,2,2,2,2,2,2,2,2,2,2,2,2,2,2,2,2,2,2,2,2,2,2,2,2,2,2,2,2,2,2,2,2,2,2,
2,2,2,2,2,2,2,2,2,2,2,2,2,2,2,2,2,2,2,2,2,2,2,2,2,2,2,2,2,2,2,4),(-2.98942615939622,
-2.94687744843447,-2.90737887780196,-2.90028833462003,-2.89626757009887,
-2.89278736806544,-2.88850740594506,-2.88194860504523,-2.83799867893463,
-2.79959280759611,-2.78803138120337,-2.78284147994681,-2.7788283302866,
-2.77655245813013,-2.7747160432841,-2.77226099931904,-2.76840197913877,
-2.74684477299445,-2.7014833079237,-2.66913041899145,-2.66227335609882,
-2.65827801354727,-2.65475565048187,-2.65033879153963,-2.64173110989955,
-2.58217996827536,-2.57531649807323,-2.55547164910086,-2.54439033061707,
-2.5410244222646,-2.53889684010004,-2.53687348626668,-2.53436524742632,
-2.52813036525468,-2.4917679525961,-2.45944377174351,-2.43180998977834,
-2.42522856169367,-2.42129812597274,-2.41777390166482,-2.41327434396693,
-2.40391952697214,-2.35010438134218,-2.33761336325053,-2.31801429303953,
-2.30702655289876,-2.30367990062065,-2.30156294068283,-2.29954488717194,
-2.29704277121525,-2.29082111843716,-2.25423947569581,-2.22151065226755,
-2.19433476155473,-2.18778874877106,-2.18386961472211,-2.18034945389465,
-2.17584679667526,-2.16645503385871,-2.11336918408685,-2.10013504463255,
-2.08062743095894,-2.06967603867303,-2.06633508998146,-2.06422055344751,
-2.06220017101256,-2.05969362054567,-2.05345255268914,-2.01714235715239,
-1.98492427180508,-1.95706758364123,-1.9504713292746,-1.94653757415735,
-1.94301382477905,-1.9385196018074,-1.92919317744503,-1.87520561547252,
-1.83454429703135,-1.83001991115689,-1.8276461646142,-1.82654679620979),
 .UNSPECIFIED.);
#953=B_SPLINE_CURVE_WITH_KNOTS('',3,(#67167,#67168,#67169,#67170,#67171,
#67172,#67173,#67174,#67175,#67176,#67177,#67178,#67179,#67180,#67181,#67182,
#67183,#67184,#67185,#67186,#67187,#67188,#67189,#67190,#67191,#67192,#67193,
#67194,#67195,#67196,#67197,#67198,#67199,#67200,#67201,#67202,#67203,#67204,
#67205,#67206,#67207,#67208,#67209,#67210,#67211,#67212,#67213,#67214,#67215,
#67216,#67217,#67218,#67219,#67220,#67221,#67222,#67223,#67224,#67225,#67226,
#67227,#67228,#67229,#67230,#67231,#67232,#67233,#67234,#67235,#67236,#67237,
#67238,#67239,#67240,#67241,#67242,#67243,#67244,#67245,#67246,#67247,#67248,
#67249,#67250,#67251,#67252,#67253,#67254,#67255,#67256,#67257,#67258,#67259,
#67260,#67261,#67262,#67263,#67264,#67265,#67266,#67267,#67268,#67269,#67270,
#67271,#67272,#67273,#67274,#67275,#67276,#67277,#67278,#67279,#67280,#67281,
#67282,#67283,#67284,#67285,#67286,#67287,#67288,#67289,#67290,#67291,#67292,
#67293,#67294,#67295,#67296,#67297,#67298,#67299,#67300,#67301,#67302,#67303,
#67304,#67305,#67306,#67307,#67308,#67309,#67310,#67311,#67312,#67313,#67314,
#67315,#67316,#67317,#67318,#67319,#67320,#67321,#67322,#67323,#67324,#67325,
#67326,#67327,#67328,#67329,#67330,#67331,#67332,#67333,#67334,#67335,#67336,
#67337,#67338,#67339,#67340,#67341,#67342,#67343,#67344,#67345,#67346,#67347,
#67348,#67349,#67350,#67351,#67352,#67353,#67354,#67355,#67356,#67357,#67358,
#67359,#67360,#67361,#67362,#67363,#67364,#67365,#67366,#67367,#67368,#67369,
#67370,#67371,#67372,#67373,#67374,#67375,#67376,#67377,#67378,#67379,#67380,
#67381,#67382),.UNSPECIFIED.,.F.,.F.,(4,2,2,2,2,2,2,2,2,2,2,2,2,2,2,2,2,
2,2,2,2,2,2,2,2,2,2,2,2,2,2,2,2,2,2,2,2,2,2,2,2,2,2,2,2,2,2,2,2,2,2,2,2,
2,2,2,2,2,2,2,2,2,2,2,2,2,2,2,2,2,2,2,2,2,2,2,2,2,2,2,2,2,2,2,2,2,2,2,2,
2,2,2,2,2,2,2,2,2,2,2,2,2,2,2,2,2,2,4),(-2.65811385973918,-2.64341887280631,
-2.63685547945785,-2.63292924488921,-2.62940468727833,-2.62489903708624,
-2.61551025001664,-2.56238128523994,-2.54919264361674,-2.52971894580261,
-2.51877761208218,-2.51543481805796,-2.51331789853485,-2.51129633688125,
-2.50878716273528,-2.50253408200726,-2.46640007387792,-2.43445651631383,
-2.40623004475929,-2.39961108197887,-2.39567265610066,-2.39215024322409,
-2.38766531765506,-2.37838640297329,-2.32371253981176,-2.31218416854247,
-2.29250660917671,-2.28148985781449,-2.27813883561977,-2.27602003237057,
-2.27399956303752,-2.27149476126776,-2.26526776294454,-2.22872118194875,
-2.1961529858716,-2.16881232025688,-2.16224953615428,-2.1583231805186,-2.15479821019637,
-2.15029161224657,-2.14089927817996,-2.08780637972958,-2.07456150657982,
-2.05509772052212,-2.04415967673414,-2.04081702101019,-2.03869999347207,
-2.03667816505093,-2.03416848444712,-2.02791325698376,-1.99179456385597,
-1.95987879084501,-1.93160587948036,-1.924983541931,-1.92104413243149,-1.91752147569834,
-1.91303711126042,-1.90376257244495,-1.84901801727298,-1.83755339109749,
-1.81786820831232,-1.80684826104643,-1.80349666903814,-1.8013775956048,
-1.79935691668679,-1.79685192957958,-1.79062483873777,-1.75406198815898,
-1.72147300873686,-1.69415644155959,-1.68759468993854,-1.68366826775868,
-1.68014280788343,-1.67563498858127,-1.66623787311483,-1.61320062663609,
-1.57165631512584,-1.56711236676727,-1.56473481914091,-1.56276388018841,
-1.56027892884346,-1.55632224374582,-1.53211804490594,-1.49545586039646,
-1.45803901320214,-1.45087621560002,-1.44677758808614,-1.44330536420355,
-1.43906067168766,-1.43099906766286,-1.38669425295883,-1.33778773774552,
-1.33106359083246,-1.32847789303883,-1.32661927783257,-1.32456966534925,
-1.32154352722031,-1.31319780845717,-1.30005877224877,-1.27130435927623,
-1.22453385002851,-1.21502442574756,-1.21047808041805,-1.20693773371413,
-1.20307033969169,-1.19678165452462,-1.17322533761841,-1.16393024442893),
 .UNSPECIFIED.);
#954=B_SPLINE_CURVE_WITH_KNOTS('',3,(#67383,#67384,#67385,#67386,#67387,
#67388,#67389,#67390,#67391,#67392,#67393,#67394,#67395,#67396,#67397,#67398,
#67399,#67400,#67401,#67402,#67403,#67404,#67405,#67406,#67407,#67408,#67409,
#67410,#67411,#67412,#67413,#67414,#67415,#67416,#67417,#67418,#67419,#67420,
#67421,#67422,#67423,#67424,#67425,#67426,#67427,#67428,#67429,#67430,#67431,
#67432,#67433,#67434,#67435,#67436,#67437,#67438,#67439,#67440,#67441,#67442,
#67443,#67444,#67445,#67446,#67447,#67448,#67449,#67450,#67451,#67452,#67453,
#67454,#67455,#67456,#67457,#67458,#67459,#67460,#67461,#67462,#67463,#67464,
#67465,#67466,#67467,#67468,#67469,#67470,#67471,#67472,#67473,#67474,#67475,
#67476,#67477,#67478,#67479,#67480,#67481,#67482,#67483,#67484,#67485,#67486,
#67487,#67488,#67489,#67490,#67491,#67492,#67493,#67494,#67495,#67496,#67497,
#67498,#67499,#67500,#67501,#67502,#67503,#67504,#67505,#67506,#67507,#67508,
#67509,#67510,#67511,#67512,#67513,#67514,#67515,#67516,#67517,#67518,#67519,
#67520,#67521,#67522,#67523,#67524,#67525,#67526,#67527,#67528,#67529,#67530,
#67531,#67532,#67533,#67534,#67535,#67536,#67537,#67538,#67539,#67540,#67541,
#67542,#67543,#67544,#67545,#67546,#67547,#67548,#67549,#67550,#67551,#67552,
#67553,#67554,#67555,#67556,#67557,#67558,#67559,#67560,#67561,#67562,#67563,
#67564,#67565,#67566,#67567,#67568,#67569,#67570,#67571,#67572,#67573,#67574,
#67575,#67576,#67577,#67578,#67579,#67580,#67581,#67582,#67583,#67584,#67585,
#67586,#67587,#67588,#67589,#67590,#67591,#67592),.UNSPECIFIED.,.F.,.F.,
(4,2,2,2,2,2,2,2,2,2,2,2,2,2,2,2,2,2,2,2,2,2,2,2,2,2,2,2,2,2,2,2,2,2,2,
2,2,2,2,2,2,2,2,2,2,2,2,2,2,2,2,2,2,2,2,2,2,2,2,2,2,2,2,2,2,2,2,2,2,2,2,
2,2,2,2,2,2,2,2,2,2,2,2,2,2,2,2,2,2,2,2,2,2,2,2,2,2,2,2,2,2,2,2,2,4),(-1.82654679620979,
-1.82567514256061,-1.82318578987642,-1.81921319040424,-1.7945975999961,
-1.78085997278393,-1.7509591994889,-1.72013307652391,-1.71336497138031,
-1.70939473836614,-1.7058785560794,-1.70144836983348,-1.69274827174082,
-1.63351771519777,-1.59712820036903,-1.59263831113477,-1.59027268554199,
-1.58830213870627,-1.58580575376867,-1.58180878732842,-1.55563188197764,
-1.54336480304901,-1.51968739046691,-1.49541669681936,-1.48036462094594,
-1.4747971116956,-1.47145663595873,-1.4678957223663,-1.46312196202823,-1.45224427397563,
-1.4122393108637,-1.3631967470555,-1.35660554113805,-1.35404011821867,-1.35218727325777,
-1.35013310945877,-1.34708239148078,-1.33855327348186,-1.32500659946013,
-1.25894060115722,-1.24314452828203,-1.23747258219032,-1.23411196404678,
-1.23056076484228,-1.22585342218376,-1.21536014310749,-1.20098137192243,
-1.15815776541184,-1.12236958235826,-1.118324968688,-1.11581402318508,-1.11384229735801,
-1.11148754612972,-1.10705055497943,-1.0743623081271,-1.02123830959475,
-1.00570661802811,-1.00007250684677,-0.996719268033883,-0.99316482249979,
-0.988434287423803,-0.977807444331893,-0.963186142593477,-0.918897988539242,
-0.885062430743449,-0.880985310049003,-0.878464863782423,-0.876492741512126,
-0.874145914767134,-0.869746244582656,-0.838975300467984,-0.79077979564977,
-0.769698590801541,-0.76340651574252,-0.759539578751323,-0.756001334220189,
-0.751382768040408,-0.741383638800634,-0.727888289896724,-0.689928879494222,
-0.650504547981136,-0.6443072230176,-0.641807771155571,-0.639788998631064,
-0.637668699900011,-0.634309761118168,-0.623215004476113,-0.603326541332951,
-0.595162166258294,-0.536884376366843,-0.52796871893014,-0.5235543137147,
-0.520039551252073,-0.51605907889055,-0.509243845237497,-0.477522095825476,
-0.430973442848463,-0.40989771349916,-0.405690896618916,-0.403359372530627,
-0.401385809699974,-0.398845112426623,-0.393478933319888,-0.355248774809182,
-0.332190119670129),.UNSPECIFIED.);
#955=B_SPLINE_CURVE_WITH_KNOTS('',3,(#67598,#67599,#67600,#67601,#67602,
#67603,#67604,#67605,#67606,#67607,#67608,#67609,#67610,#67611,#67612,#67613,
#67614,#67615,#67616,#67617,#67618,#67619,#67620,#67621,#67622,#67623,#67624,
#67625,#67626,#67627,#67628,#67629,#67630,#67631,#67632,#67633,#67634,#67635,
#67636,#67637,#67638,#67639,#67640,#67641,#67642,#67643,#67644,#67645,#67646,
#67647,#67648,#67649,#67650,#67651,#67652,#67653,#67654,#67655,#67656,#67657,
#67658,#67659,#67660,#67661,#67662,#67663,#67664,#67665,#67666,#67667,#67668,
#67669,#67670,#67671,#67672,#67673,#67674,#67675,#67676,#67677,#67678,#67679,
#67680,#67681,#67682,#67683,#67684,#67685,#67686,#67687,#67688,#67689,#67690,
#67691,#67692,#67693,#67694,#67695,#67696,#67697,#67698,#67699,#67700,#67701,
#67702,#67703,#67704,#67705,#67706,#67707,#67708,#67709,#67710,#67711,#67712,
#67713,#67714,#67715,#67716,#67717,#67718,#67719,#67720,#67721,#67722,#67723,
#67724,#67725,#67726,#67727,#67728,#67729,#67730,#67731,#67732,#67733,#67734,
#67735,#67736,#67737,#67738,#67739,#67740,#67741,#67742,#67743,#67744,#67745,
#67746,#67747,#67748,#67749,#67750,#67751,#67752,#67753,#67754,#67755,#67756,
#67757,#67758,#67759,#67760,#67761,#67762,#67763),.UNSPECIFIED.,.F.,.F.,
(4,2,2,2,2,2,2,2,2,2,2,2,2,2,2,2,2,2,2,2,2,2,2,2,2,2,2,2,2,2,2,2,2,2,2,
2,2,2,2,2,2,2,2,2,2,2,2,2,2,2,2,2,2,2,2,2,2,2,2,2,2,2,2,2,2,2,2,2,2,2,2,
2,2,2,2,2,2,2,2,2,2,2,4),(-1.16365104910194,-1.16198873409848,-1.11873333451251,
-1.08007682483228,-1.07289533808751,-1.06879292991221,-1.06532147429848,
-1.06108261121265,-1.05304736223389,-1.01380643672128,-0.974354768874303,
-0.955615421727428,-0.95154095556962,-0.949238925381929,-0.947279975777236,
-0.944706537452359,-0.939168763503621,-0.931601350956711,-0.911272521420545,
-0.864697156551351,-0.841359959454907,-0.834859417924407,-0.830946538256954,
-0.827418656268732,-0.822887438665612,-0.813364699776189,-0.800702995228171,
-0.766805215685698,-0.721392566400016,-0.715391258738159,-0.712957370947077,
-0.710954958021573,-0.708805444312101,-0.705315425122888,-0.692920314092189,
-0.669266049918139,-0.611703523646731,-0.600662162343852,-0.596217640945699,
-0.592926913172538,-0.589328930082488,-0.584341614312926,-0.572173887692835,
-0.506645012856004,-0.504000582658459,-0.493537335427797,-0.480167288699852,
-0.476449005709923,-0.474249008124355,-0.47224603922321,-0.4694720984499,
-0.462793799245578,-0.45310336172613,-0.422417340554128,-0.37169541728193,
-0.362185648162151,-0.357656682611973,-0.35412885374973,-0.35021429531376,
-0.343706866024677,-0.317203459323662,-0.28368579624041,-0.247072372632416,
-0.240849064767332,-0.238124138572478,-0.236151648600852,-0.234309633850536,
-0.231056093345189,-0.220914738422784,-0.203536525041064,-0.150699833390058,
-0.128996687355292,-0.122647285439585,-0.118767180860785,-0.11523123553389,
-0.110636222873976,-0.1007701932916,-0.0875102476811494,-0.0507450523485492,
-0.00710859726825555,-0.00274825577811126,-0.00126848880133153,-0.000702321398189432),
 .UNSPECIFIED.);
#956=B_SPLINE_CURVE_WITH_KNOTS('',3,(#67764,#67765,#67766,#67767,#67768,
#67769,#67770,#67771,#67772,#67773,#67774,#67775,#67776,#67777,#67778,#67779,
#67780,#67781,#67782,#67783,#67784,#67785,#67786,#67787,#67788,#67789,#67790,
#67791,#67792,#67793,#67794,#67795,#67796,#67797,#67798,#67799,#67800,#67801,
#67802,#67803,#67804,#67805,#67806,#67807,#67808,#67809,#67810,#67811,#67812,
#67813,#67814,#67815),.UNSPECIFIED.,.F.,.F.,(4,2,2,2,2,2,2,2,2,2,2,2,2,
2,2,2,2,2,2,2,2,2,2,2,2,4),(-2.9893848513208,-2.98893747316369,-2.9876025158476,
-2.98546557946283,-2.98216250725133,-2.97197352792502,-2.96355815815491,
-2.90631730564084,-2.88926272540383,-2.87733951087504,-2.87239217835099,
-2.86880219859959,-2.86550441099093,-2.86102835754096,-2.84979189282628,
-2.77362471164541,-2.76248320507388,-2.75507907488132,-2.75285138792675,
-2.75074533201809,-2.74881523310293,-2.7460912084198,-2.739870957641,-2.7033280354885,
-2.67077630094081,-2.65811385973918),.UNSPECIFIED.);
#957=B_SPLINE_CURVE_WITH_KNOTS('',3,(#67817,#67818,#67819,#67820,#67821,
#67822,#67823,#67824,#67825,#67826,#67827,#67828,#67829,#67830,#67831,#67832,
#67833,#67834,#67835,#67836,#67837,#67838,#67839,#67840,#67841,#67842,#67843,
#67844,#67845,#67846,#67847,#67848,#67849,#67850,#67851,#67852,#67853,#67854,
#67855,#67856,#67857,#67858,#67859,#67860,#67861,#67862,#67863,#67864,#67865,
#67866,#67867,#67868,#67869,#67870,#67871,#67872,#67873,#67874,#67875,#67876,
#67877,#67878,#67879,#67880,#67881,#67882,#67883,#67884,#67885,#67886,#67887,
#67888,#67889,#67890,#67891,#67892,#67893,#67894,#67895,#67896,#67897,#67898,
#67899,#67900,#67901,#67902,#67903,#67904,#67905,#67906,#67907,#67908,#67909,
#67910,#67911,#67912),.UNSPECIFIED.,.F.,.F.,(4,2,2,2,2,2,2,2,2,2,2,2,2,
2,2,2,2,2,2,2,2,2,2,2,2,2,2,2,2,2,2,2,2,2,2,2,2,2,2,2,2,2,2,2,2,2,2,4),
(-0.332190119670129,-0.299974256783078,-0.29076182289428,-0.286290157332493,
-0.282769813927846,-0.282625201287161,-0.282512604791512,-0.282424919666148,
-0.282356617668773,-0.282303400836696,-0.282223074884288,-0.2821468634119,
-0.282074529573626,-0.282005851482837,-0.281940621293291,-0.281878644309835,
-0.281819738143039,-0.281763731896355,-0.281710465402988,-0.281659788503258,
-0.281611560369081,-0.281565648872144,-0.281521929981461,-0.281480287226152,
-0.28144061117419,-0.281402798955855,-0.281366753823448,-0.277086765497933,
-0.268113946574196,-0.25627891769557,-0.226021878457394,-0.178535972958935,
-0.17031557559799,-0.167215471896808,-0.165356270008634,-0.163309071896805,
-0.160291684989588,-0.152003104953454,-0.10448895096256,-0.0779098348769532,
-0.05747216958326,-0.0512538036654406,-0.0474028352405869,-0.0438597472645543,
-0.0403992630740389,-0.0358762841793266,-0.023929538719514,-0.000702291658524479),
 .UNSPECIFIED.);
#958=B_SPLINE_CURVE_WITH_KNOTS('',3,(#67913,#67914,#67915,#67916,#67917,
#67918,#67919,#67920,#67921,#67922,#67923,#67924,#67925,#67926,#67927,#67928,
#67929,#67930,#67931,#67932,#67933,#67934,#67935,#67936,#67937,#67938,#67939,
#67940,#67941,#67942,#67943,#67944,#67945,#67946,#67947,#67948,#67949,#67950,
#67951,#67952,#67953,#67954,#67955,#67956,#67957,#67958,#67959,#67960,#67961,
#67962,#67963,#67964,#67965,#67966,#67967,#67968,#67969,#67970,#67971,#67972,
#67973,#67974,#67975,#67976,#67977,#67978,#67979,#67980,#67981,#67982,#67983,
#67984,#67985,#67986,#67987,#67988,#67989,#67990,#67991,#67992,#67993,#67994,
#67995,#67996,#67997,#67998,#67999,#68000,#68001,#68002,#68003,#68004,#68005,
#68006,#68007,#68008,#68009,#68010,#68011,#68012,#68013,#68014,#68015,#68016,
#68017,#68018,#68019,#68020,#68021,#68022,#68023,#68024,#68025,#68026,#68027,
#68028,#68029,#68030,#68031,#68032,#68033,#68034,#68035,#68036,#68037,#68038,
#68039,#68040,#68041,#68042,#68043,#68044,#68045,#68046,#68047,#68048,#68049,
#68050,#68051,#68052,#68053,#68054,#68055,#68056,#68057,#68058,#68059,#68060,
#68061,#68062,#68063,#68064,#68065,#68066,#68067,#68068,#68069,#68070,#68071,
#68072,#68073,#68074,#68075,#68076,#68077,#68078,#68079,#68080,#68081,#68082,
#68083,#68084,#68085,#68086,#68087,#68088,#68089,#68090,#68091,#68092,#68093,
#68094,#68095,#68096,#68097,#68098,#68099,#68100,#68101,#68102,#68103,#68104,
#68105,#68106,#68107,#68108),.UNSPECIFIED.,.F.,.F.,(4,2,2,2,2,2,2,2,2,2,
2,2,2,2,2,2,2,2,2,2,2,2,2,2,2,2,2,2,2,2,2,2,2,2,2,2,2,2,2,2,2,2,2,2,2,2,
2,2,2,2,2,2,2,2,2,2,2,2,2,2,2,2,2,2,2,2,2,2,2,2,2,2,2,2,2,2,2,2,2,2,2,2,
2,2,2,2,2,2,2,2,2,2,2,2,2,2,2,4),(-2.98897358008687,-2.92769314209762,-2.92283635649671,
-2.91891607758328,-2.91667246239068,-2.91468429829351,-2.9120511288804,
-2.90602483674824,-2.85973597595541,-2.82644850336208,-2.81392147458867,
-2.80456842641748,-2.80028193766707,-2.80021757807928,-2.80014854592242,
-2.80007429804235,-2.79999420251525,-2.79990751963336,-2.79981337778569,
-2.79971074256605,-2.79959837680186,-2.79947478825607,-2.7993381603811,
-2.79918625944562,-2.79910282444393,-2.79894676733214,-2.7986404194696,
-2.79512089876872,-2.79065274727909,-2.78145663265082,-2.7261184372274,
-2.68653475198969,-2.68201786236957,-2.67964667784219,-2.6776764846138,
-2.67518682288345,-2.67121230847029,-2.6465385500168,-2.60381980183744,
-2.57218735140361,-2.56537747406849,-2.56139840445967,-2.55788383669279,
-2.55346828700893,-2.54454549542632,-2.48629755644931,-2.47808810643394,
-2.45818707535278,-2.44708889637699,-2.44372974284319,-2.44160952912779,
-2.4395909662627,-2.43709198168734,-2.43089673012719,-2.3914888195501,-2.35356167696314,
-2.34007362068281,-2.33007780218808,-2.32545997520698,-2.32192195528628,
-2.31805492340576,-2.3117619328311,-2.29066986050776,-2.24245176471885,
-2.21166913656067,-2.20726891292452,-2.20492200279276,-2.20294992363011,
-2.20042969097544,-2.19635325451221,-2.16252425488423,-2.1577595822794,
-2.12368275873593,-2.09697182148208,-2.09045172116841,-2.08653517742575,
-2.08300913125178,-2.07848745284167,-2.06901214652698,-2.01745666702726,
-1.98731902900585,-1.97772631630079,-1.9710993642418,-1.96833439561336,
-1.96633333461326,-1.96413046746479,-1.96039731815009,-1.94685350251339,
-1.93673283316637,-1.92126868736453,-1.8800268546076,-1.86592293387262,
-1.85558121982064,-1.85090091581163,-1.84735388977835,-1.84351479821116,
-1.83735142483573,-1.82625073863295),.UNSPECIFIED.);
#959=B_SPLINE_CURVE_WITH_KNOTS('',3,(#68113,#68114,#68115,#68116,#68117,
#68118,#68119,#68120,#68121,#68122,#68123,#68124,#68125,#68126,#68127,#68128,
#68129,#68130,#68131,#68132,#68133,#68134,#68135,#68136,#68137,#68138,#68139,
#68140,#68141,#68142,#68143,#68144,#68145,#68146,#68147,#68148,#68149,#68150,
#68151,#68152,#68153,#68154,#68155,#68156,#68157,#68158,#68159,#68160,#68161,
#68162,#68163,#68164,#68165,#68166,#68167,#68168,#68169,#68170,#68171,#68172,
#68173,#68174,#68175,#68176,#68177,#68178,#68179,#68180,#68181,#68182,#68183,
#68184,#68185,#68186,#68187,#68188,#68189,#68190,#68191,#68192,#68193,#68194,
#68195,#68196,#68197,#68198,#68199,#68200,#68201,#68202,#68203,#68204,#68205,
#68206,#68207,#68208,#68209,#68210,#68211,#68212,#68213,#68214,#68215,#68216,
#68217,#68218,#68219,#68220,#68221,#68222,#68223,#68224,#68225,#68226,#68227,
#68228,#68229,#68230,#68231,#68232,#68233,#68234,#68235,#68236,#68237,#68238,
#68239,#68240,#68241,#68242,#68243,#68244,#68245,#68246,#68247,#68248,#68249,
#68250,#68251,#68252,#68253,#68254,#68255,#68256,#68257,#68258,#68259,#68260,
#68261,#68262,#68263,#68264,#68265,#68266,#68267,#68268,#68269,#68270,#68271,
#68272,#68273,#68274,#68275,#68276,#68277,#68278,#68279,#68280,#68281,#68282,
#68283,#68284,#68285,#68286,#68287,#68288,#68289,#68290,#68291,#68292,#68293,
#68294,#68295,#68296,#68297,#68298,#68299,#68300,#68301,#68302,#68303,#68304,
#68305,#68306,#68307,#68308,#68309,#68310,#68311,#68312,#68313,#68314,#68315,
#68316,#68317,#68318,#68319,#68320,#68321,#68322,#68323,#68324,#68325,#68326,
#68327,#68328,#68329,#68330,#68331,#68332),.UNSPECIFIED.,.F.,.F.,(4,2,2,
2,2,2,2,2,2,2,2,2,2,2,2,2,2,2,2,2,2,2,2,2,2,2,2,2,2,2,2,2,2,2,2,2,2,2,2,
2,2,2,2,2,2,2,2,2,2,2,2,2,2,2,2,2,2,2,2,2,2,2,2,2,2,2,2,2,2,2,2,2,2,2,2,
2,2,2,2,2,2,2,2,2,2,2,2,2,2,2,2,2,2,2,2,2,2,2,2,2,2,2,2,2,2,2,2,2,2,4),
(-2.65746774305231,-2.65261804205566,-2.64584623324261,-2.62617272996607,
-2.615158715998,-2.61180870310401,-2.60969057770515,-2.60767078381733,-2.60516685459269,
-2.59894220127053,-2.56240086795725,-2.52983407927815,-2.5025163264511,
-2.4959566011589,-2.49203172690838,-2.48850786796351,-2.48400238850228,
-2.47461125209531,-2.42156657618331,-2.40828353613625,-2.38883638532185,
-2.37790572301896,-2.37456456956123,-2.37244832301837,-2.37042708978095,
-2.36791799108521,-2.36166341956384,-2.3255746626612,-2.2936985406124,-2.26539500955471,
-2.25877237795713,-2.25483372512526,-2.25131232252042,-2.24683034551568,
-2.23756365834511,-2.18277827436322,-2.17137556262963,-2.1516918972459,
-2.14067375523214,-2.13732307541338,-2.13520466037621,-2.13318470453986,
-2.13068069407162,-2.12445643857931,-2.08788702671947,-2.0551634332501,
-2.02799948587829,-2.02144936529857,-2.0175263187276,-2.01400164189302,
-2.00949171294237,-2.00007853200098,-1.94738375203425,-1.91806825964147,
-1.90862556174804,-1.90207648863689,-1.89932450422995,-1.89732548159356,
-1.89511670599879,-1.89135670056093,-1.87751250941603,-1.86804159384396,
-1.82509180481262,-1.79421630215818,-1.78565730401293,-1.78131308838638,
-1.77780387481513,-1.77377471181276,-1.76691604016749,-1.73688615852472,
-1.68578013459207,-1.66727315857274,-1.66332871016514,-1.66107944988934,
-1.6590919804408,-1.65646702327566,-1.65048992885583,-1.60317010610248,
-1.55639897987041,-1.54815030595161,-1.54386836370732,-1.54036272421504,
-1.53628518103136,-1.5292125310971,-1.49473056438907,-1.46722289421195,
-1.46251149378335,-1.43097650505498,-1.4269038680685,-1.42438472433374,
-1.42241262300298,-1.42006456128484,-1.41565919958629,-1.38460982826758,
-1.33569511012369,-1.31546921485392,-1.30927375427337,-1.30542774023406,
-1.30188303067876,-1.29721857384015,-1.28696539389295,-1.27301799952048,
-1.20017970924618,-1.19119696202027,-1.18798359961284,-1.1861022609768,
-1.18407387501954,-1.18115436225658,-1.17354740652748,-1.16365104910194),
 .UNSPECIFIED.);
#960=B_SPLINE_CURVE_WITH_KNOTS('',3,(#68333,#68334,#68335,#68336,#68337,
#68338,#68339,#68340,#68341,#68342,#68343,#68344,#68345,#68346,#68347,#68348,
#68349,#68350,#68351,#68352,#68353,#68354,#68355,#68356,#68357,#68358,#68359,
#68360,#68361,#68362,#68363,#68364,#68365,#68366,#68367,#68368,#68369,#68370,
#68371,#68372,#68373,#68374,#68375,#68376,#68377,#68378,#68379,#68380,#68381,
#68382,#68383,#68384,#68385,#68386,#68387,#68388,#68389,#68390,#68391,#68392,
#68393,#68394,#68395,#68396,#68397,#68398,#68399,#68400,#68401,#68402,#68403,
#68404,#68405,#68406,#68407,#68408,#68409,#68410,#68411,#68412,#68413,#68414,
#68415,#68416,#68417,#68418,#68419,#68420,#68421,#68422,#68423,#68424,#68425,
#68426,#68427,#68428,#68429,#68430,#68431,#68432,#68433,#68434,#68435,#68436,
#68437,#68438,#68439,#68440,#68441,#68442,#68443,#68444,#68445,#68446,#68447,
#68448,#68449,#68450,#68451,#68452,#68453,#68454,#68455,#68456,#68457,#68458,
#68459,#68460,#68461,#68462,#68463,#68464,#68465,#68466,#68467,#68468,#68469,
#68470,#68471,#68472,#68473,#68474,#68475,#68476,#68477,#68478,#68479,#68480,
#68481,#68482,#68483,#68484,#68485,#68486,#68487,#68488,#68489,#68490,#68491,
#68492,#68493,#68494,#68495,#68496,#68497,#68498,#68499,#68500,#68501,#68502,
#68503,#68504,#68505,#68506,#68507,#68508,#68509,#68510,#68511,#68512,#68513,
#68514,#68515,#68516,#68517,#68518,#68519,#68520,#68521,#68522,#68523,#68524,
#68525,#68526,#68527,#68528,#68529,#68530,#68531,#68532,#68533,#68534,#68535,
#68536,#68537,#68538,#68539,#68540,#68541,#68542,#68543,#68544),
 .UNSPECIFIED.,.F.,.F.,(4,2,2,2,2,2,2,2,2,2,2,2,2,2,2,2,2,2,2,2,2,2,2,2,
2,2,2,2,2,2,2,2,2,2,2,2,2,2,2,2,2,2,2,2,2,2,2,2,2,2,2,2,2,2,2,2,2,2,2,2,
2,2,2,2,2,2,2,2,2,2,2,2,2,2,2,2,2,2,2,2,2,2,2,2,2,2,2,2,2,2,2,2,2,2,2,2,
2,2,2,2,2,2,2,2,2,4),(-1.82625073863295,-1.81743048083367,-1.76819131431197,
-1.7370057602039,-1.73259681582595,-1.73024795135637,-1.72827585061212,
-1.72575766004703,-1.72168845751425,-1.69070653630609,-1.65995402162083,
-1.63551189232338,-1.6251599607778,-1.61701484637726,-1.61275381803255,
-1.60958890756908,-1.60561783324043,-1.59884743904035,-1.57172333339439,
-1.57012941610718,-1.5175731179029,-1.49886167212502,-1.49490514287303,
-1.49265312027545,-1.49066610548489,-1.48799963132586,-1.48194934058225,
-1.47345024551375,-1.44894084451354,-1.38857164734317,-1.3800187117489,
-1.37561883703829,-1.3721049547582,-1.36811401181362,-1.36125184949231,
-1.3285933809597,-1.28218877469639,-1.26188622135384,-1.25772928959791,
-1.25540878585404,-1.25343370313395,-1.25087701062807,-1.24542761236607,
-1.23801716266803,-1.21834663865769,-1.20682946572698,-1.15215376976889,
-1.14287592453066,-1.13839133487293,-1.13486912035124,-1.1309308663737,
-1.12431214512924,-1.09609335014294,-1.06409684036266,-1.02791937825338,
-1.02166335560134,-1.01915371437839,-1.0171320839256,-1.01501548487916,
-1.01167399187847,-1.0007439690132,-0.98130423258884,-0.968028781115128,
-0.914962610035953,-0.905570343790112,-0.901064113184676,-0.897539589849428,
-0.893613914261244,-0.887052774060993,-0.859734433934364,-0.827109429478095,
-0.790514602968309,-0.784285731805667,-0.781780760959654,-0.779760412203886,
-0.777642073798023,-0.774292473562495,-0.763286511599889,-0.743640856571713,
-0.731864035548962,-0.677451036256476,-0.668153166831811,-0.663664940887641,
-0.660142527666568,-0.65620680828103,-0.649599014408321,-0.621550080724126,
-0.589434878029331,-0.553184169763361,-0.546934358455406,-0.544425868211862,
-0.542404632110245,-0.54028778475524,-0.536944751713608,-0.525999154515777,
-0.506516698972738,-0.493440679296154,-0.440228348932964,-0.430846043315784,
-0.426341876093813,-0.422817783558311,-0.418891368708921,-0.412326071473523,
-0.384939270089989,-0.352363406606311,-0.33180592744104),.UNSPECIFIED.);
#961=B_SPLINE_CURVE_WITH_KNOTS('',3,(#68550,#68551,#68552,#68553,#68554,
#68555,#68556,#68557,#68558,#68559,#68560,#68561,#68562,#68563,#68564,#68565,
#68566,#68567,#68568,#68569,#68570,#68571,#68572,#68573,#68574,#68575,#68576,
#68577,#68578,#68579,#68580,#68581,#68582,#68583,#68584,#68585,#68586,#68587,
#68588,#68589,#68590,#68591,#68592,#68593,#68594,#68595,#68596,#68597,#68598,
#68599,#68600,#68601,#68602,#68603,#68604,#68605,#68606,#68607,#68608,#68609,
#68610,#68611,#68612,#68613,#68614,#68615,#68616,#68617,#68618,#68619,#68620,
#68621,#68622,#68623,#68624,#68625,#68626,#68627,#68628,#68629,#68630,#68631,
#68632,#68633,#68634,#68635,#68636,#68637,#68638,#68639,#68640,#68641,#68642,
#68643,#68644,#68645,#68646,#68647,#68648,#68649,#68650,#68651,#68652,#68653,
#68654,#68655,#68656,#68657,#68658,#68659,#68660,#68661,#68662,#68663,#68664,
#68665,#68666,#68667,#68668,#68669,#68670,#68671,#68672,#68673,#68674,#68675,
#68676,#68677,#68678,#68679,#68680,#68681,#68682,#68683,#68684,#68685,#68686,
#68687,#68688,#68689,#68690,#68691,#68692,#68693,#68694,#68695,#68696,#68697,
#68698,#68699,#68700,#68701,#68702,#68703,#68704,#68705,#68706,#68707,#68708,
#68709,#68710,#68711,#68712,#68713,#68714,#68715,#68716,#68717,#68718,#68719,
#68720,#68721,#68722,#68723,#68724,#68725,#68726,#68727,#68728,#68729),
 .UNSPECIFIED.,.F.,.F.,(4,2,2,2,2,2,2,2,2,2,2,2,2,2,2,2,2,2,2,2,2,2,2,2,
2,2,2,2,2,2,2,2,2,2,2,2,2,2,2,2,2,2,2,2,2,2,2,2,2,2,2,2,2,2,2,2,2,2,2,2,
2,2,2,2,2,2,2,2,2,2,2,2,2,2,2,2,2,2,2,2,2,2,2,2,2,2,2,2,2,4),(-1.16363369234352,
-1.16295790678583,-1.15898823988006,-1.15222521336478,-1.12151620897351,
-1.0914958340154,-1.07796261271634,-1.05309843885021,-1.04911505999603,
-1.04662240929076,-1.04465156623561,-1.04228158322413,-1.0377723225715,
-0.999306261595195,-0.942744148510771,-0.933643853752399,-0.929193356432228,
-0.925674754874985,-0.921716221149426,-0.915003741001527,-0.885201841163423,
-0.854535777790885,-0.848020169730516,-0.815955518207676,-0.811881134326602,
-0.809361399704959,-0.807389161869915,-0.805041325635805,-0.800637404062841,
-0.769667244373821,-0.720955423652076,-0.700490299246686,-0.694268838917962,
-0.69041704342088,-0.686873898821883,-0.682221590823078,-0.672037005029608,
-0.658212364211504,-0.587646533901273,-0.576690947281024,-0.573223401629135,
-0.57107887319902,-0.569050507351872,-0.566131347764967,-0.558527132688328,
-0.54697430039157,-0.503767844145718,-0.465050987403647,-0.457868502874748,
-0.453765792591738,-0.450294235154145,-0.446055437065266,-0.438020902376893,
-0.398980220917527,-0.359911337502345,-0.340637027524395,-0.33653319357697,
-0.334224483342421,-0.332266412336735,-0.32970263543321,-0.32421663468579,
-0.316741411562477,-0.296800924411448,-0.257284792886249,-0.227183245499586,
-0.220308635565535,-0.216275186853487,-0.212922047147884,-0.212799261089963,
-0.212686912750328,-0.212583554354981,-0.212487997172239,-0.212399255293022,
-0.212316503547186,-0.212239045552849,-0.212166289148202,-0.21209772728177,
-0.207829510722542,-0.202892439011164,-0.194675785088698,-0.177398604672938,
-0.107522448590471,-0.10071895347576,-0.0981229310198588,-0.0962616113804328,
-0.0942146686741461,-0.0912019036092385,-0.0829525861352058,-0.0700249612576247,
-0.000702836714805313),.UNSPECIFIED.);
#962=B_SPLINE_CURVE_WITH_KNOTS('',3,(#68730,#68731,#68732,#68733,#68734,
#68735,#68736,#68737,#68738,#68739,#68740,#68741,#68742,#68743,#68744,#68745,
#68746,#68747,#68748,#68749,#68750,#68751,#68752,#68753,#68754,#68755,#68756,
#68757,#68758,#68759,#68760,#68761,#68762,#68763,#68764,#68765,#68766,#68767,
#68768,#68769,#68770,#68771,#68772,#68773,#68774,#68775,#68776,#68777,#68778,
#68779,#68780,#68781,#68782,#68783),.UNSPECIFIED.,.F.,.F.,(4,2,2,2,2,2,
2,2,2,2,2,2,2,2,2,2,2,2,2,2,2,2,2,2,2,2,4),(-2.98872595129121,-2.97578488693837,
-2.97135777031141,-2.96792934948171,-2.96453074422925,-2.96066679337635,
-2.95438691435237,-2.93333516725447,-2.89683441943583,-2.86718109747591,
-2.85767739453118,-2.85109695767192,-2.8483400404559,-2.84634053495174,
-2.84413463115462,-2.84038652557546,-2.82667029217726,-2.81346715947534,
-2.76270086129221,-2.74713932280744,-2.73949074450365,-2.7331382232944,
-2.72930337547387,-2.72596856016156,-2.72157180516364,-2.71303000503505,
-2.65746774305231),.UNSPECIFIED.);
#963=B_SPLINE_CURVE_WITH_KNOTS('',3,(#68785,#68786,#68787,#68788,#68789,
#68790,#68791,#68792,#68793,#68794,#68795,#68796,#68797,#68798,#68799,#68800,
#68801,#68802,#68803,#68804,#68805,#68806,#68807,#68808,#68809,#68810,#68811,
#68812,#68813,#68814,#68815,#68816,#68817,#68818,#68819,#68820,#68821,#68822,
#68823,#68824,#68825,#68826,#68827,#68828,#68829,#68830,#68831,#68832,#68833,
#68834,#68835,#68836,#68837,#68838,#68839,#68840,#68841,#68842,#68843,#68844,
#68845,#68846),.UNSPECIFIED.,.F.,.F.,(4,2,2,2,2,2,2,2,2,2,2,2,2,2,2,2,2,
2,2,2,2,2,2,2,2,2,2,2,2,2,4),(-0.33180592744104,-0.315805296192904,-0.30957522893432,
-0.307070148343933,-0.305049859303639,-0.302931767633533,-0.299582878262543,
-0.288582218983313,-0.268950293727248,-0.223440144617194,-0.198289806895859,
-0.191646535975279,-0.187703225161834,-0.184182389210223,-0.184091452403489,
-0.184007491759481,-0.183929715066348,-0.183857446652311,-0.183790106661967,
-0.179513058052387,-0.170230254477495,-0.157798514338694,-0.124947258169611,
-0.0779185224010441,-0.071920600512571,-0.0692920138102425,-0.067304111089287,
-0.0650570519110233,-0.0611225601528712,-0.0562441162046279,-0.000702637539615483),
 .UNSPECIFIED.);
#964=B_SPLINE_CURVE_WITH_KNOTS('',3,(#68847,#68848,#68849,#68850,#68851,
#68852,#68853,#68854,#68855,#68856,#68857,#68858,#68859,#68860,#68861,#68862,
#68863,#68864,#68865,#68866,#68867,#68868,#68869,#68870,#68871,#68872,#68873,
#68874,#68875,#68876,#68877,#68878,#68879,#68880,#68881,#68882,#68883,#68884,
#68885,#68886,#68887,#68888,#68889,#68890,#68891,#68892,#68893,#68894,#68895,
#68896,#68897,#68898,#68899,#68900,#68901,#68902,#68903,#68904,#68905,#68906,
#68907,#68908,#68909,#68910,#68911,#68912,#68913,#68914,#68915,#68916,#68917,
#68918,#68919,#68920,#68921,#68922,#68923,#68924,#68925,#68926,#68927,#68928,
#68929,#68930,#68931,#68932,#68933,#68934,#68935,#68936,#68937,#68938,#68939,
#68940,#68941,#68942,#68943,#68944,#68945,#68946,#68947,#68948,#68949,#68950,
#68951,#68952,#68953,#68954,#68955,#68956,#68957,#68958,#68959,#68960,#68961,
#68962,#68963,#68964,#68965,#68966,#68967,#68968,#68969,#68970,#68971,#68972,
#68973,#68974,#68975,#68976,#68977,#68978,#68979,#68980,#68981,#68982,#68983,
#68984,#68985,#68986,#68987,#68988,#68989,#68990,#68991,#68992,#68993,#68994,
#68995,#68996,#68997,#68998,#68999,#69000,#69001,#69002,#69003,#69004,#69005,
#69006,#69007,#69008,#69009,#69010,#69011,#69012,#69013,#69014,#69015,#69016,
#69017,#69018,#69019,#69020,#69021,#69022,#69023,#69024,#69025,#69026,#69027,
#69028,#69029,#69030,#69031,#69032,#69033,#69034,#69035,#69036),
 .UNSPECIFIED.,.F.,.F.,(4,2,2,2,2,2,2,2,2,2,2,2,2,2,2,2,2,2,2,2,2,2,2,2,
2,2,2,2,2,2,2,2,2,2,2,2,2,2,2,2,2,2,2,2,2,2,2,2,2,2,2,2,2,2,2,2,2,2,2,2,
2,2,2,2,2,2,2,2,2,2,2,2,2,2,2,2,2,2,2,2,2,2,2,2,2,2,2,2,2,2,2,2,2,2,4),
(-2.98905990044328,-2.95356430823409,-2.94714927655617,-2.94294742412976,
-2.93958726252696,-2.93642035663075,-2.93247526267118,-2.92581920350916,
-2.90044284942758,-2.87218225969175,-2.83060653310438,-2.82352687778292,
-2.82064631723278,-2.81862606589344,-2.81673656311586,-2.81347769259623,
-2.80415918418035,-2.7576997624601,-2.7277905846504,-2.7160400495557,-2.70712101398718,
-2.7028506940356,-2.70281464991139,-2.70277684132149,-2.70273717109788,
-2.70269553584728,-2.70265182547647,-2.70260592270797,-2.70255770254141,
-2.7025070316726,-2.70245376787538,-2.69894590063035,-2.69491914062542,
-2.68806671512818,-2.65812725990795,-2.61794577478734,-2.59830842794534,
-2.58730814182006,-2.58396012805575,-2.58184279810661,-2.57982339578818,
-2.57731961897877,-2.5710937022775,-2.53458065956312,-2.50205664648718,
-2.47466666310888,-2.46810324453046,-2.46417821058729,-2.46065551227561,
-2.45615334249306,-2.44677607040895,-2.39350809743223,-2.38051082805457,
-2.36099740625163,-2.35004264717796,-2.3466994201717,-2.34458307379871,
-2.34256283750361,-2.34005617094636,-2.33381372445072,-2.29756491818998,
-2.26543748373493,-2.23747517261891,-2.23087486133189,-2.22694169388657,
-2.22342037326959,-2.21893190459706,-2.20962754530034,-2.1553123885653,
-2.1434364330009,-2.12378815647395,-2.112783461603,-2.10943475344116,-2.10731712971016,
-2.10529757302389,-2.10279373648018,-2.09656833243039,-2.06002683241007,
-2.02734362059603,-2.00010997057961,-1.99355628585345,-1.98963311096651,
-1.98610959762098,-1.9816029511122,-1.97220348671927,-1.91927345342404,
-1.90574678403011,-1.88638187126658,-1.87548174853486,-1.8721442025444,
-1.87002896382351,-1.86800762120678,-1.86549731430977,-1.85923432920162,
-1.82631764215159),.UNSPECIFIED.);
#965=B_SPLINE_CURVE_WITH_KNOTS('',3,(#69041,#69042,#69043,#69044,#69045,
#69046,#69047,#69048,#69049,#69050,#69051,#69052,#69053,#69054,#69055,#69056,
#69057,#69058,#69059,#69060,#69061,#69062,#69063,#69064,#69065,#69066,#69067,
#69068,#69069,#69070,#69071,#69072,#69073,#69074,#69075,#69076,#69077,#69078,
#69079,#69080,#69081,#69082,#69083,#69084,#69085,#69086,#69087,#69088,#69089,
#69090,#69091,#69092,#69093,#69094,#69095,#69096,#69097,#69098,#69099,#69100,
#69101,#69102,#69103,#69104,#69105,#69106,#69107,#69108,#69109,#69110,#69111,
#69112,#69113,#69114,#69115,#69116,#69117,#69118,#69119,#69120,#69121,#69122,
#69123,#69124,#69125,#69126,#69127,#69128,#69129,#69130,#69131,#69132,#69133,
#69134,#69135,#69136,#69137,#69138,#69139,#69140,#69141,#69142,#69143,#69144,
#69145,#69146,#69147,#69148,#69149,#69150,#69151,#69152,#69153,#69154,#69155,
#69156,#69157,#69158,#69159,#69160,#69161,#69162,#69163,#69164,#69165,#69166,
#69167,#69168,#69169,#69170,#69171,#69172,#69173,#69174,#69175,#69176,#69177,
#69178,#69179,#69180,#69181,#69182,#69183,#69184,#69185,#69186,#69187,#69188,
#69189,#69190,#69191,#69192,#69193,#69194,#69195,#69196,#69197,#69198,#69199,
#69200,#69201,#69202,#69203,#69204,#69205,#69206,#69207,#69208,#69209,#69210,
#69211,#69212,#69213,#69214,#69215,#69216,#69217,#69218,#69219,#69220,#69221,
#69222,#69223,#69224,#69225,#69226,#69227,#69228,#69229,#69230,#69231,#69232,
#69233,#69234,#69235,#69236,#69237,#69238,#69239,#69240,#69241,#69242,#69243,
#69244,#69245,#69246,#69247,#69248,#69249,#69250),.UNSPECIFIED.,.F.,.F.,
(4,2,2,2,2,2,2,2,2,2,2,2,2,2,2,2,2,2,2,2,2,2,2,2,2,2,2,2,2,2,2,2,2,2,2,
2,2,2,2,2,2,2,2,2,2,2,2,2,2,2,2,2,2,2,2,2,2,2,2,2,2,2,2,2,2,2,2,2,2,2,2,
2,2,2,2,2,2,2,2,2,2,2,2,2,2,2,2,2,2,2,2,2,2,2,2,2,2,2,2,2,2,2,2,2,4),(-2.6576697293675,
-2.62693356030965,-2.59963849603588,-2.59307946384318,-2.58915432577582,
-2.58562980474747,-2.58112289068937,-2.57172656090521,-2.51873274140474,
-2.48961858642228,-2.48021271551229,-2.47368269100481,-2.47093379075845,
-2.46893514628557,-2.46672473782423,-2.46295770961296,-2.44903636057712,
-2.43954294382804,-2.39436598165337,-2.36281043950389,-2.35600381304448,
-2.35202498359897,-2.34850960811236,-2.34409166081447,-2.33545163989856,
-2.27577310478329,-2.25085890700078,-2.23806197693863,-2.23453475396773,
-2.23237720420162,-2.23037924308025,-2.22796302615207,-2.22182444982963,
-2.17736848466244,-2.14290057013905,-2.13011709390181,-2.12052339222402,
-2.11597916116625,-2.11244999659881,-2.10854468958577,-2.10207793278101,
-2.07920785943265,-2.03232312870307,-2.01180635265277,-2.00048504251354,
-1.99710191148193,-1.99497609620949,-1.99296031424258,-1.99047317134783,
-1.98434861621092,-1.94257217718088,-1.89025929208093,-1.88225382280685,
-1.87802128220995,-1.87455031213367,-1.87044296804023,-1.86323859252951,
-1.81779630197473,-1.78212141129576,-1.76415924880125,-1.76024667591471,
-1.75800423330561,-1.75601480347933,-1.7533768933276,-1.7473267197513,-1.70154696723194,
-1.66792529726364,-1.65532409981282,-1.64583566378124,-1.64131107444241,
-1.63778416204394,-1.63386807193642,-1.62735205102452,-1.60381133978621,
-1.55276607090862,-1.53560612823849,-1.52882308708679,-1.52373322947704,
-1.521245662974,-1.51946507544915,-1.51717209842833,-1.51313743318411,-1.49504714805063,
-1.4450067163768,-1.41388150306682,-1.40696678787983,-1.40292451817069,
-1.39941582134603,-1.39508757850367,-1.38661091855988,-1.35633736598825,
-1.30995296866614,-1.29001898432536,-1.28588066376219,-1.28356424957872,
-1.28158848375927,-1.27902543211187,-1.27354285316252,-1.26607358491697,
-1.24615740771257,-1.23867188706878,-1.17962157045517,-1.17090847983914,
-1.16647506272123,-1.16363369234352),.UNSPECIFIED.);
#966=B_SPLINE_CURVE_WITH_KNOTS('',3,(#69251,#69252,#69253,#69254,#69255,
#69256,#69257,#69258,#69259,#69260,#69261,#69262,#69263,#69264,#69265,#69266,
#69267,#69268,#69269,#69270,#69271,#69272,#69273,#69274,#69275,#69276,#69277,
#69278,#69279,#69280,#69281,#69282,#69283,#69284,#69285,#69286,#69287,#69288,
#69289,#69290,#69291,#69292,#69293,#69294,#69295,#69296,#69297,#69298,#69299,
#69300,#69301,#69302,#69303,#69304,#69305,#69306,#69307,#69308,#69309,#69310,
#69311,#69312,#69313,#69314,#69315,#69316,#69317,#69318,#69319,#69320,#69321,
#69322,#69323,#69324,#69325,#69326,#69327,#69328,#69329,#69330,#69331,#69332,
#69333,#69334,#69335,#69336,#69337,#69338,#69339,#69340,#69341,#69342,#69343,
#69344,#69345,#69346,#69347,#69348,#69349,#69350,#69351,#69352,#69353,#69354,
#69355,#69356,#69357,#69358,#69359,#69360,#69361,#69362,#69363,#69364,#69365,
#69366,#69367,#69368,#69369,#69370,#69371,#69372,#69373,#69374,#69375,#69376,
#69377,#69378,#69379,#69380,#69381,#69382,#69383,#69384,#69385,#69386,#69387,
#69388,#69389,#69390,#69391,#69392,#69393,#69394,#69395,#69396,#69397,#69398,
#69399,#69400,#69401,#69402,#69403,#69404,#69405,#69406,#69407,#69408,#69409,
#69410,#69411,#69412,#69413,#69414,#69415,#69416,#69417,#69418,#69419,#69420,
#69421,#69422,#69423,#69424,#69425,#69426,#69427,#69428,#69429,#69430,#69431,
#69432,#69433,#69434,#69435,#69436,#69437,#69438,#69439,#69440,#69441,#69442,
#69443,#69444,#69445,#69446,#69447,#69448,#69449,#69450,#69451,#69452,#69453,
#69454,#69455,#69456,#69457,#69458,#69459,#69460,#69461,#69462,#69463,#69464),
 .UNSPECIFIED.,.F.,.F.,(4,2,2,2,2,2,2,2,2,2,2,2,2,2,2,2,2,2,2,2,2,2,2,2,
2,2,2,2,2,2,2,2,2,2,2,2,2,2,2,2,2,2,2,2,2,2,2,2,2,2,2,2,2,2,2,2,2,2,2,2,
2,2,2,2,2,2,2,2,2,2,2,2,2,2,2,2,2,2,2,2,2,2,2,2,2,2,2,2,2,2,2,2,2,2,2,2,
2,2,2,2,2,2,2,2,2,2,4),(-1.82631764215159,-1.82323974212304,-1.79152376162018,
-1.76298270207981,-1.75634601678174,-1.75240470270774,-1.7488844669152,
-1.74440884748864,-1.73517333886562,-1.68030290659254,-1.66893018834484,
-1.64923526092079,-1.63821301849764,-1.63486220669421,-1.63274397836327,
-1.63072447281904,-1.62822135636435,-1.62200103721747,-1.58529636144442,
-1.55240489308472,-1.53457520866803,-1.52225548237389,-1.51724535046799,
-1.5136442226595,-1.51035968068673,-1.50593724067268,-1.49502235607148,
-1.46641734018428,-1.41376880896186,-1.40143651065848,-1.39781812808716,
-1.39564074228537,-1.39362991864508,-1.39080498538834,-1.38380786990236,
-1.37348959983616,-1.33905515883292,-1.29336992537318,-1.28372885815686,
-1.27922518629899,-1.27569230725627,-1.27180675209643,-1.26542817952572,
-1.24069225165136,-1.21145855783858,-1.16831607828925,-1.16271586727901,
-1.15977174715401,-1.15775926294019,-1.1556295362013,-1.15222711975135,
-1.14071368640189,-1.11965761476887,-1.07149671322946,-1.05038166234853,
-1.04408730632017,-1.04022007618033,-1.03668228958125,-1.03206536782902,
-1.02207402192909,-1.00859207388014,-0.970698662292824,-0.931210051675819,
-0.925002414273407,-0.922501318435399,-0.9204822266186,-0.918362882974066,
-0.915007637560058,-0.903945438473393,-0.884144897893716,-0.87447230987607,
-0.817879517185717,-0.808781412387799,-0.804331924231257,-0.800814120046543,
-0.796856502207348,-0.790145679118282,-0.760357682053604,-0.729674442472779,
-0.723479132630582,-0.691080046457897,-0.687005713714386,-0.684486280566667,
-0.682514476102601,-0.680167455892698,-0.675765919938365,-0.644881191381222,
-0.59639145952434,-0.575658933696101,-0.569408308775917,-0.565550734919029,
-0.562010421665312,-0.557373719609624,-0.547272360132232,-0.533595227739597,
-0.465426385481745,-0.452249073871324,-0.448548758491545,-0.446353157148726,
-0.444349470748219,-0.44156802406071,-0.434840934298955,-0.425054789053505,
-0.393819644382117,-0.343853452397251,-0.334314329759046,-0.33219634213793),
 .UNSPECIFIED.);
#967=B_SPLINE_CURVE_WITH_KNOTS('',3,(#69470,#69471,#69472,#69473,#69474,
#69475,#69476,#69477,#69478,#69479,#69480,#69481,#69482,#69483,#69484,#69485,
#69486,#69487,#69488,#69489,#69490,#69491,#69492,#69493,#69494,#69495,#69496,
#69497,#69498,#69499,#69500,#69501,#69502,#69503,#69504,#69505,#69506,#69507,
#69508,#69509,#69510,#69511,#69512,#69513,#69514,#69515,#69516,#69517,#69518,
#69519,#69520,#69521,#69522,#69523,#69524,#69525,#69526,#69527,#69528,#69529,
#69530,#69531,#69532,#69533,#69534,#69535,#69536,#69537,#69538,#69539,#69540,
#69541,#69542,#69543,#69544,#69545,#69546,#69547,#69548,#69549,#69550,#69551,
#69552,#69553,#69554,#69555,#69556,#69557,#69558,#69559,#69560,#69561,#69562,
#69563,#69564,#69565,#69566,#69567,#69568,#69569,#69570,#69571,#69572,#69573,
#69574,#69575,#69576,#69577,#69578,#69579,#69580,#69581,#69582,#69583,#69584,
#69585,#69586,#69587,#69588,#69589,#69590,#69591,#69592,#69593,#69594,#69595,
#69596,#69597,#69598,#69599,#69600,#69601,#69602,#69603,#69604,#69605,#69606,
#69607,#69608,#69609,#69610,#69611,#69612,#69613,#69614,#69615,#69616,#69617,
#69618,#69619,#69620,#69621,#69622,#69623,#69624,#69625,#69626,#69627,#69628,
#69629,#69630,#69631,#69632,#69633,#69634,#69635,#69636,#69637,#69638,#69639),
 .UNSPECIFIED.,.F.,.F.,(4,2,2,2,2,2,2,2,2,2,2,2,2,2,2,2,2,2,2,2,2,2,2,2,
2,2,2,2,2,2,2,2,2,2,2,2,2,2,2,2,2,2,2,2,2,2,2,2,2,2,2,2,2,2,2,2,2,2,2,2,
2,2,2,2,2,2,2,2,2,2,2,2,2,2,2,2,2,2,2,2,2,2,2,2,4),(-1.16381432242618,-1.15034453016281,
-1.14631361253183,-1.14380639924013,-1.1418343141596,-1.13947512224484,
-1.13501933608295,-1.10126307762493,-1.0452562761488,-1.03269120026321,
-1.02750312689733,-1.02423060693756,-1.02061422553913,-1.01552903802334,
-1.00273318698385,-0.983952151595484,-0.952057083173095,-0.915945783339466,
-0.909684730090513,-0.907173882166337,-0.905151596850594,-0.903034654707083,
-0.899693143534105,-0.888767569158273,-0.869340850180665,-0.856065961602515,
-0.802992184677781,-0.793600653706283,-0.789093910665508,-0.785568581601447,
-0.781641572301792,-0.775077103363844,-0.747722473777219,-0.715128091659899,
-0.6785584465486,-0.672328478162737,-0.669822970196079,-0.667802145157618,
-0.66568320272998,-0.662332394461906,-0.651319826716066,-0.631657243601803,
-0.620145463170004,-0.565471201201982,-0.556194577841849,-0.55170975195013,
-0.548186959735666,-0.544247633236188,-0.537626020356028,-0.509371007157941,
-0.477410593962117,-0.441245410368045,-0.434998076656561,-0.432489660282702,
-0.430468112729463,-0.428350427699331,-0.425005112437636,-0.414042930755737,
-0.394516619777133,-0.354898625088743,-0.324321711259594,-0.317434046355778,
-0.31339760889738,-0.309887953821573,-0.305550787110016,-0.297030998979092,
-0.266448197437599,-0.238090252622209,-0.203906000392167,-0.197684221561562,
-0.195180178397643,-0.19315980353295,-0.191040424325782,-0.187904420915456,
-0.178134655517359,-0.161526159435422,-0.127555530489142,-0.0875799587176907,
-0.0803823977286344,-0.0762762174834137,-0.0728046715442998,-0.0685695107018069,
-0.0605531604702257,-0.0504090877965985,-0.000702609627408209),
 .UNSPECIFIED.);
#968=B_SPLINE_CURVE_WITH_KNOTS('',3,(#69640,#69641,#69642,#69643,#69644,
#69645,#69646,#69647,#69648,#69649,#69650,#69651,#69652,#69653,#69654,#69655,
#69656,#69657,#69658,#69659,#69660,#69661,#69662,#69663,#69664,#69665,#69666,
#69667,#69668,#69669,#69670,#69671,#69672,#69673,#69674,#69675,#69676,#69677,
#69678,#69679,#69680,#69681,#69682,#69683,#69684,#69685,#69686,#69687,#69688,
#69689,#69690,#69691,#69692,#69693),.UNSPECIFIED.,.F.,.F.,(4,2,2,2,2,2,
2,2,2,2,2,2,2,2,2,2,2,2,2,2,2,2,2,2,2,2,4),(-2.98863346158678,-2.95253752221994,
-2.94897276709526,-2.94663648454277,-2.94476052864309,-2.94278912902029,
-2.94027942844017,-2.93623823846993,-2.90733953023107,-2.8748582676774,
-2.84132911968313,-2.83243581119988,-2.82788190376301,-2.82435205343567,
-2.82045290143933,-2.8140125313558,-2.79167428337775,-2.73689658821841,
-2.72132198789988,-2.7119512193783,-2.70895448893227,-2.70683556543818,
-2.70481573709573,-2.70231252513109,-2.69609346536451,-2.65952388738373,
-2.6576697293675),.UNSPECIFIED.);
#969=B_SPLINE_CURVE_WITH_KNOTS('',3,(#69695,#69696,#69697,#69698,#69699,
#69700,#69701,#69702,#69703,#69704,#69705,#69706,#69707,#69708,#69709,#69710,
#69711,#69712,#69713,#69714,#69715,#69716,#69717,#69718,#69719,#69720,#69721,
#69722,#69723,#69724,#69725,#69726,#69727,#69728,#69729,#69730,#69731,#69732,
#69733,#69734,#69735,#69736,#69737,#69738,#69739,#69740,#69741,#69742,#69743,
#69744,#69745,#69746,#69747,#69748,#69749,#69750,#69751,#69752,#69753,#69754,
#69755,#69756,#69757,#69758,#69759,#69760,#69761,#69762,#69763,#69764,#69765,
#69766,#69767,#69768,#69769,#69770,#69771,#69772,#69773,#69774,#69775,#69776,
#69777,#69778,#69779,#69780,#69781,#69782,#69783,#69784,#69785,#69786,#69787,
#69788,#69789,#69790,#69791,#69792,#69793,#69794,#69795,#69796,#69797,#69798),
 .UNSPECIFIED.,.F.,.F.,(4,2,2,2,2,2,2,2,2,2,2,2,2,2,2,2,2,2,2,2,2,2,2,2,
2,2,2,2,2,2,2,2,2,2,2,2,2,2,2,2,2,2,2,2,2,2,2,2,2,2,2,4),(-0.33219634213793,
-0.329780700017932,-0.326253263705674,-0.322343264986936,-0.315853218990654,
-0.289583593405523,-0.240675456116879,-0.216126043784944,-0.212163567942123,
-0.209677339654646,-0.207707026878352,-0.207685818623493,-0.207665034510622,
-0.207644659488958,-0.207624679188235,-0.207605079886582,-0.207585848468491,
-0.207566972395925,-0.207548439674398,-0.207530238828,-0.207512358866656,
-0.207494789267665,-0.207477519942781,-0.207460541221191,-0.207443843830181,
-0.207427418870173,-0.207411257791869,-0.207395352392427,-0.207379694790389,
-0.207364277408578,-0.207349092953033,-0.207334134421264,-0.207319395067114,
-0.207304868397298,-0.207290548154628,-0.207276428318404,-0.207262503074969,
-0.207248766830948,-0.207235214184885,-0.204785005062128,-0.199598524919195,
-0.192479352495597,-0.173996545250957,-0.113184680549314,-0.0991360032477435,
-0.0937136929300639,-0.0904001021820661,-0.0868217068297628,-0.0819424221188083,
-0.0704389941047528,-0.0285220420113346,-0.000702939858132017),
 .UNSPECIFIED.);
#970=B_SPLINE_CURVE_WITH_KNOTS('',3,(#69799,#69800,#69801,#69802,#69803,
#69804,#69805,#69806,#69807,#69808,#69809,#69810,#69811,#69812,#69813,#69814,
#69815,#69816,#69817,#69818,#69819,#69820,#69821,#69822,#69823,#69824,#69825,
#69826,#69827,#69828,#69829,#69830,#69831,#69832,#69833,#69834,#69835,#69836,
#69837,#69838,#69839,#69840,#69841,#69842,#69843,#69844,#69845,#69846,#69847,
#69848,#69849,#69850,#69851,#69852,#69853,#69854,#69855,#69856,#69857,#69858,
#69859,#69860,#69861,#69862,#69863,#69864,#69865,#69866,#69867,#69868,#69869,
#69870,#69871,#69872,#69873,#69874,#69875,#69876,#69877,#69878,#69879,#69880,
#69881,#69882,#69883,#69884,#69885,#69886,#69887,#69888,#69889,#69890,#69891,
#69892,#69893,#69894,#69895,#69896,#69897,#69898,#69899,#69900,#69901,#69902,
#69903,#69904,#69905,#69906,#69907,#69908,#69909,#69910,#69911,#69912,#69913,
#69914,#69915,#69916,#69917,#69918,#69919,#69920,#69921,#69922,#69923,#69924,
#69925,#69926,#69927,#69928,#69929,#69930,#69931,#69932,#69933,#69934,#69935,
#69936,#69937,#69938,#69939,#69940,#69941,#69942,#69943,#69944,#69945,#69946,
#69947,#69948,#69949,#69950,#69951,#69952,#69953,#69954,#69955,#69956,#69957,
#69958,#69959,#69960,#69961,#69962,#69963,#69964,#69965,#69966,#69967,#69968,
#69969,#69970,#69971,#69972),.UNSPECIFIED.,.F.,.F.,(4,2,2,2,2,2,2,2,2,2,
2,2,2,2,2,2,2,2,2,2,2,2,2,2,2,2,2,2,2,2,2,2,2,2,2,2,2,2,2,2,2,2,2,2,2,2,
2,2,2,2,2,2,2,2,2,2,2,2,2,2,2,2,2,2,2,2,2,2,2,2,2,2,2,2,2,2,2,2,2,2,2,2,
2,2,2,2,4),(-2.98923116400283,-2.97350991870706,-2.96578664491632,-2.9631530988098,
-2.96118316215222,-2.9592775365693,-2.95706493410813,-2.95328622285423,
-2.93922573353853,-2.92064083730378,-2.87219444671895,-2.85163865333969,
-2.84561657895374,-2.841808671401,-2.83825146479957,-2.8335812399366,-2.82300397488092,
-2.76465820540062,-2.75925053834816,-2.7392229460933,-2.73172790408425,
-2.72787624518902,-2.72465974888029,-2.72258397350011,-2.72056443361432,
-2.71806131387319,-2.7118411834863,-2.67548974943746,-2.64324945824292,
-2.61543268406738,-2.60884070663828,-2.60490889453594,-2.60138653790194,
-2.59689365497973,-2.58756866962727,-2.53349571784819,-2.52135871295193,
-2.5017323717477,-2.49073507268459,-2.48738676635101,-2.48526898138358,
-2.48324891131145,-2.48074406192153,-2.47451424885665,-2.4380334791975,
-2.40556070204055,-2.37807405548288,-2.37150300797432,-2.36757561032967,
-2.36405216580092,-2.35955094101059,-2.35018273025426,-2.29671933990866,
-2.2839249369236,-2.26437509173773,-2.25340581595576,-2.25006041290713,
-2.24794319687135,-2.2459225708695,-2.24341588188789,-2.2371757040023,-2.20085924559626,
-2.16863315120153,-2.14078883202881,-2.13419461343616,-2.13026205995826,
-2.12673941009988,-2.12224666344367,-2.1129238549481,-2.05880304139706,
-2.04670865598095,-2.0270758444224,-2.01607577759781,-2.01272695298232,
-2.01060891308836,-2.00858866296235,-2.00608365635305,-1.99985378414873,
-1.9633581611097,-1.92979684230373,-1.90327938960164,-1.89677237860318,
-1.89285864026042,-1.88933192404235,-1.88480493343468,-1.87530159794066,
-1.82652150981059),.UNSPECIFIED.);
#971=B_SPLINE_CURVE_WITH_KNOTS('',3,(#69977,#69978,#69979,#69980,#69981,
#69982,#69983,#69984,#69985,#69986,#69987,#69988,#69989,#69990,#69991,#69992,
#69993,#69994,#69995,#69996,#69997,#69998,#69999,#70000,#70001,#70002,#70003,
#70004,#70005,#70006,#70007,#70008,#70009,#70010,#70011,#70012,#70013,#70014,
#70015,#70016,#70017,#70018,#70019,#70020,#70021,#70022,#70023,#70024,#70025,
#70026,#70027,#70028,#70029,#70030,#70031,#70032,#70033,#70034,#70035,#70036,
#70037,#70038,#70039,#70040,#70041,#70042,#70043,#70044,#70045,#70046,#70047,
#70048,#70049,#70050,#70051,#70052,#70053,#70054,#70055,#70056,#70057,#70058,
#70059,#70060,#70061,#70062,#70063,#70064,#70065,#70066,#70067,#70068,#70069,
#70070,#70071,#70072,#70073,#70074,#70075,#70076,#70077,#70078,#70079,#70080,
#70081,#70082,#70083,#70084,#70085,#70086,#70087,#70088,#70089,#70090,#70091,
#70092,#70093,#70094,#70095,#70096,#70097,#70098,#70099,#70100,#70101,#70102,
#70103,#70104,#70105,#70106,#70107,#70108,#70109,#70110,#70111,#70112,#70113,
#70114,#70115,#70116,#70117,#70118,#70119,#70120,#70121,#70122,#70123,#70124,
#70125,#70126,#70127,#70128,#70129,#70130,#70131,#70132,#70133,#70134,#70135,
#70136,#70137,#70138,#70139,#70140,#70141,#70142,#70143,#70144,#70145,#70146,
#70147,#70148,#70149,#70150,#70151,#70152,#70153,#70154,#70155,#70156,#70157,
#70158,#70159,#70160,#70161,#70162,#70163,#70164,#70165,#70166,#70167,#70168,
#70169,#70170,#70171,#70172,#70173,#70174,#70175,#70176,#70177,#70178,#70179,
#70180,#70181,#70182,#70183,#70184,#70185,#70186,#70187,#70188),
 .UNSPECIFIED.,.F.,.F.,(4,2,2,2,2,2,2,2,2,2,2,2,2,2,2,2,2,2,2,2,2,2,2,2,
2,2,2,2,2,2,2,2,2,2,2,2,2,2,2,2,2,2,2,2,2,2,2,2,2,2,2,2,2,2,2,2,2,2,2,2,
2,2,2,2,2,2,2,2,2,2,2,2,2,2,2,2,2,2,2,2,2,2,2,2,2,2,2,2,2,2,2,2,2,2,2,2,
2,2,2,2,2,2,2,2,2,4),(-2.65803045946379,-2.64226021210847,-2.60283391067027,
-2.58329218308692,-2.57232559666882,-2.56898002275199,-2.56686245524302,
-2.56484124395464,-2.56233351631105,-2.55608914706894,-2.51983657207268,
-2.48770456775849,-2.45973838077491,-2.45313557848874,-2.44920059574953,
-2.44567742349223,-2.44118625988331,-2.43187494238457,-2.37760922753121,
-2.36566710851047,-2.34602694774608,-2.33502386378854,-2.33167425304181,
-2.32955572556937,-2.32753498003707,-2.32502927639262,-2.3187972248936,
-2.28234678185918,-2.24991529951816,-2.2223714872902,-2.21579537799238,
-2.21186605827334,-2.2083415585927,-2.20383988559011,-2.19447396592438,
-2.14096410474271,-2.12821561928296,-2.10866622379194,-2.09769641923997,
-2.09435027580758,-2.09223244070186,-2.09021105455898,-2.08770319432126,
-2.08145892018467,-2.04519237863354,-2.01304098640779,-1.98509444778547,
-1.97849238621133,-1.97455730643255,-1.97103371215114,-1.96654154998093,
-1.95722645550784,-1.90299233039496,-1.89101087342035,-1.87137241950139,
-1.86036957593958,-1.8570197677433,-1.85490105458919,-1.85288007929234,
-1.85037403564063,-1.84414086154228,-1.80812709664916,-1.77646543545933,
-1.74783435016955,-1.74118964342165,-1.73724517377457,-1.73372309304624,
-1.72924643422808,-1.7200134416298,-1.66476460763362,-1.65378875234948,
-1.63406228019062,-1.62302684766798,-1.61967342170932,-1.61755383339211,
-1.6155332456158,-1.61302896097876,-1.60680657728929,-1.57009141689533,
-1.53718816520174,-1.51936037772267,-1.50704009861802,-1.50202816598132,
-1.4984251755891,-1.49513853463789,-1.48987097426619,-1.47582800570569,
-1.45444190853355,-1.4041905518344,-1.38695828426794,-1.38297652127089,
-1.38069523149252,-1.37891235013502,-1.37640686913393,-1.37122724071527,
-1.3294021330354,-1.27783010482171,-1.26835652616225,-1.26383403716591,
-1.26030661010196,-1.25638774530475,-1.24986187247666,-1.22309546951146,
-1.18888163607689,-1.17856793304868,-1.16381432242618),.UNSPECIFIED.);
#972=B_SPLINE_CURVE_WITH_KNOTS('',3,(#70189,#70190,#70191,#70192,#70193,
#70194,#70195,#70196,#70197,#70198,#70199,#70200,#70201,#70202,#70203,#70204,
#70205,#70206,#70207,#70208,#70209,#70210,#70211,#70212,#70213,#70214,#70215,
#70216,#70217,#70218,#70219,#70220,#70221,#70222,#70223,#70224,#70225,#70226,
#70227,#70228,#70229,#70230,#70231,#70232,#70233,#70234,#70235,#70236,#70237,
#70238,#70239,#70240,#70241,#70242,#70243,#70244,#70245,#70246,#70247,#70248,
#70249,#70250,#70251,#70252,#70253,#70254,#70255,#70256,#70257,#70258,#70259,
#70260,#70261,#70262,#70263,#70264,#70265,#70266,#70267,#70268,#70269,#70270,
#70271,#70272,#70273,#70274,#70275,#70276,#70277,#70278,#70279,#70280,#70281,
#70282,#70283,#70284,#70285,#70286,#70287,#70288,#70289,#70290,#70291,#70292,
#70293,#70294,#70295,#70296,#70297,#70298,#70299,#70300,#70301,#70302,#70303,
#70304,#70305,#70306,#70307,#70308,#70309,#70310,#70311,#70312,#70313,#70314,
#70315,#70316,#70317,#70318,#70319,#70320,#70321,#70322,#70323,#70324,#70325,
#70326,#70327,#70328,#70329,#70330,#70331,#70332,#70333,#70334,#70335,#70336,
#70337,#70338,#70339,#70340,#70341,#70342,#70343,#70344,#70345,#70346,#70347,
#70348,#70349,#70350,#70351,#70352,#70353,#70354,#70355,#70356,#70357,#70358,
#70359,#70360,#70361,#70362,#70363,#70364,#70365,#70366,#70367,#70368,#70369,
#70370,#70371,#70372,#70373,#70374,#70375,#70376,#70377,#70378,#70379,#70380,
#70381,#70382,#70383,#70384,#70385,#70386,#70387,#70388,#70389,#70390,#70391,
#70392,#70393,#70394,#70395,#70396,#70397,#70398,#70399,#70400),
 .UNSPECIFIED.,.F.,.F.,(4,2,2,2,2,2,2,2,2,2,2,2,2,2,2,2,2,2,2,2,2,2,2,2,
2,2,2,2,2,2,2,2,2,2,2,2,2,2,2,2,2,2,2,2,2,2,2,2,2,2,2,2,2,2,2,2,2,2,2,2,
2,2,2,2,2,2,2,2,2,2,2,2,2,2,2,2,2,2,2,2,2,2,2,2,2,2,2,2,2,2,2,2,2,2,2,2,
2,2,2,2,2,2,2,2,2,4),(-1.82652150981059,-1.82436938606574,-1.79378793382466,
-1.78411596669254,-1.77744810307633,-1.77467634253647,-1.77267417723345,
-1.7704742614324,-1.76675459371402,-1.75336091165485,-1.6854537792428,-1.6717962571914,
-1.66170480454782,-1.65706968032381,-1.65352934909423,-1.6496705532801,
-1.6434152559009,-1.62264517566521,-1.57414675257705,-1.54325403633256,
-1.53885155126314,-1.53650419059199,-1.53453218780341,-1.53201263398553,
-1.52793840012921,-1.49537953414415,-1.44223245314841,-1.42672908473889,
-1.42109907187152,-1.41774675802364,-1.41419217730081,-1.40945954768364,
-1.39881962681617,-1.38417414468498,-1.33973219926227,-1.30610337622242,
-1.30202704769492,-1.29950689948934,-1.29753488080779,-1.29518801651949,
-1.2907878489589,-1.25998445097343,-1.21170428108578,-1.19072634557033,
-1.18444592019726,-1.1805816385128,-1.17704286144627,-1.17241931567192,
-1.16239202254442,-1.14884662567139,-1.08260439396749,-1.06757070578081,
-1.06370087915275,-1.06146790572012,-1.05947618839625,-1.05677415115838,
-1.05051957739217,-1.02066649511195,-0.967610382248828,-0.952041164521902,
-0.946377203075412,-0.943018172531551,-0.939466357131643,-0.934754296025357,
-0.924233766514298,-0.909805721577833,-0.86669207607966,-0.831351099773498,
-0.827262855721576,-0.82473900642763,-0.822766525063352,-0.820422001333221,
-0.816033770940867,-0.785799250185063,-0.738975316723177,-0.716270409628,
-0.709819769837866,-0.705918173118031,-0.702388533057668,-0.697838333695937,
-0.68821160420976,-0.675369237612917,-0.640628009802294,-0.596500135967312,
-0.590339045007555,-0.587919334539117,-0.585920620319059,-0.583764996257844,
-0.58024619689557,-0.567539328414932,-0.542914600957942,-0.482756059080605,
-0.474177651954468,-0.469772685899731,-0.466258644472913,-0.46227171211274,
-0.455427054685808,-0.423119707345982,-0.372679578173585,-0.355690131192574,
-0.351724357055762,-0.349447245693079,-0.347664550423079,-0.3451553943584,
-0.339953846388684,-0.332047463449011),.UNSPECIFIED.);
#973=B_SPLINE_CURVE_WITH_KNOTS('',3,(#70406,#70407,#70408,#70409,#70410,
#70411,#70412,#70413,#70414,#70415,#70416,#70417,#70418,#70419,#70420,#70421,
#70422,#70423,#70424,#70425,#70426,#70427,#70428,#70429,#70430,#70431,#70432,
#70433,#70434,#70435,#70436,#70437,#70438,#70439,#70440,#70441,#70442,#70443,
#70444,#70445,#70446,#70447,#70448,#70449,#70450,#70451,#70452,#70453,#70454,
#70455,#70456,#70457,#70458,#70459,#70460,#70461,#70462,#70463,#70464,#70465,
#70466,#70467,#70468,#70469,#70470,#70471,#70472,#70473,#70474,#70475,#70476,
#70477,#70478,#70479,#70480,#70481,#70482,#70483,#70484,#70485,#70486,#70487,
#70488,#70489,#70490,#70491,#70492,#70493,#70494,#70495,#70496,#70497,#70498,
#70499,#70500,#70501,#70502,#70503,#70504,#70505,#70506,#70507,#70508,#70509,
#70510,#70511,#70512,#70513,#70514,#70515,#70516,#70517,#70518,#70519,#70520,
#70521,#70522,#70523,#70524,#70525,#70526,#70527,#70528,#70529,#70530,#70531,
#70532,#70533,#70534,#70535,#70536,#70537,#70538,#70539,#70540,#70541,#70542,
#70543,#70544,#70545,#70546,#70547,#70548,#70549,#70550,#70551,#70552,#70553,
#70554,#70555,#70556,#70557,#70558,#70559,#70560,#70561,#70562,#70563,#70564,
#70565,#70566,#70567,#70568,#70569,#70570,#70571),.UNSPECIFIED.,.F.,.F.,
(4,2,2,2,2,2,2,2,2,2,2,2,2,2,2,2,2,2,2,2,2,2,2,2,2,2,2,2,2,2,2,2,2,2,2,
2,2,2,2,2,2,2,2,2,2,2,2,2,2,2,2,2,2,2,2,2,2,2,2,2,2,2,2,2,2,2,2,2,2,2,2,
2,2,2,2,2,2,2,2,2,2,2,4),(-1.16361468862912,-1.13591070982436,-1.12739573960449,
-1.12300314660491,-1.11948904505838,-1.11549133158903,-1.10860087101055,
-1.07536536616905,-1.03468119985899,-1.02350544422435,-1.00866901374354,
-1.00482211471208,-1.00259374415639,-1.00059988696707,-0.997886349066067,
-0.991567796525987,-0.961059762306479,-0.906062231532777,-0.892488769249181,
-0.887138685455116,-0.883837361075105,-0.880247274618603,-0.875306672853713,
-0.863434395695005,-0.798766725195472,-0.772267092181893,-0.768268255093271,
-0.765770573040939,-0.763798912615855,-0.761431740382097,-0.756938082041445,
-0.720301903177363,-0.661447563139146,-0.652707571750098,-0.648267981057946,
-0.644749529661597,-0.640782213240854,-0.634032665434681,-0.603593145875492,
-0.573360863187782,-0.561008217312841,-0.545252152865808,-0.533343227395491,
-0.529768495348602,-0.527600103862438,-0.525583740406508,-0.522731221088097,
-0.515564440822858,-0.504907929194273,-0.468289967457178,-0.425388760078435,
-0.415721958917442,-0.411212280110281,-0.407677194443301,-0.403791761436236,
-0.397419218251263,-0.372788821436176,-0.343797863991551,-0.300246372096205,
-0.294062694279302,-0.291638978528376,-0.289638846278831,-0.287484041524802,
-0.284346546321442,-0.273747708882288,-0.255105795635437,-0.196363923715957,
-0.180923789444152,-0.175301120334041,-0.171949275305025,-0.168392295787703,
-0.163651470457424,-0.153740463298352,-0.122274699879399,-0.0929452027344989,
-0.0603217159816636,-0.0562457572621282,-0.0537252348857149,-0.0517525044125253,
-0.0494042292088944,-0.046882861007685,-0.0428648294254301,-0.000702153330958493),
 .UNSPECIFIED.);
#974=B_SPLINE_CURVE_WITH_KNOTS('',3,(#70572,#70573,#70574,#70575,#70576,
#70577,#70578,#70579,#70580,#70581,#70582,#70583,#70584,#70585,#70586,#70587,
#70588,#70589,#70590,#70591,#70592,#70593,#70594,#70595,#70596,#70597,#70598,
#70599,#70600,#70601,#70602,#70603,#70604,#70605,#70606,#70607,#70608,#70609,
#70610,#70611,#70612,#70613,#70614,#70615,#70616,#70617,#70618,#70619,#70620,
#70621,#70622,#70623),.UNSPECIFIED.,.F.,.F.,(4,2,2,2,2,2,2,2,2,2,2,2,2,
2,2,2,2,2,2,2,2,2,2,2,2,4),(-2.9894592038886,-2.94072867183443,-2.93345639399262,
-2.92890227577676,-2.92463163473601,-2.92112602038026,-2.91703802497621,
-2.90992050663652,-2.8742516809235,-2.84276493212935,-2.81243649597813,
-2.80759053660584,-2.80558680107853,-2.80358191501645,-2.80138808309417,
-2.79769690939084,-2.78462552240191,-2.73789202785937,-2.71125105675867,
-2.70031357867313,-2.69181076867664,-2.68747734045533,-2.68396834782805,
-2.67993006001617,-2.6730328140185,-2.65803045946379),.UNSPECIFIED.);
#975=B_SPLINE_CURVE_WITH_KNOTS('',3,(#70625,#70626,#70627,#70628,#70629,
#70630,#70631,#70632,#70633,#70634,#70635,#70636,#70637,#70638,#70639,#70640,
#70641,#70642,#70643,#70644,#70645,#70646,#70647,#70648,#70649,#70650,#70651,
#70652,#70653,#70654,#70655,#70656,#70657,#70658,#70659,#70660,#70661,#70662,
#70663,#70664,#70665,#70666,#70667,#70668,#70669,#70670,#70671,#70672,#70673,
#70674,#70675,#70676,#70677,#70678,#70679,#70680,#70681,#70682,#70683,#70684,
#70685,#70686,#70687,#70688,#70689,#70690),.UNSPECIFIED.,.F.,.F.,(4,2,2,
2,2,2,2,2,2,2,2,2,2,2,2,2,2,2,2,2,2,2,2,2,2,2,2,2,2,2,2,2,4),(-0.332047463449011,
-0.303400555046417,-0.245829991390745,-0.237026875411861,-0.232534989753045,
-0.229098968084146,-0.228612501900887,-0.228394127212428,-0.228237036682089,
-0.228118050538032,-0.228024810459153,-0.227949958397452,-0.227888773545902,
-0.227731450566128,-0.227578535673357,-0.227428881830288,-0.22728149732593,
-0.227135505124343,-0.226990112389834,-0.226844587029383,-0.222200697807029,
-0.21079088074934,-0.171354894123508,-0.12100868122166,-0.115305898626846,
-0.112729868070505,-0.11074861658915,-0.10847020567436,-0.10439159902682,
-0.0833266707054811,-0.0240188320508272,-0.00836037945646354,-0.000702471133105883),
 .UNSPECIFIED.);
#976=B_SPLINE_CURVE_WITH_KNOTS('',3,(#70691,#70692,#70693,#70694,#70695,
#70696,#70697,#70698,#70699,#70700,#70701,#70702,#70703,#70704,#70705,#70706,
#70707,#70708,#70709,#70710,#70711,#70712,#70713,#70714,#70715,#70716,#70717,
#70718,#70719,#70720,#70721,#70722,#70723,#70724,#70725,#70726,#70727,#70728,
#70729,#70730,#70731,#70732,#70733,#70734,#70735,#70736,#70737,#70738,#70739,
#70740,#70741,#70742,#70743,#70744,#70745,#70746,#70747,#70748,#70749,#70750,
#70751,#70752,#70753,#70754,#70755,#70756,#70757,#70758,#70759,#70760,#70761,
#70762,#70763,#70764,#70765,#70766,#70767,#70768,#70769,#70770,#70771,#70772,
#70773,#70774,#70775,#70776,#70777,#70778,#70779,#70780,#70781,#70782,#70783,
#70784,#70785,#70786,#70787,#70788,#70789,#70790,#70791,#70792,#70793,#70794,
#70795,#70796,#70797,#70798,#70799,#70800,#70801,#70802,#70803,#70804,#70805,
#70806,#70807,#70808,#70809,#70810,#70811,#70812,#70813,#70814,#70815,#70816,
#70817,#70818,#70819,#70820,#70821,#70822,#70823,#70824,#70825,#70826,#70827,
#70828,#70829,#70830,#70831,#70832,#70833,#70834,#70835,#70836,#70837,#70838,
#70839,#70840,#70841,#70842,#70843,#70844,#70845,#70846,#70847,#70848,#70849,
#70850,#70851,#70852,#70853,#70854,#70855,#70856,#70857,#70858),
 .UNSPECIFIED.,.F.,.F.,(4,2,2,2,2,2,2,2,2,2,2,2,2,2,2,2,2,2,2,2,2,2,2,2,
2,2,2,2,2,2,2,2,2,2,2,2,2,2,2,2,2,2,2,2,2,2,2,2,2,2,2,2,2,2,2,2,2,2,2,2,
2,2,2,2,2,2,2,2,2,2,2,2,2,2,2,2,2,2,2,2,2,2,2,4),(-2.9888980801213,-2.98659890828846,
-2.98372924307055,-2.98037750013604,-2.97660887900156,-2.97098364046133,
-2.95463264440861,-2.93999827913173,-2.87627846302085,-2.86732908628589,
-2.86422334486029,-2.86215838745305,-2.86031599248123,-2.85730409716806,
-2.84965403019633,-2.80168606304042,-2.75794759340087,-2.75217033001485,
-2.74822915514659,-2.74445506241092,-2.74108388046826,-2.73654800310842,
-2.72753178281579,-2.67215361141063,-2.66093115514727,-2.64146094801411,
-2.63052210656701,-2.62718055804286,-2.6250645565352,-2.62304402637343,
-2.62053634261057,-2.61428806839151,-2.57811540436078,-2.5461094894657,
-2.51797645940766,-2.51136535820683,-2.50742980576017,-2.5039088629799,
-2.49942432461223,-2.49014086192319,-2.43555592122954,-2.42395092719871,
-2.40427759126799,-2.39326360791122,-2.38991386471929,-2.38779598840643,
-2.38577653862038,-2.38327319847313,-2.37705085480809,-2.34043052757807,
-2.30764415044508,-2.28056641255628,-2.27402292584378,-2.27010192077385,
-2.26657788533634,-2.26206714805437,-2.25264629305985,-2.20008228493633,
-2.15810035807378,-2.15357312426116,-2.15119987183147,-2.14922991060268,
-2.1467430050574,-2.14277743326965,-2.11831344385612,-2.10442749337622,
-2.07456474064297,-2.04368768256641,-2.03691734316567,-2.03294690440117,
-2.02943121059756,-2.02500253803345,-2.01630830097722,-1.9570621397245,
-1.94972305472276,-1.92977916688445,-1.9186654438361,-1.9153046936313,-1.91318416371864,
-1.91116589580897,-1.90866789846227,-1.90247818996896,-1.86296053730906,
-1.82609948607109),.UNSPECIFIED.);
#977=B_SPLINE_CURVE_WITH_KNOTS('',3,(#70863,#70864,#70865,#70866,#70867,
#70868,#70869,#70870,#70871,#70872,#70873,#70874,#70875,#70876,#70877,#70878,
#70879,#70880,#70881,#70882,#70883,#70884,#70885,#70886,#70887,#70888,#70889,
#70890,#70891,#70892,#70893,#70894,#70895,#70896,#70897,#70898,#70899,#70900,
#70901,#70902,#70903,#70904,#70905,#70906,#70907,#70908,#70909,#70910,#70911,
#70912,#70913,#70914,#70915,#70916,#70917,#70918,#70919,#70920,#70921,#70922,
#70923,#70924,#70925,#70926,#70927,#70928,#70929,#70930,#70931,#70932,#70933,
#70934,#70935,#70936,#70937,#70938,#70939,#70940,#70941,#70942,#70943,#70944,
#70945,#70946,#70947,#70948,#70949,#70950,#70951,#70952,#70953,#70954,#70955,
#70956,#70957,#70958,#70959,#70960,#70961,#70962,#70963,#70964,#70965,#70966,
#70967,#70968,#70969,#70970,#70971,#70972,#70973,#70974,#70975,#70976,#70977,
#70978,#70979,#70980,#70981,#70982,#70983,#70984,#70985,#70986,#70987,#70988,
#70989,#70990,#70991,#70992,#70993,#70994,#70995,#70996,#70997,#70998,#70999,
#71000,#71001,#71002,#71003,#71004,#71005,#71006,#71007,#71008,#71009,#71010,
#71011,#71012,#71013,#71014,#71015,#71016,#71017,#71018,#71019,#71020,#71021,
#71022,#71023,#71024,#71025,#71026,#71027,#71028,#71029,#71030,#71031,#71032,
#71033,#71034,#71035,#71036,#71037,#71038,#71039,#71040,#71041,#71042,#71043,
#71044,#71045,#71046,#71047,#71048,#71049,#71050,#71051,#71052,#71053,#71054,
#71055,#71056,#71057,#71058,#71059,#71060,#71061,#71062,#71063,#71064,#71065,
#71066,#71067,#71068,#71069,#71070),.UNSPECIFIED.,.F.,.F.,(4,2,2,2,2,2,
2,2,2,2,2,2,2,2,2,2,2,2,2,2,2,2,2,2,2,2,2,2,2,2,2,2,2,2,2,2,2,2,2,2,2,2,
2,2,2,2,2,2,2,2,2,2,2,2,2,2,2,2,2,2,2,2,2,2,2,2,2,2,2,2,2,2,2,2,2,2,2,2,
2,2,2,2,2,2,2,2,2,2,2,2,2,2,2,2,2,2,2,2,2,2,2,2,2,4),(-2.65786654937229,
-2.6529365402186,-2.61648033408661,-2.58403955006769,-2.55651262958186,
-2.54993782767042,-2.54600890460589,-2.54248452032328,-2.53798266299572,
-2.52861512193393,-2.4751384225726,-2.46235606426173,-2.44281234145399,
-2.43184480118368,-2.42849899929746,-2.4263813016966,-2.42435997855497,
-2.42185212503233,-2.4156075073799,-2.37935127603316,-2.34721496018183,
-2.31925058930345,-2.31264762143709,-2.30871245797945,-2.30518907286372,
-2.30069756776036,-2.29138528235673,-2.23712207514439,-2.22517348335998,
-2.20553274923148,-2.19452923598394,-2.19117945369731,-2.18906080855365,
-2.18703994283401,-2.18453408184178,-2.17830159719707,-2.14235895482372,
-2.11131316535685,-2.08206778362889,-2.07538664539881,-2.07143438562164,
-2.0679138608872,-2.06345075891303,-2.05428791893292,-1.99828144909136,
-1.98803054787728,-1.9682527331741,-1.96081640825548,-1.95535267996113,
-1.95279299150279,-1.95081731400885,-1.94849803922697,-1.94434778233372,
-1.92418216658248,-1.88578275523273,-1.84776166172448,-1.83932250656845,
-1.83500139510386,-1.83149266527866,-1.82744389699321,-1.82050206511842,
-1.78885264813844,-1.73924807985244,-1.72095566464168,-1.71702281726244,
-1.71477564877904,-1.71278686377196,-1.71015607233604,-1.70414857158634,
-1.65734930566419,-1.61503979350774,-1.60351415763342,-1.59863004531015,
-1.59504969827237,-1.59173538834381,-1.58631440511016,-1.5722833382831,
-1.51769942985883,-1.49482590101837,-1.48290401292882,-1.47932779798563,
-1.4771590216465,-1.47514271396149,-1.47229086315159,-1.46512881286195,
-1.4544819843237,-1.41793014562285,-1.37494295816848,-1.36527540143453,
-1.36076547077831,-1.35723023007053,-1.35334467007749,-1.34697201871411,
-1.32234264779079,-1.293355042916,-1.24980343393933,-1.24361357104473,-1.24118882418992,
-1.23918838409349,-1.23703393780808,-1.23352270748998,-1.22090615996886,
-1.1965683325924,-1.16361468862912),.UNSPECIFIED.);
#978=B_SPLINE_CURVE_WITH_KNOTS('',3,(#71071,#71072,#71073,#71074,#71075,
#71076,#71077,#71078,#71079,#71080,#71081,#71082,#71083,#71084,#71085,#71086,
#71087,#71088,#71089,#71090,#71091,#71092,#71093,#71094,#71095,#71096,#71097,
#71098,#71099,#71100,#71101,#71102,#71103,#71104,#71105,#71106,#71107,#71108,
#71109,#71110,#71111,#71112,#71113,#71114,#71115,#71116,#71117,#71118,#71119,
#71120,#71121,#71122,#71123,#71124,#71125,#71126,#71127,#71128,#71129,#71130,
#71131,#71132,#71133,#71134,#71135,#71136,#71137,#71138,#71139,#71140,#71141,
#71142,#71143,#71144,#71145,#71146,#71147,#71148,#71149,#71150,#71151,#71152,
#71153,#71154,#71155,#71156,#71157,#71158,#71159,#71160,#71161,#71162,#71163,
#71164,#71165,#71166,#71167,#71168,#71169,#71170,#71171,#71172,#71173,#71174,
#71175,#71176,#71177,#71178,#71179,#71180,#71181,#71182,#71183,#71184,#71185,
#71186,#71187,#71188,#71189,#71190,#71191,#71192,#71193,#71194,#71195,#71196,
#71197,#71198,#71199,#71200,#71201,#71202,#71203,#71204,#71205,#71206,#71207,
#71208,#71209,#71210,#71211,#71212,#71213,#71214,#71215,#71216,#71217,#71218,
#71219,#71220,#71221,#71222,#71223,#71224,#71225,#71226,#71227,#71228,#71229,
#71230,#71231,#71232,#71233,#71234,#71235,#71236,#71237,#71238,#71239,#71240,
#71241,#71242,#71243,#71244,#71245,#71246,#71247,#71248,#71249,#71250,#71251,
#71252,#71253,#71254,#71255,#71256,#71257,#71258,#71259,#71260,#71261,#71262,
#71263,#71264,#71265,#71266,#71267,#71268,#71269,#71270,#71271,#71272,#71273,
#71274,#71275,#71276,#71277,#71278,#71279,#71280,#71281,#71282,#71283,#71284,
#71285,#71286,#71287,#71288),.UNSPECIFIED.,.F.,.F.,(4,2,2,2,2,2,2,2,2,2,
2,2,2,2,2,2,2,2,2,2,2,2,2,2,2,2,2,2,2,2,2,2,2,2,2,2,2,2,2,2,2,2,2,2,2,2,
2,2,2,2,2,2,2,2,2,2,2,2,2,2,2,2,2,2,2,2,2,2,2,2,2,2,2,2,2,2,2,2,2,2,2,2,
2,2,2,2,2,2,2,2,2,2,2,2,2,2,2,2,2,2,2,2,2,2,2,2,2,2,4),(-1.82609948607109,
-1.82510996968395,-1.8116369689304,-1.80164973155598,-1.79703353778286,
-1.79349581271202,-1.78962815753855,-1.78333200611036,-1.76219866393818,
-1.7140161799052,-1.69294958838722,-1.68143315410374,-1.67803032566534,
-1.67590048245194,-1.67388798876404,-1.67094403250579,-1.66534467890069,
-1.62222450569465,-1.59300891821837,-1.56828106523965,-1.56190305076054,
-1.55801749114935,-1.55448437958399,-1.54998009637972,-1.54033656019384,
-1.49461990550496,-1.44845381150723,-1.44241901832225,-1.43978402625333,
-1.43779528270211,-1.43555188588275,-1.43163397910172,-1.41357468074426,
-1.37798327886645,-1.33259618679356,-1.32539282445486,-1.32128607478548,
-1.31781563837782,-1.31358380528806,-1.30557998214565,-1.29545545103272,
-1.27183423872731,-1.22155547238159,-1.20746257574622,-1.20368033329347,
-1.20146663653604,-1.19946919969576,-1.19672785001681,-1.1902424005164,
-1.18092324402375,-1.15227631392267,-1.09861442112409,-1.08926182411377,
-1.08476328800386,-1.08123983097987,-1.07731023210765,-1.07073026296823,
-1.04311677833627,-1.01069584273963,-0.974246084158036,-0.968010150439186,
-0.965504070479153,-0.963483517706516,-0.96136582288322,-0.958018733058799,
-0.947034812539828,-0.927448293919822,-0.915110099560047,-0.861243594017119,
-0.851905765605036,-0.847410120955484,-0.843887085393732,-0.839956051223714,
-0.833369093855505,-0.805644171055192,-0.773302555622228,-0.736906549956271,
-0.730667552316209,-0.728160997387964,-0.72614036307873,-0.724022957030094,
-0.720676974657335,-0.709702693275992,-0.690141965159893,-0.677593818717236,
-0.623924831487843,-0.614573571971335,-0.610075466793283,-0.606552254456802,
-0.602622832584194,-0.596042929282728,-0.568425609018339,-0.53601068474551,
-0.499565947704492,-0.493330261506392,-0.490824317619946,-0.488803889150593,
-0.486686342727361,-0.483339518987976,-0.472356762702184,-0.452772737415233,
-0.440424670819912,-0.38657171767054,-0.377233780102893,-0.372738291825032,
-0.36921547025124,-0.365284769398792,-0.358698598155218,-0.331874846602485),
 .UNSPECIFIED.);
#979=B_SPLINE_CURVE_WITH_KNOTS('',3,(#71294,#71295,#71296,#71297,#71298,
#71299,#71300,#71301,#71302),.UNSPECIFIED.,.F.,.F.,(4,1,1,1,1,1,4),(78.5398163397448,
79.1666675558176,80.1646843164291,81.1627010770406,82.1607178376521,83.1587345982636,
83.4308627901788),.UNSPECIFIED.);
#980=B_SPLINE_CURVE_WITH_KNOTS('',3,(#71303,#71304,#71305,#71306,#71307,
#71308,#71309,#71310,#71311,#71312,#71313,#71314,#71315,#71316,#71317,#71318,
#71319,#71320,#71321,#71322,#71323,#71324,#71325,#71326,#71327,#71328,#71329,
#71330,#71331,#71332,#71333,#71334,#71335,#71336,#71337,#71338,#71339,#71340,
#71341,#71342,#71343,#71344,#71345,#71346,#71347,#71348,#71349,#71350,#71351,
#71352),.UNSPECIFIED.,.F.,.F.,(4,2,2,2,2,2,2,2,2,2,2,2,2,2,2,2,2,2,2,2,
2,2,2,2,4),(-2.9889941003972,-2.94117567294498,-2.90849158293237,-2.90405444645073,
-2.9016996637602,-2.89972800366745,-2.897217195552,-2.89317276033964,-2.85752537112561,
-2.81606404242647,-2.80089711019658,-2.79338168698881,-2.78714903056937,
-2.78337719866878,-2.77985470062432,-2.77536634470668,-2.76606805850765,
-2.69980828847285,-2.68016585517106,-2.66916210449532,-2.66581251999726,
-2.66369406061272,-2.66167342460859,-2.65916790343206,-2.65786654937229),
 .UNSPECIFIED.);
#981=B_SPLINE_CURVE_WITH_KNOTS('',3,(#71354,#71355,#71356,#71357,#71358,
#71359,#71360,#71361,#71362,#71363,#71364,#71365,#71366,#71367,#71368,#71369,
#71370,#71371,#71372,#71373,#71374,#71375,#71376,#71377,#71378,#71379,#71380,
#71381,#71382,#71383,#71384,#71385,#71386,#71387,#71388,#71389,#71390,#71391,
#71392,#71393,#71394,#71395,#71396,#71397,#71398,#71399,#71400,#71401,#71402,
#71403,#71404,#71405,#71406,#71407,#71408,#71409),.UNSPECIFIED.,.F.,.F.,
(4,2,2,2,2,2,2,2,2,2,2,2,2,2,2,2,2,2,2,2,2,2,2,2,2,2,2,4),(-0.331874846602485,
-0.330981074388004,-0.2986376438995,-0.262216318443132,-0.255994998427963,
-0.25349155534447,-0.25147183558706,-0.249395938112561,-0.246159052427811,
-0.242292995033285,-0.234758194038605,-0.214564724868786,-0.16816964018585,
-0.144500175505225,-0.137975786707741,-0.134058544165221,-0.130533052275814,
-0.126013730315575,-0.116549587179866,-0.0785297517278548,-0.0345880112104803,
-0.0207453104793424,-0.016979886525497,-0.0147700193402066,-0.0128658034662866,
-0.0108942416976137,-0.00825649642932359,-0.000701672936245559),
 .UNSPECIFIED.);
#982=B_SPLINE_CURVE_WITH_KNOTS('',3,(#71410,#71411,#71412,#71413,#71414,
#71415,#71416,#71417,#71418,#71419,#71420,#71421,#71422,#71423,#71424,#71425,
#71426,#71427,#71428,#71429,#71430,#71431,#71432,#71433,#71434,#71435,#71436,
#71437,#71438,#71439,#71440,#71441,#71442,#71443,#71444,#71445,#71446,#71447,
#71448,#71449,#71450,#71451,#71452,#71453,#71454,#71455,#71456,#71457,#71458,
#71459,#71460,#71461,#71462,#71463,#71464,#71465,#71466,#71467,#71468,#71469,
#71470,#71471,#71472,#71473,#71474,#71475,#71476,#71477,#71478,#71479,#71480,
#71481,#71482,#71483,#71484,#71485,#71486,#71487,#71488,#71489,#71490,#71491,
#71492,#71493,#71494,#71495,#71496,#71497,#71498,#71499,#71500,#71501,#71502,
#71503,#71504,#71505,#71506,#71507,#71508,#71509,#71510,#71511,#71512,#71513,
#71514,#71515,#71516,#71517,#71518,#71519,#71520,#71521,#71522,#71523,#71524,
#71525,#71526,#71527,#71528,#71529,#71530,#71531,#71532,#71533,#71534,#71535,
#71536,#71537,#71538,#71539,#71540,#71541,#71542,#71543,#71544,#71545,#71546,
#71547,#71548,#71549,#71550,#71551,#71552,#71553,#71554,#71555,#71556,#71557,
#71558,#71559,#71560,#71561),.UNSPECIFIED.,.F.,.F.,(4,2,2,2,2,2,2,2,2,2,
2,2,2,2,2,2,2,2,2,2,2,2,2,2,2,2,2,2,2,2,2,2,2,2,2,2,2,2,2,2,2,2,2,2,2,2,
2,2,2,2,2,2,2,2,2,2,2,2,2,2,2,2,2,2,2,2,2,2,2,2,2,2,2,2,2,4),(-2.98947308457363,
-2.92733685589138,-2.89638058913975,-2.88960703955114,-2.88563639496454,
-2.88212153340197,-2.87769526821824,-2.8687142454158,-2.81101057210273,
-2.80104428855757,-2.78206038303968,-2.77481822994585,-2.77105751261116,
-2.76795891131662,-2.76589335283727,-2.76387418787005,-2.76137174871138,
-2.75515439156189,-2.71826833183109,-2.68498659539138,-2.65857976050418,
-2.65208173438772,-2.64817069337677,-2.64464469487812,-2.64011623552978,
-2.63060072423233,-2.58004290238287,-2.5374652052823,-2.5321516480703,-2.52962134718892,
-2.52764897186441,-2.52531067471624,-2.52107212068079,-2.49923698824174,
-2.45347336078277,-2.42185104324977,-2.4150423053918,-2.41106378256141,
-2.40754962611141,-2.40313449767996,-2.39450422966814,-2.33474836239405,
-2.30987416940064,-2.29709048226513,-2.29356514861299,-2.2914084367786,
-2.28941103148284,-2.28699531262287,-2.28085713125145,-2.23639916619518,
-2.20192705028659,-2.18914336216528,-2.17955005796697,-2.17500672324226,
-2.17147858558358,-2.16757476978702,-2.16111136876808,-2.1385051038632,
-2.09148709769598,-2.07087062992221,-2.0595142620841,-2.05612812272256,
-2.05400206684067,-2.05198749883866,-2.0495034068519,-2.04339396961612,
-2.00130874120363,-1.95382361140584,-1.94287953002613,-1.93809460359827,
-1.93453209220951,-1.93073634304694,-1.92477136632288,-1.9066149657525,
-1.85584575360824,-1.82652085594837),.UNSPECIFIED.);
#983=B_SPLINE_CURVE_WITH_KNOTS('',3,(#71567,#71568,#71569,#71570,#71571,
#71572,#71573,#71574,#71575,#71576,#71577,#71578,#71579,#71580,#71581,#71582,
#71583,#71584,#71585,#71586,#71587,#71588,#71589,#71590,#71591,#71592,#71593,
#71594,#71595,#71596,#71597,#71598,#71599,#71600,#71601,#71602,#71603,#71604,
#71605,#71606,#71607,#71608,#71609,#71610,#71611,#71612,#71613,#71614,#71615,
#71616,#71617,#71618,#71619,#71620,#71621,#71622,#71623,#71624,#71625,#71626,
#71627,#71628,#71629,#71630,#71631,#71632,#71633,#71634,#71635,#71636,#71637,
#71638,#71639,#71640,#71641,#71642,#71643,#71644,#71645,#71646,#71647,#71648,
#71649,#71650,#71651,#71652,#71653,#71654,#71655,#71656,#71657),
 .UNSPECIFIED.,.F.,.F.,(4,3,3,3,3,3,3,3,3,3,3,3,3,3,3,3,3,3,3,3,3,3,3,3,
3,3,3,3,3,3,4),(84.8230016469244,85.0319268137513,85.1547681194866,85.3334304922201,
85.5117309654079,85.6900028877257,85.8682449824607,86.0469043800704,86.1527848800981,
86.3314472528316,86.5097477260194,86.6880196483371,86.8662617430722,87.0449211406819,
87.1508016407096,87.3294640134431,87.5077644866309,87.6860364089486,87.8642785036837,
88.0429379012934,88.1488184013211,88.3274807740546,88.5057812472424,88.6840531695601,
88.8622952642952,89.0409546619049,89.1468351619326,89.3254945334179,89.503793727625,
89.6819399833619,89.7129494036681),.UNSPECIFIED.);
#984=B_SPLINE_CURVE_WITH_KNOTS('',3,(#71658,#71659,#71660,#71661,#71662),
 .UNSPECIFIED.,.F.,.F.,(4,1,4),(83.4308627901788,84.1567513588751,84.8230016469244),
 .UNSPECIFIED.);
#985=B_SPLINE_CURVE_WITH_KNOTS('',3,(#71663,#71664,#71665,#71666,#71667,
#71668,#71669,#71670,#71671,#71672,#71673,#71674,#71675,#71676,#71677,#71678,
#71679,#71680,#71681,#71682,#71683,#71684,#71685,#71686,#71687,#71688,#71689,
#71690,#71691,#71692,#71693,#71694,#71695,#71696,#71697,#71698,#71699,#71700,
#71701,#71702,#71703,#71704,#71705,#71706,#71707,#71708,#71709,#71710,#71711,
#71712,#71713,#71714,#71715,#71716,#71717,#71718,#71719,#71720,#71721,#71722,
#71723,#71724,#71725,#71726,#71727,#71728,#71729,#71730,#71731,#71732,#71733,
#71734,#71735,#71736,#71737,#71738,#71739,#71740,#71741,#71742,#71743,#71744,
#71745,#71746,#71747,#71748,#71749,#71750,#71751,#71752,#71753,#71754,#71755,
#71756,#71757,#71758,#71759,#71760,#71761,#71762,#71763,#71764,#71765,#71766,
#71767,#71768,#71769,#71770,#71771,#71772,#71773,#71774,#71775,#71776,#71777,
#71778,#71779,#71780,#71781,#71782,#71783,#71784,#71785,#71786,#71787,#71788,
#71789,#71790,#71791,#71792,#71793,#71794,#71795,#71796,#71797,#71798,#71799,
#71800,#71801,#71802,#71803,#71804,#71805,#71806,#71807,#71808,#71809,#71810,
#71811,#71812,#71813,#71814,#71815,#71816,#71817,#71818,#71819,#71820,#71821,
#71822,#71823,#71824,#71825,#71826,#71827,#71828,#71829,#71830,#71831,#71832,
#71833,#71834,#71835,#71836,#71837,#71838,#71839,#71840,#71841,#71842,#71843,
#71844,#71845,#71846,#71847,#71848,#71849,#71850,#71851,#71852,#71853,#71854,
#71855,#71856,#71857,#71858,#71859,#71860,#71861,#71862,#71863,#71864,#71865,
#71866,#71867,#71868,#71869,#71870,#71871,#71872,#71873,#71874,#71875,#71876,
#71877,#71878,#71879,#71880,#71881,#71882),.UNSPECIFIED.,.F.,.F.,(4,2,2,
2,2,2,2,2,2,2,2,2,2,2,2,2,2,2,2,2,2,2,2,2,2,2,2,2,2,2,2,2,2,2,2,2,2,2,2,
2,2,2,2,2,2,2,2,2,2,2,2,2,2,2,2,2,2,2,2,2,2,2,2,2,2,2,2,2,2,2,2,2,2,2,2,
2,2,2,2,2,2,2,2,2,2,2,2,2,2,2,2,2,2,2,2,2,2,2,2,2,2,2,2,2,2,2,2,2,2,4),
(-1.82652085594837,-1.82406204444472,-1.81964186274556,-1.81729087685041,
-1.81531930969633,-1.81280475315443,-1.80874701554698,-1.77878274140315,
-1.73297326394166,-1.70894901209819,-1.70262555105294,-1.69875202399187,
-1.69521604551064,-1.69068911637525,-1.68092074746702,-1.60672232488165,
-1.59279128133492,-1.5868869867704,-1.58231744638724,-1.57993505369438,
-1.57796500509951,-1.57548742120362,-1.571553959497,-1.54794573103635,-1.4953087126614,
-1.47184901451365,-1.46533974043969,-1.46142544076611,-1.45789872425181,
-1.4533724379117,-1.44387325730934,-1.43125181109302,-1.39753912636128,
-1.35181593332644,-1.34575844792861,-1.34311940214136,-1.34112999066883,
-1.33888859263984,-1.33498021751713,-1.31708208510641,-1.28134865949066,
-1.23591896765176,-1.22871491816466,-1.22460786486309,-1.22113722230895,
-1.21690519975155,-1.20890121066523,-1.19877657949399,-1.17515577025408,
-1.12485043332524,-1.11077443273345,-1.10699352183774,-1.10478003475333,
-1.1027823655374,-1.10004011595922,-1.09354991088976,-1.08422183417085,
-1.0555284691054,-1.00192981325635,-0.992572104563909,-0.988072434573773,
-0.9845486682627,-0.980619322144993,-0.97404121268974,-0.946461112941453,
-0.91401398756701,-0.877545494795288,-0.871310154955984,-0.868804089109916,
-0.866783458173022,-0.864665570228491,-0.861317981638216,-0.850330637741892,
-0.830735452233746,-0.818463111266026,-0.764530415381216,-0.75519654034019,
-0.750701482242022,-0.747178329724924,-0.743246568718614,-0.736656957371985,
-0.708895016571605,-0.676576249384858,-0.640194461918078,-0.633954014283076,
-0.631447125315986,-0.629426320719903,-0.62730885913475,-0.623963002758799,
-0.612991104872757,-0.593437445668221,-0.580824086013084,-0.527210797961385,
-0.517854932158082,-0.513355788937934,-0.509832278127396,-0.505903054778885,
-0.499324761201724,-0.471736955864815,-0.439298500178054,-0.402836868352165,
-0.39660167345509,-0.394095726216383,-0.392075214979328,-0.389957482383299,
-0.386610191357697,-0.375624304361944,-0.356032405917324,-0.352157376078528,
-0.332127671321822),.UNSPECIFIED.);
#986=B_SPLINE_CURVE_WITH_KNOTS('',3,(#71888,#71889,#71890,#71891,#71892,
#71893,#71894,#71895,#71896),.UNSPECIFIED.,.F.,.F.,(4,1,1,1,1,1,4),(91.1061869541039,
91.1428686831556,92.1408854437671,93.1389022043786,94.1369189649901,95.1349357256016,
95.9956065629),.UNSPECIFIED.);
#987=B_SPLINE_CURVE_WITH_KNOTS('',3,(#71897,#71898,#71899,#71900,#71901,
#71902,#71903,#71904,#71905,#71906,#71907,#71908,#71909,#71910,#71911,#71912,
#71913,#71914,#71915,#71916,#71917,#71918,#71919,#71920,#71921,#71922,#71923,
#71924),.UNSPECIFIED.,.F.,.F.,(4,3,3,3,3,3,3,3,3,4),(89.7129494036681,89.8912023488036,
90.0698639783069,90.1448519225441,90.3224643810971,90.4997174006465,90.6769397930551,
90.8541428000862,91.031738874977,91.1061866323843),.UNSPECIFIED.);
#988=B_SPLINE_CURVE_WITH_KNOTS('',3,(#71926,#71927,#71928,#71929,#71930,
#71931,#71932,#71933,#71934,#71935,#71936,#71937,#71938,#71939,#71940,#71941,
#71942,#71943,#71944,#71945,#71946,#71947,#71948,#71949,#71950,#71951,#71952,
#71953,#71954,#71955,#71956,#71957,#71958,#71959,#71960,#71961,#71962,#71963,
#71964,#71965,#71966,#71967,#71968,#71969,#71970,#71971,#71972,#71973,#71974,
#71975,#71976,#71977,#71978,#71979,#71980,#71981),.UNSPECIFIED.,.F.,.F.,
(4,2,2,2,2,2,2,2,2,2,2,2,2,2,2,2,2,2,2,2,2,2,2,2,2,2,2,4),(-0.332127671321822,
-0.299591807458999,-0.283455651450869,-0.277740657579193,-0.273998034540904,
-0.270479790062397,-0.265706351666199,-0.260339045591067,-0.251038651666556,
-0.230274082707922,-0.187317120202878,-0.16247760069458,-0.158495652787689,
-0.156003629954979,-0.154033118948062,-0.151663403654923,-0.147154364224762,
-0.10867916126003,-0.0800334345805236,-0.0554583953642009,-0.0443802412136993,
-0.0399300768661818,-0.036638401707461,-0.0333021077236981,-0.0297950850530563,
-0.0251378361559023,-0.0157283595091443,-0.000701629447673439),
 .UNSPECIFIED.);
#989=B_SPLINE_CURVE_WITH_KNOTS('',3,(#71982,#71983,#71984,#71985,#71986,
#71987,#71988,#71989,#71990),.UNSPECIFIED.,.F.,.F.,(4,1,1,1,1,1,4),(91.106194480469,
91.4563736967383,92.4543904573498,93.4524072179613,94.4504239785728,95.4484407391843,
95.996079334354),.UNSPECIFIED.);
#990=B_SPLINE_CURVE_WITH_KNOTS('',3,(#71996,#71997,#71998,#71999,#72000,
#72001,#72002,#72003,#72004,#72005,#72006,#72007,#72008,#72009,#72010,#72011,
#72012,#72013,#72014,#72015,#72016,#72017,#72018,#72019,#72020,#72021,#72022,
#72023,#72024,#72025,#72026,#72027,#72028,#72029,#72030,#72031,#72032,#72033,
#72034,#72035,#72036,#72037,#72038,#72039,#72040,#72041,#72042,#72043,#72044,
#72045,#72046,#72047,#72048,#72049,#72050,#72051,#72052,#72053,#72054,#72055,
#72056,#72057,#72058,#72059,#72060,#72061,#72062,#72063,#72064,#72065,#72066,
#72067,#72068,#72069,#72070,#72071,#72072,#72073,#72074,#72075,#72076,#72077,
#72078,#72079,#72080,#72081,#72082,#72083,#72084,#72085,#72086,#72087,#72088,
#72089,#72090,#72091,#72092,#72093,#72094,#72095,#72096,#72097,#72098,#72099,
#72100,#72101,#72102,#72103,#72104,#72105,#72106,#72107,#72108,#72109,#72110,
#72111,#72112,#72113,#72114,#72115,#72116,#72117,#72118,#72119,#72120,#72121,
#72122,#72123,#72124,#72125,#72126,#72127,#72128,#72129,#72130,#72131,#72132,
#72133,#72134,#72135,#72136,#72137,#72138,#72139,#72140,#72141,#72142,#72143,
#72144,#72145,#72146,#72147,#72148,#72149,#72150,#72151,#72152,#72153,#72154,
#72155,#72156,#72157,#72158,#72159,#72160,#72161,#72162,#72163,#72164,#72165,
#72166,#72167),.UNSPECIFIED.,.F.,.F.,(4,2,2,2,2,2,2,2,2,2,2,2,2,2,2,2,2,
2,2,2,2,2,2,2,2,2,2,2,2,2,2,2,2,2,2,2,2,2,2,2,2,2,2,2,2,2,2,2,2,2,2,2,2,
2,2,2,2,2,2,2,2,2,2,2,2,2,2,2,2,2,2,2,2,2,2,2,2,2,2,2,2,2,2,2,2,4),(-1.16377943473109,
-1.13667956176578,-1.13045090196268,-1.1279456124005,-1.12592484053518,
-1.12380580106815,-1.12045457308714,-1.1094381599184,-1.0897651603648,-1.07837264907427,
-1.02357821268739,-1.01431140261525,-1.00982843926737,-1.00630583920957,
-1.00236540661045,-0.99573873190497,-0.967402188916012,-0.935500534693839,
-0.89938622056169,-0.893125984467853,-0.890615367303459,-0.888593229381796,
-0.88647639381595,-0.883134968107134,-0.872208914988976,-0.852780266295189,
-0.839517205197489,-0.786439707263261,-0.777049210924262,-0.772542836982356,
-0.769017741164505,-0.765090934536453,-0.758526667461252,-0.7311704820101,
-0.698580374647938,-0.662014660086823,-0.655785011257002,-0.65327964941036,
-0.651258949256087,-0.649140146510012,-0.645789574347334,-0.634777923482864,
-0.615117180234838,-0.603599419819502,-0.548935353963225,-0.539658772994035,
-0.535174127642822,-0.531651547760321,-0.527712531956804,-0.521091618809152,
-0.492842901799532,-0.460881269876965,-0.424731042404923,-0.4184742426345,
-0.415964306041933,-0.413942439372104,-0.411825544199055,-0.408483428307811,
-0.3975496540837,-0.378099496376652,-0.338366396719334,-0.307799421267046,
-0.300912601073609,-0.296876512324182,-0.293367072107328,-0.289030057197502,
-0.280715454250318,-0.269957205264194,-0.24400137354993,-0.190223629223084,
-0.181909822594664,-0.178795673811416,-0.176933414545376,-0.174888038183566,
-0.171881907488153,-0.163947871844611,-0.133545860916829,-0.101653494706863,
-0.0705270088481122,-0.0636114617079553,-0.0595686484081738,-0.0560594453317889,
-0.0526885679464537,-0.0484540398396745,-0.0419619959446415,-0.000702059288745545),
 .UNSPECIFIED.);
#991=B_SPLINE_CURVE_WITH_KNOTS('',3,(#72168,#72169,#72170,#72171,#72172,
#72173),.UNSPECIFIED.,.F.,.F.,(4,1,1,4),(95.9956065629,96.1329524862131,
97.1309692468246,97.3893698744215),.UNSPECIFIED.);
#992=B_SPLINE_CURVE_WITH_KNOTS('',3,(#72175,#72176,#72177,#72178,#72179),
 .UNSPECIFIED.,.F.,.F.,(4,1,4),(95.996079334354,96.4464574997958,97.3893656567973),
 .UNSPECIFIED.);
#993=B_SPLINE_CURVE_WITH_KNOTS('',3,(#72180,#72181,#72182,#72183,#72184,
#72185,#72186,#72187,#72188,#72189,#72190,#72191,#72192,#72193,#72194,#72195,
#72196,#72197,#72198,#72199,#72200,#72201,#72202,#72203,#72204,#72205,#72206,
#72207,#72208,#72209,#72210,#72211,#72212,#72213,#72214,#72215,#72216,#72217,
#72218,#72219,#72220,#72221,#72222,#72223,#72224,#72225,#72226,#72227,#72228,
#72229,#72230,#72231,#72232,#72233,#72234,#72235,#72236,#72237,#72238,#72239,
#72240,#72241,#72242,#72243,#72244,#72245,#72246,#72247,#72248,#72249,#72250,
#72251,#72252,#72253,#72254,#72255,#72256,#72257,#72258,#72259,#72260,#72261,
#72262,#72263,#72264,#72265,#72266,#72267,#72268,#72269,#72270,#72271,#72272,
#72273,#72274,#72275,#72276,#72277,#72278,#72279,#72280,#72281,#72282,#72283,
#72284,#72285,#72286,#72287,#72288,#72289,#72290,#72291,#72292,#72293,#72294,
#72295,#72296,#72297,#72298,#72299,#72300,#72301,#72302,#72303,#72304,#72305,
#72306,#72307,#72308,#72309,#72310,#72311,#72312,#72313,#72314,#72315,#72316,
#72317,#72318,#72319,#72320,#72321,#72322,#72323,#72324,#72325,#72326,#72327,
#72328,#72329,#72330,#72331,#72332,#72333,#72334,#72335,#72336,#72337,#72338,
#72339,#72340,#72341,#72342,#72343,#72344,#72345,#72346,#72347,#72348,#72349,
#72350,#72351),.UNSPECIFIED.,.F.,.F.,(4,2,2,2,2,2,2,2,2,2,2,2,2,2,2,2,2,
2,2,2,2,2,2,2,2,2,2,2,2,2,2,2,2,2,2,2,2,2,2,2,2,2,2,2,2,2,2,2,2,2,2,2,2,
2,2,2,2,2,2,2,2,2,2,2,2,2,2,2,2,2,2,2,2,2,2,2,2,2,2,2,2,2,2,2,2,4),(-2.9892703890057,
-2.9823293267889,-2.97967926444857,-2.97770338579837,-2.97580400447087,
-2.97360337628722,-2.96987933182125,-2.95645419292063,-2.91212960597214,
-2.8740695662292,-2.86460074454386,-2.86008076832223,-2.85655543405299,
-2.85263904948626,-2.8461177294965,-2.82248807884642,-2.77601739515326,
-2.75581084499323,-2.74827323306626,-2.74440636965689,-2.74116897950214,
-2.73909314965936,-2.73707361416644,-2.73457056144009,-2.72835090623037,
-2.69180193695157,-2.65924650537483,-2.6318849924972,-2.62532228158849,
-2.62139680131418,-2.61787315794747,-2.6133690279307,-2.60398485832457,
-2.55077735558636,-2.53768969729674,-2.51818634582801,-2.50723441216217,
-2.50389097083125,-2.5017742459579,-2.49975343760858,-2.49724584057276,
-2.49099996339123,-2.45476888944137,-2.42267551461133,-2.39464810273235,
-2.38804253479454,-2.38410762668271,-2.38058561321519,-2.37609745008294,
-2.36679812367136,-2.31237591440713,-2.30059248280992,-2.28093059061991,
-2.26991997875084,-2.26657011535626,-2.26445190593492,-2.26243191603646,
-2.25992767356055,-2.2537019187108,-2.21712539431818,-2.18452001193097,
-2.15722547423224,-2.15066665133557,-2.14674175979895,-2.14321755657897,
-2.13871120606279,-2.12931677500273,-2.07625358640812,-2.06297462148709,
-2.04350718658637,-2.03256816030637,-2.02922589059238,-2.02710928228442,
-2.02508804232384,-2.02257934107501,-2.01632784170074,-1.98015906965377,
-1.94816786533809,-1.91999085337202,-1.9133754341131,-1.90943813318859,
-1.90591613654818,-1.90143095586146,-1.8921487475923,-1.83749295151946,
-1.82646872808304),.UNSPECIFIED.);
#994=B_SPLINE_CURVE_WITH_KNOTS('',3,(#72356,#72357,#72358,#72359,#72360,
#72361,#72362,#72363,#72364,#72365,#72366,#72367,#72368,#72369,#72370,#72371,
#72372,#72373,#72374,#72375,#72376,#72377,#72378,#72379,#72380,#72381,#72382,
#72383,#72384,#72385,#72386,#72387,#72388,#72389,#72390,#72391,#72392,#72393,
#72394,#72395,#72396,#72397,#72398,#72399,#72400,#72401,#72402,#72403,#72404,
#72405,#72406,#72407,#72408,#72409,#72410,#72411,#72412,#72413,#72414,#72415,
#72416,#72417,#72418,#72419,#72420,#72421,#72422,#72423,#72424,#72425,#72426,
#72427,#72428,#72429,#72430,#72431,#72432,#72433,#72434,#72435,#72436,#72437,
#72438,#72439,#72440,#72441,#72442,#72443,#72444,#72445,#72446,#72447,#72448,
#72449,#72450,#72451,#72452,#72453,#72454,#72455,#72456,#72457,#72458,#72459,
#72460,#72461,#72462,#72463,#72464,#72465,#72466,#72467,#72468,#72469,#72470,
#72471,#72472,#72473,#72474,#72475,#72476,#72477,#72478,#72479,#72480,#72481,
#72482,#72483,#72484,#72485,#72486,#72487,#72488,#72489,#72490,#72491,#72492,
#72493,#72494,#72495,#72496,#72497,#72498,#72499,#72500,#72501,#72502,#72503,
#72504,#72505,#72506,#72507,#72508,#72509,#72510,#72511,#72512,#72513,#72514,
#72515,#72516,#72517,#72518,#72519,#72520,#72521,#72522,#72523,#72524,#72525,
#72526,#72527,#72528,#72529,#72530,#72531,#72532,#72533,#72534,#72535,#72536,
#72537,#72538,#72539,#72540,#72541,#72542,#72543,#72544,#72545,#72546,#72547,
#72548,#72549,#72550,#72551,#72552,#72553,#72554,#72555,#72556,#72557,#72558,
#72559),.UNSPECIFIED.,.F.,.F.,(4,2,2,2,2,2,2,2,2,2,2,2,2,2,2,2,2,2,2,2,
2,2,2,2,2,2,2,2,2,2,2,2,2,2,2,2,2,2,2,2,2,2,2,2,2,2,2,2,2,2,2,2,2,2,2,2,
2,2,2,2,2,2,2,2,2,2,2,2,2,2,2,2,2,2,2,2,2,2,2,2,2,2,2,2,2,2,2,2,2,2,2,2,
2,2,2,2,2,2,2,2,2,4),(-2.65808389942519,-2.65277394623415,-2.59767167014398,
-2.58656866339038,-2.56685693963098,-2.55582781778381,-2.55247557922228,
-2.550356577752,-2.54833640780605,-2.54583249295435,-2.53961028581393,-2.50294823173905,
-2.47661926235894,-2.446461040162,-2.43800000313917,-2.43367490672409,-2.43016642202381,
-2.42612180169746,-2.41919665311614,-2.38786795491194,-2.33797449475571,
-2.31964093649969,-2.3157061076181,-2.31345871713196,-2.3114703727123,-2.30884098866981,
-2.30284015364627,-2.25592661949482,-2.21372771078657,-2.20220994318211,
-2.19732758064353,-2.19374794841591,-2.18998454726976,-2.18417468473529,
-2.16729995971609,-2.11538285120956,-2.09325134954899,-2.08136490569739,
-2.07792413295315,-2.07578549389969,-2.07377713317466,-2.07085765068759,
-2.06535387070975,-2.02023711114846,-2.00922190768722,-1.97601274821715,
-1.96476706798689,-1.95992981069991,-1.95635759988333,-1.95257850193309,
-1.94669594264607,-1.92923773811265,-1.87178701369637,-1.85398164354678,
-1.84703265287146,-1.84184670074219,-1.83934017996461,-1.83755738826615,
-1.83527732493811,-1.83130021278135,-1.81412985642557,-1.76387159699003,
-1.73164094020065,-1.72479917716338,-1.72081215389211,-1.71729694034793,
-1.71288903404803,-1.7043001195289,-1.64418347134513,-1.61950836537465,
-1.60678559081765,-1.60326461442913,-1.60110811297851,-1.59910890025017,
-1.59668888897386,-1.59052845049766,-1.54643273564435,-1.49514233000848,
-1.48852206849158,-1.48420538822187,-1.48069687628701,-1.47664459478316,
-1.46949997627083,-1.4294475624368,-1.39139830629019,-1.37070151275081,
-1.3665228907123,-1.36419720629851,-1.36222220233128,-1.35967134039627,
-1.35425453712602,-1.31035598933721,-1.2613934468669,-1.25276784104122,
-1.24835836250884,-1.24507586755536,-1.24146953271487,-1.23643819616118,
-1.22399226690946,-1.20591262178753,-1.17327852828172,-1.16377943473109),
 .UNSPECIFIED.);
#995=B_SPLINE_CURVE_WITH_KNOTS('',3,(#72560,#72561,#72562,#72563,#72564,
#72565,#72566,#72567,#72568,#72569,#72570,#72571,#72572,#72573,#72574,#72575,
#72576,#72577,#72578,#72579,#72580,#72581,#72582,#72583,#72584,#72585,#72586,
#72587,#72588,#72589,#72590,#72591,#72592,#72593,#72594,#72595,#72596,#72597,
#72598,#72599,#72600,#72601,#72602,#72603,#72604,#72605,#72606,#72607,#72608,
#72609,#72610,#72611,#72612,#72613,#72614,#72615,#72616,#72617,#72618,#72619,
#72620,#72621,#72622,#72623,#72624,#72625,#72626,#72627,#72628,#72629,#72630,
#72631,#72632,#72633,#72634,#72635,#72636,#72637,#72638,#72639,#72640,#72641,
#72642,#72643,#72644,#72645,#72646,#72647,#72648,#72649,#72650,#72651,#72652,
#72653,#72654,#72655,#72656,#72657,#72658,#72659,#72660,#72661,#72662,#72663,
#72664,#72665,#72666,#72667,#72668,#72669,#72670,#72671,#72672,#72673,#72674,
#72675,#72676,#72677,#72678,#72679,#72680,#72681,#72682,#72683,#72684,#72685,
#72686,#72687,#72688,#72689,#72690,#72691,#72692,#72693,#72694,#72695,#72696,
#72697,#72698,#72699,#72700,#72701,#72702,#72703,#72704,#72705,#72706,#72707,
#72708,#72709,#72710,#72711,#72712,#72713,#72714,#72715,#72716,#72717,#72718,
#72719,#72720,#72721,#72722,#72723,#72724,#72725,#72726,#72727,#72728,#72729,
#72730,#72731,#72732,#72733,#72734,#72735,#72736,#72737,#72738,#72739,#72740,
#72741,#72742,#72743,#72744,#72745,#72746,#72747,#72748,#72749,#72750,#72751,
#72752,#72753,#72754,#72755,#72756,#72757,#72758,#72759,#72760,#72761,#72762,
#72763,#72764,#72765,#72766,#72767,#72768,#72769,#72770,#72771,#72772,#72773),
 .UNSPECIFIED.,.F.,.F.,(4,2,2,2,2,2,2,2,2,2,2,2,2,2,2,2,2,2,2,2,2,2,2,2,
2,2,2,2,2,2,2,2,2,2,2,2,2,2,2,2,2,2,2,2,2,2,2,2,2,2,2,2,2,2,2,2,2,2,2,2,
2,2,2,2,2,2,2,2,2,2,2,2,2,2,2,2,2,2,2,2,2,2,2,2,2,2,2,2,2,2,2,2,2,2,2,2,
2,2,2,2,2,2,2,2,2,2,4),(-1.82646872808304,-1.79734343065746,-1.79282236795917,
-1.7904500083226,-1.78847942728732,-1.78599002003742,-1.78201728957643,
-1.75740049756953,-1.72082841589016,-1.68574819720403,-1.67732653125684,
-1.67300951028283,-1.66950177302835,-1.66545157743265,-1.65850096993108,
-1.62665625488312,-1.57722097813993,-1.55895366761575,-1.55502285629584,
-1.55277644485429,-1.55078807283716,-1.54815756432633,-1.54214968319553,
-1.49535134001273,-1.45027218291409,-1.44062165500393,-1.4361156264914,
-1.43258176884484,-1.42869602973701,-1.42231921516799,-1.39762001860241,
-1.36847462436808,-1.32516309212689,-1.31896620803045,-1.31654077706124,
-1.31454058610643,-1.312387495636,-1.30888058536324,-1.29630354879562,-1.27208731332166,
-1.21120538561776,-1.20346749532008,-1.19887023285559,-1.19532358250096,
-1.19148257080471,-1.18531097264309,-1.16313173827444,-1.12402804327183,
-1.08802186722329,-1.08178777524824,-1.07928191376428,-1.07726132907201,
-1.07514334239209,-1.07179534149392,-1.06080427782233,-1.04119906276471,
-1.02901769956693,-0.974997981890985,-0.965670356047288,-0.961176469496914,
-0.95765342988398,-0.9537209616307,-0.94712815723658,-0.919316518239307,
-0.88703245040185,-0.850673363228459,-0.844431342045032,-0.841924176859279,
-0.839903291338221,-0.837785920917063,-0.834440514550907,-0.823472911130825,
-0.803930938430001,-0.791229216561297,-0.737695413856313,-0.728334089761734,
-0.723833895929693,-0.720310249841019,-0.716381585360781,-0.709805932497879,
-0.6822595032286,-0.649792237898696,-0.61331073220674,-0.607076629892004,
-0.604570860569829,-0.602550388610375,-0.600432567798541,-0.597084912150998,
-0.586095749011207,-0.566495024707679,-0.55428458656948,-0.500296910439677,
-0.490967807783343,-0.486473817723689,-0.482950963349569,-0.47901897748105,
-0.472427645952877,-0.444634221868152,-0.412340686353847,-0.375976390572374,
-0.369735288842809,-0.367228374182216,-0.36520764329194,-0.363090376161521,
-0.359745030876317,-0.348776687020761,-0.332074222475645),.UNSPECIFIED.);
#996=B_SPLINE_CURVE_WITH_KNOTS('',3,(#72779,#72780,#72781,#72782,#72783,
#72784,#72785,#72786,#72787),.UNSPECIFIED.,.F.,.F.,(4,1,1,1,1,1,4),(109.955742875643,
110.105187134774,111.103203895386,112.101220655997,113.099237416609,114.09725417722,
114.844983025569),.UNSPECIFIED.);
#997=B_SPLINE_CURVE_WITH_KNOTS('',3,(#72788,#72789,#72790,#72791,#72792,
#72793,#72794,#72795,#72796,#72797,#72798,#72799,#72800,#72801,#72802,#72803,
#72804,#72805,#72806,#72807,#72808,#72809,#72810,#72811,#72812,#72813,#72814,
#72815,#72816,#72817,#72818,#72819,#72820,#72821,#72822,#72823,#72824,#72825,
#72826,#72827,#72828,#72829,#72830,#72831,#72832,#72833,#72834,#72835,#72836,
#72837),.UNSPECIFIED.,.F.,.F.,(4,2,2,2,2,2,2,2,2,2,2,2,2,2,2,2,2,2,2,2,
2,2,2,2,4),(-2.98948394067237,-2.93033327020979,-2.920244048379,-2.91226142318022,
-2.90803374835732,-2.9045631617174,-2.9004520241019,-2.89322997407042,-2.84953099677671,
-2.81256119808136,-2.80026151844069,-2.79237614375237,-2.78948716317769,
-2.78764833673942,-2.78562791237046,-2.78312274318819,-2.7768927054734,
-2.74083011361301,-2.70912061365899,-2.6805950398033,-2.67395791026974,
-2.67001567319296,-2.66649418458564,-2.6620163632797,-2.65808389942519),
 .UNSPECIFIED.);
#998=B_SPLINE_CURVE_WITH_KNOTS('',3,(#72839,#72840,#72841,#72842,#72843,
#72844,#72845,#72846,#72847,#72848,#72849,#72850,#72851,#72852,#72853,#72854,
#72855,#72856,#72857,#72858,#72859,#72860,#72861,#72862,#72863,#72864,#72865,
#72866,#72867,#72868,#72869,#72870,#72871,#72872,#72873,#72874,#72875,#72876,
#72877,#72878,#72879,#72880,#72881,#72882,#72883,#72884,#72885,#72886,#72887,
#72888,#72889,#72890,#72891,#72892),.UNSPECIFIED.,.F.,.F.,(4,2,2,2,2,2,
2,2,2,2,2,2,2,2,2,2,2,2,2,2,2,2,2,2,2,2,4),(-0.332074222475645,-0.32923204910345,
-0.318830590678436,-0.262639008314075,-0.253697656003321,-0.249176719081695,
-0.245807769776908,-0.242024917996104,-0.238071186744742,-0.232264168229582,
-0.190630465007277,-0.146639547020774,-0.134181037306488,-0.130549452041593,
-0.128369040640389,-0.126359289402557,-0.123541320311572,-0.116588668380137,
-0.106358990090594,-0.0724794716636102,-0.0352996703932748,-0.0192230682661245,
-0.0136314931449329,-0.00986943951079496,-0.00651983590288715,-0.00346048099933967,
-0.000736392770504616),.UNSPECIFIED.);
#999=B_SPLINE_CURVE_WITH_KNOTS('',3,(#72893,#72894,#72895,#72896,#72897,
#72898,#72899,#72900,#72901),.UNSPECIFIED.,.F.,.F.,(4,1,1,1,1,1,4),(109.955745615411,
110.418692148357,111.416708908968,112.41472566958,113.412742430191,114.410759190803,
114.846231128118),.UNSPECIFIED.);
#1000=B_SPLINE_CURVE_WITH_KNOTS('',3,(#72907,#72908,#72909,#72910,#72911,
#72912,#72913,#72914,#72915,#72916,#72917,#72918,#72919,#72920,#72921,#72922,
#72923,#72924,#72925,#72926,#72927,#72928,#72929,#72930,#72931,#72932,#72933,
#72934,#72935,#72936,#72937,#72938,#72939,#72940,#72941,#72942,#72943,#72944,
#72945,#72946,#72947,#72948,#72949,#72950,#72951,#72952,#72953,#72954,#72955,
#72956,#72957,#72958,#72959,#72960,#72961,#72962,#72963,#72964,#72965,#72966,
#72967,#72968,#72969,#72970,#72971,#72972,#72973,#72974,#72975,#72976,#72977,
#72978,#72979,#72980,#72981,#72982,#72983,#72984,#72985,#72986,#72987,#72988,
#72989,#72990,#72991,#72992,#72993,#72994,#72995,#72996,#72997,#72998,#72999,
#73000,#73001,#73002,#73003,#73004,#73005,#73006,#73007,#73008,#73009,#73010,
#73011,#73012,#73013,#73014,#73015,#73016,#73017,#73018,#73019,#73020,#73021,
#73022,#73023,#73024,#73025,#73026,#73027,#73028,#73029,#73030,#73031,#73032,
#73033,#73034,#73035,#73036,#73037,#73038,#73039,#73040,#73041,#73042,#73043,
#73044,#73045,#73046,#73047,#73048,#73049,#73050,#73051,#73052,#73053,#73054,
#73055,#73056,#73057,#73058,#73059,#73060,#73061,#73062,#73063,#73064,#73065,
#73066),.UNSPECIFIED.,.F.,.F.,(4,2,2,2,2,2,2,2,2,2,2,2,2,2,2,2,2,2,2,2,
2,2,2,2,2,2,2,2,2,2,2,2,2,2,2,2,2,2,2,2,2,2,2,2,2,2,2,2,2,2,2,2,2,2,2,2,
2,2,2,2,2,2,2,2,2,2,2,2,2,2,2,2,2,2,2,2,2,2,2,4),(-1.16399522342669,-1.1607907650581,
-1.15676753883012,-1.15426290904758,-1.15229142577373,-1.14993129837991,
-1.14546917568034,-1.11123091791317,-1.05385890063992,-1.04263838798745,
-1.03816444188207,-1.03486673191996,-1.03127542050177,-1.02632369629155,
-1.01437727086931,-0.997276965565523,-0.930525489122616,-0.92115957748363,
-0.917892990164741,-0.916001193627688,-0.913980141959651,-0.911101445563391,
-0.903766126285405,-0.892768033335116,-0.82025015374059,-0.806202941365025,
-0.800779737705798,-0.797465144405553,-0.793885294240733,-0.789003323779566,
-0.777489870506518,-0.735403155294618,-0.688311462055666,-0.682317213195112,
-0.679688716305464,-0.677700279848191,-0.675451921571445,-0.671513237591417,
-0.653115374970274,-0.602768451457007,-0.571962960154127,-0.565063896818231,
-0.561024964452434,-0.557515663186227,-0.553182178311967,-0.54468038352206,
-0.514227530682404,-0.473045419646851,-0.448495708181078,-0.444525426127836,
-0.442036568138941,-0.4400657108176,-0.437692089561676,-0.433166056534365,
-0.391822425520439,-0.338592459043075,-0.329212056146974,-0.324707748331981,
-0.32118305990655,-0.317255462249331,-0.310686891688175,-0.283260623549618,
-0.25071953658601,-0.214191025847954,-0.20795896562446,-0.205453268244515,
-0.203432551722216,-0.201356549782399,-0.198286203347804,-0.18890777918587,
-0.173270510740528,-0.138720380485088,-0.097876263984719,-0.0906666070068624,
-0.0865578429595567,-0.083086582079581,-0.0788547987316751,-0.0708542543693418,
-0.0607355454979825,-0.000706686318606294),.UNSPECIFIED.);
#1001=B_SPLINE_CURVE_WITH_KNOTS('',3,(#73067,#73068,#73069,#73070,#73071,
#73072),.UNSPECIFIED.,.F.,.F.,(4,1,1,4),(114.844983025569,115.095270937832,
116.093287698443,116.238928182822),.UNSPECIFIED.);
#1002=B_SPLINE_CURVE_WITH_KNOTS('',3,(#73074,#73075,#73076,#73077,#73078),
 .UNSPECIFIED.,.F.,.F.,(4,1,4),(114.846231128118,115.408775951414,116.238922116759),
 .UNSPECIFIED.);
#1003=B_SPLINE_CURVE_WITH_KNOTS('',3,(#73079,#73080,#73081,#73082,#73083,
#73084,#73085,#73086,#73087,#73088,#73089,#73090,#73091,#73092,#73093,#73094,
#73095,#73096,#73097,#73098,#73099,#73100,#73101,#73102,#73103,#73104,#73105,
#73106,#73107,#73108,#73109,#73110,#73111,#73112,#73113,#73114,#73115,#73116,
#73117,#73118,#73119,#73120,#73121,#73122,#73123,#73124,#73125,#73126,#73127,
#73128,#73129,#73130,#73131,#73132,#73133,#73134,#73135,#73136,#73137,#73138,
#73139,#73140,#73141,#73142,#73143,#73144,#73145,#73146,#73147,#73148,#73149,
#73150,#73151,#73152,#73153,#73154,#73155,#73156,#73157,#73158,#73159,#73160,
#73161,#73162,#73163,#73164,#73165,#73166),.UNSPECIFIED.,.F.,.F.,(4,3,3,
3,3,3,3,3,3,3,3,3,3,3,3,3,3,3,3,3,3,3,3,3,3,3,3,3,3,4),(116.238928182822,
116.406792712026,116.585455131904,116.763755652497,116.942027621902,117.120269763611,
117.298929207096,117.404809472637,117.583471744362,117.761772116778,117.940043940156,
118.118285936843,118.296945239705,118.402826233249,118.581488643105,118.759789151972,
118.938061107338,119.116303233685,119.294962660085,119.40084299386,119.579505658284,
119.757806425289,119.936078640185,120.114321027218,120.292980710927,120.398859754472,
120.581274217561,120.759594008658,120.944055807743,121.128517606828),
 .UNSPECIFIED.);
#1004=B_SPLINE_CURVE_WITH_KNOTS('',3,(#73171,#73172,#73173,#73174,#73175,
#73176,#73177,#73178,#73179,#73180,#73181,#73182,#73183,#73184,#73185,#73186,
#73187,#73188,#73189,#73190,#73191,#73192,#73193,#73194,#73195,#73196,#73197,
#73198,#73199,#73200,#73201,#73202,#73203,#73204,#73205,#73206,#73207,#73208,
#73209,#73210,#73211,#73212,#73213,#73214,#73215,#73216,#73217,#73218,#73219,
#73220,#73221,#73222,#73223,#73224,#73225,#73226,#73227,#73228,#73229,#73230,
#73231,#73232,#73233,#73234,#73235,#73236,#73237,#73238,#73239,#73240,#73241,
#73242,#73243,#73244,#73245,#73246,#73247,#73248,#73249,#73250,#73251,#73252,
#73253,#73254,#73255,#73256,#73257,#73258,#73259,#73260,#73261,#73262,#73263,
#73264,#73265,#73266,#73267,#73268,#73269,#73270,#73271,#73272,#73273,#73274,
#73275,#73276,#73277,#73278,#73279,#73280,#73281,#73282,#73283,#73284,#73285,
#73286,#73287,#73288,#73289,#73290,#73291,#73292,#73293,#73294,#73295,#73296,
#73297,#73298,#73299,#73300,#73301,#73302,#73303,#73304,#73305,#73306,#73307,
#73308,#73309,#73310,#73311,#73312,#73313,#73314,#73315,#73316,#73317,#73318,
#73319,#73320,#73321,#73322,#73323,#73324,#73325,#73326,#73327,#73328,#73329,
#73330,#73331,#73332,#73333,#73334,#73335,#73336,#73337,#73338,#73339,#73340,
#73341,#73342,#73343,#73344,#73345,#73346,#73347,#73348,#73349,#73350,#73351,
#73352,#73353,#73354,#73355,#73356,#73357,#73358,#73359,#73360,#73361,#73362,
#73363,#73364,#73365,#73366,#73367,#73368,#73369,#73370,#73371,#73372,#73373,
#73374,#73375,#73376,#73377,#73378),.UNSPECIFIED.,.F.,.F.,(4,2,2,2,2,2,
2,2,2,2,2,2,2,2,2,2,2,2,2,2,2,2,2,2,2,2,2,2,2,2,2,2,2,2,2,2,2,2,2,2,2,2,
2,2,2,2,2,2,2,2,2,2,2,2,2,2,2,2,2,2,2,2,2,2,2,2,2,2,2,2,2,2,2,2,2,2,2,2,
2,2,2,2,2,2,2,2,2,2,2,2,2,2,2,2,2,2,2,2,2,2,2,2,2,4),(-2.65819190440258,
-2.62705712494929,-2.59765357301862,-2.58818230394141,-2.58161464612472,
-2.57885718035791,-2.57685785746737,-2.57466372827504,-2.5709336624315,
-2.55727162657967,-2.54405129398292,-2.47891151641061,-2.46682567394425,
-2.46187307468181,-2.45830137698401,-2.45503587890549,-2.44978666843108,
-2.43675119578249,-2.38090755497794,-2.34715072372975,-2.34271887739022,
-2.34037695799276,-2.33841168866653,-2.33591020129654,-2.33189890701069,
-2.30470322282034,-2.26384368335237,-2.2327840173422,-2.22599043099554,
-2.22200752389696,-2.21848128088368,-2.21403969471864,-2.20531968773966,
-2.14666080293568,-2.12140817522014,-2.10850181955546,-2.10495478144744,
-2.10278655601613,-2.10078436366636,-2.09836423134815,-2.0922148311029,
-2.04793545909769,-2.01339516524246,-2.00059679224079,-1.99099412388749,
-1.9864466300786,-1.98291529562836,-1.97900793568737,-1.97253857652236,
-1.94990948815999,-1.90286790921321,-1.87265483895183,-1.86826625704765,
-1.86592166981243,-1.86395007102146,-1.86142839572219,-1.85734437447908,
-1.82219968803482,-1.7789745800374,-1.764531840932,-1.75400383553291,-1.74929267610803,
-1.74574325456806,-1.74192173749601,-1.73583077706982,-1.71653868529926,
-1.66672544670334,-1.63530910422094,-1.63089788175895,-1.62854973302512,
-1.62657798490348,-1.6240605864961,-1.61999570653607,-1.58957505440082,
-1.58367800376849,-1.58132498720718,-1.55052706117888,-1.52092595187713,
-1.51422201415437,-1.51026361139447,-1.50674208454562,-1.50228372944685,
-1.49519565036645,-1.485286693889,-1.46243578350789,-1.4346822666082,-1.42708549562084,
-1.39817940851973,-1.39413512429057,-1.39162316200219,-1.38965010783394,
-1.38729312070076,-1.38284848244978,-1.3497909124847,-1.29568288511291,
-1.28120802408501,-1.27572128797448,-1.27239497228259,-1.26882314854165,
-1.2639889239166,-1.25276219547068,-1.2205778578495,-1.18863953479716,-1.16399522342669),
 .UNSPECIFIED.);
#1005=B_SPLINE_CURVE_WITH_KNOTS('',3,(#73380,#73381,#73382,#73383,#73384,
#73385,#73386,#73387,#73388,#73389,#73390,#73391,#73392,#73393,#73394,#73395,
#73396,#73397,#73398,#73399,#73400,#73401,#73402,#73403,#73404,#73405,#73406,
#73407),.UNSPECIFIED.,.F.,.F.,(4,3,3,3,3,3,3,3,3,4),(121.128517606828,121.307176749353,
121.396876515083,121.575539354439,121.753840284705,121.932112643433,122.110355163549,
122.289014961266,122.394893275695,122.522113490002),.UNSPECIFIED.);
#1006=B_SPLINE_CURVE_WITH_KNOTS('',3,(#73408,#73409,#73410,#73411,#73412,
#73413,#73414,#73415,#73416,#73417,#73418,#73419,#73420,#73421,#73422,#73423,
#73424,#73425,#73426,#73427,#73428,#73429,#73430,#73431,#73432,#73433,#73434,
#73435,#73436,#73437,#73438,#73439,#73440,#73441,#73442,#73443,#73444,#73445,
#73446,#73447,#73448,#73449,#73450,#73451,#73452,#73453,#73454,#73455,#73456,
#73457,#73458,#73459,#73460,#73461,#73462,#73463,#73464,#73465,#73466,#73467,
#73468,#73469,#73470,#73471,#73472,#73473,#73474,#73475,#73476,#73477,#73478,
#73479,#73480,#73481,#73482,#73483,#73484,#73485,#73486,#73487,#73488,#73489,
#73490,#73491,#73492,#73493,#73494,#73495,#73496,#73497,#73498,#73499,#73500,
#73501,#73502,#73503,#73504,#73505,#73506,#73507,#73508,#73509,#73510,#73511,
#73512,#73513,#73514,#73515,#73516,#73517,#73518,#73519,#73520,#73521,#73522,
#73523,#73524,#73525,#73526,#73527,#73528,#73529,#73530,#73531,#73532,#73533,
#73534,#73535,#73536,#73537,#73538,#73539,#73540,#73541,#73542,#73543,#73544,
#73545,#73546,#73547,#73548,#73549,#73550,#73551,#73552,#73553,#73554,#73555,
#73556,#73557,#73558,#73559,#73560,#73561,#73562,#73563,#73564,#73565,#73566,
#73567,#73568,#73569,#73570,#73571,#73572,#73573,#73574,#73575,#73576,#73577,
#73578,#73579),.UNSPECIFIED.,.F.,.F.,(4,2,2,2,2,2,2,2,2,2,2,2,2,2,2,2,2,
2,2,2,2,2,2,2,2,2,2,2,2,2,2,2,2,2,2,2,2,2,2,2,2,2,2,2,2,2,2,2,2,2,2,2,2,
2,2,2,2,2,2,2,2,2,2,2,2,2,2,2,2,2,2,2,2,2,2,2,2,2,2,2,2,2,2,2,2,4),(1.16375694728592,
1.16380572379371,1.16756314774595,1.16977105475773,1.17176855571367,1.17451819235809,
1.18106226091327,1.19049733908575,1.21977817780083,1.27257455330762,1.28198220795045,
1.28648837836552,1.29000951314699,1.29392790987802,1.30046832523159,1.32754326642328,
1.36036792674952,1.39703180321458,1.40325307475061,1.40575526496874,1.40777345122844,
1.40989154291943,1.41324007375119,1.42423574989435,1.44385599928274,1.45602068439686,
1.51009100934789,1.51942029204224,1.52391532427349,1.52743943895535,1.53137332141279,
1.53796913868854,1.56581731978394,1.59800829457104,1.63428741328967,1.64052917013522,
1.64303692870204,1.64505862845649,1.64717646704278,1.65052381119274,1.66150847642566,
1.68109953840757,1.69354314423061,1.74731784145461,1.75666325606489,1.7611601238046,
1.76468304513515,1.76861284203001,1.77519506653898,1.80285485901953,1.83521594225092,
1.87162355399383,1.87785781582318,1.88036323445556,1.88238327569664,1.88450030533758,
1.88784628997681,1.89882542779452,1.91840370721812,1.93098657621613,1.98463441923818,
1.99398879792609,1.99848679136185,2.00200918517096,2.00593692917007,2.01251217539737,
2.04007898461954,2.07249460519876,2.10894638508053,2.11517037862647,2.11767394279111,
2.11969338955896,2.12176873444242,2.12485030980061,2.12860467378489,2.13582880444578,
2.15473808286976,2.16252615307732,2.22309145171865,2.23161895358931,2.23601272974263,
2.23952516454979,2.24351815164137,2.25039323963597,2.28336705928181,2.32678697888738),
 .UNSPECIFIED.);
#1007=B_SPLINE_CURVE_WITH_KNOTS('',3,(#73583,#73584,#73585,#73586,#73587,
#73588,#73589,#73590,#73591,#73592,#73593,#73594,#73595,#73596,#73597,#73598,
#73599,#73600,#73601,#73602,#73603,#73604,#73605,#73606,#73607,#73608,#73609,
#73610,#73611,#73612,#73613,#73614,#73615,#73616,#73617,#73618,#73619,#73620,
#73621,#73622),.UNSPECIFIED.,.F.,.F.,(4,3,3,3,3,3,3,3,3,3,3,3,3,4),(-4.09293042013065,
-3.992067042446,-3.82244776231553,-3.65315968078964,-3.48390880876262,-3.31470709998066,
-3.14511254726307,-2.9940502818345,-2.82636267585639,-2.65899488979554,
-2.49165994935383,-2.32435113337687,-2.15669226772051,-2.06882272292704),
 .UNSPECIFIED.);
#1008=B_SPLINE_CURVE_WITH_KNOTS('',3,(#73626,#73627,#73628,#73629,#73630,
#73631,#73632,#73633,#73634,#73635,#73636,#73637,#73638,#73639,#73640,#73641,
#73642,#73643,#73644,#73645,#73646,#73647),.UNSPECIFIED.,.F.,.F.,(4,3,3,
3,3,3,3,4),(4.61444669507962E-15,0.17333570362943,0.346547214765417,0.519954753279274,
0.693441640210306,0.867424673888169,0.998016760611494,1.11730040836813),
 .UNSPECIFIED.);
#1009=B_SPLINE_CURVE_WITH_KNOTS('',3,(#73649,#73650,#73651,#73652,#73653,
#73654,#73655,#73656,#73657,#73658,#73659,#73660,#73661,#73662,#73663,#73664,
#73665,#73666,#73667,#73668,#73669,#73670,#73671,#73672,#73673,#73674,#73675,
#73676,#73677,#73678,#73679,#73680,#73681,#73682,#73683,#73684,#73685,#73686,
#73687,#73688,#73689,#73690,#73691,#73692,#73693,#73694,#73695,#73696,#73697,
#73698,#73699,#73700,#73701,#73702,#73703,#73704,#73705,#73706,#73707,#73708,
#73709,#73710,#73711,#73712,#73713,#73714,#73715,#73716,#73717,#73718,#73719,
#73720,#73721,#73722,#73723,#73724,#73725,#73726,#73727,#73728,#73729,#73730,
#73731,#73732,#73733,#73734,#73735,#73736,#73737,#73738,#73739,#73740,#73741,
#73742,#73743,#73744,#73745,#73746,#73747,#73748,#73749,#73750,#73751,#73752,
#73753,#73754,#73755,#73756,#73757,#73758,#73759,#73760,#73761,#73762,#73763,
#73764,#73765,#73766),.UNSPECIFIED.,.F.,.F.,(4,3,3,3,3,3,3,3,3,3,3,3,3,
3,3,3,3,3,3,3,3,3,3,3,3,3,3,3,3,3,3,3,3,3,3,3,3,3,3,4),(1.11730040857138,
1.28258742205918,1.4475801664024,1.61257569629296,1.77757610156023,1.94293553368316,
1.996033521223,2.16557749727504,2.33479223618305,2.50397357895414,2.67310773704729,
2.84263918138715,2.9940502818345,3.16364173365622,3.33291309222664,3.50216444093724,
3.67137606968638,3.84099599146778,3.992067042446,4.16113100258707,4.32986127689689,
4.49855861854032,4.66720816578798,4.83626436321027,4.9900838030575,5.15942585196637,
5.32843906253154,5.49742264590328,5.66636077829777,5.83570339435669,5.988100563669,
6.15742914576441,6.32642978538965,6.49540238342449,6.66433038075115,6.83366451994832,
6.9861173242805,7.17227412937206,7.35714291321279,7.40048531495325),
 .UNSPECIFIED.);
#1010=B_SPLINE_CURVE_WITH_KNOTS('',3,(#73768,#73769,#73770,#73771,#73772,
#73773,#73774,#73775,#73776,#73777),.UNSPECIFIED.,.F.,.F.,(4,1,1,1,1,1,
1,4),(7.40048571554771,7.984134084892,8.98215084550351,9.98016760611501,
10.9781843667265,11.976201127338,12.9742178879495,13.6836710227273),
 .UNSPECIFIED.);
#1011=B_SPLINE_CURVE_WITH_KNOTS('',3,(#73779,#73780,#73781,#73782,#73783,
#73784,#73785,#73786,#73787,#73788,#73789,#73790,#73791,#73792,#73793,#73794,
#73795,#73796,#73797,#73798,#73799,#73800,#73801,#73802,#73803,#73804,#73805,
#73806,#73807,#73808,#73809,#73810,#73811,#73812,#73813,#73814,#73815,#73816,
#73817,#73818,#73819,#73820,#73821,#73822,#73823,#73824,#73825,#73826,#73827,
#73828,#73829,#73830,#73831,#73832,#73833,#73834,#73835,#73836,#73837,#73838,
#73839,#73840,#73841,#73842,#73843,#73844,#73845,#73846,#73847,#73848,#73849,
#73850,#73851,#73852,#73853,#73854,#73855,#73856,#73857,#73858,#73859,#73860,
#73861,#73862,#73863,#73864,#73865,#73866,#73867,#73868,#73869,#73870,#73871,
#73872,#73873,#73874,#73875,#73876,#73877,#73878,#73879,#73880,#73881,#73882,
#73883,#73884,#73885,#73886,#73887,#73888,#73889,#73890,#73891,#73892,#73893,
#73894,#73895,#73896),.UNSPECIFIED.,.F.,.F.,(4,3,3,3,3,3,3,3,3,3,3,3,3,
3,3,3,3,3,3,3,3,3,3,3,3,3,3,3,3,3,3,3,3,3,3,3,3,3,3,4),(13.6836711800844,
13.8911898125104,13.972234648561,14.1415281762225,14.3104926228966,14.4794278048088,
14.6483176482061,14.8176131987297,14.9702514091725,15.1395446921665,15.3085088919621,
15.4774438272913,15.6463334238238,15.8156287322797,15.968268169784,16.137561335811,
16.3065254144919,16.4754602240832,16.6443496921161,16.8136448701357,16.9662849303955,
17.1355782298889,17.3045424449965,17.4734773935573,17.6423670022045,17.8116623206224,
17.964301691007,18.1335949468184,18.302559117701,18.4714940218612,18.6403835859313,
18.8096788604258,18.9623184516185,19.1316116956298,19.3005758542088,19.4695107454679,
19.6384002962861,19.807695557217,19.96033521223,19.9668563299069),
 .UNSPECIFIED.);
#1012=B_SPLINE_CURVE_WITH_KNOTS('',3,(#73898,#73899,#73900,#73901,#73902,
#73903,#73904,#73905,#73906,#73907,#73908,#73909,#73910,#73911,#73912,#73913,
#73914,#73915,#73916,#73917,#73918,#73919,#73920,#73921,#73922,#73923,#73924,
#73925,#73926,#73927,#73928,#73929,#73930,#73931,#73932,#73933,#73934,#73935,
#73936,#73937,#73938,#73939,#73940,#73941,#73942,#73943,#73944,#73945,#73946,
#73947,#73948,#73949,#73950,#73951,#73952,#73953,#73954,#73955,#73956,#73957,
#73958,#73959,#73960,#73961,#73962,#73963,#73964,#73965,#73966,#73967,#73968,
#73969,#73970,#73971,#73972,#73973,#73974,#73975,#73976,#73977,#73978,#73979,
#73980,#73981,#73982,#73983,#73984,#73985,#73986,#73987,#73988,#73989,#73990,
#73991,#73992,#73993,#73994,#73995,#73996,#73997,#73998,#73999,#74000,#74001,
#74002,#74003,#74004,#74005,#74006,#74007,#74008,#74009,#74010,#74011,#74012),
 .UNSPECIFIED.,.F.,.F.,(4,3,3,3,3,3,3,3,3,3,3,3,3,3,3,3,3,3,3,3,3,3,3,3,
3,3,3,3,3,3,3,3,3,3,3,3,3,3,4),(19.9668563300962,20.135952811592,20.3047208147562,
20.4734598895618,20.6421556318704,20.8112536713725,20.9583519728415,21.1276452281632,
21.2966093983786,21.4655443016053,21.6344338645944,21.8037291377806,21.956368733453,
22.1256619878341,22.2946261570513,22.4635610592055,22.6324506210793,22.8017458931016,
22.9543854940645,23.1236787509982,23.2926429228304,23.4615778276573,23.6304673922401,
23.7997626669753,23.952402254676,24.1216955104188,24.2906596810405,24.4595945846445,
24.6284841479956,24.7977794215101,24.9504190152875,25.1197122710063,25.2886764415981,
25.4576113451634,25.6265009084708,25.7957961819343,25.948435775899,26.1527578523688,
26.2500414524452),.UNSPECIFIED.);
#1013=B_SPLINE_CURVE_WITH_KNOTS('',3,(#74014,#74015,#74016,#74017,#74018,
#74019,#74020,#74021,#74022,#74023),.UNSPECIFIED.,.F.,.F.,(4,1,1,1,1,1,
1,4),(26.2500416370865,26.9464525365105,27.944469297122,28.9424860577335,
29.940502818345,30.9385195789565,31.936536339568,32.5332269442661),
 .UNSPECIFIED.);
#1014=B_SPLINE_CURVE_WITH_KNOTS('',3,(#74025,#74026,#74027,#74028,#74029,
#74030,#74031,#74032,#74033,#74034,#74035,#74036,#74037,#74038,#74039,#74040,
#74041,#74042,#74043,#74044,#74045,#74046,#74047,#74048,#74049,#74050,#74051,
#74052,#74053,#74054,#74055,#74056,#74057,#74058,#74059,#74060,#74061,#74062,
#74063,#74064,#74065,#74066,#74067,#74068,#74069,#74070,#74071,#74072,#74073,
#74074,#74075,#74076,#74077,#74078,#74079,#74080,#74081,#74082,#74083,#74084,
#74085,#74086,#74087,#74088,#74089,#74090,#74091,#74092,#74093,#74094,#74095,
#74096,#74097,#74098,#74099,#74100,#74101,#74102,#74103,#74104,#74105,#74106,
#74107,#74108,#74109,#74110,#74111,#74112,#74113,#74114,#74115,#74116,#74117,
#74118,#74119,#74120,#74121,#74122,#74123,#74124,#74125,#74126,#74127,#74128,
#74129,#74130,#74131,#74132,#74133,#74134,#74135,#74136,#74137,#74138,#74139,
#74140,#74141,#74142),.UNSPECIFIED.,.F.,.F.,(4,3,3,3,3,3,3,3,3,3,3,3,3,
3,3,3,3,3,3,3,3,3,3,3,3,3,3,3,3,3,3,3,3,3,3,3,3,3,3,4),(32.5332271627877,
32.7196079893562,32.9074239211681,32.9345531001795,33.1038463560855,33.2728105268702,
33.4417454306341,33.6106349941438,33.7799302678113,33.932569860791,34.1018631166979,
34.2708272874833,34.4397621912481,34.6086517547587,34.7779470284269,34.9305866214025,
35.09987987731,35.2688440480961,35.4377789518616,35.6066685153728,35.7759637890418,
35.928603382014,36.0978966379209,36.2668608087064,36.4357957124713,36.6046852759818,
36.7739805496502,36.9266201426255,37.0959133985326,37.2648775693182,37.4338124730832,
37.602702036594,37.7719973102625,37.924636903237,38.0917435228824,38.258524840331,
38.4252546296913,38.5919573763902,38.758969368588,38.8164122512189),
 .UNSPECIFIED.);
#1015=B_SPLINE_CURVE_WITH_KNOTS('',3,(#74144,#74145,#74146,#74147,#74148,
#74149,#74150,#74151,#74152,#74153,#74154,#74155,#74156,#74157,#74158,#74159,
#74160,#74161,#74162,#74163,#74164,#74165,#74166,#74167,#74168,#74169,#74170,
#74171,#74172,#74173,#74174,#74175,#74176,#74177,#74178,#74179,#74180,#74181,
#74182,#74183,#74184,#74185,#74186,#74187,#74188,#74189,#74190,#74191,#74192,
#74193,#74194,#74195,#74196,#74197,#74198,#74199,#74200,#74201,#74202,#74203,
#74204,#74205,#74206,#74207,#74208,#74209,#74210,#74211,#74212,#74213,#74214,
#74215,#74216,#74217,#74218,#74219,#74220,#74221,#74222,#74223,#74224,#74225,
#74226,#74227,#74228,#74229,#74230,#74231,#74232,#74233,#74234,#74235,#74236,
#74237,#74238,#74239,#74240,#74241,#74242,#74243,#74244,#74245,#74246,#74247,
#74248,#74249,#74250,#74251,#74252,#74253,#74254,#74255,#74256,#74257,#74258),
 .UNSPECIFIED.,.F.,.F.,(4,3,3,3,3,3,3,3,3,3,3,3,3,3,3,3,3,3,3,3,3,3,3,3,
3,3,3,3,3,3,3,3,3,3,3,3,3,3,4),(38.8164122514457,38.9226536638485,39.0919469197561,
39.2609110905423,39.4298459943078,39.5987355578191,39.7680308314881,39.92067042446,
40.089963680367,40.2589278511526,40.4278627549176,40.5967523184283,40.7660475920968,
40.9186871850715,41.0879804409785,41.2569446117641,41.4258795155291,41.5947690790398,
41.7640643527083,41.916703945683,42.0859972015901,42.2549613723759,42.4238962761409,
42.5927858396518,42.7620811133203,42.9147207062945,43.0840139622016,43.2529781329872,
43.4219130367523,43.590802600263,43.7600978739315,43.912737466906,44.0820307228131,
44.2509948935988,44.4199297973638,44.5888193608746,44.7581146345431,44.9107542275175,
45.0995975586252),.UNSPECIFIED.);
#1016=B_SPLINE_CURVE_WITH_KNOTS('',3,(#74260,#74261,#74262,#74263,#74264,
#74265,#74266,#74267,#74268,#74269),.UNSPECIFIED.,.F.,.F.,(4,1,1,1,1,1,
1,4),(45.0996018360204,45.908770988129,46.9067877487405,47.904804509352,
48.9028212699635,49.900838030575,50.8988547911865,51.3827816994375),
 .UNSPECIFIED.);
#1017=B_SPLINE_CURVE_WITH_KNOTS('',3,(#74271,#74272,#74273,#74274,#74275,
#74276,#74277,#74278,#74279,#74280,#74281,#74282,#74283,#74284,#74285,#74286,
#74287,#74288,#74289,#74290,#74291,#74292,#74293,#74294,#74295,#74296,#74297,
#74298,#74299,#74300,#74301,#74302,#74303,#74304,#74305,#74306,#74307,#74308,
#74309,#74310,#74311,#74312,#74313,#74314,#74315,#74316,#74317,#74318,#74319,
#74320,#74321,#74322,#74323,#74324,#74325,#74326,#74327,#74328,#74329,#74330,
#74331,#74332,#74333,#74334,#74335,#74336,#74337,#74338,#74339,#74340,#74341,
#74342,#74343,#74344,#74345,#74346,#74347,#74348,#74349,#74350,#74351,#74352,
#74353,#74354,#74355,#74356,#74357,#74358,#74359,#74360,#74361,#74362,#74363,
#74364,#74365,#74366,#74367,#74368,#74369,#74370,#74371,#74372,#74373,#74374,
#74375,#74376,#74377,#74378,#74379,#74380,#74381,#74382,#74383,#74384,#74385),
 .UNSPECIFIED.,.F.,.F.,(4,3,3,3,3,3,3,3,3,3,3,3,3,3,3,3,3,3,3,3,3,3,3,3,
3,3,3,3,3,3,3,3,3,3,3,3,3,3,4),(51.3827828658048,51.558714250667,51.7353860088453,
51.896871551798,52.0661648077051,52.2351289784908,52.4040638822558,52.5729534457665,
52.742248719435,52.8948883124095,53.0641815683166,53.2331457391023,53.4020806428674,
53.5709702063782,53.7402654800468,53.8929050730211,54.0621983289282,54.2311624997139,
54.4000974034789,54.5689869669897,54.7382822406583,54.8909218336326,55.0602150895396,
55.2291792603252,55.3981141640902,55.567003727601,55.7362990012695,55.8889385942441,
56.0582318501512,56.2271960209369,56.3961309247019,56.5650204882127,56.7343157618812,
56.8869553548556,57.0539545270545,57.2206780393154,57.3872309280649,57.5539523877524,
57.6659681729844),.UNSPECIFIED.);
#1018=B_SPLINE_CURVE_WITH_KNOTS('',3,(#74387,#74388,#74389,#74390,#74391,
#74392,#74393,#74394,#74395,#74396,#74397),.UNSPECIFIED.,.F.,.F.,(4,1,1,
1,1,1,1,1,4),(57.6659681729844,57.8849721154671,58.8829888760786,59.8810056366901,
60.8790223973016,61.8770391579131,62.8750559185246,63.8730726791361,63.949153480164),
 .UNSPECIFIED.);
#1019=B_SPLINE_CURVE_WITH_KNOTS('',3,(#74399,#74400,#74401,#74402,#74403,
#74404,#74405,#74406,#74407,#74408),.UNSPECIFIED.,.F.,.F.,(4,1,1,1,1,1,
1,4),(63.949153480164,64.8710894397476,65.8691062003591,66.8671229609706,
67.8651397215821,68.8631564821936,69.8611732428051,70.2323312382351),
 .UNSPECIFIED.);
#1020=B_SPLINE_CURVE_WITH_KNOTS('',3,(#74410,#74411,#74412,#74413,#74414,
#74415,#74416,#74417,#74418,#74419,#74420,#74421,#74422,#74423,#74424,#74425,
#74426,#74427,#74428,#74429,#74430,#74431,#74432,#74433,#74434,#74435,#74436,
#74437,#74438,#74439,#74440,#74441,#74442,#74443,#74444,#74445,#74446,#74447,
#74448,#74449,#74450,#74451,#74452,#74453,#74454,#74455,#74456,#74457,#74458,
#74459,#74460,#74461,#74462,#74463,#74464,#74465,#74466,#74467,#74468,#74469,
#74470,#74471,#74472,#74473,#74474,#74475,#74476,#74477,#74478,#74479,#74480,
#74481,#74482,#74483,#74484,#74485,#74486,#74487,#74488,#74489,#74490,#74491,
#74492,#74493,#74494,#74495,#74496,#74497,#74498,#74499,#74500,#74501,#74502,
#74503,#74504,#74505,#74506,#74507,#74508,#74509,#74510,#74511,#74512,#74513,
#74514,#74515,#74516,#74517,#74518,#74519,#74520,#74521,#74522,#74523,#74524),
 .UNSPECIFIED.,.F.,.F.,(4,3,3,3,3,3,3,3,3,3,3,3,3,3,3,3,3,3,3,3,3,3,3,3,
3,3,3,3,3,3,3,3,3,3,3,3,3,3,4),(70.2323387873436,70.402412598027,70.5725181553533,
70.7430744181846,70.8591900034166,71.0284832593237,71.1974474301093,71.3663823338743,
71.5352718973851,71.7045671710536,71.8572067640281,72.0265000199352,72.1954641907208,
72.3643990944859,72.5332886579967,72.7025839316653,72.8552235246396,73.0245167805467,
73.1934809513323,73.3624158550973,73.531305418608,73.7006006922766,73.8532402852511,
74.0225335411582,74.1914977119439,74.3604326157089,74.5293221792196,74.6986174528881,
74.8512570458626,75.0205503017697,75.1895144725554,75.3584493763205,75.5273389398313,
75.6966342134998,75.8492738064741,76.0184566568934,76.1873006327343,76.3560790711469,
76.5155240945232),.UNSPECIFIED.);
#1021=B_SPLINE_CURVE_WITH_KNOTS('',3,(#74526,#74527,#74528,#74529,#74530,
#74531,#74532,#74533,#74534,#74535),.UNSPECIFIED.,.F.,.F.,(4,1,1,1,1,1,
1,4),(76.5155312281036,76.8472905670856,77.8453073276971,78.8433240883086,
79.8413408489201,80.8393576095316,81.8373743701431,82.7987045196599),
 .UNSPECIFIED.);
#1022=B_SPLINE_CURVE_WITH_KNOTS('',3,(#74537,#74538,#74539,#74540,#74541,
#74542,#74543,#74544,#74545,#74546,#74547,#74548,#74549,#74550,#74551,#74552,
#74553,#74554,#74555,#74556,#74557,#74558,#74559,#74560,#74561,#74562,#74563,
#74564,#74565,#74566,#74567,#74568,#74569,#74570,#74571,#74572,#74573,#74574,
#74575,#74576,#74577,#74578,#74579,#74580,#74581,#74582,#74583,#74584,#74585,
#74586,#74587,#74588,#74589,#74590,#74591,#74592,#74593,#74594,#74595,#74596,
#74597,#74598,#74599,#74600,#74601,#74602,#74603,#74604,#74605,#74606,#74607,
#74608,#74609,#74610,#74611,#74612,#74613,#74614,#74615,#74616,#74617,#74618,
#74619,#74620,#74621,#74622,#74623,#74624,#74625,#74626,#74627,#74628,#74629,
#74630,#74631,#74632,#74633,#74634,#74635,#74636,#74637,#74638,#74639,#74640,
#74641,#74642,#74643,#74644,#74645,#74646,#74647,#74648,#74649,#74650,#74651,
#74652,#74653,#74654),.UNSPECIFIED.,.F.,.F.,(4,3,3,3,3,3,3,3,3,3,3,3,3,
3,3,3,3,3,3,3,3,3,3,3,3,3,3,3,3,3,3,3,3,3,3,3,3,3,3,4),(82.7987094017028,
82.8353911307546,83.0046843866608,83.1736485574456,83.3425834612097,83.5114730247196,
83.6807682983872,83.8334078913661,84.0027011472735,84.1716653180594,84.3406002218248,
84.5094897853358,84.6787850590047,84.8314246519776,85.0007179078847,85.1696820786705,
85.3386169824355,85.5075065459464,85.676801819615,85.8294414125891,85.9987346684959,
86.1676988392813,86.336633743046,86.5055233065565,86.6748185802248,86.8274581732006,
86.9967514291082,87.1657155998943,87.3346505036598,87.5035400671711,87.6728353408401,
87.8254749338121,87.9947681897189,88.1637323605044,88.3326672642691,88.5015568277797,
88.670852101448,88.8234916944236,89.0397925300301,89.0818945515453),
 .UNSPECIFIED.);
#1023=B_SPLINE_CURVE_WITH_KNOTS('',3,(#74656,#74657,#74658,#74659,#74660,
#74661,#74662,#74663,#74664,#74665),.UNSPECIFIED.,.F.,.F.,(4,1,1,1,1,1,
1,4),(89.0818947088824,89.8215084550351,90.8195252156466,91.8175419762581,
92.8155587368696,93.8135754974811,94.8115922580926,95.365080016062),
 .UNSPECIFIED.);
#1024=B_SPLINE_CURVE_WITH_KNOTS('',3,(#74667,#74668,#74669,#74670,#74671,
#74672,#74673,#74674,#74675,#74676),.UNSPECIFIED.,.F.,.F.,(4,1,1,1,1,1,
1,4),(95.365080016062,95.8096090187041,96.8076257793156,97.8056425399271,
98.8036593005386,99.8016760611501,100.799692821762,101.64825793954),
 .UNSPECIFIED.);
#1025=B_SPLINE_CURVE_WITH_KNOTS('',3,(#74678,#74679,#74680,#74681,#74682,
#74683,#74684,#74685,#74686,#74687,#74688,#74689,#74690,#74691,#74692,#74693,
#74694,#74695,#74696,#74697,#74698,#74699,#74700,#74701,#74702,#74703,#74704,
#74705,#74706,#74707,#74708,#74709,#74710,#74711,#74712,#74713,#74714,#74715,
#74716,#74717,#74718,#74719,#74720,#74721,#74722,#74723,#74724,#74725,#74726,
#74727,#74728,#74729,#74730,#74731,#74732,#74733,#74734,#74735,#74736,#74737,
#74738,#74739,#74740,#74741,#74742,#74743,#74744,#74745,#74746,#74747,#74748,
#74749,#74750,#74751,#74752,#74753,#74754,#74755,#74756,#74757,#74758,#74759,
#74760,#74761,#74762,#74763,#74764,#74765,#74766,#74767,#74768,#74769,#74770,
#74771,#74772,#74773,#74774,#74775,#74776,#74777,#74778,#74779,#74780,#74781,
#74782,#74783,#74784,#74785,#74786,#74787,#74788,#74789,#74790,#74791,#74792),
 .UNSPECIFIED.,.F.,.F.,(4,3,3,3,3,3,3,3,3,3,3,3,3,3,3,3,3,3,3,3,3,3,3,3,
3,3,3,3,3,3,3,3,3,3,3,3,3,3,4),(101.648265323242,101.797709582373,101.967002845301,
102.135967023136,102.304901933891,102.473791504371,102.643086784828,102.795726342985,
102.965019586104,103.133983744144,103.302918635414,103.471808186543,103.641103448279,
103.793743103596,103.963036360376,104.132000531843,104.300935435991,104.469824999722,
104.639120273341,104.791759864208,104.961053164949,105.130017380809,105.298952329355,
105.467841937566,105.637137254857,105.789776624819,105.95906978473,106.128033859723,
106.296968669389,106.465858139561,106.635153323104,106.787793385431,106.957086676536,
107.126050881224,107.294985816453,107.463875410149,107.633170711279,107.785810146042,
107.931450630421),.UNSPECIFIED.);
#1026=B_SPLINE_CURVE_WITH_KNOTS('',3,(#74794,#74795,#74796,#74797,#74798,
#74799,#74800,#74801,#74802,#74803),.UNSPECIFIED.,.F.,.F.,(4,1,1,1,1,1,
1,4),(107.931458239655,108.783826906654,109.781843667265,110.779860427877,
111.777877188488,112.7758939491,113.773910709711,114.214635937601),
 .UNSPECIFIED.);
#1027=B_SPLINE_CURVE_WITH_KNOTS('',3,(#74805,#74806,#74807,#74808,#74809,
#74810,#74811,#74812,#74813,#74814),.UNSPECIFIED.,.F.,.F.,(4,1,1,1,1,1,
1,4),(114.214635937601,114.771927470323,115.769944230934,116.767960991546,
117.765977752157,118.763994512769,119.76201127338,120.49782124478),
 .UNSPECIFIED.);
#1028=B_SPLINE_CURVE_WITH_KNOTS('',3,(#74822,#74823,#74824,#74825,#74826,
#74827,#74828,#74829,#74830),.UNSPECIFIED.,.F.,.F.,(4,1,1,1,1,1,4),(-122.756061555215,
-121.758044794603,-120.760028033992,-119.76201127338,-118.763994512769,
-117.765977752157,-117.190265949363),.UNSPECIFIED.);
#1029=B_SPLINE_CURVE_WITH_KNOTS('',3,(#74832,#74833,#74834,#74835,#74836,
#74837,#74838,#74839,#74840,#74841),.UNSPECIFIED.,.F.,.F.,(4,1,1,1,1,1,
1,4),(-117.190265949363,-116.767960991546,-115.769944230934,-114.771927470323,
-113.773910709711,-112.7758939491,-111.777877188488,-110.907080642184),
 .UNSPECIFIED.);
#1030=B_SPLINE_CURVE_WITH_KNOTS('',3,(#74843,#74844,#74845,#74846,#74847,
#74848,#74849,#74850,#74851,#74852,#74853),.UNSPECIFIED.,.F.,.F.,(4,1,1,
1,1,1,1,1,4),(-110.907080642184,-110.779860427877,-109.781843667265,-108.783826906654,
-107.785810146042,-106.787793385431,-105.789776624819,-104.791759864208,
-104.623895335004),.UNSPECIFIED.);
#1031=B_SPLINE_CURVE_WITH_KNOTS('',3,(#74855,#74856,#74857,#74858,#74859,
#74860,#74861,#74862,#74863,#74864,#74865,#74866,#74867,#74868,#74869,#74870,
#74871,#74872,#74873,#74874,#74875,#74876,#74877,#74878,#74879,#74880,#74881,
#74882,#74883,#74884,#74885,#74886,#74887,#74888,#74889,#74890,#74891,#74892,
#74893,#74894,#74895,#74896,#74897,#74898,#74899,#74900,#74901,#74902,#74903,
#74904,#74905,#74906,#74907,#74908,#74909,#74910,#74911,#74912,#74913,#74914,
#74915,#74916,#74917,#74918,#74919,#74920,#74921,#74922,#74923,#74924,#74925,
#74926,#74927,#74928,#74929,#74930,#74931,#74932,#74933,#74934,#74935,#74936,
#74937,#74938,#74939,#74940,#74941,#74942,#74943,#74944,#74945,#74946,#74947,
#74948,#74949,#74950,#74951,#74952,#74953,#74954,#74955,#74956,#74957,#74958,
#74959,#74960,#74961,#74962,#74963,#74964,#74965,#74966,#74967,#74968,#74969),
 .UNSPECIFIED.,.F.,.F.,(4,3,3,3,3,3,3,3,3,3,3,3,3,3,3,3,3,3,3,3,3,3,3,3,
3,3,3,3,3,3,3,3,3,3,3,3,3,3,4),(-104.623895335004,-104.45732649546,-104.29085058873,
-104.124460630739,-103.957682801808,-103.793743103596,-103.624449859544,
-103.455485700924,-103.286550809622,-103.11766125876,-102.948365997786,
-102.795726342985,-102.626433080327,-102.457468902668,-102.288533991942,
-102.119644421409,-101.950349140766,-101.797709582373,-101.628416327047,
-101.459452156828,-101.290517253598,-101.121627690605,-100.952332417415,
-100.799692821762,-100.630399567375,-100.461435398152,-100.292500495991,
-100.123610934111,-99.9543156620825,-99.8016760611501,-99.6323828042209,
-99.4634186323931,-99.294483727571,-99.1255941629928,-98.9562988882624,
-98.8036593005386,-98.6226668537811,-98.4425781871584,-98.3407102215442),
 .UNSPECIFIED.);
#1032=B_SPLINE_CURVE_WITH_KNOTS('',3,(#74971,#74972,#74973,#74974,#74975,
#74976,#74977,#74978,#74979,#74980),.UNSPECIFIED.,.F.,.F.,(4,1,1,1,1,1,
1,4),(-98.3407100278245,-97.8056425399271,-96.8076257793156,-95.8096090187041,
-94.8115922580926,-93.8135754974811,-92.8155587368696,-92.0575247206449),
 .UNSPECIFIED.);
#1033=B_SPLINE_CURVE_WITH_KNOTS('',3,(#74982,#74983,#74984,#74985,#74986,
#74987,#74988,#74989,#74990,#74991,#74992),.UNSPECIFIED.,.F.,.F.,(4,1,1,
1,1,1,1,1,4),(-92.0575247206449,-91.8175419762581,-90.8195252156466,-89.8215084550351,
-88.8234916944236,-87.8254749338121,-86.8274581732006,-85.8294414125891,
-85.7743394134653),.UNSPECIFIED.);
#1034=B_SPLINE_CURVE_WITH_KNOTS('',3,(#74994,#74995,#74996,#74997,#74998,
#74999,#75000,#75001,#75002,#75003,#75004,#75005,#75006,#75007,#75008,#75009,
#75010,#75011,#75012,#75013,#75014,#75015,#75016,#75017,#75018,#75019,#75020,
#75021,#75022,#75023,#75024,#75025,#75026,#75027,#75028,#75029,#75030,#75031,
#75032,#75033,#75034,#75035,#75036,#75037,#75038,#75039,#75040,#75041,#75042,
#75043,#75044,#75045,#75046,#75047,#75048,#75049,#75050,#75051,#75052,#75053,
#75054,#75055,#75056,#75057,#75058,#75059,#75060,#75061,#75062,#75063,#75064,
#75065,#75066,#75067,#75068,#75069,#75070,#75071,#75072,#75073,#75074,#75075,
#75076,#75077,#75078,#75079,#75080,#75081,#75082,#75083,#75084,#75085,#75086,
#75087,#75088,#75089,#75090,#75091,#75092,#75093,#75094,#75095,#75096,#75097,
#75098,#75099,#75100,#75101,#75102,#75103,#75104,#75105,#75106,#75107,#75108),
 .UNSPECIFIED.,.F.,.F.,(4,3,3,3,3,3,3,3,3,3,3,3,3,3,3,3,3,3,3,3,3,3,3,3,
3,3,3,3,3,3,3,3,3,3,3,3,3,3,4),(-85.7743394134653,-85.6064724999714,-85.4389194739953,
-85.2713832903716,-85.1038697181618,-84.9359767817762,-84.8314246519776,
-84.6621313960704,-84.4931672252848,-84.3242323215197,-84.1553427580088,
-83.9860474843402,-83.8334078913661,-83.664114635459,-83.4951504646734,
-83.3262155609084,-83.1573259973976,-82.9880307237291,-82.8353911307546,
-82.6660978748475,-82.4971337040618,-82.3281988002967,-82.1593092367859,
-81.9900139631174,-81.8373743701431,-81.668081114236,-81.4991169434503,
-81.3301820396853,-81.1612924761746,-80.991997202506,-80.8393576095316,
-80.6700643536246,-80.5011001828388,-80.3321652790738,-80.1632757155631,
-79.9939804418945,-79.8413408489201,-79.6466720371967,-79.4911543477215),
 .UNSPECIFIED.);
#1035=B_SPLINE_CURVE_WITH_KNOTS('',3,(#75110,#75111,#75112,#75113,#75114,
#75115,#75116,#75117,#75118,#75119),.UNSPECIFIED.,.F.,.F.,(4,1,1,1,1,1,
1,4),(-79.4911541062857,-78.8433240883086,-77.8453073276971,-76.8472905670856,
-75.8492738064741,-74.8512570458626,-73.853240285251,-73.2079687991061),
 .UNSPECIFIED.);
#1036=B_SPLINE_CURVE_WITH_KNOTS('',3,(#75121,#75122,#75123,#75124,#75125,
#75126,#75127,#75128,#75129,#75130,#75131,#75132,#75133,#75134,#75135,#75136,
#75137,#75138,#75139,#75140,#75141,#75142,#75143,#75144,#75145,#75146,#75147,
#75148,#75149,#75150,#75151,#75152,#75153,#75154,#75155,#75156,#75157,#75158,
#75159,#75160,#75161,#75162,#75163,#75164,#75165,#75166,#75167,#75168,#75169,
#75170,#75171,#75172,#75173,#75174,#75175,#75176,#75177,#75178,#75179,#75180,
#75181,#75182,#75183,#75184,#75185,#75186,#75187,#75188,#75189,#75190,#75191,
#75192,#75193,#75194,#75195,#75196,#75197,#75198,#75199,#75200,#75201,#75202,
#75203,#75204,#75205,#75206,#75207,#75208,#75209,#75210,#75211,#75212,#75213,
#75214,#75215,#75216,#75217,#75218,#75219,#75220,#75221,#75222,#75223,#75224,
#75225,#75226,#75227,#75228,#75229,#75230,#75231,#75232,#75233,#75234,#75235),
 .UNSPECIFIED.,.F.,.F.,(4,3,3,3,3,3,3,3,3,3,3,3,3,3,3,3,3,3,3,3,3,3,3,3,
3,3,3,3,3,3,3,3,3,3,3,3,3,3,4),(-73.2079685568002,-73.0137286976384,-72.8552235246396,
-72.6859302687325,-72.5169660979467,-72.3480311941816,-72.1791416306707,
-72.0098463570021,-71.8572067640281,-71.687913508121,-71.5189493373353,
-71.3500144335703,-71.1811248700595,-71.011829596391,-70.8591900034166,
-70.6898967475095,-70.5209325767238,-70.3519976729588,-70.183108109448,
-70.0138128357795,-69.8611732428051,-69.691879986898,-69.5229158161123,
-69.3539809123473,-69.1850913488366,-69.015796075168,-68.8631564821936,
-68.6938632262865,-68.5248990555009,-68.3559641517358,-68.1870745882251,
-68.0177793145566,-67.8651397215821,-67.6972941225137,-67.5297746092041,
-67.3622911014372,-67.1948402465308,-67.0270286612039,-66.9247834919265),
 .UNSPECIFIED.);
#1037=B_SPLINE_CURVE_WITH_KNOTS('',3,(#75237,#75238,#75239,#75240,#75241,
#75242,#75243,#75244,#75245,#75246,#75247),.UNSPECIFIED.,.F.,.F.,(4,1,1,
1,1,1,1,1,4),(-66.9247834919265,-66.8671229609706,-65.8691062003591,-64.8710894397476,
-63.8730726791361,-62.8750559185245,-61.8770391579131,-60.8790223973016,
-60.641598184747),.UNSPECIFIED.);
#1038=B_SPLINE_CURVE_WITH_KNOTS('',3,(#75249,#75250,#75251,#75252,#75253,
#75254,#75255,#75256,#75257,#75258),.UNSPECIFIED.,.F.,.F.,(4,1,1,1,1,1,
1,4),(-60.641598184747,-59.8810056366901,-58.8829888760786,-57.8849721154671,
-56.8869553548555,-55.8889385942441,-54.8909218336326,-54.3584128775674),
 .UNSPECIFIED.);
#1039=B_SPLINE_CURVE_WITH_KNOTS('',3,(#75260,#75261,#75262,#75263,#75264,
#75265,#75266,#75267,#75268,#75269,#75270,#75271,#75272,#75273,#75274,#75275,
#75276,#75277,#75278,#75279,#75280,#75281,#75282,#75283,#75284,#75285,#75286,
#75287,#75288,#75289,#75290,#75291,#75292,#75293,#75294,#75295,#75296,#75297,
#75298,#75299,#75300,#75301,#75302,#75303,#75304,#75305,#75306,#75307,#75308,
#75309,#75310,#75311,#75312,#75313,#75314,#75315,#75316,#75317,#75318,#75319,
#75320,#75321,#75322,#75323,#75324,#75325,#75326,#75327,#75328,#75329,#75330,
#75331,#75332,#75333,#75334,#75335,#75336,#75337,#75338,#75339,#75340,#75341,
#75342,#75343,#75344,#75345,#75346,#75347,#75348,#75349,#75350,#75351,#75352,
#75353,#75354,#75355,#75356,#75357,#75358,#75359,#75360,#75361,#75362,#75363,
#75364,#75365,#75366,#75367,#75368,#75369,#75370,#75371,#75372,#75373,#75374),
 .UNSPECIFIED.,.F.,.F.,(4,3,3,3,3,3,3,3,3,3,3,3,3,3,3,3,3,3,3,3,3,3,3,3,
3,3,3,3,3,3,3,3,3,3,3,3,3,3,4),(-54.3584126969109,-54.1786932265056,-53.998027905295,
-53.892905073021,-53.7236118171141,-53.5546476463285,-53.3857127425637,
-53.216823179053,-53.0475279053846,-52.8948883124096,-52.7255950565025,
-52.5566308857167,-52.3876959819517,-52.2188064184408,-52.0495111447722,
-51.896871551798,-51.7275782958909,-51.5586141251052,-51.3896792213402,
-51.2207896578294,-51.0514943841608,-50.8988547911866,-50.7295615352796,
-50.5605973644939,-50.3916624607289,-50.2227728972182,-50.0534776235497,
-49.9008380305751,-49.731544774668,-49.5625806038823,-49.3936457001172,
-49.2247561366064,-49.0554608629379,-48.9028212699636,-48.7360498525631,
-48.5695217660508,-48.4031605705744,-48.236550279102,-48.0752275703878),
 .UNSPECIFIED.);
#1040=B_SPLINE_CURVE_WITH_KNOTS('',3,(#75376,#75377,#75378,#75379,#75380,
#75381,#75382,#75383,#75384,#75385,#75386),.UNSPECIFIED.,.F.,.F.,(4,1,1,
1,1,1,1,1,4),(-48.0752275703878,-47.9048045093521,-46.9067877487405,-45.908770988129,
-44.9107542275176,-43.912737466906,-42.9147207062945,-41.916703945683,-41.7920422632082),
 .UNSPECIFIED.);
#1041=B_SPLINE_CURVE_WITH_KNOTS('',3,(#75388,#75389,#75390,#75391,#75392,
#75393,#75394,#75395,#75396,#75397,#75398,#75399,#75400,#75401,#75402,#75403,
#75404,#75405,#75406,#75407,#75408,#75409,#75410,#75411,#75412,#75413,#75414,
#75415,#75416,#75417,#75418,#75419,#75420,#75421,#75422,#75423,#75424,#75425,
#75426,#75427,#75428,#75429,#75430,#75431,#75432,#75433,#75434,#75435,#75436,
#75437,#75438,#75439,#75440,#75441,#75442,#75443,#75444,#75445,#75446,#75447,
#75448,#75449,#75450,#75451,#75452,#75453,#75454,#75455,#75456,#75457,#75458,
#75459,#75460,#75461,#75462,#75463,#75464,#75465,#75466,#75467,#75468,#75469,
#75470,#75471,#75472,#75473,#75474,#75475,#75476,#75477,#75478,#75479,#75480,
#75481,#75482,#75483,#75484,#75485,#75486,#75487,#75488,#75489,#75490,#75491,
#75492,#75493,#75494,#75495,#75496,#75497,#75498,#75499,#75500,#75501,#75502,
#75503,#75504,#75505),.UNSPECIFIED.,.F.,.F.,(4,3,3,3,3,3,3,3,3,3,3,3,3,
3,3,3,3,3,3,3,3,3,3,3,3,3,3,3,3,3,3,3,3,3,3,3,3,3,3,4),(-41.7920422632082,
-41.6252296124417,-41.4586871830981,-41.2921234036511,-41.1255384648325,
-40.9585984248305,-40.9186871850715,-40.7493939291644,-40.5804297583788,
-40.4114948546138,-40.242605291103,-40.0733100174345,-39.92067042446,-39.751377168553,
-39.5824129977674,-39.4134780940024,-39.2445885304916,-39.0752932568231,
-38.9226536638485,-38.7533604079413,-38.5843962371556,-38.4154613333905,
-38.2465717698797,-38.0772764962111,-37.924636903237,-37.7553436473299,
-37.5863794765442,-37.4174445727792,-37.2485550092685,-37.0792597356,-36.9266201426255,
-36.7573268867186,-36.588362715933,-36.4194278121681,-36.2505382486576,
-36.0812429749892,-35.928603382014,-35.7430372886009,-35.5587073803211,
-35.5088569562119),.UNSPECIFIED.);
#1042=B_SPLINE_CURVE_WITH_KNOTS('',3,(#75507,#75508,#75509,#75510,#75511,
#75512,#75513,#75514,#75515,#75516,#75517,#75518,#75519,#75520,#75521,#75522,
#75523,#75524,#75525,#75526,#75527,#75528,#75529,#75530,#75531,#75532,#75533,
#75534,#75535,#75536,#75537,#75538,#75539,#75540,#75541,#75542,#75543,#75544,
#75545,#75546,#75547,#75548,#75549,#75550,#75551,#75552,#75553,#75554,#75555,
#75556,#75557,#75558,#75559,#75560,#75561,#75562,#75563,#75564,#75565,#75566,
#75567,#75568,#75569,#75570,#75571,#75572,#75573,#75574,#75575,#75576,#75577,
#75578,#75579,#75580,#75581,#75582,#75583,#75584,#75585,#75586,#75587,#75588,
#75589,#75590,#75591,#75592,#75593,#75594,#75595,#75596,#75597,#75598,#75599,
#75600,#75601,#75602,#75603,#75604,#75605,#75606,#75607,#75608,#75609,#75610,
#75611,#75612,#75613,#75614,#75615,#75616,#75617,#75618,#75619,#75620,#75621,
#75622,#75623,#75624),.UNSPECIFIED.,.F.,.F.,(4,3,3,3,3,3,3,3,3,3,3,3,3,
3,3,3,3,3,3,3,3,3,3,3,3,3,3,3,3,3,3,3,3,3,3,3,3,3,3,4),(-35.5088569560286,
-35.3366913932997,-35.1643891329436,-34.9915938457824,-34.9305866214025,
-34.7612933654957,-34.5923291947103,-34.4233942909455,-34.254504727435,
-34.0852094537667,-33.932569860791,-33.763276604885,-33.5943124341005,-33.4253775303366,
-33.256487966827,-33.0871926931595,-32.9345531001795,-32.7652598442691,
-32.5962956734802,-32.4273607697119,-32.258471206198,-32.0891759325263,
-31.936536339568,-31.7672430836636,-31.5982789128805,-31.4293440091181,
-31.2604544456098,-31.0911591719436,-30.9385195789565,-30.7692263230558,
-30.6002621522766,-30.431327248518,-30.2624376850138,-30.0931424113516,
-29.940502818345,-29.7725436020734,-29.6049127376607,-29.4374658129547,
-29.2699561832517,-29.225671648849),.UNSPECIFIED.);
#1043=B_SPLINE_CURVE_WITH_KNOTS('',3,(#75626,#75627,#75628,#75629,#75630,
#75631,#75632,#75633,#75634,#75635,#75636),.UNSPECIFIED.,.F.,.F.,(4,1,1,
1,1,1,1,1,4),(-29.2256671317155,-28.9424860577335,-27.944469297122,-26.9464525365105,
-25.948435775899,-24.9504190152875,-23.952402254676,-22.9543854940645,-22.9424863416694),
 .UNSPECIFIED.);
#1044=B_SPLINE_CURVE_WITH_KNOTS('',3,(#75638,#75639,#75640,#75641,#75642,
#75643,#75644,#75645,#75646,#75647,#75648,#75649,#75650,#75651,#75652,#75653,
#75654,#75655,#75656,#75657,#75658,#75659,#75660,#75661,#75662,#75663,#75664,
#75665,#75666,#75667,#75668,#75669,#75670,#75671,#75672,#75673,#75674,#75675,
#75676,#75677,#75678,#75679,#75680,#75681,#75682,#75683,#75684,#75685,#75686,
#75687,#75688,#75689,#75690,#75691,#75692,#75693,#75694,#75695,#75696,#75697,
#75698,#75699,#75700,#75701,#75702,#75703,#75704,#75705,#75706,#75707,#75708,
#75709,#75710,#75711,#75712,#75713,#75714,#75715,#75716,#75717,#75718,#75719,
#75720,#75721,#75722,#75723,#75724,#75725,#75726,#75727,#75728,#75729,#75730,
#75731,#75732,#75733,#75734,#75735,#75736,#75737,#75738,#75739,#75740,#75741,
#75742,#75743,#75744,#75745,#75746,#75747,#75748,#75749,#75750,#75751,#75752),
 .UNSPECIFIED.,.F.,.F.,(4,3,3,3,3,3,3,3,3,3,3,3,3,3,3,3,3,3,3,3,3,3,3,3,
3,3,3,3,3,3,3,3,3,3,3,3,3,3,4),(-22.9424863416694,-22.7735464381667,-22.6049342401408,
-22.436350429138,-22.2678081433635,-22.0988663171801,-21.956368733453,-21.7870754780197,
-21.6181113077355,-21.4491764045062,-21.280286841551,-21.1109915684584,
-20.9583519728415,-20.7890587099447,-20.6200945321411,-20.451159621418,
-20.2822700509694,-20.1129747705427,-19.96033521223,-19.7910419690666,-19.6220778109816,
-19.4531429196686,-19.2842533684958,-19.1149581067184,-18.9623184516185,
-18.7930251948294,-18.6240610233531,-18.4551261191945,-18.2862365554524,
-18.1169412818215,-17.964301691007,-17.7950083904281,-17.6260441747308,
-17.4571092263467,-17.2882196182969,-17.1189243011628,-16.9662849303955,
-16.763195454698,-16.6593012290017),.UNSPECIFIED.);
#1045=B_SPLINE_CURVE_WITH_KNOTS('',3,(#75754,#75755,#75756,#75757,#75758,
#75759,#75760,#75761,#75762,#75763),.UNSPECIFIED.,.F.,.F.,(4,1,1,1,1,1,
1,4),(-16.6593010344898,-15.968268169784,-14.9702514091725,-13.972234648561,
-12.9742178879495,-11.976201127338,-10.9781843667265,-10.3761157273102),
 .UNSPECIFIED.);
#1046=B_SPLINE_CURVE_WITH_KNOTS('',3,(#75764,#75765,#75766,#75767,#75768,
#75769,#75770,#75771,#75772,#75773),.UNSPECIFIED.,.F.,.F.,(4,1,1,1,1,1,
1,4),(-10.3761157273102,-9.98016760611501,-8.98215084550351,-7.98413408489201,
-6.98611732428051,-5.98810056366901,-4.9900838030575,-4.09293928071616),
 .UNSPECIFIED.);
#1047=B_SPLINE_CURVE_WITH_KNOTS('',3,(#75776,#75777,#75778,#75779,#75780,
#75781,#75782,#75783,#75784,#75785,#75786,#75787,#75788,#75789,#75790,#75791,
#75792,#75793,#75794,#75795,#75796,#75797,#75798,#75799,#75800,#75801,#75802,
#75803,#75804,#75805,#75806,#75807,#75808,#75809,#75810,#75811,#75812,#75813,
#75814,#75815,#75816,#75817,#75818,#75819,#75820,#75821,#75822,#75823,#75824,
#75825,#75826,#75827,#75828,#75829,#75830,#75831,#75832,#75833,#75834,#75835,
#75836,#75837,#75838,#75839,#75840,#75841,#75842,#75843,#75844,#75845,#75846,
#75847,#75848,#75849,#75850,#75851,#75852,#75853,#75854,#75855,#75856,#75857,
#75858,#75859,#75860,#75861,#75862,#75863,#75864,#75865,#75866,#75867,#75868,
#75869,#75870,#75871,#75872,#75873,#75874,#75875,#75876,#75877,#75878,#75879,
#75880,#75881,#75882,#75883,#75884,#75885,#75886,#75887,#75888,#75889,#75890,
#75891,#75892,#75893,#75894,#75895,#75896,#75897,#75898,#75899,#75900,#75901,
#75902,#75903,#75904,#75905,#75906,#75907,#75908,#75909,#75910,#75911,#75912,
#75913,#75914,#75915,#75916,#75917,#75918,#75919,#75920,#75921,#75922,#75923,
#75924,#75925,#75926,#75927,#75928,#75929,#75930,#75931,#75932,#75933,#75934,
#75935,#75936,#75937,#75938,#75939,#75940,#75941,#75942,#75943,#75944,#75945,
#75946,#75947,#75948,#75949,#75950,#75951,#75952,#75953,#75954,#75955,#75956,
#75957,#75958,#75959,#75960,#75961,#75962,#75963,#75964,#75965,#75966,#75967,
#75968,#75969,#75970,#75971,#75972,#75973,#75974,#75975,#75976,#75977,#75978,
#75979,#75980,#75981,#75982,#75983,#75984,#75985,#75986,#75987,#75988,#75989,
#75990,#75991,#75992,#75993,#75994,#75995,#75996,#75997,#75998,#75999,#76000,
#76001,#76002,#76003,#76004,#76005,#76006,#76007),.UNSPECIFIED.,.F.,.F.,
(4,2,2,2,2,2,2,2,2,2,2,2,2,2,2,2,2,2,2,2,2,2,2,2,2,2,2,2,2,2,2,2,2,2,2,
2,2,2,2,2,2,2,2,2,2,2,2,2,2,2,2,2,2,2,2,2,2,2,2,2,2,2,2,2,2,2,2,2,2,2,2,
2,2,2,2,2,2,2,2,2,2,2,2,2,2,2,2,2,2,2,2,2,2,2,2,2,2,2,2,2,2,2,2,2,2,2,2,
2,2,2,2,2,2,2,2,4),(0.00386804990396825,0.0562394845893352,0.0855082425021677,
0.0967963778164743,0.101688678092589,0.105316915758188,0.109170828160612,
0.115206022997764,0.13352155193086,0.18214966217015,0.184505714254096,0.210496838182648,
0.216408804068253,0.21898183194266,0.219001669665326,0.219021656865823,
0.219041800143975,0.219062106303896,0.219082582367891,0.219103235589411,
0.219124073456259,0.219145103705878,0.21916633434941,0.219187773677002,
0.219209430278248,0.219231313055561,0.219253431238468,0.21927579440997,
0.219298412519007,0.219321295907952,0.219344455331709,0.219367901981367,
0.219391647508508,0.219415704054726,0.219440084280359,0.219456149678306,
0.219473316498225,0.219491677543212,0.219511335758724,0.219532405688436,
0.219555015155175,0.219579307277774,0.219605442856093,0.219633603231849,
0.21966399372401,0.219696847787709,0.21973243208813,0.219771052729119,0.219813062929726,
0.219858872626143,0.219896283448798,0.21995497467274,0.220103383909864,
0.222085813063994,0.224833395424335,0.231063205287695,0.267083001906452,
0.298908358386698,0.327015401127584,0.333646285187427,0.337599873377424,
0.341141196559091,0.345657839892338,0.355031731773855,0.409461104368223,
0.42212031792051,0.44147760840121,0.452386379069429,0.455728112289525,0.457846204907444,
0.459857139166811,0.462351221071398,0.468558193129114,0.505221941771184,
0.538022947485726,0.555995885137095,0.568369504724233,0.573366873604649,
0.576946354421215,0.58020234353761,0.584572579694303,0.593107307405052,
0.64484900429152,0.687001284439138,0.692128675899164,0.694610873875239,
0.696383997866516,0.698664122325341,0.702641545605574,0.719799480324097,
0.770150687164016,0.802462215093125,0.809319052133648,0.813315044379787,
0.816838441202234,0.821257209706951,0.829870588557781,0.889369746514473,
0.914109200745218,0.926855260915289,0.930387020161787,0.932551544688672,
0.934554760316714,0.936980728884274,0.943169252980154,0.986704068278608,
1.01565528028879,1.04026175474148,1.04663258402857,1.05051787081069,1.05405341606083,
1.05856448569977,1.0682373468359,1.11278921194253,1.14817633214325,1.16375694728592),
 .UNSPECIFIED.);
#1048=B_SPLINE_CURVE_WITH_KNOTS('',3,(#76011,#76012,#76013,#76014,#76015,
#76016,#76017,#76018,#76019,#76020,#76021,#76022,#76023,#76024,#76025,#76026,
#76027,#76028,#76029,#76030,#76031,#76032,#76033,#76034,#76035,#76036,#76037,
#76038,#76039,#76040,#76041,#76042,#76043,#76044,#76045,#76046,#76047,#76048,
#76049,#76050,#76051,#76052,#76053),.UNSPECIFIED.,.F.,.F.,(4,3,3,3,3,3,
3,3,3,3,3,3,3,3,4),(128.80529879753,129.037126539512,129.067505586393,129.244234518971,
129.420602827541,129.596971260776,129.773322085525,129.950145844604,130.065522347004,
130.24915598036,130.432352008113,130.615311891496,130.798119431239,130.981055100704,
131.063539107616),.UNSPECIFIED.);
#1049=B_SPLINE_CURVE_WITH_KNOTS('',3,(#76054,#76055,#76056,#76057,#76058,
#76059,#76060,#76061,#76062,#76063,#76064,#76065,#76066,#76067,#76068,#76069,
#76070,#76071,#76072,#76073,#76074,#76075,#76076,#76077,#76078,#76079,#76080,
#76081,#76082,#76083,#76084,#76085,#76086,#76087,#76088,#76089,#76090,#76091,
#76092,#76093,#76094,#76095,#76096,#76097,#76098,#76099,#76100,#76101,#76102,
#76103),.UNSPECIFIED.,.F.,.F.,(4,2,2,2,2,2,2,2,2,2,2,2,2,2,2,2,2,2,2,2,
2,2,2,2,4),(-2.98961655725948,-2.95583465484829,-2.9418819665473,-2.93716913675111,
-2.93276629062489,-2.92919655162135,-2.92508182892515,-2.91803211560185,
-2.88502465965471,-2.84900598810215,-2.82377017441525,-2.81864302010618,
-2.81604948517044,-2.81402857579406,-2.81164374604156,-2.80726775189915,
-2.78285881200516,-2.73132000540922,-2.7078524312586,-2.70166823698996,
-2.69772318235366,-2.69417904573976,-2.68964433807738,-2.68017874108153,
-2.65819190440258),.UNSPECIFIED.);
#1050=B_SPLINE_CURVE_WITH_KNOTS('',3,(#76107,#76108,#76109,#76110,#76111,
#76112,#76113,#76114,#76115,#76116,#76117,#76118,#76119,#76120,#76121,#76122,
#76123,#76124,#76125,#76126,#76127,#76128,#76129,#76130,#76131,#76132,#76133,
#76134,#76135,#76136,#76137,#76138,#76139,#76140,#76141,#76142,#76143,#76144,
#76145,#76146,#76147,#76148,#76149,#76150,#76151,#76152,#76153,#76154,#76155,
#76156,#76157,#76158,#76159,#76160,#76161),.UNSPECIFIED.,.F.,.F.,(4,3,3,
3,3,3,3,3,3,3,3,3,3,3,3,3,3,3,4),(-0.547315088709847,-0.531428325283962,
-0.490979859218829,-0.459260446609245,-0.418148761644263,-0.399517638250514,
-0.380002035550477,-0.330811395611051,-0.294813706749318,-0.256386932726606,
-0.252448329891692,-0.213875797295427,-0.196110964560955,-0.178602317878619,
-0.131364170579549,-0.0981581995066324,-0.0854921122832515,-0.0410303375732965,
0.),.UNSPECIFIED.);
#1051=B_SPLINE_CURVE_WITH_KNOTS('',3,(#76163,#76164,#76165,#76166),
 .UNSPECIFIED.,.F.,.F.,(4,4),(0.,0.0133475310981651),.UNSPECIFIED.);
#1052=B_SPLINE_CURVE_WITH_KNOTS('',3,(#76167,#76168,#76169,#76170,#76171,
#76172,#76173,#76174,#76175,#76176,#76177,#76178,#76179,#76180,#76181,#76182,
#76183,#76184,#76185,#76186,#76187,#76188,#76189,#76190,#76191,#76192,#76193,
#76194,#76195,#76196,#76197,#76198,#76199,#76200,#76201,#76202,#76203,#76204,
#76205,#76206,#76207,#76208,#76209,#76210,#76211,#76212,#76213,#76214,#76215,
#76216,#76217,#76218,#76219,#76220,#76221,#76222,#76223,#76224),
 .UNSPECIFIED.,.F.,.F.,(4,3,3,3,3,3,3,3,3,3,3,3,3,3,3,3,3,3,3,4),(-0.555272788399299,
-0.537779111114978,-0.501074110893508,-0.477787886406151,-0.446868439925717,
-0.42563948423308,-0.408907819583257,-0.360744333019942,-0.329827946927358,
-0.312213887820072,-0.282444121695023,-0.234073861148414,-0.224809052384305,
-0.20825707532324,-0.15619280649243,-0.130527661559902,-0.110867144085924,
-0.0896774338839242,-0.0374232998864532,0.),.UNSPECIFIED.);
#1053=B_SPLINE_CURVE_WITH_KNOTS('',3,(#76729,#76730,#76731,#76732),
 .UNSPECIFIED.,.F.,.F.,(4,4),(-0.00544371575786758,0.),.UNSPECIFIED.);
#1054=B_SPLINE_CURVE_WITH_KNOTS('',3,(#76733,#76734,#76735,#76736,#76737,
#76738,#76739,#76740,#76741,#76742,#76743,#76744,#76745,#76746,#76747,#76748,
#76749,#76750,#76751,#76752,#76753,#76754,#76755,#76756,#76757,#76758,#76759,
#76760,#76761,#76762,#76763,#76764,#76765,#76766,#76767,#76768,#76769,#76770,
#76771,#76772,#76773,#76774,#76775,#76776,#76777,#76778,#76779,#76780,#76781,
#76782,#76783,#76784,#76785,#76786,#76787,#76788,#76789,#76790),
 .UNSPECIFIED.,.F.,.F.,(4,3,3,3,3,3,3,3,3,3,3,3,3,3,3,3,3,3,3,4),(-0.555272788399386,
-0.537779111115071,-0.501074112362602,-0.477787892025313,-0.446868055693454,
-0.425638893303973,-0.408906546180235,-0.360743046457414,-0.329827221992677,
-0.312213870800153,-0.282444121695054,-0.247138606483173,-0.225449912105354,
-0.208551551306268,-0.156413663479703,-0.130587374300692,-0.110975709681529,
-0.089976587580161,-0.0377183992018807,-5.54359081993786E-15),
 .UNSPECIFIED.);
#1055=B_SPLINE_CURVE_WITH_KNOTS('',3,(#76796,#76797,#76798,#76799,#76800,
#76801,#76802,#76803,#76804,#76805,#76806,#76807,#76808,#76809,#76810,#76811,
#76812,#76813,#76814,#76815,#76816,#76817,#76818,#76819,#76820,#76821,#76822,
#76823,#76824,#76825,#76826,#76827,#76828,#76829,#76830,#76831,#76832,#76833,
#76834,#76835,#76836,#76837,#76838,#76839,#76840,#76841,#76842,#76843,#76844,
#76845,#76846,#76847,#76848,#76849,#76850),.UNSPECIFIED.,.F.,.F.,(4,3,3,
3,3,3,3,3,3,3,3,3,3,3,3,3,3,3,4),(-0.547315281725085,-0.531428325284014,
-0.496555825859975,-0.475791121788961,-0.449884625300703,-0.41656343962899,
-0.397878131514439,-0.372466266802526,-0.323055462904821,-0.303122396484449,
-0.284649768256134,-0.252448329891705,-0.202775577609412,-0.18183632959102,
-0.136377247193265,-0.103314858687064,-0.0827138692056586,-0.0383174249070739,
0.),.UNSPECIFIED.);
#1056=B_SPLINE_CURVE_WITH_KNOTS('',3,(#77355,#77356,#77357,#77358),
 .UNSPECIFIED.,.F.,.F.,(4,4),(0.,0.00545462077073238),.UNSPECIFIED.);
#1057=B_SPLINE_CURVE_WITH_KNOTS('',3,(#77452,#77453,#77454,#77455,#77456,
#77457,#77458,#77459,#77460,#77461,#77462,#77463,#77464,#77465,#77466,#77467,
#77468,#77469,#77470,#77471,#77472,#77473,#77474,#77475,#77476,#77477,#77478,
#77479,#77480,#77481,#77482,#77483,#77484,#77485,#77486,#77487,#77488,#77489,
#77490,#77491,#77492,#77493,#77494,#77495,#77496,#77497,#77498,#77499,#77500,
#77501,#77502,#77503,#77504,#77505,#77506,#77507,#77508,#77509,#77510,#77511,
#77512,#77513,#77514,#77515,#77516,#77517,#77518,#77519,#77520,#77521,#77522,
#77523,#77524,#77525,#77526,#77527),.UNSPECIFIED.,.F.,.F.,(4,3,3,3,3,3,
3,3,3,3,3,3,3,3,3,3,3,3,3,3,3,3,3,3,3,4),(10.3765279447494,10.5534408108777,
10.7390672436552,10.9156311402548,11.092209959865,11.2691639748381,11.2959465419876,
11.4749627408317,11.6536283105826,11.8322755610944,12.0108999290652,12.1899418681108,
12.2921028718499,12.4705669207875,12.6486653263687,12.8267315154106,13.0047661728317,
13.1832164114546,13.2882592017121,13.4670164932441,13.6454135437631,13.8237819839401,
14.0021213662665,14.1808742422402,14.2844155315743,14.3150784600182),
 .UNSPECIFIED.);
#1058=B_SPLINE_CURVE_WITH_KNOTS('',3,(#77530,#77531,#77532,#77533,#77534,
#77535,#77536,#77537,#77538,#77539,#77540,#77541,#77542,#77543,#77544,#77545,
#77546,#77547,#77548,#77549,#77550,#77551,#77552,#77553,#77554,#77555,#77556,
#77557,#77558,#77559,#77560,#77561,#77562,#77563,#77564,#77565,#77566,#77567,
#77568,#77569,#77570,#77571,#77572,#77573,#77574,#77575,#77576,#77577,#77578),
 .UNSPECIFIED.,.F.,.F.,(4,3,3,3,3,3,3,3,3,3,3,3,3,3,3,3,4),(11.6150328478182,
11.7979860071945,11.9808051200463,12.1638372320247,12.3469748436598,12.5306212400219,
12.6111891776804,12.7880694650036,12.9645487109607,13.1409651633225,13.3173295184066,
13.4941088918777,13.6073455075426,13.7863288313326,13.9649582660013,14.1435821147139,
14.3143563514564),.UNSPECIFIED.);
#1059=B_SPLINE_CURVE_WITH_KNOTS('',3,(#77584,#77585,#77586,#77587,#77588,
#77589,#77590,#77591,#77592,#77593,#77594,#77595,#77596,#77597,#77598,#77599,
#77600,#77601,#77602,#77603,#77604,#77605,#77606,#77607,#77608,#77609,#77610,
#77611,#77612,#77613,#77614,#77615,#77616,#77617,#77618,#77619,#77620,#77621,
#77622,#77623,#77624,#77625,#77626,#77627,#77628,#77629,#77630,#77631,#77632,
#77633,#77634,#77635,#77636,#77637,#77638,#77639,#77640,#77641,#77642,#77643,
#77644,#77645,#77646,#77647,#77648,#77649,#77650,#77651,#77652,#77653,#77654,
#77655,#77656,#77657,#77658,#77659,#77660,#77661,#77662,#77663,#77664,#77665,
#77666,#77667,#77668,#77669,#77670,#77671,#77672,#77673,#77674,#77675,#77676,
#77677,#77678,#77679,#77680,#77681,#77682,#77683,#77684,#77685,#77686,#77687,
#77688,#77689,#77690,#77691,#77692,#77693,#77694,#77695,#77696,#77697,#77698,
#77699,#77700,#77701,#77702,#77703,#77704,#77705,#77706,#77707,#77708,#77709,
#77710,#77711,#77712,#77713,#77714,#77715,#77716,#77717,#77718,#77719,#77720,
#77721,#77722,#77723,#77724,#77725,#77726,#77727,#77728,#77729,#77730,#77731,
#77732,#77733,#77734,#77735,#77736,#77737,#77738,#77739,#77740,#77741),
 .UNSPECIFIED.,.F.,.F.,(4,2,2,2,2,2,2,2,2,2,2,2,2,2,2,2,2,2,2,2,2,2,2,2,
2,2,2,2,2,2,2,2,2,2,2,2,2,2,2,2,2,2,2,2,2,2,2,2,2,2,2,2,2,2,2,2,2,2,2,2,
2,2,2,2,2,2,2,2,2,2,2,2,2,2,2,2,2,2,4),(-1.1637686371979,-1.15330190866645,
-1.1266227046362,-1.09256064921497,-1.08738467839962,-1.08447804691533,
-1.08221855966446,-1.078997200995,-1.0720929569109,-1.04172615958735,-0.985477222491362,
-0.973796375831997,-0.968166209598214,-0.963720443538658,-0.958703261039998,
-0.950091205374077,-0.939562238885692,-0.916459677578588,-0.889953461342887,
-0.855674071252519,-0.850495008033263,-0.847587736517607,-0.845328814306583,
-0.84210950273686,-0.835213509442295,-0.804921450089816,-0.748914527944634,
-0.737014184892147,-0.731344381402372,-0.726895540281821,-0.721904410910814,
-0.713411634220441,-0.664373131981111,-0.621067249054008,-0.614391305574181,
-0.611213164706316,-0.608717662740495,-0.605671704503774,-0.599674578529323,
-0.591733080982927,-0.571582639447149,-0.524620788345343,-0.503713938265148,
-0.496545413852407,-0.491834230609183,-0.48728251741021,-0.480927115237638,
-0.464837122792203,-0.440267116686382,-0.389050830868198,-0.379089415497616,
-0.375263526244851,-0.372703238844456,-0.36999731328955,-0.365610004255846,
-0.349585865669542,-0.315288663196602,-0.272878790086403,-0.263461724321359,
-0.257718225983789,-0.253258721643605,-0.248303879589581,-0.239991273220952,
-0.19806005041918,-0.155468977463997,-0.142952258400057,-0.138787202372248,
-0.136393940808784,-0.133822998673744,-0.13006462663369,-0.119778194296598,
-0.103142576294788,-0.050478661657663,-0.0298185732069449,-0.0226922099751356,
-0.0179928562598389,-0.0137879733802478,-0.00934196527458575,-0.000699766182984735),
 .UNSPECIFIED.);
#1060=B_SPLINE_CURVE_WITH_KNOTS('',3,(#77742,#77743,#77744,#77745,#77746,
#77747,#77748,#77749,#77750,#77751,#77752,#77753,#77754,#77755,#77756,#77757,
#77758,#77759,#77760,#77761,#77762,#77763,#77764,#77765,#77766,#77767,#77768,
#77769),.UNSPECIFIED.,.F.,.F.,(4,3,3,3,3,3,3,3,3,4),(14.3150784600182,14.4937457776235,
14.6720840543341,14.8504232808183,15.0287613104912,15.2075061341743,15.2805718614365,
15.4753006968871,15.6687760212031,15.7079632676679),.UNSPECIFIED.);
#1061=B_SPLINE_CURVE_WITH_KNOTS('',3,(#77771,#77772,#77773,#77774,#77775,
#77776,#77777,#77778,#77779,#77780,#77781,#77782,#77783,#77784,#77785,#77786,
#77787,#77788,#77789,#77790,#77791,#77792,#77793,#77794,#77795,#77796,#77797,
#77798),.UNSPECIFIED.,.F.,.F.,(4,3,3,3,3,3,3,3,3,4),(14.3143563514564,14.4933094485465,
14.6035018374048,14.782517919735,14.9611833677346,15.1398304904322,15.3184547270006,
15.4974965315266,15.5996581672671,15.7079632679489),.UNSPECIFIED.);
#1062=B_SPLINE_CURVE_WITH_KNOTS('',3,(#77799,#77800,#77801,#77802,#77803,
#77804,#77805,#77806,#77807),.UNSPECIFIED.,.F.,.F.,(4,1,1,1,1,1,4),(15.7079719561269,
16.5958144971293,17.5919708269915,18.5881271568537,19.5842834867159,20.5804398165781,
20.5982114559267),.UNSPECIFIED.);
#1063=B_SPLINE_CURVE_WITH_KNOTS('',3,(#77812,#77813,#77814,#77815,#77816,
#77817,#77818,#77819,#77820,#77821,#77822,#77823,#77824,#77825,#77826,#77827,
#77828,#77829,#77830,#77831,#77832,#77833,#77834,#77835,#77836,#77837,#77838,
#77839,#77840,#77841,#77842,#77843,#77844,#77845,#77846,#77847,#77848,#77849,
#77850,#77851,#77852,#77853,#77854,#77855,#77856,#77857,#77858,#77859,#77860,
#77861,#77862,#77863,#77864,#77865,#77866,#77867,#77868,#77869,#77870,#77871,
#77872,#77873,#77874,#77875,#77876,#77877,#77878,#77879,#77880,#77881,#77882,
#77883,#77884,#77885,#77886,#77887,#77888,#77889,#77890,#77891,#77892,#77893,
#77894,#77895,#77896,#77897,#77898,#77899,#77900,#77901,#77902,#77903,#77904,
#77905,#77906,#77907,#77908,#77909,#77910,#77911,#77912,#77913,#77914,#77915,
#77916,#77917,#77918,#77919,#77920,#77921,#77922,#77923,#77924,#77925,#77926,
#77927,#77928,#77929,#77930,#77931,#77932,#77933,#77934,#77935,#77936,#77937,
#77938,#77939,#77940,#77941,#77942,#77943,#77944,#77945,#77946,#77947,#77948,
#77949,#77950,#77951,#77952,#77953,#77954,#77955,#77956,#77957,#77958,#77959,
#77960,#77961,#77962,#77963,#77964,#77965,#77966,#77967,#77968,#77969,#77970,
#77971,#77972,#77973,#77974,#77975,#77976,#77977,#77978,#77979,#77980,#77981,
#77982,#77983,#77984,#77985,#77986,#77987,#77988,#77989,#77990,#77991,#77992,
#77993,#77994,#77995,#77996,#77997,#77998,#77999,#78000,#78001,#78002,#78003,
#78004,#78005,#78006,#78007,#78008,#78009,#78010,#78011),.UNSPECIFIED.,
 .F.,.F.,(4,2,2,2,2,2,2,2,2,2,2,2,2,2,2,2,2,2,2,2,2,2,2,2,2,2,2,2,2,2,2,
2,2,2,2,2,2,2,2,2,2,2,2,2,2,2,2,2,2,2,2,2,2,2,2,2,2,2,2,2,2,2,2,2,2,2,2,
2,2,2,2,2,2,2,2,2,2,2,2,2,2,2,2,2,2,2,2,2,2,2,2,2,2,2,2,2,2,2,2,4),(-2.65808856585573,
-2.63896562788725,-2.63024927627796,-2.62521051743156,-2.62076872278231,
-2.61517461241825,-2.6062689530765,-2.5513950124766,-2.51544918010836,-2.50936210629664,
-2.50629807350984,-2.50380303304675,-2.50064471262094,-2.49407411644601,
-2.44976929489784,-2.40203764363037,-2.39331977274927,-2.38828057986316,
-2.38383866330352,-2.37824474799765,-2.36934011948885,-2.31445077379584,
-2.27851439127394,-2.27242733281257,-2.26936323959744,-2.2668681185348,
-2.26370965614897,-2.25713861298752,-2.2017312222126,-2.17077686377812,
-2.15859407969893,-2.15287242873246,-2.14841731415237,-2.14345454859754,
-2.13509748541681,-2.0951234442445,-2.05593101002078,-2.0387950323599,-2.03431776630312,
-2.03159340734376,-2.02904621173316,-2.02588911944168,-2.01787577779181,
-1.96444395966839,-1.93959584089493,-1.92857108602373,-1.91964494170661,
-1.91456171004154,-1.91012494278449,-1.90459542172365,-1.89381350566269,
-1.83664403989336,-1.80598134791393,-1.79904746452727,-1.79582076722484,
-1.79356077273059,-1.79065792279702,-1.78549903676126,-1.75436601730428,
-1.74873945594128,-1.72440702662619,-1.70150725376204,-1.68616841063085,
-1.67992413442162,-1.67539174120084,-1.67121220600676,-1.66437677015089,
-1.64621779537558,-1.59677293989029,-1.57591590069346,-1.56395836850383,
-1.55998444930628,-1.55736887806426,-1.55469837777831,-1.55046830899439,
-1.53739869282542,-1.4952686832497,-1.45374841823445,-1.44537309055035,
-1.44040618715214,-1.43595146846488,-1.43023605973783,-1.41808965995798,
-1.38854667801837,-1.37144368022104,-1.3320774905639,-1.32522592009405,
-1.32201448470216,-1.31951701519194,-1.31649796412889,-1.31063541532598,
-1.27331494399624,-1.21970325024029,-1.2106828051401,-1.20505488719733,
-1.20060947887647,-1.19559121578042,-1.18697354308848,-1.1764356290778,
-1.1637686371979),.UNSPECIFIED.);
#1064=B_SPLINE_CURVE_WITH_KNOTS('',3,(#78013,#78014,#78015,#78016,#78017),
 .UNSPECIFIED.,.F.,.F.,(4,1,4),(20.5982114559267,21.5765961464403,21.9911426690459),
 .UNSPECIFIED.);
#1065=B_SPLINE_CURVE_WITH_KNOTS('',3,(#78018,#78019,#78020,#78021,#78022,
#78023,#78024,#78025,#78026,#78027,#78028,#78029,#78030,#78031,#78032,#78033,
#78034,#78035,#78036,#78037,#78038,#78039,#78040,#78041,#78042,#78043,#78044,
#78045,#78046,#78047,#78048,#78049,#78050,#78051,#78052,#78053,#78054,#78055,
#78056,#78057,#78058,#78059,#78060,#78061,#78062,#78063,#78064,#78065,#78066,
#78067,#78068,#78069,#78070,#78071,#78072,#78073,#78074,#78075,#78076,#78077,
#78078,#78079,#78080,#78081,#78082,#78083,#78084,#78085,#78086,#78087,#78088,
#78089,#78090,#78091,#78092,#78093,#78094,#78095,#78096,#78097,#78098,#78099,
#78100,#78101,#78102,#78103,#78104,#78105,#78106,#78107,#78108,#78109,#78110,
#78111,#78112,#78113,#78114,#78115,#78116,#78117,#78118,#78119,#78120,#78121,
#78122,#78123,#78124,#78125,#78126,#78127,#78128,#78129,#78130,#78131,#78132,
#78133,#78134,#78135,#78136,#78137,#78138,#78139,#78140,#78141,#78142,#78143,
#78144,#78145,#78146,#78147,#78148,#78149,#78150,#78151,#78152,#78153,#78154,
#78155,#78156,#78157,#78158,#78159,#78160,#78161,#78162,#78163,#78164,#78165,
#78166,#78167,#78168,#78169,#78170,#78171,#78172,#78173,#78174,#78175,#78176,
#78177,#78178,#78179),.UNSPECIFIED.,.F.,.F.,(4,2,2,2,2,2,2,2,2,2,2,2,2,
2,2,2,2,2,2,2,2,2,2,2,2,2,2,2,2,2,2,2,2,2,2,2,2,2,2,2,2,2,2,2,2,2,2,2,2,
2,2,2,2,2,2,2,2,2,2,2,2,2,2,2,2,2,2,2,2,2,2,2,2,2,2,2,2,2,2,2,4),(-2.98904427612266,
-2.98271778473439,-2.97723402516263,-2.972808221092,-2.96859102543041,-2.9638636072836,
-2.95660538824093,-2.9347749884518,-2.8780081973523,-2.86484611471672,-2.85611824490066,
-2.85258738524914,-2.85005559451206,-2.84723593943615,-2.84231751051577,
-2.82084252248546,-2.77782499244362,-2.75666538903467,-2.74214902509585,
-2.73603421462947,-2.73152544592232,-2.72731801991099,-2.72032021305432,
-2.70093465123872,-2.65264122893888,-2.63211123115884,-2.62407775210138,
-2.61802862591414,-2.61497288896346,-2.61247871788276,-2.60931409623699,
-2.60270569116392,-2.55889221680947,-2.51069964266647,-2.50201121946722,
-2.49697984405979,-2.49253943310642,-2.48694023389954,-2.47541478443228,
-2.4189661619931,-2.38852972679637,-2.38162043088732,-2.3783993783485,-2.37614113267091,
-2.37323753987195,-2.36807078495652,-2.33461177733176,-2.30788095203421,
-2.28444726017468,-2.27382408444184,-2.26515242446383,-2.260124416451,-2.25568323515178,
-2.25007803662293,-2.23852146689319,-2.18210551792869,-2.15167878190711,
-2.14477021088004,-2.1415491492634,-2.13929074525505,-2.13638671022134,
-2.13121871603868,-2.0976648901883,-2.07107968066547,-2.04761151404457,
-2.03697807939041,-2.02829972680073,-2.02326999295449,-2.01882855559658,
-2.01322473389622,-2.00428263892065,-1.94016200242408,-1.92088338084325,
-1.91316033955907,-1.90729069036377,-1.90427084749759,-1.90177442137465,
-1.89856660520185,-1.89173066883819,-1.85200521610118,-1.82619474000714),
 .UNSPECIFIED.);
#1066=B_SPLINE_CURVE_WITH_KNOTS('',3,(#78185,#78186,#78187,#78188,#78189,
#78190,#78191,#78192,#78193,#78194,#78195,#78196,#78197,#78198,#78199,#78200,
#78201,#78202,#78203,#78204,#78205,#78206,#78207,#78208,#78209,#78210,#78211,
#78212,#78213,#78214,#78215,#78216,#78217,#78218,#78219,#78220,#78221,#78222,
#78223,#78224,#78225,#78226,#78227,#78228,#78229,#78230,#78231,#78232,#78233,
#78234,#78235,#78236,#78237,#78238,#78239,#78240,#78241,#78242,#78243,#78244,
#78245,#78246,#78247,#78248,#78249,#78250,#78251,#78252,#78253,#78254,#78255,
#78256,#78257,#78258,#78259,#78260,#78261,#78262,#78263,#78264,#78265,#78266,
#78267,#78268,#78269,#78270,#78271,#78272,#78273,#78274,#78275,#78276,#78277,
#78278,#78279,#78280,#78281,#78282,#78283,#78284,#78285,#78286,#78287,#78288,
#78289,#78290,#78291,#78292,#78293,#78294,#78295,#78296,#78297,#78298,#78299,
#78300,#78301,#78302,#78303,#78304,#78305,#78306,#78307,#78308,#78309,#78310,
#78311,#78312,#78313,#78314,#78315,#78316,#78317,#78318,#78319,#78320,#78321,
#78322,#78323,#78324,#78325,#78326,#78327,#78328,#78329,#78330,#78331,#78332,
#78333,#78334),.UNSPECIFIED.,.F.,.F.,(4,2,2,2,2,2,2,2,2,2,2,2,2,2,2,2,2,
2,2,2,2,2,2,2,2,2,2,2,2,2,2,2,2,2,2,2,2,2,2,2,2,2,2,2,2,2,2,2,2,2,2,2,2,
2,2,2,2,2,2,2,2,2,2,2,2,2,2,2,2,2,2,2,2,2,4),(-1.16370274550239,-1.1568070636298,
-1.13677589009422,-1.09022559976082,-1.06886026428964,-1.06164448485992,
-1.05692378948761,-1.0523786955524,-1.04605868477085,-1.03020861191811,
-1.00617866458583,-0.960418696062841,-0.945412959897615,-0.940975534683176,
-0.938259967017763,-0.935677531247388,-0.931866614661771,-0.921205588553841,
-0.903674646488405,-0.850676930739111,-0.831467699059262,-0.824489994217004,
-0.820285042041834,-0.81577164368852,-0.809637560886505,-0.795009473094288,
-0.773617630303817,-0.730663875046565,-0.709419145398833,-0.704509960324899,
-0.701691479497393,-0.69915723216955,-0.695618378437064,-0.686847962239203,
-0.673600358750618,-0.640301644144528,-0.597358254095201,-0.589007533560267,
-0.584046121250254,-0.579590717172288,-0.573866598030166,-0.561670356831813,
-0.530349090617642,-0.475447713250732,-0.468765208229255,-0.465585489510032,
-0.463089540991608,-0.460043956096899,-0.454049880629331,-0.419293719725962,
-0.362790523781181,-0.354060467579551,-0.348517507309125,-0.344079690939804,
-0.339005837902028,-0.330124410646265,-0.319169620966451,-0.29457213689166,
-0.24317543339214,-0.233373696231229,-0.229572198251925,-0.227088455460331,
-0.224467495629112,-0.220543910049425,-0.215691303369064,-0.185311480080651,
-0.129024907015343,-0.117373078218063,-0.111748538710975,-0.107303611633095,
-0.102283579199003,-0.093656951979499,-0.045572454012865,-0.0264879389893685,
-0.000696886015620926),.UNSPECIFIED.);
#1067=B_SPLINE_CURVE_WITH_KNOTS('',3,(#78335,#78336,#78337,#78338,#78339,
#78340,#78341,#78342,#78343,#78344,#78345,#78346,#78347,#78348,#78349,#78350,
#78351,#78352,#78353,#78354,#78355,#78356,#78357,#78358,#78359,#78360,#78361,
#78362,#78363,#78364,#78365,#78366,#78367,#78368,#78369,#78370,#78371,#78372,
#78373,#78374,#78375,#78376,#78377,#78378,#78379,#78380,#78381,#78382,#78383,
#78384),.UNSPECIFIED.,.F.,.F.,(4,2,2,2,2,2,2,2,2,2,2,2,2,2,2,2,2,2,2,2,
2,2,2,2,4),(-2.98929417603817,-2.98366351093371,-2.98108078519344,-2.97872868114393,
-2.97602838999981,-2.97166071400982,-2.95731736208476,-2.90550643056215,
-2.88469583141012,-2.87034731868861,-2.86425776659884,-2.85975166729322,
-2.85553532914993,-2.84849538068428,-2.82877056877828,-2.78076354833954,
-2.76031364017731,-2.7522987727458,-2.74625987964001,-2.74320552365715,
-2.74071023304375,-2.73754130231533,-2.73091460922501,-2.68712217695227,
-2.65808856585573),.UNSPECIFIED.);
#1068=B_SPLINE_CURVE_WITH_KNOTS('',3,(#78385,#78386,#78387,#78388,#78389,
#78390,#78391,#78392,#78393,#78394,#78395,#78396,#78397,#78398,#78399,#78400,
#78401,#78402,#78403,#78404,#78405,#78406,#78407,#78408,#78409,#78410,#78411,
#78412,#78413,#78414,#78415,#78416,#78417,#78418,#78419,#78420,#78421,#78422,
#78423,#78424,#78425,#78426,#78427,#78428,#78429,#78430,#78431,#78432,#78433,
#78434,#78435,#78436,#78437,#78438,#78439,#78440,#78441,#78442,#78443,#78444,
#78445,#78446,#78447,#78448,#78449,#78450,#78451,#78452,#78453,#78454,#78455,
#78456,#78457,#78458,#78459,#78460,#78461,#78462,#78463,#78464,#78465,#78466,
#78467,#78468,#78469,#78470,#78471,#78472,#78473,#78474,#78475,#78476,#78477,
#78478,#78479,#78480,#78481,#78482,#78483,#78484,#78485,#78486,#78487,#78488,
#78489,#78490,#78491,#78492,#78493,#78494,#78495,#78496,#78497,#78498,#78499,
#78500,#78501,#78502,#78503,#78504,#78505,#78506,#78507,#78508,#78509,#78510,
#78511,#78512,#78513,#78514,#78515,#78516,#78517,#78518,#78519,#78520,#78521,
#78522,#78523,#78524,#78525,#78526,#78527,#78528,#78529,#78530,#78531,#78532,
#78533,#78534,#78535,#78536,#78537,#78538,#78539,#78540,#78541,#78542,#78543,
#78544,#78545,#78546,#78547,#78548,#78549,#78550,#78551,#78552,#78553,#78554,
#78555,#78556,#78557,#78558,#78559,#78560,#78561,#78562,#78563,#78564,#78565,
#78566,#78567,#78568,#78569,#78570,#78571,#78572,#78573,#78574,#78575,#78576,
#78577,#78578,#78579,#78580,#78581,#78582,#78583,#78584,#78585,#78586,#78587,
#78588,#78589,#78590),.UNSPECIFIED.,.F.,.F.,(4,2,2,2,2,2,2,2,2,2,2,2,2,
2,2,2,2,2,2,2,2,2,2,2,2,2,2,2,2,2,2,2,2,2,2,2,2,2,2,2,2,2,2,2,2,2,2,2,2,
2,2,2,2,2,2,2,2,2,2,2,2,2,2,2,2,2,2,2,2,2,2,2,2,2,2,2,2,2,2,2,2,2,2,2,2,
2,2,2,2,2,2,2,2,2,2,2,2,2,2,2,2,2,4),(-1.82619474000714,-1.81669741450079,
-1.79650086386287,-1.789613921023,-1.78496136321705,-1.78042251728144,-1.77491811234969,
-1.76127711035731,-1.74625882417755,-1.68188711327217,-1.67211761041369,
-1.66842967734056,-1.66587063032776,-1.66311420019153,-1.65848885920151,
-1.64151002192613,-1.60225772689917,-1.56897584375519,-1.55672051941941,
-1.55098639324071,-1.54653051962872,-1.54157609445583,-1.53325563140524,
-1.49466335660825,-1.45743394032513,-1.437550799349,-1.43271462594213,-1.42991222682865,
-1.42737282286278,-1.42379962009082,-1.41480533885329,-1.40108138580043,
-1.34043394780875,-1.32244194173736,-1.31563144561288,-1.31145732217809,
-1.30692316509088,-1.30066249446532,-1.28520789385302,-1.26205154942839,
-1.2352577680559,-1.20133550613098,-1.19616217617814,-1.19325661030326,
-1.19099786028261,-1.18777748573651,-1.18087490185015,-1.15051586874477,
-1.09430007401147,-1.08258277692584,-1.07694694805024,-1.07250191359706,
-1.06749108174361,-1.0589041346484,-1.04841376525451,-1.02544119200211,
-1.00018973591792,-0.96714389852926,-0.960900215830101,-0.957762813917686,
-0.955221096582854,-0.952489029087609,-0.947974317147941,-0.930342404916655,
-0.888683926910013,-0.851675930912225,-0.843385475754152,-0.838437776911538,
-0.833981018607295,-0.828236015619667,-0.815918204719248,-0.780911992980148,
-0.738774158470005,-0.725680028827143,-0.721447940407098,-0.718777634633902,
-0.716163722646667,-0.712194629329707,-0.700269438407626,-0.679498921374576,
-0.630347434893704,-0.611914528525312,-0.605042390726706,-0.600857341912173,
-0.596331960689134,-0.590121185929433,-0.574993877641159,-0.552545240818545,
-0.525568261588957,-0.490706261849459,-0.485516419066132,-0.482607273277968,
-0.480349276223882,-0.477134579256861,-0.470261993623915,-0.440196236852249,
-0.384897242937592,-0.372356597316411,-0.366634047993919,-0.362168080016405,
-0.357259060357152,-0.349149922815078,-0.331944024529),.UNSPECIFIED.);
#1069=B_SPLINE_CURVE_WITH_KNOTS('',3,(#78595,#78596,#78597,#78598,#78599,
#78600,#78601,#78602,#78603,#78604,#78605,#78606,#78607,#78608,#78609,#78610,
#78611,#78612,#78613,#78614,#78615,#78616,#78617,#78618,#78619,#78620,#78621,
#78622,#78623,#78624,#78625,#78626,#78627,#78628,#78629,#78630,#78631,#78632,
#78633,#78634,#78635,#78636,#78637,#78638,#78639,#78640,#78641,#78642,#78643,
#78644,#78645,#78646,#78647,#78648,#78649,#78650,#78651,#78652,#78653,#78654,
#78655,#78656,#78657,#78658,#78659,#78660,#78661,#78662,#78663,#78664,#78665,
#78666,#78667,#78668,#78669,#78670,#78671,#78672,#78673,#78674,#78675,#78676,
#78677,#78678,#78679,#78680,#78681,#78682,#78683,#78684,#78685,#78686,#78687,
#78688,#78689,#78690,#78691,#78692,#78693,#78694,#78695,#78696,#78697,#78698,
#78699,#78700,#78701,#78702,#78703,#78704,#78705,#78706,#78707,#78708,#78709,
#78710,#78711,#78712,#78713,#78714,#78715,#78716,#78717,#78718,#78719,#78720,
#78721,#78722,#78723,#78724,#78725,#78726,#78727,#78728,#78729,#78730,#78731,
#78732,#78733,#78734,#78735,#78736,#78737,#78738,#78739,#78740,#78741,#78742,
#78743,#78744,#78745,#78746,#78747,#78748,#78749,#78750,#78751,#78752,#78753,
#78754,#78755,#78756,#78757,#78758,#78759,#78760,#78761,#78762,#78763,#78764,
#78765,#78766,#78767,#78768,#78769,#78770,#78771,#78772,#78773,#78774,#78775,
#78776,#78777,#78778,#78779,#78780,#78781,#78782,#78783,#78784,#78785,#78786,
#78787,#78788,#78789,#78790,#78791,#78792),.UNSPECIFIED.,.F.,.F.,(4,2,2,
2,2,2,2,2,2,2,2,2,2,2,2,2,2,2,2,2,2,2,2,2,2,2,2,2,2,2,2,2,2,2,2,2,2,2,2,
2,2,2,2,2,2,2,2,2,2,2,2,2,2,2,2,2,2,2,2,2,2,2,2,2,2,2,2,2,2,2,2,2,2,2,2,
2,2,2,2,2,2,2,2,2,2,2,2,2,2,2,2,2,2,2,2,2,2,2,4),(-2.65779610798801,-2.64562846272747,
-2.60539466897641,-2.59993510794725,-2.59699977757073,-2.59449419130625,
-2.59122688046561,-2.58387137384898,-2.52947682521431,-2.5045178668195,
-2.49346363101895,-2.48451958776003,-2.47943357363947,-2.47499861327236,
-2.46947687916789,-2.45836581710353,-2.40144586488319,-2.37086433866569,
-2.36393979188862,-2.3607154206473,-2.3584562875984,-2.35555347922215,-2.35039226412067,
-2.31812074255177,-2.31274400261798,-2.2892518720084,-2.26640335760273,
-2.25594928612956,-2.24738482600682,-2.24237868461594,-2.23793270748448,
-2.23228870337808,-2.22321002925658,-2.17029679400594,-2.13275401676145,
-2.12665282896889,-2.12358626746513,-2.12109169838593,-2.11793716643286,
-2.1113848807021,-2.06676972492304,-2.01930673296878,-2.01060593952897,
-2.00557084313888,-2.00112913862138,-1.99553093590684,-1.98661005050956,
-1.93190836177424,-1.89505724763879,-1.88944323507208,-1.88647547099182,
-1.88397380115751,-1.88075105932935,-1.87364845895274,-1.82617224122379,
-1.78178492927898,-1.77341929044655,-1.76845513984121,-1.76400104671987,
-1.75828386923519,-1.74895229982513,-1.70113421315615,-1.65903167114846,
-1.65288311093852,-1.64980701890483,-1.64731252070541,-1.6441679185956,
-1.63766814368582,-1.59197443816894,-1.57816910688654,-1.5555758876386,
-1.54037970337555,-1.53415780035787,-1.52962986346544,-1.5248794105215,
-1.51752078509346,-1.49484243099641,-1.45484019718156,-1.42066591456986,
-1.41548888453754,-1.41258223510258,-1.41032322344123,-1.40710314550051,
-1.4002036909885,-1.36987820446382,-1.31375981100097,-1.30196519050354,
-1.29631459278727,-1.29186747410937,-1.28686429341757,-1.27831569524545,
-1.22924081769557,-1.18611808435823,-1.17941967489536,-1.17623716529217,
-1.17374136543791,-1.17069882392811,-1.16471888888895,-1.16370274550239),
 .UNSPECIFIED.);
#1070=B_SPLINE_CURVE_WITH_KNOTS('',3,(#78794,#78795,#78796,#78797,#78798,
#78799,#78800,#78801,#78802,#78803,#78804,#78805,#78806,#78807,#78808,#78809,
#78810,#78811,#78812,#78813,#78814,#78815,#78816,#78817,#78818,#78819,#78820,
#78821,#78822,#78823,#78824,#78825,#78826,#78827,#78828,#78829,#78830,#78831,
#78832,#78833,#78834,#78835,#78836,#78837,#78838,#78839,#78840,#78841,#78842,
#78843),.UNSPECIFIED.,.F.,.F.,(4,2,2,2,2,2,2,2,2,2,2,2,2,2,2,2,2,2,2,2,
2,2,2,2,4),(-0.331944024529,-0.312841878134531,-0.295797672941764,-0.256356303392932,
-0.249523574006143,-0.246316348325045,-0.24381997457475,-0.240799682720564,
-0.234927739803417,-0.195081674214772,-0.144398316709289,-0.135177121109271,
-0.129492211160779,-0.125042428831186,-0.12006158181438,-0.111614647314127,
-0.10134315480156,-0.0791140033701062,-0.0287009707118166,-0.0151068306855188,
-0.0108193652246315,-0.00813703130472152,-0.00579380909874595,-0.00316163883082362,
-0.000696074731363536),.UNSPECIFIED.);
#1071=B_SPLINE_CURVE_WITH_KNOTS('',3,(#78844,#78845,#78846,#78847,#78848,
#78849,#78850,#78851,#78852,#78853,#78854,#78855,#78856,#78857,#78858,#78859,
#78860,#78861,#78862,#78863,#78864,#78865,#78866,#78867,#78868,#78869,#78870,
#78871,#78872,#78873,#78874,#78875,#78876,#78877,#78878,#78879,#78880,#78881,
#78882,#78883,#78884,#78885,#78886,#78887,#78888,#78889,#78890,#78891,#78892,
#78893,#78894,#78895,#78896,#78897,#78898,#78899,#78900,#78901,#78902,#78903,
#78904,#78905,#78906,#78907,#78908,#78909,#78910,#78911,#78912,#78913,#78914,
#78915,#78916,#78917,#78918,#78919,#78920,#78921,#78922,#78923,#78924,#78925,
#78926,#78927,#78928,#78929,#78930,#78931,#78932,#78933,#78934,#78935,#78936,
#78937,#78938,#78939,#78940,#78941,#78942,#78943,#78944,#78945,#78946,#78947,
#78948,#78949,#78950,#78951,#78952,#78953,#78954,#78955,#78956,#78957,#78958,
#78959,#78960,#78961,#78962,#78963,#78964,#78965,#78966,#78967,#78968,#78969,
#78970,#78971,#78972,#78973,#78974,#78975,#78976,#78977,#78978,#78979,#78980,
#78981,#78982,#78983,#78984,#78985,#78986,#78987,#78988,#78989,#78990,#78991,
#78992,#78993,#78994,#78995,#78996,#78997,#78998,#78999,#79000,#79001,#79002,
#79003,#79004,#79005,#79006,#79007,#79008,#79009,#79010,#79011,#79012,#79013,
#79014,#79015,#79016,#79017,#79018,#79019,#79020,#79021,#79022,#79023,#79024,
#79025,#79026,#79027,#79028,#79029,#79030,#79031,#79032,#79033,#79034,#79035,
#79036,#79037,#79038,#79039),.UNSPECIFIED.,.F.,.F.,(4,2,2,2,2,2,2,2,2,2,
2,2,2,2,2,2,2,2,2,2,2,2,2,2,2,2,2,2,2,2,2,2,2,2,2,2,2,2,2,2,2,2,2,2,2,2,
2,2,2,2,2,2,2,2,2,2,2,2,2,2,2,2,2,2,2,2,2,2,2,2,2,2,2,2,2,2,2,2,2,2,2,2,
2,2,2,2,2,2,2,2,2,2,2,2,2,2,2,4),(-2.98986290590906,-2.9811645609045,-2.93860454829328,
-2.89411772806824,-2.88536790530145,-2.8803230618328,-2.87588370936346,
-2.87030313328637,-2.86144069728388,-2.79693950862918,-2.77781347126643,
-2.77012912135672,-2.76594868825332,-2.76245881001136,-2.76241330075756,
-2.76236793090525,-2.7623226514419,-2.76227741250219,-2.76223216313041,
-2.76218685102507,-2.7621414222526,-2.76209582093373,-2.7620499889014,-2.76200386531906,
-2.76195738624712,-2.7619104841631,-2.76186308740373,-2.76181511954432,
-2.76176649867618,-2.76171713657784,-2.76166693774644,-2.76161579827013,
-2.76156360450819,-2.76151023152379,-2.76145554121485,-2.76139938008659,
-2.76134157654138,-2.76130713089662,-2.7588952078203,-2.75575019173004,
-2.74924639835194,-2.70397057987953,-2.65698912986836,-2.64833458917462,
-2.64330966533014,-2.63886715545892,-2.63325481985386,-2.62166306138798,
-2.56527676212363,-2.53485753660154,-2.52794910234861,-2.52472774225655,
-2.52246900472342,-2.51956438114988,-2.51439489299499,-2.48075844393766,
-2.45428442783653,-2.43079032625652,-2.42014887725035,-2.41146516604408,
-2.40643384957864,-2.40199191514795,-2.3963886777886,-2.38484700688701,
-2.32839887375958,-2.29795931995531,-2.29104856636941,-2.28782664159736,
-2.2855677078503,-2.28266311284791,-2.2774942984965,-2.24396712553781,-2.21694798800437,
-2.18885651097065,-2.17675251197165,-2.17104566766734,-2.1665928882549,
-2.16162330150009,-2.1532316396023,-2.10914264085504,-2.07326352521092,
-2.05686094880649,-2.05244370148903,-2.04973277551116,-2.0471784146474,
-2.04337912651513,-2.03358852798327,-1.98220305753126,-1.95761568076255,
-1.94151656959651,-1.93516060948433,-1.93060946631103,-1.92589974097122,
-1.91873524137024,-1.89786176046146,-1.85083914353397,-1.83066715315173,
-1.82676239401596),.UNSPECIFIED.);
#1072=B_SPLINE_CURVE_WITH_KNOTS('',3,(#79045,#79046,#79047,#79048,#79049,
#79050,#79051,#79052,#79053,#79054,#79055,#79056,#79057,#79058,#79059,#79060,
#79061,#79062,#79063,#79064,#79065,#79066,#79067,#79068,#79069,#79070,#79071,
#79072,#79073,#79074,#79075,#79076,#79077,#79078,#79079,#79080,#79081,#79082,
#79083,#79084,#79085,#79086,#79087,#79088,#79089,#79090,#79091,#79092,#79093,
#79094,#79095,#79096,#79097,#79098,#79099,#79100,#79101,#79102,#79103,#79104,
#79105,#79106,#79107,#79108,#79109,#79110,#79111,#79112,#79113,#79114,#79115,
#79116,#79117,#79118,#79119,#79120,#79121,#79122,#79123,#79124,#79125,#79126,
#79127,#79128,#79129,#79130,#79131,#79132,#79133,#79134,#79135,#79136,#79137,
#79138,#79139,#79140,#79141,#79142,#79143,#79144,#79145,#79146,#79147,#79148,
#79149,#79150,#79151,#79152,#79153,#79154,#79155,#79156,#79157,#79158,#79159,
#79160,#79161,#79162,#79163,#79164,#79165,#79166,#79167,#79168,#79169,#79170,
#79171,#79172,#79173,#79174,#79175,#79176,#79177,#79178,#79179,#79180,#79181,
#79182,#79183,#79184,#79185,#79186,#79187,#79188,#79189,#79190,#79191,#79192,
#79193,#79194,#79195,#79196,#79197,#79198,#79199,#79200),.UNSPECIFIED.,
 .F.,.F.,(4,2,2,2,2,2,2,2,2,2,2,2,2,2,2,2,2,2,2,2,2,2,2,2,2,2,2,2,2,2,2,
2,2,2,2,2,2,2,2,2,2,2,2,2,2,2,2,2,2,2,2,2,2,2,2,2,2,2,2,2,2,2,2,2,2,2,2,
2,2,2,2,2,2,2,2,2,2,4),(-1.16379924314915,-1.15636896341719,-1.15072066708933,
-1.14627242167782,-1.14126489131265,-1.13270105731949,-1.122248306252,-1.09940987025486,
-1.07662727515485,-1.04094595192493,-1.0339798750836,-1.03074690518291,
-1.02824774255948,-1.02524482100174,-1.01946304593492,-1.01189225967026,
-0.993214480620849,-0.930428876149755,-0.919137758977803,-0.91358027292429,
-0.909140699661688,-0.904075522018791,-0.89523755988362,-0.848586864867644,
-0.803271713780177,-0.796745700141823,-0.79359547923121,-0.791100113886125,
-0.788027371158756,-0.781898592007223,-0.741786031843394,-0.691828023119278,
-0.68256938397034,-0.676872150100689,-0.672419035246775,-0.667440953377183,
-0.659014738978724,-0.610846558273101,-0.566350925816522,-0.559786690543437,
-0.556629115506364,-0.554133508653195,-0.551067343783175,-0.544971869070915,
-0.508097090812731,-0.45439106830036,-0.445377150286841,-0.43975067632214,
-0.43530481552055,-0.430284357372875,-0.421658607396983,-0.411108472381106,
-0.387934685436907,-0.361082605444902,-0.327237667455879,-0.32206376080669,
-0.319157366076106,-0.31689761785202,-0.31367527182871,-0.306766223562171,
-0.276355430680164,-0.220041575978518,-0.208419630605263,-0.202800111613543,
-0.198355065547207,-0.193585482945275,-0.185515120101929,-0.175629661124755,
-0.15468558629736,-0.126343850363146,-0.0930276647544607,-0.0861036582085444,
-0.0828786447279151,-0.0803802108174482,-0.0773715980702051,-0.0715610444402044,
-0.0639408967511788,-0.000697042157991375),.UNSPECIFIED.);
#1073=B_SPLINE_CURVE_WITH_KNOTS('',3,(#79201,#79202,#79203,#79204,#79205,
#79206,#79207,#79208,#79209,#79210,#79211,#79212,#79213,#79214,#79215,#79216,
#79217,#79218,#79219,#79220,#79221,#79222,#79223,#79224,#79225,#79226,#79227,
#79228,#79229,#79230,#79231,#79232,#79233,#79234,#79235,#79236,#79237,#79238,
#79239,#79240,#79241,#79242,#79243,#79244,#79245,#79246,#79247,#79248),
 .UNSPECIFIED.,.F.,.F.,(4,2,2,2,2,2,2,2,2,2,2,2,2,2,2,2,2,2,2,2,2,2,2,4),
(-2.98915910611891,-2.97245947833514,-2.96192457934277,-2.95701634474704,
-2.95285674097329,-2.94840886300484,-2.94274081448435,-2.93357753277321,
-2.90038509321121,-2.85100678772585,-2.84310478890941,-2.83713139739069,
-2.83409067085517,-2.83159548951468,-2.82841268419511,-2.82170994269704,
-2.77869299185966,-2.72942034717541,-2.72097004287315,-2.71598853099697,
-2.71153890583765,-2.70585519559141,-2.69663786776816,-2.65779610798801),
 .UNSPECIFIED.);
#1074=B_SPLINE_CURVE_WITH_KNOTS('',3,(#79249,#79250,#79251,#79252,#79253,
#79254,#79255,#79256,#79257,#79258,#79259,#79260,#79261,#79262,#79263,#79264,
#79265,#79266,#79267,#79268,#79269,#79270,#79271,#79272,#79273,#79274,#79275,
#79276,#79277,#79278,#79279,#79280,#79281,#79282,#79283,#79284,#79285,#79286,
#79287,#79288,#79289,#79290,#79291,#79292,#79293,#79294,#79295,#79296,#79297,
#79298,#79299,#79300,#79301,#79302,#79303,#79304,#79305,#79306,#79307,#79308,
#79309,#79310,#79311,#79312,#79313,#79314,#79315,#79316,#79317,#79318,#79319,
#79320,#79321,#79322,#79323,#79324,#79325,#79326,#79327,#79328,#79329,#79330,
#79331,#79332,#79333,#79334,#79335,#79336,#79337,#79338,#79339,#79340,#79341,
#79342,#79343,#79344,#79345,#79346,#79347,#79348,#79349,#79350,#79351,#79352,
#79353,#79354,#79355,#79356,#79357,#79358,#79359,#79360,#79361,#79362,#79363,
#79364,#79365,#79366,#79367,#79368,#79369,#79370,#79371,#79372,#79373,#79374,
#79375,#79376,#79377,#79378,#79379,#79380,#79381,#79382,#79383,#79384,#79385,
#79386,#79387,#79388,#79389,#79390,#79391,#79392,#79393,#79394,#79395,#79396,
#79397,#79398,#79399,#79400,#79401,#79402,#79403,#79404,#79405,#79406,#79407,
#79408,#79409,#79410,#79411,#79412,#79413,#79414,#79415,#79416,#79417,#79418,
#79419,#79420,#79421,#79422,#79423,#79424,#79425,#79426,#79427,#79428,#79429,
#79430,#79431,#79432,#79433,#79434,#79435,#79436,#79437,#79438,#79439,#79440,
#79441,#79442,#79443,#79444,#79445,#79446),.UNSPECIFIED.,.F.,.F.,(4,2,2,
2,2,2,2,2,2,2,2,2,2,2,2,2,2,2,2,2,2,2,2,2,2,2,2,2,2,2,2,2,2,2,2,2,2,2,2,
2,2,2,2,2,2,2,2,2,2,2,2,2,2,2,2,2,2,2,2,2,2,2,2,2,2,2,2,2,2,2,2,2,2,2,2,
2,2,2,2,2,2,2,2,2,2,2,2,2,2,2,2,2,2,2,2,2,2,2,4),(-1.82676239401596,-1.82272046736094,
-1.81672091864089,-1.81367460450555,-1.81117924027603,-1.80800188504408,
-1.8013298649085,-1.7580267840685,-1.70924301533283,-1.70062747953582,-1.69561033741196,
-1.69116586736496,-1.68553910548193,-1.67652046621759,-1.61274221472753,
-1.59331247162085,-1.58189494164362,-1.57798706850257,-1.57538545123259,
-1.57269840983678,-1.56839104192817,-1.55463061891724,-1.4955156127764,
-1.47041984850611,-1.46275451371483,-1.45793950490291,-1.45344188485792,
-1.44740446573964,-1.43337791652622,-1.413220985141,-1.38407955151575,-1.38005003406147,
-1.34749079807617,-1.34232668583597,-1.33942307286952,-1.33716382487661,
-1.33394011285789,-1.32702015150965,-1.29649124919368,-1.23973617586962,
-1.22848682257969,-1.22293841141856,-1.21850097949893,-1.21343274810444,
-1.20457502187683,-1.15733511690643,-1.11269733616998,-1.10614179980468,
-1.10298658428462,-1.10049195548535,-1.09742599605467,-1.09132813154709,
-1.05408312357184,-1.00082882547132,-0.99177827370505,-0.986142248348315,
-0.981696912608493,-0.976685587035129,-0.968097401569503,-0.957605304200283,
-0.934627738823065,-0.909330944315578,-0.876330208293993,-0.869413873939793,
-0.866190919756722,-0.863693398680025,-0.860685152702294,-0.854873429719196,
-0.847250648331001,-0.82836692863714,-0.763302226245086,-0.754566639982387,
-0.749022920635514,-0.744586250510679,-0.739515645666495,-0.730645165239772,
-0.683031336154004,-0.638842550674269,-0.632260667672222,-0.629100609290637,
-0.626606077557796,-0.623545066603632,-0.617471143539917,-0.582497314957043,
-0.526431192927454,-0.517653839910276,-0.512097855466582,-0.50766019084905,
-0.502597991192227,-0.493767450989743,-0.447247709854124,-0.401792231986257,
-0.395275352028411,-0.39212771591288,-0.389633504948396,-0.386561177872874,
-0.380430377273958,-0.339941241296865,-0.332197600308329),.UNSPECIFIED.);
#1075=B_SPLINE_CURVE_WITH_KNOTS('',3,(#79451,#79452,#79453,#79454,#79455,
#79456,#79457,#79458,#79459,#79460,#79461,#79462,#79463,#79464,#79465,#79466,
#79467,#79468,#79469,#79470,#79471,#79472,#79473,#79474,#79475,#79476,#79477,
#79478,#79479,#79480,#79481,#79482,#79483,#79484,#79485,#79486,#79487,#79488,
#79489,#79490,#79491,#79492,#79493,#79494,#79495,#79496,#79497,#79498,#79499,
#79500,#79501,#79502,#79503,#79504,#79505,#79506,#79507,#79508,#79509,#79510,
#79511,#79512,#79513,#79514,#79515,#79516,#79517,#79518,#79519,#79520,#79521,
#79522,#79523,#79524,#79525,#79526,#79527,#79528,#79529,#79530,#79531,#79532,
#79533,#79534,#79535,#79536,#79537,#79538,#79539,#79540,#79541,#79542,#79543,
#79544,#79545,#79546,#79547,#79548,#79549,#79550,#79551,#79552,#79553,#79554,
#79555,#79556,#79557,#79558,#79559,#79560,#79561,#79562,#79563,#79564,#79565,
#79566,#79567,#79568,#79569,#79570,#79571,#79572,#79573,#79574,#79575,#79576,
#79577,#79578,#79579,#79580,#79581,#79582,#79583,#79584,#79585,#79586,#79587,
#79588,#79589,#79590,#79591,#79592,#79593,#79594,#79595,#79596,#79597,#79598,
#79599,#79600,#79601,#79602,#79603,#79604,#79605,#79606,#79607,#79608,#79609,
#79610,#79611,#79612,#79613,#79614,#79615,#79616,#79617,#79618,#79619,#79620,
#79621,#79622,#79623,#79624,#79625,#79626,#79627,#79628,#79629,#79630,#79631,
#79632,#79633,#79634,#79635,#79636,#79637,#79638,#79639,#79640),
 .UNSPECIFIED.,.F.,.F.,(4,2,2,2,2,2,2,2,2,2,2,2,2,2,2,2,2,2,2,2,2,2,2,2,
2,2,2,2,2,2,2,2,2,2,2,2,2,2,2,2,2,2,2,2,2,2,2,2,2,2,2,2,2,2,2,2,2,2,2,2,
2,2,2,2,2,2,2,2,2,2,2,2,2,2,2,2,2,2,2,2,2,2,2,2,2,2,2,2,2,2,2,2,2,2,4),
(-2.65859608544945,-2.62817910170511,-2.58437028368493,-2.57601440365146,
-2.571051323549,-2.56659528312859,-2.5608715489283,-2.55152047038777,-2.49369700679251,
-2.46283216116232,-2.45587742894055,-2.45264657005837,-2.45038579877802,
-2.44748496724804,-2.44233627240993,-2.41233954330086,-2.40526107340166,
-2.38119073015443,-2.3583020538318,-2.347834471791,-2.33926050119821,-2.33425083955854,
-2.32980295714294,-2.32415819594495,-2.31508180698964,-2.25156923357792,
-2.23202522553656,-2.22056246588569,-2.2166479852476,-2.21404426909698,
-2.21135738552999,-2.20705406924471,-2.19334050291578,-2.15169049035824,
-2.11696751793303,-2.10465790537969,-2.09891227863287,-2.09445312207183,
-2.08950077478548,-2.08119764972497,-2.04378958095283,-1.99125956410559,
-1.98265868956199,-1.97914565951749,-1.97661460206172,-1.97378222075131,
-1.96881201920436,-1.94630493608452,-1.88114589965967,-1.86800701449476,
-1.86211633147386,-1.85763872917848,-1.85275879231972,-1.84479471115785,
-1.81479636460211,-1.76670608254294,-1.74793815324269,-1.74333865183246,
-1.740587009559,-1.73805288610591,-1.73495088315162,-1.72885517867193,-1.68626225621433,
-1.6425125587349,-1.63048752591444,-1.62479329641393,-1.62033998404953,
-1.61535904853054,-1.60692146675987,-1.564779200056,-1.53311180376467,-1.51841426851518,
-1.50897317785005,-1.5053318262702,-1.50278007777218,-1.50000379410264,
-1.49529141098926,-1.47479374619411,-1.41286016526844,-1.3959282015441,
-1.389271789414,-1.38512366001183,-1.38056335713426,-1.37416400039939,-1.35777411797176,
-1.33252148097241,-1.27740740931621,-1.27076402206258,-1.26759127004963,
-1.26509504021232,-1.26204205650427,-1.25601317382717,-1.21827261936714,
-1.16545743281103,-1.16379924314915),.UNSPECIFIED.);
#1076=B_SPLINE_CURVE_WITH_KNOTS('',3,(#79642,#79643,#79644,#79645,#79646,
#79647,#79648,#79649,#79650,#79651,#79652,#79653,#79654,#79655,#79656,#79657,
#79658,#79659,#79660,#79661,#79662,#79663,#79664,#79665,#79666,#79667,#79668,
#79669,#79670,#79671,#79672,#79673,#79674,#79675,#79676,#79677,#79678,#79679,
#79680,#79681,#79682,#79683,#79684,#79685,#79686,#79687),.UNSPECIFIED.,
 .F.,.F.,(4,2,2,2,2,2,2,2,2,2,2,2,2,2,2,2,2,2,2,2,2,2,4),(-0.332197600308329,
-0.290459994424418,-0.281158016782542,-0.275449637666639,-0.270996994379766,
-0.266028932018693,-0.257643229512439,-0.21223658910391,-0.164557803963349,
-0.158226854367379,-0.155115112347663,-0.152621276036858,-0.149514409956841,
-0.143208445307593,-0.134725934841315,-0.0826658288797491,-0.0497946970644482,
-0.0415948920940171,-0.0366663182927132,-0.0323511497472415,-0.0280322450478533,
-0.0224655565253524,-0.000695812465232673),.UNSPECIFIED.);
#1077=B_SPLINE_CURVE_WITH_KNOTS('',3,(#79688,#79689,#79690,#79691,#79692,
#79693,#79694,#79695,#79696,#79697,#79698,#79699,#79700,#79701,#79702,#79703,
#79704,#79705,#79706,#79707,#79708,#79709,#79710,#79711,#79712,#79713,#79714,
#79715,#79716,#79717,#79718,#79719,#79720,#79721,#79722,#79723,#79724,#79725,
#79726,#79727,#79728,#79729,#79730,#79731,#79732,#79733,#79734,#79735,#79736,
#79737,#79738,#79739,#79740,#79741,#79742,#79743,#79744,#79745,#79746,#79747,
#79748,#79749,#79750,#79751,#79752,#79753,#79754,#79755,#79756,#79757,#79758,
#79759,#79760,#79761,#79762,#79763,#79764,#79765,#79766,#79767,#79768,#79769,
#79770,#79771,#79772,#79773,#79774,#79775),.UNSPECIFIED.,.F.,.F.,(4,3,3,
3,3,3,3,3,3,3,3,3,3,3,3,3,3,3,3,3,3,3,3,3,3,3,3,3,3,4),(47.1238898042296,
47.3286926477564,47.4766607228577,47.6553657376643,47.8337102124053,48.0120264379798,
48.1903137393774,48.3690157785142,48.4728170527199,48.6515220675267,48.8298665422679,
49.0081827678426,49.1864700692404,49.3651721083774,49.4689733825821,49.647678397389,
49.8260228721303,50.004339097705,50.1826263991029,50.36132843824,50.4651297124443,
50.6438347272511,50.8221792019923,51.0004954275669,51.1787827289647,51.3574847681017,
51.4612860423065,51.6399881173827,51.8269247910562,52.0138614647296),
 .UNSPECIFIED.);
#1078=B_SPLINE_CURVE_WITH_KNOTS('',3,(#79781,#79782,#79783,#79784,#79785,
#79786,#79787,#79788,#79789,#79790,#79791,#79792,#79793,#79794,#79795,#79796,
#79797,#79798,#79799,#79800,#79801,#79802,#79803,#79804,#79805,#79806,#79807,
#79808,#79809,#79810,#79811,#79812,#79813,#79814,#79815,#79816,#79817,#79818,
#79819,#79820,#79821,#79822,#79823,#79824,#79825,#79826,#79827,#79828,#79829,
#79830,#79831,#79832,#79833,#79834,#79835,#79836,#79837,#79838,#79839,#79840,
#79841,#79842,#79843,#79844,#79845,#79846,#79847,#79848,#79849,#79850,#79851,
#79852,#79853,#79854,#79855,#79856,#79857,#79858,#79859,#79860,#79861,#79862,
#79863,#79864,#79865,#79866,#79867,#79868,#79869,#79870,#79871,#79872,#79873,
#79874,#79875,#79876,#79877,#79878,#79879,#79880,#79881,#79882,#79883,#79884,
#79885,#79886,#79887,#79888,#79889,#79890,#79891,#79892,#79893,#79894,#79895,
#79896,#79897,#79898,#79899,#79900,#79901,#79902,#79903,#79904,#79905,#79906,
#79907,#79908,#79909,#79910,#79911,#79912,#79913,#79914,#79915,#79916,#79917,
#79918,#79919,#79920,#79921,#79922,#79923,#79924,#79925,#79926,#79927,#79928,
#79929,#79930,#79931,#79932,#79933,#79934,#79935,#79936),.UNSPECIFIED.,
 .F.,.F.,(4,2,2,2,2,2,2,2,2,2,2,2,2,2,2,2,2,2,2,2,2,2,2,2,2,2,2,2,2,2,2,
2,2,2,2,2,2,2,2,2,2,2,2,2,2,2,2,2,2,2,2,2,2,2,2,2,2,2,2,2,2,2,2,2,2,2,2,
2,2,2,2,2,2,2,2,2,2,4),(-1.16393257116699,-1.13155274745225,-1.12508806491967,
-1.12194991398079,-1.11945515879177,-1.11637208757233,-1.11018972849946,
-1.10192554845814,-1.08044126644041,-1.02872142490933,-1.01297389570421,
-1.0065022436161,-1.00197480216914,-0.99730401055951,-0.990332310858646,
-0.96940172797567,-0.931778065923655,-0.89532455660756,-0.888423995035991,
-0.885203506784727,-0.882705566670822,-0.879693897099228,-0.873867475291317,
-0.86621997042688,-0.847241099589446,-0.782427276276276,-0.773638560814754,
-0.768078550296022,-0.763639584726894,-0.758577934423205,-0.749753602736751,
-0.703428419713985,-0.657754162968758,-0.651249509549554,-0.648103773210307,
-0.645609003600592,-0.642533342645965,-0.636387935069918,-0.594544566656325,
-0.546486952813495,-0.537163651934748,-0.531448438119805,-0.526994087816146,
-0.522027811896464,-0.513654114227301,-0.468960984030539,-0.420395221834905,
-0.41416299930872,-0.411070136488645,-0.408575570263599,-0.405447822538307,
-0.399036818154827,-0.363229375887451,-0.308855308108324,-0.299906966489975,
-0.294300145689517,-0.289856880380281,-0.284825625308487,-0.276146012998223,
-0.26551053925916,-0.242038703259375,-0.196888389307316,-0.180593129937533,
-0.176038425688853,-0.173297083493113,-0.170729374605992,-0.166996425831666,
-0.15738313407824,-0.130095110759329,-0.0901850250516212,-0.0672920231607177,
-0.059911131319319,-0.0551555669674362,-0.0506293516416139,-0.0461590020233244,
-0.0401480748676892,-0.0268826235989323,-0.00069612616442647),
 .UNSPECIFIED.);
#1079=B_SPLINE_CURVE_WITH_KNOTS('',3,(#79937,#79938,#79939,#79940,#79941,
#79942,#79943,#79944,#79945,#79946,#79947,#79948,#79949,#79950,#79951,#79952,
#79953,#79954,#79955,#79956,#79957,#79958,#79959,#79960,#79961,#79962,#79963,
#79964,#79965,#79966,#79967,#79968,#79969,#79970,#79971,#79972,#79973,#79974,
#79975,#79976,#79977,#79978,#79979,#79980,#79981,#79982,#79983,#79984,#79985,
#79986,#79987,#79988,#79989,#79990,#79991,#79992,#79993,#79994,#79995,#79996,
#79997,#79998,#79999,#80000,#80001,#80002,#80003,#80004,#80005,#80006,#80007,
#80008,#80009,#80010,#80011,#80012),.UNSPECIFIED.,.F.,.F.,(4,2,2,2,2,2,
2,2,2,2,2,2,2,2,2,2,2,2,2,2,2,2,2,2,2,2,2,2,2,2,2,2,2,2,2,2,2,4),(-2.98974118664277,
-2.9416975746077,-2.93336580449747,-2.92978943526336,-2.92656213697401,
-2.92430195639035,-2.921399211717,-2.91624122597365,-2.88532156037506,-2.84760447046011,
-2.82915334249667,-2.81608733299606,-2.81111829359434,-2.8109105208265,
-2.81069964473556,-2.81063190304778,-2.81055390944443,-2.81046354560391,
-2.81035807252723,-2.81023387906299,-2.81008609442015,-2.80990796855895,
-2.80968983646161,-2.80941729046844,-2.80906772872268,-2.80853924051187,
-2.80410704328531,-2.79865537218159,-2.79023542997861,-2.7311467053471,
-2.70772846347949,-2.69486040900539,-2.69078207162925,-2.68814425328089,
-2.68581230526217,-2.68259562236814,-2.6743501568114,-2.65859608544945),
 .UNSPECIFIED.);
#1080=B_SPLINE_CURVE_WITH_KNOTS('',3,(#80014,#80015,#80016,#80017,#80018,
#80019,#80020,#80021,#80022,#80023,#80024,#80025,#80026,#80027,#80028,#80029,
#80030,#80031,#80032,#80033,#80034,#80035,#80036,#80037,#80038,#80039,#80040,
#80041),.UNSPECIFIED.,.F.,.F.,(4,3,3,3,3,3,3,3,3,4),(52.0138614647296,52.1921543062006,
52.3708570227255,52.4574423721687,52.6348644963006,52.8119290116488,52.9889615116405,
53.1659777362677,53.3433764698701,53.4070747282947),.UNSPECIFIED.);
#1081=B_SPLINE_CURVE_WITH_KNOTS('',3,(#80042,#80043,#80044,#80045,#80046,
#80047,#80048,#80049,#80050),.UNSPECIFIED.,.F.,.F.,(4,1,1,1,1,1,4),(53.4070751110264,
53.4535987020309,54.4497550318931,55.4459113617553,56.4420676916176,57.4382240214798,
58.2964842709159),.UNSPECIFIED.);
#1082=B_SPLINE_CURVE_WITH_KNOTS('',3,(#80055,#80056,#80057,#80058,#80059,
#80060,#80061,#80062,#80063,#80064,#80065,#80066,#80067,#80068,#80069,#80070,
#80071,#80072,#80073,#80074,#80075,#80076,#80077,#80078,#80079,#80080,#80081,
#80082,#80083,#80084,#80085,#80086,#80087,#80088,#80089,#80090,#80091,#80092,
#80093,#80094,#80095,#80096,#80097,#80098,#80099,#80100,#80101,#80102,#80103,
#80104,#80105,#80106,#80107,#80108,#80109,#80110,#80111,#80112,#80113,#80114,
#80115,#80116,#80117,#80118,#80119,#80120,#80121,#80122,#80123,#80124,#80125,
#80126,#80127,#80128,#80129,#80130,#80131,#80132,#80133,#80134,#80135,#80136,
#80137,#80138,#80139,#80140,#80141,#80142,#80143,#80144,#80145,#80146,#80147,
#80148,#80149,#80150,#80151,#80152,#80153,#80154,#80155,#80156,#80157,#80158,
#80159,#80160,#80161,#80162,#80163,#80164,#80165,#80166,#80167,#80168,#80169,
#80170,#80171,#80172,#80173,#80174,#80175,#80176,#80177,#80178,#80179,#80180,
#80181,#80182,#80183,#80184,#80185,#80186,#80187,#80188,#80189,#80190,#80191,
#80192,#80193,#80194,#80195,#80196,#80197,#80198,#80199,#80200,#80201,#80202,
#80203,#80204,#80205,#80206,#80207,#80208,#80209,#80210,#80211,#80212,#80213,
#80214,#80215,#80216,#80217,#80218,#80219,#80220,#80221,#80222,#80223,#80224,
#80225,#80226,#80227,#80228,#80229,#80230,#80231,#80232,#80233,#80234,#80235,
#80236,#80237,#80238,#80239,#80240,#80241,#80242,#80243,#80244,#80245,#80246),
 .UNSPECIFIED.,.F.,.F.,(4,2,2,2,2,2,2,2,2,2,2,2,2,2,2,2,2,2,2,2,2,2,2,2,
2,2,2,2,2,2,2,2,2,2,2,2,2,2,2,2,2,2,2,2,2,2,2,2,2,2,2,2,2,2,2,2,2,2,2,2,
2,2,2,2,2,2,2,2,2,2,2,2,2,2,2,2,2,2,2,2,2,2,2,2,2,2,2,2,2,2,2,2,2,2,2,4),
(-2.65812282560335,-2.65609699128128,-2.64955229356263,-2.63339689211074,
-2.58207407150936,-2.56069569338651,-2.55245727120162,-2.54629043259187,
-2.54321084446186,-2.54071658851728,-2.53757615897018,-2.53109744581758,
-2.48509912782643,-2.43835965870025,-2.42995458367584,-2.42498218460008,
-2.42052997378903,-2.41482810673074,-2.40554937263751,-2.35612514627718,
-2.31506274394733,-2.30920697324126,-2.30618966912741,-2.30369261021286,
-2.30048039587027,-2.29362251326402,-2.25497219199909,-2.23716803001726,
-2.21304675727553,-2.1971548306507,-2.19082894486108,-2.18628297735503,
-2.18156429881501,-2.1743574920879,-2.15307812928642,-2.10642116379529,
-2.08635600590746,-2.07843585955492,-2.07245165207644,-2.0694083257875,
-2.06691265799576,-2.06373132326798,-2.05703873172475,-2.01391759173219,
-1.96467170210203,-1.95623993787477,-1.95126162790353,-1.94681015305105,
-1.94111757200194,-1.9318718907078,-1.88162993264105,-1.84175288919916,
-1.83562701974959,-1.83255536611484,-1.83006067600227,-1.82691105577105,
-1.82038544458358,-1.77515741683054,-1.76093619671953,-1.72696074534334,
-1.71896295912128,-1.714076913027,-1.70960311978179,-1.70383039747025,-1.69100500895248,
-1.63598476414788,-1.60600401440032,-1.59913947131505,-1.59592577583619,
-1.59366741375037,-1.59075613963496,-1.58555880492903,-1.55044120753398,
-1.5099349408516,-1.49535496976521,-1.4844335683876,-1.47887576359204,-1.47443686612957,
-1.46937346486588,-1.46054125620643,-1.41401142198338,-1.36857378073382,
-1.36205553265905,-1.35890713458109,-1.35641223781902,-1.35333886831204,
-1.34720528298511,-1.30652825722033,-1.25720599546436,-1.24792404146539,
-1.24222062929442,-1.23776750125297,-1.23279437272048,-1.22438884000068,
-1.17781105905313,-1.16393257116699),.UNSPECIFIED.);
#1083=B_SPLINE_CURVE_WITH_KNOTS('',3,(#80248,#80249,#80250,#80251,#80252,
#80253),.UNSPECIFIED.,.F.,.F.,(4,1,1,4),(58.2964842709159,58.434380351342,
59.4305366812042,59.6902579129782),.UNSPECIFIED.);
#1084=B_SPLINE_CURVE_WITH_KNOTS('',3,(#80254,#80255,#80256,#80257,#80258,
#80259,#80260,#80261,#80262,#80263,#80264,#80265,#80266,#80267,#80268,#80269,
#80270,#80271,#80272,#80273,#80274,#80275,#80276,#80277,#80278,#80279,#80280,
#80281,#80282,#80283,#80284,#80285,#80286,#80287,#80288,#80289,#80290,#80291,
#80292,#80293,#80294,#80295,#80296,#80297,#80298,#80299,#80300,#80301,#80302,
#80303,#80304,#80305,#80306,#80307,#80308,#80309,#80310,#80311,#80312,#80313,
#80314,#80315,#80316,#80317,#80318,#80319,#80320,#80321,#80322,#80323,#80324,
#80325,#80326,#80327,#80328,#80329,#80330,#80331,#80332,#80333,#80334,#80335,
#80336,#80337,#80338,#80339,#80340,#80341,#80342,#80343,#80344,#80345,#80346,
#80347,#80348,#80349,#80350,#80351,#80352,#80353,#80354,#80355,#80356,#80357,
#80358,#80359,#80360,#80361,#80362,#80363,#80364,#80365,#80366,#80367,#80368,
#80369,#80370,#80371,#80372,#80373,#80374,#80375,#80376,#80377,#80378,#80379,
#80380,#80381,#80382,#80383,#80384,#80385,#80386,#80387,#80388,#80389,#80390,
#80391,#80392,#80393,#80394,#80395,#80396,#80397,#80398,#80399,#80400,#80401,
#80402,#80403,#80404,#80405,#80406,#80407,#80408,#80409,#80410,#80411,#80412,
#80413),.UNSPECIFIED.,.F.,.F.,(4,2,2,2,2,2,2,2,2,2,2,2,2,2,2,2,2,2,2,2,
2,2,2,2,2,2,2,2,2,2,2,2,2,2,2,2,2,2,2,2,2,2,2,2,2,2,2,2,2,2,2,2,2,2,2,2,
2,2,2,2,2,2,2,2,2,2,2,2,2,2,2,2,2,2,2,2,2,2,2,4),(-2.98927830252312,-2.96007703371949,
-2.94627172720157,-2.94043632582468,-2.93602942806353,-2.93153805841539,
-2.92671432558015,-2.91900124319429,-2.89258098671331,-2.84704520996693,
-2.82333748062794,-2.81803075287548,-2.81502772865095,-2.81253080016714,
-2.80930383533054,-2.80260575670843,-2.76173416207959,-2.72719450521302,
-2.70725443875293,-2.70039854341351,-2.69575307636219,-2.69121058733973,
-2.68568869997879,-2.6719730477799,-2.60595704463375,-2.59189767154082,
-2.58274940190906,-2.57915338819893,-2.57661080786696,-2.57381939323942,
-2.56903149346558,-2.54976264042986,-2.54549026530621,-2.47961753095012,
-2.46747261778621,-2.46175968744556,-2.45730764938475,-2.45234453173439,
-2.44397768525016,-2.40087635545215,-2.36421314368282,-2.34763317326389,
-2.34320235560184,-2.34048911236113,-2.33793773003614,-2.33415050794017,
-2.32442998449772,-2.27298913602557,-2.24840100875826,-2.23745049704346,
-2.22857202021463,-2.2235005399539,-2.21906521324565,-2.21352594924394,
-2.20231873073976,-2.14550632849385,-2.11495651631871,-2.10803575456699,
-2.10481253480691,-2.10255399373007,-2.09965173184545,-2.09449111839401,
-2.0622021565422,-2.0579190497288,-2.02874782315065,-2.00865073859859,-1.99465383451477,
-1.98862248674134,-1.98412693369933,-1.97931182704577,-1.9716413137151,
-1.9459971387455,-1.8819292548182,-1.87228165100106,-1.86861162301658,-1.86605609540221,
-1.86329368678732,-1.85863965119246,-1.84129763632644,-1.8262871493728),
 .UNSPECIFIED.);
#1085=B_SPLINE_CURVE_WITH_KNOTS('',3,(#80419,#80420,#80421,#80422,#80423,
#80424,#80425,#80426,#80427,#80428,#80429,#80430,#80431,#80432,#80433,#80434,
#80435,#80436,#80437,#80438,#80439,#80440,#80441,#80442,#80443,#80444,#80445,
#80446,#80447,#80448,#80449,#80450,#80451,#80452,#80453,#80454,#80455,#80456,
#80457,#80458,#80459,#80460,#80461,#80462,#80463,#80464,#80465,#80466,#80467,
#80468,#80469,#80470,#80471,#80472,#80473,#80474,#80475,#80476,#80477,#80478,
#80479,#80480,#80481,#80482,#80483,#80484,#80485,#80486,#80487,#80488,#80489,
#80490,#80491,#80492,#80493,#80494,#80495,#80496,#80497,#80498,#80499,#80500,
#80501,#80502,#80503,#80504,#80505,#80506,#80507,#80508,#80509,#80510,#80511,
#80512,#80513,#80514,#80515,#80516,#80517,#80518,#80519,#80520,#80521,#80522,
#80523,#80524,#80525,#80526,#80527,#80528,#80529,#80530,#80531,#80532,#80533,
#80534,#80535,#80536,#80537,#80538,#80539,#80540,#80541,#80542,#80543,#80544,
#80545,#80546,#80547,#80548,#80549,#80550,#80551,#80552,#80553,#80554,#80555,
#80556,#80557,#80558,#80559,#80560,#80561,#80562,#80563,#80564,#80565,#80566,
#80567,#80568,#80569,#80570,#80571,#80572,#80573,#80574,#80575,#80576),
 .UNSPECIFIED.,.F.,.F.,(4,2,2,2,2,2,2,2,2,2,2,2,2,2,2,2,2,2,2,2,2,2,2,2,
2,2,2,2,2,2,2,2,2,2,2,2,2,2,2,2,2,2,2,2,2,2,2,2,2,2,2,2,2,2,2,2,2,2,2,2,
2,2,2,2,2,2,2,2,2,2,2,2,2,2,2,2,2,2,4),(-1.16355052402537,-1.11305031683564,
-1.10152596335983,-1.09592528045025,-1.09148272382327,-1.08644784742858,
-1.07775055560716,-1.03061364858019,-0.985569135421594,-0.979032311349418,
-0.975880384273367,-0.973385441481947,-0.970315406463096,-0.964198472860405,
-0.92512811681522,-0.874022662882113,-0.864822853670405,-0.859143163638298,
-0.854692692973826,-0.849706086437886,-0.841236835269212,-0.79201087328454,
-0.748883051222585,-0.742184258743587,-0.739001515207173,-0.736505506455984,
-0.733462679148961,-0.727482093872668,-0.719569348803431,-0.699535464588616,
-0.652977667494132,-0.631614703220788,-0.624398752927781,-0.619677750668199,
-0.615132218307279,-0.608811362045385,-0.592957825392288,-0.568921095850618,
-0.52315079265491,-0.508155617381412,-0.50371899288127,-0.501003453474276,
-0.498420638942382,-0.494608572700817,-0.483940387963933,-0.466392730706132,
-0.413273339262541,-0.394171618112931,-0.38720759832878,-0.383004907155321,
-0.378489423675612,-0.372344420091701,-0.357648890096711,-0.336116874575393,
-0.293888591595522,-0.272185266102778,-0.267253496571308,-0.264429985420716,
-0.261897136644301,-0.258368366494303,-0.249663408043189,-0.236553980462424,
-0.183645076248432,-0.158706404247294,-0.151054888756445,-0.146242199275311,
-0.141742374417978,-0.135695240735358,-0.121613073214625,-0.10134426098883,
-0.065061020047664,-0.0415041796078312,-0.0326900434510546,-0.0290461462357153,
-0.0265196476117824,-0.0241882205948804,-0.0214282766404578,-0.0173833660770604,
-0.000695720168090065),.UNSPECIFIED.);
#1086=B_SPLINE_CURVE_WITH_KNOTS('',3,(#80577,#80578,#80579,#80580,#80581,
#80582,#80583,#80584,#80585,#80586,#80587,#80588,#80589,#80590,#80591,#80592,
#80593,#80594,#80595,#80596,#80597,#80598,#80599,#80600,#80601,#80602,#80603,
#80604,#80605,#80606,#80607,#80608,#80609,#80610,#80611,#80612,#80613,#80614,
#80615,#80616,#80617,#80618,#80619,#80620,#80621,#80622),.UNSPECIFIED.,
 .F.,.F.,(4,2,2,2,2,2,2,2,2,2,2,2,2,2,2,2,2,2,2,2,2,2,4),(-2.98951265346651,
-2.98409967932115,-2.91825065185881,-2.90610864682674,-2.90039505197607,
-2.89594160028733,-2.89097595314149,-2.88260239747836,-2.84093330960873,
-2.81069275544095,-2.7947630285004,-2.78793211548667,-2.7827841882569,-2.7798871036176,
-2.777388936278,-2.77415583531056,-2.76743020143402,-2.72751422494492,-2.69232778408112,
-2.67217175728409,-2.66528917333918,-2.66063715892619,-2.65812282560335),
 .UNSPECIFIED.);
#1087=B_SPLINE_CURVE_WITH_KNOTS('',3,(#80623,#80624,#80625,#80626,#80627,
#80628,#80629,#80630,#80631,#80632,#80633,#80634,#80635,#80636,#80637,#80638,
#80639,#80640,#80641,#80642,#80643,#80644,#80645,#80646,#80647,#80648,#80649,
#80650,#80651,#80652,#80653,#80654,#80655,#80656,#80657,#80658,#80659,#80660,
#80661,#80662,#80663,#80664,#80665,#80666,#80667,#80668,#80669,#80670,#80671,
#80672,#80673,#80674,#80675,#80676,#80677,#80678,#80679,#80680,#80681,#80682,
#80683,#80684,#80685,#80686,#80687,#80688,#80689,#80690,#80691,#80692,#80693,
#80694,#80695,#80696,#80697,#80698,#80699,#80700,#80701,#80702,#80703,#80704,
#80705,#80706,#80707,#80708,#80709,#80710,#80711,#80712,#80713,#80714,#80715,
#80716,#80717,#80718,#80719,#80720,#80721,#80722,#80723,#80724,#80725,#80726,
#80727,#80728,#80729,#80730,#80731,#80732,#80733,#80734,#80735,#80736,#80737,
#80738,#80739,#80740,#80741,#80742,#80743,#80744,#80745,#80746,#80747,#80748,
#80749,#80750,#80751,#80752,#80753,#80754,#80755,#80756,#80757,#80758,#80759,
#80760,#80761,#80762,#80763,#80764,#80765,#80766,#80767,#80768,#80769,#80770,
#80771,#80772,#80773,#80774,#80775,#80776,#80777,#80778,#80779,#80780,#80781,
#80782,#80783,#80784,#80785,#80786,#80787,#80788,#80789,#80790,#80791,#80792,
#80793,#80794,#80795,#80796,#80797,#80798,#80799,#80800,#80801,#80802,#80803,
#80804,#80805,#80806,#80807,#80808,#80809,#80810,#80811,#80812,#80813,#80814,
#80815,#80816,#80817,#80818,#80819,#80820),.UNSPECIFIED.,.F.,.F.,(4,2,2,
2,2,2,2,2,2,2,2,2,2,2,2,2,2,2,2,2,2,2,2,2,2,2,2,2,2,2,2,2,2,2,2,2,2,2,2,
2,2,2,2,2,2,2,2,2,2,2,2,2,2,2,2,2,2,2,2,2,2,2,2,2,2,2,2,2,2,2,2,2,2,2,2,
2,2,2,2,2,2,2,2,2,2,2,2,2,2,2,2,2,2,2,2,2,2,2,4),(-1.8262871493728,-1.80231153183424,
-1.76317482492192,-1.75458341261169,-1.74957200192133,-1.74512764668482,
-1.73949430107403,-1.73045098226865,-1.67708805318982,-1.63952445875179,
-1.63366206118258,-1.63064371219958,-1.62814720372425,-1.62493760734453,
-1.61809210874062,-1.57885366766302,-1.54321036276671,-1.52957411040255,
-1.51906339441778,-1.51365803596146,-1.50922989415587,-1.5040540523161,
-1.49493674754578,-1.48342831534252,-1.45679658909519,-1.41757600249844,
-1.40051642176199,-1.39588458032644,-1.39312690873883,-1.3905688321058,
-1.38688535720896,-1.37714522893103,-1.31287498189162,-1.28761151980343,
-1.27993194034675,-1.27511452193528,-1.27061909236573,-1.26459140667491,
-1.25062010980713,-1.2305730718803,-1.20129097680454,-1.19694774515022,
-1.16467323340541,-1.15951111923406,-1.15660829078806,-1.15434944133921,
-1.15112602167638,-1.14420561004622,-1.11366484499995,-1.05686365683889,
-1.04566575910983,-1.04012777584703,-1.03569194194172,-1.03061821398927,
-1.02173142218677,-1.01076702095896,-0.986131013649406,-0.934426257952615,
-0.924901040653196,-0.921144895470947,-0.918599012583689,-0.915875003085733,
-0.911396556173234,-0.894230505109473,-0.854880502643915,-0.815140363222623,
-0.806794432270155,-0.801835142114099,-0.797381233503409,-0.791658504462818,
-0.779463359793706,-0.74811391703015,-0.693256936246748,-0.686566635393643,
-0.683386101912153,-0.680890962640978,-0.677848233663168,-0.671865222917363,
-0.640466832042411,-0.585326097563374,-0.573891800094391,-0.568225906993194,
-0.564061034403986,-0.55952030999714,-0.553219711707989,-0.537494340710455,
-0.513740587855433,-0.468351771957618,-0.452650916068628,-0.448149534932015,
-0.445420442114275,-0.442847332738486,-0.439082302120109,-0.428758307467109,
-0.412035592363433,-0.381659463879675,-0.341395124898333,-0.333023989020014,
-0.33210769087985),.UNSPECIFIED.);
#1088=B_SPLINE_CURVE_WITH_KNOTS('',3,(#80825,#80826,#80827,#80828,#80829,
#80830,#80831,#80832,#80833,#80834,#80835,#80836,#80837,#80838,#80839,#80840,
#80841,#80842,#80843,#80844,#80845,#80846,#80847,#80848,#80849,#80850,#80851,
#80852,#80853,#80854,#80855,#80856,#80857,#80858,#80859,#80860,#80861,#80862,
#80863,#80864,#80865,#80866,#80867,#80868,#80869,#80870,#80871,#80872,#80873,
#80874,#80875,#80876,#80877,#80878,#80879,#80880,#80881,#80882,#80883,#80884,
#80885,#80886,#80887,#80888,#80889,#80890,#80891,#80892,#80893,#80894,#80895,
#80896,#80897,#80898,#80899,#80900,#80901,#80902,#80903,#80904,#80905,#80906,
#80907,#80908,#80909,#80910,#80911,#80912,#80913,#80914,#80915,#80916,#80917,
#80918,#80919,#80920,#80921,#80922,#80923,#80924,#80925,#80926,#80927,#80928,
#80929,#80930,#80931,#80932,#80933,#80934,#80935,#80936,#80937,#80938,#80939,
#80940,#80941,#80942,#80943,#80944,#80945,#80946,#80947,#80948,#80949,#80950,
#80951,#80952,#80953,#80954,#80955,#80956,#80957,#80958,#80959,#80960,#80961,
#80962,#80963,#80964,#80965,#80966,#80967,#80968,#80969,#80970,#80971,#80972,
#80973,#80974,#80975,#80976,#80977,#80978,#80979,#80980,#80981,#80982,#80983,
#80984,#80985,#80986,#80987,#80988,#80989,#80990,#80991,#80992,#80993,#80994,
#80995,#80996,#80997,#80998,#80999,#81000,#81001,#81002,#81003,#81004,#81005,
#81006,#81007,#81008,#81009,#81010,#81011,#81012,#81013,#81014,#81015,#81016,
#81017,#81018,#81019,#81020,#81021,#81022),.UNSPECIFIED.,.F.,.F.,(4,2,2,
2,2,2,2,2,2,2,2,2,2,2,2,2,2,2,2,2,2,2,2,2,2,2,2,2,2,2,2,2,2,2,2,2,2,2,2,
2,2,2,2,2,2,2,2,2,2,2,2,2,2,2,2,2,2,2,2,2,2,2,2,2,2,2,2,2,2,2,2,2,2,2,2,
2,2,2,2,2,2,2,2,2,2,2,2,2,2,2,2,2,2,2,2,2,2,2,4),(-2.65781287416919,-2.64452458263601,
-2.63763443226677,-2.6344163790306,-2.63215791714073,-2.62925068407198,
-2.62406985834844,-2.58961924028388,-2.56330650341922,-2.54024357241541,
-2.52972695456487,-2.5211225969632,-2.51610793400733,-2.51166322141039,
-2.50603280806457,-2.49700118311198,-2.44351098074392,-2.40644724033001,
-2.40035087378956,-2.39728523066004,-2.39479057739968,-2.3916348901716,
-2.38507677746596,-2.32962104463382,-2.29199842368044,-2.28383444530008,
-2.27891335216599,-2.27444973177503,-2.26874847442395,-2.25925642730268,
-2.1954186295027,-2.17662729409528,-2.16902820931757,-2.16323075013755,
-2.16022522160023,-2.15772714908705,-2.15449981001434,-2.14756081804742,
-2.11213657532916,-2.07385580968631,-2.05272779956298,-2.04573496809047,
-2.04106023952762,-2.03653656997462,-2.03008359002822,-2.01443384402534,
-1.96258581996294,-1.94106195088109,-1.93278861124956,-1.92660168798422,
-1.92351790494313,-1.92102341739039,-1.91788667059428,-1.91142827520871,
-1.86514624005752,-1.81937373430837,-1.81057139679469,-1.80551446017698,
-1.80107501721763,-1.79550830048053,-1.78669640842405,-1.73090798214196,
-1.69559636414734,-1.68957275138425,-1.68652136761554,-1.68402583644888,
-1.68085321850392,-1.67420755885897,-1.63070156683914,-1.58229125606155,
-1.57357002651287,-1.5685300904386,-1.56408822303984,-1.55849531224362,
-1.54959423227013,-1.49466742663082,-1.4872583395619,-1.45730012689484,
-1.45215228713223,-1.44925201259168,-1.44699168114663,-1.44376152696734,
-1.43680844822086,-1.40595251031668,-1.34812381945398,-1.33881054290913,
-1.33309820891804,-1.32864418493815,-1.32367630115275,-1.315295037307,-1.27019914879147,
-1.22214161567689,-1.21585191515742,-1.21274778148194,-1.21025330736599,
-1.20713713731564,-1.20078575746744,-1.17550652352677,-1.16355052402537),
 .UNSPECIFIED.);
#1089=B_SPLINE_CURVE_WITH_KNOTS('',3,(#81024,#81025,#81026,#81027,#81028,
#81029,#81030,#81031,#81032,#81033,#81034,#81035,#81036,#81037,#81038,#81039,
#81040,#81041,#81042,#81043,#81044,#81045,#81046,#81047,#81048,#81049,#81050,
#81051,#81052,#81053,#81054,#81055,#81056,#81057,#81058,#81059,#81060,#81061,
#81062,#81063,#81064,#81065,#81066,#81067,#81068,#81069,#81070,#81071),
 .UNSPECIFIED.,.F.,.F.,(4,2,2,2,2,2,2,2,2,2,2,2,2,2,2,2,2,2,2,2,2,2,2,4),
(-0.33210769087985,-0.328059088261506,-0.323605902234908,-0.31789213185177,
-0.305748148990684,-0.276217211565336,-0.259902966633279,-0.219658665821679,
-0.212943503580916,-0.209712607696378,-0.207214780482136,-0.204349414940198,
-0.199210667556835,-0.192416821766954,-0.176619567210251,-0.146253599696267,
-0.10453081021936,-0.0961590965829314,-0.0911940749908607,-0.0867409169303314,
-0.0810273722970079,-0.0688846258861045,-0.039398452645496,-0.000697109447201426),
 .UNSPECIFIED.);
#1090=B_SPLINE_CURVE_WITH_KNOTS('',3,(#81072,#81073,#81074,#81075,#81076,
#81077,#81078,#81079,#81080,#81081,#81082,#81083,#81084,#81085,#81086,#81087,
#81088,#81089,#81090,#81091,#81092,#81093,#81094,#81095,#81096,#81097,#81098,
#81099,#81100,#81101,#81102,#81103,#81104,#81105,#81106,#81107,#81108,#81109,
#81110,#81111,#81112,#81113,#81114,#81115,#81116,#81117,#81118,#81119,#81120,
#81121,#81122,#81123,#81124,#81125,#81126,#81127,#81128,#81129,#81130,#81131,
#81132,#81133,#81134,#81135,#81136,#81137,#81138,#81139,#81140,#81141,#81142,
#81143,#81144,#81145,#81146,#81147,#81148,#81149,#81150,#81151,#81152,#81153,
#81154,#81155,#81156,#81157,#81158,#81159,#81160,#81161,#81162,#81163,#81164,
#81165,#81166,#81167,#81168,#81169,#81170,#81171,#81172,#81173,#81174,#81175,
#81176,#81177,#81178,#81179,#81180,#81181,#81182,#81183,#81184,#81185,#81186,
#81187,#81188,#81189,#81190,#81191,#81192,#81193,#81194,#81195,#81196,#81197,
#81198,#81199,#81200,#81201,#81202,#81203,#81204,#81205,#81206,#81207,#81208,
#81209,#81210,#81211,#81212,#81213,#81214,#81215,#81216,#81217,#81218,#81219,
#81220,#81221,#81222,#81223,#81224,#81225,#81226,#81227,#81228,#81229,#81230,
#81231,#81232,#81233,#81234,#81235),.UNSPECIFIED.,.F.,.F.,(4,2,2,2,2,2,
2,2,2,2,2,2,2,2,2,2,2,2,2,2,2,2,2,2,2,2,2,2,2,2,2,2,2,2,2,2,2,2,2,2,2,2,
2,2,2,2,2,2,2,2,2,2,2,2,2,2,2,2,2,2,2,2,2,2,2,2,2,2,2,2,2,2,2,2,2,2,2,2,
2,2,2,4),(-2.98939743642882,-2.96835144039151,-2.9647712532952,-2.96219240493113,
-2.95983841105715,-2.95746526525625,-2.95340026082852,-2.94167647306,-2.91588423164734,
-2.86658934259498,-2.85168263796954,-2.84550571718206,-2.84098586649046,
-2.83622166805944,-2.82879551810349,-2.80545418853011,-2.75655623314502,
-2.73962359178398,-2.72921181604712,-2.7254346039411,-2.72285901348154,
-2.72013352220118,-2.71564940110566,-2.70014088060965,-2.65469733861,-2.63086652725387,
-2.61510458520335,-2.60879819721514,-2.60425606021241,-2.59953246006995,
-2.59230030085221,-2.57077638517103,-2.52431636916258,-2.50430537704207,
-2.49639864036218,-2.49042224854389,-2.48738068552722,-2.48488524393333,
-2.4817027474507,-2.47500294878607,-2.43192614339766,-2.41853940276316,
-2.39425261496233,-2.37828663069864,-2.37195011035848,-2.3674024978012,
-2.36268737663663,-2.35549660725407,-2.33436986387042,-2.28756598933452,
-2.26745652904114,-2.25952532087595,-2.25353473207695,-2.25049024547462,
-2.24799483986087,-2.24481547920095,-2.23813268746026,-2.18326252362536,
-2.14524523089891,-2.13706533189525,-2.13214087507022,-2.12767817400871,
-2.12198357181017,-2.10960490711176,-2.05408794301891,-2.02394370074289,
-2.01706266851227,-2.01384615013527,-2.01158772873051,-2.00867917593621,
-2.0034930462812,-1.96881826720647,-1.96719841414491,-1.93881374806733,
-1.91809286439524,-1.90378779879486,-1.8977053555061,-1.89320059286199,
-1.88898272223026,-1.88193359129712,-1.86212851150957,-1.82653497020089),
 .UNSPECIFIED.);
#1091=B_SPLINE_CURVE_WITH_KNOTS('',3,(#81241,#81242,#81243,#81244,#81245,
#81246,#81247,#81248,#81249,#81250,#81251,#81252,#81253,#81254,#81255,#81256,
#81257,#81258,#81259,#81260,#81261,#81262,#81263,#81264,#81265,#81266,#81267,
#81268,#81269,#81270,#81271,#81272,#81273,#81274,#81275,#81276,#81277,#81278,
#81279,#81280,#81281,#81282,#81283,#81284,#81285,#81286,#81287,#81288,#81289,
#81290,#81291,#81292,#81293,#81294,#81295,#81296,#81297,#81298,#81299,#81300,
#81301,#81302,#81303,#81304,#81305,#81306,#81307,#81308,#81309,#81310,#81311,
#81312,#81313,#81314,#81315,#81316,#81317,#81318,#81319,#81320,#81321,#81322,
#81323,#81324,#81325,#81326,#81327,#81328,#81329,#81330,#81331,#81332,#81333,
#81334,#81335,#81336,#81337,#81338,#81339,#81340,#81341,#81342,#81343,#81344,
#81345,#81346,#81347,#81348,#81349,#81350,#81351,#81352,#81353,#81354,#81355,
#81356,#81357,#81358,#81359,#81360,#81361,#81362,#81363,#81364,#81365,#81366,
#81367,#81368,#81369,#81370,#81371,#81372,#81373,#81374,#81375,#81376,#81377,
#81378,#81379,#81380,#81381,#81382,#81383,#81384,#81385,#81386,#81387,#81388),
 .UNSPECIFIED.,.F.,.F.,(4,2,2,2,2,2,2,2,2,2,2,2,2,2,2,2,2,2,2,2,2,2,2,2,
2,2,2,2,2,2,2,2,2,2,2,2,2,2,2,2,2,2,2,2,2,2,2,2,2,2,2,2,2,2,2,2,2,2,2,2,
2,2,2,2,2,2,2,2,2,2,2,2,2,4),(-1.16384962784558,-1.13264335480885,-1.07715530874494,
-1.07059133960003,-1.06743397258959,-1.06493857029011,-1.06187270615642,
-1.0557779741105,-1.01892944759953,-0.965199630107386,-0.956188937264403,
-0.950563649251036,-0.946118225201842,-0.941097731460923,-0.932470567389394,
-0.921917960664898,-0.898734552015196,-0.871842118459206,-0.838060186815542,
-0.832887368854638,-0.829981362007405,-0.827721775901371,-0.824499479219632,
-0.817589829347381,-0.787169934316597,-0.730758840244741,-0.719212225213826,
-0.713607026565303,-0.709163647339682,-0.704130774896473,-0.695444530628105,
-0.684798810565613,-0.661292250463344,-0.634801420664341,-0.601144198999232,
-0.595972829888898,-0.593067215233445,-0.590807670862498,-0.587585090621078,
-0.580673498084995,-0.55023286625569,-0.493754106648572,-0.482269168287115,
-0.476675636536854,-0.472233474315141,-0.467193412963167,-0.458472563350708,
-0.410693023895285,-0.366384122349361,-0.359809939061885,-0.356650751067447,
-0.354155460181701,-0.351091641407931,-0.345006552785591,-0.309055812988115,
-0.254217043324424,-0.245314970891639,-0.239721543313514,-0.235279364284549,
-0.230239177579371,-0.221517835180842,-0.175626962922634,-0.129244721292173,
-0.122789592906387,-0.119653223917238,-0.117158420905985,-0.114073477391005,
-0.107881932826869,-0.0996017141090048,-0.0780501408867098,-0.0249406429271444,
-0.0102564647077087,-0.00445491911353678,-0.000696437445735352),
 .UNSPECIFIED.);
#1092=B_SPLINE_CURVE_WITH_KNOTS('',3,(#81389,#81390,#81391,#81392,#81393,
#81394,#81395,#81396,#81397,#81398,#81399,#81400,#81401,#81402,#81403,#81404,
#81405,#81406,#81407,#81408,#81409,#81410,#81411,#81412,#81413,#81414,#81415,
#81416,#81417,#81418,#81419,#81420,#81421,#81422,#81423,#81424,#81425,#81426,
#81427,#81428),.UNSPECIFIED.,.F.,.F.,(4,2,2,2,2,2,2,2,2,2,2,2,2,2,2,2,2,
2,2,4),(-2.98908128197759,-2.98562339621579,-2.98018070717797,-2.96981470620473,
-2.92242024352145,-2.88025232492701,-2.87410391415925,-2.87102811807109,
-2.86853398070648,-2.86538998549565,-2.85889195534857,-2.81319177366175,
-2.76619866467017,-2.75779080014898,-2.75281805627472,-2.74836633530827,
-2.74266620295889,-2.73059757337088,-2.67476448383729,-2.65781287416919),
 .UNSPECIFIED.);
#1093=B_SPLINE_CURVE_WITH_KNOTS('',3,(#81429,#81430,#81431,#81432,#81433,
#81434,#81435,#81436,#81437,#81438,#81439,#81440,#81441,#81442,#81443,#81444,
#81445,#81446,#81447,#81448,#81449,#81450,#81451,#81452,#81453,#81454,#81455,
#81456,#81457,#81458,#81459,#81460,#81461,#81462,#81463,#81464,#81465,#81466,
#81467,#81468,#81469,#81470,#81471,#81472,#81473,#81474,#81475,#81476,#81477,
#81478,#81479,#81480,#81481,#81482,#81483,#81484,#81485,#81486,#81487,#81488,
#81489,#81490,#81491,#81492,#81493,#81494,#81495,#81496,#81497,#81498,#81499,
#81500,#81501,#81502,#81503,#81504,#81505,#81506,#81507,#81508,#81509,#81510,
#81511,#81512,#81513,#81514,#81515,#81516,#81517,#81518,#81519,#81520,#81521,
#81522,#81523,#81524,#81525,#81526,#81527,#81528,#81529,#81530,#81531,#81532,
#81533,#81534,#81535,#81536,#81537,#81538,#81539,#81540,#81541,#81542,#81543,
#81544,#81545,#81546,#81547,#81548,#81549,#81550,#81551,#81552,#81553,#81554,
#81555,#81556,#81557,#81558,#81559,#81560,#81561,#81562,#81563,#81564,#81565,
#81566,#81567,#81568,#81569,#81570,#81571,#81572,#81573,#81574,#81575,#81576,
#81577,#81578,#81579,#81580,#81581,#81582,#81583,#81584,#81585,#81586,#81587,
#81588,#81589,#81590,#81591,#81592,#81593,#81594,#81595,#81596,#81597,#81598,
#81599,#81600,#81601,#81602,#81603,#81604,#81605,#81606,#81607,#81608,#81609,
#81610,#81611,#81612,#81613,#81614,#81615,#81616,#81617,#81618,#81619,#81620,
#81621,#81622,#81623,#81624,#81625,#81626,#81627,#81628,#81629,#81630,#81631,
#81632,#81633,#81634),.UNSPECIFIED.,.F.,.F.,(4,2,2,2,2,2,2,2,2,2,2,2,2,
2,2,2,2,2,2,2,2,2,2,2,2,2,2,2,2,2,2,2,2,2,2,2,2,2,2,2,2,2,2,2,2,2,2,2,2,
2,2,2,2,2,2,2,2,2,2,2,2,2,2,2,2,2,2,2,2,2,2,2,2,2,2,2,2,2,2,2,2,2,2,2,2,
2,2,2,2,2,2,2,2,2,2,2,2,2,2,2,2,2,4),(-1.82653497020089,-1.80970112590821,
-1.79223671915726,-1.78160366613386,-1.77779654584285,-1.77521499236538,
-1.77283311144874,-1.76872392079423,-1.75665454088319,-1.71373795786615,
-1.67162914340665,-1.66331574795128,-1.65836263079241,-1.65390612043639,
-1.64816863631824,-1.63633962047401,-1.58037622390727,-1.5500883571337,
-1.54319246721,-1.53997305408032,-1.53771417055892,-1.5348072324978,-1.52962889991144,
-1.49537729579061,-1.43656226837672,-1.42810495650653,-1.4226429597602,
-1.41821132711221,-1.41307957725786,-1.40391956544992,-1.39251914782045,
-1.3662945897991,-1.32810688953579,-1.30957141369085,-1.30482950014318,
-1.30204754187357,-1.29949989274249,-1.29587758674125,-1.28655857555477,
-1.27213009987825,-1.21883910084207,-1.19588830545804,-1.18850229049503,
-1.18374628345475,-1.17922171494027,-1.17301839267407,-1.15794298019146,
-1.13560674937987,-1.10851324759428,-1.07357300437759,-1.06838069201022,
-1.06547076784632,-1.06321254212297,-1.05999800865932,-1.05312766154127,
-1.02308871631241,-0.967877693020767,-0.955247820130009,-0.949509277762876,
-0.945040663176737,-0.940138728298648,-0.932064768603922,-0.896549822177602,
-0.851311238800805,-0.835306948598925,-0.830778069511122,-0.828042671806354,
-0.825472451545619,-0.821724346534809,-0.811526696793529,-0.795103250329995,
-0.764916273838363,-0.724067180882814,-0.715648247158712,-0.710672661396939,
-0.706220696233654,-0.700523478843023,-0.688474018259306,-0.644969752440523,
-0.602092906725322,-0.595362899456894,-0.592174485393937,-0.589678522256883,
-0.586641333543003,-0.580687761865217,-0.572821570930227,-0.552975160005654,
-0.490249253756482,-0.481024746731182,-0.475338339429444,-0.470887707456453,
-0.465906243441543,-0.457459094231963,-0.447187788532852,-0.424961487981722,
-0.397763238210572,-0.36275099754082,-0.35755692854549,-0.354646635873784,
-0.352388506059758,-0.349174606164239,-0.342307530389767,-0.332036819262125),
 .UNSPECIFIED.);
#1094=B_SPLINE_CURVE_WITH_KNOTS('',3,(#81639,#81640,#81641,#81642,#81643,
#81644,#81645,#81646,#81647,#81648,#81649,#81650,#81651,#81652,#81653,#81654,
#81655,#81656,#81657,#81658,#81659,#81660,#81661,#81662,#81663,#81664,#81665,
#81666,#81667,#81668,#81669,#81670,#81671,#81672,#81673,#81674,#81675,#81676,
#81677,#81678,#81679,#81680,#81681,#81682,#81683,#81684,#81685,#81686,#81687,
#81688,#81689,#81690,#81691,#81692,#81693,#81694,#81695,#81696,#81697,#81698,
#81699,#81700,#81701,#81702,#81703,#81704,#81705,#81706,#81707,#81708,#81709,
#81710,#81711,#81712,#81713,#81714,#81715,#81716,#81717,#81718,#81719,#81720,
#81721,#81722,#81723,#81724,#81725,#81726,#81727,#81728,#81729,#81730,#81731,
#81732,#81733,#81734,#81735,#81736,#81737,#81738,#81739,#81740,#81741,#81742,
#81743,#81744,#81745,#81746,#81747,#81748,#81749,#81750,#81751,#81752,#81753,
#81754,#81755,#81756,#81757,#81758,#81759,#81760,#81761,#81762,#81763,#81764,
#81765,#81766,#81767,#81768,#81769,#81770,#81771,#81772,#81773,#81774,#81775,
#81776,#81777,#81778,#81779,#81780,#81781,#81782,#81783,#81784,#81785,#81786,
#81787,#81788,#81789,#81790,#81791,#81792,#81793,#81794,#81795,#81796,#81797,
#81798,#81799,#81800,#81801,#81802,#81803,#81804,#81805,#81806,#81807,#81808,
#81809,#81810,#81811,#81812,#81813,#81814,#81815,#81816,#81817,#81818,#81819,
#81820,#81821,#81822,#81823,#81824,#81825,#81826,#81827,#81828),
 .UNSPECIFIED.,.F.,.F.,(4,2,2,2,2,2,2,2,2,2,2,2,2,2,2,2,2,2,2,2,2,2,2,2,
2,2,2,2,2,2,2,2,2,2,2,2,2,2,2,2,2,2,2,2,2,2,2,2,2,2,2,2,2,2,2,2,2,2,2,2,
2,2,2,2,2,2,2,2,2,2,2,2,2,2,2,2,2,2,2,2,2,2,2,2,2,2,2,2,2,2,2,2,2,2,4),
(-2.65823196508423,-2.62110632888272,-2.61260737370035,-2.60761486878515,
-2.60316612921432,-2.59749825886872,-2.58833798236918,-2.53654601965269,
-2.49804054988087,-2.49192895580075,-2.48886017720573,-2.48636546161178,
-2.48321283390219,-2.47667132807758,-2.43180034859266,-2.38404627703729,
-2.37562801733836,-2.37065256201901,-2.3662005135559,-2.36050287082104,
-2.35123965814575,-2.30140043264854,-2.26115885295507,-2.25502920647947,
-2.25195679406253,-2.2494621128433,-2.24631329017173,-2.23979187175334,
-2.19447794775182,-2.14712476661639,-2.13871097780566,-2.13373640570348,
-2.12928407254857,-2.12358457635096,-2.11431514562047,-2.06462207977832,
-2.02424534077738,-2.01811417731508,-2.01504142661204,-2.01254669968366,
-2.00939810899445,-2.00287812134408,-1.95753201883435,-1.91074393192334,
-1.90203820104005,-1.89700165348496,-1.89255949656753,-1.88696183311689,
-1.87804410547757,-1.82329139556471,-1.78724515641804,-1.78115848851448,
-1.7780945186559,-1.77559945337939,-1.77244100577951,-1.76586982460099,
-1.72157259258723,-1.67410050420845,-1.66523473290619,-1.66016431823936,
-1.655726314816,-1.65017891756596,-1.64143325680447,-1.57637817630137,-1.55747048118079,
-1.54984112311895,-1.54402573878985,-1.54101627206618,-1.53851808255814,
-1.53529464053577,-1.52837837356498,-1.49536490985464,-1.43847530064763,
-1.42978861385701,-1.42425835965677,-1.41982145750941,-1.41473856344693,
-1.40581438615714,-1.3947916545609,-1.36995071078761,-1.3166640969491,-1.30854201286324,
-1.30534551307528,-1.30278805391383,-1.30008043360708,-1.29568022180041,
-1.27948573374916,-1.24448601134699,-1.20304942653334,-1.19355766283247,
-1.18785570882297,-1.18339107176011,-1.17846837607184,-1.17030063341044,
-1.16384962784558),.UNSPECIFIED.);
#1095=B_SPLINE_CURVE_WITH_KNOTS('',3,(#81830,#81831,#81832,#81833,#81834,
#81835,#81836,#81837,#81838,#81839,#81840,#81841,#81842,#81843,#81844,#81845,
#81846,#81847,#81848,#81849,#81850,#81851,#81852,#81853,#81854,#81855,#81856,
#81857,#81858,#81859,#81860,#81861,#81862,#81863,#81864,#81865,#81866,#81867,
#81868,#81869,#81870,#81871),.UNSPECIFIED.,.F.,.F.,(4,2,2,2,2,2,2,2,2,2,
2,2,2,2,2,2,2,2,2,2,4),(-0.332036819262125,-0.312300142779555,-0.257186157337942,
-0.244467488921226,-0.238713611913341,-0.23424293479366,-0.229348731392269,
-0.22131084064477,-0.186545904668108,-0.159874092150857,-0.125791004616353,
-0.120615431454693,-0.117709309595276,-0.115450563461532,-0.112230764800162,
-0.105331638943737,-0.0750080527306256,-0.0161391283607585,-0.00623627656673708,
-0.00289603065962882,-0.000696476426962337),.UNSPECIFIED.);
#1096=B_SPLINE_CURVE_WITH_KNOTS('',3,(#81872,#81873,#81874,#81875,#81876,
#81877,#81878,#81879,#81880,#81881,#81882,#81883,#81884,#81885,#81886,#81887,
#81888,#81889,#81890,#81891,#81892,#81893,#81894,#81895,#81896,#81897,#81898,
#81899,#81900,#81901,#81902,#81903,#81904,#81905,#81906,#81907,#81908,#81909,
#81910,#81911,#81912,#81913,#81914,#81915,#81916,#81917,#81918,#81919,#81920,
#81921,#81922,#81923,#81924,#81925,#81926,#81927,#81928,#81929,#81930,#81931,
#81932,#81933,#81934,#81935,#81936,#81937,#81938,#81939,#81940,#81941,#81942,
#81943,#81944,#81945,#81946,#81947,#81948,#81949,#81950,#81951,#81952,#81953,
#81954,#81955,#81956,#81957,#81958,#81959,#81960,#81961,#81962,#81963,#81964,
#81965,#81966,#81967,#81968,#81969,#81970,#81971,#81972,#81973,#81974,#81975,
#81976,#81977,#81978,#81979,#81980,#81981,#81982,#81983,#81984,#81985,#81986,
#81987,#81988,#81989,#81990,#81991,#81992,#81993,#81994,#81995,#81996,#81997,
#81998,#81999,#82000,#82001,#82002,#82003,#82004,#82005,#82006,#82007,#82008,
#82009,#82010,#82011,#82012,#82013,#82014,#82015,#82016,#82017,#82018,#82019,
#82020,#82021,#82022,#82023,#82024,#82025,#82026,#82027,#82028,#82029,#82030,
#82031),.UNSPECIFIED.,.F.,.F.,(4,2,2,2,2,2,2,2,2,2,2,2,2,2,2,2,2,2,2,2,
2,2,2,2,2,2,2,2,2,2,2,2,2,2,2,2,2,2,2,2,2,2,2,2,2,2,2,2,2,2,2,2,2,2,2,2,
2,2,2,2,2,2,2,2,2,2,2,2,2,2,2,2,2,2,2,2,2,2,2,4),(-2.98894236366457,-2.98719149497955,
-2.98443472872881,-2.97928353659024,-2.96996586450606,-2.91021203323611,
-2.87979806344222,-2.87289157639098,-2.86967129382463,-2.8674133773373,
-2.86450990169052,-2.8593426609542,-2.82575399741682,-2.7992377903783,-2.77576224811274,
-2.76512756988451,-2.75644886827549,-2.75141979058993,-2.74697944090185,
-2.74137767630826,-2.73244029328463,-2.67797095581945,-2.64094100389821,
-2.63532294805655,-2.63235510916507,-2.62985468633074,-2.62663528583978,
-2.61980101151154,-2.58650162489828,-2.55805194956485,-2.53721659057297,
-2.522857418972,-2.51676780410154,-2.51226328374442,-2.50804960782287,-2.50101700566144,
-2.48133850377286,-2.42880805142329,-2.41133405691687,-2.40069840458855,
-2.39689187828238,-2.3943111619637,-2.39159610067171,-2.38715737684294,
-2.37212450614887,-2.32644037719591,-2.29713038581901,-2.28499762108514,
-2.27928669817212,-2.27483468300157,-2.26987000698712,-2.26149663538401,
-2.21998530978775,-2.19016840541577,-2.1738674119672,-2.1637240432157,-2.15998428942998,
-2.15741636088112,-2.15467964946188,-2.15014177579511,-2.13401942462286,
-2.0889146535275,-2.06533955199009,-2.05467593333234,-2.04597869801342,
-2.04094541600944,-2.03650520492702,-2.03090878091542,-2.01939841783481,
-1.96293407093485,-1.93249298140593,-1.92558314687327,-1.92236193561823,
-1.92010361250951,-1.91719995817811,-1.91203316117005,-1.87858219865173,
-1.85183610129742,-1.82840647336711,-1.82633887734828),.UNSPECIFIED.);
#1097=B_SPLINE_CURVE_WITH_KNOTS('',3,(#82037,#82038,#82039,#82040,#82041,
#82042,#82043,#82044,#82045,#82046,#82047,#82048,#82049,#82050,#82051,#82052,
#82053,#82054,#82055,#82056,#82057,#82058,#82059,#82060,#82061,#82062,#82063,
#82064,#82065,#82066,#82067,#82068,#82069,#82070,#82071,#82072,#82073,#82074,
#82075,#82076,#82077,#82078,#82079,#82080,#82081,#82082,#82083,#82084,#82085,
#82086,#82087,#82088,#82089,#82090,#82091,#82092,#82093,#82094,#82095,#82096,
#82097,#82098,#82099,#82100,#82101,#82102,#82103,#82104,#82105,#82106,#82107,
#82108,#82109,#82110,#82111,#82112,#82113,#82114,#82115,#82116,#82117,#82118,
#82119,#82120,#82121,#82122,#82123,#82124,#82125,#82126,#82127,#82128,#82129,
#82130,#82131,#82132,#82133,#82134,#82135,#82136,#82137,#82138,#82139,#82140,
#82141,#82142,#82143,#82144,#82145,#82146,#82147,#82148,#82149,#82150,#82151,
#82152,#82153,#82154,#82155,#82156,#82157,#82158,#82159,#82160,#82161,#82162,
#82163,#82164,#82165,#82166,#82167,#82168,#82169,#82170,#82171,#82172,#82173,
#82174,#82175,#82176,#82177,#82178,#82179,#82180,#82181,#82182,#82183,#82184,
#82185,#82186,#82187,#82188,#82189,#82190,#82191,#82192),.UNSPECIFIED.,
 .F.,.F.,(4,2,2,2,2,2,2,2,2,2,2,2,2,2,2,2,2,2,2,2,2,2,2,2,2,2,2,2,2,2,2,
2,2,2,2,2,2,2,2,2,2,2,2,2,2,2,2,2,2,2,2,2,2,2,2,2,2,2,2,2,2,2,2,2,2,2,2,
2,2,2,2,2,2,2,2,2,2,4),(-1.16376602945442,-1.16069183205709,-1.15788286783102,
-1.15534608126095,-1.15178827005644,-1.14289274022277,-1.12937902479356,
-1.07160488054321,-1.05111372195162,-1.04399028483296,-1.03928943753722,
-1.03473338399442,-1.02834798046327,-1.01204166188582,-0.986976188406588,
-0.931462349770898,-0.924907314360272,-0.921752336311438,-0.919257683878152,
-0.916191330562035,-0.910092298094168,-0.872713837837185,-0.819644568669884,
-0.810580671528279,-0.804940403647636,-0.800494115179469,-0.795484189056702,
-0.78690454654695,-0.738174578636503,-0.694706752770642,-0.688052232068289,
-0.684877863401551,-0.682382267047372,-0.679332385297111,-0.673315895924059,
-0.665340757268196,-0.645052723320984,-0.597600621152522,-0.577284300091211,
-0.570178639171276,-0.565480807648226,-0.560921155593607,-0.554519718165925,
-0.538106663783663,-0.512796923779453,-0.457844888627675,-0.451173484115442,
-0.447996040263678,-0.445500401990743,-0.442453399209398,-0.436451416613632,
-0.428501483072402,-0.408316308829892,-0.361227182980276,-0.340485179414432,
-0.333334250511204,-0.328626938157609,-0.324073265515375,-0.317705627872007,
-0.301529337907284,-0.276763475956864,-0.224150018076021,-0.215441685501549,
-0.211811169687327,-0.209261854479781,-0.206655163671707,-0.202527887014327,
-0.197317962810966,-0.18669839331063,-0.153474588505777,-0.109606078461187,
-0.100196887992094,-0.0944569491039428,-0.0899996154102394,-0.0850466495916382,
-0.0767360479998006,-0.0347791378764354,-0.000700874915968101),
 .UNSPECIFIED.);
#1098=B_SPLINE_CURVE_WITH_KNOTS('',3,(#82193,#82194,#82195,#82196,#82197,
#82198,#82199,#82200,#82201,#82202,#82203,#82204,#82205,#82206,#82207,#82208,
#82209,#82210,#82211,#82212,#82213,#82214,#82215,#82216,#82217,#82218,#82219,
#82220,#82221,#82222,#82223,#82224,#82225,#82226,#82227,#82228,#82229,#82230,
#82231,#82232,#82233,#82234,#82235,#82236,#82237,#82238,#82239,#82240,#82241,
#82242,#82243,#82244),.UNSPECIFIED.,.F.,.F.,(4,2,2,2,2,2,2,2,2,2,2,2,2,
2,2,2,2,2,2,2,2,2,2,2,2,4),(-2.9893126115947,-2.97005979873191,-2.96636877391737,
-2.96374759619947,-2.96141745538025,-2.95908107747098,-2.95521289072605,
-2.94493468189805,-2.92042789239686,-2.86975750041926,-2.85356624816674,
-2.84719691549601,-2.84264325775646,-2.83793701408568,-2.83078981462581,
-2.81008153844967,-2.76293463701884,-2.74272978446433,-2.73477523313501,
-2.72877119265797,-2.72572393422581,-2.72322851526505,-2.72005190500433,
-2.71338406009976,-2.67023979413528,-2.65823196508423),.UNSPECIFIED.);
#1099=B_SPLINE_CURVE_WITH_KNOTS('',3,(#82245,#82246,#82247,#82248,#82249,
#82250,#82251,#82252,#82253,#82254,#82255,#82256,#82257,#82258,#82259,#82260,
#82261,#82262,#82263,#82264,#82265,#82266,#82267,#82268,#82269,#82270,#82271,
#82272,#82273,#82274,#82275,#82276,#82277,#82278,#82279,#82280,#82281,#82282,
#82283,#82284,#82285,#82286,#82287,#82288,#82289,#82290,#82291,#82292,#82293,
#82294,#82295,#82296,#82297,#82298,#82299,#82300,#82301,#82302,#82303,#82304,
#82305,#82306,#82307,#82308,#82309,#82310,#82311,#82312,#82313,#82314,#82315,
#82316,#82317,#82318,#82319,#82320,#82321,#82322,#82323,#82324,#82325,#82326,
#82327,#82328,#82329,#82330,#82331,#82332,#82333,#82334,#82335,#82336,#82337,
#82338,#82339,#82340,#82341,#82342,#82343,#82344,#82345,#82346,#82347,#82348,
#82349,#82350,#82351,#82352,#82353,#82354,#82355,#82356,#82357,#82358,#82359,
#82360,#82361,#82362,#82363,#82364,#82365,#82366,#82367,#82368,#82369,#82370,
#82371,#82372,#82373,#82374,#82375,#82376,#82377,#82378,#82379,#82380,#82381,
#82382,#82383,#82384,#82385,#82386,#82387,#82388,#82389,#82390,#82391,#82392,
#82393,#82394,#82395,#82396,#82397,#82398,#82399,#82400,#82401,#82402,#82403,
#82404,#82405,#82406,#82407,#82408,#82409,#82410,#82411,#82412,#82413,#82414,
#82415,#82416,#82417,#82418,#82419,#82420,#82421,#82422,#82423,#82424,#82425,
#82426,#82427,#82428,#82429,#82430,#82431,#82432,#82433,#82434,#82435,#82436),
 .UNSPECIFIED.,.F.,.F.,(4,2,2,2,2,2,2,2,2,2,2,2,2,2,2,2,2,2,2,2,2,2,2,2,
2,2,2,2,2,2,2,2,2,2,2,2,2,2,2,2,2,2,2,2,2,2,2,2,2,2,2,2,2,2,2,2,2,2,2,2,
2,2,2,2,2,2,2,2,2,2,2,2,2,2,2,2,2,2,2,2,2,2,2,2,2,2,2,2,2,2,2,2,2,2,2,4),
(-1.82633887734828,-1.81778438982932,-1.80911337743571,-1.80408541932622,
-1.79964408722359,-1.79403843363767,-1.78247992116622,-1.72606559545518,
-1.69563933742603,-1.68873073421178,-1.68550961687525,-1.6832511741358,
-1.68034710540596,-1.67517899349204,-1.64161586580808,-1.63875966479735,
-1.61414104677741,-1.59122616610754,-1.58075296432143,-1.5721765304958,
-1.56716836970222,-1.56272361565377,-1.55708530700346,-1.5480246417816,
-1.49487570158239,-1.45878925147032,-1.45187245394213,-1.44864969526387,
-1.44615251690247,-1.4431449137955,-1.43733506746339,-1.42971516231225,
-1.41084110585146,-1.34576832318268,-1.33703781485929,-1.33149601454951,
-1.32706006941872,-1.32198941293647,-1.31311650352168,-1.26540547197718,
-1.22134970219043,-1.21475849771345,-1.21159693789433,-1.20910270947118,
-1.20604390169432,-1.19997966466723,-1.16400355881563,-1.10918103807951,
-1.10027672432412,-1.09468401753295,-1.09024375636261,-1.08520721585225,
-1.07649610651083,-1.02998165767351,-0.984299111980955,-0.977796403120067,
-0.974651757277269,-0.972157961488794,-0.96908373430611,-0.962941999958468,
-0.921310530522911,-0.873028955391398,-0.863714270511721,-0.85800266421684,
-0.853550189728759,-0.84858507725612,-0.840211156485884,-0.795393860740249,
-0.746991056580356,-0.740741741693939,-0.737646220303662,-0.735152642582859,
-0.732030147604351,-0.725642726513586,-0.700044265587319,-0.635016468947442,
-0.626276268734541,-0.62073157684054,-0.616295340693097,-0.611226544975979,
-0.602362709434634,-0.554908348522705,-0.510543429062609,-0.503975026865087,
-0.500817793190879,-0.498323688466495,-0.495260989210625,-0.489177160976494,
-0.453157721312071,-0.398425869330592,-0.389512560884695,-0.38391725076205,
-0.37947678512828,-0.374442000829828,-0.365739087200185,-0.332021502204684),
 .UNSPECIFIED.);
#1100=B_SPLINE_CURVE_WITH_KNOTS('',3,(#82441,#82442,#82443,#82444,#82445,
#82446,#82447,#82448,#82449,#82450,#82451,#82452,#82453,#82454,#82455,#82456,
#82457,#82458,#82459,#82460,#82461,#82462,#82463,#82464,#82465,#82466,#82467,
#82468,#82469,#82470,#82471,#82472,#82473,#82474,#82475,#82476,#82477,#82478,
#82479,#82480,#82481,#82482,#82483,#82484,#82485,#82486,#82487,#82488,#82489,
#82490,#82491,#82492,#82493,#82494,#82495,#82496,#82497,#82498,#82499,#82500,
#82501,#82502,#82503,#82504,#82505,#82506,#82507,#82508,#82509,#82510,#82511,
#82512,#82513,#82514,#82515,#82516,#82517,#82518,#82519,#82520,#82521,#82522,
#82523,#82524,#82525,#82526,#82527,#82528,#82529,#82530,#82531,#82532,#82533,
#82534,#82535,#82536,#82537,#82538,#82539,#82540,#82541,#82542,#82543,#82544,
#82545,#82546,#82547,#82548,#82549,#82550,#82551,#82552,#82553,#82554,#82555,
#82556,#82557,#82558,#82559,#82560,#82561,#82562,#82563,#82564,#82565,#82566,
#82567,#82568,#82569,#82570,#82571,#82572,#82573,#82574,#82575,#82576,#82577,
#82578,#82579,#82580,#82581,#82582,#82583,#82584,#82585,#82586,#82587,#82588,
#82589,#82590,#82591,#82592,#82593,#82594,#82595,#82596,#82597,#82598,#82599,
#82600,#82601,#82602,#82603,#82604,#82605,#82606,#82607,#82608,#82609,#82610,
#82611,#82612,#82613,#82614,#82615,#82616,#82617,#82618,#82619,#82620,#82621,
#82622,#82623,#82624,#82625,#82626,#82627,#82628,#82629,#82630,#82631,#82632,
#82633,#82634,#82635,#82636,#82637,#82638),.UNSPECIFIED.,.F.,.F.,(4,2,2,
2,2,2,2,2,2,2,2,2,2,2,2,2,2,2,2,2,2,2,2,2,2,2,2,2,2,2,2,2,2,2,2,2,2,2,2,
2,2,2,2,2,2,2,2,2,2,2,2,2,2,2,2,2,2,2,2,2,2,2,2,2,2,2,2,2,2,2,2,2,2,2,2,
2,2,2,2,2,2,2,2,2,2,2,2,2,2,2,2,2,2,2,2,2,2,2,4),(-2.65783630003039,-2.62025724672317,
-2.59026002352647,-2.58338687452484,-2.58016987293391,-2.5779147849277,
-2.57502409443245,-2.56987023535567,-2.53601410385819,-2.53220384264842,
-2.49351727602241,-2.47229634900656,-2.46532441422057,-2.46067808289738,
-2.45619347261433,-2.44981793026436,-2.43447698099005,-2.37014745084294,
-2.35617882808727,-2.34708317286216,-2.34351202890345,-2.34098411339723,
-2.33819456913727,-2.33342023946376,-2.31439865527741,-2.27656576230403,
-2.25046201662442,-2.2336953270014,-2.22723427987696,-2.22265502762685,
-2.21850597538671,-2.21188319660244,-2.1952193536177,-2.13968639896198,
-2.12187022712013,-2.11108962809155,-2.10725338800942,-2.10465873617751,
-2.10194101691624,-2.09750404117048,-2.08253386131033,-2.03682544207648,
-2.00077115297086,-1.99267221472486,-1.98776352547717,-1.9832940128199,
-1.9775615295873,-1.96497607002037,-1.90962833227616,-1.87953157722104,
-1.87265534989017,-1.86944013225431,-1.86718284167032,-1.8642768303556,
-1.85909501772978,-1.82448791316893,-1.82281279576623,-1.79437275401685,
-1.77368709296597,-1.75940217335275,-1.75332653976141,-1.74882637293204,
-1.74461255893049,-1.73756980486417,-1.71778446752739,-1.65914474589488,
-1.64556051353102,-1.6366337722647,-1.63307296305554,-1.63053680646219,
-1.62772995463092,-1.6228752428456,-1.60267263019481,-1.5595181903213,-1.52774610497277,
-1.51916513964252,-1.51415363199657,-1.50970538931478,-1.50406182407289,
-1.4949905037558,-1.45921070096346,-1.42149493248338,-1.40234472336841,
-1.3975609912891,-1.39476861893207,-1.39222334445913,-1.38861959501525,
-1.37942803110678,-1.36527856082562,-1.29750524316419,-1.28502018875945,
-1.27922076477125,-1.27474336494521,-1.26987046074447,-1.26193349746236,
-1.22909285958213,-1.18598859412965,-1.16555856101527,-1.16376602945442),
 .UNSPECIFIED.);
#1101=B_SPLINE_CURVE_WITH_KNOTS('',3,(#82640,#82641,#82642,#82643,#82644,
#82645,#82646,#82647,#82648,#82649,#82650,#82651,#82652,#82653,#82654,#82655,
#82656,#82657,#82658,#82659,#82660,#82661,#82662,#82663,#82664,#82665,#82666,
#82667,#82668,#82669,#82670,#82671,#82672,#82673,#82674,#82675,#82676,#82677,
#82678,#82679,#82680,#82681,#82682,#82683,#82684,#82685,#82686,#82687,#82688,
#82689),.UNSPECIFIED.,.F.,.F.,(4,2,2,2,2,2,2,2,2,2,2,2,2,2,2,2,2,2,2,2,
2,2,2,2,4),(-0.332021502204684,-0.314750276325415,-0.273945377692634,-0.267828768211411,
-0.264722750239849,-0.262188964339053,-0.259442466591306,-0.254860805888606,
-0.236311830470826,-0.201955244629108,-0.158843121856831,-0.150476168811389,
-0.145512529941376,-0.14105972825867,-0.135345410942993,-0.12319611792551,
-0.05728481023809,-0.0357895690043997,-0.0298688139829515,-0.0268006421772528,
-0.0245072135341658,-0.0221157627278488,-0.0190823675188528,-0.0121964569415065,
-0.000855159943180343),.UNSPECIFIED.);
#1102=B_SPLINE_CURVE_WITH_KNOTS('',3,(#82690,#82691,#82692,#82693,#82694,
#82695,#82696,#82697,#82698,#82699,#82700,#82701,#82702,#82703,#82704,#82705,
#82706,#82707,#82708,#82709,#82710,#82711,#82712,#82713,#82714,#82715,#82716,
#82717,#82718,#82719,#82720,#82721,#82722,#82723,#82724,#82725,#82726,#82727,
#82728,#82729,#82730,#82731,#82732,#82733,#82734,#82735,#82736,#82737,#82738,
#82739,#82740,#82741,#82742,#82743,#82744,#82745,#82746,#82747,#82748,#82749,
#82750,#82751,#82752,#82753,#82754,#82755,#82756,#82757,#82758,#82759,#82760,
#82761,#82762,#82763,#82764,#82765,#82766,#82767,#82768,#82769,#82770,#82771,
#82772,#82773,#82774,#82775,#82776,#82777,#82778,#82779,#82780,#82781,#82782,
#82783,#82784,#82785,#82786,#82787,#82788,#82789,#82790,#82791,#82792,#82793,
#82794,#82795,#82796,#82797,#82798,#82799,#82800,#82801,#82802,#82803,#82804,
#82805,#82806,#82807,#82808,#82809,#82810,#82811,#82812,#82813,#82814,#82815,
#82816,#82817,#82818,#82819,#82820,#82821,#82822,#82823,#82824,#82825,#82826,
#82827,#82828,#82829,#82830,#82831,#82832,#82833,#82834,#82835,#82836,#82837,
#82838,#82839,#82840,#82841,#82842,#82843,#82844,#82845,#82846,#82847,#82848,
#82849,#82850,#82851),.UNSPECIFIED.,.F.,.F.,(4,2,2,2,2,2,2,2,2,2,2,2,2,
2,2,2,2,2,2,2,2,2,2,2,2,2,2,2,2,2,2,2,2,2,2,2,2,2,2,2,2,2,2,2,2,2,2,2,2,
2,2,2,2,2,2,2,2,2,2,2,2,2,2,2,2,2,2,2,2,2,2,2,2,2,2,2,2,2,2,2,4),(1.16366148960649,
1.16368973496222,1.16649156184632,1.16902779165957,1.17259386188237,1.18155821463464,
1.19522459278802,1.25504508512148,1.27376199386646,1.28066823112477,1.28485582794688,
1.28936993467832,1.29553965423417,1.31043035232553,1.33237825308395,1.37553549347217,
1.39574582192838,1.4005868449715,1.4033878162072,1.40592494672093,1.4094909219926,
1.41844118160067,1.4320738560481,1.49139262735065,1.51053614798074,1.51750495550926,
1.52170799288443,1.52622192218291,1.53236145229041,1.54702780299661,1.56850079790653,
1.61077965475065,1.63238866505133,1.6373149755014,1.64013737238837,1.64266977575962,
1.64619984252791,1.65491927423381,1.66806293992059,1.72134718560026,1.74593068914121,
1.75354531019233,1.75834813960603,1.76284784104249,1.76890878188728,1.78309104304976,
1.80356421713465,1.83230168321304,1.83454973361319,1.86865084058222,1.87382418604824,
1.87672887053467,1.87898624884471,1.88220381332518,1.88909702423443,1.91938336237638,
1.97536231073971,1.98611570852936,1.99161727673111,1.99615375622198,2.00080384543155,
2.00768701961816,2.02787095104097,2.06315115545376,2.10291576507191,2.10972923896683,
2.11293185190813,2.11529397402805,2.11821543299602,2.12325668911744,2.12992878450712,
2.14529984158548,2.17611547722575,2.21808329528982,2.22645135701701,2.23141448867634,
2.23586611452627,2.24157793785585,2.25371829376451,2.31956693196985,2.32642657710849),
 .UNSPECIFIED.);
#1103=B_SPLINE_CURVE_WITH_KNOTS('',3,(#82855,#82856,#82857,#82858,#82859,
#82860),.UNSPECIFIED.,.F.,.F.,(4,1,1,4),(-4.09293042013066,-3.98462531944883,
-2.98846898958662,-2.06883560534994),.UNSPECIFIED.);
#1104=B_SPLINE_CURVE_WITH_KNOTS('',3,(#82864,#82865,#82866,#82867,#82868),
 .UNSPECIFIED.,.F.,.F.,(4,1,4),(0.,0.996156329862203,1.11730040836818),
 .UNSPECIFIED.);
#1105=B_SPLINE_CURVE_WITH_KNOTS('',3,(#82870,#82871,#82872,#82873,#82874,
#82875,#82876,#82877,#82878,#82879,#82880,#82881,#82882,#82883,#82884,#82885,
#82886,#82887,#82888,#82889,#82890,#82891,#82892,#82893,#82894,#82895,#82896,
#82897,#82898,#82899,#82900,#82901,#82902,#82903,#82904,#82905,#82906,#82907,
#82908,#82909,#82910,#82911,#82912,#82913,#82914,#82915,#82916,#82917,#82918,
#82919,#82920,#82921,#82922,#82923,#82924,#82925,#82926,#82927,#82928,#82929,
#82930,#82931,#82932,#82933,#82934,#82935,#82936,#82937,#82938,#82939,#82940,
#82941,#82942,#82943,#82944,#82945,#82946,#82947,#82948,#82949,#82950,#82951,
#82952,#82953,#82954,#82955,#82956,#82957,#82958,#82959,#82960,#82961,#82962,
#82963,#82964,#82965,#82966,#82967,#82968,#82969,#82970,#82971,#82972,#82973,
#82974,#82975,#82976,#82977,#82978,#82979,#82980,#82981,#82982,#82983,#82984,
#82985,#82986,#82987),.UNSPECIFIED.,.F.,.F.,(4,3,3,3,3,3,3,3,3,3,3,3,3,
3,3,3,3,3,3,3,3,3,3,3,3,3,3,3,3,3,3,3,3,3,3,3,3,3,3,4),(1.11730040836818,
1.28262178372048,1.44765157556473,1.61268575152221,1.77772714966095,1.94312500432988,
1.99231265972441,2.16189896620006,2.33115735598945,2.50038270972217,2.66956176012431,
2.83913553552575,2.98846898958662,3.15809751684031,3.32740711791633,3.49669689813223,
3.66594774295676,3.83560425255262,3.98462531944882,4.15373065172872,4.32250351684065,
4.49124368676202,4.65993689797336,4.82903410602685,4.98078164931103,5.15016484644186,
5.31922045795961,5.48824672073902,5.6572283792484,5.82661190548429,5.97693797917324,
6.14630615262454,6.31534759373514,6.48436122853589,6.6533310844071,6.82270445493501,
6.97309430903544,7.15761149677957,7.34097651449696,7.40048571521261),
 .UNSPECIFIED.);
#1106=B_SPLINE_CURVE_WITH_KNOTS('',3,(#82989,#82990,#82991,#82992,#82993,
#82994,#82995,#82996,#82997,#82998,#82999,#83000,#83001,#83002,#83003,#83004,
#83005,#83006,#83007,#83008,#83009,#83010,#83011,#83012,#83013,#83014,#83015,
#83016,#83017,#83018,#83019,#83020,#83021,#83022,#83023,#83024,#83025,#83026,
#83027,#83028,#83029,#83030,#83031,#83032,#83033,#83034,#83035,#83036,#83037,
#83038,#83039,#83040,#83041,#83042,#83043,#83044,#83045,#83046,#83047,#83048,
#83049,#83050,#83051,#83052,#83053,#83054,#83055,#83056,#83057,#83058,#83059,
#83060,#83061,#83062,#83063,#83064,#83065,#83066,#83067,#83068,#83069,#83070,
#83071,#83072,#83073,#83074,#83075,#83076,#83077,#83078,#83079,#83080,#83081,
#83082,#83083,#83084,#83085,#83086,#83087,#83088,#83089,#83090,#83091,#83092,
#83093,#83094,#83095,#83096,#83097,#83098,#83099,#83100,#83101,#83102,#83103,
#83104,#83105,#83106),.UNSPECIFIED.,.F.,.F.,(4,3,3,3,3,3,3,3,3,3,3,3,3,
3,3,3,3,3,3,3,3,3,3,3,3,3,3,3,3,3,3,3,3,3,3,3,3,3,3,4),(7.40048571554775,
7.57307735536024,7.74582609884619,7.91907496157944,7.96925063889765,8.13859372637515,
8.30760905245861,8.47659536915156,8.64553719871405,8.81488194247415,8.96540696875986,
9.13474435570046,9.30375402266731,9.47273483050185,9.64167122408181,9.81101077077705,
9.96156329862207,10.1308922600792,10.299893255479,10.4688651405637,10.6377924578226,
10.8071228616149,10.9577196284843,11.127054944352,11.2960624227752,11.465040892599,
11.6339748619994,11.8033118903903,11.9538759583465,12.1232099666738,12.2922161317669,
12.461193299171,12.6301259698601,12.7994617334433,12.9500322882087,13.1176514663611,
13.2849613103928,13.4520936828031,13.6193212956903,13.6836710227273),
 .UNSPECIFIED.);
#1107=B_SPLINE_CURVE_WITH_KNOTS('',3,(#83108,#83109,#83110,#83111,#83112,
#83113,#83114,#83115,#83116,#83117,#83118,#83119,#83120,#83121,#83122,#83123,
#83124,#83125,#83126,#83127,#83128,#83129,#83130,#83131,#83132,#83133,#83134,
#83135,#83136,#83137,#83138,#83139,#83140,#83141,#83142,#83143,#83144,#83145,
#83146,#83147,#83148,#83149,#83150,#83151,#83152,#83153,#83154,#83155,#83156,
#83157,#83158,#83159,#83160,#83161,#83162,#83163,#83164,#83165,#83166,#83167,
#83168,#83169,#83170,#83171,#83172,#83173,#83174,#83175,#83176,#83177,#83178,
#83179,#83180,#83181,#83182,#83183,#83184,#83185,#83186,#83187,#83188,#83189,
#83190,#83191,#83192,#83193,#83194,#83195,#83196,#83197,#83198,#83199,#83200,
#83201,#83202,#83203,#83204,#83205,#83206,#83207,#83208,#83209,#83210,#83211,
#83212,#83213,#83214,#83215,#83216,#83217,#83218,#83219,#83220,#83221,#83222,
#83223,#83224,#83225),.UNSPECIFIED.,.F.,.F.,(4,3,3,3,3,3,3,3,3,3,3,3,3,
3,3,3,3,3,3,3,3,3,3,3,3,3,3,3,3,3,3,3,3,3,3,3,3,3,3,4),(13.6836710228995,
13.8982811297081,13.9461886180709,14.1155225548806,14.2845286362706,14.4535057022928,
14.6224382617149,14.7917738996828,14.9423449479331,15.1116786313851,15.2806844569256,
15.4496612671025,15.6185935702331,15.7879289566079,15.9385012777953,16.1078348519791,
16.2768405642568,16.445817256677,16.6147494393768,16.7840847033611,16.9346576076575,
17.1039913134022,17.272997160196,17.4419739896877,17.6109063111027,17.7802417136301,
17.9308139375197,18.1001475983451,18.2691533996324,18.4381301833948,18.6070624588776,
18.7763978161076,18.9269702673819,19.0963039177279,19.2653097080604,19.4342864802948,
19.6032187439149,19.7725540889681,19.9231265972441,19.9668563299069),
 .UNSPECIFIED.);
#1108=B_SPLINE_CURVE_WITH_KNOTS('',3,(#83227,#83228,#83229,#83230,#83231,
#83232,#83233,#83234,#83235,#83236,#83237,#83238,#83239,#83240,#83241,#83242,
#83243,#83244,#83245,#83246,#83247,#83248,#83249,#83250,#83251,#83252,#83253,
#83254,#83255,#83256,#83257,#83258,#83259,#83260,#83261,#83262,#83263,#83264,
#83265,#83266,#83267,#83268,#83269,#83270,#83271,#83272,#83273,#83274,#83275,
#83276,#83277,#83278,#83279,#83280,#83281,#83282,#83283,#83284,#83285,#83286,
#83287,#83288,#83289,#83290,#83291,#83292,#83293,#83294,#83295,#83296,#83297,
#83298,#83299,#83300,#83301,#83302,#83303,#83304,#83305,#83306,#83307,#83308,
#83309,#83310,#83311,#83312,#83313,#83314,#83315,#83316,#83317,#83318,#83319,
#83320,#83321,#83322,#83323,#83324,#83325,#83326,#83327,#83328,#83329,#83330,
#83331,#83332,#83333,#83334,#83335,#83336,#83337,#83338,#83339,#83340,#83341),
 .UNSPECIFIED.,.F.,.F.,(4,3,3,3,3,3,3,3,3,3,3,3,3,3,3,3,3,3,3,3,3,3,3,3,
3,3,3,3,3,3,3,3,3,3,3,3,3,3,4),(19.966856330194,20.135016386822,20.3028589202274,
20.4706807137549,20.6384750732032,20.8066513695237,20.9192829271063,21.0886165881965,
21.2576223895894,21.4265991732081,21.5955314484101,21.7648668051334,21.9154392569686,
22.0847729173349,22.2537787179511,22.4227555007232,22.5916877750386,22.7610231308267,
22.9115955868308,23.080929249669,23.2499350528188,23.4189118381815,23.5878441151235,
23.7571794735431,23.907751916693,24.0770855783232,24.2460913802444,24.415068164365,
24.5840004400555,24.7533357972341,24.9039082465552,25.0732419081956,25.2422477101218,
25.4112244942395,25.5801567699226,25.7494921270864,25.9000645764174,26.0945925740695,
26.2500413990553),.UNSPECIFIED.);
#1109=B_SPLINE_CURVE_WITH_KNOTS('',3,(#83343,#83344,#83345,#83346,#83347,
#83348,#83349,#83350,#83351,#83352),.UNSPECIFIED.,.F.,.F.,(4,1,1,1,1,1,
1,4),(26.2500416370865,26.8962209062796,27.8923772361418,28.888533566004,
29.8846898958662,30.8808462257284,31.8770025555906,32.5332269442661),
 .UNSPECIFIED.);
#1110=B_SPLINE_CURVE_WITH_KNOTS('',3,(#83354,#83355,#83356,#83357,#83358,
#83359,#83360,#83361,#83362,#83363),.UNSPECIFIED.,.F.,.F.,(4,1,1,1,1,1,
1,4),(32.5332269442661,32.8731588854528,33.869315215315,34.8654715451772,
35.8616278750394,36.8577842049016,37.8539405347639,38.8164122514457),
 .UNSPECIFIED.);
#1111=B_SPLINE_CURVE_WITH_KNOTS('',3,(#83365,#83366,#83367,#83368,#83369,
#83370,#83371,#83372,#83373,#83374,#83375),.UNSPECIFIED.,.F.,.F.,(4,1,1,
1,1,1,1,1,4),(38.8164122514457,38.8500968646261,39.8462531944883,40.8424095243505,
41.8385658542127,42.8347221840749,43.8308785139371,44.8270348437993,45.0995938882313),
 .UNSPECIFIED.);
#1112=B_SPLINE_CURVE_WITH_KNOTS('',3,(#83377,#83378,#83379,#83380,#83381,
#83382,#83383,#83384,#83385,#83386,#83387,#83388,#83389,#83390,#83391,#83392,
#83393,#83394,#83395,#83396,#83397,#83398,#83399,#83400,#83401,#83402,#83403,
#83404,#83405,#83406,#83407,#83408,#83409,#83410,#83411,#83412,#83413,#83414,
#83415,#83416,#83417,#83418,#83419,#83420,#83421,#83422,#83423,#83424,#83425,
#83426,#83427,#83428,#83429,#83430,#83431,#83432,#83433,#83434,#83435,#83436,
#83437,#83438,#83439,#83440,#83441,#83442,#83443,#83444,#83445,#83446,#83447,
#83448,#83449,#83450,#83451,#83452,#83453,#83454,#83455,#83456,#83457,#83458,
#83459,#83460,#83461,#83462,#83463,#83464,#83465,#83466,#83467,#83468,#83469,
#83470,#83471,#83472,#83473,#83474,#83475,#83476,#83477,#83478,#83479,#83480,
#83481,#83482,#83483,#83484,#83485,#83486,#83487,#83488,#83489,#83490,#83491,
#83492,#83493,#83494),.UNSPECIFIED.,.F.,.F.,(4,3,3,3,3,3,3,3,3,3,3,3,3,
3,3,3,3,3,3,3,3,3,3,3,3,3,3,3,3,3,3,3,3,3,3,3,3,3,3,4),(45.0995975586253,
45.2669647013515,45.4343603268434,45.6017766473786,45.7695612509881,45.8231911736615,
45.9925248354768,46.1615306375833,46.330507421887,46.4994396977595,46.6687750551146,
46.8193475035237,46.988681165339,47.1576869674455,47.3266637517491,47.4955960276217,
47.6649313849767,47.8155038333859,47.9848374952012,48.1538432973077,48.3228200816114,
48.4917523574839,48.6610877148389,48.8116601632481,48.9809938250634,49.14999962717,
49.3189764114737,49.4879086873463,49.6572440447014,49.8078164931104,49.9771501549257,
50.1461559570324,50.3151327413361,50.4840650172086,50.6534003745637,50.8039728229726,
50.9766852054187,51.1489995200855,51.3210324932485,51.3827828658049),
 .UNSPECIFIED.);
#1113=B_SPLINE_CURVE_WITH_KNOTS('',3,(#83496,#83497,#83498,#83499,#83500,
#83501,#83502,#83503,#83504,#83505,#83506,#83507,#83508,#83509,#83510,#83511,
#83512,#83513,#83514,#83515,#83516,#83517,#83518,#83519,#83520,#83521,#83522,
#83523,#83524,#83525,#83526,#83527,#83528,#83529,#83530,#83531,#83532,#83533,
#83534,#83535,#83536,#83537,#83538,#83539,#83540,#83541,#83542,#83543,#83544,
#83545,#83546,#83547,#83548,#83549,#83550,#83551,#83552,#83553,#83554,#83555,
#83556,#83557,#83558,#83559,#83560,#83561,#83562,#83563,#83564,#83565,#83566,
#83567,#83568,#83569,#83570,#83571,#83572,#83573,#83574,#83575,#83576,#83577,
#83578,#83579,#83580,#83581,#83582,#83583,#83584,#83585,#83586,#83587,#83588,
#83589,#83590,#83591,#83592,#83593,#83594,#83595,#83596,#83597,#83598,#83599,
#83600,#83601,#83602,#83603,#83604,#83605,#83606,#83607,#83608,#83609,#83610,
#83611,#83612,#83613),.UNSPECIFIED.,.F.,.F.,(4,3,3,3,3,3,3,3,3,3,3,3,3,
3,3,3,3,3,3,3,3,3,3,3,3,3,3,3,3,3,3,3,3,3,3,3,3,3,3,4),(51.3827828659881,
51.5671902339565,51.7528607040205,51.8001291528347,51.9694628146501,52.1384686167567,
52.3074454010605,52.4763776769332,52.6457130342883,52.796285482697,52.9656191445123,
53.1346249466188,53.3036017309224,53.472534006795,53.64186936415,53.7924418125592,
53.9617754743744,54.1307812764809,54.2997580607846,54.4686903366571,54.6380256940121,
54.7885981424214,54.9579318042367,55.1269376063432,55.2959143906469,55.4648466665194,
55.6341820238745,55.7847544722836,55.9540881340989,56.1230939362054,56.292070720509,
56.4610029963816,56.6303383537366,56.7809108021458,56.9480120911382,57.1147891675956,
57.281513061229,57.4482111102018,57.6152110190328,57.665968172762),
 .UNSPECIFIED.);
#1114=B_SPLINE_CURVE_WITH_KNOTS('',3,(#83615,#83616,#83617,#83618,#83619,
#83620,#83621,#83622,#83623,#83624,#83625,#83626,#83627,#83628,#83629,#83630,
#83631,#83632,#83633,#83634,#83635,#83636,#83637,#83638,#83639,#83640,#83641,
#83642,#83643,#83644,#83645,#83646,#83647,#83648,#83649,#83650,#83651,#83652,
#83653,#83654,#83655,#83656,#83657,#83658,#83659,#83660,#83661,#83662,#83663,
#83664,#83665,#83666,#83667,#83668,#83669,#83670,#83671,#83672,#83673,#83674,
#83675,#83676,#83677,#83678,#83679,#83680,#83681,#83682,#83683,#83684,#83685,
#83686,#83687,#83688,#83689,#83690,#83691,#83692,#83693,#83694,#83695,#83696,
#83697,#83698,#83699,#83700,#83701,#83702,#83703,#83704,#83705,#83706,#83707,
#83708,#83709,#83710,#83711,#83712,#83713,#83714,#83715,#83716,#83717,#83718,
#83719,#83720,#83721,#83722,#83723,#83724,#83725,#83726,#83727,#83728,#83729),
 .UNSPECIFIED.,.F.,.F.,(4,3,3,3,3,3,3,3,3,3,3,3,3,3,3,3,3,3,3,3,3,3,3,3,
3,3,3,3,3,3,3,3,3,3,3,3,3,3,4),(57.6659681729845,57.777067132008,57.9464007938234,
58.1154065959299,58.2843833802337,58.4533156561063,58.6226510134614,58.7732234618702,
58.9425571236855,59.1115629257921,59.2805397100958,59.4494719859684,59.6188073433234,
59.7693797917324,59.9387134535477,60.1077192556542,60.2766960399578,60.4456283158303,
60.6149636731854,60.7655361215946,60.9348697834097,61.103875585516,61.2728523698194,
61.4417846456918,61.6111200030466,61.7616924514568,61.9310261132726,62.1000319153795,
62.2690086996837,62.4379409755567,62.6072763329121,62.7578487813191,62.9271824431342,
63.0961882452405,63.265165029544,63.4340973054164,63.6034326627713,63.7540051111813,
63.9491534801641),.UNSPECIFIED.);
#1115=B_SPLINE_CURVE_WITH_KNOTS('',3,(#83731,#83732,#83733,#83734,#83735,
#83736,#83737,#83738,#83739,#83740),.UNSPECIFIED.,.F.,.F.,(4,1,1,1,1,1,
1,4),(63.9491570786823,64.7501614410435,65.7463177709057,66.7424741007679,
67.7386304306301,68.7347867604923,69.7309430903545,70.2323387873437),
 .UNSPECIFIED.);
#1116=B_SPLINE_CURVE_WITH_KNOTS('',3,(#83742,#83743,#83744,#83745,#83746,
#83747,#83748,#83749,#83750,#83751),.UNSPECIFIED.,.F.,.F.,(4,1,1,1,1,1,
1,4),(70.2323387873437,70.7270994202167,71.7232557500789,72.7194120799411,
73.7155684098033,74.7117247396655,75.7078810695277,76.5155240945233),
 .UNSPECIFIED.);
#1117=B_SPLINE_CURVE_WITH_KNOTS('',3,(#83753,#83754,#83755,#83756,#83757,
#83758,#83759,#83760,#83761,#83762,#83763),.UNSPECIFIED.,.F.,.F.,(4,1,1,
1,1,1,1,1,4),(76.5155240945233,76.7040373993899,77.7001937292521,78.6963500591144,
79.6925063889766,80.6886627188388,81.684819048701,82.6809753785631,82.7987094017029),
 .UNSPECIFIED.);
#1118=B_SPLINE_CURVE_WITH_KNOTS('',3,(#83765,#83766,#83767,#83768,#83769,
#83770,#83771,#83772,#83773,#83774,#83775,#83776,#83777,#83778,#83779,#83780,
#83781,#83782,#83783,#83784,#83785,#83786,#83787,#83788,#83789,#83790,#83791,
#83792,#83793,#83794,#83795,#83796,#83797,#83798,#83799,#83800,#83801,#83802,
#83803,#83804,#83805,#83806,#83807,#83808,#83809,#83810,#83811,#83812,#83813,
#83814,#83815,#83816,#83817,#83818,#83819,#83820,#83821,#83822,#83823,#83824,
#83825,#83826,#83827,#83828,#83829,#83830,#83831,#83832,#83833,#83834,#83835,
#83836,#83837,#83838,#83839,#83840,#83841,#83842,#83843,#83844,#83845,#83846,
#83847,#83848,#83849,#83850,#83851,#83852,#83853,#83854,#83855,#83856,#83857,
#83858,#83859,#83860,#83861,#83862,#83863,#83864,#83865,#83866,#83867,#83868,
#83869,#83870,#83871,#83872,#83873,#83874,#83875,#83876,#83877,#83878,#83879,
#83880,#83881,#83882),.UNSPECIFIED.,.F.,.F.,(4,3,3,3,3,3,3,3,3,3,3,3,3,
3,3,3,3,3,3,3,3,3,3,3,3,3,3,3,3,3,3,3,3,3,3,3,3,3,3,4),(82.7987094017029,
82.965636580998,83.1322893848818,83.2989591266341,83.4656459127014,83.632687711285,
83.6771317084254,83.8464646791663,84.0154697909957,84.1844458962506,84.3533774980481,
84.5227122036214,84.6732880382876,84.842622109511,85.0116283124841,85.1806054790275,
85.3495381275839,85.5188738342397,85.6694443681498,85.8387797027031,86.00778719238,
86.176765661948,86.3456996247729,86.5150366362511,86.665600698012,86.8349293911137,
87.00393022489,87.1729021136412,87.3418295253239,87.511160171998,87.6617570278742,
87.8310949042705,88.0001048660142,88.1690856671441,88.3380218884775,88.5073609921549,
88.6579133577364,88.8428584338325,89.0266242915967,89.0818943520482),
 .UNSPECIFIED.);
#1119=B_SPLINE_CURVE_WITH_KNOTS('',3,(#83884,#83885,#83886,#83887,#83888,
#83889,#83890,#83891,#83892,#83893),.UNSPECIFIED.,.F.,.F.,(4,1,1,1,1,1,
1,4),(89.0818947088824,89.6540696875986,90.6502260174608,91.646382347323,
92.6425386771853,93.6386950070475,94.6348513369097,95.365080016062),
 .UNSPECIFIED.);
#1120=B_SPLINE_CURVE_WITH_KNOTS('',3,(#83901,#83902,#83903,#83904,#83905,
#83906,#83907,#83908,#83909),.UNSPECIFIED.,.F.,.F.,(4,1,1,1,1,1,4),(-97.6233203264963,
-96.6271639966341,-95.6310076667719,-94.6348513369097,-93.6386950070475,
-92.6425386771853,-92.0575247206449),.UNSPECIFIED.);
#1121=B_SPLINE_CURVE_WITH_KNOTS('',3,(#83911,#83912,#83913,#83914,#83915,
#83916,#83917,#83918,#83919,#83920,#83921,#83922,#83923,#83924,#83925,#83926,
#83927,#83928,#83929,#83930,#83931,#83932,#83933,#83934,#83935,#83936,#83937,
#83938,#83939,#83940,#83941,#83942,#83943,#83944,#83945,#83946,#83947,#83948,
#83949,#83950,#83951,#83952,#83953,#83954,#83955,#83956,#83957,#83958,#83959,
#83960,#83961,#83962,#83963,#83964,#83965,#83966,#83967,#83968,#83969,#83970,
#83971,#83972,#83973,#83974,#83975,#83976,#83977,#83978,#83979,#83980,#83981,
#83982,#83983,#83984,#83985,#83986,#83987,#83988,#83989,#83990,#83991,#83992,
#83993,#83994,#83995,#83996,#83997,#83998,#83999,#84000,#84001,#84002,#84003,
#84004,#84005,#84006,#84007,#84008,#84009,#84010,#84011,#84012,#84013,#84014,
#84015,#84016,#84017,#84018,#84019,#84020,#84021,#84022,#84023,#84024,#84025,
#84026,#84027,#84028),.UNSPECIFIED.,.F.,.F.,(4,3,3,3,3,3,3,3,3,3,3,3,3,
3,3,3,3,3,3,3,3,3,3,3,3,3,3,3,3,3,3,3,3,3,3,3,3,3,3,4),(-92.0575243311351,
-91.8725281814524,-91.686228476792,-91.6463823473231,-91.4770142027803,
-91.3079727917837,-91.1389591885252,-90.9699893650353,-90.8006160276294,
-90.6502260174609,-90.4809254554687,-90.3119534642138,-90.1430110847365,
-89.9741136005011,-89.8048129492577,-89.6540696875987,-89.4847266274735,
-89.3157113291214,-89.1467250403316,-88.9777832388153,-88.8084385227493,
-88.6579133577364,-88.4885759751671,-88.3195663127972,-88.1505855098421,
-87.9816491213052,-87.8123095798237,-87.6617570278742,-87.4924280547676,
-87.3234270474557,-87.1544551502299,-86.9855278206825,-86.8161974046127,
-86.665600698012,-86.4984322992574,-86.3315880451506,-86.1647945025351,
-85.9980272414912,-85.8309511841658,-85.7743394136888),.UNSPECIFIED.);
#1122=B_SPLINE_CURVE_WITH_KNOTS('',3,(#84030,#84031,#84032,#84033,#84034,
#84035,#84036,#84037,#84038,#84039,#84040,#84041,#84042,#84043,#84044,#84045,
#84046,#84047,#84048,#84049,#84050,#84051,#84052,#84053,#84054,#84055,#84056,
#84057,#84058,#84059,#84060,#84061,#84062,#84063,#84064,#84065,#84066,#84067,
#84068,#84069,#84070,#84071,#84072,#84073,#84074,#84075,#84076,#84077,#84078,
#84079,#84080,#84081,#84082,#84083,#84084,#84085,#84086,#84087,#84088,#84089,
#84090,#84091,#84092,#84093,#84094,#84095,#84096,#84097,#84098,#84099,#84100,
#84101,#84102,#84103,#84104,#84105,#84106,#84107,#84108,#84109,#84110,#84111,
#84112,#84113,#84114,#84115,#84116,#84117,#84118,#84119,#84120,#84121,#84122,
#84123,#84124,#84125,#84126,#84127,#84128,#84129,#84130,#84131,#84132,#84133,
#84134,#84135,#84136,#84137,#84138,#84139,#84140,#84141,#84142,#84143,#84144),
 .UNSPECIFIED.,.F.,.F.,(4,3,3,3,3,3,3,3,3,3,3,3,3,3,3,3,3,3,3,3,3,3,3,3,
3,3,3,3,3,3,3,3,3,3,3,3,3,3,4),(-85.7743394134653,-85.6694443681498,-85.500110360217,
-85.3311041955529,-85.1621270286254,-84.9931943584398,-84.8238585953951,
-84.6732880382876,-84.503955024643,-84.334949886129,-84.1659737793373,-83.9970421898078,
-83.8277075191266,-83.6771317084254,-83.5077977726898,-83.3387916923914,
-83.1698146274717,-83.0008820691601,-82.8315464322925,-82.6809753785632,
-82.5116416950953,-82.3426358695433,-82.173659059362,-82.0047267562309,
-81.8353913698622,-81.684819048701,-81.5154854741947,-81.3464797615862,
-81.1775030688277,-81.0085708857849,-80.8392356214567,-80.6886627188388,
-80.5193290132907,-80.350323166697,-80.1813463374077,-80.0124140161968,
-79.8430786138719,-79.6925063889766,-79.4911541062857),.UNSPECIFIED.);
#1123=B_SPLINE_CURVE_WITH_KNOTS('',3,(#84146,#84147,#84148,#84149,#84150,
#84151,#84152,#84153,#84154,#84155,#84156,#84157,#84158,#84159,#84160,#84161,
#84162,#84163,#84164,#84165,#84166,#84167,#84168,#84169,#84170,#84171,#84172,
#84173,#84174,#84175,#84176,#84177,#84178,#84179,#84180,#84181,#84182,#84183,
#84184,#84185,#84186,#84187,#84188,#84189,#84190,#84191,#84192,#84193,#84194,
#84195,#84196,#84197,#84198,#84199,#84200,#84201,#84202,#84203,#84204,#84205,
#84206,#84207,#84208,#84209,#84210,#84211,#84212,#84213,#84214,#84215,#84216,
#84217,#84218,#84219,#84220,#84221,#84222,#84223,#84224,#84225,#84226,#84227,
#84228,#84229,#84230,#84231,#84232,#84233,#84234,#84235,#84236,#84237,#84238,
#84239,#84240,#84241,#84242,#84243,#84244,#84245,#84246,#84247,#84248,#84249,
#84250,#84251,#84252,#84253,#84254,#84255,#84256,#84257,#84258,#84259,#84260),
 .UNSPECIFIED.,.F.,.F.,(4,3,3,3,3,3,3,3,3,3,3,3,3,3,3,3,3,3,3,3,3,3,3,3,
3,3,3,3,3,3,3,3,3,3,3,3,3,3,4),(-79.4911541059791,-79.3245057004151,-79.1579164140378,
-78.9913821131007,-78.8244722076974,-78.6963500591144,-78.5270164087195,
-78.3580106183368,-78.189033846051,-78.0201015823787,-77.8507662372729,
-77.7001937292522,-77.530860060675,-77.3618542516806,-77.1928774603977,
-77.0239451774834,-76.854609813131,-76.7040373993899,-76.5347037382941,
-76.3656979368956,-76.1967211532715,-76.0277888780641,-75.8584535213355,
-75.7078810695277,-75.5385474091545,-75.369541608531,-75.2005648257516,
-75.0316325514286,-74.862297195633,-74.7117247396655,-74.542391076833,-74.3733852736891,
-74.2044084883325,-74.0354762113964,-73.8661408529829,-73.7155684098033,
-73.5384040357233,-73.3618892358082,-73.2079687991062),.UNSPECIFIED.);
#1124=B_SPLINE_CURVE_WITH_KNOTS('',3,(#84262,#84263,#84264,#84265,#84266,
#84267,#84268,#84269,#84270,#84271),.UNSPECIFIED.,.F.,.F.,(4,1,1,1,1,1,
1,4),(-73.2079680704952,-72.7194120799411,-71.7232557500789,-70.7270994202167,
-69.7309430903545,-68.7347867604923,-67.7386304306301,-66.9247834919266),
 .UNSPECIFIED.);
#1125=B_SPLINE_CURVE_WITH_KNOTS('',3,(#84273,#84274,#84275,#84276,#84277,
#84278,#84279,#84280,#84281,#84282,#84283),.UNSPECIFIED.,.F.,.F.,(4,1,1,
1,1,1,1,1,4),(-66.9247834919266,-66.7424741007679,-65.7463177709057,-64.7501614410435,
-63.7540051111813,-62.757848781319,-61.7616924514569,-60.7655361215946,
-60.641598184747),.UNSPECIFIED.);
#1126=B_SPLINE_CURVE_WITH_KNOTS('',3,(#84285,#84286,#84287,#84288,#84289,
#84290,#84291,#84292,#84293,#84294),.UNSPECIFIED.,.F.,.F.,(4,1,1,1,1,1,
1,4),(-60.641598184747,-59.7693797917324,-58.7732234618702,-57.777067132008,
-56.7809108021458,-55.7847544722836,-54.7885981424214,-54.35841793122),
 .UNSPECIFIED.);
#1127=B_SPLINE_CURVE_WITH_KNOTS('',3,(#84296,#84297,#84298,#84299,#84300,
#84301,#84302,#84303,#84304,#84305,#84306,#84307,#84308,#84309,#84310,#84311,
#84312,#84313,#84314,#84315,#84316,#84317,#84318,#84319,#84320,#84321,#84322,
#84323,#84324,#84325,#84326,#84327,#84328,#84329,#84330,#84331,#84332,#84333,
#84334,#84335,#84336,#84337,#84338,#84339,#84340,#84341,#84342,#84343,#84344,
#84345,#84346,#84347,#84348,#84349,#84350,#84351,#84352,#84353,#84354,#84355,
#84356,#84357,#84358,#84359,#84360,#84361,#84362,#84363,#84364,#84365,#84366,
#84367,#84368,#84369,#84370,#84371,#84372,#84373,#84374,#84375,#84376,#84377,
#84378,#84379,#84380,#84381,#84382,#84383,#84384,#84385,#84386,#84387,#84388,
#84389,#84390,#84391,#84392,#84393,#84394,#84395,#84396,#84397,#84398,#84399,
#84400,#84401,#84402,#84403,#84404,#84405,#84406,#84407,#84408,#84409,#84410,
#84411,#84412,#84413),.UNSPECIFIED.,.F.,.F.,(4,3,3,3,3,3,3,3,3,3,3,3,3,
3,3,3,3,3,3,3,3,3,3,3,3,3,3,3,3,3,3,3,3,3,3,3,3,3,3,4),(-54.3584128775674,
-54.1856448261282,-54.0127120160945,-53.8392756664467,-53.7924418125592,
-53.6231081507439,-53.4541023486374,-53.2851255643338,-53.1161932884612,
-52.9468579311062,-52.796285482697,-52.6269518208817,-52.4579460187752,
-52.2889692344716,-52.120036958599,-51.950701601244,-51.8001291528348,-51.6307954910195,
-51.461789688913,-51.2928129046094,-51.1238806287368,-50.9545452713818,
-50.8039728229726,-50.6346391611574,-50.4656333590508,-50.2966565747472,
-50.1277242988747,-49.9583889415196,-49.8078164931104,-49.6384828312951,
-49.4694770291886,-49.3005002448849,-49.1315679690123,-48.9622326116573,
-48.8116601632482,-48.6440875454568,-48.4768218743308,-48.3097330096438,
-48.1425443209698,-48.0752275703878),.UNSPECIFIED.);
#1128=B_SPLINE_CURVE_WITH_KNOTS('',3,(#84415,#84416,#84417,#84418,#84419,
#84420,#84421,#84422,#84423,#84424,#84425,#84426,#84427,#84428,#84429,#84430,
#84431,#84432,#84433,#84434,#84435,#84436,#84437,#84438,#84439,#84440,#84441,
#84442,#84443,#84444,#84445,#84446,#84447,#84448,#84449,#84450,#84451,#84452,
#84453,#84454,#84455,#84456,#84457,#84458,#84459,#84460,#84461,#84462,#84463,
#84464,#84465,#84466,#84467,#84468,#84469,#84470,#84471,#84472,#84473,#84474,
#84475,#84476,#84477,#84478,#84479,#84480,#84481,#84482,#84483,#84484,#84485,
#84486,#84487,#84488,#84489,#84490,#84491,#84492,#84493,#84494,#84495,#84496,
#84497,#84498,#84499,#84500,#84501,#84502,#84503,#84504,#84505,#84506,#84507,
#84508,#84509,#84510,#84511,#84512,#84513,#84514,#84515,#84516,#84517,#84518,
#84519,#84520,#84521,#84522,#84523,#84524,#84525,#84526,#84527,#84528,#84529,
#84530,#84531,#84532),.UNSPECIFIED.,.F.,.F.,(4,3,3,3,3,3,3,3,3,3,3,3,3,
3,3,3,3,3,3,3,3,3,3,3,3,3,3,3,3,3,3,3,3,3,3,3,3,3,3,4),(-48.0752275700732,
-47.8597259048151,-47.8155038333859,-47.6461701715708,-47.4771643694644,
-47.3081875851609,-47.1392553092885,-46.9699199519336,-46.8193475035237,
-46.6500138417084,-46.4810080396019,-46.3120312552982,-46.1430989794257,
-45.9737636220706,-45.8231911736615,-45.6538575118462,-45.4848517097396,
-45.3158749254359,-45.1469426495634,-44.9776072922083,-44.8270348437993,
-44.657701181984,-44.4886953798776,-44.3197185955739,-44.1507863197014,
-43.9814509623464,-43.8308785139371,-43.6615448521218,-43.4925390500153,
-43.3235622657117,-43.1546299898391,-42.9852946324841,-42.8347221840749,
-42.6653885222596,-42.4963827201531,-42.3274059358494,-42.1584736599769,
-41.9891383026218,-41.8385658542127,-41.7920422632082),.UNSPECIFIED.);
#1129=B_SPLINE_CURVE_WITH_KNOTS('',3,(#84534,#84535,#84536,#84537,#84538,
#84539,#84540,#84541,#84542,#84543,#84544,#84545,#84546,#84547,#84548,#84549,
#84550,#84551,#84552,#84553,#84554,#84555,#84556,#84557,#84558,#84559,#84560,
#84561,#84562,#84563,#84564,#84565,#84566,#84567,#84568,#84569,#84570,#84571,
#84572,#84573,#84574,#84575,#84576,#84577,#84578,#84579,#84580,#84581,#84582,
#84583,#84584,#84585,#84586,#84587,#84588,#84589,#84590,#84591,#84592,#84593,
#84594,#84595,#84596,#84597,#84598,#84599,#84600,#84601,#84602,#84603,#84604,
#84605,#84606,#84607,#84608,#84609,#84610,#84611,#84612,#84613,#84614,#84615,
#84616,#84617,#84618,#84619,#84620,#84621,#84622,#84623,#84624,#84625,#84626,
#84627,#84628,#84629,#84630,#84631,#84632,#84633,#84634,#84635,#84636,#84637,
#84638,#84639,#84640,#84641,#84642,#84643,#84644,#84645,#84646,#84647,#84648),
 .UNSPECIFIED.,.F.,.F.,(4,3,3,3,3,3,3,3,3,3,3,3,3,3,3,3,3,3,3,3,3,3,3,3,
3,3,3,3,3,3,3,3,3,3,3,3,3,3,4),(-41.7920422629071,-41.6239457944974,-41.456165739063,
-41.2884054719728,-41.1206712858633,-40.9525563903589,-40.8424095243505,
-40.6730758625352,-40.5040700604288,-40.3350932761251,-40.1661610002525,
-39.9968256428975,-39.8462531944883,-39.6769195326731,-39.5079137305666,
-39.338936946263,-39.1700046703904,-39.0006693130355,-38.8500968646261,
-38.6807632028108,-38.5117574007042,-38.3427806164005,-38.1738483405279,
-38.0045129831728,-37.8539405347639,-37.6846068729486,-37.5156010708421,
-37.3466242865385,-37.1776920106659,-37.0083566533109,-36.8577842049017,
-36.6884505430866,-36.5194447409802,-36.3504679566768,-36.1815356808044,
-36.0122003234496,-35.8616278750395,-35.6675649622913,-35.5088571949304),
 .UNSPECIFIED.);
#1130=B_SPLINE_CURVE_WITH_KNOTS('',3,(#84650,#84651,#84652,#84653,#84654,
#84655,#84656,#84657,#84658,#84659),.UNSPECIFIED.,.F.,.F.,(4,1,1,1,1,1,
1,4),(-35.5088569560286,-34.8654715451773,-33.869315215315,-32.8731588854528,
-31.8770025555906,-30.8808462257284,-29.8846898958662,-29.225671648849),
 .UNSPECIFIED.);
#1131=B_SPLINE_CURVE_WITH_KNOTS('',3,(#84661,#84662,#84663,#84664,#84665,
#84666,#84667,#84668,#84669,#84670),.UNSPECIFIED.,.F.,.F.,(4,1,1,1,1,1,
1,4),(-29.225671648849,-28.888533566004,-27.8923772361418,-26.8962209062796,
-25.9000645764174,-24.9039082465552,-23.907751916693,-22.9424863416694),
 .UNSPECIFIED.);
#1132=B_SPLINE_CURVE_WITH_KNOTS('',3,(#84672,#84673,#84674,#84675,#84676,
#84677,#84678,#84679,#84680,#84681,#84682),.UNSPECIFIED.,.F.,.F.,(4,1,1,
1,1,1,1,1,4),(-22.9424863416694,-22.9115955868308,-21.9154392569686,-20.9192829271064,
-19.9231265972441,-18.9269702673819,-17.9308139375197,-16.9346576076575,
-16.6593049270061),.UNSPECIFIED.);
#1133=B_SPLINE_CURVE_WITH_KNOTS('',3,(#84684,#84685,#84686,#84687,#84688,
#84689,#84690,#84691,#84692,#84693,#84694,#84695,#84696,#84697,#84698,#84699,
#84700,#84701,#84702,#84703,#84704,#84705,#84706,#84707,#84708,#84709,#84710,
#84711,#84712,#84713,#84714,#84715,#84716,#84717,#84718,#84719,#84720,#84721,
#84722,#84723,#84724,#84725,#84726,#84727,#84728,#84729,#84730,#84731,#84732,
#84733,#84734,#84735,#84736,#84737,#84738,#84739,#84740,#84741,#84742,#84743,
#84744,#84745,#84746,#84747,#84748,#84749,#84750,#84751,#84752,#84753,#84754,
#84755,#84756,#84757,#84758,#84759,#84760,#84761,#84762,#84763,#84764,#84765,
#84766,#84767,#84768,#84769,#84770,#84771,#84772,#84773,#84774,#84775,#84776,
#84777,#84778,#84779,#84780,#84781,#84782,#84783,#84784,#84785,#84786,#84787,
#84788,#84789,#84790,#84791,#84792,#84793,#84794,#84795,#84796,#84797,#84798,
#84799,#84800,#84801),.UNSPECIFIED.,.F.,.F.,(4,3,3,3,3,3,3,3,3,3,3,3,3,
3,3,3,3,3,3,3,3,3,3,3,3,3,3,3,3,3,3,3,3,3,3,3,3,3,3,4),(-16.6593010344898,
-16.4918869660773,-16.3244404407765,-16.1569698807986,-15.9891309057531,
-15.9385012777953,-15.7691675865852,-15.6001617563704,-15.4311849462951,
-15.2622526458884,-15.0929172665271,-14.9423449479331,-14.7730110061835,
-14.6040049222631,-14.4350278574257,-14.2660953012303,-14.0967596698059,
-13.9461886180709,-13.776855645198,-13.6078505312393,-13.4388744238898,
-13.2699428200133,-13.1006081124298,-12.9500322882087,-12.7806982175314,
-12.6116920150786,-12.4427148490098,-12.2737822009037,-12.1044464946493,
-11.9538759583465,-11.7845406294793,-11.6155331455289,-11.4465546816653,
-11.2776207245426,-11.1082837186434,-10.9577196284843,-10.785155110263,
-10.6129857262874,-10.4410898767007,-10.3761157273103),.UNSPECIFIED.);
#1134=B_SPLINE_CURVE_WITH_KNOTS('',3,(#84802,#84803,#84804,#84805,#84806,
#84807,#84808,#84809,#84810,#84811,#84812,#84813,#84814,#84815,#84816,#84817,
#84818,#84819,#84820,#84821,#84822,#84823,#84824,#84825,#84826,#84827,#84828,
#84829,#84830,#84831,#84832,#84833,#84834,#84835,#84836,#84837,#84838,#84839,
#84840,#84841,#84842,#84843,#84844,#84845,#84846,#84847,#84848,#84849,#84850,
#84851,#84852,#84853,#84854,#84855,#84856,#84857,#84858,#84859,#84860,#84861,
#84862,#84863,#84864,#84865,#84866,#84867,#84868,#84869,#84870,#84871,#84872,
#84873,#84874,#84875,#84876,#84877,#84878,#84879,#84880,#84881,#84882,#84883,
#84884,#84885,#84886,#84887,#84888,#84889,#84890,#84891,#84892,#84893,#84894,
#84895,#84896,#84897,#84898,#84899,#84900,#84901,#84902,#84903,#84904,#84905,
#84906,#84907,#84908,#84909,#84910,#84911,#84912,#84913,#84914,#84915,#84916,
#84917,#84918,#84919),.UNSPECIFIED.,.F.,.F.,(4,3,3,3,3,3,3,3,3,3,3,3,3,
3,3,3,3,3,3,3,3,3,3,3,3,3,3,3,3,3,3,3,3,3,3,3,3,3,3,4),(-10.3761157271227,
-10.1914014079995,-10.0053992180424,-9.96156329862207,-9.79222542748429,
-9.62321547087196,-9.45423467460939,-9.28529845800698,-9.11595935874042,
-8.96540696875987,-8.79606394541769,-8.62704866921784,-8.45806237992334,
-8.28912056546132,-8.11977581610114,-7.96925063889766,-7.7999517813462,
-7.63098081674628,-7.46203841417896,-7.29314033051832,-7.12383813689975,
-6.97309430903545,-6.80372247429962,-6.6346788411425,-6.46566528890928,
-6.29669676477763,-6.12732676810572,-5.97693797917325,-5.80755632104186,
-5.63850168868863,-5.46947553628278,-5.30049351124867,-5.13110883596115,
-4.98078164931104,-4.8138683916711,-4.64727985048099,-4.48074211867273,
-4.314230116654,-4.14740991101127,-4.09293042013066),.UNSPECIFIED.);
#1135=B_SPLINE_CURVE_WITH_KNOTS('',3,(#84922,#84923,#84924,#84925,#84926,
#84927,#84928,#84929,#84930,#84931,#84932,#84933,#84934,#84935,#84936,#84937,
#84938,#84939,#84940,#84941,#84942,#84943,#84944,#84945,#84946,#84947,#84948,
#84949,#84950,#84951,#84952,#84953,#84954,#84955,#84956,#84957,#84958,#84959,
#84960,#84961,#84962,#84963,#84964,#84965,#84966,#84967,#84968,#84969,#84970,
#84971,#84972,#84973,#84974,#84975,#84976,#84977,#84978,#84979,#84980,#84981,
#84982,#84983,#84984,#84985,#84986,#84987,#84988,#84989,#84990,#84991,#84992,
#84993,#84994,#84995,#84996,#84997,#84998,#84999,#85000,#85001,#85002,#85003,
#85004,#85005,#85006,#85007,#85008,#85009,#85010,#85011,#85012,#85013,#85014,
#85015,#85016,#85017,#85018,#85019,#85020,#85021,#85022,#85023,#85024,#85025,
#85026,#85027,#85028,#85029,#85030,#85031,#85032,#85033,#85034,#85035,#85036,
#85037,#85038,#85039,#85040,#85041,#85042,#85043,#85044,#85045,#85046,#85047,
#85048,#85049,#85050,#85051,#85052,#85053,#85054,#85055,#85056,#85057,#85058,
#85059,#85060,#85061,#85062,#85063,#85064,#85065,#85066,#85067,#85068,#85069,
#85070,#85071,#85072,#85073,#85074,#85075,#85076,#85077,#85078,#85079,#85080,
#85081),.UNSPECIFIED.,.F.,.F.,(4,2,2,2,2,2,2,2,2,2,2,2,2,2,2,2,2,2,2,2,
2,2,2,2,2,2,2,2,2,2,2,2,2,2,2,2,2,2,2,2,2,2,2,2,2,2,2,2,2,2,2,2,2,2,2,2,
2,2,2,2,2,2,2,2,2,2,2,2,2,2,2,2,2,2,2,2,2,2,2,4),(0.0037894336419437,0.0430356641860205,
0.0816654995582311,0.0944090195370889,0.10028843357464,0.104826742950533,
0.109844865848441,0.118215085431042,0.158714606729488,0.18953617842965,
0.203985206295049,0.213340553110937,0.216833118665897,0.216873434713236,
0.21691409292274,0.216955135511277,0.21699660669252,0.217038552916791,0.217081023126943,
0.21962791747299,0.222392878739332,0.227007458458016,0.244659730636135,
0.283265341964775,0.316028949995482,0.328266850645602,0.334014749141327,
0.338491571663838,0.343480349474412,0.351886723920434,0.39549170993468,
0.432154251058751,0.443340737203487,0.451101966433715,0.454477510257664,
0.456985700903143,0.459871212205737,0.465002090560286,0.495183546490613,
0.501954524685721,0.53129663610334,0.561154378227613,0.568873002424849,
0.57367596829627,0.578130790318737,0.583959426123131,0.597265089807999,
0.652012489915787,0.674374418380701,0.686862979979659,0.69087766331876,
0.693487609183072,0.695821509488802,0.699679311169684,0.709878809040578,
0.754382509818591,0.790721901918114,0.80311274421278,0.808879711359274,
0.813349033484928,0.818306542891483,0.826604873211624,0.863880795845579,
0.916066721898791,0.924649096982799,0.928166674428858,0.930704235403835,
0.933544348212949,0.938544735806543,0.961543109543472,1.02756233922703,
1.03971098335327,1.04542649467273,1.04988097155688,1.05484728448991,1.06322075096602,
1.10523472414197,1.13607244536971,1.15885208833088,1.16366148960649),
 .UNSPECIFIED.);
#1136=B_SPLINE_CURVE_WITH_KNOTS('',3,(#85085,#85086,#85087,#85088,#85089,
#85090,#85091,#85092,#85093,#85094,#85095,#85096,#85097,#85098,#85099,#85100,
#85101,#85102,#85103,#85104,#85105,#85106,#85107,#85108,#85109,#85110,#85111,
#85112,#85113,#85114,#85115,#85116,#85117,#85118,#85119,#85120,#85121,#85122,
#85123,#85124,#85125,#85126,#85127),.UNSPECIFIED.,.F.,.F.,(4,3,3,3,3,3,
3,3,3,3,3,3,3,3,4),(103.672557568796,103.902573542604,103.938485219173,
104.115263612104,104.291682738526,104.468102235349,104.644505119859,104.821378175675,
104.934641549035,105.118296438428,105.301515543515,105.48449990958,105.667333099215,
105.850293575283,105.930797878897),.UNSPECIFIED.);
#1137=B_SPLINE_CURVE_WITH_KNOTS('',3,(#85128,#85129,#85130,#85131,#85132,
#85133,#85134,#85135,#85136,#85137,#85138,#85139,#85140,#85141,#85142,#85143,
#85144,#85145,#85146,#85147,#85148,#85149,#85150,#85151,#85152,#85153,#85154,
#85155,#85156,#85157,#85158,#85159,#85160,#85161,#85162,#85163,#85164,#85165,
#85166,#85167,#85168,#85169,#85170,#85171,#85172,#85173,#85174,#85175,#85176,
#85177),.UNSPECIFIED.,.F.,.F.,(4,2,2,2,2,2,2,2,2,2,2,2,2,2,2,2,2,2,2,2,
2,2,2,2,4),(-2.98914753351539,-2.95921878800075,-2.94518237031271,-2.93931598206595,
-2.93485723662925,-2.93029823022713,-2.92535465387828,-2.91733473317169,
-2.8871990170832,-2.84176481800093,-2.82559177589516,-2.81999954053876,
-2.81687727857855,-2.81432736386882,-2.81108041717311,-2.8041445851037,
-2.77114378395878,-2.74348280282388,-2.71161027045087,-2.70371041291119,
-2.69882975919512,-2.69432439898856,-2.68845850206672,-2.67518725330161,
-2.65783630003039),.UNSPECIFIED.);
#1138=B_SPLINE_CURVE_WITH_KNOTS('',3,(#85181,#85182,#85183,#85184,#85185,
#85186,#85187,#85188,#85189,#85190,#85191,#85192,#85193,#85194,#85195,#85196,
#85197,#85198,#85199,#85200,#85201,#85202,#85203,#85204,#85205,#85206,#85207,
#85208,#85209,#85210,#85211,#85212,#85213,#85214,#85215,#85216,#85217,#85218,
#85219,#85220,#85221,#85222,#85223,#85224,#85225,#85226,#85227,#85228,#85229,
#85230,#85231,#85232,#85233,#85234,#85235,#85236,#85237,#85238),
 .UNSPECIFIED.,.F.,.F.,(4,3,3,3,3,3,3,3,3,3,3,3,3,3,3,3,3,3,3,4),(-0.547417054864566,
-0.53033882791749,-0.495307986319534,-0.475290491773116,-0.447607237097599,
-0.419654534866616,-0.400079102935313,-0.381999937381865,-0.332300949859174,
-0.29983044961068,-0.283628237747696,-0.251952142272621,-0.205914518250308,
-0.18058812353789,-0.13617659674883,-0.103458346379604,-0.0834567189867998,
-0.0389725148624793,-0.00294201638164863,0.),.UNSPECIFIED.);
#1139=B_SPLINE_CURVE_WITH_KNOTS('',3,(#85240,#85241,#85242,#85243),
 .UNSPECIFIED.,.F.,.F.,(4,4),(0.,0.0130412808333173),.UNSPECIFIED.);
#1140=B_SPLINE_CURVE_WITH_KNOTS('',3,(#85244,#85245,#85246,#85247,#85248,
#85249,#85250,#85251,#85252,#85253,#85254,#85255,#85256,#85257,#85258,#85259,
#85260,#85261,#85262,#85263,#85264,#85265,#85266,#85267,#85268,#85269,#85270,
#85271,#85272,#85273,#85274,#85275,#85276,#85277,#85278,#85279,#85280,#85281,
#85282,#85283,#85284,#85285,#85286,#85287,#85288,#85289,#85290,#85291,#85292,
#85293,#85294,#85295,#85296,#85297,#85298,#85299,#85300,#85301),
 .UNSPECIFIED.,.F.,.F.,(4,3,3,3,3,3,3,3,3,3,3,3,3,3,3,3,3,3,3,4),(-0.555272788399386,
-0.536878011109323,-0.499667654095302,-0.47690792776006,-0.441414459291682,
-0.425702691834984,-0.411668346210502,-0.363225278150133,-0.331446939414361,
-0.313088391824243,-0.28194190366226,-0.246699165704478,-0.225030257188244,
-0.2082576414013,-0.156193231050975,-0.129811100532013,-0.111596852253624,
-0.0945316768920992,-0.0422149050010466,0.),.UNSPECIFIED.);
#1141=B_SPLINE_CURVE_WITH_KNOTS('',3,(#85706,#85707,#85708,#85709),
 .UNSPECIFIED.,.F.,.F.,(4,4),(-0.00534461024793257,0.),.UNSPECIFIED.);
#1142=B_SPLINE_CURVE_WITH_KNOTS('',3,(#85710,#85711,#85712,#85713,#85714,
#85715,#85716,#85717,#85718,#85719,#85720,#85721,#85722,#85723,#85724,#85725,
#85726,#85727,#85728,#85729,#85730,#85731,#85732,#85733,#85734,#85735,#85736,
#85737,#85738,#85739,#85740,#85741,#85742,#85743,#85744,#85745,#85746,#85747,
#85748,#85749,#85750,#85751,#85752,#85753,#85754,#85755,#85756,#85757,#85758,
#85759,#85760,#85761,#85762,#85763,#85764,#85765,#85766,#85767),
 .UNSPECIFIED.,.F.,.F.,(4,3,3,3,3,3,3,3,3,3,3,3,3,3,3,3,3,3,3,4),(-0.555272788399383,
-0.536878011109319,-0.49966765582956,-0.476907936094555,-0.441413399121164,
-0.425725415706225,-0.411671954797729,-0.363223558783216,-0.331446021165907,
-0.313087741258502,-0.281941903662256,-0.246699165704475,-0.225030248355765,
-0.208257626954711,-0.156193220216035,-0.129811093853198,-0.111596847794653,
-0.094531660643926,-0.0422148723537678,-6.70332118037912E-15),
 .UNSPECIFIED.);
#1143=B_SPLINE_CURVE_WITH_KNOTS('',3,(#85773,#85774,#85775,#85776,#85777,
#85778,#85779,#85780,#85781,#85782,#85783,#85784,#85785,#85786,#85787,#85788,
#85789,#85790,#85791,#85792,#85793,#85794,#85795,#85796,#85797,#85798,#85799,
#85800,#85801,#85802,#85803,#85804,#85805,#85806,#85807,#85808,#85809,#85810,
#85811,#85812,#85813,#85814,#85815,#85816,#85817,#85818,#85819,#85820,#85821,
#85822,#85823,#85824,#85825,#85826,#85827,#85828,#85829,#85830),
 .UNSPECIFIED.,.F.,.F.,(4,3,3,3,3,3,3,3,3,3,3,3,3,3,3,3,3,3,3,4),(-0.5474172947136,
-0.530338827917456,-0.495308046545021,-0.475290501025032,-0.447608014023609,
-0.419656418536863,-0.400079548458063,-0.382001269621687,-0.332302227775843,
-0.299831205494185,-0.283628559844453,-0.251952142272604,-0.205910804141385,
-0.180596553086976,-0.136182931568932,-0.103452591178888,-0.0834625820348813,
-0.0389782829583399,-0.00294206701479738,0.),.UNSPECIFIED.);
#1144=B_SPLINE_CURVE_WITH_KNOTS('',3,(#86235,#86236,#86237,#86238),
 .UNSPECIFIED.,.F.,.F.,(4,4),(0.,0.00538265464589753),.UNSPECIFIED.);
#1145=CONICAL_SURFACE('',#15935,5.75,0.785398163397448);
#1146=CONICAL_SURFACE('',#15938,0.85,0.78539816339745);
#1147=CONICAL_SURFACE('',#15944,0.85,0.78539816339745);
#1148=CONICAL_SURFACE('',#15947,5.75,0.785398163397453);
#1149=CONICAL_SURFACE('',#15950,0.85,0.78539816339745);
#1150=CONICAL_SURFACE('',#15956,0.85,0.78539816339745);
#1151=CONICAL_SURFACE('',#15959,5.75,0.785398163397448);
#1152=CONICAL_SURFACE('',#15962,0.85,0.785398163397452);
#1153=CONICAL_SURFACE('',#15965,5.75,0.785398163397448);
#1154=CONICAL_SURFACE('',#15968,0.85,0.785398163397452);
#1155=CONICAL_SURFACE('',#15985,0.5575,0.785398163397445);
#1156=CONICAL_SURFACE('',#15987,0.2025,1.02974425867666);
#1157=CONICAL_SURFACE('',#15991,0.455,0.785398163397457);
#1158=CONICAL_SURFACE('',#16001,0.2025,1.02974425867666);
#1159=CONICAL_SURFACE('',#16005,0.455000000000001,0.785398163397459);
#1160=CONICAL_SURFACE('',#16008,0.2025,1.02974425867666);
#1161=CONICAL_SURFACE('',#16012,0.455,0.785398163397457);
#1162=CONICAL_SURFACE('',#16015,0.2025,1.02974425867666);
#1163=CONICAL_SURFACE('',#16019,0.455000000000001,0.785398163397459);
#1164=CONICAL_SURFACE('',#16020,0.1525,1.02974425867665);
#1165=CONICAL_SURFACE('',#16024,0.355,0.785398163397444);
#1166=CONICAL_SURFACE('',#16025,0.1525,1.02974425867665);
#1167=CONICAL_SURFACE('',#16029,0.355,0.785398163397446);
#1168=CONICAL_SURFACE('',#16031,0.1525,1.02974425867665);
#1169=CONICAL_SURFACE('',#16035,0.355,0.785398163397446);
#1170=CONICAL_SURFACE('',#16036,0.1525,1.02974425867665);
#1171=CONICAL_SURFACE('',#16040,0.355,0.785398163397444);
#1172=CONICAL_SURFACE('',#16042,0.1525,1.02974425867665);
#1173=CONICAL_SURFACE('',#16046,0.355,0.785398163397444);
#1174=CONICAL_SURFACE('',#16047,0.1525,1.02974425867665);
#1175=CONICAL_SURFACE('',#16051,0.355,0.785398163397444);
#1176=CONICAL_SURFACE('',#16053,0.1525,1.02974425867665);
#1177=CONICAL_SURFACE('',#16057,0.355,0.785398163397444);
#1178=CONICAL_SURFACE('',#16058,0.1525,1.02974425867665);
#1179=CONICAL_SURFACE('',#16062,0.355,0.785398163397444);
#1180=CONICAL_SURFACE('',#16064,0.1525,1.02974425867665);
#1181=CONICAL_SURFACE('',#16068,0.355,0.785398163397451);
#1182=CONICAL_SURFACE('',#16069,0.1525,1.02974425867665);
#1183=CONICAL_SURFACE('',#16073,0.355,0.785398163397448);
#1184=CONICAL_SURFACE('',#16074,0.1525,1.02974425867665);
#1185=CONICAL_SURFACE('',#16078,0.355,0.785398163397451);
#1186=CONICAL_SURFACE('',#16079,0.1525,1.02974425867665);
#1187=CONICAL_SURFACE('',#16083,0.355,0.785398163397448);
#1188=CONICAL_SURFACE('',#16087,0.462499999999999,0.785398163397447);
#1189=CONICAL_SURFACE('',#16092,0.4625,0.785398163397444);
#1190=CONICAL_SURFACE('',#16097,0.462499999999999,0.785398163397447);
#1191=CONICAL_SURFACE('',#16102,0.4625,0.785398163397444);
#1192=CONICAL_SURFACE('',#16199,3.155,0.785398163397444);
#1193=CONICAL_SURFACE('',#16204,5.245,0.785398163397446);
#1194=CONICAL_SURFACE('',#16211,5.75,0.785398163397448);
#1195=CONICAL_SURFACE('',#16214,0.85,0.785398163397452);
#1196=CONICAL_SURFACE('',#16217,5.75,0.785398163397448);
#1197=CONICAL_SURFACE('',#16220,0.85,0.785398163397451);
#1198=CONICAL_SURFACE('',#16223,5.75,0.785398163397453);
#1199=CONICAL_SURFACE('',#16226,0.85,0.785398163397449);
#1200=CONICAL_SURFACE('',#16229,5.75,0.785398163397448);
#1201=CONICAL_SURFACE('',#16232,0.85,0.785398163397452);
#1202=CONICAL_SURFACE('',#16249,0.342499999999999,0.32175055439664);
#1203=CONICAL_SURFACE('',#16254,0.342499999999999,0.785398163397439);
#1204=CONICAL_SURFACE('',#16259,0.342499999999999,0.321750554396635);
#1205=CONICAL_SURFACE('',#16264,0.342499999999999,0.785398163397431);
#1206=CONICAL_SURFACE('',#16269,0.342499999999999,0.321750554396635);
#1207=CONICAL_SURFACE('',#16274,0.342499999999999,0.785398163397431);
#1208=CONICAL_SURFACE('',#16279,0.342499999999999,0.321750554396635);
#1209=CONICAL_SURFACE('',#16284,0.342499999999999,0.785398163397431);
#1210=CONICAL_SURFACE('',#16289,3.155,0.785398163397444);
#1211=CONICAL_SURFACE('',#16324,0.3425,0.321750554396649);
#1212=CONICAL_SURFACE('',#16329,0.3425,0.785398163397466);
#1213=CONICAL_SURFACE('',#16335,0.3425,0.321750554396644);
#1214=CONICAL_SURFACE('',#16340,0.3425,0.785398163397457);
#1215=CONICAL_SURFACE('',#16346,0.3425,0.321750554396649);
#1216=CONICAL_SURFACE('',#16351,0.3425,0.785398163397466);
#1217=CONICAL_SURFACE('',#16357,0.3425,0.321750554396644);
#1218=CONICAL_SURFACE('',#16362,0.3425,0.785398163397457);
#1219=CONICAL_SURFACE('',#16368,0.49,0.785398163397448);
#1220=CONICAL_SURFACE('',#16373,0.49,0.785398163397443);
#1221=CONICAL_SURFACE('',#16374,0.49,0.785398163397448);
#1222=CONICAL_SURFACE('',#16379,0.49,0.785398163397443);
#1223=CONICAL_SURFACE('',#16380,0.49,0.785398163397448);
#1224=CONICAL_SURFACE('',#16385,0.49,0.785398163397443);
#1225=CONICAL_SURFACE('',#16386,0.49,0.785398163397448);
#1226=CONICAL_SURFACE('',#16391,0.49,0.785398163397443);
#1227=CONICAL_SURFACE('',#16438,0.74,0.785398163397459);
#1228=CONICAL_SURFACE('',#16440,0.35,1.02974425867665);
#1229=CONICAL_SURFACE('',#16444,1.764,0.7936624380571);
#1230=CONICAL_SURFACE('',#16445,1.764,0.7936624380571);
#1231=CONICAL_SURFACE('',#16453,1.21,0.785398163397459);
#1232=CONICAL_SURFACE('',#16459,1.525,0.785398163397448);
#1233=CONICAL_SURFACE('',#16468,1.525,0.785398163397448);
#1234=CONICAL_SURFACE('',#16474,1.21,0.785398163397459);
#1235=CONICAL_SURFACE('',#16478,3.325,0.785398163397446);
#1236=CONICAL_SURFACE('',#16516,3.325,0.785398163397448);
#1237=CONICAL_SURFACE('',#16549,4.9,0.785398163397446);
#1238=CONICAL_SURFACE('',#16557,4.9,0.785398163397446);
#1239=CONICAL_SURFACE('',#16558,4.9,0.785398163397446);
#1240=CONICAL_SURFACE('',#16566,4.9,0.785398163397446);
#1241=CONICAL_SURFACE('',#16567,4.9,0.785398163397446);
#1242=CONICAL_SURFACE('',#16575,4.9,0.785398163397446);
#1243=CONICAL_SURFACE('',#16576,4.9,0.785398163397446);
#1244=CONICAL_SURFACE('',#16584,4.9,0.785398163397446);
#1245=CONICAL_SURFACE('',#16585,4.9,0.785398163397446);
#1246=CONICAL_SURFACE('',#16593,4.9,0.785398163397446);
#1247=CONICAL_SURFACE('',#16594,4.9,0.785398163397446);
#1248=CONICAL_SURFACE('',#16602,4.9,0.785398163397446);
#1249=CONICAL_SURFACE('',#16603,4.9,0.785398163397446);
#1250=CONICAL_SURFACE('',#16611,4.9,0.785398163397446);
#1251=CONICAL_SURFACE('',#16612,4.9,0.785398163397446);
#1252=CONICAL_SURFACE('',#16620,4.9,0.785398163397446);
#1253=CONICAL_SURFACE('',#16621,4.9,0.785398163397446);
#1254=CONICAL_SURFACE('',#16629,4.9,0.785398163397446);
#1255=CONICAL_SURFACE('',#16630,4.9,0.785398163397446);
#1256=CONICAL_SURFACE('',#16638,4.9,0.785398163397446);
#1257=CONICAL_SURFACE('',#16639,4.9,0.785398163397446);
#1258=CONICAL_SURFACE('',#16647,4.9,0.785398163397446);
#1259=CONICAL_SURFACE('',#16648,4.9,0.785398163397446);
#1260=CONICAL_SURFACE('',#16656,4.9,0.785398163397446);
#1261=CONICAL_SURFACE('',#16657,4.9,0.785398163397446);
#1262=CONICAL_SURFACE('',#16665,4.9,0.785398163397446);
#1263=CONICAL_SURFACE('',#16666,4.9,0.785398163397446);
#1264=CONICAL_SURFACE('',#16674,4.9,0.785398163397446);
#1265=CONICAL_SURFACE('',#16675,4.9,0.785398163397446);
#1266=CONICAL_SURFACE('',#16683,4.9,0.785398163397446);
#1267=CONICAL_SURFACE('',#16684,4.9,0.785398163397446);
#1268=CONICAL_SURFACE('',#16692,4.9,0.785398163397446);
#1269=CONICAL_SURFACE('',#16693,4.9,0.785398163397446);
#1270=CONICAL_SURFACE('',#16701,4.9,0.785398163397446);
#1271=CONICAL_SURFACE('',#16702,4.9,0.785398163397446);
#1272=CONICAL_SURFACE('',#16710,4.9,0.785398163397446);
#1273=CONICAL_SURFACE('',#16711,4.9,0.785398163397446);
#1274=CONICAL_SURFACE('',#16719,4.9,0.785398163397446);
#1275=CONICAL_SURFACE('',#16720,4.9,0.785398163397446);
#1276=CONICAL_SURFACE('',#16728,4.9,0.785398163397446);
#1277=CONICAL_SURFACE('',#16729,4.9,0.785398163397446);
#1278=CONICAL_SURFACE('',#16737,4.9,0.785398163397446);
#1279=CONICAL_SURFACE('',#16738,4.9,0.785398163397446);
#1280=CONICAL_SURFACE('',#16746,4.9,0.785398163397446);
#1281=CONICAL_SURFACE('',#16747,4.9,0.785398163397446);
#1282=CONICAL_SURFACE('',#16755,4.9,0.785398163397446);
#1283=CONICAL_SURFACE('',#16756,4.9,0.785398163397446);
#1284=CONICAL_SURFACE('',#16764,4.9,0.785398163397446);
#1285=CONICAL_SURFACE('',#16765,4.9,0.785398163397446);
#1286=CONICAL_SURFACE('',#16773,4.9,0.785398163397446);
#1287=CONICAL_SURFACE('',#16774,4.9,0.785398163397446);
#1288=CONICAL_SURFACE('',#16782,4.9,0.785398163397446);
#1289=CONICAL_SURFACE('',#16783,4.9,0.785398163397446);
#1290=CONICAL_SURFACE('',#16791,4.9,0.785398163397446);
#1291=CONICAL_SURFACE('',#16792,4.9,0.785398163397446);
#1292=CONICAL_SURFACE('',#16794,4.9,0.785398163397446);
#1293=CONICAL_SURFACE('',#16802,4.9,0.785398163397446);
#1294=CONICAL_SURFACE('',#16803,4.9,0.785398163397446);
#1295=CONICAL_SURFACE('',#16809,4.9,0.785398163397446);
#1296=CONICAL_SURFACE('',#16818,4.9,0.785398163397446);
#1297=CONICAL_SURFACE('',#16826,1.3,0.785398163397457);
#1298=CONICAL_SURFACE('',#16828,2.21,0.785398163397443);
#1299=CONICAL_SURFACE('',#16834,2.575,0.785398163397453);
#1300=CONICAL_SURFACE('',#16846,2.575,0.785398163397453);
#1301=CONICAL_SURFACE('',#16852,2.21,0.785398163397443);
#1302=CONICAL_SURFACE('',#16856,1.3,0.785398163397457);
#1303=CONICAL_SURFACE('',#16863,2.575,0.785398163397451);
#1304=CONICAL_SURFACE('',#16867,2.58,0.785398163397448);
#1305=CONICAL_SURFACE('',#16875,1.325,0.785398163397448);
#1306=CONICAL_SURFACE('',#16879,1.35,1.10714871779409);
#1307=CONICAL_SURFACE('',#16881,1.525,0.643501108793285);
#1308=CONICAL_SURFACE('',#16899,2.58,0.785398163397448);
#1309=CONICAL_SURFACE('',#16920,0.320138837486628,1.0471975511966);
#1310=CONICAL_SURFACE('',#16925,0.1225,1.0267507402002);
#1311=CONICAL_SURFACE('',#16933,0.465,0.785398163397448);
#1312=CONICAL_SURFACE('',#16941,0.69,0.785398163397449);
#1313=CONICAL_SURFACE('',#16945,0.68,0.785398163397449);
#1314=CONICAL_SURFACE('',#16949,0.515,0.785398163397449);
#1315=CONICAL_SURFACE('',#16954,0.695,0.785398163397443);
#1316=CONICAL_SURFACE('',#16958,0.695,0.785398163397443);
#1317=CONICAL_SURFACE('',#16962,0.515,0.785398163397448);
#1318=CONICAL_SURFACE('',#16971,0.68,0.785398163397448);
#1319=CONICAL_SURFACE('',#16977,1.875,0.785398163397447);
#1320=CONICAL_SURFACE('',#16981,1.88,0.785398163397446);
#1321=CONICAL_SURFACE('',#17007,1.28,0.785398163397449);
#1322=CONICAL_SURFACE('',#17011,1.99,1.40138328290528);
#1323=CONICAL_SURFACE('',#17013,2.21,0.785398163397445);
#1324=CONICAL_SURFACE('',#17016,2.57,0.785398163397449);
#1325=CONICAL_SURFACE('',#17020,2.57,0.785398163397448);
#1326=CONICAL_SURFACE('',#17027,1.28,0.785398163397448);
#1327=CONICAL_SURFACE('',#17032,2.28,0.785398163397449);
#1328=CONICAL_SURFACE('',#17044,3.72,0.785398163397449);
#1329=CONICAL_SURFACE('',#17048,3.72,0.785398163397448);
#1330=CONICAL_SURFACE('',#17060,2.28,0.785398163397448);
#1331=CONICAL_SURFACE('',#17065,3.075,0.785398163397451);
#1332=CONICAL_SURFACE('',#17069,3.08,0.785398163397448);
#1333=CONICAL_SURFACE('',#17077,2.325,0.722979353401491);
#1334=CONICAL_SURFACE('',#17081,2.35,1.03037682652431);
#1335=CONICAL_SURFACE('',#17083,2.525,0.558599315343562);
#1336=CONICAL_SURFACE('',#17085,0.135,0.785398163397449);
#1337=CONICAL_SURFACE('',#17098,0.135,0.785398163397448);
#1338=CONICAL_SURFACE('',#17108,0.135,0.785398163397449);
#1339=CONICAL_SURFACE('',#17112,0.135,0.785398163397448);
#1340=CONICAL_SURFACE('',#17159,0.320138837486628,1.0471975511966);
#1341=CONICAL_SURFACE('',#17164,0.1225,1.0267507402002);
#1342=CONICAL_SURFACE('',#17179,0.2775,0.785398163397449);
#1343=CONICAL_SURFACE('',#17180,0.49,0.785398163397449);
#1344=CONICAL_SURFACE('',#17215,0.320138837486628,1.0471975511966);
#1345=CONICAL_SURFACE('',#17220,0.1225,1.0267507402002);
#1346=CONICAL_SURFACE('',#17235,0.2775,0.785398163397449);
#1347=CONICAL_SURFACE('',#17236,0.49,0.785398163397449);
#1348=CONICAL_SURFACE('',#17243,1.23,0.785398163397448);
#1349=CONICAL_SURFACE('',#17249,1.575,0.785398163397449);
#1350=CONICAL_SURFACE('',#17253,1.58,0.785398163397449);
#1351=CYLINDRICAL_SURFACE('',#15906,5.8);
#1352=CYLINDRICAL_SURFACE('',#15909,0.9);
#1353=CYLINDRICAL_SURFACE('',#15915,0.9);
#1354=CYLINDRICAL_SURFACE('',#15971,0.9);
#1355=CYLINDRICAL_SURFACE('',#15972,5.8);
#1356=CYLINDRICAL_SURFACE('',#15973,0.9);
#1357=CYLINDRICAL_SURFACE('',#15974,5.8);
#1358=CYLINDRICAL_SURFACE('',#15975,0.9);
#1359=CYLINDRICAL_SURFACE('',#15976,5.8);
#1360=CYLINDRICAL_SURFACE('',#15983,0.505);
#1361=CYLINDRICAL_SURFACE('',#15989,0.405);
#1362=CYLINDRICAL_SURFACE('',#16003,0.405);
#1363=CYLINDRICAL_SURFACE('',#16006,0.6);
#1364=CYLINDRICAL_SURFACE('',#16010,0.405);
#1365=CYLINDRICAL_SURFACE('',#16013,0.6);
#1366=CYLINDRICAL_SURFACE('',#16017,0.405);
#1367=CYLINDRICAL_SURFACE('',#16022,0.305);
#1368=CYLINDRICAL_SURFACE('',#16027,0.305);
#1369=CYLINDRICAL_SURFACE('',#16033,0.305);
#1370=CYLINDRICAL_SURFACE('',#16038,0.305);
#1371=CYLINDRICAL_SURFACE('',#16044,0.305);
#1372=CYLINDRICAL_SURFACE('',#16049,0.305);
#1373=CYLINDRICAL_SURFACE('',#16055,0.305);
#1374=CYLINDRICAL_SURFACE('',#16060,0.305);
#1375=CYLINDRICAL_SURFACE('',#16066,0.305);
#1376=CYLINDRICAL_SURFACE('',#16071,0.305);
#1377=CYLINDRICAL_SURFACE('',#16076,0.305);
#1378=CYLINDRICAL_SURFACE('',#16081,0.305);
#1379=CYLINDRICAL_SURFACE('',#16084,0.425);
#1380=CYLINDRICAL_SURFACE('',#16089,0.425000000000001);
#1381=CYLINDRICAL_SURFACE('',#16094,0.425);
#1382=CYLINDRICAL_SURFACE('',#16099,0.425000000000001);
#1383=CYLINDRICAL_SURFACE('',#16120,0.9);
#1384=CYLINDRICAL_SURFACE('',#16122,0.9);
#1385=CYLINDRICAL_SURFACE('',#16123,0.9);
#1386=CYLINDRICAL_SURFACE('',#16164,2.6);
#1387=CYLINDRICAL_SURFACE('',#16168,2.75);
#1388=CYLINDRICAL_SURFACE('',#16172,2.6);
#1389=CYLINDRICAL_SURFACE('',#16176,2.3);
#1390=CYLINDRICAL_SURFACE('',#16180,2.6);
#1391=CYLINDRICAL_SURFACE('',#16184,2.75);
#1392=CYLINDRICAL_SURFACE('',#16188,2.6);
#1393=CYLINDRICAL_SURFACE('',#16189,5.3);
#1394=CYLINDRICAL_SURFACE('',#16193,3.75);
#1395=CYLINDRICAL_SURFACE('',#16197,3.1);
#1396=CYLINDRICAL_SURFACE('',#16200,5.8);
#1397=CYLINDRICAL_SURFACE('',#16201,0.6);
#1398=CYLINDRICAL_SURFACE('',#16202,0.6);
#1399=CYLINDRICAL_SURFACE('',#16207,5.295);
#1400=CYLINDRICAL_SURFACE('',#16235,0.9);
#1401=CYLINDRICAL_SURFACE('',#16237,5.8);
#1402=CYLINDRICAL_SURFACE('',#16239,0.9);
#1403=CYLINDRICAL_SURFACE('',#16241,5.8);
#1404=CYLINDRICAL_SURFACE('',#16252,0.33);
#1405=CYLINDRICAL_SURFACE('',#16258,0.55);
#1406=CYLINDRICAL_SURFACE('',#16262,0.33);
#1407=CYLINDRICAL_SURFACE('',#16268,0.55);
#1408=CYLINDRICAL_SURFACE('',#16272,0.33);
#1409=CYLINDRICAL_SURFACE('',#16278,0.55);
#1410=CYLINDRICAL_SURFACE('',#16282,0.33);
#1411=CYLINDRICAL_SURFACE('',#16288,0.55);
#1412=CYLINDRICAL_SURFACE('',#16291,3.1);
#1413=CYLINDRICAL_SURFACE('',#16295,3.75);
#1414=CYLINDRICAL_SURFACE('',#16296,0.9);
#1415=CYLINDRICAL_SURFACE('',#16298,5.8);
#1416=CYLINDRICAL_SURFACE('',#16300,0.9);
#1417=CYLINDRICAL_SURFACE('',#16302,5.8);
#1418=CYLINDRICAL_SURFACE('',#16327,0.33);
#1419=CYLINDRICAL_SURFACE('',#16333,0.55);
#1420=CYLINDRICAL_SURFACE('',#16338,0.33);
#1421=CYLINDRICAL_SURFACE('',#16344,0.55);
#1422=CYLINDRICAL_SURFACE('',#16349,0.33);
#1423=CYLINDRICAL_SURFACE('',#16355,0.55);
#1424=CYLINDRICAL_SURFACE('',#16360,0.33);
#1425=CYLINDRICAL_SURFACE('',#16366,0.55);
#1426=CYLINDRICAL_SURFACE('',#16371,0.45);
#1427=CYLINDRICAL_SURFACE('',#16377,0.45);
#1428=CYLINDRICAL_SURFACE('',#16383,0.45);
#1429=CYLINDRICAL_SURFACE('',#16389,0.45);
#1430=CYLINDRICAL_SURFACE('',#16408,2.);
#1431=CYLINDRICAL_SURFACE('',#16411,5.501);
#1432=CYLINDRICAL_SURFACE('',#16420,1.4);
#1433=CYLINDRICAL_SURFACE('',#16422,1.4);
#1434=CYLINDRICAL_SURFACE('',#16423,1.4);
#1435=CYLINDRICAL_SURFACE('',#16424,1.4);
#1436=CYLINDRICAL_SURFACE('',#16425,1.4);
#1437=CYLINDRICAL_SURFACE('',#16426,1.4);
#1438=CYLINDRICAL_SURFACE('',#16427,1.4);
#1439=CYLINDRICAL_SURFACE('',#16434,0.699999999999999);
#1440=CYLINDRICAL_SURFACE('',#16441,1.398);
#1441=CYLINDRICAL_SURFACE('',#16447,1.398);
#1442=CYLINDRICAL_SURFACE('',#16455,1.25);
#1443=CYLINDRICAL_SURFACE('',#16461,1.55);
#1444=CYLINDRICAL_SURFACE('',#16466,1.55);
#1445=CYLINDRICAL_SURFACE('',#16472,1.25);
#1446=CYLINDRICAL_SURFACE('',#16482,3.3);
#1447=CYLINDRICAL_SURFACE('',#16551,4.95);
#1448=CYLINDRICAL_SURFACE('',#16555,4.95);
#1449=CYLINDRICAL_SURFACE('',#16560,4.95);
#1450=CYLINDRICAL_SURFACE('',#16564,4.95);
#1451=CYLINDRICAL_SURFACE('',#16569,4.95);
#1452=CYLINDRICAL_SURFACE('',#16573,4.95);
#1453=CYLINDRICAL_SURFACE('',#16578,4.95);
#1454=CYLINDRICAL_SURFACE('',#16582,4.95);
#1455=CYLINDRICAL_SURFACE('',#16587,4.95);
#1456=CYLINDRICAL_SURFACE('',#16591,4.95);
#1457=CYLINDRICAL_SURFACE('',#16596,4.95);
#1458=CYLINDRICAL_SURFACE('',#16600,4.95);
#1459=CYLINDRICAL_SURFACE('',#16605,4.95);
#1460=CYLINDRICAL_SURFACE('',#16609,4.95);
#1461=CYLINDRICAL_SURFACE('',#16614,4.95);
#1462=CYLINDRICAL_SURFACE('',#16618,4.95);
#1463=CYLINDRICAL_SURFACE('',#16623,4.95);
#1464=CYLINDRICAL_SURFACE('',#16627,4.95);
#1465=CYLINDRICAL_SURFACE('',#16632,4.95);
#1466=CYLINDRICAL_SURFACE('',#16636,4.95);
#1467=CYLINDRICAL_SURFACE('',#16641,4.95);
#1468=CYLINDRICAL_SURFACE('',#16645,4.95);
#1469=CYLINDRICAL_SURFACE('',#16650,4.95);
#1470=CYLINDRICAL_SURFACE('',#16654,4.95);
#1471=CYLINDRICAL_SURFACE('',#16659,4.95);
#1472=CYLINDRICAL_SURFACE('',#16663,4.95);
#1473=CYLINDRICAL_SURFACE('',#16668,4.95);
#1474=CYLINDRICAL_SURFACE('',#16672,4.95);
#1475=CYLINDRICAL_SURFACE('',#16677,4.95);
#1476=CYLINDRICAL_SURFACE('',#16681,4.95);
#1477=CYLINDRICAL_SURFACE('',#16686,4.95);
#1478=CYLINDRICAL_SURFACE('',#16690,4.95);
#1479=CYLINDRICAL_SURFACE('',#16695,4.95);
#1480=CYLINDRICAL_SURFACE('',#16699,4.95);
#1481=CYLINDRICAL_SURFACE('',#16704,4.95);
#1482=CYLINDRICAL_SURFACE('',#16708,4.95);
#1483=CYLINDRICAL_SURFACE('',#16713,4.95);
#1484=CYLINDRICAL_SURFACE('',#16717,4.95);
#1485=CYLINDRICAL_SURFACE('',#16722,4.95);
#1486=CYLINDRICAL_SURFACE('',#16726,4.95);
#1487=CYLINDRICAL_SURFACE('',#16731,4.95);
#1488=CYLINDRICAL_SURFACE('',#16735,4.95);
#1489=CYLINDRICAL_SURFACE('',#16740,4.95);
#1490=CYLINDRICAL_SURFACE('',#16744,4.95);
#1491=CYLINDRICAL_SURFACE('',#16749,4.95);
#1492=CYLINDRICAL_SURFACE('',#16753,4.95);
#1493=CYLINDRICAL_SURFACE('',#16758,4.95);
#1494=CYLINDRICAL_SURFACE('',#16762,4.95);
#1495=CYLINDRICAL_SURFACE('',#16767,4.95);
#1496=CYLINDRICAL_SURFACE('',#16771,4.95);
#1497=CYLINDRICAL_SURFACE('',#16776,4.95);
#1498=CYLINDRICAL_SURFACE('',#16780,4.95);
#1499=CYLINDRICAL_SURFACE('',#16785,4.95);
#1500=CYLINDRICAL_SURFACE('',#16789,4.95);
#1501=CYLINDRICAL_SURFACE('',#16796,4.95);
#1502=CYLINDRICAL_SURFACE('',#16800,4.95);
#1503=CYLINDRICAL_SURFACE('',#16805,4.95);
#1504=CYLINDRICAL_SURFACE('',#16807,4.95);
#1505=CYLINDRICAL_SURFACE('',#16813,4.95);
#1506=CYLINDRICAL_SURFACE('',#16814,4.95);
#1507=CYLINDRICAL_SURFACE('',#16830,2.25);
#1508=CYLINDRICAL_SURFACE('',#16836,2.6);
#1509=CYLINDRICAL_SURFACE('',#16840,3.3);
#1510=CYLINDRICAL_SURFACE('',#16844,2.6);
#1511=CYLINDRICAL_SURFACE('',#16850,2.25);
#1512=CYLINDRICAL_SURFACE('',#16858,1.25);
#1513=CYLINDRICAL_SURFACE('',#16865,2.6);
#1514=CYLINDRICAL_SURFACE('',#16871,1.7);
#1515=CYLINDRICAL_SURFACE('',#16877,1.25);
#1516=CYLINDRICAL_SURFACE('',#16883,1.);
#1517=CYLINDRICAL_SURFACE('',#16888,1.12);
#1518=CYLINDRICAL_SURFACE('',#16892,2.52);
#1519=CYLINDRICAL_SURFACE('',#16897,2.6);
#1520=CYLINDRICAL_SURFACE('',#16903,0.4372);
#1521=CYLINDRICAL_SURFACE('',#16905,0.4372);
#1522=CYLINDRICAL_SURFACE('',#16906,0.4372);
#1523=CYLINDRICAL_SURFACE('',#16907,0.4372);
#1524=CYLINDRICAL_SURFACE('',#16908,0.4372);
#1525=CYLINDRICAL_SURFACE('',#16909,0.4372);
#1526=CYLINDRICAL_SURFACE('',#16910,0.4942);
#1527=CYLINDRICAL_SURFACE('',#16913,0.4372);
#1528=CYLINDRICAL_SURFACE('',#16937,0.44);
#1529=CYLINDRICAL_SURFACE('',#16943,0.7);
#1530=CYLINDRICAL_SURFACE('',#16956,0.7);
#1531=CYLINDRICAL_SURFACE('',#16964,0.51);
#1532=CYLINDRICAL_SURFACE('',#16966,0.55);
#1533=CYLINDRICAL_SURFACE('',#16973,0.7);
#1534=CYLINDRICAL_SURFACE('',#16979,1.9);
#1535=CYLINDRICAL_SURFACE('',#16986,2.26);
#1536=CYLINDRICAL_SURFACE('',#16989,2.3);
#1537=CYLINDRICAL_SURFACE('',#16993,1.68);
#1538=CYLINDRICAL_SURFACE('',#16998,1.72);
#1539=CYLINDRICAL_SURFACE('',#17004,1.25);
#1540=CYLINDRICAL_SURFACE('',#17018,2.6);
#1541=CYLINDRICAL_SURFACE('',#17024,1.95);
#1542=CYLINDRICAL_SURFACE('',#17029,2.25);
#1543=CYLINDRICAL_SURFACE('',#17036,2.67);
#1544=CYLINDRICAL_SURFACE('',#17040,3.18);
#1545=CYLINDRICAL_SURFACE('',#17046,3.75);
#1546=CYLINDRICAL_SURFACE('',#17052,3.18);
#1547=CYLINDRICAL_SURFACE('',#17056,2.67);
#1548=CYLINDRICAL_SURFACE('',#17067,3.1);
#1549=CYLINDRICAL_SURFACE('',#17073,2.65);
#1550=CYLINDRICAL_SURFACE('',#17079,2.25);
#1551=CYLINDRICAL_SURFACE('',#17088,0.125);
#1552=CYLINDRICAL_SURFACE('',#17110,0.125);
#1553=CYLINDRICAL_SURFACE('',#17115,2.345);
#1554=CYLINDRICAL_SURFACE('',#17116,0.3);
#1555=CYLINDRICAL_SURFACE('',#17117,2.345);
#1556=CYLINDRICAL_SURFACE('',#17118,0.3);
#1557=CYLINDRICAL_SURFACE('',#17119,2.345);
#1558=CYLINDRICAL_SURFACE('',#17120,2.75);
#1559=CYLINDRICAL_SURFACE('',#17122,0.237175);
#1560=CYLINDRICAL_SURFACE('',#17124,0.237175);
#1561=CYLINDRICAL_SURFACE('',#17125,0.237175);
#1562=CYLINDRICAL_SURFACE('',#17126,0.237175);
#1563=CYLINDRICAL_SURFACE('',#17127,0.237175);
#1564=CYLINDRICAL_SURFACE('',#17128,0.237175);
#1565=CYLINDRICAL_SURFACE('',#17129,0.237175);
#1566=CYLINDRICAL_SURFACE('',#17130,0.237175);
#1567=CYLINDRICAL_SURFACE('',#17131,0.237175);
#1568=CYLINDRICAL_SURFACE('',#17132,0.237175);
#1569=CYLINDRICAL_SURFACE('',#17133,0.237175);
#1570=CYLINDRICAL_SURFACE('',#17134,0.237175);
#1571=CYLINDRICAL_SURFACE('',#17135,0.237175);
#1572=CYLINDRICAL_SURFACE('',#17136,0.237175);
#1573=CYLINDRICAL_SURFACE('',#17137,0.237175);
#1574=CYLINDRICAL_SURFACE('',#17138,0.237175);
#1575=CYLINDRICAL_SURFACE('',#17139,0.237175);
#1576=CYLINDRICAL_SURFACE('',#17140,0.237175);
#1577=CYLINDRICAL_SURFACE('',#17141,0.237175);
#1578=CYLINDRICAL_SURFACE('',#17142,0.2942);
#1579=CYLINDRICAL_SURFACE('',#17147,0.237175);
#1580=CYLINDRICAL_SURFACE('',#17174,0.5);
#1581=CYLINDRICAL_SURFACE('',#17182,0.237175);
#1582=CYLINDRICAL_SURFACE('',#17184,0.237175);
#1583=CYLINDRICAL_SURFACE('',#17185,0.237175);
#1584=CYLINDRICAL_SURFACE('',#17186,0.237175);
#1585=CYLINDRICAL_SURFACE('',#17187,0.237175);
#1586=CYLINDRICAL_SURFACE('',#17188,0.237175);
#1587=CYLINDRICAL_SURFACE('',#17189,0.237175);
#1588=CYLINDRICAL_SURFACE('',#17190,0.237175);
#1589=CYLINDRICAL_SURFACE('',#17191,0.237175);
#1590=CYLINDRICAL_SURFACE('',#17192,0.237175);
#1591=CYLINDRICAL_SURFACE('',#17193,0.237175);
#1592=CYLINDRICAL_SURFACE('',#17194,0.237175);
#1593=CYLINDRICAL_SURFACE('',#17195,0.237175);
#1594=CYLINDRICAL_SURFACE('',#17196,0.237175);
#1595=CYLINDRICAL_SURFACE('',#17197,0.237175);
#1596=CYLINDRICAL_SURFACE('',#17198,0.2942);
#1597=CYLINDRICAL_SURFACE('',#17203,0.237175);
#1598=CYLINDRICAL_SURFACE('',#17230,0.5);
#1599=CYLINDRICAL_SURFACE('',#17238,1.1);
#1600=CYLINDRICAL_SURFACE('',#17245,1.25);
#1601=CYLINDRICAL_SURFACE('',#17251,1.6);
#1602=FACE_BOUND('',#3290,.T.);
#1603=FACE_BOUND('',#3291,.T.);
#1604=FACE_BOUND('',#3292,.T.);
#1605=FACE_BOUND('',#3293,.T.);
#1606=FACE_BOUND('',#3294,.T.);
#1607=FACE_BOUND('',#3328,.T.);
#1608=FACE_BOUND('',#3329,.T.);
#1609=FACE_BOUND('',#3330,.T.);
#1610=FACE_BOUND('',#3331,.T.);
#1611=FACE_BOUND('',#3332,.T.);
#1612=FACE_BOUND('',#3333,.T.);
#1613=FACE_BOUND('',#3334,.T.);
#1614=FACE_BOUND('',#3366,.T.);
#1615=FACE_BOUND('',#3367,.T.);
#1616=FACE_BOUND('',#3368,.T.);
#1617=FACE_BOUND('',#3369,.T.);
#1618=FACE_BOUND('',#3370,.T.);
#1619=FACE_BOUND('',#3377,.T.);
#1620=FACE_BOUND('',#3378,.T.);
#1621=FACE_BOUND('',#3379,.T.);
#1622=FACE_BOUND('',#3380,.T.);
#1623=FACE_BOUND('',#3381,.T.);
#1624=FACE_BOUND('',#3382,.T.);
#1625=FACE_BOUND('',#3383,.T.);
#1626=FACE_BOUND('',#3386,.T.);
#1627=FACE_BOUND('',#3428,.T.);
#1628=FACE_BOUND('',#3443,.T.);
#1629=FACE_BOUND('',#3447,.T.);
#1630=FACE_BOUND('',#3449,.T.);
#1631=FACE_BOUND('',#3450,.T.);
#1632=FACE_BOUND('',#3451,.T.);
#1633=FACE_BOUND('',#3452,.T.);
#1634=FACE_BOUND('',#3453,.T.);
#1635=FACE_BOUND('',#3454,.T.);
#1636=FACE_BOUND('',#3456,.T.);
#1637=FACE_BOUND('',#3462,.T.);
#1638=FACE_BOUND('',#3472,.T.);
#1639=FACE_BOUND('',#3473,.T.);
#1640=FACE_BOUND('',#3475,.T.);
#1641=FACE_BOUND('',#3476,.T.);
#1642=FACE_BOUND('',#3509,.T.);
#1643=FACE_BOUND('',#3512,.T.);
#1644=FACE_BOUND('',#3515,.T.);
#1645=FACE_BOUND('',#3517,.T.);
#1646=FACE_BOUND('',#3519,.T.);
#1647=FACE_BOUND('',#3522,.T.);
#1648=FACE_BOUND('',#3525,.T.);
#1649=FACE_BOUND('',#3528,.T.);
#1650=FACE_BOUND('',#3530,.T.);
#1651=FACE_BOUND('',#3533,.T.);
#1652=FACE_BOUND('',#3542,.T.);
#1653=FACE_BOUND('',#3556,.T.);
#1654=FACE_BOUND('',#3557,.T.);
#1655=FACE_BOUND('',#3558,.T.);
#1656=FACE_BOUND('',#3559,.T.);
#1657=FACE_BOUND('',#3560,.T.);
#1658=FACE_BOUND('',#3565,.T.);
#1659=FACE_BOUND('',#3571,.T.);
#1660=FACE_BOUND('',#3577,.T.);
#1661=FACE_BOUND('',#3583,.T.);
#1662=FACE_BOUND('',#3588,.T.);
#1663=FACE_BOUND('',#3595,.T.);
#1664=FACE_BOUND('',#3596,.T.);
#1665=FACE_BOUND('',#3597,.T.);
#1666=FACE_BOUND('',#3598,.T.);
#1667=FACE_BOUND('',#3599,.T.);
#1668=FACE_BOUND('',#3613,.T.);
#1669=FACE_BOUND('',#3614,.T.);
#1670=FACE_BOUND('',#3615,.T.);
#1671=FACE_BOUND('',#3616,.T.);
#1672=FACE_BOUND('',#3617,.T.);
#1673=FACE_BOUND('',#3618,.T.);
#1674=FACE_BOUND('',#3619,.T.);
#1675=FACE_BOUND('',#3620,.T.);
#1676=FACE_BOUND('',#3621,.T.);
#1677=FACE_BOUND('',#3626,.T.);
#1678=FACE_BOUND('',#3632,.T.);
#1679=FACE_BOUND('',#3638,.T.);
#1680=FACE_BOUND('',#3644,.T.);
#1681=FACE_BOUND('',#3677,.T.);
#1682=FACE_BOUND('',#3678,.T.);
#1683=FACE_BOUND('',#3679,.T.);
#1684=FACE_BOUND('',#3680,.T.);
#1685=FACE_BOUND('',#3681,.T.);
#1686=FACE_BOUND('',#3687,.T.);
#1687=FACE_BOUND('',#3688,.T.);
#1688=FACE_BOUND('',#3689,.T.);
#1689=FACE_BOUND('',#3690,.T.);
#1690=FACE_BOUND('',#3691,.T.);
#1691=FACE_BOUND('',#3692,.T.);
#1692=FACE_BOUND('',#3693,.T.);
#1693=FACE_BOUND('',#3694,.T.);
#1694=FACE_BOUND('',#3695,.T.);
#1695=FACE_BOUND('',#3696,.T.);
#1696=FACE_BOUND('',#3697,.T.);
#1697=FACE_BOUND('',#3698,.T.);
#1698=FACE_BOUND('',#3699,.T.);
#1699=FACE_BOUND('',#3727,.T.);
#1700=FACE_BOUND('',#3731,.T.);
#1701=FACE_BOUND('',#3733,.T.);
#1702=FACE_BOUND('',#3737,.T.);
#1703=FACE_BOUND('',#3741,.T.);
#1704=FACE_BOUND('',#3745,.T.);
#1705=FACE_BOUND('',#3748,.T.);
#1706=FACE_BOUND('',#3993,.T.);
#1707=FACE_BOUND('',#3998,.T.);
#1708=FACE_BOUND('',#4002,.T.);
#1709=FACE_BOUND('',#4005,.T.);
#1710=FACE_BOUND('',#4009,.T.);
#1711=FACE_BOUND('',#4013,.T.);
#1712=FACE_BOUND('',#4017,.T.);
#1713=FACE_BOUND('',#4022,.T.);
#1714=FACE_BOUND('',#4025,.T.);
#1715=FACE_BOUND('',#4032,.T.);
#1716=FACE_BOUND('',#4035,.T.);
#1717=FACE_BOUND('',#4038,.T.);
#1718=FACE_BOUND('',#4064,.T.);
#1719=FACE_BOUND('',#4070,.T.);
#1720=FACE_BOUND('',#4075,.T.);
#1721=FACE_BOUND('',#4078,.T.);
#1722=FACE_BOUND('',#4083,.T.);
#1723=FACE_BOUND('',#4088,.T.);
#1724=FACE_BOUND('',#4092,.T.);
#1725=FACE_BOUND('',#4101,.T.);
#1726=FACE_BOUND('',#4104,.T.);
#1727=FACE_BOUND('',#4107,.T.);
#1728=FACE_BOUND('',#4109,.T.);
#1729=FACE_BOUND('',#4113,.T.);
#1730=FACE_BOUND('',#4117,.T.);
#1731=FACE_BOUND('',#4122,.T.);
#1732=FACE_BOUND('',#4125,.T.);
#1733=FACE_BOUND('',#4130,.T.);
#1734=FACE_BOUND('',#4133,.T.);
#1735=FACE_BOUND('',#4136,.T.);
#1736=FACE_BOUND('',#4141,.T.);
#1737=FACE_BOUND('',#4144,.T.);
#1738=FACE_BOUND('',#4147,.T.);
#1739=FACE_BOUND('',#4150,.T.);
#1740=FACE_BOUND('',#4155,.T.);
#1741=FACE_BOUND('',#4158,.T.);
#1742=FACE_BOUND('',#4166,.T.);
#1743=FACE_BOUND('',#4167,.T.);
#1744=FACE_BOUND('',#4170,.T.);
#1745=FACE_BOUND('',#4171,.T.);
#1746=FACE_BOUND('',#4210,.T.);
#1747=FACE_BOUND('',#4220,.T.);
#1748=FACE_BOUND('',#4224,.T.);
#1749=FACE_BOUND('',#4251,.T.);
#1750=FACE_BOUND('',#4261,.T.);
#1751=FACE_BOUND('',#4265,.T.);
#1752=FACE_BOUND('',#4271,.T.);
#1753=FACE_BOUND('',#4275,.T.);
#1754=CIRCLE('',#15865,2.6);
#1755=CIRCLE('',#15899,0.355);
#1756=CIRCLE('',#15900,0.355);
#1757=CIRCLE('',#15901,0.355);
#1758=CIRCLE('',#15902,0.355);
#1759=CIRCLE('',#15903,2.6);
#1760=CIRCLE('',#15904,0.355);
#1761=CIRCLE('',#15905,0.355);
#1762=CIRCLE('',#15907,5.8);
#1763=CIRCLE('',#15908,5.8);
#1764=CIRCLE('',#15910,0.9);
#1765=CIRCLE('',#15911,0.9);
#1766=CIRCLE('',#15916,0.9);
#1767=CIRCLE('',#15917,0.9);
#1768=CIRCLE('',#15923,0.9);
#1769=CIRCLE('',#15924,0.9);
#1770=CIRCLE('',#15925,5.8);
#1771=CIRCLE('',#15927,0.9);
#1772=CIRCLE('',#15928,5.8);
#1773=CIRCLE('',#15929,0.9);
#1774=CIRCLE('',#15930,0.6);
#1775=CIRCLE('',#15931,0.6);
#1776=CIRCLE('',#15932,0.9);
#1777=CIRCLE('',#15933,5.8);
#1778=CIRCLE('',#15934,0.9);
#1779=CIRCLE('',#15936,5.7);
#1780=CIRCLE('',#15937,5.8);
#1781=CIRCLE('',#15939,0.8);
#1782=CIRCLE('',#15941,0.9);
#1783=CIRCLE('',#15945,0.8);
#1784=CIRCLE('',#15946,0.9);
#1785=CIRCLE('',#15948,5.7);
#1786=CIRCLE('',#15949,5.8);
#1787=CIRCLE('',#15951,0.8);
#1788=CIRCLE('',#15953,0.9);
#1789=CIRCLE('',#15957,0.9);
#1790=CIRCLE('',#15958,0.8);
#1791=CIRCLE('',#15960,5.8);
#1792=CIRCLE('',#15961,5.7);
#1793=CIRCLE('',#15963,0.9);
#1794=CIRCLE('',#15964,0.8);
#1795=CIRCLE('',#15966,5.8);
#1796=CIRCLE('',#15967,5.7);
#1797=CIRCLE('',#15969,0.9);
#1798=CIRCLE('',#15970,0.8);
#1799=CIRCLE('',#15978,3.15);
#1800=CIRCLE('',#15979,0.355);
#1801=CIRCLE('',#15980,0.355);
#1802=CIRCLE('',#15981,0.355);
#1803=CIRCLE('',#15982,0.355);
#1804=CIRCLE('',#15984,0.505);
#1805=CIRCLE('',#15986,0.559999999999998);
#1806=CIRCLE('',#15988,0.405);
#1807=CIRCLE('',#15990,0.405);
#1808=CIRCLE('',#15992,0.455);
#1809=CIRCLE('',#15993,0.455);
#1810=CIRCLE('',#15995,0.455);
#1811=CIRCLE('',#15996,0.455);
#1812=CIRCLE('',#15997,0.455000000000001);
#1813=CIRCLE('',#15998,0.455000000000001);
#1814=CIRCLE('',#15999,0.455000000000001);
#1815=CIRCLE('',#16000,0.455000000000001);
#1816=CIRCLE('',#16002,0.405);
#1817=CIRCLE('',#16004,0.405);
#1818=CIRCLE('',#16007,0.6);
#1819=CIRCLE('',#16009,0.405);
#1820=CIRCLE('',#16011,0.405);
#1821=CIRCLE('',#16014,0.6);
#1822=CIRCLE('',#16016,0.405);
#1823=CIRCLE('',#16018,0.405);
#1824=CIRCLE('',#16021,0.305);
#1825=CIRCLE('',#16023,0.305);
#1826=CIRCLE('',#16026,0.305);
#1827=CIRCLE('',#16028,0.305);
#1828=CIRCLE('',#16030,0.355);
#1829=CIRCLE('',#16032,0.305);
#1830=CIRCLE('',#16034,0.305);
#1831=CIRCLE('',#16037,0.305);
#1832=CIRCLE('',#16039,0.305);
#1833=CIRCLE('',#16041,0.355);
#1834=CIRCLE('',#16043,0.305);
#1835=CIRCLE('',#16045,0.305);
#1836=CIRCLE('',#16048,0.305);
#1837=CIRCLE('',#16050,0.305);
#1838=CIRCLE('',#16052,0.355);
#1839=CIRCLE('',#16054,0.305);
#1840=CIRCLE('',#16056,0.305);
#1841=CIRCLE('',#16059,0.305);
#1842=CIRCLE('',#16061,0.305);
#1843=CIRCLE('',#16063,0.355);
#1844=CIRCLE('',#16065,0.305);
#1845=CIRCLE('',#16067,0.305);
#1846=CIRCLE('',#16070,0.305);
#1847=CIRCLE('',#16072,0.305);
#1848=CIRCLE('',#16075,0.305);
#1849=CIRCLE('',#16077,0.305);
#1850=CIRCLE('',#16080,0.305);
#1851=CIRCLE('',#16082,0.305);
#1852=CIRCLE('',#16085,0.425);
#1853=CIRCLE('',#16086,0.425);
#1854=CIRCLE('',#16088,0.45);
#1855=CIRCLE('',#16090,0.425000000000001);
#1856=CIRCLE('',#16091,0.425000000000001);
#1857=CIRCLE('',#16093,0.45);
#1858=CIRCLE('',#16095,0.425);
#1859=CIRCLE('',#16096,0.425);
#1860=CIRCLE('',#16098,0.45);
#1861=CIRCLE('',#16100,0.425000000000001);
#1862=CIRCLE('',#16101,0.425000000000001);
#1863=CIRCLE('',#16103,0.45);
#1864=CIRCLE('',#16110,0.6);
#1865=CIRCLE('',#16111,0.6);
#1866=CIRCLE('',#16112,5.3);
#1867=CIRCLE('',#16121,0.9);
#1868=CIRCLE('',#16124,0.9);
#1869=CIRCLE('',#16126,0.6);
#1870=CIRCLE('',#16127,0.6);
#1871=CIRCLE('',#16128,5.8);
#1872=CIRCLE('',#16165,2.6);
#1873=CIRCLE('',#16167,2.75);
#1874=CIRCLE('',#16169,2.75);
#1875=CIRCLE('',#16171,2.6);
#1876=CIRCLE('',#16173,2.6);
#1877=CIRCLE('',#16175,2.3);
#1878=CIRCLE('',#16177,2.3);
#1879=CIRCLE('',#16179,2.6);
#1880=CIRCLE('',#16181,2.6);
#1881=CIRCLE('',#16183,2.75);
#1882=CIRCLE('',#16185,2.75);
#1883=CIRCLE('',#16187,2.6);
#1884=CIRCLE('',#16190,5.3);
#1885=CIRCLE('',#16192,3.75);
#1886=CIRCLE('',#16194,3.75);
#1887=CIRCLE('',#16196,3.1);
#1888=CIRCLE('',#16198,3.1);
#1889=CIRCLE('',#16205,5.295);
#1890=CIRCLE('',#16206,5.195);
#1891=CIRCLE('',#16208,5.295);
#1892=CIRCLE('',#16210,3.75);
#1893=CIRCLE('',#16212,5.7);
#1894=CIRCLE('',#16213,5.8);
#1895=CIRCLE('',#16215,0.8);
#1896=CIRCLE('',#16216,0.9);
#1897=CIRCLE('',#16218,5.7);
#1898=CIRCLE('',#16219,5.8);
#1899=CIRCLE('',#16221,0.8);
#1900=CIRCLE('',#16222,0.9);
#1901=CIRCLE('',#16224,5.7);
#1902=CIRCLE('',#16225,5.8);
#1903=CIRCLE('',#16227,0.9);
#1904=CIRCLE('',#16228,0.8);
#1905=CIRCLE('',#16230,5.8);
#1906=CIRCLE('',#16231,5.7);
#1907=CIRCLE('',#16233,0.9);
#1908=CIRCLE('',#16234,0.8);
#1909=CIRCLE('',#16236,0.9);
#1910=CIRCLE('',#16238,5.8);
#1911=CIRCLE('',#16240,0.9);
#1912=CIRCLE('',#16242,5.8);
#1913=CIRCLE('',#16244,3.15);
#1914=CIRCLE('',#16245,0.55);
#1915=CIRCLE('',#16246,0.55);
#1916=CIRCLE('',#16247,0.55);
#1917=CIRCLE('',#16248,0.55);
#1918=CIRCLE('',#16250,0.33);
#1919=CIRCLE('',#16251,0.338333333333333);
#1920=CIRCLE('',#16253,0.33);
#1921=CIRCLE('',#16255,0.355);
#1922=CIRCLE('',#16257,0.55);
#1923=CIRCLE('',#16260,0.33);
#1924=CIRCLE('',#16261,0.338333333333333);
#1925=CIRCLE('',#16263,0.33);
#1926=CIRCLE('',#16265,0.355);
#1927=CIRCLE('',#16267,0.55);
#1928=CIRCLE('',#16270,0.33);
#1929=CIRCLE('',#16271,0.338333333333333);
#1930=CIRCLE('',#16273,0.33);
#1931=CIRCLE('',#16275,0.355);
#1932=CIRCLE('',#16277,0.55);
#1933=CIRCLE('',#16280,0.33);
#1934=CIRCLE('',#16281,0.338333333333333);
#1935=CIRCLE('',#16283,0.33);
#1936=CIRCLE('',#16285,0.355);
#1937=CIRCLE('',#16287,0.55);
#1938=CIRCLE('',#16290,3.1);
#1939=CIRCLE('',#16292,3.1);
#1940=CIRCLE('',#16294,3.75);
#1941=CIRCLE('',#16297,0.9);
#1942=CIRCLE('',#16299,5.8);
#1943=CIRCLE('',#16301,0.9);
#1944=CIRCLE('',#16303,5.8);
#1945=CIRCLE('',#16319,0.480000000000001);
#1946=CIRCLE('',#16320,5.501);
#1947=CIRCLE('',#16321,0.480000000000001);
#1948=CIRCLE('',#16322,0.480000000000001);
#1949=CIRCLE('',#16323,0.480000000000001);
#1950=CIRCLE('',#16325,0.33);
#1951=CIRCLE('',#16326,0.338333333333333);
#1952=CIRCLE('',#16328,0.33);
#1953=CIRCLE('',#16330,0.355);
#1954=CIRCLE('',#16332,0.55);
#1955=CIRCLE('',#16334,0.55);
#1956=CIRCLE('',#16336,0.33);
#1957=CIRCLE('',#16337,0.338333333333333);
#1958=CIRCLE('',#16339,0.33);
#1959=CIRCLE('',#16341,0.355);
#1960=CIRCLE('',#16343,0.55);
#1961=CIRCLE('',#16345,0.55);
#1962=CIRCLE('',#16347,0.33);
#1963=CIRCLE('',#16348,0.338333333333333);
#1964=CIRCLE('',#16350,0.33);
#1965=CIRCLE('',#16352,0.355);
#1966=CIRCLE('',#16354,0.55);
#1967=CIRCLE('',#16356,0.55);
#1968=CIRCLE('',#16358,0.33);
#1969=CIRCLE('',#16359,0.338333333333333);
#1970=CIRCLE('',#16361,0.33);
#1971=CIRCLE('',#16363,0.355);
#1972=CIRCLE('',#16365,0.55);
#1973=CIRCLE('',#16367,0.55);
#1974=CIRCLE('',#16369,0.45);
#1975=CIRCLE('',#16370,0.48);
#1976=CIRCLE('',#16372,0.45);
#1977=CIRCLE('',#16375,0.45);
#1978=CIRCLE('',#16376,0.48);
#1979=CIRCLE('',#16378,0.45);
#1980=CIRCLE('',#16381,0.45);
#1981=CIRCLE('',#16382,0.48);
#1982=CIRCLE('',#16384,0.45);
#1983=CIRCLE('',#16387,0.45);
#1984=CIRCLE('',#16388,0.48);
#1985=CIRCLE('',#16390,0.45);
#1986=CIRCLE('',#16409,2.);
#1987=CIRCLE('',#16410,2.);
#1988=CIRCLE('',#16412,5.501);
#1989=CIRCLE('',#16421,1.4);
#1990=CIRCLE('',#16428,1.4);
#1991=CIRCLE('',#16431,0.699999999999999);
#1992=CIRCLE('',#16435,0.699999999999999);
#1993=CIRCLE('',#16436,0.699999999999999);
#1994=CIRCLE('',#16437,0.699999999999999);
#1995=CIRCLE('',#16439,0.73);
#1996=CIRCLE('',#16442,1.398);
#1997=CIRCLE('',#16443,1.398);
#1998=CIRCLE('',#16446,1.398);
#1999=CIRCLE('',#16448,1.398);
#2000=CIRCLE('',#16452,1.17);
#2001=CIRCLE('',#16454,1.25);
#2002=CIRCLE('',#16456,1.25);
#2003=CIRCLE('',#16458,1.5);
#2004=CIRCLE('',#16460,1.55);
#2005=CIRCLE('',#16462,1.55);
#2006=CIRCLE('',#16465,1.55);
#2007=CIRCLE('',#16467,1.55);
#2008=CIRCLE('',#16469,1.5);
#2009=CIRCLE('',#16471,1.25);
#2010=CIRCLE('',#16473,1.25);
#2011=CIRCLE('',#16475,1.17);
#2012=CIRCLE('',#16479,3.3);
#2013=CIRCLE('',#16480,3.35);
#2014=CIRCLE('',#16481,3.3);
#2015=CIRCLE('',#16483,3.3);
#2016=CIRCLE('',#16484,3.3);
#2017=CIRCLE('',#16486,4.85);
#2018=CIRCLE('',#16487,4.85);
#2019=CIRCLE('',#16488,4.85);
#2020=CIRCLE('',#16489,4.85);
#2021=CIRCLE('',#16490,4.85);
#2022=CIRCLE('',#16491,4.85);
#2023=CIRCLE('',#16492,4.85);
#2024=CIRCLE('',#16493,4.85);
#2025=CIRCLE('',#16494,4.85);
#2026=CIRCLE('',#16495,4.85);
#2027=CIRCLE('',#16496,4.85);
#2028=CIRCLE('',#16497,4.85);
#2029=CIRCLE('',#16498,4.85);
#2030=CIRCLE('',#16499,4.85);
#2031=CIRCLE('',#16500,4.85);
#2032=CIRCLE('',#16501,4.85);
#2033=CIRCLE('',#16502,4.85);
#2034=CIRCLE('',#16503,4.85);
#2035=CIRCLE('',#16504,4.85);
#2036=CIRCLE('',#16505,4.85);
#2037=CIRCLE('',#16506,4.85);
#2038=CIRCLE('',#16507,4.85);
#2039=CIRCLE('',#16508,4.85);
#2040=CIRCLE('',#16509,4.85);
#2041=CIRCLE('',#16510,4.85);
#2042=CIRCLE('',#16511,4.85);
#2043=CIRCLE('',#16512,4.85);
#2044=CIRCLE('',#16513,4.85);
#2045=CIRCLE('',#16514,4.85);
#2046=CIRCLE('',#16515,4.85);
#2047=CIRCLE('',#16517,3.35);
#2048=CIRCLE('',#16519,4.85);
#2049=CIRCLE('',#16520,4.85);
#2050=CIRCLE('',#16521,4.85);
#2051=CIRCLE('',#16522,4.85);
#2052=CIRCLE('',#16523,4.85);
#2053=CIRCLE('',#16524,4.85);
#2054=CIRCLE('',#16525,4.85);
#2055=CIRCLE('',#16526,4.85);
#2056=CIRCLE('',#16527,4.85);
#2057=CIRCLE('',#16528,4.85);
#2058=CIRCLE('',#16529,4.85);
#2059=CIRCLE('',#16530,4.85);
#2060=CIRCLE('',#16531,4.85);
#2061=CIRCLE('',#16532,4.85);
#2062=CIRCLE('',#16533,4.85);
#2063=CIRCLE('',#16534,4.85);
#2064=CIRCLE('',#16535,4.85);
#2065=CIRCLE('',#16536,4.85);
#2066=CIRCLE('',#16537,4.85);
#2067=CIRCLE('',#16538,4.85);
#2068=CIRCLE('',#16539,4.85);
#2069=CIRCLE('',#16540,4.85);
#2070=CIRCLE('',#16541,4.85);
#2071=CIRCLE('',#16542,4.85);
#2072=CIRCLE('',#16543,4.85);
#2073=CIRCLE('',#16544,4.85);
#2074=CIRCLE('',#16545,4.85);
#2075=CIRCLE('',#16546,4.85);
#2076=CIRCLE('',#16547,4.85);
#2077=CIRCLE('',#16548,4.85);
#2078=CIRCLE('',#16550,4.95);
#2079=CIRCLE('',#16552,4.95);
#2080=CIRCLE('',#16554,4.95);
#2081=CIRCLE('',#16556,4.95);
#2082=CIRCLE('',#16559,4.95);
#2083=CIRCLE('',#16561,4.95);
#2084=CIRCLE('',#16563,4.95);
#2085=CIRCLE('',#16565,4.95);
#2086=CIRCLE('',#16568,4.95);
#2087=CIRCLE('',#16570,4.95);
#2088=CIRCLE('',#16572,4.95);
#2089=CIRCLE('',#16574,4.95);
#2090=CIRCLE('',#16577,4.95);
#2091=CIRCLE('',#16579,4.95);
#2092=CIRCLE('',#16581,4.95);
#2093=CIRCLE('',#16583,4.95);
#2094=CIRCLE('',#16586,4.95);
#2095=CIRCLE('',#16588,4.95);
#2096=CIRCLE('',#16590,4.95);
#2097=CIRCLE('',#16592,4.95);
#2098=CIRCLE('',#16595,4.95);
#2099=CIRCLE('',#16597,4.95);
#2100=CIRCLE('',#16599,4.95);
#2101=CIRCLE('',#16601,4.95);
#2102=CIRCLE('',#16604,4.95);
#2103=CIRCLE('',#16606,4.95);
#2104=CIRCLE('',#16608,4.95);
#2105=CIRCLE('',#16610,4.95);
#2106=CIRCLE('',#16613,4.95);
#2107=CIRCLE('',#16615,4.95);
#2108=CIRCLE('',#16617,4.95);
#2109=CIRCLE('',#16619,4.95);
#2110=CIRCLE('',#16622,4.95);
#2111=CIRCLE('',#16624,4.95);
#2112=CIRCLE('',#16626,4.95);
#2113=CIRCLE('',#16628,4.95);
#2114=CIRCLE('',#16631,4.95);
#2115=CIRCLE('',#16633,4.95);
#2116=CIRCLE('',#16635,4.95);
#2117=CIRCLE('',#16637,4.95);
#2118=CIRCLE('',#16640,4.95);
#2119=CIRCLE('',#16642,4.95);
#2120=CIRCLE('',#16644,4.95);
#2121=CIRCLE('',#16646,4.95);
#2122=CIRCLE('',#16649,4.95);
#2123=CIRCLE('',#16651,4.95);
#2124=CIRCLE('',#16653,4.95);
#2125=CIRCLE('',#16655,4.95);
#2126=CIRCLE('',#16658,4.95);
#2127=CIRCLE('',#16660,4.95);
#2128=CIRCLE('',#16662,4.95);
#2129=CIRCLE('',#16664,4.95);
#2130=CIRCLE('',#16667,4.95);
#2131=CIRCLE('',#16669,4.95);
#2132=CIRCLE('',#16671,4.95);
#2133=CIRCLE('',#16673,4.95);
#2134=CIRCLE('',#16676,4.95);
#2135=CIRCLE('',#16678,4.95);
#2136=CIRCLE('',#16680,4.95);
#2137=CIRCLE('',#16682,4.95);
#2138=CIRCLE('',#16685,4.95);
#2139=CIRCLE('',#16687,4.95);
#2140=CIRCLE('',#16689,4.95);
#2141=CIRCLE('',#16691,4.95);
#2142=CIRCLE('',#16694,4.95);
#2143=CIRCLE('',#16696,4.95);
#2144=CIRCLE('',#16698,4.95);
#2145=CIRCLE('',#16700,4.95);
#2146=CIRCLE('',#16703,4.95);
#2147=CIRCLE('',#16705,4.95);
#2148=CIRCLE('',#16707,4.95);
#2149=CIRCLE('',#16709,4.95);
#2150=CIRCLE('',#16712,4.95);
#2151=CIRCLE('',#16714,4.95);
#2152=CIRCLE('',#16716,4.95);
#2153=CIRCLE('',#16718,4.95);
#2154=CIRCLE('',#16721,4.95);
#2155=CIRCLE('',#16723,4.95);
#2156=CIRCLE('',#16725,4.95);
#2157=CIRCLE('',#16727,4.95);
#2158=CIRCLE('',#16730,4.95);
#2159=CIRCLE('',#16732,4.95);
#2160=CIRCLE('',#16734,4.95);
#2161=CIRCLE('',#16736,4.95);
#2162=CIRCLE('',#16739,4.95);
#2163=CIRCLE('',#16741,4.95);
#2164=CIRCLE('',#16743,4.95);
#2165=CIRCLE('',#16745,4.95);
#2166=CIRCLE('',#16748,4.95);
#2167=CIRCLE('',#16750,4.95);
#2168=CIRCLE('',#16752,4.95);
#2169=CIRCLE('',#16754,4.95);
#2170=CIRCLE('',#16757,4.95);
#2171=CIRCLE('',#16759,4.95);
#2172=CIRCLE('',#16761,4.95);
#2173=CIRCLE('',#16763,4.95);
#2174=CIRCLE('',#16766,4.95);
#2175=CIRCLE('',#16768,4.95);
#2176=CIRCLE('',#16770,4.95);
#2177=CIRCLE('',#16772,4.95);
#2178=CIRCLE('',#16775,4.95);
#2179=CIRCLE('',#16777,4.95);
#2180=CIRCLE('',#16779,4.95);
#2181=CIRCLE('',#16781,4.95);
#2182=CIRCLE('',#16784,4.95);
#2183=CIRCLE('',#16786,4.95);
#2184=CIRCLE('',#16788,4.95);
#2185=CIRCLE('',#16790,4.95);
#2186=CIRCLE('',#16793,4.95);
#2187=CIRCLE('',#16795,4.95);
#2188=CIRCLE('',#16797,4.95);
#2189=CIRCLE('',#16799,4.95);
#2190=CIRCLE('',#16801,4.95);
#2191=CIRCLE('',#16804,4.95);
#2192=CIRCLE('',#16806,4.95);
#2193=CIRCLE('',#16808,4.95);
#2194=CIRCLE('',#16810,4.95);
#2195=CIRCLE('',#16812,4.95);
#2196=CIRCLE('',#16815,4.95);
#2197=CIRCLE('',#16816,4.95);
#2198=CIRCLE('',#16824,2.17);
#2199=CIRCLE('',#16825,1.35);
#2200=CIRCLE('',#16827,1.25);
#2201=CIRCLE('',#16829,2.25);
#2202=CIRCLE('',#16831,2.25);
#2203=CIRCLE('',#16833,2.55);
#2204=CIRCLE('',#16835,2.6);
#2205=CIRCLE('',#16837,2.6);
#2206=CIRCLE('',#16839,3.3);
#2207=CIRCLE('',#16841,3.3);
#2208=CIRCLE('',#16843,2.6);
#2209=CIRCLE('',#16845,2.6);
#2210=CIRCLE('',#16847,2.55);
#2211=CIRCLE('',#16849,2.25);
#2212=CIRCLE('',#16851,2.25);
#2213=CIRCLE('',#16853,2.17);
#2214=CIRCLE('',#16855,1.35);
#2215=CIRCLE('',#16857,1.25);
#2216=CIRCLE('',#16861,2.55);
#2217=CIRCLE('',#16862,1.6);
#2218=CIRCLE('',#16864,2.6);
#2219=CIRCLE('',#16866,2.6);
#2220=CIRCLE('',#16868,2.56);
#2221=CIRCLE('',#16870,1.7);
#2222=CIRCLE('',#16872,1.7);
#2223=CIRCLE('',#16874,1.4);
#2224=CIRCLE('',#16876,1.25);
#2225=CIRCLE('',#16878,1.25);
#2226=CIRCLE('',#16880,1.45);
#2227=CIRCLE('',#16884,1.);
#2228=CIRCLE('',#16885,1.);
#2229=CIRCLE('',#16887,1.12);
#2230=CIRCLE('',#16889,1.12);
#2231=CIRCLE('',#16891,2.56);
#2232=CIRCLE('',#16893,2.52);
#2233=CIRCLE('',#16894,2.52);
#2234=CIRCLE('',#16896,2.6);
#2235=CIRCLE('',#16898,2.6);
#2236=CIRCLE('',#16904,0.4372);
#2237=CIRCLE('',#16911,0.4942);
#2238=CIRCLE('',#16912,0.4942);
#2239=CIRCLE('',#16914,0.4372);
#2240=CIRCLE('',#16916,0.44);
#2241=CIRCLE('',#16918,0.4942);
#2242=CIRCLE('',#16919,0.4942);
#2243=CIRCLE('',#16921,0.308675134594813);
#2244=CIRCLE('',#16926,0.243346949651439);
#2245=CIRCLE('',#16932,0.43);
#2246=CIRCLE('',#16935,0.44);
#2247=CIRCLE('',#16936,0.44);
#2248=CIRCLE('',#16938,0.44);
#2249=CIRCLE('',#16940,0.68);
#2250=CIRCLE('',#16942,0.7);
#2251=CIRCLE('',#16944,0.7);
#2252=CIRCLE('',#16946,0.66);
#2253=CIRCLE('',#16950,0.51);
#2254=CIRCLE('',#16951,0.52);
#2255=CIRCLE('',#16953,0.69);
#2256=CIRCLE('',#16955,0.7);
#2257=CIRCLE('',#16957,0.7);
#2258=CIRCLE('',#16959,0.69);
#2259=CIRCLE('',#16961,0.52);
#2260=CIRCLE('',#16963,0.51);
#2261=CIRCLE('',#16967,0.55);
#2262=CIRCLE('',#16968,0.55);
#2263=CIRCLE('',#16970,0.66);
#2264=CIRCLE('',#16972,0.7);
#2265=CIRCLE('',#16974,0.7);
#2266=CIRCLE('',#16976,1.85);
#2267=CIRCLE('',#16978,1.9);
#2268=CIRCLE('',#16980,1.9);
#2269=CIRCLE('',#16982,1.86);
#2270=CIRCLE('',#16987,2.26);
#2271=CIRCLE('',#16988,2.26);
#2272=CIRCLE('',#16990,2.3);
#2273=CIRCLE('',#16991,2.3);
#2274=CIRCLE('',#16994,1.68);
#2275=CIRCLE('',#16995,1.68);
#2276=CIRCLE('',#16997,1.72);
#2277=CIRCLE('',#16999,1.72);
#2278=CIRCLE('',#17001,2.54);
#2279=CIRCLE('',#17003,1.95);
#2280=CIRCLE('',#17005,1.25);
#2281=CIRCLE('',#17006,1.25);
#2282=CIRCLE('',#17008,1.31);
#2283=CIRCLE('',#17010,1.8);
#2284=CIRCLE('',#17012,2.18);
#2285=CIRCLE('',#17014,2.24);
#2286=CIRCLE('',#17017,2.6);
#2287=CIRCLE('',#17019,2.6);
#2288=CIRCLE('',#17021,2.54);
#2289=CIRCLE('',#17023,1.95);
#2290=CIRCLE('',#17026,1.31);
#2291=CIRCLE('',#17030,2.25);
#2292=CIRCLE('',#17031,2.25);
#2293=CIRCLE('',#17033,2.31);
#2294=CIRCLE('',#17035,2.67);
#2295=CIRCLE('',#17037,2.67);
#2296=CIRCLE('',#17039,3.18);
#2297=CIRCLE('',#17041,3.18);
#2298=CIRCLE('',#17043,3.69);
#2299=CIRCLE('',#17045,3.75);
#2300=CIRCLE('',#17047,3.75);
#2301=CIRCLE('',#17049,3.69);
#2302=CIRCLE('',#17051,3.18);
#2303=CIRCLE('',#17053,3.18);
#2304=CIRCLE('',#17055,2.67);
#2305=CIRCLE('',#17057,2.67);
#2306=CIRCLE('',#17059,2.31);
#2307=CIRCLE('',#17063,3.05);
#2308=CIRCLE('',#17064,2.6);
#2309=CIRCLE('',#17066,3.1);
#2310=CIRCLE('',#17068,3.1);
#2311=CIRCLE('',#17070,3.06);
#2312=CIRCLE('',#17072,2.65);
#2313=CIRCLE('',#17074,2.65);
#2314=CIRCLE('',#17076,2.4);
#2315=CIRCLE('',#17078,2.25);
#2316=CIRCLE('',#17080,2.25);
#2317=CIRCLE('',#17082,2.45);
#2318=CIRCLE('',#17086,0.125);
#2319=CIRCLE('',#17087,0.145);
#2320=CIRCLE('',#17089,0.125);
#2321=CIRCLE('',#17091,2.75);
#2322=CIRCLE('',#17092,2.345);
#2323=CIRCLE('',#17093,0.3);
#2324=CIRCLE('',#17094,2.345);
#2325=CIRCLE('',#17095,0.3);
#2326=CIRCLE('',#17096,2.345);
#2327=CIRCLE('',#17097,0.145);
#2328=CIRCLE('',#17099,0.145);
#2329=CIRCLE('',#17101,2.345);
#2330=CIRCLE('',#17102,0.3);
#2331=CIRCLE('',#17103,2.345);
#2332=CIRCLE('',#17104,0.3);
#2333=CIRCLE('',#17105,2.345);
#2334=CIRCLE('',#17106,2.75);
#2335=CIRCLE('',#17107,0.145);
#2336=CIRCLE('',#17109,0.125);
#2337=CIRCLE('',#17111,0.125);
#2338=CIRCLE('',#17123,0.237175);
#2339=CIRCLE('',#17143,0.2942);
#2340=CIRCLE('',#17144,0.295065936436295);
#2341=CIRCLE('',#17145,0.2942);
#2342=CIRCLE('',#17146,0.2942);
#2343=CIRCLE('',#17148,0.237175);
#2344=CIRCLE('',#17150,0.2942);
#2345=CIRCLE('',#17152,0.2942);
#2346=CIRCLE('',#17153,0.2942);
#2347=CIRCLE('',#17155,0.3342);
#2348=CIRCLE('',#17156,0.04);
#2349=CIRCLE('',#17158,0.48);
#2350=CIRCLE('',#17160,0.308675134594813);
#2351=CIRCLE('',#17165,0.243346949651439);
#2352=CIRCLE('',#17171,0.44);
#2353=CIRCLE('',#17172,0.06);
#2354=CIRCLE('',#17173,0.5);
#2355=CIRCLE('',#17175,0.5);
#2356=CIRCLE('',#17178,0.255);
#2357=CIRCLE('',#17183,0.237175);
#2358=CIRCLE('',#17199,0.2942);
#2359=CIRCLE('',#17200,0.295065672210827);
#2360=CIRCLE('',#17201,0.2942);
#2361=CIRCLE('',#17202,0.2942);
#2362=CIRCLE('',#17204,0.237175);
#2363=CIRCLE('',#17206,0.2942);
#2364=CIRCLE('',#17208,0.2942);
#2365=CIRCLE('',#17209,0.2942);
#2366=CIRCLE('',#17211,0.3342);
#2367=CIRCLE('',#17212,0.04);
#2368=CIRCLE('',#17214,0.48);
#2369=CIRCLE('',#17216,0.308675134594813);
#2370=CIRCLE('',#17221,0.243346949651439);
#2371=CIRCLE('',#17227,0.44);
#2372=CIRCLE('',#17228,0.06);
#2373=CIRCLE('',#17229,0.5);
#2374=CIRCLE('',#17231,0.5);
#2375=CIRCLE('',#17234,0.255);
#2376=CIRCLE('',#17239,1.1);
#2377=CIRCLE('',#17240,1.1);
#2378=CIRCLE('',#17242,1.21);
#2379=CIRCLE('',#17244,1.25);
#2380=CIRCLE('',#17246,1.25);
#2381=CIRCLE('',#17248,1.55);
#2382=CIRCLE('',#17250,1.6);
#2383=CIRCLE('',#17252,1.6);
#2384=CIRCLE('',#17254,1.56);
#2385=FACE_OUTER_BOUND('',#3257,.T.);
#2386=FACE_OUTER_BOUND('',#3258,.T.);
#2387=FACE_OUTER_BOUND('',#3259,.T.);
#2388=FACE_OUTER_BOUND('',#3260,.T.);
#2389=FACE_OUTER_BOUND('',#3261,.T.);
#2390=FACE_OUTER_BOUND('',#3262,.T.);
#2391=FACE_OUTER_BOUND('',#3263,.T.);
#2392=FACE_OUTER_BOUND('',#3264,.T.);
#2393=FACE_OUTER_BOUND('',#3265,.T.);
#2394=FACE_OUTER_BOUND('',#3266,.T.);
#2395=FACE_OUTER_BOUND('',#3267,.T.);
#2396=FACE_OUTER_BOUND('',#3268,.T.);
#2397=FACE_OUTER_BOUND('',#3269,.T.);
#2398=FACE_OUTER_BOUND('',#3270,.T.);
#2399=FACE_OUTER_BOUND('',#3271,.T.);
#2400=FACE_OUTER_BOUND('',#3272,.T.);
#2401=FACE_OUTER_BOUND('',#3273,.T.);
#2402=FACE_OUTER_BOUND('',#3274,.T.);
#2403=FACE_OUTER_BOUND('',#3275,.T.);
#2404=FACE_OUTER_BOUND('',#3276,.T.);
#2405=FACE_OUTER_BOUND('',#3277,.T.);
#2406=FACE_OUTER_BOUND('',#3278,.T.);
#2407=FACE_OUTER_BOUND('',#3279,.T.);
#2408=FACE_OUTER_BOUND('',#3280,.T.);
#2409=FACE_OUTER_BOUND('',#3281,.T.);
#2410=FACE_OUTER_BOUND('',#3282,.T.);
#2411=FACE_OUTER_BOUND('',#3283,.T.);
#2412=FACE_OUTER_BOUND('',#3284,.T.);
#2413=FACE_OUTER_BOUND('',#3285,.T.);
#2414=FACE_OUTER_BOUND('',#3286,.T.);
#2415=FACE_OUTER_BOUND('',#3287,.T.);
#2416=FACE_OUTER_BOUND('',#3288,.T.);
#2417=FACE_OUTER_BOUND('',#3289,.T.);
#2418=FACE_OUTER_BOUND('',#3295,.T.);
#2419=FACE_OUTER_BOUND('',#3296,.T.);
#2420=FACE_OUTER_BOUND('',#3297,.T.);
#2421=FACE_OUTER_BOUND('',#3298,.T.);
#2422=FACE_OUTER_BOUND('',#3299,.T.);
#2423=FACE_OUTER_BOUND('',#3300,.T.);
#2424=FACE_OUTER_BOUND('',#3301,.T.);
#2425=FACE_OUTER_BOUND('',#3302,.T.);
#2426=FACE_OUTER_BOUND('',#3303,.T.);
#2427=FACE_OUTER_BOUND('',#3304,.T.);
#2428=FACE_OUTER_BOUND('',#3305,.T.);
#2429=FACE_OUTER_BOUND('',#3306,.T.);
#2430=FACE_OUTER_BOUND('',#3307,.T.);
#2431=FACE_OUTER_BOUND('',#3308,.T.);
#2432=FACE_OUTER_BOUND('',#3309,.T.);
#2433=FACE_OUTER_BOUND('',#3310,.T.);
#2434=FACE_OUTER_BOUND('',#3311,.T.);
#2435=FACE_OUTER_BOUND('',#3312,.T.);
#2436=FACE_OUTER_BOUND('',#3313,.T.);
#2437=FACE_OUTER_BOUND('',#3314,.T.);
#2438=FACE_OUTER_BOUND('',#3315,.T.);
#2439=FACE_OUTER_BOUND('',#3316,.T.);
#2440=FACE_OUTER_BOUND('',#3317,.T.);
#2441=FACE_OUTER_BOUND('',#3318,.T.);
#2442=FACE_OUTER_BOUND('',#3319,.T.);
#2443=FACE_OUTER_BOUND('',#3320,.T.);
#2444=FACE_OUTER_BOUND('',#3321,.T.);
#2445=FACE_OUTER_BOUND('',#3322,.T.);
#2446=FACE_OUTER_BOUND('',#3323,.T.);
#2447=FACE_OUTER_BOUND('',#3324,.T.);
#2448=FACE_OUTER_BOUND('',#3325,.T.);
#2449=FACE_OUTER_BOUND('',#3326,.T.);
#2450=FACE_OUTER_BOUND('',#3327,.T.);
#2451=FACE_OUTER_BOUND('',#3335,.T.);
#2452=FACE_OUTER_BOUND('',#3336,.T.);
#2453=FACE_OUTER_BOUND('',#3337,.T.);
#2454=FACE_OUTER_BOUND('',#3338,.T.);
#2455=FACE_OUTER_BOUND('',#3339,.T.);
#2456=FACE_OUTER_BOUND('',#3340,.T.);
#2457=FACE_OUTER_BOUND('',#3341,.T.);
#2458=FACE_OUTER_BOUND('',#3342,.T.);
#2459=FACE_OUTER_BOUND('',#3343,.T.);
#2460=FACE_OUTER_BOUND('',#3344,.T.);
#2461=FACE_OUTER_BOUND('',#3345,.T.);
#2462=FACE_OUTER_BOUND('',#3346,.T.);
#2463=FACE_OUTER_BOUND('',#3347,.T.);
#2464=FACE_OUTER_BOUND('',#3348,.T.);
#2465=FACE_OUTER_BOUND('',#3349,.T.);
#2466=FACE_OUTER_BOUND('',#3350,.T.);
#2467=FACE_OUTER_BOUND('',#3351,.T.);
#2468=FACE_OUTER_BOUND('',#3352,.T.);
#2469=FACE_OUTER_BOUND('',#3353,.T.);
#2470=FACE_OUTER_BOUND('',#3354,.T.);
#2471=FACE_OUTER_BOUND('',#3355,.T.);
#2472=FACE_OUTER_BOUND('',#3356,.T.);
#2473=FACE_OUTER_BOUND('',#3357,.T.);
#2474=FACE_OUTER_BOUND('',#3358,.T.);
#2475=FACE_OUTER_BOUND('',#3359,.T.);
#2476=FACE_OUTER_BOUND('',#3360,.T.);
#2477=FACE_OUTER_BOUND('',#3361,.T.);
#2478=FACE_OUTER_BOUND('',#3362,.T.);
#2479=FACE_OUTER_BOUND('',#3363,.T.);
#2480=FACE_OUTER_BOUND('',#3364,.T.);
#2481=FACE_OUTER_BOUND('',#3365,.T.);
#2482=FACE_OUTER_BOUND('',#3371,.T.);
#2483=FACE_OUTER_BOUND('',#3372,.T.);
#2484=FACE_OUTER_BOUND('',#3373,.T.);
#2485=FACE_OUTER_BOUND('',#3374,.T.);
#2486=FACE_OUTER_BOUND('',#3375,.T.);
#2487=FACE_OUTER_BOUND('',#3376,.T.);
#2488=FACE_OUTER_BOUND('',#3384,.T.);
#2489=FACE_OUTER_BOUND('',#3385,.T.);
#2490=FACE_OUTER_BOUND('',#3387,.T.);
#2491=FACE_OUTER_BOUND('',#3388,.T.);
#2492=FACE_OUTER_BOUND('',#3389,.T.);
#2493=FACE_OUTER_BOUND('',#3390,.T.);
#2494=FACE_OUTER_BOUND('',#3391,.T.);
#2495=FACE_OUTER_BOUND('',#3392,.T.);
#2496=FACE_OUTER_BOUND('',#3393,.T.);
#2497=FACE_OUTER_BOUND('',#3394,.T.);
#2498=FACE_OUTER_BOUND('',#3395,.T.);
#2499=FACE_OUTER_BOUND('',#3396,.T.);
#2500=FACE_OUTER_BOUND('',#3397,.T.);
#2501=FACE_OUTER_BOUND('',#3398,.T.);
#2502=FACE_OUTER_BOUND('',#3399,.T.);
#2503=FACE_OUTER_BOUND('',#3400,.T.);
#2504=FACE_OUTER_BOUND('',#3401,.T.);
#2505=FACE_OUTER_BOUND('',#3402,.T.);
#2506=FACE_OUTER_BOUND('',#3403,.T.);
#2507=FACE_OUTER_BOUND('',#3404,.T.);
#2508=FACE_OUTER_BOUND('',#3405,.T.);
#2509=FACE_OUTER_BOUND('',#3406,.T.);
#2510=FACE_OUTER_BOUND('',#3407,.T.);
#2511=FACE_OUTER_BOUND('',#3408,.T.);
#2512=FACE_OUTER_BOUND('',#3409,.T.);
#2513=FACE_OUTER_BOUND('',#3410,.T.);
#2514=FACE_OUTER_BOUND('',#3411,.T.);
#2515=FACE_OUTER_BOUND('',#3412,.T.);
#2516=FACE_OUTER_BOUND('',#3413,.T.);
#2517=FACE_OUTER_BOUND('',#3414,.T.);
#2518=FACE_OUTER_BOUND('',#3415,.T.);
#2519=FACE_OUTER_BOUND('',#3416,.T.);
#2520=FACE_OUTER_BOUND('',#3417,.T.);
#2521=FACE_OUTER_BOUND('',#3418,.T.);
#2522=FACE_OUTER_BOUND('',#3419,.T.);
#2523=FACE_OUTER_BOUND('',#3420,.T.);
#2524=FACE_OUTER_BOUND('',#3421,.T.);
#2525=FACE_OUTER_BOUND('',#3422,.T.);
#2526=FACE_OUTER_BOUND('',#3423,.T.);
#2527=FACE_OUTER_BOUND('',#3424,.T.);
#2528=FACE_OUTER_BOUND('',#3425,.T.);
#2529=FACE_OUTER_BOUND('',#3426,.T.);
#2530=FACE_OUTER_BOUND('',#3427,.T.);
#2531=FACE_OUTER_BOUND('',#3429,.T.);
#2532=FACE_OUTER_BOUND('',#3430,.T.);
#2533=FACE_OUTER_BOUND('',#3431,.T.);
#2534=FACE_OUTER_BOUND('',#3432,.T.);
#2535=FACE_OUTER_BOUND('',#3433,.T.);
#2536=FACE_OUTER_BOUND('',#3434,.T.);
#2537=FACE_OUTER_BOUND('',#3435,.T.);
#2538=FACE_OUTER_BOUND('',#3436,.T.);
#2539=FACE_OUTER_BOUND('',#3437,.T.);
#2540=FACE_OUTER_BOUND('',#3438,.T.);
#2541=FACE_OUTER_BOUND('',#3439,.T.);
#2542=FACE_OUTER_BOUND('',#3440,.T.);
#2543=FACE_OUTER_BOUND('',#3441,.T.);
#2544=FACE_OUTER_BOUND('',#3442,.T.);
#2545=FACE_OUTER_BOUND('',#3444,.T.);
#2546=FACE_OUTER_BOUND('',#3445,.T.);
#2547=FACE_OUTER_BOUND('',#3446,.T.);
#2548=FACE_OUTER_BOUND('',#3448,.T.);
#2549=FACE_OUTER_BOUND('',#3455,.T.);
#2550=FACE_OUTER_BOUND('',#3457,.T.);
#2551=FACE_OUTER_BOUND('',#3458,.T.);
#2552=FACE_OUTER_BOUND('',#3459,.T.);
#2553=FACE_OUTER_BOUND('',#3460,.T.);
#2554=FACE_OUTER_BOUND('',#3461,.T.);
#2555=FACE_OUTER_BOUND('',#3463,.T.);
#2556=FACE_OUTER_BOUND('',#3464,.T.);
#2557=FACE_OUTER_BOUND('',#3465,.T.);
#2558=FACE_OUTER_BOUND('',#3466,.T.);
#2559=FACE_OUTER_BOUND('',#3467,.T.);
#2560=FACE_OUTER_BOUND('',#3468,.T.);
#2561=FACE_OUTER_BOUND('',#3469,.T.);
#2562=FACE_OUTER_BOUND('',#3470,.T.);
#2563=FACE_OUTER_BOUND('',#3471,.T.);
#2564=FACE_OUTER_BOUND('',#3474,.T.);
#2565=FACE_OUTER_BOUND('',#3477,.T.);
#2566=FACE_OUTER_BOUND('',#3478,.T.);
#2567=FACE_OUTER_BOUND('',#3479,.T.);
#2568=FACE_OUTER_BOUND('',#3480,.T.);
#2569=FACE_OUTER_BOUND('',#3481,.T.);
#2570=FACE_OUTER_BOUND('',#3482,.T.);
#2571=FACE_OUTER_BOUND('',#3483,.T.);
#2572=FACE_OUTER_BOUND('',#3484,.T.);
#2573=FACE_OUTER_BOUND('',#3485,.T.);
#2574=FACE_OUTER_BOUND('',#3486,.T.);
#2575=FACE_OUTER_BOUND('',#3487,.T.);
#2576=FACE_OUTER_BOUND('',#3488,.T.);
#2577=FACE_OUTER_BOUND('',#3489,.T.);
#2578=FACE_OUTER_BOUND('',#3490,.T.);
#2579=FACE_OUTER_BOUND('',#3491,.T.);
#2580=FACE_OUTER_BOUND('',#3492,.T.);
#2581=FACE_OUTER_BOUND('',#3493,.T.);
#2582=FACE_OUTER_BOUND('',#3494,.T.);
#2583=FACE_OUTER_BOUND('',#3495,.T.);
#2584=FACE_OUTER_BOUND('',#3496,.T.);
#2585=FACE_OUTER_BOUND('',#3497,.T.);
#2586=FACE_OUTER_BOUND('',#3498,.T.);
#2587=FACE_OUTER_BOUND('',#3499,.T.);
#2588=FACE_OUTER_BOUND('',#3500,.T.);
#2589=FACE_OUTER_BOUND('',#3501,.T.);
#2590=FACE_OUTER_BOUND('',#3502,.T.);
#2591=FACE_OUTER_BOUND('',#3503,.T.);
#2592=FACE_OUTER_BOUND('',#3504,.T.);
#2593=FACE_OUTER_BOUND('',#3505,.T.);
#2594=FACE_OUTER_BOUND('',#3506,.T.);
#2595=FACE_OUTER_BOUND('',#3507,.T.);
#2596=FACE_OUTER_BOUND('',#3508,.T.);
#2597=FACE_OUTER_BOUND('',#3510,.T.);
#2598=FACE_OUTER_BOUND('',#3511,.T.);
#2599=FACE_OUTER_BOUND('',#3513,.T.);
#2600=FACE_OUTER_BOUND('',#3514,.T.);
#2601=FACE_OUTER_BOUND('',#3516,.T.);
#2602=FACE_OUTER_BOUND('',#3518,.T.);
#2603=FACE_OUTER_BOUND('',#3520,.T.);
#2604=FACE_OUTER_BOUND('',#3521,.T.);
#2605=FACE_OUTER_BOUND('',#3523,.T.);
#2606=FACE_OUTER_BOUND('',#3524,.T.);
#2607=FACE_OUTER_BOUND('',#3526,.T.);
#2608=FACE_OUTER_BOUND('',#3527,.T.);
#2609=FACE_OUTER_BOUND('',#3529,.T.);
#2610=FACE_OUTER_BOUND('',#3531,.T.);
#2611=FACE_OUTER_BOUND('',#3532,.T.);
#2612=FACE_OUTER_BOUND('',#3534,.T.);
#2613=FACE_OUTER_BOUND('',#3535,.T.);
#2614=FACE_OUTER_BOUND('',#3536,.T.);
#2615=FACE_OUTER_BOUND('',#3537,.T.);
#2616=FACE_OUTER_BOUND('',#3538,.T.);
#2617=FACE_OUTER_BOUND('',#3539,.T.);
#2618=FACE_OUTER_BOUND('',#3540,.T.);
#2619=FACE_OUTER_BOUND('',#3541,.T.);
#2620=FACE_OUTER_BOUND('',#3543,.T.);
#2621=FACE_OUTER_BOUND('',#3544,.T.);
#2622=FACE_OUTER_BOUND('',#3545,.T.);
#2623=FACE_OUTER_BOUND('',#3546,.T.);
#2624=FACE_OUTER_BOUND('',#3547,.T.);
#2625=FACE_OUTER_BOUND('',#3548,.T.);
#2626=FACE_OUTER_BOUND('',#3549,.T.);
#2627=FACE_OUTER_BOUND('',#3550,.T.);
#2628=FACE_OUTER_BOUND('',#3551,.T.);
#2629=FACE_OUTER_BOUND('',#3552,.T.);
#2630=FACE_OUTER_BOUND('',#3553,.T.);
#2631=FACE_OUTER_BOUND('',#3554,.T.);
#2632=FACE_OUTER_BOUND('',#3555,.T.);
#2633=FACE_OUTER_BOUND('',#3561,.T.);
#2634=FACE_OUTER_BOUND('',#3562,.T.);
#2635=FACE_OUTER_BOUND('',#3563,.T.);
#2636=FACE_OUTER_BOUND('',#3564,.T.);
#2637=FACE_OUTER_BOUND('',#3566,.T.);
#2638=FACE_OUTER_BOUND('',#3567,.T.);
#2639=FACE_OUTER_BOUND('',#3568,.T.);
#2640=FACE_OUTER_BOUND('',#3569,.T.);
#2641=FACE_OUTER_BOUND('',#3570,.T.);
#2642=FACE_OUTER_BOUND('',#3572,.T.);
#2643=FACE_OUTER_BOUND('',#3573,.T.);
#2644=FACE_OUTER_BOUND('',#3574,.T.);
#2645=FACE_OUTER_BOUND('',#3575,.T.);
#2646=FACE_OUTER_BOUND('',#3576,.T.);
#2647=FACE_OUTER_BOUND('',#3578,.T.);
#2648=FACE_OUTER_BOUND('',#3579,.T.);
#2649=FACE_OUTER_BOUND('',#3580,.T.);
#2650=FACE_OUTER_BOUND('',#3581,.T.);
#2651=FACE_OUTER_BOUND('',#3582,.T.);
#2652=FACE_OUTER_BOUND('',#3584,.T.);
#2653=FACE_OUTER_BOUND('',#3585,.T.);
#2654=FACE_OUTER_BOUND('',#3586,.T.);
#2655=FACE_OUTER_BOUND('',#3587,.T.);
#2656=FACE_OUTER_BOUND('',#3589,.T.);
#2657=FACE_OUTER_BOUND('',#3590,.T.);
#2658=FACE_OUTER_BOUND('',#3591,.T.);
#2659=FACE_OUTER_BOUND('',#3592,.T.);
#2660=FACE_OUTER_BOUND('',#3593,.T.);
#2661=FACE_OUTER_BOUND('',#3594,.T.);
#2662=FACE_OUTER_BOUND('',#3600,.T.);
#2663=FACE_OUTER_BOUND('',#3601,.T.);
#2664=FACE_OUTER_BOUND('',#3602,.T.);
#2665=FACE_OUTER_BOUND('',#3603,.T.);
#2666=FACE_OUTER_BOUND('',#3604,.T.);
#2667=FACE_OUTER_BOUND('',#3605,.T.);
#2668=FACE_OUTER_BOUND('',#3606,.T.);
#2669=FACE_OUTER_BOUND('',#3607,.T.);
#2670=FACE_OUTER_BOUND('',#3608,.T.);
#2671=FACE_OUTER_BOUND('',#3609,.T.);
#2672=FACE_OUTER_BOUND('',#3610,.T.);
#2673=FACE_OUTER_BOUND('',#3611,.T.);
#2674=FACE_OUTER_BOUND('',#3612,.T.);
#2675=FACE_OUTER_BOUND('',#3622,.T.);
#2676=FACE_OUTER_BOUND('',#3623,.T.);
#2677=FACE_OUTER_BOUND('',#3624,.T.);
#2678=FACE_OUTER_BOUND('',#3625,.T.);
#2679=FACE_OUTER_BOUND('',#3627,.T.);
#2680=FACE_OUTER_BOUND('',#3628,.T.);
#2681=FACE_OUTER_BOUND('',#3629,.T.);
#2682=FACE_OUTER_BOUND('',#3630,.T.);
#2683=FACE_OUTER_BOUND('',#3631,.T.);
#2684=FACE_OUTER_BOUND('',#3633,.T.);
#2685=FACE_OUTER_BOUND('',#3634,.T.);
#2686=FACE_OUTER_BOUND('',#3635,.T.);
#2687=FACE_OUTER_BOUND('',#3636,.T.);
#2688=FACE_OUTER_BOUND('',#3637,.T.);
#2689=FACE_OUTER_BOUND('',#3639,.T.);
#2690=FACE_OUTER_BOUND('',#3640,.T.);
#2691=FACE_OUTER_BOUND('',#3641,.T.);
#2692=FACE_OUTER_BOUND('',#3642,.T.);
#2693=FACE_OUTER_BOUND('',#3643,.T.);
#2694=FACE_OUTER_BOUND('',#3645,.T.);
#2695=FACE_OUTER_BOUND('',#3646,.T.);
#2696=FACE_OUTER_BOUND('',#3647,.T.);
#2697=FACE_OUTER_BOUND('',#3648,.T.);
#2698=FACE_OUTER_BOUND('',#3649,.T.);
#2699=FACE_OUTER_BOUND('',#3650,.T.);
#2700=FACE_OUTER_BOUND('',#3651,.T.);
#2701=FACE_OUTER_BOUND('',#3652,.T.);
#2702=FACE_OUTER_BOUND('',#3653,.T.);
#2703=FACE_OUTER_BOUND('',#3654,.T.);
#2704=FACE_OUTER_BOUND('',#3655,.T.);
#2705=FACE_OUTER_BOUND('',#3656,.T.);
#2706=FACE_OUTER_BOUND('',#3657,.T.);
#2707=FACE_OUTER_BOUND('',#3658,.T.);
#2708=FACE_OUTER_BOUND('',#3659,.T.);
#2709=FACE_OUTER_BOUND('',#3660,.T.);
#2710=FACE_OUTER_BOUND('',#3661,.T.);
#2711=FACE_OUTER_BOUND('',#3662,.T.);
#2712=FACE_OUTER_BOUND('',#3663,.T.);
#2713=FACE_OUTER_BOUND('',#3664,.T.);
#2714=FACE_OUTER_BOUND('',#3665,.T.);
#2715=FACE_OUTER_BOUND('',#3666,.T.);
#2716=FACE_OUTER_BOUND('',#3667,.T.);
#2717=FACE_OUTER_BOUND('',#3668,.T.);
#2718=FACE_OUTER_BOUND('',#3669,.T.);
#2719=FACE_OUTER_BOUND('',#3670,.T.);
#2720=FACE_OUTER_BOUND('',#3671,.T.);
#2721=FACE_OUTER_BOUND('',#3672,.T.);
#2722=FACE_OUTER_BOUND('',#3673,.T.);
#2723=FACE_OUTER_BOUND('',#3674,.T.);
#2724=FACE_OUTER_BOUND('',#3675,.T.);
#2725=FACE_OUTER_BOUND('',#3676,.T.);
#2726=FACE_OUTER_BOUND('',#3682,.T.);
#2727=FACE_OUTER_BOUND('',#3683,.T.);
#2728=FACE_OUTER_BOUND('',#3684,.T.);
#2729=FACE_OUTER_BOUND('',#3685,.T.);
#2730=FACE_OUTER_BOUND('',#3686,.T.);
#2731=FACE_OUTER_BOUND('',#3700,.T.);
#2732=FACE_OUTER_BOUND('',#3701,.T.);
#2733=FACE_OUTER_BOUND('',#3702,.T.);
#2734=FACE_OUTER_BOUND('',#3703,.T.);
#2735=FACE_OUTER_BOUND('',#3704,.T.);
#2736=FACE_OUTER_BOUND('',#3705,.T.);
#2737=FACE_OUTER_BOUND('',#3706,.T.);
#2738=FACE_OUTER_BOUND('',#3707,.T.);
#2739=FACE_OUTER_BOUND('',#3708,.T.);
#2740=FACE_OUTER_BOUND('',#3709,.T.);
#2741=FACE_OUTER_BOUND('',#3710,.T.);
#2742=FACE_OUTER_BOUND('',#3711,.T.);
#2743=FACE_OUTER_BOUND('',#3712,.T.);
#2744=FACE_OUTER_BOUND('',#3713,.T.);
#2745=FACE_OUTER_BOUND('',#3714,.T.);
#2746=FACE_OUTER_BOUND('',#3715,.T.);
#2747=FACE_OUTER_BOUND('',#3716,.T.);
#2748=FACE_OUTER_BOUND('',#3717,.T.);
#2749=FACE_OUTER_BOUND('',#3718,.T.);
#2750=FACE_OUTER_BOUND('',#3719,.T.);
#2751=FACE_OUTER_BOUND('',#3720,.T.);
#2752=FACE_OUTER_BOUND('',#3721,.T.);
#2753=FACE_OUTER_BOUND('',#3722,.T.);
#2754=FACE_OUTER_BOUND('',#3723,.T.);
#2755=FACE_OUTER_BOUND('',#3724,.T.);
#2756=FACE_OUTER_BOUND('',#3725,.T.);
#2757=FACE_OUTER_BOUND('',#3726,.T.);
#2758=FACE_OUTER_BOUND('',#3728,.T.);
#2759=FACE_OUTER_BOUND('',#3729,.T.);
#2760=FACE_OUTER_BOUND('',#3730,.T.);
#2761=FACE_OUTER_BOUND('',#3732,.T.);
#2762=FACE_OUTER_BOUND('',#3734,.T.);
#2763=FACE_OUTER_BOUND('',#3735,.T.);
#2764=FACE_OUTER_BOUND('',#3736,.T.);
#2765=FACE_OUTER_BOUND('',#3738,.T.);
#2766=FACE_OUTER_BOUND('',#3739,.T.);
#2767=FACE_OUTER_BOUND('',#3740,.T.);
#2768=FACE_OUTER_BOUND('',#3742,.T.);
#2769=FACE_OUTER_BOUND('',#3743,.T.);
#2770=FACE_OUTER_BOUND('',#3744,.T.);
#2771=FACE_OUTER_BOUND('',#3746,.T.);
#2772=FACE_OUTER_BOUND('',#3747,.T.);
#2773=FACE_OUTER_BOUND('',#3749,.T.);
#2774=FACE_OUTER_BOUND('',#3750,.T.);
#2775=FACE_OUTER_BOUND('',#3751,.T.);
#2776=FACE_OUTER_BOUND('',#3752,.T.);
#2777=FACE_OUTER_BOUND('',#3753,.T.);
#2778=FACE_OUTER_BOUND('',#3754,.T.);
#2779=FACE_OUTER_BOUND('',#3755,.T.);
#2780=FACE_OUTER_BOUND('',#3756,.T.);
#2781=FACE_OUTER_BOUND('',#3757,.T.);
#2782=FACE_OUTER_BOUND('',#3758,.T.);
#2783=FACE_OUTER_BOUND('',#3759,.T.);
#2784=FACE_OUTER_BOUND('',#3760,.T.);
#2785=FACE_OUTER_BOUND('',#3761,.T.);
#2786=FACE_OUTER_BOUND('',#3762,.T.);
#2787=FACE_OUTER_BOUND('',#3763,.T.);
#2788=FACE_OUTER_BOUND('',#3764,.T.);
#2789=FACE_OUTER_BOUND('',#3765,.T.);
#2790=FACE_OUTER_BOUND('',#3766,.T.);
#2791=FACE_OUTER_BOUND('',#3767,.T.);
#2792=FACE_OUTER_BOUND('',#3768,.T.);
#2793=FACE_OUTER_BOUND('',#3769,.T.);
#2794=FACE_OUTER_BOUND('',#3770,.T.);
#2795=FACE_OUTER_BOUND('',#3771,.T.);
#2796=FACE_OUTER_BOUND('',#3772,.T.);
#2797=FACE_OUTER_BOUND('',#3773,.T.);
#2798=FACE_OUTER_BOUND('',#3774,.T.);
#2799=FACE_OUTER_BOUND('',#3775,.T.);
#2800=FACE_OUTER_BOUND('',#3776,.T.);
#2801=FACE_OUTER_BOUND('',#3777,.T.);
#2802=FACE_OUTER_BOUND('',#3778,.T.);
#2803=FACE_OUTER_BOUND('',#3779,.T.);
#2804=FACE_OUTER_BOUND('',#3780,.T.);
#2805=FACE_OUTER_BOUND('',#3781,.T.);
#2806=FACE_OUTER_BOUND('',#3782,.T.);
#2807=FACE_OUTER_BOUND('',#3783,.T.);
#2808=FACE_OUTER_BOUND('',#3784,.T.);
#2809=FACE_OUTER_BOUND('',#3785,.T.);
#2810=FACE_OUTER_BOUND('',#3786,.T.);
#2811=FACE_OUTER_BOUND('',#3787,.T.);
#2812=FACE_OUTER_BOUND('',#3788,.T.);
#2813=FACE_OUTER_BOUND('',#3789,.T.);
#2814=FACE_OUTER_BOUND('',#3790,.T.);
#2815=FACE_OUTER_BOUND('',#3791,.T.);
#2816=FACE_OUTER_BOUND('',#3792,.T.);
#2817=FACE_OUTER_BOUND('',#3793,.T.);
#2818=FACE_OUTER_BOUND('',#3794,.T.);
#2819=FACE_OUTER_BOUND('',#3795,.T.);
#2820=FACE_OUTER_BOUND('',#3796,.T.);
#2821=FACE_OUTER_BOUND('',#3797,.T.);
#2822=FACE_OUTER_BOUND('',#3798,.T.);
#2823=FACE_OUTER_BOUND('',#3799,.T.);
#2824=FACE_OUTER_BOUND('',#3800,.T.);
#2825=FACE_OUTER_BOUND('',#3801,.T.);
#2826=FACE_OUTER_BOUND('',#3802,.T.);
#2827=FACE_OUTER_BOUND('',#3803,.T.);
#2828=FACE_OUTER_BOUND('',#3804,.T.);
#2829=FACE_OUTER_BOUND('',#3805,.T.);
#2830=FACE_OUTER_BOUND('',#3806,.T.);
#2831=FACE_OUTER_BOUND('',#3807,.T.);
#2832=FACE_OUTER_BOUND('',#3808,.T.);
#2833=FACE_OUTER_BOUND('',#3809,.T.);
#2834=FACE_OUTER_BOUND('',#3810,.T.);
#2835=FACE_OUTER_BOUND('',#3811,.T.);
#2836=FACE_OUTER_BOUND('',#3812,.T.);
#2837=FACE_OUTER_BOUND('',#3813,.T.);
#2838=FACE_OUTER_BOUND('',#3814,.T.);
#2839=FACE_OUTER_BOUND('',#3815,.T.);
#2840=FACE_OUTER_BOUND('',#3816,.T.);
#2841=FACE_OUTER_BOUND('',#3817,.T.);
#2842=FACE_OUTER_BOUND('',#3818,.T.);
#2843=FACE_OUTER_BOUND('',#3819,.T.);
#2844=FACE_OUTER_BOUND('',#3820,.T.);
#2845=FACE_OUTER_BOUND('',#3821,.T.);
#2846=FACE_OUTER_BOUND('',#3822,.T.);
#2847=FACE_OUTER_BOUND('',#3823,.T.);
#2848=FACE_OUTER_BOUND('',#3824,.T.);
#2849=FACE_OUTER_BOUND('',#3825,.T.);
#2850=FACE_OUTER_BOUND('',#3826,.T.);
#2851=FACE_OUTER_BOUND('',#3827,.T.);
#2852=FACE_OUTER_BOUND('',#3828,.T.);
#2853=FACE_OUTER_BOUND('',#3829,.T.);
#2854=FACE_OUTER_BOUND('',#3830,.T.);
#2855=FACE_OUTER_BOUND('',#3831,.T.);
#2856=FACE_OUTER_BOUND('',#3832,.T.);
#2857=FACE_OUTER_BOUND('',#3833,.T.);
#2858=FACE_OUTER_BOUND('',#3834,.T.);
#2859=FACE_OUTER_BOUND('',#3835,.T.);
#2860=FACE_OUTER_BOUND('',#3836,.T.);
#2861=FACE_OUTER_BOUND('',#3837,.T.);
#2862=FACE_OUTER_BOUND('',#3838,.T.);
#2863=FACE_OUTER_BOUND('',#3839,.T.);
#2864=FACE_OUTER_BOUND('',#3840,.T.);
#2865=FACE_OUTER_BOUND('',#3841,.T.);
#2866=FACE_OUTER_BOUND('',#3842,.T.);
#2867=FACE_OUTER_BOUND('',#3843,.T.);
#2868=FACE_OUTER_BOUND('',#3844,.T.);
#2869=FACE_OUTER_BOUND('',#3845,.T.);
#2870=FACE_OUTER_BOUND('',#3846,.T.);
#2871=FACE_OUTER_BOUND('',#3847,.T.);
#2872=FACE_OUTER_BOUND('',#3848,.T.);
#2873=FACE_OUTER_BOUND('',#3849,.T.);
#2874=FACE_OUTER_BOUND('',#3850,.T.);
#2875=FACE_OUTER_BOUND('',#3851,.T.);
#2876=FACE_OUTER_BOUND('',#3852,.T.);
#2877=FACE_OUTER_BOUND('',#3853,.T.);
#2878=FACE_OUTER_BOUND('',#3854,.T.);
#2879=FACE_OUTER_BOUND('',#3855,.T.);
#2880=FACE_OUTER_BOUND('',#3856,.T.);
#2881=FACE_OUTER_BOUND('',#3857,.T.);
#2882=FACE_OUTER_BOUND('',#3858,.T.);
#2883=FACE_OUTER_BOUND('',#3859,.T.);
#2884=FACE_OUTER_BOUND('',#3860,.T.);
#2885=FACE_OUTER_BOUND('',#3861,.T.);
#2886=FACE_OUTER_BOUND('',#3862,.T.);
#2887=FACE_OUTER_BOUND('',#3863,.T.);
#2888=FACE_OUTER_BOUND('',#3864,.T.);
#2889=FACE_OUTER_BOUND('',#3865,.T.);
#2890=FACE_OUTER_BOUND('',#3866,.T.);
#2891=FACE_OUTER_BOUND('',#3867,.T.);
#2892=FACE_OUTER_BOUND('',#3868,.T.);
#2893=FACE_OUTER_BOUND('',#3869,.T.);
#2894=FACE_OUTER_BOUND('',#3870,.T.);
#2895=FACE_OUTER_BOUND('',#3871,.T.);
#2896=FACE_OUTER_BOUND('',#3872,.T.);
#2897=FACE_OUTER_BOUND('',#3873,.T.);
#2898=FACE_OUTER_BOUND('',#3874,.T.);
#2899=FACE_OUTER_BOUND('',#3875,.T.);
#2900=FACE_OUTER_BOUND('',#3876,.T.);
#2901=FACE_OUTER_BOUND('',#3877,.T.);
#2902=FACE_OUTER_BOUND('',#3878,.T.);
#2903=FACE_OUTER_BOUND('',#3879,.T.);
#2904=FACE_OUTER_BOUND('',#3880,.T.);
#2905=FACE_OUTER_BOUND('',#3881,.T.);
#2906=FACE_OUTER_BOUND('',#3882,.T.);
#2907=FACE_OUTER_BOUND('',#3883,.T.);
#2908=FACE_OUTER_BOUND('',#3884,.T.);
#2909=FACE_OUTER_BOUND('',#3885,.T.);
#2910=FACE_OUTER_BOUND('',#3886,.T.);
#2911=FACE_OUTER_BOUND('',#3887,.T.);
#2912=FACE_OUTER_BOUND('',#3888,.T.);
#2913=FACE_OUTER_BOUND('',#3889,.T.);
#2914=FACE_OUTER_BOUND('',#3890,.T.);
#2915=FACE_OUTER_BOUND('',#3891,.T.);
#2916=FACE_OUTER_BOUND('',#3892,.T.);
#2917=FACE_OUTER_BOUND('',#3893,.T.);
#2918=FACE_OUTER_BOUND('',#3894,.T.);
#2919=FACE_OUTER_BOUND('',#3895,.T.);
#2920=FACE_OUTER_BOUND('',#3896,.T.);
#2921=FACE_OUTER_BOUND('',#3897,.T.);
#2922=FACE_OUTER_BOUND('',#3898,.T.);
#2923=FACE_OUTER_BOUND('',#3899,.T.);
#2924=FACE_OUTER_BOUND('',#3900,.T.);
#2925=FACE_OUTER_BOUND('',#3901,.T.);
#2926=FACE_OUTER_BOUND('',#3902,.T.);
#2927=FACE_OUTER_BOUND('',#3903,.T.);
#2928=FACE_OUTER_BOUND('',#3904,.T.);
#2929=FACE_OUTER_BOUND('',#3905,.T.);
#2930=FACE_OUTER_BOUND('',#3906,.T.);
#2931=FACE_OUTER_BOUND('',#3907,.T.);
#2932=FACE_OUTER_BOUND('',#3908,.T.);
#2933=FACE_OUTER_BOUND('',#3909,.T.);
#2934=FACE_OUTER_BOUND('',#3910,.T.);
#2935=FACE_OUTER_BOUND('',#3911,.T.);
#2936=FACE_OUTER_BOUND('',#3912,.T.);
#2937=FACE_OUTER_BOUND('',#3913,.T.);
#2938=FACE_OUTER_BOUND('',#3914,.T.);
#2939=FACE_OUTER_BOUND('',#3915,.T.);
#2940=FACE_OUTER_BOUND('',#3916,.T.);
#2941=FACE_OUTER_BOUND('',#3917,.T.);
#2942=FACE_OUTER_BOUND('',#3918,.T.);
#2943=FACE_OUTER_BOUND('',#3919,.T.);
#2944=FACE_OUTER_BOUND('',#3920,.T.);
#2945=FACE_OUTER_BOUND('',#3921,.T.);
#2946=FACE_OUTER_BOUND('',#3922,.T.);
#2947=FACE_OUTER_BOUND('',#3923,.T.);
#2948=FACE_OUTER_BOUND('',#3924,.T.);
#2949=FACE_OUTER_BOUND('',#3925,.T.);
#2950=FACE_OUTER_BOUND('',#3926,.T.);
#2951=FACE_OUTER_BOUND('',#3927,.T.);
#2952=FACE_OUTER_BOUND('',#3928,.T.);
#2953=FACE_OUTER_BOUND('',#3929,.T.);
#2954=FACE_OUTER_BOUND('',#3930,.T.);
#2955=FACE_OUTER_BOUND('',#3931,.T.);
#2956=FACE_OUTER_BOUND('',#3932,.T.);
#2957=FACE_OUTER_BOUND('',#3933,.T.);
#2958=FACE_OUTER_BOUND('',#3934,.T.);
#2959=FACE_OUTER_BOUND('',#3935,.T.);
#2960=FACE_OUTER_BOUND('',#3936,.T.);
#2961=FACE_OUTER_BOUND('',#3937,.T.);
#2962=FACE_OUTER_BOUND('',#3938,.T.);
#2963=FACE_OUTER_BOUND('',#3939,.T.);
#2964=FACE_OUTER_BOUND('',#3940,.T.);
#2965=FACE_OUTER_BOUND('',#3941,.T.);
#2966=FACE_OUTER_BOUND('',#3942,.T.);
#2967=FACE_OUTER_BOUND('',#3943,.T.);
#2968=FACE_OUTER_BOUND('',#3944,.T.);
#2969=FACE_OUTER_BOUND('',#3945,.T.);
#2970=FACE_OUTER_BOUND('',#3946,.T.);
#2971=FACE_OUTER_BOUND('',#3947,.T.);
#2972=FACE_OUTER_BOUND('',#3948,.T.);
#2973=FACE_OUTER_BOUND('',#3949,.T.);
#2974=FACE_OUTER_BOUND('',#3950,.T.);
#2975=FACE_OUTER_BOUND('',#3951,.T.);
#2976=FACE_OUTER_BOUND('',#3952,.T.);
#2977=FACE_OUTER_BOUND('',#3953,.T.);
#2978=FACE_OUTER_BOUND('',#3954,.T.);
#2979=FACE_OUTER_BOUND('',#3955,.T.);
#2980=FACE_OUTER_BOUND('',#3956,.T.);
#2981=FACE_OUTER_BOUND('',#3957,.T.);
#2982=FACE_OUTER_BOUND('',#3958,.T.);
#2983=FACE_OUTER_BOUND('',#3959,.T.);
#2984=FACE_OUTER_BOUND('',#3960,.T.);
#2985=FACE_OUTER_BOUND('',#3961,.T.);
#2986=FACE_OUTER_BOUND('',#3962,.T.);
#2987=FACE_OUTER_BOUND('',#3963,.T.);
#2988=FACE_OUTER_BOUND('',#3964,.T.);
#2989=FACE_OUTER_BOUND('',#3965,.T.);
#2990=FACE_OUTER_BOUND('',#3966,.T.);
#2991=FACE_OUTER_BOUND('',#3967,.T.);
#2992=FACE_OUTER_BOUND('',#3968,.T.);
#2993=FACE_OUTER_BOUND('',#3969,.T.);
#2994=FACE_OUTER_BOUND('',#3970,.T.);
#2995=FACE_OUTER_BOUND('',#3971,.T.);
#2996=FACE_OUTER_BOUND('',#3972,.T.);
#2997=FACE_OUTER_BOUND('',#3973,.T.);
#2998=FACE_OUTER_BOUND('',#3974,.T.);
#2999=FACE_OUTER_BOUND('',#3975,.T.);
#3000=FACE_OUTER_BOUND('',#3976,.T.);
#3001=FACE_OUTER_BOUND('',#3977,.T.);
#3002=FACE_OUTER_BOUND('',#3978,.T.);
#3003=FACE_OUTER_BOUND('',#3979,.T.);
#3004=FACE_OUTER_BOUND('',#3980,.T.);
#3005=FACE_OUTER_BOUND('',#3981,.T.);
#3006=FACE_OUTER_BOUND('',#3982,.T.);
#3007=FACE_OUTER_BOUND('',#3983,.T.);
#3008=FACE_OUTER_BOUND('',#3984,.T.);
#3009=FACE_OUTER_BOUND('',#3985,.T.);
#3010=FACE_OUTER_BOUND('',#3986,.T.);
#3011=FACE_OUTER_BOUND('',#3987,.T.);
#3012=FACE_OUTER_BOUND('',#3988,.T.);
#3013=FACE_OUTER_BOUND('',#3989,.T.);
#3014=FACE_OUTER_BOUND('',#3990,.T.);
#3015=FACE_OUTER_BOUND('',#3991,.T.);
#3016=FACE_OUTER_BOUND('',#3992,.T.);
#3017=FACE_OUTER_BOUND('',#3994,.T.);
#3018=FACE_OUTER_BOUND('',#3995,.T.);
#3019=FACE_OUTER_BOUND('',#3996,.T.);
#3020=FACE_OUTER_BOUND('',#3997,.T.);
#3021=FACE_OUTER_BOUND('',#3999,.T.);
#3022=FACE_OUTER_BOUND('',#4000,.T.);
#3023=FACE_OUTER_BOUND('',#4001,.T.);
#3024=FACE_OUTER_BOUND('',#4003,.T.);
#3025=FACE_OUTER_BOUND('',#4004,.T.);
#3026=FACE_OUTER_BOUND('',#4006,.T.);
#3027=FACE_OUTER_BOUND('',#4007,.T.);
#3028=FACE_OUTER_BOUND('',#4008,.T.);
#3029=FACE_OUTER_BOUND('',#4010,.T.);
#3030=FACE_OUTER_BOUND('',#4011,.T.);
#3031=FACE_OUTER_BOUND('',#4012,.T.);
#3032=FACE_OUTER_BOUND('',#4014,.T.);
#3033=FACE_OUTER_BOUND('',#4015,.T.);
#3034=FACE_OUTER_BOUND('',#4016,.T.);
#3035=FACE_OUTER_BOUND('',#4018,.T.);
#3036=FACE_OUTER_BOUND('',#4019,.T.);
#3037=FACE_OUTER_BOUND('',#4020,.T.);
#3038=FACE_OUTER_BOUND('',#4021,.T.);
#3039=FACE_OUTER_BOUND('',#4023,.T.);
#3040=FACE_OUTER_BOUND('',#4024,.T.);
#3041=FACE_OUTER_BOUND('',#4026,.T.);
#3042=FACE_OUTER_BOUND('',#4027,.T.);
#3043=FACE_OUTER_BOUND('',#4028,.T.);
#3044=FACE_OUTER_BOUND('',#4029,.T.);
#3045=FACE_OUTER_BOUND('',#4030,.T.);
#3046=FACE_OUTER_BOUND('',#4031,.T.);
#3047=FACE_OUTER_BOUND('',#4033,.T.);
#3048=FACE_OUTER_BOUND('',#4034,.T.);
#3049=FACE_OUTER_BOUND('',#4036,.T.);
#3050=FACE_OUTER_BOUND('',#4037,.T.);
#3051=FACE_OUTER_BOUND('',#4039,.T.);
#3052=FACE_OUTER_BOUND('',#4040,.T.);
#3053=FACE_OUTER_BOUND('',#4041,.T.);
#3054=FACE_OUTER_BOUND('',#4042,.T.);
#3055=FACE_OUTER_BOUND('',#4043,.T.);
#3056=FACE_OUTER_BOUND('',#4044,.T.);
#3057=FACE_OUTER_BOUND('',#4045,.T.);
#3058=FACE_OUTER_BOUND('',#4046,.T.);
#3059=FACE_OUTER_BOUND('',#4047,.T.);
#3060=FACE_OUTER_BOUND('',#4048,.T.);
#3061=FACE_OUTER_BOUND('',#4049,.T.);
#3062=FACE_OUTER_BOUND('',#4050,.T.);
#3063=FACE_OUTER_BOUND('',#4051,.T.);
#3064=FACE_OUTER_BOUND('',#4052,.T.);
#3065=FACE_OUTER_BOUND('',#4053,.T.);
#3066=FACE_OUTER_BOUND('',#4054,.T.);
#3067=FACE_OUTER_BOUND('',#4055,.T.);
#3068=FACE_OUTER_BOUND('',#4056,.T.);
#3069=FACE_OUTER_BOUND('',#4057,.T.);
#3070=FACE_OUTER_BOUND('',#4058,.T.);
#3071=FACE_OUTER_BOUND('',#4059,.T.);
#3072=FACE_OUTER_BOUND('',#4060,.T.);
#3073=FACE_OUTER_BOUND('',#4061,.T.);
#3074=FACE_OUTER_BOUND('',#4062,.T.);
#3075=FACE_OUTER_BOUND('',#4063,.T.);
#3076=FACE_OUTER_BOUND('',#4065,.T.);
#3077=FACE_OUTER_BOUND('',#4066,.T.);
#3078=FACE_OUTER_BOUND('',#4067,.T.);
#3079=FACE_OUTER_BOUND('',#4068,.T.);
#3080=FACE_OUTER_BOUND('',#4069,.T.);
#3081=FACE_OUTER_BOUND('',#4071,.T.);
#3082=FACE_OUTER_BOUND('',#4072,.T.);
#3083=FACE_OUTER_BOUND('',#4073,.T.);
#3084=FACE_OUTER_BOUND('',#4074,.T.);
#3085=FACE_OUTER_BOUND('',#4076,.T.);
#3086=FACE_OUTER_BOUND('',#4077,.T.);
#3087=FACE_OUTER_BOUND('',#4079,.T.);
#3088=FACE_OUTER_BOUND('',#4080,.T.);
#3089=FACE_OUTER_BOUND('',#4081,.T.);
#3090=FACE_OUTER_BOUND('',#4082,.T.);
#3091=FACE_OUTER_BOUND('',#4084,.T.);
#3092=FACE_OUTER_BOUND('',#4085,.T.);
#3093=FACE_OUTER_BOUND('',#4086,.T.);
#3094=FACE_OUTER_BOUND('',#4087,.T.);
#3095=FACE_OUTER_BOUND('',#4089,.T.);
#3096=FACE_OUTER_BOUND('',#4090,.T.);
#3097=FACE_OUTER_BOUND('',#4091,.T.);
#3098=FACE_OUTER_BOUND('',#4093,.T.);
#3099=FACE_OUTER_BOUND('',#4094,.T.);
#3100=FACE_OUTER_BOUND('',#4095,.T.);
#3101=FACE_OUTER_BOUND('',#4096,.T.);
#3102=FACE_OUTER_BOUND('',#4097,.T.);
#3103=FACE_OUTER_BOUND('',#4098,.T.);
#3104=FACE_OUTER_BOUND('',#4099,.T.);
#3105=FACE_OUTER_BOUND('',#4100,.T.);
#3106=FACE_OUTER_BOUND('',#4102,.T.);
#3107=FACE_OUTER_BOUND('',#4103,.T.);
#3108=FACE_OUTER_BOUND('',#4105,.T.);
#3109=FACE_OUTER_BOUND('',#4106,.T.);
#3110=FACE_OUTER_BOUND('',#4108,.T.);
#3111=FACE_OUTER_BOUND('',#4110,.T.);
#3112=FACE_OUTER_BOUND('',#4111,.T.);
#3113=FACE_OUTER_BOUND('',#4112,.T.);
#3114=FACE_OUTER_BOUND('',#4114,.T.);
#3115=FACE_OUTER_BOUND('',#4115,.T.);
#3116=FACE_OUTER_BOUND('',#4116,.T.);
#3117=FACE_OUTER_BOUND('',#4118,.T.);
#3118=FACE_OUTER_BOUND('',#4119,.T.);
#3119=FACE_OUTER_BOUND('',#4120,.T.);
#3120=FACE_OUTER_BOUND('',#4121,.T.);
#3121=FACE_OUTER_BOUND('',#4123,.T.);
#3122=FACE_OUTER_BOUND('',#4124,.T.);
#3123=FACE_OUTER_BOUND('',#4126,.T.);
#3124=FACE_OUTER_BOUND('',#4127,.T.);
#3125=FACE_OUTER_BOUND('',#4128,.T.);
#3126=FACE_OUTER_BOUND('',#4129,.T.);
#3127=FACE_OUTER_BOUND('',#4131,.T.);
#3128=FACE_OUTER_BOUND('',#4132,.T.);
#3129=FACE_OUTER_BOUND('',#4134,.T.);
#3130=FACE_OUTER_BOUND('',#4135,.T.);
#3131=FACE_OUTER_BOUND('',#4137,.T.);
#3132=FACE_OUTER_BOUND('',#4138,.T.);
#3133=FACE_OUTER_BOUND('',#4139,.T.);
#3134=FACE_OUTER_BOUND('',#4140,.T.);
#3135=FACE_OUTER_BOUND('',#4142,.T.);
#3136=FACE_OUTER_BOUND('',#4143,.T.);
#3137=FACE_OUTER_BOUND('',#4145,.T.);
#3138=FACE_OUTER_BOUND('',#4146,.T.);
#3139=FACE_OUTER_BOUND('',#4148,.T.);
#3140=FACE_OUTER_BOUND('',#4149,.T.);
#3141=FACE_OUTER_BOUND('',#4151,.T.);
#3142=FACE_OUTER_BOUND('',#4152,.T.);
#3143=FACE_OUTER_BOUND('',#4153,.T.);
#3144=FACE_OUTER_BOUND('',#4154,.T.);
#3145=FACE_OUTER_BOUND('',#4156,.T.);
#3146=FACE_OUTER_BOUND('',#4157,.T.);
#3147=FACE_OUTER_BOUND('',#4159,.T.);
#3148=FACE_OUTER_BOUND('',#4160,.T.);
#3149=FACE_OUTER_BOUND('',#4161,.T.);
#3150=FACE_OUTER_BOUND('',#4162,.T.);
#3151=FACE_OUTER_BOUND('',#4163,.T.);
#3152=FACE_OUTER_BOUND('',#4164,.T.);
#3153=FACE_OUTER_BOUND('',#4165,.T.);
#3154=FACE_OUTER_BOUND('',#4168,.T.);
#3155=FACE_OUTER_BOUND('',#4169,.T.);
#3156=FACE_OUTER_BOUND('',#4172,.T.);
#3157=FACE_OUTER_BOUND('',#4173,.T.);
#3158=FACE_OUTER_BOUND('',#4174,.T.);
#3159=FACE_OUTER_BOUND('',#4175,.T.);
#3160=FACE_OUTER_BOUND('',#4176,.T.);
#3161=FACE_OUTER_BOUND('',#4177,.T.);
#3162=FACE_OUTER_BOUND('',#4178,.T.);
#3163=FACE_OUTER_BOUND('',#4179,.T.);
#3164=FACE_OUTER_BOUND('',#4180,.T.);
#3165=FACE_OUTER_BOUND('',#4181,.T.);
#3166=FACE_OUTER_BOUND('',#4182,.T.);
#3167=FACE_OUTER_BOUND('',#4183,.T.);
#3168=FACE_OUTER_BOUND('',#4184,.T.);
#3169=FACE_OUTER_BOUND('',#4185,.T.);
#3170=FACE_OUTER_BOUND('',#4186,.T.);
#3171=FACE_OUTER_BOUND('',#4187,.T.);
#3172=FACE_OUTER_BOUND('',#4188,.T.);
#3173=FACE_OUTER_BOUND('',#4189,.T.);
#3174=FACE_OUTER_BOUND('',#4190,.T.);
#3175=FACE_OUTER_BOUND('',#4191,.T.);
#3176=FACE_OUTER_BOUND('',#4192,.T.);
#3177=FACE_OUTER_BOUND('',#4193,.T.);
#3178=FACE_OUTER_BOUND('',#4194,.T.);
#3179=FACE_OUTER_BOUND('',#4195,.T.);
#3180=FACE_OUTER_BOUND('',#4196,.T.);
#3181=FACE_OUTER_BOUND('',#4197,.T.);
#3182=FACE_OUTER_BOUND('',#4198,.T.);
#3183=FACE_OUTER_BOUND('',#4199,.T.);
#3184=FACE_OUTER_BOUND('',#4200,.T.);
#3185=FACE_OUTER_BOUND('',#4201,.T.);
#3186=FACE_OUTER_BOUND('',#4202,.T.);
#3187=FACE_OUTER_BOUND('',#4203,.T.);
#3188=FACE_OUTER_BOUND('',#4204,.T.);
#3189=FACE_OUTER_BOUND('',#4205,.T.);
#3190=FACE_OUTER_BOUND('',#4206,.T.);
#3191=FACE_OUTER_BOUND('',#4207,.T.);
#3192=FACE_OUTER_BOUND('',#4208,.T.);
#3193=FACE_OUTER_BOUND('',#4209,.T.);
#3194=FACE_OUTER_BOUND('',#4211,.T.);
#3195=FACE_OUTER_BOUND('',#4212,.T.);
#3196=FACE_OUTER_BOUND('',#4213,.T.);
#3197=FACE_OUTER_BOUND('',#4214,.T.);
#3198=FACE_OUTER_BOUND('',#4215,.T.);
#3199=FACE_OUTER_BOUND('',#4216,.T.);
#3200=FACE_OUTER_BOUND('',#4217,.T.);
#3201=FACE_OUTER_BOUND('',#4218,.T.);
#3202=FACE_OUTER_BOUND('',#4219,.T.);
#3203=FACE_OUTER_BOUND('',#4221,.T.);
#3204=FACE_OUTER_BOUND('',#4222,.T.);
#3205=FACE_OUTER_BOUND('',#4223,.T.);
#3206=FACE_OUTER_BOUND('',#4225,.T.);
#3207=FACE_OUTER_BOUND('',#4226,.T.);
#3208=FACE_OUTER_BOUND('',#4227,.T.);
#3209=FACE_OUTER_BOUND('',#4228,.T.);
#3210=FACE_OUTER_BOUND('',#4229,.T.);
#3211=FACE_OUTER_BOUND('',#4230,.T.);
#3212=FACE_OUTER_BOUND('',#4231,.T.);
#3213=FACE_OUTER_BOUND('',#4232,.T.);
#3214=FACE_OUTER_BOUND('',#4233,.T.);
#3215=FACE_OUTER_BOUND('',#4234,.T.);
#3216=FACE_OUTER_BOUND('',#4235,.T.);
#3217=FACE_OUTER_BOUND('',#4236,.T.);
#3218=FACE_OUTER_BOUND('',#4237,.T.);
#3219=FACE_OUTER_BOUND('',#4238,.T.);
#3220=FACE_OUTER_BOUND('',#4239,.T.);
#3221=FACE_OUTER_BOUND('',#4240,.T.);
#3222=FACE_OUTER_BOUND('',#4241,.T.);
#3223=FACE_OUTER_BOUND('',#4242,.T.);
#3224=FACE_OUTER_BOUND('',#4243,.T.);
#3225=FACE_OUTER_BOUND('',#4244,.T.);
#3226=FACE_OUTER_BOUND('',#4245,.T.);
#3227=FACE_OUTER_BOUND('',#4246,.T.);
#3228=FACE_OUTER_BOUND('',#4247,.T.);
#3229=FACE_OUTER_BOUND('',#4248,.T.);
#3230=FACE_OUTER_BOUND('',#4249,.T.);
#3231=FACE_OUTER_BOUND('',#4250,.T.);
#3232=FACE_OUTER_BOUND('',#4252,.T.);
#3233=FACE_OUTER_BOUND('',#4253,.T.);
#3234=FACE_OUTER_BOUND('',#4254,.T.);
#3235=FACE_OUTER_BOUND('',#4255,.T.);
#3236=FACE_OUTER_BOUND('',#4256,.T.);
#3237=FACE_OUTER_BOUND('',#4257,.T.);
#3238=FACE_OUTER_BOUND('',#4258,.T.);
#3239=FACE_OUTER_BOUND('',#4259,.T.);
#3240=FACE_OUTER_BOUND('',#4260,.T.);
#3241=FACE_OUTER_BOUND('',#4262,.T.);
#3242=FACE_OUTER_BOUND('',#4263,.T.);
#3243=FACE_OUTER_BOUND('',#4264,.T.);
#3244=FACE_OUTER_BOUND('',#4266,.T.);
#3245=FACE_OUTER_BOUND('',#4267,.T.);
#3246=FACE_OUTER_BOUND('',#4268,.T.);
#3247=FACE_OUTER_BOUND('',#4269,.T.);
#3248=FACE_OUTER_BOUND('',#4270,.T.);
#3249=FACE_OUTER_BOUND('',#4272,.T.);
#3250=FACE_OUTER_BOUND('',#4273,.T.);
#3251=FACE_OUTER_BOUND('',#4274,.T.);
#3252=FACE_OUTER_BOUND('',#4276,.T.);
#3253=FACE_OUTER_BOUND('',#4277,.T.);
#3254=FACE_OUTER_BOUND('',#4278,.T.);
#3255=FACE_OUTER_BOUND('',#4279,.T.);
#3256=FACE_OUTER_BOUND('',#4280,.T.);
#3257=EDGE_LOOP('',(#9851,#9852,#9853,#9854));
#3258=EDGE_LOOP('',(#9855,#9856,#9857,#9858));
#3259=EDGE_LOOP('',(#9859,#9860,#9861,#9862));
#3260=EDGE_LOOP('',(#9863,#9864,#9865,#9866));
#3261=EDGE_LOOP('',(#9867,#9868,#9869,#9870));
#3262=EDGE_LOOP('',(#9871,#9872,#9873,#9874));
#3263=EDGE_LOOP('',(#9875,#9876,#9877,#9878,#9879,#9880));
#3264=EDGE_LOOP('',(#9881,#9882,#9883,#9884));
#3265=EDGE_LOOP('',(#9885,#9886,#9887,#9888));
#3266=EDGE_LOOP('',(#9889,#9890,#9891,#9892));
#3267=EDGE_LOOP('',(#9893,#9894,#9895,#9896));
#3268=EDGE_LOOP('',(#9897,#9898,#9899,#9900));
#3269=EDGE_LOOP('',(#9901,#9902,#9903,#9904));
#3270=EDGE_LOOP('',(#9905,#9906,#9907,#9908));
#3271=EDGE_LOOP('',(#9909,#9910,#9911,#9912));
#3272=EDGE_LOOP('',(#9913,#9914,#9915,#9916));
#3273=EDGE_LOOP('',(#9917,#9918,#9919,#9920));
#3274=EDGE_LOOP('',(#9921,#9922,#9923,#9924));
#3275=EDGE_LOOP('',(#9925,#9926,#9927,#9928));
#3276=EDGE_LOOP('',(#9929,#9930,#9931,#9932));
#3277=EDGE_LOOP('',(#9933,#9934,#9935,#9936));
#3278=EDGE_LOOP('',(#9937,#9938,#9939,#9940));
#3279=EDGE_LOOP('',(#9941,#9942,#9943,#9944));
#3280=EDGE_LOOP('',(#9945,#9946,#9947,#9948));
#3281=EDGE_LOOP('',(#9949,#9950,#9951,#9952));
#3282=EDGE_LOOP('',(#9953,#9954,#9955,#9956));
#3283=EDGE_LOOP('',(#9957,#9958,#9959,#9960));
#3284=EDGE_LOOP('',(#9961,#9962,#9963,#9964));
#3285=EDGE_LOOP('',(#9965,#9966,#9967,#9968));
#3286=EDGE_LOOP('',(#9969,#9970,#9971,#9972,#9973,#9974));
#3287=EDGE_LOOP('',(#9975,#9976,#9977,#9978,#9979,#9980));
#3288=EDGE_LOOP('',(#9981,#9982,#9983,#9984,#9985,#9986));
#3289=EDGE_LOOP('',(#9987,#9988,#9989,#9990,#9991,#9992,#9993,#9994,#9995,
#9996,#9997,#9998,#9999,#10000,#10001,#10002,#10003,#10004,#10005,#10006));
#3290=EDGE_LOOP('',(#10007));
#3291=EDGE_LOOP('',(#10008,#10009,#10010,#10011));
#3292=EDGE_LOOP('',(#10012,#10013,#10014,#10015));
#3293=EDGE_LOOP('',(#10016,#10017,#10018,#10019));
#3294=EDGE_LOOP('',(#10020,#10021,#10022,#10023));
#3295=EDGE_LOOP('',(#10024,#10025,#10026,#10027));
#3296=EDGE_LOOP('',(#10028,#10029,#10030,#10031));
#3297=EDGE_LOOP('',(#10032,#10033,#10034,#10035));
#3298=EDGE_LOOP('',(#10036,#10037,#10038,#10039));
#3299=EDGE_LOOP('',(#10040,#10041,#10042,#10043));
#3300=EDGE_LOOP('',(#10044,#10045,#10046,#10047));
#3301=EDGE_LOOP('',(#10048,#10049,#10050,#10051));
#3302=EDGE_LOOP('',(#10052,#10053,#10054,#10055));
#3303=EDGE_LOOP('',(#10056,#10057,#10058,#10059));
#3304=EDGE_LOOP('',(#10060,#10061,#10062,#10063,#10064,#10065));
#3305=EDGE_LOOP('',(#10066,#10067,#10068,#10069));
#3306=EDGE_LOOP('',(#10070,#10071,#10072,#10073));
#3307=EDGE_LOOP('',(#10074,#10075,#10076,#10077));
#3308=EDGE_LOOP('',(#10078,#10079,#10080,#10081));
#3309=EDGE_LOOP('',(#10082,#10083,#10084,#10085));
#3310=EDGE_LOOP('',(#10086,#10087,#10088,#10089));
#3311=EDGE_LOOP('',(#10090,#10091,#10092,#10093));
#3312=EDGE_LOOP('',(#10094,#10095,#10096,#10097));
#3313=EDGE_LOOP('',(#10098,#10099,#10100,#10101));
#3314=EDGE_LOOP('',(#10102,#10103,#10104,#10105));
#3315=EDGE_LOOP('',(#10106,#10107,#10108,#10109));
#3316=EDGE_LOOP('',(#10110,#10111,#10112,#10113));
#3317=EDGE_LOOP('',(#10114,#10115,#10116,#10117));
#3318=EDGE_LOOP('',(#10118,#10119,#10120,#10121));
#3319=EDGE_LOOP('',(#10122,#10123,#10124,#10125));
#3320=EDGE_LOOP('',(#10126,#10127,#10128,#10129));
#3321=EDGE_LOOP('',(#10130,#10131,#10132,#10133));
#3322=EDGE_LOOP('',(#10134,#10135,#10136,#10137));
#3323=EDGE_LOOP('',(#10138,#10139,#10140,#10141));
#3324=EDGE_LOOP('',(#10142,#10143,#10144,#10145,#10146,#10147));
#3325=EDGE_LOOP('',(#10148,#10149,#10150,#10151,#10152,#10153));
#3326=EDGE_LOOP('',(#10154,#10155,#10156,#10157,#10158,#10159));
#3327=EDGE_LOOP('',(#10160,#10161,#10162,#10163,#10164,#10165,#10166,#10167,
#10168,#10169,#10170,#10171,#10172,#10173,#10174,#10175,#10176,#10177,#10178,
#10179,#10180,#10181,#10182,#10183,#10184,#10185));
#3328=EDGE_LOOP('',(#10186));
#3329=EDGE_LOOP('',(#10187));
#3330=EDGE_LOOP('',(#10188));
#3331=EDGE_LOOP('',(#10189,#10190,#10191,#10192));
#3332=EDGE_LOOP('',(#10193,#10194,#10195,#10196));
#3333=EDGE_LOOP('',(#10197,#10198,#10199,#10200));
#3334=EDGE_LOOP('',(#10201,#10202,#10203,#10204));
#3335=EDGE_LOOP('',(#10205,#10206,#10207,#10208));
#3336=EDGE_LOOP('',(#10209,#10210,#10211,#10212));
#3337=EDGE_LOOP('',(#10213,#10214,#10215,#10216));
#3338=EDGE_LOOP('',(#10217,#10218,#10219,#10220));
#3339=EDGE_LOOP('',(#10221,#10222,#10223,#10224));
#3340=EDGE_LOOP('',(#10225,#10226,#10227,#10228));
#3341=EDGE_LOOP('',(#10229,#10230,#10231,#10232,#10233,#10234));
#3342=EDGE_LOOP('',(#10235,#10236,#10237,#10238));
#3343=EDGE_LOOP('',(#10239,#10240,#10241,#10242));
#3344=EDGE_LOOP('',(#10243,#10244,#10245,#10246));
#3345=EDGE_LOOP('',(#10247,#10248,#10249,#10250,#10251,#10252));
#3346=EDGE_LOOP('',(#10253,#10254,#10255,#10256,#10257,#10258,#10259,#10260,
#10261,#10262,#10263,#10264,#10265,#10266,#10267,#10268,#10269,#10270));
#3347=EDGE_LOOP('',(#10271,#10272,#10273,#10274));
#3348=EDGE_LOOP('',(#10275,#10276,#10277,#10278));
#3349=EDGE_LOOP('',(#10279,#10280,#10281,#10282));
#3350=EDGE_LOOP('',(#10283,#10284,#10285,#10286));
#3351=EDGE_LOOP('',(#10287,#10288,#10289,#10290));
#3352=EDGE_LOOP('',(#10291,#10292,#10293,#10294));
#3353=EDGE_LOOP('',(#10295,#10296,#10297,#10298));
#3354=EDGE_LOOP('',(#10299,#10300,#10301,#10302));
#3355=EDGE_LOOP('',(#10303,#10304,#10305,#10306));
#3356=EDGE_LOOP('',(#10307,#10308,#10309,#10310));
#3357=EDGE_LOOP('',(#10311,#10312,#10313,#10314));
#3358=EDGE_LOOP('',(#10315,#10316,#10317,#10318));
#3359=EDGE_LOOP('',(#10319,#10320,#10321,#10322));
#3360=EDGE_LOOP('',(#10323,#10324,#10325,#10326));
#3361=EDGE_LOOP('',(#10327,#10328,#10329,#10330,#10331,#10332));
#3362=EDGE_LOOP('',(#10333,#10334,#10335,#10336));
#3363=EDGE_LOOP('',(#10337,#10338,#10339,#10340,#10341,#10342));
#3364=EDGE_LOOP('',(#10343,#10344,#10345,#10346));
#3365=EDGE_LOOP('',(#10347,#10348,#10349,#10350,#10351,#10352,#10353,#10354,
#10355,#10356,#10357,#10358));
#3366=EDGE_LOOP('',(#10359));
#3367=EDGE_LOOP('',(#10360));
#3368=EDGE_LOOP('',(#10361));
#3369=EDGE_LOOP('',(#10362));
#3370=EDGE_LOOP('',(#10363));
#3371=EDGE_LOOP('',(#10364,#10365,#10366,#10367,#10368));
#3372=EDGE_LOOP('',(#10369,#10370,#10371,#10372));
#3373=EDGE_LOOP('',(#10373,#10374,#10375));
#3374=EDGE_LOOP('',(#10376,#10377,#10378,#10379,#10380,#10381,#10382,#10383,
#10384));
#3375=EDGE_LOOP('',(#10385,#10386,#10387,#10388,#10389,#10390));
#3376=EDGE_LOOP('',(#10391,#10392,#10393,#10394,#10395,#10396,#10397,#10398,
#10399,#10400,#10401,#10402,#10403,#10404,#10405,#10406));
#3377=EDGE_LOOP('',(#10407));
#3378=EDGE_LOOP('',(#10408,#10409,#10410,#10411));
#3379=EDGE_LOOP('',(#10412,#10413,#10414,#10415));
#3380=EDGE_LOOP('',(#10416,#10417,#10418,#10419));
#3381=EDGE_LOOP('',(#10420,#10421,#10422,#10423));
#3382=EDGE_LOOP('',(#10424,#10425,#10426,#10427));
#3383=EDGE_LOOP('',(#10428,#10429,#10430,#10431));
#3384=EDGE_LOOP('',(#10432,#10433,#10434));
#3385=EDGE_LOOP('',(#10435,#10436,#10437,#10438));
#3386=EDGE_LOOP('',(#10439,#10440));
#3387=EDGE_LOOP('',(#10441,#10442,#10443,#10444,#10445,#10446));
#3388=EDGE_LOOP('',(#10447,#10448,#10449,#10450,#10451,#10452,#10453,#10454,
#10455,#10456,#10457,#10458));
#3389=EDGE_LOOP('',(#10459,#10460,#10461));
#3390=EDGE_LOOP('',(#10462,#10463,#10464,#10465));
#3391=EDGE_LOOP('',(#10466,#10467,#10468,#10469,#10470,#10471));
#3392=EDGE_LOOP('',(#10472,#10473,#10474,#10475,#10476,#10477,#10478,#10479));
#3393=EDGE_LOOP('',(#10480,#10481,#10482));
#3394=EDGE_LOOP('',(#10483,#10484,#10485,#10486));
#3395=EDGE_LOOP('',(#10487,#10488,#10489,#10490,#10491,#10492));
#3396=EDGE_LOOP('',(#10493,#10494,#10495));
#3397=EDGE_LOOP('',(#10496,#10497,#10498,#10499));
#3398=EDGE_LOOP('',(#10500,#10501,#10502,#10503));
#3399=EDGE_LOOP('',(#10504,#10505,#10506));
#3400=EDGE_LOOP('',(#10507,#10508,#10509,#10510));
#3401=EDGE_LOOP('',(#10511,#10512,#10513,#10514));
#3402=EDGE_LOOP('',(#10515,#10516,#10517));
#3403=EDGE_LOOP('',(#10518,#10519,#10520,#10521));
#3404=EDGE_LOOP('',(#10522,#10523,#10524,#10525));
#3405=EDGE_LOOP('',(#10526,#10527,#10528));
#3406=EDGE_LOOP('',(#10529,#10530,#10531,#10532));
#3407=EDGE_LOOP('',(#10533,#10534,#10535,#10536));
#3408=EDGE_LOOP('',(#10537,#10538,#10539));
#3409=EDGE_LOOP('',(#10540,#10541,#10542,#10543));
#3410=EDGE_LOOP('',(#10544,#10545,#10546,#10547));
#3411=EDGE_LOOP('',(#10548,#10549,#10550));
#3412=EDGE_LOOP('',(#10551,#10552,#10553,#10554));
#3413=EDGE_LOOP('',(#10555,#10556,#10557,#10558));
#3414=EDGE_LOOP('',(#10559,#10560,#10561));
#3415=EDGE_LOOP('',(#10562,#10563,#10564,#10565));
#3416=EDGE_LOOP('',(#10566,#10567,#10568,#10569));
#3417=EDGE_LOOP('',(#10570,#10571,#10572));
#3418=EDGE_LOOP('',(#10573,#10574,#10575,#10576));
#3419=EDGE_LOOP('',(#10577,#10578,#10579,#10580));
#3420=EDGE_LOOP('',(#10581,#10582,#10583));
#3421=EDGE_LOOP('',(#10584,#10585,#10586,#10587));
#3422=EDGE_LOOP('',(#10588,#10589,#10590,#10591));
#3423=EDGE_LOOP('',(#10592,#10593,#10594));
#3424=EDGE_LOOP('',(#10595,#10596,#10597,#10598));
#3425=EDGE_LOOP('',(#10599,#10600,#10601,#10602));
#3426=EDGE_LOOP('',(#10603,#10604,#10605));
#3427=EDGE_LOOP('',(#10606,#10607,#10608,#10609));
#3428=EDGE_LOOP('',(#10610,#10611,#10612));
#3429=EDGE_LOOP('',(#10613,#10614,#10615,#10616,#10617,#10618));
#3430=EDGE_LOOP('',(#10619,#10620,#10621));
#3431=EDGE_LOOP('',(#10622,#10623,#10624,#10625,#10626,#10627,#10628,#10629));
#3432=EDGE_LOOP('',(#10630,#10631,#10632,#10633,#10634,#10635));
#3433=EDGE_LOOP('',(#10636,#10637,#10638,#10639));
#3434=EDGE_LOOP('',(#10640,#10641,#10642,#10643));
#3435=EDGE_LOOP('',(#10644,#10645,#10646,#10647));
#3436=EDGE_LOOP('',(#10648,#10649,#10650,#10651));
#3437=EDGE_LOOP('',(#10652,#10653,#10654,#10655));
#3438=EDGE_LOOP('',(#10656,#10657,#10658,#10659));
#3439=EDGE_LOOP('',(#10660,#10661,#10662,#10663));
#3440=EDGE_LOOP('',(#10664,#10665,#10666,#10667));
#3441=EDGE_LOOP('',(#10668,#10669,#10670,#10671));
#3442=EDGE_LOOP('',(#10672,#10673,#10674,#10675));
#3443=EDGE_LOOP('',(#10676));
#3444=EDGE_LOOP('',(#10677,#10678,#10679,#10680,#10681,#10682));
#3445=EDGE_LOOP('',(#10683,#10684,#10685,#10686));
#3446=EDGE_LOOP('',(#10687,#10688,#10689,#10690));
#3447=EDGE_LOOP('',(#10691));
#3448=EDGE_LOOP('',(#10692,#10693,#10694,#10695,#10696,#10697,#10698,#10699,
#10700,#10701,#10702,#10703,#10704,#10705,#10706,#10707,#10708,#10709,#10710,
#10711));
#3449=EDGE_LOOP('',(#10712,#10713,#10714,#10715,#10716,#10717));
#3450=EDGE_LOOP('',(#10718));
#3451=EDGE_LOOP('',(#10719));
#3452=EDGE_LOOP('',(#10720));
#3453=EDGE_LOOP('',(#10721));
#3454=EDGE_LOOP('',(#10722));
#3455=EDGE_LOOP('',(#10723,#10724,#10725,#10726));
#3456=EDGE_LOOP('',(#10727));
#3457=EDGE_LOOP('',(#10728,#10729,#10730,#10731,#10732,#10733));
#3458=EDGE_LOOP('',(#10734,#10735,#10736,#10737,#10738,#10739,#10740,#10741));
#3459=EDGE_LOOP('',(#10742,#10743,#10744,#10745,#10746,#10747));
#3460=EDGE_LOOP('',(#10748,#10749,#10750,#10751,#10752,#10753,#10754,#10755));
#3461=EDGE_LOOP('',(#10756,#10757,#10758,#10759));
#3462=EDGE_LOOP('',(#10760));
#3463=EDGE_LOOP('',(#10761,#10762,#10763,#10764,#10765,#10766));
#3464=EDGE_LOOP('',(#10767,#10768,#10769,#10770));
#3465=EDGE_LOOP('',(#10771,#10772,#10773,#10774));
#3466=EDGE_LOOP('',(#10775,#10776,#10777,#10778));
#3467=EDGE_LOOP('',(#10779,#10780,#10781,#10782,#10783,#10784,#10785,#10786,
#10787,#10788,#10789,#10790,#10791,#10792,#10793,#10794));
#3468=EDGE_LOOP('',(#10795,#10796,#10797,#10798));
#3469=EDGE_LOOP('',(#10799,#10800,#10801,#10802));
#3470=EDGE_LOOP('',(#10803,#10804,#10805,#10806));
#3471=EDGE_LOOP('',(#10807,#10808,#10809,#10810));
#3472=EDGE_LOOP('',(#10811));
#3473=EDGE_LOOP('',(#10812));
#3474=EDGE_LOOP('',(#10813,#10814,#10815,#10816));
#3475=EDGE_LOOP('',(#10817));
#3476=EDGE_LOOP('',(#10818));
#3477=EDGE_LOOP('',(#10819,#10820,#10821,#10822));
#3478=EDGE_LOOP('',(#10823,#10824,#10825,#10826));
#3479=EDGE_LOOP('',(#10827,#10828,#10829,#10830));
#3480=EDGE_LOOP('',(#10831,#10832,#10833,#10834));
#3481=EDGE_LOOP('',(#10835,#10836,#10837,#10838));
#3482=EDGE_LOOP('',(#10839,#10840,#10841,#10842));
#3483=EDGE_LOOP('',(#10843,#10844,#10845,#10846));
#3484=EDGE_LOOP('',(#10847,#10848,#10849,#10850));
#3485=EDGE_LOOP('',(#10851,#10852,#10853,#10854));
#3486=EDGE_LOOP('',(#10855,#10856,#10857,#10858));
#3487=EDGE_LOOP('',(#10859,#10860,#10861,#10862));
#3488=EDGE_LOOP('',(#10863,#10864,#10865,#10866));
#3489=EDGE_LOOP('',(#10867,#10868,#10869,#10870));
#3490=EDGE_LOOP('',(#10871,#10872,#10873,#10874));
#3491=EDGE_LOOP('',(#10875,#10876,#10877,#10878));
#3492=EDGE_LOOP('',(#10879,#10880,#10881,#10882));
#3493=EDGE_LOOP('',(#10883,#10884,#10885,#10886));
#3494=EDGE_LOOP('',(#10887,#10888,#10889,#10890));
#3495=EDGE_LOOP('',(#10891,#10892,#10893,#10894));
#3496=EDGE_LOOP('',(#10895,#10896,#10897,#10898));
#3497=EDGE_LOOP('',(#10899,#10900,#10901,#10902));
#3498=EDGE_LOOP('',(#10903,#10904,#10905,#10906));
#3499=EDGE_LOOP('',(#10907,#10908,#10909,#10910));
#3500=EDGE_LOOP('',(#10911,#10912,#10913,#10914));
#3501=EDGE_LOOP('',(#10915,#10916,#10917,#10918));
#3502=EDGE_LOOP('',(#10919,#10920,#10921,#10922));
#3503=EDGE_LOOP('',(#10923,#10924,#10925,#10926));
#3504=EDGE_LOOP('',(#10927,#10928,#10929,#10930));
#3505=EDGE_LOOP('',(#10931,#10932,#10933,#10934));
#3506=EDGE_LOOP('',(#10935,#10936,#10937,#10938));
#3507=EDGE_LOOP('',(#10939,#10940,#10941,#10942));
#3508=EDGE_LOOP('',(#10943));
#3509=EDGE_LOOP('',(#10944));
#3510=EDGE_LOOP('',(#10945,#10946,#10947,#10948));
#3511=EDGE_LOOP('',(#10949));
#3512=EDGE_LOOP('',(#10950));
#3513=EDGE_LOOP('',(#10951,#10952,#10953,#10954));
#3514=EDGE_LOOP('',(#10955));
#3515=EDGE_LOOP('',(#10956));
#3516=EDGE_LOOP('',(#10957,#10958,#10959,#10960,#10961,#10962,#10963,#10964,
#10965));
#3517=EDGE_LOOP('',(#10966,#10967));
#3518=EDGE_LOOP('',(#10968));
#3519=EDGE_LOOP('',(#10969));
#3520=EDGE_LOOP('',(#10970,#10971,#10972,#10973));
#3521=EDGE_LOOP('',(#10974));
#3522=EDGE_LOOP('',(#10975));
#3523=EDGE_LOOP('',(#10976,#10977,#10978,#10979));
#3524=EDGE_LOOP('',(#10980));
#3525=EDGE_LOOP('',(#10981));
#3526=EDGE_LOOP('',(#10982,#10983,#10984,#10985));
#3527=EDGE_LOOP('',(#10986,#10987,#10988,#10989));
#3528=EDGE_LOOP('',(#10990,#10991,#10992));
#3529=EDGE_LOOP('',(#10993));
#3530=EDGE_LOOP('',(#10994));
#3531=EDGE_LOOP('',(#10995,#10996,#10997,#10998));
#3532=EDGE_LOOP('',(#10999));
#3533=EDGE_LOOP('',(#11000));
#3534=EDGE_LOOP('',(#11001,#11002,#11003,#11004));
#3535=EDGE_LOOP('',(#11005,#11006,#11007,#11008));
#3536=EDGE_LOOP('',(#11009,#11010,#11011,#11012));
#3537=EDGE_LOOP('',(#11013,#11014,#11015,#11016));
#3538=EDGE_LOOP('',(#11017,#11018,#11019,#11020));
#3539=EDGE_LOOP('',(#11021,#11022,#11023,#11024));
#3540=EDGE_LOOP('',(#11025,#11026,#11027,#11028));
#3541=EDGE_LOOP('',(#11029));
#3542=EDGE_LOOP('',(#11030));
#3543=EDGE_LOOP('',(#11031,#11032,#11033,#11034));
#3544=EDGE_LOOP('',(#11035,#11036,#11037,#11038));
#3545=EDGE_LOOP('',(#11039,#11040,#11041,#11042));
#3546=EDGE_LOOP('',(#11043,#11044,#11045,#11046));
#3547=EDGE_LOOP('',(#11047,#11048,#11049,#11050));
#3548=EDGE_LOOP('',(#11051,#11052,#11053,#11054));
#3549=EDGE_LOOP('',(#11055,#11056,#11057,#11058));
#3550=EDGE_LOOP('',(#11059,#11060,#11061,#11062));
#3551=EDGE_LOOP('',(#11063,#11064,#11065,#11066));
#3552=EDGE_LOOP('',(#11067,#11068,#11069,#11070));
#3553=EDGE_LOOP('',(#11071,#11072,#11073,#11074));
#3554=EDGE_LOOP('',(#11075,#11076,#11077,#11078));
#3555=EDGE_LOOP('',(#11079,#11080,#11081,#11082,#11083,#11084,#11085,#11086));
#3556=EDGE_LOOP('',(#11087));
#3557=EDGE_LOOP('',(#11088));
#3558=EDGE_LOOP('',(#11089));
#3559=EDGE_LOOP('',(#11090));
#3560=EDGE_LOOP('',(#11091));
#3561=EDGE_LOOP('',(#11092,#11093,#11094,#11095));
#3562=EDGE_LOOP('',(#11096,#11097,#11098,#11099));
#3563=EDGE_LOOP('',(#11100,#11101,#11102,#11103));
#3564=EDGE_LOOP('',(#11104));
#3565=EDGE_LOOP('',(#11105));
#3566=EDGE_LOOP('',(#11106,#11107,#11108,#11109));
#3567=EDGE_LOOP('',(#11110,#11111,#11112,#11113));
#3568=EDGE_LOOP('',(#11114,#11115,#11116,#11117));
#3569=EDGE_LOOP('',(#11118,#11119,#11120,#11121));
#3570=EDGE_LOOP('',(#11122));
#3571=EDGE_LOOP('',(#11123));
#3572=EDGE_LOOP('',(#11124,#11125,#11126,#11127));
#3573=EDGE_LOOP('',(#11128,#11129,#11130,#11131));
#3574=EDGE_LOOP('',(#11132,#11133,#11134,#11135));
#3575=EDGE_LOOP('',(#11136,#11137,#11138,#11139));
#3576=EDGE_LOOP('',(#11140));
#3577=EDGE_LOOP('',(#11141));
#3578=EDGE_LOOP('',(#11142,#11143,#11144,#11145));
#3579=EDGE_LOOP('',(#11146,#11147,#11148,#11149));
#3580=EDGE_LOOP('',(#11150,#11151,#11152,#11153));
#3581=EDGE_LOOP('',(#11154,#11155,#11156,#11157));
#3582=EDGE_LOOP('',(#11158));
#3583=EDGE_LOOP('',(#11159));
#3584=EDGE_LOOP('',(#11160,#11161,#11162,#11163));
#3585=EDGE_LOOP('',(#11164,#11165,#11166,#11167));
#3586=EDGE_LOOP('',(#11168,#11169,#11170,#11171));
#3587=EDGE_LOOP('',(#11172));
#3588=EDGE_LOOP('',(#11173));
#3589=EDGE_LOOP('',(#11174,#11175,#11176,#11177));
#3590=EDGE_LOOP('',(#11178,#11179,#11180,#11181));
#3591=EDGE_LOOP('',(#11182,#11183,#11184,#11185));
#3592=EDGE_LOOP('',(#11186,#11187,#11188,#11189));
#3593=EDGE_LOOP('',(#11190,#11191,#11192,#11193));
#3594=EDGE_LOOP('',(#11194,#11195,#11196,#11197,#11198,#11199,#11200,#11201));
#3595=EDGE_LOOP('',(#11202));
#3596=EDGE_LOOP('',(#11203));
#3597=EDGE_LOOP('',(#11204));
#3598=EDGE_LOOP('',(#11205));
#3599=EDGE_LOOP('',(#11206));
#3600=EDGE_LOOP('',(#11207,#11208,#11209,#11210));
#3601=EDGE_LOOP('',(#11211,#11212,#11213,#11214));
#3602=EDGE_LOOP('',(#11215,#11216,#11217,#11218));
#3603=EDGE_LOOP('',(#11219,#11220,#11221,#11222));
#3604=EDGE_LOOP('',(#11223,#11224,#11225,#11226));
#3605=EDGE_LOOP('',(#11227,#11228,#11229,#11230));
#3606=EDGE_LOOP('',(#11231,#11232,#11233,#11234));
#3607=EDGE_LOOP('',(#11235,#11236,#11237,#11238));
#3608=EDGE_LOOP('',(#11239,#11240,#11241,#11242));
#3609=EDGE_LOOP('',(#11243,#11244,#11245,#11246));
#3610=EDGE_LOOP('',(#11247,#11248,#11249,#11250));
#3611=EDGE_LOOP('',(#11251,#11252,#11253,#11254));
#3612=EDGE_LOOP('',(#11255,#11256,#11257,#11258,#11259,#11260,#11261,#11262));
#3613=EDGE_LOOP('',(#11263));
#3614=EDGE_LOOP('',(#11264,#11265,#11266,#11267));
#3615=EDGE_LOOP('',(#11268,#11269,#11270,#11271));
#3616=EDGE_LOOP('',(#11272,#11273,#11274,#11275));
#3617=EDGE_LOOP('',(#11276,#11277,#11278,#11279));
#3618=EDGE_LOOP('',(#11280));
#3619=EDGE_LOOP('',(#11281));
#3620=EDGE_LOOP('',(#11282));
#3621=EDGE_LOOP('',(#11283));
#3622=EDGE_LOOP('',(#11284,#11285,#11286,#11287));
#3623=EDGE_LOOP('',(#11288,#11289,#11290,#11291));
#3624=EDGE_LOOP('',(#11292,#11293,#11294,#11295));
#3625=EDGE_LOOP('',(#11296));
#3626=EDGE_LOOP('',(#11297));
#3627=EDGE_LOOP('',(#11298,#11299,#11300,#11301));
#3628=EDGE_LOOP('',(#11302,#11303,#11304,#11305));
#3629=EDGE_LOOP('',(#11306,#11307,#11308,#11309));
#3630=EDGE_LOOP('',(#11310,#11311,#11312,#11313));
#3631=EDGE_LOOP('',(#11314));
#3632=EDGE_LOOP('',(#11315));
#3633=EDGE_LOOP('',(#11316,#11317,#11318,#11319));
#3634=EDGE_LOOP('',(#11320,#11321,#11322,#11323));
#3635=EDGE_LOOP('',(#11324,#11325,#11326,#11327));
#3636=EDGE_LOOP('',(#11328,#11329,#11330,#11331));
#3637=EDGE_LOOP('',(#11332));
#3638=EDGE_LOOP('',(#11333));
#3639=EDGE_LOOP('',(#11334,#11335,#11336,#11337));
#3640=EDGE_LOOP('',(#11338,#11339,#11340,#11341));
#3641=EDGE_LOOP('',(#11342,#11343,#11344,#11345));
#3642=EDGE_LOOP('',(#11346,#11347,#11348,#11349));
#3643=EDGE_LOOP('',(#11350));
#3644=EDGE_LOOP('',(#11351));
#3645=EDGE_LOOP('',(#11352,#11353,#11354,#11355));
#3646=EDGE_LOOP('',(#11356,#11357,#11358,#11359));
#3647=EDGE_LOOP('',(#11360,#11361,#11362,#11363));
#3648=EDGE_LOOP('',(#11364,#11365,#11366,#11367));
#3649=EDGE_LOOP('',(#11368,#11369,#11370,#11371));
#3650=EDGE_LOOP('',(#11372,#11373,#11374,#11375));
#3651=EDGE_LOOP('',(#11376,#11377,#11378,#11379));
#3652=EDGE_LOOP('',(#11380,#11381,#11382,#11383));
#3653=EDGE_LOOP('',(#11384,#11385,#11386,#11387));
#3654=EDGE_LOOP('',(#11388,#11389,#11390,#11391));
#3655=EDGE_LOOP('',(#11392,#11393,#11394,#11395));
#3656=EDGE_LOOP('',(#11396,#11397,#11398,#11399));
#3657=EDGE_LOOP('',(#11400,#11401,#11402,#11403));
#3658=EDGE_LOOP('',(#11404,#11405,#11406,#11407));
#3659=EDGE_LOOP('',(#11408,#11409,#11410,#11411));
#3660=EDGE_LOOP('',(#11412,#11413,#11414,#11415));
#3661=EDGE_LOOP('',(#11416,#11417,#11418,#11419));
#3662=EDGE_LOOP('',(#11420,#11421,#11422,#11423));
#3663=EDGE_LOOP('',(#11424,#11425,#11426,#11427));
#3664=EDGE_LOOP('',(#11428,#11429,#11430,#11431));
#3665=EDGE_LOOP('',(#11432,#11433,#11434,#11435));
#3666=EDGE_LOOP('',(#11436,#11437,#11438,#11439));
#3667=EDGE_LOOP('',(#11440,#11441,#11442,#11443));
#3668=EDGE_LOOP('',(#11444,#11445,#11446,#11447));
#3669=EDGE_LOOP('',(#11448,#11449,#11450,#11451));
#3670=EDGE_LOOP('',(#11452,#11453,#11454,#11455));
#3671=EDGE_LOOP('',(#11456,#11457,#11458,#11459));
#3672=EDGE_LOOP('',(#11460,#11461,#11462,#11463));
#3673=EDGE_LOOP('',(#11464,#11465,#11466,#11467));
#3674=EDGE_LOOP('',(#11468,#11469,#11470,#11471));
#3675=EDGE_LOOP('',(#11472,#11473,#11474,#11475));
#3676=EDGE_LOOP('',(#11476));
#3677=EDGE_LOOP('',(#11477));
#3678=EDGE_LOOP('',(#11478));
#3679=EDGE_LOOP('',(#11479));
#3680=EDGE_LOOP('',(#11480));
#3681=EDGE_LOOP('',(#11481));
#3682=EDGE_LOOP('',(#11482,#11483,#11484,#11485));
#3683=EDGE_LOOP('',(#11486,#11487,#11488,#11489));
#3684=EDGE_LOOP('',(#11490,#11491,#11492,#11493));
#3685=EDGE_LOOP('',(#11494,#11495,#11496,#11497));
#3686=EDGE_LOOP('',(#11498,#11499,#11500,#11501,#11502,#11503,#11504,#11505));
#3687=EDGE_LOOP('',(#11506));
#3688=EDGE_LOOP('',(#11507));
#3689=EDGE_LOOP('',(#11508));
#3690=EDGE_LOOP('',(#11509));
#3691=EDGE_LOOP('',(#11510));
#3692=EDGE_LOOP('',(#11511));
#3693=EDGE_LOOP('',(#11512,#11513,#11514,#11515));
#3694=EDGE_LOOP('',(#11516,#11517,#11518,#11519));
#3695=EDGE_LOOP('',(#11520,#11521,#11522,#11523));
#3696=EDGE_LOOP('',(#11524,#11525,#11526,#11527));
#3697=EDGE_LOOP('',(#11528));
#3698=EDGE_LOOP('',(#11529));
#3699=EDGE_LOOP('',(#11530));
#3700=EDGE_LOOP('',(#11531,#11532,#11533,#11534,#11535));
#3701=EDGE_LOOP('',(#11536,#11537,#11538,#11539));
#3702=EDGE_LOOP('',(#11540,#11541,#11542,#11543));
#3703=EDGE_LOOP('',(#11544,#11545,#11546,#11547));
#3704=EDGE_LOOP('',(#11548,#11549,#11550,#11551));
#3705=EDGE_LOOP('',(#11552,#11553,#11554,#11555));
#3706=EDGE_LOOP('',(#11556,#11557,#11558,#11559,#11560));
#3707=EDGE_LOOP('',(#11561,#11562,#11563,#11564,#11565));
#3708=EDGE_LOOP('',(#11566,#11567,#11568,#11569));
#3709=EDGE_LOOP('',(#11570,#11571,#11572,#11573,#11574));
#3710=EDGE_LOOP('',(#11575,#11576,#11577,#11578));
#3711=EDGE_LOOP('',(#11579,#11580,#11581,#11582,#11583,#11584,#11585,#11586));
#3712=EDGE_LOOP('',(#11587,#11588,#11589,#11590,#11591));
#3713=EDGE_LOOP('',(#11592,#11593,#11594));
#3714=EDGE_LOOP('',(#11595,#11596,#11597,#11598));
#3715=EDGE_LOOP('',(#11599,#11600,#11601,#11602,#11603,#11604,#11605,#11606,
#11607));
#3716=EDGE_LOOP('',(#11608,#11609,#11610,#11611,#11612,#11613,#11614,#11615));
#3717=EDGE_LOOP('',(#11616,#11617,#11618,#11619));
#3718=EDGE_LOOP('',(#11620,#11621,#11622,#11623));
#3719=EDGE_LOOP('',(#11624,#11625,#11626,#11627,#11628,#11629,#11630,#11631,
#11632,#11633,#11634,#11635));
#3720=EDGE_LOOP('',(#11636,#11637,#11638));
#3721=EDGE_LOOP('',(#11639,#11640,#11641,#11642,#11643,#11644,#11645,#11646,
#11647,#11648,#11649));
#3722=EDGE_LOOP('',(#11650,#11651,#11652));
#3723=EDGE_LOOP('',(#11653));
#3724=EDGE_LOOP('',(#11654,#11655,#11656,#11657));
#3725=EDGE_LOOP('',(#11658,#11659,#11660,#11661));
#3726=EDGE_LOOP('',(#11662));
#3727=EDGE_LOOP('',(#11663));
#3728=EDGE_LOOP('',(#11664,#11665,#11666,#11667));
#3729=EDGE_LOOP('',(#11668,#11669,#11670,#11671));
#3730=EDGE_LOOP('',(#11672));
#3731=EDGE_LOOP('',(#11673));
#3732=EDGE_LOOP('',(#11674));
#3733=EDGE_LOOP('',(#11675));
#3734=EDGE_LOOP('',(#11676,#11677,#11678,#11679));
#3735=EDGE_LOOP('',(#11680,#11681,#11682,#11683));
#3736=EDGE_LOOP('',(#11684));
#3737=EDGE_LOOP('',(#11685));
#3738=EDGE_LOOP('',(#11686,#11687,#11688,#11689));
#3739=EDGE_LOOP('',(#11690,#11691,#11692,#11693));
#3740=EDGE_LOOP('',(#11694));
#3741=EDGE_LOOP('',(#11695,#11696,#11697,#11698));
#3742=EDGE_LOOP('',(#11699,#11700,#11701,#11702,#11703));
#3743=EDGE_LOOP('',(#11704,#11705,#11706,#11707,#11708,#11709));
#3744=EDGE_LOOP('',(#11710,#11711,#11712,#11713,#11714,#11715,#11716,#11717,
#11718,#11719,#11720,#11721,#11722,#11723,#11724,#11725,#11726,#11727,#11728,
#11729,#11730,#11731,#11732,#11733,#11734,#11735,#11736,#11737,#11738,#11739,
#11740,#11741,#11742,#11743,#11744,#11745,#11746,#11747,#11748,#11749,#11750,
#11751,#11752,#11753,#11754,#11755,#11756,#11757,#11758,#11759,#11760,#11761,
#11762,#11763,#11764,#11765,#11766,#11767,#11768,#11769,#11770,#11771,#11772,
#11773,#11774,#11775,#11776,#11777,#11778,#11779,#11780,#11781,#11782,#11783,
#11784,#11785,#11786,#11787,#11788,#11789,#11790,#11791,#11792,#11793,#11794,
#11795,#11796,#11797,#11798,#11799,#11800,#11801,#11802,#11803,#11804,#11805,
#11806,#11807,#11808,#11809,#11810,#11811,#11812,#11813,#11814,#11815,#11816,
#11817,#11818,#11819,#11820,#11821,#11822,#11823,#11824,#11825,#11826,#11827,
#11828,#11829));
#3745=EDGE_LOOP('',(#11830));
#3746=EDGE_LOOP('',(#11831,#11832,#11833,#11834,#11835));
#3747=EDGE_LOOP('',(#11836,#11837,#11838,#11839,#11840,#11841,#11842,#11843,
#11844,#11845,#11846,#11847,#11848,#11849,#11850,#11851,#11852,#11853,#11854,
#11855,#11856,#11857,#11858,#11859,#11860,#11861,#11862,#11863,#11864,#11865,
#11866,#11867,#11868,#11869,#11870,#11871,#11872,#11873,#11874,#11875,#11876,
#11877,#11878,#11879,#11880,#11881,#11882,#11883,#11884,#11885,#11886,#11887,
#11888,#11889,#11890,#11891,#11892,#11893,#11894,#11895,#11896,#11897,#11898,
#11899,#11900,#11901,#11902,#11903,#11904,#11905,#11906,#11907,#11908,#11909,
#11910,#11911,#11912,#11913,#11914,#11915,#11916,#11917,#11918,#11919,#11920,
#11921,#11922,#11923,#11924,#11925,#11926,#11927,#11928,#11929,#11930,#11931,
#11932,#11933,#11934,#11935,#11936,#11937,#11938,#11939,#11940,#11941,#11942,
#11943,#11944,#11945,#11946,#11947,#11948,#11949,#11950,#11951,#11952,#11953,
#11954,#11955));
#3748=EDGE_LOOP('',(#11956));
#3749=EDGE_LOOP('',(#11957,#11958,#11959,#11960,#11961,#11962,#11963,#11964));
#3750=EDGE_LOOP('',(#11965,#11966,#11967,#11968));
#3751=EDGE_LOOP('',(#11969,#11970,#11971,#11972,#11973,#11974,#11975,#11976));
#3752=EDGE_LOOP('',(#11977,#11978,#11979,#11980));
#3753=EDGE_LOOP('',(#11981,#11982,#11983,#11984));
#3754=EDGE_LOOP('',(#11985,#11986,#11987,#11988));
#3755=EDGE_LOOP('',(#11989,#11990,#11991,#11992));
#3756=EDGE_LOOP('',(#11993,#11994,#11995,#11996));
#3757=EDGE_LOOP('',(#11997,#11998,#11999,#12000,#12001,#12002,#12003,#12004));
#3758=EDGE_LOOP('',(#12005,#12006,#12007,#12008));
#3759=EDGE_LOOP('',(#12009,#12010,#12011,#12012,#12013,#12014,#12015,#12016));
#3760=EDGE_LOOP('',(#12017,#12018,#12019,#12020));
#3761=EDGE_LOOP('',(#12021,#12022,#12023,#12024));
#3762=EDGE_LOOP('',(#12025,#12026,#12027,#12028));
#3763=EDGE_LOOP('',(#12029,#12030,#12031,#12032));
#3764=EDGE_LOOP('',(#12033,#12034,#12035,#12036));
#3765=EDGE_LOOP('',(#12037,#12038,#12039,#12040,#12041,#12042,#12043,#12044));
#3766=EDGE_LOOP('',(#12045,#12046,#12047,#12048));
#3767=EDGE_LOOP('',(#12049,#12050,#12051,#12052,#12053,#12054,#12055,#12056));
#3768=EDGE_LOOP('',(#12057,#12058,#12059,#12060));
#3769=EDGE_LOOP('',(#12061,#12062,#12063,#12064));
#3770=EDGE_LOOP('',(#12065,#12066,#12067,#12068));
#3771=EDGE_LOOP('',(#12069,#12070,#12071,#12072));
#3772=EDGE_LOOP('',(#12073,#12074,#12075,#12076));
#3773=EDGE_LOOP('',(#12077,#12078,#12079,#12080,#12081,#12082,#12083,#12084));
#3774=EDGE_LOOP('',(#12085,#12086,#12087,#12088));
#3775=EDGE_LOOP('',(#12089,#12090,#12091,#12092,#12093,#12094,#12095,#12096));
#3776=EDGE_LOOP('',(#12097,#12098,#12099,#12100));
#3777=EDGE_LOOP('',(#12101,#12102,#12103,#12104));
#3778=EDGE_LOOP('',(#12105,#12106,#12107,#12108));
#3779=EDGE_LOOP('',(#12109,#12110,#12111,#12112));
#3780=EDGE_LOOP('',(#12113,#12114,#12115,#12116));
#3781=EDGE_LOOP('',(#12117,#12118,#12119,#12120,#12121,#12122,#12123,#12124));
#3782=EDGE_LOOP('',(#12125,#12126,#12127,#12128));
#3783=EDGE_LOOP('',(#12129,#12130,#12131,#12132,#12133,#12134,#12135,#12136));
#3784=EDGE_LOOP('',(#12137,#12138,#12139,#12140));
#3785=EDGE_LOOP('',(#12141,#12142,#12143,#12144));
#3786=EDGE_LOOP('',(#12145,#12146,#12147,#12148));
#3787=EDGE_LOOP('',(#12149,#12150,#12151,#12152));
#3788=EDGE_LOOP('',(#12153,#12154,#12155,#12156));
#3789=EDGE_LOOP('',(#12157,#12158,#12159,#12160,#12161,#12162,#12163,#12164));
#3790=EDGE_LOOP('',(#12165,#12166,#12167,#12168));
#3791=EDGE_LOOP('',(#12169,#12170,#12171,#12172,#12173,#12174,#12175,#12176));
#3792=EDGE_LOOP('',(#12177,#12178,#12179,#12180));
#3793=EDGE_LOOP('',(#12181,#12182,#12183,#12184));
#3794=EDGE_LOOP('',(#12185,#12186,#12187,#12188));
#3795=EDGE_LOOP('',(#12189,#12190,#12191,#12192));
#3796=EDGE_LOOP('',(#12193,#12194,#12195,#12196));
#3797=EDGE_LOOP('',(#12197,#12198,#12199,#12200,#12201,#12202,#12203,#12204));
#3798=EDGE_LOOP('',(#12205,#12206,#12207,#12208));
#3799=EDGE_LOOP('',(#12209,#12210,#12211,#12212,#12213,#12214,#12215,#12216));
#3800=EDGE_LOOP('',(#12217,#12218,#12219,#12220));
#3801=EDGE_LOOP('',(#12221,#12222,#12223,#12224));
#3802=EDGE_LOOP('',(#12225,#12226,#12227,#12228));
#3803=EDGE_LOOP('',(#12229,#12230,#12231,#12232));
#3804=EDGE_LOOP('',(#12233,#12234,#12235,#12236));
#3805=EDGE_LOOP('',(#12237,#12238,#12239,#12240,#12241,#12242,#12243,#12244));
#3806=EDGE_LOOP('',(#12245,#12246,#12247,#12248));
#3807=EDGE_LOOP('',(#12249,#12250,#12251,#12252,#12253,#12254,#12255,#12256));
#3808=EDGE_LOOP('',(#12257,#12258,#12259,#12260));
#3809=EDGE_LOOP('',(#12261,#12262,#12263,#12264));
#3810=EDGE_LOOP('',(#12265,#12266,#12267,#12268));
#3811=EDGE_LOOP('',(#12269,#12270,#12271,#12272));
#3812=EDGE_LOOP('',(#12273,#12274,#12275,#12276));
#3813=EDGE_LOOP('',(#12277,#12278,#12279,#12280,#12281,#12282,#12283,#12284));
#3814=EDGE_LOOP('',(#12285,#12286,#12287,#12288));
#3815=EDGE_LOOP('',(#12289,#12290,#12291,#12292,#12293,#12294,#12295,#12296));
#3816=EDGE_LOOP('',(#12297,#12298,#12299,#12300));
#3817=EDGE_LOOP('',(#12301,#12302,#12303,#12304));
#3818=EDGE_LOOP('',(#12305,#12306,#12307,#12308));
#3819=EDGE_LOOP('',(#12309,#12310,#12311,#12312));
#3820=EDGE_LOOP('',(#12313,#12314,#12315,#12316));
#3821=EDGE_LOOP('',(#12317,#12318,#12319,#12320,#12321,#12322,#12323,#12324));
#3822=EDGE_LOOP('',(#12325,#12326,#12327,#12328));
#3823=EDGE_LOOP('',(#12329,#12330,#12331,#12332,#12333,#12334,#12335,#12336));
#3824=EDGE_LOOP('',(#12337,#12338,#12339,#12340));
#3825=EDGE_LOOP('',(#12341,#12342,#12343,#12344));
#3826=EDGE_LOOP('',(#12345,#12346,#12347,#12348));
#3827=EDGE_LOOP('',(#12349,#12350,#12351,#12352));
#3828=EDGE_LOOP('',(#12353,#12354,#12355,#12356));
#3829=EDGE_LOOP('',(#12357,#12358,#12359,#12360,#12361,#12362,#12363,#12364));
#3830=EDGE_LOOP('',(#12365,#12366,#12367,#12368));
#3831=EDGE_LOOP('',(#12369,#12370,#12371,#12372,#12373,#12374,#12375,#12376));
#3832=EDGE_LOOP('',(#12377,#12378,#12379,#12380));
#3833=EDGE_LOOP('',(#12381,#12382,#12383,#12384));
#3834=EDGE_LOOP('',(#12385,#12386,#12387,#12388));
#3835=EDGE_LOOP('',(#12389,#12390,#12391,#12392));
#3836=EDGE_LOOP('',(#12393,#12394,#12395,#12396));
#3837=EDGE_LOOP('',(#12397,#12398,#12399,#12400,#12401,#12402,#12403,#12404));
#3838=EDGE_LOOP('',(#12405,#12406,#12407,#12408));
#3839=EDGE_LOOP('',(#12409,#12410,#12411,#12412,#12413,#12414,#12415,#12416));
#3840=EDGE_LOOP('',(#12417,#12418,#12419,#12420));
#3841=EDGE_LOOP('',(#12421,#12422,#12423,#12424));
#3842=EDGE_LOOP('',(#12425,#12426,#12427,#12428));
#3843=EDGE_LOOP('',(#12429,#12430,#12431,#12432));
#3844=EDGE_LOOP('',(#12433,#12434,#12435,#12436));
#3845=EDGE_LOOP('',(#12437,#12438,#12439,#12440,#12441,#12442,#12443,#12444));
#3846=EDGE_LOOP('',(#12445,#12446,#12447,#12448));
#3847=EDGE_LOOP('',(#12449,#12450,#12451,#12452,#12453,#12454,#12455,#12456));
#3848=EDGE_LOOP('',(#12457,#12458,#12459,#12460));
#3849=EDGE_LOOP('',(#12461,#12462,#12463,#12464));
#3850=EDGE_LOOP('',(#12465,#12466,#12467,#12468));
#3851=EDGE_LOOP('',(#12469,#12470,#12471,#12472));
#3852=EDGE_LOOP('',(#12473,#12474,#12475,#12476));
#3853=EDGE_LOOP('',(#12477,#12478,#12479,#12480,#12481,#12482,#12483,#12484));
#3854=EDGE_LOOP('',(#12485,#12486,#12487,#12488));
#3855=EDGE_LOOP('',(#12489,#12490,#12491,#12492,#12493,#12494,#12495,#12496));
#3856=EDGE_LOOP('',(#12497,#12498,#12499,#12500));
#3857=EDGE_LOOP('',(#12501,#12502,#12503,#12504));
#3858=EDGE_LOOP('',(#12505,#12506,#12507,#12508));
#3859=EDGE_LOOP('',(#12509,#12510,#12511,#12512));
#3860=EDGE_LOOP('',(#12513,#12514,#12515,#12516));
#3861=EDGE_LOOP('',(#12517,#12518,#12519,#12520,#12521,#12522,#12523,#12524));
#3862=EDGE_LOOP('',(#12525,#12526,#12527,#12528));
#3863=EDGE_LOOP('',(#12529,#12530,#12531,#12532,#12533,#12534,#12535,#12536));
#3864=EDGE_LOOP('',(#12537,#12538,#12539,#12540));
#3865=EDGE_LOOP('',(#12541,#12542,#12543,#12544));
#3866=EDGE_LOOP('',(#12545,#12546,#12547,#12548));
#3867=EDGE_LOOP('',(#12549,#12550,#12551,#12552));
#3868=EDGE_LOOP('',(#12553,#12554,#12555,#12556));
#3869=EDGE_LOOP('',(#12557,#12558,#12559,#12560,#12561,#12562,#12563,#12564));
#3870=EDGE_LOOP('',(#12565,#12566,#12567,#12568));
#3871=EDGE_LOOP('',(#12569,#12570,#12571,#12572,#12573,#12574,#12575,#12576));
#3872=EDGE_LOOP('',(#12577,#12578,#12579,#12580));
#3873=EDGE_LOOP('',(#12581,#12582,#12583,#12584));
#3874=EDGE_LOOP('',(#12585,#12586,#12587,#12588));
#3875=EDGE_LOOP('',(#12589,#12590,#12591,#12592));
#3876=EDGE_LOOP('',(#12593,#12594,#12595,#12596));
#3877=EDGE_LOOP('',(#12597,#12598,#12599,#12600,#12601,#12602,#12603,#12604));
#3878=EDGE_LOOP('',(#12605,#12606,#12607,#12608));
#3879=EDGE_LOOP('',(#12609,#12610,#12611,#12612,#12613,#12614,#12615,#12616));
#3880=EDGE_LOOP('',(#12617,#12618,#12619,#12620));
#3881=EDGE_LOOP('',(#12621,#12622,#12623,#12624));
#3882=EDGE_LOOP('',(#12625,#12626,#12627,#12628));
#3883=EDGE_LOOP('',(#12629,#12630,#12631,#12632));
#3884=EDGE_LOOP('',(#12633,#12634,#12635,#12636));
#3885=EDGE_LOOP('',(#12637,#12638,#12639,#12640,#12641,#12642,#12643,#12644));
#3886=EDGE_LOOP('',(#12645,#12646,#12647,#12648));
#3887=EDGE_LOOP('',(#12649,#12650,#12651,#12652,#12653,#12654,#12655,#12656));
#3888=EDGE_LOOP('',(#12657,#12658,#12659,#12660));
#3889=EDGE_LOOP('',(#12661,#12662,#12663,#12664));
#3890=EDGE_LOOP('',(#12665,#12666,#12667,#12668));
#3891=EDGE_LOOP('',(#12669,#12670,#12671,#12672));
#3892=EDGE_LOOP('',(#12673,#12674,#12675,#12676));
#3893=EDGE_LOOP('',(#12677,#12678,#12679,#12680,#12681,#12682,#12683,#12684));
#3894=EDGE_LOOP('',(#12685,#12686,#12687,#12688));
#3895=EDGE_LOOP('',(#12689,#12690,#12691,#12692,#12693,#12694,#12695,#12696));
#3896=EDGE_LOOP('',(#12697,#12698,#12699,#12700));
#3897=EDGE_LOOP('',(#12701,#12702,#12703,#12704));
#3898=EDGE_LOOP('',(#12705,#12706,#12707,#12708));
#3899=EDGE_LOOP('',(#12709,#12710,#12711,#12712));
#3900=EDGE_LOOP('',(#12713,#12714,#12715,#12716));
#3901=EDGE_LOOP('',(#12717,#12718,#12719,#12720,#12721,#12722,#12723,#12724));
#3902=EDGE_LOOP('',(#12725,#12726,#12727,#12728));
#3903=EDGE_LOOP('',(#12729,#12730,#12731,#12732,#12733,#12734,#12735,#12736));
#3904=EDGE_LOOP('',(#12737,#12738,#12739,#12740));
#3905=EDGE_LOOP('',(#12741,#12742,#12743,#12744));
#3906=EDGE_LOOP('',(#12745,#12746,#12747,#12748));
#3907=EDGE_LOOP('',(#12749,#12750,#12751,#12752));
#3908=EDGE_LOOP('',(#12753,#12754,#12755,#12756));
#3909=EDGE_LOOP('',(#12757,#12758,#12759,#12760,#12761,#12762,#12763,#12764));
#3910=EDGE_LOOP('',(#12765,#12766,#12767,#12768));
#3911=EDGE_LOOP('',(#12769,#12770,#12771,#12772,#12773,#12774,#12775,#12776));
#3912=EDGE_LOOP('',(#12777,#12778,#12779,#12780));
#3913=EDGE_LOOP('',(#12781,#12782,#12783,#12784));
#3914=EDGE_LOOP('',(#12785,#12786,#12787,#12788));
#3915=EDGE_LOOP('',(#12789,#12790,#12791,#12792));
#3916=EDGE_LOOP('',(#12793,#12794,#12795,#12796));
#3917=EDGE_LOOP('',(#12797,#12798,#12799,#12800,#12801,#12802,#12803,#12804));
#3918=EDGE_LOOP('',(#12805,#12806,#12807,#12808));
#3919=EDGE_LOOP('',(#12809,#12810,#12811,#12812,#12813,#12814,#12815,#12816));
#3920=EDGE_LOOP('',(#12817,#12818,#12819,#12820));
#3921=EDGE_LOOP('',(#12821,#12822,#12823,#12824));
#3922=EDGE_LOOP('',(#12825,#12826,#12827,#12828));
#3923=EDGE_LOOP('',(#12829,#12830,#12831,#12832));
#3924=EDGE_LOOP('',(#12833,#12834,#12835,#12836));
#3925=EDGE_LOOP('',(#12837,#12838,#12839,#12840,#12841,#12842,#12843,#12844));
#3926=EDGE_LOOP('',(#12845,#12846,#12847,#12848));
#3927=EDGE_LOOP('',(#12849,#12850,#12851,#12852,#12853,#12854,#12855,#12856));
#3928=EDGE_LOOP('',(#12857,#12858,#12859,#12860));
#3929=EDGE_LOOP('',(#12861,#12862,#12863,#12864));
#3930=EDGE_LOOP('',(#12865,#12866,#12867,#12868));
#3931=EDGE_LOOP('',(#12869,#12870,#12871,#12872));
#3932=EDGE_LOOP('',(#12873,#12874,#12875,#12876));
#3933=EDGE_LOOP('',(#12877,#12878,#12879,#12880,#12881,#12882,#12883,#12884));
#3934=EDGE_LOOP('',(#12885,#12886,#12887,#12888));
#3935=EDGE_LOOP('',(#12889,#12890,#12891,#12892,#12893,#12894,#12895,#12896));
#3936=EDGE_LOOP('',(#12897,#12898,#12899,#12900));
#3937=EDGE_LOOP('',(#12901,#12902,#12903,#12904));
#3938=EDGE_LOOP('',(#12905,#12906,#12907,#12908));
#3939=EDGE_LOOP('',(#12909,#12910,#12911,#12912));
#3940=EDGE_LOOP('',(#12913,#12914,#12915,#12916));
#3941=EDGE_LOOP('',(#12917,#12918,#12919,#12920,#12921,#12922,#12923,#12924));
#3942=EDGE_LOOP('',(#12925,#12926,#12927,#12928));
#3943=EDGE_LOOP('',(#12929,#12930,#12931,#12932,#12933,#12934,#12935,#12936));
#3944=EDGE_LOOP('',(#12937,#12938,#12939,#12940));
#3945=EDGE_LOOP('',(#12941,#12942,#12943,#12944));
#3946=EDGE_LOOP('',(#12945,#12946,#12947,#12948));
#3947=EDGE_LOOP('',(#12949,#12950,#12951,#12952));
#3948=EDGE_LOOP('',(#12953,#12954,#12955,#12956));
#3949=EDGE_LOOP('',(#12957,#12958,#12959,#12960,#12961,#12962,#12963,#12964));
#3950=EDGE_LOOP('',(#12965,#12966,#12967,#12968));
#3951=EDGE_LOOP('',(#12969,#12970,#12971,#12972,#12973,#12974,#12975,#12976));
#3952=EDGE_LOOP('',(#12977,#12978,#12979,#12980));
#3953=EDGE_LOOP('',(#12981,#12982,#12983,#12984));
#3954=EDGE_LOOP('',(#12985,#12986,#12987,#12988));
#3955=EDGE_LOOP('',(#12989,#12990,#12991,#12992));
#3956=EDGE_LOOP('',(#12993,#12994,#12995,#12996));
#3957=EDGE_LOOP('',(#12997,#12998,#12999,#13000,#13001,#13002,#13003,#13004));
#3958=EDGE_LOOP('',(#13005,#13006,#13007,#13008));
#3959=EDGE_LOOP('',(#13009,#13010,#13011,#13012,#13013,#13014,#13015,#13016));
#3960=EDGE_LOOP('',(#13017,#13018,#13019,#13020));
#3961=EDGE_LOOP('',(#13021,#13022,#13023,#13024));
#3962=EDGE_LOOP('',(#13025,#13026,#13027,#13028));
#3963=EDGE_LOOP('',(#13029,#13030,#13031,#13032));
#3964=EDGE_LOOP('',(#13033,#13034,#13035,#13036));
#3965=EDGE_LOOP('',(#13037,#13038,#13039,#13040,#13041,#13042,#13043,#13044));
#3966=EDGE_LOOP('',(#13045,#13046,#13047,#13048));
#3967=EDGE_LOOP('',(#13049,#13050,#13051,#13052,#13053,#13054,#13055,#13056));
#3968=EDGE_LOOP('',(#13057,#13058,#13059,#13060));
#3969=EDGE_LOOP('',(#13061,#13062,#13063,#13064));
#3970=EDGE_LOOP('',(#13065,#13066,#13067,#13068));
#3971=EDGE_LOOP('',(#13069,#13070,#13071,#13072));
#3972=EDGE_LOOP('',(#13073,#13074,#13075,#13076));
#3973=EDGE_LOOP('',(#13077,#13078,#13079,#13080));
#3974=EDGE_LOOP('',(#13081,#13082,#13083,#13084,#13085,#13086,#13087,#13088));
#3975=EDGE_LOOP('',(#13089,#13090,#13091,#13092));
#3976=EDGE_LOOP('',(#13093,#13094,#13095,#13096,#13097,#13098,#13099,#13100));
#3977=EDGE_LOOP('',(#13101,#13102,#13103,#13104));
#3978=EDGE_LOOP('',(#13105,#13106,#13107,#13108));
#3979=EDGE_LOOP('',(#13109,#13110,#13111,#13112));
#3980=EDGE_LOOP('',(#13113,#13114,#13115,#13116));
#3981=EDGE_LOOP('',(#13117,#13118,#13119,#13120));
#3982=EDGE_LOOP('',(#13121,#13122,#13123,#13124));
#3983=EDGE_LOOP('',(#13125,#13126,#13127,#13128,#13129,#13130,#13131,#13132));
#3984=EDGE_LOOP('',(#13133,#13134,#13135,#13136));
#3985=EDGE_LOOP('',(#13137,#13138,#13139,#13140,#13141,#13142,#13143,#13144));
#3986=EDGE_LOOP('',(#13145,#13146,#13147,#13148));
#3987=EDGE_LOOP('',(#13149,#13150,#13151,#13152));
#3988=EDGE_LOOP('',(#13153,#13154,#13155,#13156));
#3989=EDGE_LOOP('',(#13157,#13158,#13159,#13160,#13161,#13162));
#3990=EDGE_LOOP('',(#13163,#13164,#13165,#13166));
#3991=EDGE_LOOP('',(#13167,#13168,#13169,#13170,#13171,#13172));
#3992=EDGE_LOOP('',(#13173));
#3993=EDGE_LOOP('',(#13174,#13175,#13176,#13177));
#3994=EDGE_LOOP('',(#13178,#13179,#13180,#13181));
#3995=EDGE_LOOP('',(#13182,#13183,#13184,#13185));
#3996=EDGE_LOOP('',(#13186,#13187,#13188,#13189));
#3997=EDGE_LOOP('',(#13190));
#3998=EDGE_LOOP('',(#13191));
#3999=EDGE_LOOP('',(#13192,#13193,#13194,#13195));
#4000=EDGE_LOOP('',(#13196,#13197,#13198,#13199));
#4001=EDGE_LOOP('',(#13200));
#4002=EDGE_LOOP('',(#13201));
#4003=EDGE_LOOP('',(#13202,#13203,#13204,#13205));
#4004=EDGE_LOOP('',(#13206));
#4005=EDGE_LOOP('',(#13207));
#4006=EDGE_LOOP('',(#13208,#13209,#13210,#13211));
#4007=EDGE_LOOP('',(#13212,#13213,#13214,#13215));
#4008=EDGE_LOOP('',(#13216));
#4009=EDGE_LOOP('',(#13217));
#4010=EDGE_LOOP('',(#13218,#13219,#13220,#13221));
#4011=EDGE_LOOP('',(#13222,#13223,#13224,#13225));
#4012=EDGE_LOOP('',(#13226));
#4013=EDGE_LOOP('',(#13227,#13228,#13229,#13230));
#4014=EDGE_LOOP('',(#13231,#13232,#13233,#13234));
#4015=EDGE_LOOP('',(#13235,#13236,#13237,#13238));
#4016=EDGE_LOOP('',(#13239));
#4017=EDGE_LOOP('',(#13240));
#4018=EDGE_LOOP('',(#13241,#13242,#13243,#13244));
#4019=EDGE_LOOP('',(#13245,#13246,#13247,#13248));
#4020=EDGE_LOOP('',(#13249,#13250,#13251,#13252));
#4021=EDGE_LOOP('',(#13253));
#4022=EDGE_LOOP('',(#13254));
#4023=EDGE_LOOP('',(#13255,#13256,#13257,#13258));
#4024=EDGE_LOOP('',(#13259));
#4025=EDGE_LOOP('',(#13260));
#4026=EDGE_LOOP('',(#13261,#13262,#13263,#13264));
#4027=EDGE_LOOP('',(#13265,#13266,#13267,#13268));
#4028=EDGE_LOOP('',(#13269,#13270,#13271,#13272));
#4029=EDGE_LOOP('',(#13273,#13274,#13275,#13276));
#4030=EDGE_LOOP('',(#13277,#13278,#13279,#13280));
#4031=EDGE_LOOP('',(#13281));
#4032=EDGE_LOOP('',(#13282));
#4033=EDGE_LOOP('',(#13283,#13284,#13285,#13286));
#4034=EDGE_LOOP('',(#13287));
#4035=EDGE_LOOP('',(#13288));
#4036=EDGE_LOOP('',(#13289,#13290,#13291,#13292));
#4037=EDGE_LOOP('',(#13293));
#4038=EDGE_LOOP('',(#13294));
#4039=EDGE_LOOP('',(#13295,#13296,#13297,#13298));
#4040=EDGE_LOOP('',(#13299,#13300,#13301,#13302));
#4041=EDGE_LOOP('',(#13303));
#4042=EDGE_LOOP('',(#13304));
#4043=EDGE_LOOP('',(#13305,#13306,#13307,#13308));
#4044=EDGE_LOOP('',(#13309,#13310,#13311,#13312,#13313,#13314));
#4045=EDGE_LOOP('',(#13315,#13316,#13317,#13318,#13319,#13320));
#4046=EDGE_LOOP('',(#13321,#13322,#13323,#13324,#13325,#13326));
#4047=EDGE_LOOP('',(#13327,#13328,#13329,#13330,#13331,#13332));
#4048=EDGE_LOOP('',(#13333,#13334,#13335,#13336,#13337,#13338));
#4049=EDGE_LOOP('',(#13339,#13340,#13341,#13342,#13343,#13344,#13345,#13346,
#13347,#13348,#13349,#13350,#13351,#13352,#13353,#13354));
#4050=EDGE_LOOP('',(#13355,#13356,#13357,#13358,#13359,#13360));
#4051=EDGE_LOOP('',(#13361,#13362,#13363,#13364));
#4052=EDGE_LOOP('',(#13365,#13366,#13367,#13368,#13369,#13370,#13371,#13372,
#13373,#13374,#13375,#13376,#13377,#13378,#13379,#13380,#13381,#13382,#13383,
#13384,#13385,#13386,#13387,#13388));
#4053=EDGE_LOOP('',(#13389,#13390,#13391,#13392,#13393));
#4054=EDGE_LOOP('',(#13394,#13395,#13396,#13397,#13398,#13399,#13400,#13401,
#13402,#13403,#13404,#13405,#13406,#13407,#13408,#13409,#13410,#13411,#13412,
#13413,#13414,#13415,#13416,#13417,#13418));
#4055=EDGE_LOOP('',(#13419,#13420,#13421,#13422,#13423,#13424,#13425,#13426,
#13427,#13428));
#4056=EDGE_LOOP('',(#13429,#13430,#13431,#13432));
#4057=EDGE_LOOP('',(#13433,#13434,#13435,#13436));
#4058=EDGE_LOOP('',(#13437,#13438,#13439,#13440));
#4059=EDGE_LOOP('',(#13441,#13442,#13443));
#4060=EDGE_LOOP('',(#13444,#13445,#13446,#13447));
#4061=EDGE_LOOP('',(#13448,#13449,#13450,#13451));
#4062=EDGE_LOOP('',(#13452,#13453,#13454,#13455,#13456));
#4063=EDGE_LOOP('',(#13457,#13458,#13459,#13460,#13461,#13462));
#4064=EDGE_LOOP('',(#13463));
#4065=EDGE_LOOP('',(#13464));
#4066=EDGE_LOOP('',(#13465,#13466,#13467,#13468,#13469,#13470,#13471));
#4067=EDGE_LOOP('',(#13472,#13473,#13474,#13475,#13476));
#4068=EDGE_LOOP('',(#13477,#13478,#13479,#13480,#13481,#13482,#13483,#13484));
#4069=EDGE_LOOP('',(#13485));
#4070=EDGE_LOOP('',(#13486));
#4071=EDGE_LOOP('',(#13487,#13488,#13489,#13490));
#4072=EDGE_LOOP('',(#13491,#13492,#13493,#13494));
#4073=EDGE_LOOP('',(#13495,#13496,#13497,#13498));
#4074=EDGE_LOOP('',(#13499));
#4075=EDGE_LOOP('',(#13500));
#4076=EDGE_LOOP('',(#13501,#13502,#13503,#13504));
#4077=EDGE_LOOP('',(#13505));
#4078=EDGE_LOOP('',(#13506));
#4079=EDGE_LOOP('',(#13507,#13508,#13509,#13510));
#4080=EDGE_LOOP('',(#13511,#13512,#13513,#13514));
#4081=EDGE_LOOP('',(#13515,#13516,#13517,#13518));
#4082=EDGE_LOOP('',(#13519));
#4083=EDGE_LOOP('',(#13520));
#4084=EDGE_LOOP('',(#13521,#13522,#13523,#13524));
#4085=EDGE_LOOP('',(#13525,#13526,#13527,#13528));
#4086=EDGE_LOOP('',(#13529,#13530,#13531,#13532));
#4087=EDGE_LOOP('',(#13533));
#4088=EDGE_LOOP('',(#13534));
#4089=EDGE_LOOP('',(#13535,#13536,#13537,#13538));
#4090=EDGE_LOOP('',(#13539,#13540,#13541,#13542));
#4091=EDGE_LOOP('',(#13543));
#4092=EDGE_LOOP('',(#13544));
#4093=EDGE_LOOP('',(#13545,#13546,#13547,#13548));
#4094=EDGE_LOOP('',(#13549,#13550,#13551,#13552));
#4095=EDGE_LOOP('',(#13553,#13554,#13555,#13556));
#4096=EDGE_LOOP('',(#13557));
#4097=EDGE_LOOP('',(#13558));
#4098=EDGE_LOOP('',(#13559,#13560,#13561,#13562));
#4099=EDGE_LOOP('',(#13563,#13564,#13565,#13566));
#4100=EDGE_LOOP('',(#13567));
#4101=EDGE_LOOP('',(#13568));
#4102=EDGE_LOOP('',(#13569,#13570,#13571,#13572));
#4103=EDGE_LOOP('',(#13573));
#4104=EDGE_LOOP('',(#13574));
#4105=EDGE_LOOP('',(#13575,#13576,#13577,#13578));
#4106=EDGE_LOOP('',(#13579));
#4107=EDGE_LOOP('',(#13580));
#4108=EDGE_LOOP('',(#13581));
#4109=EDGE_LOOP('',(#13582));
#4110=EDGE_LOOP('',(#13583,#13584,#13585,#13586));
#4111=EDGE_LOOP('',(#13587,#13588,#13589,#13590));
#4112=EDGE_LOOP('',(#13591));
#4113=EDGE_LOOP('',(#13592));
#4114=EDGE_LOOP('',(#13593,#13594,#13595,#13596));
#4115=EDGE_LOOP('',(#13597,#13598,#13599,#13600));
#4116=EDGE_LOOP('',(#13601));
#4117=EDGE_LOOP('',(#13602));
#4118=EDGE_LOOP('',(#13603,#13604,#13605,#13606));
#4119=EDGE_LOOP('',(#13607,#13608,#13609,#13610));
#4120=EDGE_LOOP('',(#13611,#13612,#13613,#13614));
#4121=EDGE_LOOP('',(#13615));
#4122=EDGE_LOOP('',(#13616));
#4123=EDGE_LOOP('',(#13617,#13618,#13619,#13620));
#4124=EDGE_LOOP('',(#13621));
#4125=EDGE_LOOP('',(#13622));
#4126=EDGE_LOOP('',(#13623,#13624,#13625,#13626));
#4127=EDGE_LOOP('',(#13627,#13628,#13629,#13630));
#4128=EDGE_LOOP('',(#13631,#13632,#13633,#13634));
#4129=EDGE_LOOP('',(#13635));
#4130=EDGE_LOOP('',(#13636));
#4131=EDGE_LOOP('',(#13637,#13638,#13639,#13640));
#4132=EDGE_LOOP('',(#13641));
#4133=EDGE_LOOP('',(#13642));
#4134=EDGE_LOOP('',(#13643,#13644,#13645,#13646));
#4135=EDGE_LOOP('',(#13647));
#4136=EDGE_LOOP('',(#13648));
#4137=EDGE_LOOP('',(#13649,#13650,#13651,#13652));
#4138=EDGE_LOOP('',(#13653,#13654,#13655,#13656));
#4139=EDGE_LOOP('',(#13657,#13658,#13659,#13660));
#4140=EDGE_LOOP('',(#13661));
#4141=EDGE_LOOP('',(#13662));
#4142=EDGE_LOOP('',(#13663,#13664,#13665,#13666));
#4143=EDGE_LOOP('',(#13667));
#4144=EDGE_LOOP('',(#13668));
#4145=EDGE_LOOP('',(#13669,#13670,#13671,#13672));
#4146=EDGE_LOOP('',(#13673));
#4147=EDGE_LOOP('',(#13674));
#4148=EDGE_LOOP('',(#13675,#13676,#13677,#13678));
#4149=EDGE_LOOP('',(#13679));
#4150=EDGE_LOOP('',(#13680));
#4151=EDGE_LOOP('',(#13681,#13682,#13683,#13684));
#4152=EDGE_LOOP('',(#13685,#13686,#13687,#13688));
#4153=EDGE_LOOP('',(#13689,#13690,#13691,#13692));
#4154=EDGE_LOOP('',(#13693));
#4155=EDGE_LOOP('',(#13694));
#4156=EDGE_LOOP('',(#13695,#13696,#13697,#13698));
#4157=EDGE_LOOP('',(#13699));
#4158=EDGE_LOOP('',(#13700));
#4159=EDGE_LOOP('',(#13701,#13702,#13703,#13704));
#4160=EDGE_LOOP('',(#13705,#13706,#13707,#13708));
#4161=EDGE_LOOP('',(#13709,#13710,#13711,#13712));
#4162=EDGE_LOOP('',(#13713,#13714,#13715,#13716));
#4163=EDGE_LOOP('',(#13717,#13718,#13719,#13720));
#4164=EDGE_LOOP('',(#13721,#13722,#13723,#13724));
#4165=EDGE_LOOP('',(#13725,#13726,#13727,#13728,#13729,#13730,#13731,#13732));
#4166=EDGE_LOOP('',(#13733));
#4167=EDGE_LOOP('',(#13734));
#4168=EDGE_LOOP('',(#13735,#13736,#13737,#13738));
#4169=EDGE_LOOP('',(#13739,#13740,#13741,#13742,#13743,#13744,#13745,#13746));
#4170=EDGE_LOOP('',(#13747));
#4171=EDGE_LOOP('',(#13748));
#4172=EDGE_LOOP('',(#13749,#13750,#13751,#13752));
#4173=EDGE_LOOP('',(#13753,#13754,#13755,#13756));
#4174=EDGE_LOOP('',(#13757,#13758,#13759,#13760));
#4175=EDGE_LOOP('',(#13761,#13762,#13763,#13764));
#4176=EDGE_LOOP('',(#13765,#13766,#13767,#13768));
#4177=EDGE_LOOP('',(#13769,#13770,#13771,#13772));
#4178=EDGE_LOOP('',(#13773,#13774,#13775,#13776));
#4179=EDGE_LOOP('',(#13777,#13778,#13779,#13780));
#4180=EDGE_LOOP('',(#13781,#13782,#13783,#13784));
#4181=EDGE_LOOP('',(#13785,#13786,#13787,#13788));
#4182=EDGE_LOOP('',(#13789,#13790,#13791,#13792));
#4183=EDGE_LOOP('',(#13793,#13794,#13795,#13796));
#4184=EDGE_LOOP('',(#13797,#13798,#13799,#13800,#13801,#13802));
#4185=EDGE_LOOP('',(#13803,#13804,#13805,#13806));
#4186=EDGE_LOOP('',(#13807,#13808,#13809,#13810,#13811,#13812));
#4187=EDGE_LOOP('',(#13813,#13814,#13815,#13816));
#4188=EDGE_LOOP('',(#13817,#13818,#13819,#13820,#13821,#13822));
#4189=EDGE_LOOP('',(#13823,#13824,#13825,#13826));
#4190=EDGE_LOOP('',(#13827,#13828,#13829,#13830,#13831,#13832));
#4191=EDGE_LOOP('',(#13833,#13834,#13835,#13836));
#4192=EDGE_LOOP('',(#13837,#13838,#13839,#13840,#13841,#13842));
#4193=EDGE_LOOP('',(#13843,#13844,#13845,#13846));
#4194=EDGE_LOOP('',(#13847,#13848,#13849,#13850,#13851,#13852));
#4195=EDGE_LOOP('',(#13853,#13854,#13855,#13856,#13857));
#4196=EDGE_LOOP('',(#13858,#13859,#13860,#13861,#13862,#13863));
#4197=EDGE_LOOP('',(#13864,#13865,#13866,#13867,#13868,#13869));
#4198=EDGE_LOOP('',(#13870,#13871,#13872,#13873));
#4199=EDGE_LOOP('',(#13874,#13875,#13876,#13877,#13878,#13879));
#4200=EDGE_LOOP('',(#13880,#13881,#13882,#13883,#13884,#13885));
#4201=EDGE_LOOP('',(#13886,#13887,#13888,#13889,#13890));
#4202=EDGE_LOOP('',(#13891,#13892,#13893,#13894,#13895,#13896,#13897,#13898,
#13899,#13900,#13901,#13902,#13903,#13904,#13905,#13906,#13907,#13908,#13909,
#13910,#13911,#13912,#13913,#13914,#13915,#13916,#13917,#13918,#13919,#13920,
#13921,#13922,#13923,#13924,#13925,#13926,#13927,#13928,#13929,#13930,#13931,
#13932,#13933,#13934));
#4203=EDGE_LOOP('',(#13935,#13936,#13937,#13938,#13939));
#4204=EDGE_LOOP('',(#13940,#13941,#13942,#13943,#13944));
#4205=EDGE_LOOP('',(#13945,#13946,#13947,#13948,#13949,#13950,#13951,#13952,
#13953,#13954,#13955,#13956,#13957,#13958,#13959,#13960,#13961,#13962,#13963,
#13964,#13965,#13966,#13967,#13968,#13969,#13970,#13971,#13972,#13973,#13974,
#13975,#13976,#13977,#13978,#13979,#13980,#13981,#13982,#13983,#13984,#13985,
#13986,#13987,#13988,#13989,#13990,#13991,#13992,#13993,#13994,#13995,#13996,
#13997,#13998,#13999,#14000));
#4206=EDGE_LOOP('',(#14001,#14002,#14003,#14004,#14005));
#4207=EDGE_LOOP('',(#14006,#14007,#14008,#14009,#14010,#14011,#14012,#14013,
#14014,#14015,#14016,#14017,#14018,#14019,#14020,#14021,#14022,#14023,#14024,
#14025,#14026,#14027,#14028,#14029,#14030,#14031,#14032,#14033,#14034,#14035,
#14036,#14037,#14038,#14039,#14040,#14041,#14042,#14043,#14044,#14045,#14046,
#14047,#14048,#14049,#14050,#14051,#14052,#14053,#14054,#14055,#14056,#14057,
#14058,#14059,#14060));
#4208=EDGE_LOOP('',(#14061,#14062,#14063,#14064,#14065,#14066,#14067));
#4209=EDGE_LOOP('',(#14068));
#4210=EDGE_LOOP('',(#14069));
#4211=EDGE_LOOP('',(#14070,#14071,#14072,#14073,#14074,#14075,#14076,#14077,
#14078,#14079));
#4212=EDGE_LOOP('',(#14080,#14081,#14082,#14083));
#4213=EDGE_LOOP('',(#14084,#14085,#14086,#14087));
#4214=EDGE_LOOP('',(#14088,#14089,#14090,#14091));
#4215=EDGE_LOOP('',(#14092,#14093,#14094));
#4216=EDGE_LOOP('',(#14095,#14096,#14097,#14098));
#4217=EDGE_LOOP('',(#14099,#14100,#14101,#14102));
#4218=EDGE_LOOP('',(#14103,#14104,#14105,#14106,#14107));
#4219=EDGE_LOOP('',(#14108,#14109,#14110,#14111,#14112,#14113));
#4220=EDGE_LOOP('',(#14114));
#4221=EDGE_LOOP('',(#14115,#14116,#14117,#14118));
#4222=EDGE_LOOP('',(#14119,#14120,#14121,#14122));
#4223=EDGE_LOOP('',(#14123));
#4224=EDGE_LOOP('',(#14124));
#4225=EDGE_LOOP('',(#14125));
#4226=EDGE_LOOP('',(#14126,#14127,#14128,#14129,#14130,#14131,#14132));
#4227=EDGE_LOOP('',(#14133,#14134,#14135,#14136));
#4228=EDGE_LOOP('',(#14137,#14138,#14139,#14140));
#4229=EDGE_LOOP('',(#14141,#14142,#14143,#14144,#14145,#14146));
#4230=EDGE_LOOP('',(#14147,#14148,#14149,#14150,#14151));
#4231=EDGE_LOOP('',(#14152,#14153,#14154,#14155,#14156));
#4232=EDGE_LOOP('',(#14157,#14158,#14159,#14160,#14161));
#4233=EDGE_LOOP('',(#14162,#14163,#14164,#14165,#14166));
#4234=EDGE_LOOP('',(#14167,#14168,#14169,#14170,#14171));
#4235=EDGE_LOOP('',(#14172,#14173,#14174,#14175,#14176,#14177));
#4236=EDGE_LOOP('',(#14178,#14179,#14180,#14181,#14182));
#4237=EDGE_LOOP('',(#14183,#14184,#14185,#14186,#14187));
#4238=EDGE_LOOP('',(#14188,#14189,#14190,#14191,#14192));
#4239=EDGE_LOOP('',(#14193,#14194,#14195,#14196,#14197));
#4240=EDGE_LOOP('',(#14198,#14199,#14200,#14201,#14202));
#4241=EDGE_LOOP('',(#14203,#14204,#14205,#14206,#14207));
#4242=EDGE_LOOP('',(#14208,#14209,#14210,#14211,#14212));
#4243=EDGE_LOOP('',(#14213,#14214,#14215,#14216,#14217,#14218,#14219,#14220,
#14221,#14222,#14223,#14224,#14225,#14226,#14227,#14228,#14229,#14230,#14231,
#14232,#14233,#14234,#14235,#14236,#14237,#14238,#14239,#14240,#14241,#14242,
#14243,#14244,#14245,#14246,#14247,#14248));
#4244=EDGE_LOOP('',(#14249,#14250,#14251,#14252,#14253));
#4245=EDGE_LOOP('',(#14254,#14255,#14256,#14257,#14258));
#4246=EDGE_LOOP('',(#14259,#14260,#14261,#14262,#14263,#14264,#14265,#14266,
#14267,#14268,#14269,#14270,#14271,#14272,#14273,#14274,#14275,#14276,#14277,
#14278,#14279,#14280,#14281,#14282,#14283,#14284,#14285,#14286,#14287,#14288,
#14289,#14290,#14291,#14292,#14293,#14294,#14295,#14296,#14297,#14298,#14299,
#14300,#14301,#14302));
#4247=EDGE_LOOP('',(#14303,#14304,#14305,#14306,#14307));
#4248=EDGE_LOOP('',(#14308,#14309,#14310,#14311,#14312,#14313,#14314,#14315,
#14316,#14317,#14318,#14319,#14320,#14321,#14322,#14323,#14324,#14325,#14326,
#14327,#14328,#14329,#14330,#14331,#14332,#14333,#14334,#14335,#14336,#14337,
#14338,#14339,#14340,#14341,#14342,#14343,#14344,#14345,#14346,#14347,#14348,
#14349,#14350,#14351,#14352));
#4249=EDGE_LOOP('',(#14353,#14354,#14355,#14356,#14357,#14358,#14359));
#4250=EDGE_LOOP('',(#14360));
#4251=EDGE_LOOP('',(#14361));
#4252=EDGE_LOOP('',(#14362,#14363,#14364,#14365,#14366,#14367,#14368,#14369,
#14370,#14371));
#4253=EDGE_LOOP('',(#14372,#14373,#14374,#14375));
#4254=EDGE_LOOP('',(#14376,#14377,#14378,#14379));
#4255=EDGE_LOOP('',(#14380,#14381,#14382,#14383));
#4256=EDGE_LOOP('',(#14384,#14385,#14386));
#4257=EDGE_LOOP('',(#14387,#14388,#14389,#14390));
#4258=EDGE_LOOP('',(#14391,#14392,#14393,#14394));
#4259=EDGE_LOOP('',(#14395,#14396,#14397,#14398,#14399));
#4260=EDGE_LOOP('',(#14400,#14401,#14402,#14403,#14404,#14405));
#4261=EDGE_LOOP('',(#14406));
#4262=EDGE_LOOP('',(#14407,#14408,#14409,#14410));
#4263=EDGE_LOOP('',(#14411,#14412,#14413,#14414));
#4264=EDGE_LOOP('',(#14415));
#4265=EDGE_LOOP('',(#14416));
#4266=EDGE_LOOP('',(#14417));
#4267=EDGE_LOOP('',(#14418,#14419,#14420,#14421,#14422,#14423,#14424));
#4268=EDGE_LOOP('',(#14425,#14426,#14427,#14428));
#4269=EDGE_LOOP('',(#14429,#14430,#14431,#14432));
#4270=EDGE_LOOP('',(#14433));
#4271=EDGE_LOOP('',(#14434));
#4272=EDGE_LOOP('',(#14435,#14436,#14437,#14438));
#4273=EDGE_LOOP('',(#14439,#14440,#14441,#14442));
#4274=EDGE_LOOP('',(#14443));
#4275=EDGE_LOOP('',(#14444));
#4276=EDGE_LOOP('',(#14445,#14446,#14447,#14448));
#4277=EDGE_LOOP('',(#14449,#14450,#14451,#14452));
#4278=EDGE_LOOP('',(#14453,#14454,#14455,#14456));
#4279=EDGE_LOOP('',(#14457));
#4280=EDGE_LOOP('',(#14458));
#4281=LINE('',#21063,#5141);
#4282=LINE('',#21065,#5142);
#4283=LINE('',#21067,#5143);
#4284=LINE('',#21068,#5144);
#4285=LINE('',#21071,#5145);
#4286=LINE('',#21073,#5146);
#4287=LINE('',#21074,#5147);
#4288=LINE('',#21077,#5148);
#4289=LINE('',#21079,#5149);
#4290=LINE('',#21080,#5150);
#4291=LINE('',#21082,#5151);
#4292=LINE('',#21083,#5152);
#4293=LINE('',#21088,#5153);
#4294=LINE('',#21090,#5154);
#4295=LINE('',#21092,#5155);
#4296=LINE('',#21093,#5156);
#4297=LINE('',#21096,#5157);
#4298=LINE('',#21098,#5158);
#4299=LINE('',#21100,#5159);
#4300=LINE('',#21102,#5160);
#4301=LINE('',#21103,#5161);
#4302=LINE('',#21106,#5162);
#4303=LINE('',#21107,#5163);
#4304=LINE('',#21110,#5164);
#4305=LINE('',#21111,#5165);
#4306=LINE('',#21114,#5166);
#4307=LINE('',#21115,#5167);
#4308=LINE('',#21119,#5168);
#4309=LINE('',#21121,#5169);
#4310=LINE('',#21123,#5170);
#4311=LINE('',#21124,#5171);
#4312=LINE('',#21127,#5172);
#4313=LINE('',#21129,#5173);
#4314=LINE('',#21130,#5174);
#4315=LINE('',#21133,#5175);
#4316=LINE('',#21135,#5176);
#4317=LINE('',#21136,#5177);
#4318=LINE('',#21138,#5178);
#4319=LINE('',#21139,#5179);
#4320=LINE('',#21144,#5180);
#4321=LINE('',#21146,#5181);
#4322=LINE('',#21148,#5182);
#4323=LINE('',#21149,#5183);
#4324=LINE('',#21152,#5184);
#4325=LINE('',#21154,#5185);
#4326=LINE('',#21155,#5186);
#4327=LINE('',#21158,#5187);
#4328=LINE('',#21160,#5188);
#4329=LINE('',#21161,#5189);
#4330=LINE('',#21163,#5190);
#4331=LINE('',#21164,#5191);
#4332=LINE('',#21169,#5192);
#4333=LINE('',#21171,#5193);
#4334=LINE('',#21173,#5194);
#4335=LINE('',#21174,#5195);
#4336=LINE('',#21177,#5196);
#4337=LINE('',#21179,#5197);
#4338=LINE('',#21180,#5198);
#4339=LINE('',#21183,#5199);
#4340=LINE('',#21185,#5200);
#4341=LINE('',#21186,#5201);
#4342=LINE('',#21188,#5202);
#4343=LINE('',#21189,#5203);
#4344=LINE('',#21194,#5204);
#4345=LINE('',#21196,#5205);
#4346=LINE('',#21198,#5206);
#4347=LINE('',#21199,#5207);
#4348=LINE('',#21203,#5208);
#4349=LINE('',#21205,#5209);
#4350=LINE('',#21207,#5210);
#4351=LINE('',#21208,#5211);
#4352=LINE('',#21211,#5212);
#4353=LINE('',#21213,#5213);
#4354=LINE('',#21214,#5214);
#4355=LINE('',#21216,#5215);
#4356=LINE('',#21217,#5216);
#4357=LINE('',#21220,#5217);
#4358=LINE('',#21221,#5218);
#4359=LINE('',#21224,#5219);
#4360=LINE('',#21226,#5220);
#4361=LINE('',#21228,#5221);
#4362=LINE('',#21229,#5222);
#4363=LINE('',#21232,#5223);
#4364=LINE('',#21234,#5224);
#4365=LINE('',#21235,#5225);
#4366=LINE('',#21238,#5226);
#4367=LINE('',#21240,#5227);
#4368=LINE('',#21242,#5228);
#4369=LINE('',#21244,#5229);
#4370=LINE('',#21246,#5230);
#4371=LINE('',#21247,#5231);
#4372=LINE('',#21249,#5232);
#4373=LINE('',#21251,#5233);
#4374=LINE('',#21253,#5234);
#4375=LINE('',#21254,#5235);
#4376=LINE('',#21260,#5236);
#4377=LINE('',#21262,#5237);
#4378=LINE('',#21264,#5238);
#4379=LINE('',#21265,#5239);
#4380=LINE('',#21268,#5240);
#4381=LINE('',#21270,#5241);
#4382=LINE('',#21271,#5242);
#4383=LINE('',#21274,#5243);
#4384=LINE('',#21276,#5244);
#4385=LINE('',#21277,#5245);
#4386=LINE('',#21279,#5246);
#4387=LINE('',#21280,#5247);
#4388=LINE('',#21285,#5248);
#4389=LINE('',#21287,#5249);
#4390=LINE('',#21289,#5250);
#4391=LINE('',#21290,#5251);
#4392=LINE('',#21294,#5252);
#4393=LINE('',#21296,#5253);
#4394=LINE('',#21298,#5254);
#4395=LINE('',#21299,#5255);
#4396=LINE('',#21301,#5256);
#4397=LINE('',#21302,#5257);
#4398=LINE('',#21306,#5258);
#4399=LINE('',#21307,#5259);
#4400=LINE('',#21308,#5260);
#4401=LINE('',#21311,#5261);
#4402=LINE('',#21312,#5262);
#4403=LINE('',#21316,#5263);
#4404=LINE('',#21318,#5264);
#4405=LINE('',#21320,#5265);
#4406=LINE('',#21321,#5266);
#4407=LINE('',#21324,#5267);
#4408=LINE('',#21326,#5268);
#4409=LINE('',#21327,#5269);
#4410=LINE('',#21330,#5270);
#4411=LINE('',#21332,#5271);
#4412=LINE('',#21333,#5272);
#4413=LINE('',#21335,#5273);
#4414=LINE('',#21336,#5274);
#4415=LINE('',#21341,#5275);
#4416=LINE('',#21343,#5276);
#4417=LINE('',#21345,#5277);
#4418=LINE('',#21346,#5278);
#4419=LINE('',#21349,#5279);
#4420=LINE('',#21351,#5280);
#4421=LINE('',#21352,#5281);
#4422=LINE('',#21355,#5282);
#4423=LINE('',#21357,#5283);
#4424=LINE('',#21358,#5284);
#4425=LINE('',#21360,#5285);
#4426=LINE('',#21361,#5286);
#4427=LINE('',#21366,#5287);
#4428=LINE('',#21368,#5288);
#4429=LINE('',#21370,#5289);
#4430=LINE('',#21371,#5290);
#4431=LINE('',#21374,#5291);
#4432=LINE('',#21376,#5292);
#4433=LINE('',#21377,#5293);
#4434=LINE('',#21380,#5294);
#4435=LINE('',#21382,#5295);
#4436=LINE('',#21383,#5296);
#4437=LINE('',#21385,#5297);
#4438=LINE('',#21386,#5298);
#4439=LINE('',#21391,#5299);
#4440=LINE('',#21393,#5300);
#4441=LINE('',#21395,#5301);
#4442=LINE('',#21396,#5302);
#4443=LINE('',#21399,#5303);
#4444=LINE('',#21401,#5304);
#4445=LINE('',#21402,#5305);
#4446=LINE('',#21406,#5306);
#4447=LINE('',#21408,#5307);
#4448=LINE('',#21410,#5308);
#4449=LINE('',#21411,#5309);
#4450=LINE('',#21413,#5310);
#4451=LINE('',#21414,#5311);
#4452=LINE('',#21417,#5312);
#4453=LINE('',#21418,#5313);
#4454=LINE('',#21421,#5314);
#4455=LINE('',#21423,#5315);
#4456=LINE('',#21425,#5316);
#4457=LINE('',#21426,#5317);
#4458=LINE('',#21429,#5318);
#4459=LINE('',#21431,#5319);
#4460=LINE('',#21433,#5320);
#4461=LINE('',#21434,#5321);
#4462=LINE('',#21437,#5322);
#4463=LINE('',#21439,#5323);
#4464=LINE('',#21441,#5324);
#4465=LINE('',#21447,#5325);
#4466=LINE('',#21453,#5326);
#4467=LINE('',#21454,#5327);
#4468=LINE('',#21456,#5328);
#4469=LINE('',#21458,#5329);
#4470=LINE('',#21460,#5330);
#4471=LINE('',#21462,#5331);
#4472=LINE('',#21464,#5332);
#4473=LINE('',#21465,#5333);
#4474=LINE('',#21477,#5334);
#4475=LINE('',#21480,#5335);
#4476=LINE('',#21485,#5336);
#4477=LINE('',#21489,#5337);
#4478=LINE('',#21491,#5338);
#4479=LINE('',#21492,#5339);
#4480=LINE('',#21495,#5340);
#4481=LINE('',#21497,#5341);
#4482=LINE('',#21498,#5342);
#4483=LINE('',#21501,#5343);
#4484=LINE('',#21503,#5344);
#4485=LINE('',#21504,#5345);
#4486=LINE('',#21512,#5346);
#4487=LINE('',#21514,#5347);
#4488=LINE('',#21516,#5348);
#4489=LINE('',#21517,#5349);
#4490=LINE('',#21520,#5350);
#4491=LINE('',#21522,#5351);
#4492=LINE('',#21523,#5352);
#4493=LINE('',#21526,#5353);
#4494=LINE('',#21528,#5354);
#4495=LINE('',#21529,#5355);
#4496=LINE('',#21543,#5356);
#4497=LINE('',#21547,#5357);
#4498=LINE('',#21550,#5358);
#4499=LINE('',#21552,#5359);
#4500=LINE('',#21581,#5360);
#4501=LINE('',#21584,#5361);
#4502=LINE('',#21611,#5362);
#4503=LINE('',#21614,#5363);
#4504=LINE('',#21655,#5364);
#4505=LINE('',#21656,#5365);
#4506=LINE('',#21658,#5366);
#4507=LINE('',#21660,#5367);
#4508=LINE('',#21662,#5368);
#4509=LINE('',#21664,#5369);
#4510=LINE('',#21666,#5370);
#4511=LINE('',#21718,#5371);
#4512=LINE('',#21722,#5372);
#4513=LINE('',#21727,#5373);
#4514=LINE('',#21731,#5374);
#4515=LINE('',#21763,#5375);
#4516=LINE('',#21794,#5376);
#4517=LINE('',#21811,#5377);
#4518=LINE('',#21813,#5378);
#4519=LINE('',#21815,#5379);
#4520=LINE('',#21821,#5380);
#4521=LINE('',#21826,#5381);
#4522=LINE('',#21828,#5382);
#4523=LINE('',#21833,#5383);
#4524=LINE('',#21836,#5384);
#4525=LINE('',#21838,#5385);
#4526=LINE('',#21840,#5386);
#4527=LINE('',#21841,#5387);
#4528=LINE('',#21844,#5388);
#4529=LINE('',#21846,#5389);
#4530=LINE('',#21848,#5390);
#4531=LINE('',#21849,#5391);
#4532=LINE('',#21852,#5392);
#4533=LINE('',#21854,#5393);
#4534=LINE('',#21856,#5394);
#4535=LINE('',#21857,#5395);
#4536=LINE('',#21860,#5396);
#4537=LINE('',#21862,#5397);
#4538=LINE('',#21864,#5398);
#4539=LINE('',#21865,#5399);
#4540=LINE('',#21868,#5400);
#4541=LINE('',#21870,#5401);
#4542=LINE('',#21872,#5402);
#4543=LINE('',#21873,#5403);
#4544=LINE('',#21876,#5404);
#4545=LINE('',#21878,#5405);
#4546=LINE('',#21880,#5406);
#4547=LINE('',#21881,#5407);
#4548=LINE('',#21885,#5408);
#4549=LINE('',#21889,#5409);
#4550=LINE('',#21946,#5410);
#4551=LINE('',#22008,#5411);
#4552=LINE('',#22012,#5412);
#4553=LINE('',#22015,#5413);
#4554=LINE('',#22041,#5414);
#4555=LINE('',#22045,#5415);
#4556=LINE('',#22048,#5416);
#4557=LINE('',#22052,#5417);
#4558=LINE('',#22056,#5418);
#4559=LINE('',#22059,#5419);
#4560=LINE('',#22063,#5420);
#4561=LINE('',#22067,#5421);
#4562=LINE('',#22071,#5422);
#4563=LINE('',#22076,#5423);
#4564=LINE('',#22080,#5424);
#4565=LINE('',#22083,#5425);
#4566=LINE('',#22087,#5426);
#4567=LINE('',#22091,#5427);
#4568=LINE('',#22095,#5428);
#4569=LINE('',#22100,#5429);
#4570=LINE('',#22104,#5430);
#4571=LINE('',#22107,#5431);
#4572=LINE('',#22111,#5432);
#4573=LINE('',#22115,#5433);
#4574=LINE('',#22119,#5434);
#4575=LINE('',#22124,#5435);
#4576=LINE('',#22128,#5436);
#4577=LINE('',#22131,#5437);
#4578=LINE('',#22135,#5438);
#4579=LINE('',#22139,#5439);
#4580=LINE('',#22143,#5440);
#4581=LINE('',#22148,#5441);
#4582=LINE('',#22152,#5442);
#4583=LINE('',#22155,#5443);
#4584=LINE('',#22159,#5444);
#4585=LINE('',#22163,#5445);
#4586=LINE('',#22166,#5446);
#4587=LINE('',#22170,#5447);
#4588=LINE('',#22174,#5448);
#4589=LINE('',#22177,#5449);
#4590=LINE('',#22181,#5450);
#4591=LINE('',#22184,#5451);
#4592=LINE('',#22186,#5452);
#4593=LINE('',#22189,#5453);
#4594=LINE('',#22194,#5454);
#4595=LINE('',#22198,#5455);
#4596=LINE('',#22204,#5456);
#4597=LINE('',#22208,#5457);
#4598=LINE('',#22214,#5458);
#4599=LINE('',#22218,#5459);
#4600=LINE('',#22224,#5460);
#4601=LINE('',#22228,#5461);
#4602=LINE('',#22232,#5462);
#4603=LINE('',#22233,#5463);
#4604=LINE('',#22235,#5464);
#4605=LINE('',#22238,#5465);
#4606=LINE('',#22239,#5466);
#4607=LINE('',#22242,#5467);
#4608=LINE('',#22243,#5468);
#4609=LINE('',#22245,#5469);
#4610=LINE('',#22250,#5470);
#4611=LINE('',#22252,#5471);
#4612=LINE('',#22254,#5472);
#4613=LINE('',#22256,#5473);
#4614=LINE('',#22258,#5474);
#4615=LINE('',#22264,#5475);
#4616=LINE('',#22266,#5476);
#4617=LINE('',#22267,#5477);
#4618=LINE('',#22270,#5478);
#4619=LINE('',#22271,#5479);
#4620=LINE('',#22273,#5480);
#4621=LINE('',#22275,#5481);
#4622=LINE('',#22276,#5482);
#4623=LINE('',#22280,#5483);
#4624=LINE('',#22282,#5484);
#4625=LINE('',#22284,#5485);
#4626=LINE('',#22285,#5486);
#4627=LINE('',#22286,#5487);
#4628=LINE('',#22288,#5488);
#4629=LINE('',#22289,#5489);
#4630=LINE('',#22294,#5490);
#4631=LINE('',#22298,#5491);
#4632=LINE('',#22304,#5492);
#4633=LINE('',#22306,#5493);
#4634=LINE('',#22308,#5494);
#4635=LINE('',#22310,#5495);
#4636=LINE('',#22312,#5496);
#4637=LINE('',#22316,#5497);
#4638=LINE('',#22317,#5498);
#4639=LINE('',#22319,#5499);
#4640=LINE('',#22320,#5500);
#4641=LINE('',#22323,#5501);
#4642=LINE('',#22325,#5502);
#4643=LINE('',#22328,#5503);
#4644=LINE('',#22330,#5504);
#4645=LINE('',#22331,#5505);
#4646=LINE('',#22334,#5506);
#4647=LINE('',#22335,#5507);
#4648=LINE('',#22338,#5508);
#4649=LINE('',#22339,#5509);
#4650=LINE('',#22341,#5510);
#4651=LINE('',#22345,#5511);
#4652=LINE('',#22347,#5512);
#4653=LINE('',#22348,#5513);
#4654=LINE('',#22351,#5514);
#4655=LINE('',#22352,#5515);
#4656=LINE('',#22355,#5516);
#4657=LINE('',#22356,#5517);
#4658=LINE('',#22358,#5518);
#4659=LINE('',#22362,#5519);
#4660=LINE('',#22364,#5520);
#4661=LINE('',#22365,#5521);
#4662=LINE('',#22368,#5522);
#4663=LINE('',#22369,#5523);
#4664=LINE('',#22372,#5524);
#4665=LINE('',#22373,#5525);
#4666=LINE('',#22375,#5526);
#4667=LINE('',#22379,#5527);
#4668=LINE('',#22381,#5528);
#4669=LINE('',#22382,#5529);
#4670=LINE('',#22385,#5530);
#4671=LINE('',#22386,#5531);
#4672=LINE('',#22389,#5532);
#4673=LINE('',#22390,#5533);
#4674=LINE('',#22392,#5534);
#4675=LINE('',#22396,#5535);
#4676=LINE('',#22398,#5536);
#4677=LINE('',#22399,#5537);
#4678=LINE('',#22402,#5538);
#4679=LINE('',#22403,#5539);
#4680=LINE('',#22406,#5540);
#4681=LINE('',#22407,#5541);
#4682=LINE('',#22409,#5542);
#4683=LINE('',#22413,#5543);
#4684=LINE('',#22415,#5544);
#4685=LINE('',#22416,#5545);
#4686=LINE('',#22419,#5546);
#4687=LINE('',#22420,#5547);
#4688=LINE('',#22423,#5548);
#4689=LINE('',#22424,#5549);
#4690=LINE('',#22426,#5550);
#4691=LINE('',#22430,#5551);
#4692=LINE('',#22437,#5552);
#4693=LINE('',#22444,#5553);
#4694=LINE('',#22451,#5554);
#4695=LINE('',#22491,#5555);
#4696=LINE('',#22533,#5556);
#4697=LINE('',#22540,#5557);
#4698=LINE('',#22546,#5558);
#4699=LINE('',#22549,#5559);
#4700=LINE('',#22556,#5560);
#4701=LINE('',#22563,#5561);
#4702=LINE('',#22566,#5562);
#4703=LINE('',#22575,#5563);
#4704=LINE('',#22579,#5564);
#4705=LINE('',#22658,#5565);
#4706=LINE('',#22661,#5566);
#4707=LINE('',#22664,#5567);
#4708=LINE('',#22668,#5568);
#4709=LINE('',#22672,#5569);
#4710=LINE('',#22689,#5570);
#4711=LINE('',#22693,#5571);
#4712=LINE('',#22697,#5572);
#4713=LINE('',#22703,#5573);
#4714=LINE('',#22708,#5574);
#4715=LINE('',#22712,#5575);
#4716=LINE('',#22716,#5576);
#4717=LINE('',#22722,#5577);
#4718=LINE('',#22727,#5578);
#4719=LINE('',#22731,#5579);
#4720=LINE('',#22735,#5580);
#4721=LINE('',#22741,#5581);
#4722=LINE('',#22746,#5582);
#4723=LINE('',#22750,#5583);
#4724=LINE('',#22754,#5584);
#4725=LINE('',#22760,#5585);
#4726=LINE('',#22764,#5586);
#4727=LINE('',#22767,#5587);
#4728=LINE('',#22773,#5588);
#4729=LINE('',#22776,#5589);
#4730=LINE('',#22780,#5590);
#4731=LINE('',#22784,#5591);
#4732=LINE('',#22793,#5592);
#4733=LINE('',#22795,#5593);
#4734=LINE('',#22797,#5594);
#4735=LINE('',#22798,#5595);
#4736=LINE('',#22801,#5596);
#4737=LINE('',#22803,#5597);
#4738=LINE('',#22804,#5598);
#4739=LINE('',#22807,#5599);
#4740=LINE('',#22809,#5600);
#4741=LINE('',#22810,#5601);
#4742=LINE('',#22813,#5602);
#4743=LINE('',#22815,#5603);
#4744=LINE('',#22816,#5604);
#4745=LINE('',#22819,#5605);
#4746=LINE('',#22821,#5606);
#4747=LINE('',#22822,#5607);
#4748=LINE('',#22825,#5608);
#4749=LINE('',#22827,#5609);
#4750=LINE('',#22828,#5610);
#4751=LINE('',#22831,#5611);
#4752=LINE('',#22833,#5612);
#4753=LINE('',#22834,#5613);
#4754=LINE('',#22836,#5614);
#4755=LINE('',#22837,#5615);
#4756=LINE('',#22840,#5616);
#4757=LINE('',#22842,#5617);
#4758=LINE('',#22843,#5618);
#4759=LINE('',#22846,#5619);
#4760=LINE('',#22847,#5620);
#4761=LINE('',#22850,#5621);
#4762=LINE('',#22851,#5622);
#4763=LINE('',#22854,#5623);
#4764=LINE('',#22855,#5624);
#4765=LINE('',#22861,#5625);
#4766=LINE('',#22863,#5626);
#4767=LINE('',#22865,#5627);
#4768=LINE('',#22866,#5628);
#4769=LINE('',#22869,#5629);
#4770=LINE('',#22871,#5630);
#4771=LINE('',#22873,#5631);
#4772=LINE('',#22874,#5632);
#4773=LINE('',#22877,#5633);
#4774=LINE('',#22879,#5634);
#4775=LINE('',#22881,#5635);
#4776=LINE('',#22882,#5636);
#4777=LINE('',#22885,#5637);
#4778=LINE('',#22887,#5638);
#4779=LINE('',#22889,#5639);
#4780=LINE('',#22890,#5640);
#4781=LINE('',#22903,#5641);
#4782=LINE('',#22907,#5642);
#4783=LINE('',#22911,#5643);
#4784=LINE('',#22918,#5644);
#4785=LINE('',#22924,#5645);
#4786=LINE('',#22928,#5646);
#4787=LINE('',#22932,#5647);
#4788=LINE('',#22939,#5648);
#4789=LINE('',#22945,#5649);
#4790=LINE('',#22949,#5650);
#4791=LINE('',#22953,#5651);
#4792=LINE('',#22960,#5652);
#4793=LINE('',#22966,#5653);
#4794=LINE('',#22970,#5654);
#4795=LINE('',#22974,#5655);
#4796=LINE('',#22981,#5656);
#4797=LINE('',#22987,#5657);
#4798=LINE('',#22991,#5658);
#4799=LINE('',#22994,#5659);
#4800=LINE('',#22999,#5660);
#4801=LINE('',#23003,#5661);
#4802=LINE('',#23006,#5662);
#4803=LINE('',#23011,#5663);
#4804=LINE('',#23015,#5664);
#4805=LINE('',#23018,#5665);
#4806=LINE('',#23023,#5666);
#4807=LINE('',#23027,#5667);
#4808=LINE('',#23030,#5668);
#4809=LINE('',#23034,#5669);
#4810=LINE('',#23035,#5670);
#4811=LINE('',#23036,#5671);
#4812=LINE('',#23039,#5672);
#4813=LINE('',#23040,#5673);
#4814=LINE('',#23043,#5674);
#4815=LINE('',#23044,#5675);
#4816=LINE('',#23046,#5676);
#4817=LINE('',#23050,#5677);
#4818=LINE('',#23051,#5678);
#4819=LINE('',#23052,#5679);
#4820=LINE('',#23055,#5680);
#4821=LINE('',#23056,#5681);
#4822=LINE('',#23059,#5682);
#4823=LINE('',#23060,#5683);
#4824=LINE('',#23062,#5684);
#4825=LINE('',#23066,#5685);
#4826=LINE('',#23067,#5686);
#4827=LINE('',#23068,#5687);
#4828=LINE('',#23071,#5688);
#4829=LINE('',#23072,#5689);
#4830=LINE('',#23075,#5690);
#4831=LINE('',#23076,#5691);
#4832=LINE('',#23078,#5692);
#4833=LINE('',#23082,#5693);
#4834=LINE('',#23083,#5694);
#4835=LINE('',#23084,#5695);
#4836=LINE('',#23087,#5696);
#4837=LINE('',#23088,#5697);
#4838=LINE('',#23091,#5698);
#4839=LINE('',#23092,#5699);
#4840=LINE('',#23094,#5700);
#4841=LINE('',#23099,#5701);
#4842=LINE('',#23103,#5702);
#4843=LINE('',#23108,#5703);
#4844=LINE('',#23109,#5704);
#4845=LINE('',#23112,#5705);
#4846=LINE('',#23113,#5706);
#4847=LINE('',#23116,#5707);
#4848=LINE('',#23117,#5708);
#4849=LINE('',#23119,#5709);
#4850=LINE('',#23125,#5710);
#4851=LINE('',#23192,#5711);
#4852=LINE('',#23202,#5712);
#4853=LINE('',#23322,#5713);
#4854=LINE('',#23452,#5714);
#4855=LINE('',#23592,#5715);
#4856=LINE('',#23722,#5716);
#4857=LINE('',#23906,#5717);
#4858=LINE('',#23936,#5718);
#4859=LINE('',#23938,#5719);
#4860=LINE('',#23940,#5720);
#4861=LINE('',#23942,#5721);
#4862=LINE('',#23950,#5722);
#4863=LINE('',#23951,#5723);
#4864=LINE('',#23955,#5724);
#4865=LINE('',#23960,#5725);
#4866=LINE('',#23961,#5726);
#4867=LINE('',#23963,#5727);
#4868=LINE('',#23968,#5728);
#4869=LINE('',#23975,#5729);
#4870=LINE('',#23980,#5730);
#4871=LINE('',#24011,#5731);
#4872=LINE('',#24204,#5732);
#4873=LINE('',#24267,#5733);
#4874=LINE('',#24269,#5734);
#4875=LINE('',#24273,#5735);
#4876=LINE('',#26136,#5736);
#4877=LINE('',#26762,#5737);
#4878=LINE('',#26770,#5738);
#4879=LINE('',#26774,#5739);
#4880=LINE('',#26781,#5740);
#4881=LINE('',#26785,#5741);
#4882=LINE('',#26793,#5742);
#4883=LINE('',#26796,#5743);
#4884=LINE('',#26804,#5744);
#4885=LINE('',#26807,#5745);
#4886=LINE('',#26816,#5746);
#4887=LINE('',#26821,#5747);
#4888=LINE('',#26870,#5748);
#4889=LINE('',#26913,#5749);
#4890=LINE('',#26958,#5750);
#4891=LINE('',#27004,#5751);
#4892=LINE('',#27047,#5752);
#4893=LINE('',#27090,#5753);
#4894=LINE('',#27132,#5754);
#4895=LINE('',#27173,#5755);
#4896=LINE('',#27215,#5756);
#4897=LINE('',#27258,#5757);
#4898=LINE('',#27296,#5758);
#4899=LINE('',#27333,#5759);
#4900=LINE('',#27374,#5760);
#4901=LINE('',#27410,#5761);
#4902=LINE('',#27450,#5762);
#4903=LINE('',#27487,#5763);
#4904=LINE('',#27526,#5764);
#4905=LINE('',#27587,#5765);
#4906=LINE('',#27625,#5766);
#4907=LINE('',#27661,#5767);
#4908=LINE('',#27703,#5768);
#4909=LINE('',#27737,#5769);
#4910=LINE('',#27780,#5770);
#4911=LINE('',#27827,#5771);
#4912=LINE('',#27870,#5772);
#4913=LINE('',#27913,#5773);
#4914=LINE('',#27958,#5774);
#4915=LINE('',#27996,#5775);
#4916=LINE('',#28042,#5776);
#4917=LINE('',#28111,#5777);
#4918=LINE('',#28114,#5778);
#4919=LINE('',#28128,#5779);
#4920=LINE('',#28170,#5780);
#4921=LINE('',#28252,#5781);
#4922=LINE('',#28279,#5782);
#4923=LINE('',#28358,#5783);
#4924=LINE('',#28389,#5784);
#4925=LINE('',#28420,#5785);
#4926=LINE('',#28495,#5786);
#4927=LINE('',#28538,#5787);
#4928=LINE('',#28581,#5788);
#4929=LINE('',#28612,#5789);
#4930=LINE('',#28639,#5790);
#4931=LINE('',#28668,#5791);
#4932=LINE('',#28697,#5792);
#4933=LINE('',#28726,#5793);
#4934=LINE('',#28785,#5794);
#4935=LINE('',#28819,#5795);
#4936=LINE('',#28845,#5796);
#4937=LINE('',#28918,#5797);
#4938=LINE('',#28979,#5798);
#4939=LINE('',#29008,#5799);
#4940=LINE('',#29040,#5800);
#4941=LINE('',#29071,#5801);
#4942=LINE('',#29100,#5802);
#4943=LINE('',#29172,#5803);
#4944=LINE('',#29245,#5804);
#4945=LINE('',#29277,#5805);
#4946=LINE('',#29312,#5806);
#4947=LINE('',#29391,#5807);
#4948=LINE('',#29424,#5808);
#4949=LINE('',#63086,#5809);
#4950=LINE('',#63088,#5810);
#4951=LINE('',#63090,#5811);
#4952=LINE('',#63096,#5812);
#4953=LINE('',#63102,#5813);
#4954=LINE('',#63104,#5814);
#4955=LINE('',#63105,#5815);
#4956=LINE('',#63108,#5816);
#4957=LINE('',#63114,#5817);
#4958=LINE('',#63119,#5818);
#4959=LINE('',#63129,#5819);
#4960=LINE('',#63133,#5820);
#4961=LINE('',#63140,#5821);
#4962=LINE('',#63144,#5822);
#4963=LINE('',#63151,#5823);
#4964=LINE('',#63158,#5824);
#4965=LINE('',#63161,#5825);
#4966=LINE('',#63169,#5826);
#4967=LINE('',#63172,#5827);
#4968=LINE('',#63188,#5828);
#4969=LINE('',#63192,#5829);
#4970=LINE('',#63195,#5830);
#4971=LINE('',#63203,#5831);
#4972=LINE('',#63210,#5832);
#4973=LINE('',#63214,#5833);
#4974=LINE('',#63217,#5834);
#4975=LINE('',#63220,#5835);
#4976=LINE('',#63226,#5836);
#4977=LINE('',#63233,#5837);
#4978=LINE('',#63242,#5838);
#4979=LINE('',#63250,#5839);
#4980=LINE('',#63252,#5840);
#4981=LINE('',#63259,#5841);
#4982=LINE('',#63400,#5842);
#4983=LINE('',#63677,#5843);
#4984=LINE('',#63957,#5844);
#4985=LINE('',#64234,#5845);
#4986=LINE('',#64514,#5846);
#4987=LINE('',#66246,#5847);
#4988=LINE('',#66250,#5848);
#4989=LINE('',#66252,#5849);
#4990=LINE('',#66253,#5850);
#4991=LINE('',#66256,#5851);
#4992=LINE('',#66257,#5852);
#4993=LINE('',#66260,#5853);
#4994=LINE('',#66261,#5854);
#4995=LINE('',#66265,#5855);
#4996=LINE('',#66269,#5856);
#4997=LINE('',#66270,#5857);
#4998=LINE('',#66273,#5858);
#4999=LINE('',#66274,#5859);
#5000=LINE('',#66276,#5860);
#5001=LINE('',#66282,#5861);
#5002=LINE('',#66290,#5862);
#5003=LINE('',#66297,#5863);
#5004=LINE('',#66301,#5864);
#5005=LINE('',#66304,#5865);
#5006=LINE('',#66312,#5866);
#5007=LINE('',#66320,#5867);
#5008=LINE('',#66324,#5868);
#5009=LINE('',#66327,#5869);
#5010=LINE('',#66335,#5870);
#5011=LINE('',#66337,#5871);
#5012=LINE('',#66343,#5872);
#5013=LINE('',#66351,#5873);
#5014=LINE('',#66355,#5874);
#5015=LINE('',#66362,#5875);
#5016=LINE('',#66366,#5876);
#5017=LINE('',#66369,#5877);
#5018=LINE('',#66378,#5878);
#5019=LINE('',#66384,#5879);
#5020=LINE('',#66391,#5880);
#5021=LINE('',#66398,#5881);
#5022=LINE('',#66410,#5882);
#5023=LINE('',#66414,#5883);
#5024=LINE('',#66421,#5884);
#5025=LINE('',#66425,#5885);
#5026=LINE('',#66431,#5886);
#5027=LINE('',#66435,#5887);
#5028=LINE('',#66438,#5888);
#5029=LINE('',#66444,#5889);
#5030=LINE('',#66449,#5890);
#5031=LINE('',#66455,#5891);
#5032=LINE('',#66459,#5892);
#5033=LINE('',#66467,#5893);
#5034=LINE('',#66474,#5894);
#5035=LINE('',#66481,#5895);
#5036=LINE('',#66485,#5896);
#5037=LINE('',#66488,#5897);
#5038=LINE('',#66496,#5898);
#5039=LINE('',#66503,#5899);
#5040=LINE('',#66508,#5900);
#5041=LINE('',#66518,#5901);
#5042=LINE('',#66522,#5902);
#5043=LINE('',#66525,#5903);
#5044=LINE('',#66533,#5904);
#5045=LINE('',#66540,#5905);
#5046=LINE('',#66544,#5906);
#5047=LINE('',#66547,#5907);
#5048=LINE('',#66550,#5908);
#5049=LINE('',#66556,#5909);
#5050=LINE('',#66560,#5910);
#5051=LINE('',#66565,#5911);
#5052=LINE('',#66569,#5912);
#5053=LINE('',#66583,#5913);
#5054=LINE('',#66588,#5914);
#5055=LINE('',#66600,#5915);
#5056=LINE('',#66607,#5916);
#5057=LINE('',#66610,#5917);
#5058=LINE('',#66613,#5918);
#5059=LINE('',#66615,#5919);
#5060=LINE('',#66616,#5920);
#5061=LINE('',#66618,#5921);
#5062=LINE('',#66619,#5922);
#5063=LINE('',#66621,#5923);
#5064=LINE('',#66623,#5924);
#5065=LINE('',#66625,#5925);
#5066=LINE('',#66627,#5926);
#5067=LINE('',#66634,#5927);
#5068=LINE('',#66766,#5928);
#5069=LINE('',#67166,#5929);
#5070=LINE('',#67596,#5930);
#5071=LINE('',#68112,#5931);
#5072=LINE('',#68548,#5932);
#5073=LINE('',#69040,#5933);
#5074=LINE('',#69468,#5934);
#5075=LINE('',#69976,#5935);
#5076=LINE('',#70404,#5936);
#5077=LINE('',#70862,#5937);
#5078=LINE('',#71292,#5938);
#5079=LINE('',#71565,#5939);
#5080=LINE('',#71886,#5940);
#5081=LINE('',#71994,#5941);
#5082=LINE('',#72355,#5942);
#5083=LINE('',#72777,#5943);
#5084=LINE('',#72905,#5944);
#5085=LINE('',#73170,#5945);
#5086=LINE('',#77396,#5946);
#5087=LINE('',#77400,#5947);
#5088=LINE('',#77402,#5948);
#5089=LINE('',#77403,#5949);
#5090=LINE('',#77406,#5950);
#5091=LINE('',#77407,#5951);
#5092=LINE('',#77410,#5952);
#5093=LINE('',#77411,#5953);
#5094=LINE('',#77415,#5954);
#5095=LINE('',#77419,#5955);
#5096=LINE('',#77420,#5956);
#5097=LINE('',#77423,#5957);
#5098=LINE('',#77424,#5958);
#5099=LINE('',#77426,#5959);
#5100=LINE('',#77436,#5960);
#5101=LINE('',#77443,#5961);
#5102=LINE('',#77445,#5962);
#5103=LINE('',#77450,#5963);
#5104=LINE('',#77582,#5964);
#5105=LINE('',#77811,#5965);
#5106=LINE('',#78183,#5966);
#5107=LINE('',#78594,#5967);
#5108=LINE('',#79043,#5968);
#5109=LINE('',#79450,#5969);
#5110=LINE('',#79779,#5970);
#5111=LINE('',#80054,#5971);
#5112=LINE('',#80417,#5972);
#5113=LINE('',#80824,#5973);
#5114=LINE('',#81239,#5974);
#5115=LINE('',#81638,#5975);
#5116=LINE('',#82035,#5976);
#5117=LINE('',#82440,#5977);
#5118=LINE('',#86276,#5978);
#5119=LINE('',#86280,#5979);
#5120=LINE('',#86282,#5980);
#5121=LINE('',#86283,#5981);
#5122=LINE('',#86286,#5982);
#5123=LINE('',#86287,#5983);
#5124=LINE('',#86290,#5984);
#5125=LINE('',#86291,#5985);
#5126=LINE('',#86295,#5986);
#5127=LINE('',#86299,#5987);
#5128=LINE('',#86300,#5988);
#5129=LINE('',#86303,#5989);
#5130=LINE('',#86304,#5990);
#5131=LINE('',#86306,#5991);
#5132=LINE('',#86316,#5992);
#5133=LINE('',#86323,#5993);
#5134=LINE('',#86325,#5994);
#5135=LINE('',#86331,#5995);
#5136=LINE('',#86339,#5996);
#5137=LINE('',#86343,#5997);
#5138=LINE('',#86350,#5998);
#5139=LINE('',#86354,#5999);
#5140=LINE('',#86357,#6000);
#5141=VECTOR('',#17292,1.);
#5142=VECTOR('',#17293,1.);
#5143=VECTOR('',#17294,1.);
#5144=VECTOR('',#17295,1.);
#5145=VECTOR('',#17298,1.);
#5146=VECTOR('',#17299,1.);
#5147=VECTOR('',#17300,1.);
#5148=VECTOR('',#17303,1.);
#5149=VECTOR('',#17304,1.);
#5150=VECTOR('',#17305,1.);
#5151=VECTOR('',#17308,1.);
#5152=VECTOR('',#17309,1.);
#5153=VECTOR('',#17314,1.);
#5154=VECTOR('',#17315,1.);
#5155=VECTOR('',#17316,1.);
#5156=VECTOR('',#17317,1.);
#5157=VECTOR('',#17320,1.);
#5158=VECTOR('',#17321,1.);
#5159=VECTOR('',#17322,1.);
#5160=VECTOR('',#17323,1.);
#5161=VECTOR('',#17324,1.);
#5162=VECTOR('',#17327,1.);
#5163=VECTOR('',#17328,1.);
#5164=VECTOR('',#17331,1.);
#5165=VECTOR('',#17332,1.);
#5166=VECTOR('',#17335,1.);
#5167=VECTOR('',#17336,1.);
#5168=VECTOR('',#17339,1.);
#5169=VECTOR('',#17340,1.);
#5170=VECTOR('',#17341,1.);
#5171=VECTOR('',#17342,1.);
#5172=VECTOR('',#17345,1.);
#5173=VECTOR('',#17346,1.);
#5174=VECTOR('',#17347,1.);
#5175=VECTOR('',#17350,1.);
#5176=VECTOR('',#17351,1.);
#5177=VECTOR('',#17352,1.);
#5178=VECTOR('',#17355,1.);
#5179=VECTOR('',#17356,1.);
#5180=VECTOR('',#17361,1.);
#5181=VECTOR('',#17362,1.);
#5182=VECTOR('',#17363,1.);
#5183=VECTOR('',#17364,1.);
#5184=VECTOR('',#17367,1.);
#5185=VECTOR('',#17368,1.);
#5186=VECTOR('',#17369,1.);
#5187=VECTOR('',#17372,1.);
#5188=VECTOR('',#17373,1.);
#5189=VECTOR('',#17374,1.);
#5190=VECTOR('',#17377,1.);
#5191=VECTOR('',#17378,1.);
#5192=VECTOR('',#17383,1.);
#5193=VECTOR('',#17384,1.);
#5194=VECTOR('',#17385,1.);
#5195=VECTOR('',#17386,1.);
#5196=VECTOR('',#17389,1.);
#5197=VECTOR('',#17390,1.);
#5198=VECTOR('',#17391,1.);
#5199=VECTOR('',#17394,1.);
#5200=VECTOR('',#17395,1.);
#5201=VECTOR('',#17396,1.);
#5202=VECTOR('',#17399,1.);
#5203=VECTOR('',#17400,1.);
#5204=VECTOR('',#17405,1.);
#5205=VECTOR('',#17406,1.);
#5206=VECTOR('',#17407,1.);
#5207=VECTOR('',#17408,1.);
#5208=VECTOR('',#17411,1.);
#5209=VECTOR('',#17412,1.);
#5210=VECTOR('',#17413,1.);
#5211=VECTOR('',#17414,1.);
#5212=VECTOR('',#17417,1.);
#5213=VECTOR('',#17418,1.);
#5214=VECTOR('',#17419,1.);
#5215=VECTOR('',#17422,1.);
#5216=VECTOR('',#17423,1.);
#5217=VECTOR('',#17426,1.);
#5218=VECTOR('',#17427,1.);
#5219=VECTOR('',#17430,1.);
#5220=VECTOR('',#17431,1.);
#5221=VECTOR('',#17432,1.);
#5222=VECTOR('',#17433,1.);
#5223=VECTOR('',#17436,1.);
#5224=VECTOR('',#17437,1.);
#5225=VECTOR('',#17438,1.);
#5226=VECTOR('',#17441,1.);
#5227=VECTOR('',#17442,1.);
#5228=VECTOR('',#17443,1.);
#5229=VECTOR('',#17444,1.);
#5230=VECTOR('',#17445,1.);
#5231=VECTOR('',#17446,1.);
#5232=VECTOR('',#17447,1.);
#5233=VECTOR('',#17448,1.);
#5234=VECTOR('',#17449,1.);
#5235=VECTOR('',#17450,1.);
#5236=VECTOR('',#17455,1.);
#5237=VECTOR('',#17456,1.);
#5238=VECTOR('',#17457,1.);
#5239=VECTOR('',#17458,1.);
#5240=VECTOR('',#17461,1.);
#5241=VECTOR('',#17462,1.);
#5242=VECTOR('',#17463,1.);
#5243=VECTOR('',#17466,1.);
#5244=VECTOR('',#17467,1.);
#5245=VECTOR('',#17468,1.);
#5246=VECTOR('',#17471,1.);
#5247=VECTOR('',#17472,1.);
#5248=VECTOR('',#17477,1.);
#5249=VECTOR('',#17478,1.);
#5250=VECTOR('',#17479,1.);
#5251=VECTOR('',#17480,1.);
#5252=VECTOR('',#17483,1.);
#5253=VECTOR('',#17484,1.);
#5254=VECTOR('',#17485,1.);
#5255=VECTOR('',#17486,1.);
#5256=VECTOR('',#17489,1.);
#5257=VECTOR('',#17490,1.);
#5258=VECTOR('',#17493,1.);
#5259=VECTOR('',#17494,1.);
#5260=VECTOR('',#17495,1.);
#5261=VECTOR('',#17498,1.);
#5262=VECTOR('',#17499,1.);
#5263=VECTOR('',#17502,1.);
#5264=VECTOR('',#17503,1.);
#5265=VECTOR('',#17504,1.);
#5266=VECTOR('',#17505,1.);
#5267=VECTOR('',#17508,1.);
#5268=VECTOR('',#17509,1.);
#5269=VECTOR('',#17510,1.);
#5270=VECTOR('',#17513,1.);
#5271=VECTOR('',#17514,1.);
#5272=VECTOR('',#17515,1.);
#5273=VECTOR('',#17518,1.);
#5274=VECTOR('',#17519,1.);
#5275=VECTOR('',#17524,1.);
#5276=VECTOR('',#17525,1.);
#5277=VECTOR('',#17526,1.);
#5278=VECTOR('',#17527,1.);
#5279=VECTOR('',#17530,1.);
#5280=VECTOR('',#17531,1.);
#5281=VECTOR('',#17532,1.);
#5282=VECTOR('',#17535,1.);
#5283=VECTOR('',#17536,1.);
#5284=VECTOR('',#17537,1.);
#5285=VECTOR('',#17540,1.);
#5286=VECTOR('',#17541,1.);
#5287=VECTOR('',#17546,1.);
#5288=VECTOR('',#17547,1.);
#5289=VECTOR('',#17548,1.);
#5290=VECTOR('',#17549,1.);
#5291=VECTOR('',#17552,1.);
#5292=VECTOR('',#17553,1.);
#5293=VECTOR('',#17554,1.);
#5294=VECTOR('',#17557,1.);
#5295=VECTOR('',#17558,1.);
#5296=VECTOR('',#17559,1.);
#5297=VECTOR('',#17562,1.);
#5298=VECTOR('',#17563,1.);
#5299=VECTOR('',#17568,1.);
#5300=VECTOR('',#17569,1.);
#5301=VECTOR('',#17570,1.);
#5302=VECTOR('',#17571,1.);
#5303=VECTOR('',#17574,1.);
#5304=VECTOR('',#17575,1.);
#5305=VECTOR('',#17576,1.);
#5306=VECTOR('',#17579,1.);
#5307=VECTOR('',#17580,1.);
#5308=VECTOR('',#17581,1.);
#5309=VECTOR('',#17582,1.);
#5310=VECTOR('',#17585,1.);
#5311=VECTOR('',#17586,1.);
#5312=VECTOR('',#17589,1.);
#5313=VECTOR('',#17590,1.);
#5314=VECTOR('',#17593,1.);
#5315=VECTOR('',#17594,1.);
#5316=VECTOR('',#17595,1.);
#5317=VECTOR('',#17596,1.);
#5318=VECTOR('',#17599,1.);
#5319=VECTOR('',#17600,1.);
#5320=VECTOR('',#17601,1.);
#5321=VECTOR('',#17602,1.);
#5322=VECTOR('',#17605,1.);
#5323=VECTOR('',#17606,1.);
#5324=VECTOR('',#17607,1.);
#5325=VECTOR('',#17612,1.);
#5326=VECTOR('',#17617,1.);
#5327=VECTOR('',#17618,1.);
#5328=VECTOR('',#17619,1.);
#5329=VECTOR('',#17620,1.);
#5330=VECTOR('',#17621,1.);
#5331=VECTOR('',#17622,1.);
#5332=VECTOR('',#17623,1.);
#5333=VECTOR('',#17624,1.);
#5334=VECTOR('',#17635,1.);
#5335=VECTOR('',#17638,1.);
#5336=VECTOR('',#17643,1.);
#5337=VECTOR('',#17648,1.);
#5338=VECTOR('',#17649,1.);
#5339=VECTOR('',#17650,1.);
#5340=VECTOR('',#17653,1.);
#5341=VECTOR('',#17654,1.);
#5342=VECTOR('',#17655,1.);
#5343=VECTOR('',#17658,1.);
#5344=VECTOR('',#17659,1.);
#5345=VECTOR('',#17660,1.);
#5346=VECTOR('',#17671,1.);
#5347=VECTOR('',#17672,1.);
#5348=VECTOR('',#17673,1.);
#5349=VECTOR('',#17674,1.);
#5350=VECTOR('',#17677,1.);
#5351=VECTOR('',#17678,1.);
#5352=VECTOR('',#17679,1.);
#5353=VECTOR('',#17682,1.);
#5354=VECTOR('',#17683,1.);
#5355=VECTOR('',#17684,1.);
#5356=VECTOR('',#17701,1.);
#5357=VECTOR('',#17704,1.);
#5358=VECTOR('',#17707,1.);
#5359=VECTOR('',#17708,1.);
#5360=VECTOR('',#17731,1.);
#5361=VECTOR('',#17734,1.);
#5362=VECTOR('',#17757,1.);
#5363=VECTOR('',#17760,1.);
#5364=VECTOR('',#17793,1.);
#5365=VECTOR('',#17794,1.);
#5366=VECTOR('',#17797,1.);
#5367=VECTOR('',#17800,1.);
#5368=VECTOR('',#17803,1.);
#5369=VECTOR('',#17806,1.);
#5370=VECTOR('',#17809,1.);
#5371=VECTOR('',#17824,0.505);
#5372=VECTOR('',#17829,0.5575);
#5373=VECTOR('',#17834,0.2025);
#5374=VECTOR('',#17839,0.405);
#5375=VECTOR('',#17840,0.405);
#5376=VECTOR('',#17845,0.455);
#5377=VECTOR('',#17852,1.);
#5378=VECTOR('',#17853,1.);
#5379=VECTOR('',#17854,1.);
#5380=VECTOR('',#17859,1.);
#5381=VECTOR('',#17864,1.);
#5382=VECTOR('',#17865,1.);
#5383=VECTOR('',#17870,1.);
#5384=VECTOR('',#17871,1.);
#5385=VECTOR('',#17872,1.);
#5386=VECTOR('',#17873,1.);
#5387=VECTOR('',#17874,1.);
#5388=VECTOR('',#17875,1.);
#5389=VECTOR('',#17876,1.);
#5390=VECTOR('',#17877,1.);
#5391=VECTOR('',#17878,1.);
#5392=VECTOR('',#17879,1.);
#5393=VECTOR('',#17880,1.);
#5394=VECTOR('',#17881,1.);
#5395=VECTOR('',#17882,1.);
#5396=VECTOR('',#17883,1.);
#5397=VECTOR('',#17884,1.);
#5398=VECTOR('',#17885,1.);
#5399=VECTOR('',#17886,1.);
#5400=VECTOR('',#17887,1.);
#5401=VECTOR('',#17888,1.);
#5402=VECTOR('',#17889,1.);
#5403=VECTOR('',#17890,1.);
#5404=VECTOR('',#17891,1.);
#5405=VECTOR('',#17892,1.);
#5406=VECTOR('',#17893,1.);
#5407=VECTOR('',#17894,1.);
#5408=VECTOR('',#17897,0.2025);
#5409=VECTOR('',#17902,0.405);
#5410=VECTOR('',#17907,0.455000000000001);
#5411=VECTOR('',#17914,0.2025);
#5412=VECTOR('',#17919,0.405);
#5413=VECTOR('',#17924,0.455);
#5414=VECTOR('',#17931,0.2025);
#5415=VECTOR('',#17936,0.405);
#5416=VECTOR('',#17941,0.455000000000001);
#5417=VECTOR('',#17944,0.1525);
#5418=VECTOR('',#17949,0.305);
#5419=VECTOR('',#17954,0.355);
#5420=VECTOR('',#17957,0.1525);
#5421=VECTOR('',#17962,0.305);
#5422=VECTOR('',#17967,0.355);
#5423=VECTOR('',#17972,0.1525);
#5424=VECTOR('',#17977,0.305);
#5425=VECTOR('',#17982,0.355);
#5426=VECTOR('',#17985,0.1525);
#5427=VECTOR('',#17990,0.305);
#5428=VECTOR('',#17995,0.355);
#5429=VECTOR('',#18000,0.1525);
#5430=VECTOR('',#18005,0.305);
#5431=VECTOR('',#18010,0.355);
#5432=VECTOR('',#18013,0.1525);
#5433=VECTOR('',#18018,0.305);
#5434=VECTOR('',#18023,0.355);
#5435=VECTOR('',#18028,0.1525);
#5436=VECTOR('',#18033,0.305);
#5437=VECTOR('',#18038,0.355);
#5438=VECTOR('',#18041,0.1525);
#5439=VECTOR('',#18046,0.305);
#5440=VECTOR('',#18051,0.355);
#5441=VECTOR('',#18056,0.1525);
#5442=VECTOR('',#18061,0.305);
#5443=VECTOR('',#18066,0.355);
#5444=VECTOR('',#18069,0.1525);
#5445=VECTOR('',#18074,0.305);
#5446=VECTOR('',#18079,0.355);
#5447=VECTOR('',#18082,0.1525);
#5448=VECTOR('',#18087,0.305);
#5449=VECTOR('',#18092,0.355);
#5450=VECTOR('',#18095,0.1525);
#5451=VECTOR('',#18100,0.305);
#5452=VECTOR('',#18101,0.305);
#5453=VECTOR('',#18106,0.355);
#5454=VECTOR('',#18111,0.425);
#5455=VECTOR('',#18116,0.462499999999999);
#5456=VECTOR('',#18123,0.425000000000001);
#5457=VECTOR('',#18128,0.4625);
#5458=VECTOR('',#18135,0.425);
#5459=VECTOR('',#18140,0.462499999999999);
#5460=VECTOR('',#18147,0.425000000000001);
#5461=VECTOR('',#18152,0.4625);
#5462=VECTOR('',#18157,1.);
#5463=VECTOR('',#18158,1.);
#5464=VECTOR('',#18161,1.);
#5465=VECTOR('',#18164,1.);
#5466=VECTOR('',#18165,1.);
#5467=VECTOR('',#18168,1.);
#5468=VECTOR('',#18169,1.);
#5469=VECTOR('',#18172,1.);
#5470=VECTOR('',#18177,1.);
#5471=VECTOR('',#18178,1.);
#5472=VECTOR('',#18179,1.);
#5473=VECTOR('',#18180,1.);
#5474=VECTOR('',#18181,1.);
#5475=VECTOR('',#18188,1.);
#5476=VECTOR('',#18189,1.);
#5477=VECTOR('',#18190,1.);
#5478=VECTOR('',#18193,1.);
#5479=VECTOR('',#18194,1.);
#5480=VECTOR('',#18197,1.);
#5481=VECTOR('',#18198,1.);
#5482=VECTOR('',#18199,1.);
#5483=VECTOR('',#18204,1.);
#5484=VECTOR('',#18205,1.);
#5485=VECTOR('',#18206,1.);
#5486=VECTOR('',#18207,1.);
#5487=VECTOR('',#18208,1.);
#5488=VECTOR('',#18211,1.);
#5489=VECTOR('',#18212,1.);
#5490=VECTOR('',#18219,1.);
#5491=VECTOR('',#18224,1.);
#5492=VECTOR('',#18231,1.);
#5493=VECTOR('',#18232,1.);
#5494=VECTOR('',#18233,1.);
#5495=VECTOR('',#18234,1.);
#5496=VECTOR('',#18235,1.);
#5497=VECTOR('',#18242,1.);
#5498=VECTOR('',#18243,1.);
#5499=VECTOR('',#18246,1.);
#5500=VECTOR('',#18247,1.);
#5501=VECTOR('',#18252,1.);
#5502=VECTOR('',#18255,1.);
#5503=VECTOR('',#18258,1.);
#5504=VECTOR('',#18259,1.);
#5505=VECTOR('',#18260,1.);
#5506=VECTOR('',#18263,1.);
#5507=VECTOR('',#18264,1.);
#5508=VECTOR('',#18267,1.);
#5509=VECTOR('',#18268,1.);
#5510=VECTOR('',#18271,1.);
#5511=VECTOR('',#18276,1.);
#5512=VECTOR('',#18277,1.);
#5513=VECTOR('',#18278,1.);
#5514=VECTOR('',#18281,1.);
#5515=VECTOR('',#18282,1.);
#5516=VECTOR('',#18285,1.);
#5517=VECTOR('',#18286,1.);
#5518=VECTOR('',#18289,1.);
#5519=VECTOR('',#18294,1.);
#5520=VECTOR('',#18295,1.);
#5521=VECTOR('',#18296,1.);
#5522=VECTOR('',#18299,1.);
#5523=VECTOR('',#18300,1.);
#5524=VECTOR('',#18303,1.);
#5525=VECTOR('',#18304,1.);
#5526=VECTOR('',#18307,1.);
#5527=VECTOR('',#18312,1.);
#5528=VECTOR('',#18313,1.);
#5529=VECTOR('',#18314,1.);
#5530=VECTOR('',#18317,1.);
#5531=VECTOR('',#18318,1.);
#5532=VECTOR('',#18321,1.);
#5533=VECTOR('',#18322,1.);
#5534=VECTOR('',#18325,1.);
#5535=VECTOR('',#18330,1.);
#5536=VECTOR('',#18331,1.);
#5537=VECTOR('',#18332,1.);
#5538=VECTOR('',#18335,1.);
#5539=VECTOR('',#18336,1.);
#5540=VECTOR('',#18339,1.);
#5541=VECTOR('',#18340,1.);
#5542=VECTOR('',#18343,1.);
#5543=VECTOR('',#18348,1.);
#5544=VECTOR('',#18349,1.);
#5545=VECTOR('',#18350,1.);
#5546=VECTOR('',#18353,1.);
#5547=VECTOR('',#18354,1.);
#5548=VECTOR('',#18357,1.);
#5549=VECTOR('',#18358,1.);
#5550=VECTOR('',#18361,1.);
#5551=VECTOR('',#18366,2.6);
#5552=VECTOR('',#18375,2.75);
#5553=VECTOR('',#18384,2.6);
#5554=VECTOR('',#18393,2.3);
#5555=VECTOR('',#18394,2.3);
#5556=VECTOR('',#18403,2.6);
#5557=VECTOR('',#18412,2.75);
#5558=VECTOR('',#18421,2.6);
#5559=VECTOR('',#18424,5.3);
#5560=VECTOR('',#18433,3.75);
#5561=VECTOR('',#18442,3.1);
#5562=VECTOR('',#18447,3.155);
#5563=VECTOR('',#18460,5.245);
#5564=VECTOR('',#18465,5.295);
#5565=VECTOR('',#18522,1.);
#5566=VECTOR('',#18525,1.);
#5567=VECTOR('',#18528,1.);
#5568=VECTOR('',#18533,1.);
#5569=VECTOR('',#18538,1.);
#5570=VECTOR('',#18557,0.342499999999999);
#5571=VECTOR('',#18562,0.33);
#5572=VECTOR('',#18567,0.342499999999999);
#5573=VECTOR('',#18576,0.55);
#5574=VECTOR('',#18581,0.342499999999999);
#5575=VECTOR('',#18586,0.33);
#5576=VECTOR('',#18591,0.342499999999999);
#5577=VECTOR('',#18600,0.55);
#5578=VECTOR('',#18605,0.342499999999999);
#5579=VECTOR('',#18610,0.33);
#5580=VECTOR('',#18615,0.342499999999999);
#5581=VECTOR('',#18624,0.55);
#5582=VECTOR('',#18629,0.342499999999999);
#5583=VECTOR('',#18634,0.33);
#5584=VECTOR('',#18639,0.342499999999999);
#5585=VECTOR('',#18648,0.55);
#5586=VECTOR('',#18653,3.155);
#5587=VECTOR('',#18656,3.1);
#5588=VECTOR('',#18665,3.75);
#5589=VECTOR('',#18668,1.);
#5590=VECTOR('',#18673,1.);
#5591=VECTOR('',#18678,1.);
#5592=VECTOR('',#18691,1.);
#5593=VECTOR('',#18692,1.);
#5594=VECTOR('',#18693,1.);
#5595=VECTOR('',#18694,0.999999999999999);
#5596=VECTOR('',#18697,1.);
#5597=VECTOR('',#18698,1.);
#5598=VECTOR('',#18699,1.);
#5599=VECTOR('',#18702,1.);
#5600=VECTOR('',#18703,1.);
#5601=VECTOR('',#18704,1.);
#5602=VECTOR('',#18707,1.);
#5603=VECTOR('',#18708,0.999999999999999);
#5604=VECTOR('',#18709,1.);
#5605=VECTOR('',#18712,1.);
#5606=VECTOR('',#18713,0.999999999999999);
#5607=VECTOR('',#18714,1.);
#5608=VECTOR('',#18717,1.);
#5609=VECTOR('',#18718,1.);
#5610=VECTOR('',#18719,1.);
#5611=VECTOR('',#18722,1.);
#5612=VECTOR('',#18723,1.);
#5613=VECTOR('',#18724,1.);
#5614=VECTOR('',#18727,1.);
#5615=VECTOR('',#18728,1.);
#5616=VECTOR('',#18731,1.);
#5617=VECTOR('',#18732,1.);
#5618=VECTOR('',#18733,1.);
#5619=VECTOR('',#18736,1.);
#5620=VECTOR('',#18737,1.);
#5621=VECTOR('',#18740,1.);
#5622=VECTOR('',#18741,1.);
#5623=VECTOR('',#18744,1.);
#5624=VECTOR('',#18745,1.);
#5625=VECTOR('',#18750,1.);
#5626=VECTOR('',#18751,1.);
#5627=VECTOR('',#18752,1.);
#5628=VECTOR('',#18753,1.);
#5629=VECTOR('',#18754,1.);
#5630=VECTOR('',#18755,1.);
#5631=VECTOR('',#18756,1.);
#5632=VECTOR('',#18757,1.);
#5633=VECTOR('',#18758,1.);
#5634=VECTOR('',#18759,1.);
#5635=VECTOR('',#18760,1.);
#5636=VECTOR('',#18761,1.);
#5637=VECTOR('',#18762,1.);
#5638=VECTOR('',#18763,1.);
#5639=VECTOR('',#18764,1.);
#5640=VECTOR('',#18765,1.);
#5641=VECTOR('',#18778,0.3425);
#5642=VECTOR('',#18783,0.33);
#5643=VECTOR('',#18788,0.3425);
#5644=VECTOR('',#18797,0.55);
#5645=VECTOR('',#18804,0.3425);
#5646=VECTOR('',#18809,0.33);
#5647=VECTOR('',#18814,0.3425);
#5648=VECTOR('',#18823,0.55);
#5649=VECTOR('',#18830,0.3425);
#5650=VECTOR('',#18835,0.33);
#5651=VECTOR('',#18840,0.3425);
#5652=VECTOR('',#18849,0.55);
#5653=VECTOR('',#18856,0.3425);
#5654=VECTOR('',#18861,0.33);
#5655=VECTOR('',#18866,0.3425);
#5656=VECTOR('',#18875,0.55);
#5657=VECTOR('',#18882,0.49);
#5658=VECTOR('',#18887,0.45);
#5659=VECTOR('',#18892,0.49);
#5660=VECTOR('',#18897,0.49);
#5661=VECTOR('',#18902,0.45);
#5662=VECTOR('',#18907,0.49);
#5663=VECTOR('',#18912,0.49);
#5664=VECTOR('',#18917,0.45);
#5665=VECTOR('',#18922,0.49);
#5666=VECTOR('',#18927,0.49);
#5667=VECTOR('',#18932,0.45);
#5668=VECTOR('',#18937,0.49);
#5669=VECTOR('',#18940,1.);
#5670=VECTOR('',#18941,1.);
#5671=VECTOR('',#18942,1.);
#5672=VECTOR('',#18945,1.);
#5673=VECTOR('',#18946,1.);
#5674=VECTOR('',#18949,1.);
#5675=VECTOR('',#18950,1.);
#5676=VECTOR('',#18953,1.);
#5677=VECTOR('',#18956,1.);
#5678=VECTOR('',#18957,1.);
#5679=VECTOR('',#18958,1.);
#5680=VECTOR('',#18961,1.);
#5681=VECTOR('',#18962,1.);
#5682=VECTOR('',#18965,1.);
#5683=VECTOR('',#18966,1.);
#5684=VECTOR('',#18969,1.);
#5685=VECTOR('',#18972,1.);
#5686=VECTOR('',#18973,1.);
#5687=VECTOR('',#18974,1.);
#5688=VECTOR('',#18977,1.);
#5689=VECTOR('',#18978,1.);
#5690=VECTOR('',#18981,1.);
#5691=VECTOR('',#18982,1.);
#5692=VECTOR('',#18985,1.);
#5693=VECTOR('',#18988,1.);
#5694=VECTOR('',#18989,1.);
#5695=VECTOR('',#18990,1.);
#5696=VECTOR('',#18993,1.);
#5697=VECTOR('',#18994,1.);
#5698=VECTOR('',#18997,1.);
#5699=VECTOR('',#18998,1.);
#5700=VECTOR('',#19001,1.);
#5701=VECTOR('',#19006,2.);
#5702=VECTOR('',#19011,5.501);
#5703=VECTOR('',#19018,1.);
#5704=VECTOR('',#19019,1.);
#5705=VECTOR('',#19022,1.);
#5706=VECTOR('',#19023,1.);
#5707=VECTOR('',#19026,1.);
#5708=VECTOR('',#19027,1.);
#5709=VECTOR('',#19030,1.);
#5710=VECTOR('',#19037,1.4);
#5711=VECTOR('',#19040,1.);
#5712=VECTOR('',#19043,1.4);
#5713=VECTOR('',#19046,1.4);
#5714=VECTOR('',#19049,1.4);
#5715=VECTOR('',#19052,1.4);
#5716=VECTOR('',#19055,1.4);
#5717=VECTOR('',#19060,1.);
#5718=VECTOR('',#19063,1.);
#5719=VECTOR('',#19064,1.);
#5720=VECTOR('',#19065,1.);
#5721=VECTOR('',#19066,1.);
#5722=VECTOR('',#19071,1.);
#5723=VECTOR('',#19072,1.);
#5724=VECTOR('',#19075,1.);
#5725=VECTOR('',#19076,1.);
#5726=VECTOR('',#19077,1.);
#5727=VECTOR('',#19080,1.);
#5728=VECTOR('',#19085,0.699999999999999);
#5729=VECTOR('',#19096,0.35);
#5730=VECTOR('',#19101,1.398);
#5731=VECTOR('',#19106,1.);
#5732=VECTOR('',#19107,1.764);
#5733=VECTOR('',#19110,1.);
#5734=VECTOR('',#19111,1.764);
#5735=VECTOR('',#19116,1.398);
#5736=VECTOR('',#19119,1.);
#5737=VECTOR('',#19122,1.);
#5738=VECTOR('',#19133,1.21);
#5739=VECTOR('',#19138,1.25);
#5740=VECTOR('',#19147,1.525);
#5741=VECTOR('',#19152,1.55);
#5742=VECTOR('',#19163,1.55);
#5743=VECTOR('',#19166,1.525);
#5744=VECTOR('',#19177,1.25);
#5745=VECTOR('',#19180,1.21);
#5746=VECTOR('',#19191,3.325);
#5747=VECTOR('',#19198,3.3);
#5748=VECTOR('',#19207,1.);
#5749=VECTOR('',#19210,1.);
#5750=VECTOR('',#19213,1.);
#5751=VECTOR('',#19216,1.);
#5752=VECTOR('',#19219,1.);
#5753=VECTOR('',#19222,1.);
#5754=VECTOR('',#19225,1.);
#5755=VECTOR('',#19228,1.);
#5756=VECTOR('',#19231,1.);
#5757=VECTOR('',#19234,1.);
#5758=VECTOR('',#19237,1.);
#5759=VECTOR('',#19240,1.);
#5760=VECTOR('',#19243,1.);
#5761=VECTOR('',#19246,1.);
#5762=VECTOR('',#19249,1.);
#5763=VECTOR('',#19252,1.);
#5764=VECTOR('',#19255,1.);
#5765=VECTOR('',#19258,1.);
#5766=VECTOR('',#19261,1.);
#5767=VECTOR('',#19264,1.);
#5768=VECTOR('',#19267,1.);
#5769=VECTOR('',#19270,1.);
#5770=VECTOR('',#19273,1.);
#5771=VECTOR('',#19276,1.);
#5772=VECTOR('',#19279,1.);
#5773=VECTOR('',#19282,1.);
#5774=VECTOR('',#19285,1.);
#5775=VECTOR('',#19288,1.);
#5776=VECTOR('',#19291,1.);
#5777=VECTOR('',#19294,1.);
#5778=VECTOR('',#19297,3.325);
#5779=VECTOR('',#19302,1.);
#5780=VECTOR('',#19305,1.);
#5781=VECTOR('',#19308,1.);
#5782=VECTOR('',#19311,1.);
#5783=VECTOR('',#19314,1.);
#5784=VECTOR('',#19317,1.);
#5785=VECTOR('',#19320,1.);
#5786=VECTOR('',#19323,1.);
#5787=VECTOR('',#19326,1.);
#5788=VECTOR('',#19329,1.);
#5789=VECTOR('',#19332,1.);
#5790=VECTOR('',#19335,1.);
#5791=VECTOR('',#19338,1.);
#5792=VECTOR('',#19341,1.);
#5793=VECTOR('',#19344,1.);
#5794=VECTOR('',#19347,1.);
#5795=VECTOR('',#19350,1.);
#5796=VECTOR('',#19353,1.);
#5797=VECTOR('',#19356,1.);
#5798=VECTOR('',#19359,1.);
#5799=VECTOR('',#19362,1.);
#5800=VECTOR('',#19365,1.);
#5801=VECTOR('',#19368,1.);
#5802=VECTOR('',#19371,1.);
#5803=VECTOR('',#19374,1.);
#5804=VECTOR('',#19377,1.);
#5805=VECTOR('',#19380,1.);
#5806=VECTOR('',#19383,1.);
#5807=VECTOR('',#19386,1.);
#5808=VECTOR('',#19389,1.);
#5809=VECTOR('',#19936,1.);
#5810=VECTOR('',#19937,1.);
#5811=VECTOR('',#19938,1.);
#5812=VECTOR('',#19939,1.);
#5813=VECTOR('',#19942,1.);
#5814=VECTOR('',#19943,1.);
#5815=VECTOR('',#19944,1.);
#5816=VECTOR('',#19947,1.);
#5817=VECTOR('',#19948,1.);
#5818=VECTOR('',#19949,1.);
#5819=VECTOR('',#19964,2.21);
#5820=VECTOR('',#19969,2.25);
#5821=VECTOR('',#19978,2.575);
#5822=VECTOR('',#19983,2.6);
#5823=VECTOR('',#19992,3.3);
#5824=VECTOR('',#20001,2.6);
#5825=VECTOR('',#20004,2.575);
#5826=VECTOR('',#20015,2.25);
#5827=VECTOR('',#20018,2.21);
#5828=VECTOR('',#20043,2.575);
#5829=VECTOR('',#20048,2.6);
#5830=VECTOR('',#20051,2.58);
#5831=VECTOR('',#20062,1.7);
#5832=VECTOR('',#20071,1.325);
#5833=VECTOR('',#20076,1.25);
#5834=VECTOR('',#20079,1.35);
#5835=VECTOR('',#20084,1.525);
#5836=VECTOR('',#20091,1.);
#5837=VECTOR('',#20100,1.12);
#5838=VECTOR('',#20111,2.52);
#5839=VECTOR('',#20122,2.6);
#5840=VECTOR('',#20125,2.58);
#5841=VECTOR('',#20134,0.4372);
#5842=VECTOR('',#20139,0.4372);
#5843=VECTOR('',#20142,0.4372);
#5844=VECTOR('',#20145,0.4372);
#5845=VECTOR('',#20148,0.4372);
#5846=VECTOR('',#20151,0.4372);
#5847=VECTOR('',#20174,0.320138837486628);
#5848=VECTOR('',#20179,1.);
#5849=VECTOR('',#20180,1.);
#5850=VECTOR('',#20181,1.);
#5851=VECTOR('',#20184,1.);
#5852=VECTOR('',#20185,1.);
#5853=VECTOR('',#20188,1.);
#5854=VECTOR('',#20189,1.);
#5855=VECTOR('',#20192,0.1225);
#5856=VECTOR('',#20197,1.);
#5857=VECTOR('',#20198,1.);
#5858=VECTOR('',#20201,1.);
#5859=VECTOR('',#20202,1.);
#5860=VECTOR('',#20205,1.);
#5861=VECTOR('',#20214,0.465);
#5862=VECTOR('',#20225,0.44);
#5863=VECTOR('',#20234,0.69);
#5864=VECTOR('',#20239,0.7);
#5865=VECTOR('',#20242,0.68);
#5866=VECTOR('',#20253,0.515);
#5867=VECTOR('',#20264,0.695);
#5868=VECTOR('',#20269,0.7);
#5869=VECTOR('',#20272,0.695);
#5870=VECTOR('',#20283,0.515);
#5871=VECTOR('',#20286,0.51);
#5872=VECTOR('',#20293,0.55);
#5873=VECTOR('',#20304,0.68);
#5874=VECTOR('',#20309,0.7);
#5875=VECTOR('',#20318,1.875);
#5876=VECTOR('',#20323,1.9);
#5877=VECTOR('',#20326,1.88);
#5878=VECTOR('',#20339,2.26);
#5879=VECTOR('',#20346,2.3);
#5880=VECTOR('',#20355,1.68);
#5881=VECTOR('',#20364,1.72);
#5882=VECTOR('',#20379,1.25);
#5883=VECTOR('',#20384,1.28);
#5884=VECTOR('',#20393,1.99);
#5885=VECTOR('',#20398,2.21);
#5886=VECTOR('',#20407,2.57);
#5887=VECTOR('',#20412,2.6);
#5888=VECTOR('',#20415,2.57);
#5889=VECTOR('',#20424,1.95);
#5890=VECTOR('',#20431,1.28);
#5891=VECTOR('',#20438,2.25);
#5892=VECTOR('',#20443,2.28);
#5893=VECTOR('',#20454,2.67);
#5894=VECTOR('',#20463,3.18);
#5895=VECTOR('',#20472,3.72);
#5896=VECTOR('',#20477,3.75);
#5897=VECTOR('',#20480,3.72);
#5898=VECTOR('',#20491,3.18);
#5899=VECTOR('',#20500,2.67);
#5900=VECTOR('',#20507,2.28);
#5901=VECTOR('',#20520,3.075);
#5902=VECTOR('',#20525,3.1);
#5903=VECTOR('',#20528,3.08);
#5904=VECTOR('',#20539,2.65);
#5905=VECTOR('',#20548,2.325);
#5906=VECTOR('',#20553,2.25);
#5907=VECTOR('',#20556,2.35);
#5908=VECTOR('',#20561,2.525);
#5909=VECTOR('',#20568,0.135);
#5910=VECTOR('',#20573,0.125);
#5911=VECTOR('',#20578,1.);
#5912=VECTOR('',#20581,1.);
#5913=VECTOR('',#20596,0.135);
#5914=VECTOR('',#20601,1.);
#5915=VECTOR('',#20612,1.);
#5916=VECTOR('',#20621,0.135);
#5917=VECTOR('',#20624,0.125);
#5918=VECTOR('',#20629,0.135);
#5919=VECTOR('',#20632,1.);
#5920=VECTOR('',#20633,1.);
#5921=VECTOR('',#20636,1.);
#5922=VECTOR('',#20637,1.);
#5923=VECTOR('',#20640,1.);
#5924=VECTOR('',#20643,1.);
#5925=VECTOR('',#20646,1.);
#5926=VECTOR('',#20649,1.);
#5927=VECTOR('',#20658,0.237175);
#5928=VECTOR('',#20663,0.237175);
#5929=VECTOR('',#20666,0.237175);
#5930=VECTOR('',#20669,0.237175);
#5931=VECTOR('',#20672,0.237175);
#5932=VECTOR('',#20675,0.237175);
#5933=VECTOR('',#20678,0.237175);
#5934=VECTOR('',#20681,0.237175);
#5935=VECTOR('',#20684,0.237175);
#5936=VECTOR('',#20687,0.237175);
#5937=VECTOR('',#20690,0.237175);
#5938=VECTOR('',#20693,0.237175);
#5939=VECTOR('',#20696,0.237175);
#5940=VECTOR('',#20699,0.237175);
#5941=VECTOR('',#20702,0.237175);
#5942=VECTOR('',#20705,0.237175);
#5943=VECTOR('',#20708,0.237175);
#5944=VECTOR('',#20711,0.237175);
#5945=VECTOR('',#20714,0.237175);
#5946=VECTOR('',#20751,0.320138837486628);
#5947=VECTOR('',#20756,1.);
#5948=VECTOR('',#20757,1.);
#5949=VECTOR('',#20758,1.);
#5950=VECTOR('',#20761,1.);
#5951=VECTOR('',#20762,1.);
#5952=VECTOR('',#20765,1.);
#5953=VECTOR('',#20766,1.);
#5954=VECTOR('',#20769,0.1225);
#5955=VECTOR('',#20774,1.);
#5956=VECTOR('',#20775,1.);
#5957=VECTOR('',#20778,1.);
#5958=VECTOR('',#20779,1.);
#5959=VECTOR('',#20782,1.);
#5960=VECTOR('',#20795,0.5);
#5961=VECTOR('',#20806,0.2775);
#5962=VECTOR('',#20809,0.49);
#5963=VECTOR('',#20814,0.237175);
#5964=VECTOR('',#20819,0.237175);
#5965=VECTOR('',#20822,0.237175);
#5966=VECTOR('',#20825,0.237175);
#5967=VECTOR('',#20828,0.237175);
#5968=VECTOR('',#20831,0.237175);
#5969=VECTOR('',#20834,0.237175);
#5970=VECTOR('',#20837,0.237175);
#5971=VECTOR('',#20840,0.237175);
#5972=VECTOR('',#20843,0.237175);
#5973=VECTOR('',#20846,0.237175);
#5974=VECTOR('',#20849,0.237175);
#5975=VECTOR('',#20852,0.237175);
#5976=VECTOR('',#20855,0.237175);
#5977=VECTOR('',#20858,0.237175);
#5978=VECTOR('',#20895,0.320138837486628);
#5979=VECTOR('',#20900,1.);
#5980=VECTOR('',#20901,1.);
#5981=VECTOR('',#20902,1.);
#5982=VECTOR('',#20905,1.);
#5983=VECTOR('',#20906,1.);
#5984=VECTOR('',#20909,1.);
#5985=VECTOR('',#20910,1.);
#5986=VECTOR('',#20913,0.1225);
#5987=VECTOR('',#20918,1.);
#5988=VECTOR('',#20919,1.);
#5989=VECTOR('',#20922,1.);
#5990=VECTOR('',#20923,1.);
#5991=VECTOR('',#20926,1.);
#5992=VECTOR('',#20939,0.5);
#5993=VECTOR('',#20950,0.2775);
#5994=VECTOR('',#20953,0.49);
#5995=VECTOR('',#20960,1.1);
#5996=VECTOR('',#20971,1.23);
#5997=VECTOR('',#20976,1.25);
#5998=VECTOR('',#20985,1.575);
#5999=VECTOR('',#20990,1.6);
#6000=VECTOR('',#20993,1.58);
#6001=VERTEX_POINT('',#21061);
#6002=VERTEX_POINT('',#21062);
#6003=VERTEX_POINT('',#21064);
#6004=VERTEX_POINT('',#21066);
#6005=VERTEX_POINT('',#21070);
#6006=VERTEX_POINT('',#21072);
#6007=VERTEX_POINT('',#21076);
#6008=VERTEX_POINT('',#21078);
#6009=VERTEX_POINT('',#21086);
#6010=VERTEX_POINT('',#21087);
#6011=VERTEX_POINT('',#21089);
#6012=VERTEX_POINT('',#21091);
#6013=VERTEX_POINT('',#21095);
#6014=VERTEX_POINT('',#21097);
#6015=VERTEX_POINT('',#21099);
#6016=VERTEX_POINT('',#21101);
#6017=VERTEX_POINT('',#21105);
#6018=VERTEX_POINT('',#21109);
#6019=VERTEX_POINT('',#21113);
#6020=VERTEX_POINT('',#21117);
#6021=VERTEX_POINT('',#21118);
#6022=VERTEX_POINT('',#21120);
#6023=VERTEX_POINT('',#21122);
#6024=VERTEX_POINT('',#21126);
#6025=VERTEX_POINT('',#21128);
#6026=VERTEX_POINT('',#21132);
#6027=VERTEX_POINT('',#21134);
#6028=VERTEX_POINT('',#21142);
#6029=VERTEX_POINT('',#21143);
#6030=VERTEX_POINT('',#21145);
#6031=VERTEX_POINT('',#21147);
#6032=VERTEX_POINT('',#21151);
#6033=VERTEX_POINT('',#21153);
#6034=VERTEX_POINT('',#21157);
#6035=VERTEX_POINT('',#21159);
#6036=VERTEX_POINT('',#21167);
#6037=VERTEX_POINT('',#21168);
#6038=VERTEX_POINT('',#21170);
#6039=VERTEX_POINT('',#21172);
#6040=VERTEX_POINT('',#21176);
#6041=VERTEX_POINT('',#21178);
#6042=VERTEX_POINT('',#21182);
#6043=VERTEX_POINT('',#21184);
#6044=VERTEX_POINT('',#21192);
#6045=VERTEX_POINT('',#21193);
#6046=VERTEX_POINT('',#21195);
#6047=VERTEX_POINT('',#21197);
#6048=VERTEX_POINT('',#21201);
#6049=VERTEX_POINT('',#21202);
#6050=VERTEX_POINT('',#21204);
#6051=VERTEX_POINT('',#21206);
#6052=VERTEX_POINT('',#21210);
#6053=VERTEX_POINT('',#21212);
#6054=VERTEX_POINT('',#21219);
#6055=VERTEX_POINT('',#21223);
#6056=VERTEX_POINT('',#21225);
#6057=VERTEX_POINT('',#21227);
#6058=VERTEX_POINT('',#21231);
#6059=VERTEX_POINT('',#21233);
#6060=VERTEX_POINT('',#21237);
#6061=VERTEX_POINT('',#21239);
#6062=VERTEX_POINT('',#21241);
#6063=VERTEX_POINT('',#21243);
#6064=VERTEX_POINT('',#21245);
#6065=VERTEX_POINT('',#21248);
#6066=VERTEX_POINT('',#21250);
#6067=VERTEX_POINT('',#21252);
#6068=VERTEX_POINT('',#21255);
#6069=VERTEX_POINT('',#21258);
#6070=VERTEX_POINT('',#21259);
#6071=VERTEX_POINT('',#21261);
#6072=VERTEX_POINT('',#21263);
#6073=VERTEX_POINT('',#21267);
#6074=VERTEX_POINT('',#21269);
#6075=VERTEX_POINT('',#21273);
#6076=VERTEX_POINT('',#21275);
#6077=VERTEX_POINT('',#21283);
#6078=VERTEX_POINT('',#21284);
#6079=VERTEX_POINT('',#21286);
#6080=VERTEX_POINT('',#21288);
#6081=VERTEX_POINT('',#21292);
#6082=VERTEX_POINT('',#21293);
#6083=VERTEX_POINT('',#21295);
#6084=VERTEX_POINT('',#21297);
#6085=VERTEX_POINT('',#21304);
#6086=VERTEX_POINT('',#21305);
#6087=VERTEX_POINT('',#21310);
#6088=VERTEX_POINT('',#21314);
#6089=VERTEX_POINT('',#21315);
#6090=VERTEX_POINT('',#21317);
#6091=VERTEX_POINT('',#21319);
#6092=VERTEX_POINT('',#21323);
#6093=VERTEX_POINT('',#21325);
#6094=VERTEX_POINT('',#21329);
#6095=VERTEX_POINT('',#21331);
#6096=VERTEX_POINT('',#21339);
#6097=VERTEX_POINT('',#21340);
#6098=VERTEX_POINT('',#21342);
#6099=VERTEX_POINT('',#21344);
#6100=VERTEX_POINT('',#21348);
#6101=VERTEX_POINT('',#21350);
#6102=VERTEX_POINT('',#21354);
#6103=VERTEX_POINT('',#21356);
#6104=VERTEX_POINT('',#21364);
#6105=VERTEX_POINT('',#21365);
#6106=VERTEX_POINT('',#21367);
#6107=VERTEX_POINT('',#21369);
#6108=VERTEX_POINT('',#21373);
#6109=VERTEX_POINT('',#21375);
#6110=VERTEX_POINT('',#21379);
#6111=VERTEX_POINT('',#21381);
#6112=VERTEX_POINT('',#21389);
#6113=VERTEX_POINT('',#21390);
#6114=VERTEX_POINT('',#21392);
#6115=VERTEX_POINT('',#21394);
#6116=VERTEX_POINT('',#21398);
#6117=VERTEX_POINT('',#21400);
#6118=VERTEX_POINT('',#21404);
#6119=VERTEX_POINT('',#21405);
#6120=VERTEX_POINT('',#21407);
#6121=VERTEX_POINT('',#21409);
#6122=VERTEX_POINT('',#21416);
#6123=VERTEX_POINT('',#21420);
#6124=VERTEX_POINT('',#21422);
#6125=VERTEX_POINT('',#21424);
#6126=VERTEX_POINT('',#21428);
#6127=VERTEX_POINT('',#21430);
#6128=VERTEX_POINT('',#21432);
#6129=VERTEX_POINT('',#21436);
#6130=VERTEX_POINT('',#21438);
#6131=VERTEX_POINT('',#21440);
#6132=VERTEX_POINT('',#21442);
#6133=VERTEX_POINT('',#21444);
#6134=VERTEX_POINT('',#21446);
#6135=VERTEX_POINT('',#21448);
#6136=VERTEX_POINT('',#21450);
#6137=VERTEX_POINT('',#21452);
#6138=VERTEX_POINT('',#21455);
#6139=VERTEX_POINT('',#21457);
#6140=VERTEX_POINT('',#21459);
#6141=VERTEX_POINT('',#21461);
#6142=VERTEX_POINT('',#21463);
#6143=VERTEX_POINT('',#21466);
#6144=VERTEX_POINT('',#21468);
#6145=VERTEX_POINT('',#21470);
#6146=VERTEX_POINT('',#21473);
#6147=VERTEX_POINT('',#21474);
#6148=VERTEX_POINT('',#21476);
#6149=VERTEX_POINT('',#21478);
#6150=VERTEX_POINT('',#21482);
#6151=VERTEX_POINT('',#21484);
#6152=VERTEX_POINT('',#21488);
#6153=VERTEX_POINT('',#21490);
#6154=VERTEX_POINT('',#21494);
#6155=VERTEX_POINT('',#21496);
#6156=VERTEX_POINT('',#21500);
#6157=VERTEX_POINT('',#21502);
#6158=VERTEX_POINT('',#21510);
#6159=VERTEX_POINT('',#21511);
#6160=VERTEX_POINT('',#21513);
#6161=VERTEX_POINT('',#21515);
#6162=VERTEX_POINT('',#21519);
#6163=VERTEX_POINT('',#21521);
#6164=VERTEX_POINT('',#21525);
#6165=VERTEX_POINT('',#21527);
#6166=VERTEX_POINT('',#21531);
#6167=VERTEX_POINT('',#21533);
#6168=VERTEX_POINT('',#21537);
#6169=VERTEX_POINT('',#21539);
#6170=VERTEX_POINT('',#21541);
#6171=VERTEX_POINT('',#21544);
#6172=VERTEX_POINT('',#21546);
#6173=VERTEX_POINT('',#21549);
#6174=VERTEX_POINT('',#21551);
#6175=VERTEX_POINT('',#21553);
#6176=VERTEX_POINT('',#21555);
#6177=VERTEX_POINT('',#21559);
#6178=VERTEX_POINT('',#21560);
#6179=VERTEX_POINT('',#21562);
#6180=VERTEX_POINT('',#21567);
#6181=VERTEX_POINT('',#21574);
#6182=VERTEX_POINT('',#21576);
#6183=VERTEX_POINT('',#21580);
#6184=VERTEX_POINT('',#21582);
#6185=VERTEX_POINT('',#21586);
#6186=VERTEX_POINT('',#21588);
#6187=VERTEX_POINT('',#21595);
#6188=VERTEX_POINT('',#21597);
#6189=VERTEX_POINT('',#21604);
#6190=VERTEX_POINT('',#21606);
#6191=VERTEX_POINT('',#21610);
#6192=VERTEX_POINT('',#21612);
#6193=VERTEX_POINT('',#21616);
#6194=VERTEX_POINT('',#21618);
#6195=VERTEX_POINT('',#21625);
#6196=VERTEX_POINT('',#21627);
#6197=VERTEX_POINT('',#21634);
#6198=VERTEX_POINT('',#21636);
#6199=VERTEX_POINT('',#21643);
#6200=VERTEX_POINT('',#21645);
#6201=VERTEX_POINT('',#21668);
#6202=VERTEX_POINT('',#21670);
#6203=VERTEX_POINT('',#21672);
#6204=VERTEX_POINT('',#21674);
#6205=VERTEX_POINT('',#21676);
#6206=VERTEX_POINT('',#21679);
#6207=VERTEX_POINT('',#21680);
#6208=VERTEX_POINT('',#21717);
#6209=VERTEX_POINT('',#21721);
#6210=VERTEX_POINT('',#21725);
#6211=VERTEX_POINT('',#21726);
#6212=VERTEX_POINT('',#21730);
#6213=VERTEX_POINT('',#21732);
#6214=VERTEX_POINT('',#21747);
#6215=VERTEX_POINT('',#21762);
#6216=VERTEX_POINT('',#21793);
#6217=VERTEX_POINT('',#21795);
#6218=VERTEX_POINT('',#21797);
#6219=VERTEX_POINT('',#21810);
#6220=VERTEX_POINT('',#21812);
#6221=VERTEX_POINT('',#21814);
#6222=VERTEX_POINT('',#21816);
#6223=VERTEX_POINT('',#21818);
#6224=VERTEX_POINT('',#21820);
#6225=VERTEX_POINT('',#21822);
#6226=VERTEX_POINT('',#21824);
#6227=VERTEX_POINT('',#21827);
#6228=VERTEX_POINT('',#21829);
#6229=VERTEX_POINT('',#21831);
#6230=VERTEX_POINT('',#21834);
#6231=VERTEX_POINT('',#21835);
#6232=VERTEX_POINT('',#21837);
#6233=VERTEX_POINT('',#21839);
#6234=VERTEX_POINT('',#21842);
#6235=VERTEX_POINT('',#21843);
#6236=VERTEX_POINT('',#21845);
#6237=VERTEX_POINT('',#21847);
#6238=VERTEX_POINT('',#21850);
#6239=VERTEX_POINT('',#21851);
#6240=VERTEX_POINT('',#21853);
#6241=VERTEX_POINT('',#21855);
#6242=VERTEX_POINT('',#21858);
#6243=VERTEX_POINT('',#21859);
#6244=VERTEX_POINT('',#21861);
#6245=VERTEX_POINT('',#21863);
#6246=VERTEX_POINT('',#21866);
#6247=VERTEX_POINT('',#21867);
#6248=VERTEX_POINT('',#21869);
#6249=VERTEX_POINT('',#21871);
#6250=VERTEX_POINT('',#21874);
#6251=VERTEX_POINT('',#21875);
#6252=VERTEX_POINT('',#21877);
#6253=VERTEX_POINT('',#21879);
#6254=VERTEX_POINT('',#21883);
#6255=VERTEX_POINT('',#21884);
#6256=VERTEX_POINT('',#21888);
#6257=VERTEX_POINT('',#21891);
#6258=VERTEX_POINT('',#21892);
#6259=VERTEX_POINT('',#22006);
#6260=VERTEX_POINT('',#22007);
#6261=VERTEX_POINT('',#22011);
#6262=VERTEX_POINT('',#22039);
#6263=VERTEX_POINT('',#22040);
#6264=VERTEX_POINT('',#22044);
#6265=VERTEX_POINT('',#22050);
#6266=VERTEX_POINT('',#22051);
#6267=VERTEX_POINT('',#22055);
#6268=VERTEX_POINT('',#22061);
#6269=VERTEX_POINT('',#22062);
#6270=VERTEX_POINT('',#22066);
#6271=VERTEX_POINT('',#22070);
#6272=VERTEX_POINT('',#22074);
#6273=VERTEX_POINT('',#22075);
#6274=VERTEX_POINT('',#22079);
#6275=VERTEX_POINT('',#22085);
#6276=VERTEX_POINT('',#22086);
#6277=VERTEX_POINT('',#22090);
#6278=VERTEX_POINT('',#22094);
#6279=VERTEX_POINT('',#22098);
#6280=VERTEX_POINT('',#22099);
#6281=VERTEX_POINT('',#22103);
#6282=VERTEX_POINT('',#22109);
#6283=VERTEX_POINT('',#22110);
#6284=VERTEX_POINT('',#22114);
#6285=VERTEX_POINT('',#22118);
#6286=VERTEX_POINT('',#22122);
#6287=VERTEX_POINT('',#22123);
#6288=VERTEX_POINT('',#22127);
#6289=VERTEX_POINT('',#22133);
#6290=VERTEX_POINT('',#22134);
#6291=VERTEX_POINT('',#22138);
#6292=VERTEX_POINT('',#22142);
#6293=VERTEX_POINT('',#22146);
#6294=VERTEX_POINT('',#22147);
#6295=VERTEX_POINT('',#22151);
#6296=VERTEX_POINT('',#22157);
#6297=VERTEX_POINT('',#22158);
#6298=VERTEX_POINT('',#22162);
#6299=VERTEX_POINT('',#22168);
#6300=VERTEX_POINT('',#22169);
#6301=VERTEX_POINT('',#22173);
#6302=VERTEX_POINT('',#22179);
#6303=VERTEX_POINT('',#22180);
#6304=VERTEX_POINT('',#22185);
#6305=VERTEX_POINT('',#22191);
#6306=VERTEX_POINT('',#22193);
#6307=VERTEX_POINT('',#22197);
#6308=VERTEX_POINT('',#22201);
#6309=VERTEX_POINT('',#22203);
#6310=VERTEX_POINT('',#22207);
#6311=VERTEX_POINT('',#22211);
#6312=VERTEX_POINT('',#22213);
#6313=VERTEX_POINT('',#22217);
#6314=VERTEX_POINT('',#22221);
#6315=VERTEX_POINT('',#22223);
#6316=VERTEX_POINT('',#22227);
#6317=VERTEX_POINT('',#22231);
#6318=VERTEX_POINT('',#22237);
#6319=VERTEX_POINT('',#22241);
#6320=VERTEX_POINT('',#22247);
#6321=VERTEX_POINT('',#22249);
#6322=VERTEX_POINT('',#22251);
#6323=VERTEX_POINT('',#22253);
#6324=VERTEX_POINT('',#22255);
#6325=VERTEX_POINT('',#22257);
#6326=VERTEX_POINT('',#22260);
#6327=VERTEX_POINT('',#22263);
#6328=VERTEX_POINT('',#22265);
#6329=VERTEX_POINT('',#22269);
#6330=VERTEX_POINT('',#22274);
#6331=VERTEX_POINT('',#22279);
#6332=VERTEX_POINT('',#22281);
#6333=VERTEX_POINT('',#22283);
#6334=VERTEX_POINT('',#22292);
#6335=VERTEX_POINT('',#22297);
#6336=VERTEX_POINT('',#22301);
#6337=VERTEX_POINT('',#22303);
#6338=VERTEX_POINT('',#22305);
#6339=VERTEX_POINT('',#22307);
#6340=VERTEX_POINT('',#22309);
#6341=VERTEX_POINT('',#22311);
#6342=VERTEX_POINT('',#22327);
#6343=VERTEX_POINT('',#22329);
#6344=VERTEX_POINT('',#22333);
#6345=VERTEX_POINT('',#22337);
#6346=VERTEX_POINT('',#22344);
#6347=VERTEX_POINT('',#22346);
#6348=VERTEX_POINT('',#22350);
#6349=VERTEX_POINT('',#22354);
#6350=VERTEX_POINT('',#22361);
#6351=VERTEX_POINT('',#22363);
#6352=VERTEX_POINT('',#22367);
#6353=VERTEX_POINT('',#22371);
#6354=VERTEX_POINT('',#22378);
#6355=VERTEX_POINT('',#22380);
#6356=VERTEX_POINT('',#22384);
#6357=VERTEX_POINT('',#22388);
#6358=VERTEX_POINT('',#22395);
#6359=VERTEX_POINT('',#22397);
#6360=VERTEX_POINT('',#22401);
#6361=VERTEX_POINT('',#22405);
#6362=VERTEX_POINT('',#22412);
#6363=VERTEX_POINT('',#22414);
#6364=VERTEX_POINT('',#22418);
#6365=VERTEX_POINT('',#22422);
#6366=VERTEX_POINT('',#22429);
#6367=VERTEX_POINT('',#22433);
#6368=VERTEX_POINT('',#22436);
#6369=VERTEX_POINT('',#22440);
#6370=VERTEX_POINT('',#22443);
#6371=VERTEX_POINT('',#22447);
#6372=VERTEX_POINT('',#22450);
#6373=VERTEX_POINT('',#22452);
#6374=VERTEX_POINT('',#22471);
#6375=VERTEX_POINT('',#22490);
#6376=VERTEX_POINT('',#22529);
#6377=VERTEX_POINT('',#22532);
#6378=VERTEX_POINT('',#22536);
#6379=VERTEX_POINT('',#22539);
#6380=VERTEX_POINT('',#22543);
#6381=VERTEX_POINT('',#22548);
#6382=VERTEX_POINT('',#22552);
#6383=VERTEX_POINT('',#22555);
#6384=VERTEX_POINT('',#22559);
#6385=VERTEX_POINT('',#22562);
#6386=VERTEX_POINT('',#22572);
#6387=VERTEX_POINT('',#22574);
#6388=VERTEX_POINT('',#22578);
#6389=VERTEX_POINT('',#22582);
#6390=VERTEX_POINT('',#22585);
#6391=VERTEX_POINT('',#22586);
#6392=VERTEX_POINT('',#22588);
#6393=VERTEX_POINT('',#22593);
#6394=VERTEX_POINT('',#22600);
#6395=VERTEX_POINT('',#22602);
#6396=VERTEX_POINT('',#22609);
#6397=VERTEX_POINT('',#22611);
#6398=VERTEX_POINT('',#22618);
#6399=VERTEX_POINT('',#22620);
#6400=VERTEX_POINT('',#22627);
#6401=VERTEX_POINT('',#22629);
#6402=VERTEX_POINT('',#22636);
#6403=VERTEX_POINT('',#22638);
#6404=VERTEX_POINT('',#22645);
#6405=VERTEX_POINT('',#22647);
#6406=VERTEX_POINT('',#22657);
#6407=VERTEX_POINT('',#22659);
#6408=VERTEX_POINT('',#22663);
#6409=VERTEX_POINT('',#22667);
#6410=VERTEX_POINT('',#22671);
#6411=VERTEX_POINT('',#22675);
#6412=VERTEX_POINT('',#22677);
#6413=VERTEX_POINT('',#22679);
#6414=VERTEX_POINT('',#22681);
#6415=VERTEX_POINT('',#22683);
#6416=VERTEX_POINT('',#22686);
#6417=VERTEX_POINT('',#22688);
#6418=VERTEX_POINT('',#22692);
#6419=VERTEX_POINT('',#22696);
#6420=VERTEX_POINT('',#22700);
#6421=VERTEX_POINT('',#22705);
#6422=VERTEX_POINT('',#22707);
#6423=VERTEX_POINT('',#22711);
#6424=VERTEX_POINT('',#22715);
#6425=VERTEX_POINT('',#22719);
#6426=VERTEX_POINT('',#22724);
#6427=VERTEX_POINT('',#22726);
#6428=VERTEX_POINT('',#22730);
#6429=VERTEX_POINT('',#22734);
#6430=VERTEX_POINT('',#22738);
#6431=VERTEX_POINT('',#22743);
#6432=VERTEX_POINT('',#22745);
#6433=VERTEX_POINT('',#22749);
#6434=VERTEX_POINT('',#22753);
#6435=VERTEX_POINT('',#22757);
#6436=VERTEX_POINT('',#22762);
#6437=VERTEX_POINT('',#22766);
#6438=VERTEX_POINT('',#22770);
#6439=VERTEX_POINT('',#22775);
#6440=VERTEX_POINT('',#22779);
#6441=VERTEX_POINT('',#22783);
#6442=VERTEX_POINT('',#22791);
#6443=VERTEX_POINT('',#22792);
#6444=VERTEX_POINT('',#22794);
#6445=VERTEX_POINT('',#22796);
#6446=VERTEX_POINT('',#22800);
#6447=VERTEX_POINT('',#22802);
#6448=VERTEX_POINT('',#22806);
#6449=VERTEX_POINT('',#22808);
#6450=VERTEX_POINT('',#22812);
#6451=VERTEX_POINT('',#22814);
#6452=VERTEX_POINT('',#22818);
#6453=VERTEX_POINT('',#22820);
#6454=VERTEX_POINT('',#22824);
#6455=VERTEX_POINT('',#22826);
#6456=VERTEX_POINT('',#22830);
#6457=VERTEX_POINT('',#22832);
#6458=VERTEX_POINT('',#22839);
#6459=VERTEX_POINT('',#22841);
#6460=VERTEX_POINT('',#22845);
#6461=VERTEX_POINT('',#22849);
#6462=VERTEX_POINT('',#22853);
#6463=VERTEX_POINT('',#22857);
#6464=VERTEX_POINT('',#22859);
#6465=VERTEX_POINT('',#22860);
#6466=VERTEX_POINT('',#22862);
#6467=VERTEX_POINT('',#22864);
#6468=VERTEX_POINT('',#22867);
#6469=VERTEX_POINT('',#22868);
#6470=VERTEX_POINT('',#22870);
#6471=VERTEX_POINT('',#22872);
#6472=VERTEX_POINT('',#22875);
#6473=VERTEX_POINT('',#22876);
#6474=VERTEX_POINT('',#22878);
#6475=VERTEX_POINT('',#22880);
#6476=VERTEX_POINT('',#22883);
#6477=VERTEX_POINT('',#22884);
#6478=VERTEX_POINT('',#22886);
#6479=VERTEX_POINT('',#22888);
#6480=VERTEX_POINT('',#22891);
#6481=VERTEX_POINT('',#22893);
#6482=VERTEX_POINT('',#22895);
#6483=VERTEX_POINT('',#22897);
#6484=VERTEX_POINT('',#22900);
#6485=VERTEX_POINT('',#22902);
#6486=VERTEX_POINT('',#22906);
#6487=VERTEX_POINT('',#22910);
#6488=VERTEX_POINT('',#22914);
#6489=VERTEX_POINT('',#22917);
#6490=VERTEX_POINT('',#22921);
#6491=VERTEX_POINT('',#22923);
#6492=VERTEX_POINT('',#22927);
#6493=VERTEX_POINT('',#22931);
#6494=VERTEX_POINT('',#22935);
#6495=VERTEX_POINT('',#22938);
#6496=VERTEX_POINT('',#22942);
#6497=VERTEX_POINT('',#22944);
#6498=VERTEX_POINT('',#22948);
#6499=VERTEX_POINT('',#22952);
#6500=VERTEX_POINT('',#22956);
#6501=VERTEX_POINT('',#22959);
#6502=VERTEX_POINT('',#22963);
#6503=VERTEX_POINT('',#22965);
#6504=VERTEX_POINT('',#22969);
#6505=VERTEX_POINT('',#22973);
#6506=VERTEX_POINT('',#22977);
#6507=VERTEX_POINT('',#22980);
#6508=VERTEX_POINT('',#22984);
#6509=VERTEX_POINT('',#22986);
#6510=VERTEX_POINT('',#22990);
#6511=VERTEX_POINT('',#22996);
#6512=VERTEX_POINT('',#22998);
#6513=VERTEX_POINT('',#23002);
#6514=VERTEX_POINT('',#23008);
#6515=VERTEX_POINT('',#23010);
#6516=VERTEX_POINT('',#23014);
#6517=VERTEX_POINT('',#23020);
#6518=VERTEX_POINT('',#23022);
#6519=VERTEX_POINT('',#23026);
#6520=VERTEX_POINT('',#23032);
#6521=VERTEX_POINT('',#23033);
#6522=VERTEX_POINT('',#23038);
#6523=VERTEX_POINT('',#23042);
#6524=VERTEX_POINT('',#23048);
#6525=VERTEX_POINT('',#23049);
#6526=VERTEX_POINT('',#23054);
#6527=VERTEX_POINT('',#23058);
#6528=VERTEX_POINT('',#23064);
#6529=VERTEX_POINT('',#23065);
#6530=VERTEX_POINT('',#23070);
#6531=VERTEX_POINT('',#23074);
#6532=VERTEX_POINT('',#23080);
#6533=VERTEX_POINT('',#23081);
#6534=VERTEX_POINT('',#23086);
#6535=VERTEX_POINT('',#23090);
#6536=VERTEX_POINT('',#23096);
#6537=VERTEX_POINT('',#23098);
#6538=VERTEX_POINT('',#23102);
#6539=VERTEX_POINT('',#23107);
#6540=VERTEX_POINT('',#23111);
#6541=VERTEX_POINT('',#23115);
#6542=VERTEX_POINT('',#23123);
#6543=VERTEX_POINT('',#23124);
#6544=VERTEX_POINT('',#23126);
#6545=VERTEX_POINT('',#23189);
#6546=VERTEX_POINT('',#23191);
#6547=VERTEX_POINT('',#23200);
#6548=VERTEX_POINT('',#23201);
#6549=VERTEX_POINT('',#23320);
#6550=VERTEX_POINT('',#23321);
#6551=VERTEX_POINT('',#23450);
#6552=VERTEX_POINT('',#23451);
#6553=VERTEX_POINT('',#23590);
#6554=VERTEX_POINT('',#23591);
#6555=VERTEX_POINT('',#23720);
#6556=VERTEX_POINT('',#23721);
#6557=VERTEX_POINT('',#23844);
#6558=VERTEX_POINT('',#23903);
#6559=VERTEX_POINT('',#23905);
#6560=VERTEX_POINT('',#23934);
#6561=VERTEX_POINT('',#23935);
#6562=VERTEX_POINT('',#23937);
#6563=VERTEX_POINT('',#23939);
#6564=VERTEX_POINT('',#23941);
#6565=VERTEX_POINT('',#23947);
#6566=VERTEX_POINT('',#23949);
#6567=VERTEX_POINT('',#23953);
#6568=VERTEX_POINT('',#23954);
#6569=VERTEX_POINT('',#23956);
#6570=VERTEX_POINT('',#23965);
#6571=VERTEX_POINT('',#23967);
#6572=VERTEX_POINT('',#23974);
#6573=VERTEX_POINT('',#23977);
#6574=VERTEX_POINT('',#23979);
#6575=VERTEX_POINT('',#23983);
#6576=VERTEX_POINT('',#23984);
#6577=VERTEX_POINT('',#24012);
#6578=VERTEX_POINT('',#24119);
#6579=VERTEX_POINT('',#24206);
#6580=VERTEX_POINT('',#24233);
#6581=VERTEX_POINT('',#24248);
#6582=VERTEX_POINT('',#24268);
#6583=VERTEX_POINT('',#24272);
#6584=VERTEX_POINT('',#26765);
#6585=VERTEX_POINT('',#26768);
#6586=VERTEX_POINT('',#26772);
#6587=VERTEX_POINT('',#26776);
#6588=VERTEX_POINT('',#26779);
#6589=VERTEX_POINT('',#26783);
#6590=VERTEX_POINT('',#26788);
#6591=VERTEX_POINT('',#26791);
#6592=VERTEX_POINT('',#26795);
#6593=VERTEX_POINT('',#26799);
#6594=VERTEX_POINT('',#26802);
#6595=VERTEX_POINT('',#26806);
#6596=VERTEX_POINT('',#26812);
#6597=VERTEX_POINT('',#26813);
#6598=VERTEX_POINT('',#26815);
#6599=VERTEX_POINT('',#26820);
#6600=VERTEX_POINT('',#26822);
#6601=VERTEX_POINT('',#26826);
#6602=VERTEX_POINT('',#26827);
#6603=VERTEX_POINT('',#26847);
#6604=VERTEX_POINT('',#26849);
#6605=VERTEX_POINT('',#26869);
#6606=VERTEX_POINT('',#26871);
#6607=VERTEX_POINT('',#26890);
#6608=VERTEX_POINT('',#26892);
#6609=VERTEX_POINT('',#26912);
#6610=VERTEX_POINT('',#26914);
#6611=VERTEX_POINT('',#26936);
#6612=VERTEX_POINT('',#26938);
#6613=VERTEX_POINT('',#26957);
#6614=VERTEX_POINT('',#26959);
#6615=VERTEX_POINT('',#26979);
#6616=VERTEX_POINT('',#26981);
#6617=VERTEX_POINT('',#27003);
#6618=VERTEX_POINT('',#27005);
#6619=VERTEX_POINT('',#27025);
#6620=VERTEX_POINT('',#27027);
#6621=VERTEX_POINT('',#27046);
#6622=VERTEX_POINT('',#27048);
#6623=VERTEX_POINT('',#27068);
#6624=VERTEX_POINT('',#27070);
#6625=VERTEX_POINT('',#27089);
#6626=VERTEX_POINT('',#27091);
#6627=VERTEX_POINT('',#27111);
#6628=VERTEX_POINT('',#27113);
#6629=VERTEX_POINT('',#27131);
#6630=VERTEX_POINT('',#27133);
#6631=VERTEX_POINT('',#27154);
#6632=VERTEX_POINT('',#27156);
#6633=VERTEX_POINT('',#27172);
#6634=VERTEX_POINT('',#27174);
#6635=VERTEX_POINT('',#27194);
#6636=VERTEX_POINT('',#27196);
#6637=VERTEX_POINT('',#27214);
#6638=VERTEX_POINT('',#27216);
#6639=VERTEX_POINT('',#27236);
#6640=VERTEX_POINT('',#27238);
#6641=VERTEX_POINT('',#27257);
#6642=VERTEX_POINT('',#27259);
#6643=VERTEX_POINT('',#27275);
#6644=VERTEX_POINT('',#27277);
#6645=VERTEX_POINT('',#27295);
#6646=VERTEX_POINT('',#27297);
#6647=VERTEX_POINT('',#27314);
#6648=VERTEX_POINT('',#27316);
#6649=VERTEX_POINT('',#27332);
#6650=VERTEX_POINT('',#27334);
#6651=VERTEX_POINT('',#27355);
#6652=VERTEX_POINT('',#27357);
#6653=VERTEX_POINT('',#27373);
#6654=VERTEX_POINT('',#27375);
#6655=VERTEX_POINT('',#27392);
#6656=VERTEX_POINT('',#27394);
#6657=VERTEX_POINT('',#27409);
#6658=VERTEX_POINT('',#27411);
#6659=VERTEX_POINT('',#27428);
#6660=VERTEX_POINT('',#27430);
#6661=VERTEX_POINT('',#27449);
#6662=VERTEX_POINT('',#27451);
#6663=VERTEX_POINT('',#27467);
#6664=VERTEX_POINT('',#27469);
#6665=VERTEX_POINT('',#27486);
#6666=VERTEX_POINT('',#27488);
#6667=VERTEX_POINT('',#27505);
#6668=VERTEX_POINT('',#27507);
#6669=VERTEX_POINT('',#27525);
#6670=VERTEX_POINT('',#27527);
#6671=VERTEX_POINT('',#27543);
#6672=VERTEX_POINT('',#27545);
#6673=VERTEX_POINT('',#27586);
#6674=VERTEX_POINT('',#27588);
#6675=VERTEX_POINT('',#27604);
#6676=VERTEX_POINT('',#27606);
#6677=VERTEX_POINT('',#27624);
#6678=VERTEX_POINT('',#27626);
#6679=VERTEX_POINT('',#27642);
#6680=VERTEX_POINT('',#27644);
#6681=VERTEX_POINT('',#27660);
#6682=VERTEX_POINT('',#27662);
#6683=VERTEX_POINT('',#27682);
#6684=VERTEX_POINT('',#27684);
#6685=VERTEX_POINT('',#27702);
#6686=VERTEX_POINT('',#27704);
#6687=VERTEX_POINT('',#27713);
#6688=VERTEX_POINT('',#27715);
#6689=VERTEX_POINT('',#27736);
#6690=VERTEX_POINT('',#27738);
#6691=VERTEX_POINT('',#27757);
#6692=VERTEX_POINT('',#27759);
#6693=VERTEX_POINT('',#27779);
#6694=VERTEX_POINT('',#27781);
#6695=VERTEX_POINT('',#27800);
#6696=VERTEX_POINT('',#27802);
#6697=VERTEX_POINT('',#27826);
#6698=VERTEX_POINT('',#27828);
#6699=VERTEX_POINT('',#27847);
#6700=VERTEX_POINT('',#27849);
#6701=VERTEX_POINT('',#27869);
#6702=VERTEX_POINT('',#27871);
#6703=VERTEX_POINT('',#27890);
#6704=VERTEX_POINT('',#27892);
#6705=VERTEX_POINT('',#27912);
#6706=VERTEX_POINT('',#27914);
#6707=VERTEX_POINT('',#27936);
#6708=VERTEX_POINT('',#27938);
#6709=VERTEX_POINT('',#27957);
#6710=VERTEX_POINT('',#27959);
#6711=VERTEX_POINT('',#27977);
#6712=VERTEX_POINT('',#27979);
#6713=VERTEX_POINT('',#27995);
#6714=VERTEX_POINT('',#27997);
#6715=VERTEX_POINT('',#28020);
#6716=VERTEX_POINT('',#28022);
#6717=VERTEX_POINT('',#28041);
#6718=VERTEX_POINT('',#28043);
#6719=VERTEX_POINT('',#28050);
#6720=VERTEX_POINT('',#28052);
#6721=VERTEX_POINT('',#28113);
#6722=VERTEX_POINT('',#28117);
#6723=VERTEX_POINT('',#28118);
#6724=VERTEX_POINT('',#28127);
#6725=VERTEX_POINT('',#28129);
#6726=VERTEX_POINT('',#28148);
#6727=VERTEX_POINT('',#28150);
#6728=VERTEX_POINT('',#28169);
#6729=VERTEX_POINT('',#28171);
#6730=VERTEX_POINT('',#28190);
#6731=VERTEX_POINT('',#28192);
#6732=VERTEX_POINT('',#28251);
#6733=VERTEX_POINT('',#28253);
#6734=VERTEX_POINT('',#28269);
#6735=VERTEX_POINT('',#28271);
#6736=VERTEX_POINT('',#28278);
#6737=VERTEX_POINT('',#28280);
#6738=VERTEX_POINT('',#28299);
#6739=VERTEX_POINT('',#28301);
#6740=VERTEX_POINT('',#28357);
#6741=VERTEX_POINT('',#28359);
#6742=VERTEX_POINT('',#28379);
#6743=VERTEX_POINT('',#28381);
#6744=VERTEX_POINT('',#28388);
#6745=VERTEX_POINT('',#28390);
#6746=VERTEX_POINT('',#28410);
#6747=VERTEX_POINT('',#28412);
#6748=VERTEX_POINT('',#28419);
#6749=VERTEX_POINT('',#28421);
#6750=VERTEX_POINT('',#28445);
#6751=VERTEX_POINT('',#28447);
#6752=VERTEX_POINT('',#28494);
#6753=VERTEX_POINT('',#28496);
#6754=VERTEX_POINT('',#28516);
#6755=VERTEX_POINT('',#28518);
#6756=VERTEX_POINT('',#28537);
#6757=VERTEX_POINT('',#28539);
#6758=VERTEX_POINT('',#28560);
#6759=VERTEX_POINT('',#28562);
#6760=VERTEX_POINT('',#28580);
#6761=VERTEX_POINT('',#28582);
#6762=VERTEX_POINT('',#28600);
#6763=VERTEX_POINT('',#28602);
#6764=VERTEX_POINT('',#28611);
#6765=VERTEX_POINT('',#28613);
#6766=VERTEX_POINT('',#28629);
#6767=VERTEX_POINT('',#28631);
#6768=VERTEX_POINT('',#28638);
#6769=VERTEX_POINT('',#28640);
#6770=VERTEX_POINT('',#28658);
#6771=VERTEX_POINT('',#28660);
#6772=VERTEX_POINT('',#28667);
#6773=VERTEX_POINT('',#28669);
#6774=VERTEX_POINT('',#28687);
#6775=VERTEX_POINT('',#28689);
#6776=VERTEX_POINT('',#28696);
#6777=VERTEX_POINT('',#28698);
#6778=VERTEX_POINT('',#28716);
#6779=VERTEX_POINT('',#28718);
#6780=VERTEX_POINT('',#28725);
#6781=VERTEX_POINT('',#28727);
#6782=VERTEX_POINT('',#28744);
#6783=VERTEX_POINT('',#28746);
#6784=VERTEX_POINT('',#28784);
#6785=VERTEX_POINT('',#28786);
#6786=VERTEX_POINT('',#28805);
#6787=VERTEX_POINT('',#28807);
#6788=VERTEX_POINT('',#28818);
#6789=VERTEX_POINT('',#28820);
#6790=VERTEX_POINT('',#28835);
#6791=VERTEX_POINT('',#28837);
#6792=VERTEX_POINT('',#28844);
#6793=VERTEX_POINT('',#28846);
#6794=VERTEX_POINT('',#28862);
#6795=VERTEX_POINT('',#28864);
#6796=VERTEX_POINT('',#28917);
#6797=VERTEX_POINT('',#28919);
#6798=VERTEX_POINT('',#28935);
#6799=VERTEX_POINT('',#28937);
#6800=VERTEX_POINT('',#28978);
#6801=VERTEX_POINT('',#28980);
#6802=VERTEX_POINT('',#28998);
#6803=VERTEX_POINT('',#29000);
#6804=VERTEX_POINT('',#29007);
#6805=VERTEX_POINT('',#29009);
#6806=VERTEX_POINT('',#29028);
#6807=VERTEX_POINT('',#29030);
#6808=VERTEX_POINT('',#29039);
#6809=VERTEX_POINT('',#29041);
#6810=VERTEX_POINT('',#29059);
#6811=VERTEX_POINT('',#29061);
#6812=VERTEX_POINT('',#29070);
#6813=VERTEX_POINT('',#29072);
#6814=VERTEX_POINT('',#29088);
#6815=VERTEX_POINT('',#29090);
#6816=VERTEX_POINT('',#29099);
#6817=VERTEX_POINT('',#29101);
#6818=VERTEX_POINT('',#29119);
#6819=VERTEX_POINT('',#29121);
#6820=VERTEX_POINT('',#29171);
#6821=VERTEX_POINT('',#29173);
#6822=VERTEX_POINT('',#29192);
#6823=VERTEX_POINT('',#29194);
#6824=VERTEX_POINT('',#29244);
#6825=VERTEX_POINT('',#29246);
#6826=VERTEX_POINT('',#29265);
#6827=VERTEX_POINT('',#29267);
#6828=VERTEX_POINT('',#29276);
#6829=VERTEX_POINT('',#29278);
#6830=VERTEX_POINT('',#29300);
#6831=VERTEX_POINT('',#29302);
#6832=VERTEX_POINT('',#29311);
#6833=VERTEX_POINT('',#29313);
#6834=VERTEX_POINT('',#29332);
#6835=VERTEX_POINT('',#29334);
#6836=VERTEX_POINT('',#29390);
#6837=VERTEX_POINT('',#29392);
#6838=VERTEX_POINT('',#29412);
#6839=VERTEX_POINT('',#29414);
#6840=VERTEX_POINT('',#29423);
#6841=VERTEX_POINT('',#29425);
#6842=VERTEX_POINT('',#29936);
#6843=VERTEX_POINT('',#29947);
#6844=VERTEX_POINT('',#29954);
#6845=VERTEX_POINT('',#29969);
#6846=VERTEX_POINT('',#30570);
#6847=VERTEX_POINT('',#30577);
#6848=VERTEX_POINT('',#30588);
#6849=VERTEX_POINT('',#30603);
#6850=VERTEX_POINT('',#30617);
#6851=VERTEX_POINT('',#30626);
#6852=VERTEX_POINT('',#30637);
#6853=VERTEX_POINT('',#30654);
#6854=VERTEX_POINT('',#31187);
#6855=VERTEX_POINT('',#31198);
#6856=VERTEX_POINT('',#31209);
#6857=VERTEX_POINT('',#31224);
#6858=VERTEX_POINT('',#31881);
#6859=VERTEX_POINT('',#31888);
#6860=VERTEX_POINT('',#31899);
#6861=VERTEX_POINT('',#31914);
#6862=VERTEX_POINT('',#32472);
#6863=VERTEX_POINT('',#32483);
#6864=VERTEX_POINT('',#32494);
#6865=VERTEX_POINT('',#32509);
#6866=VERTEX_POINT('',#33250);
#6867=VERTEX_POINT('',#33257);
#6868=VERTEX_POINT('',#33264);
#6869=VERTEX_POINT('',#33279);
#6870=VERTEX_POINT('',#33879);
#6871=VERTEX_POINT('',#33888);
#6872=VERTEX_POINT('',#33895);
#6873=VERTEX_POINT('',#33910);
#6874=VERTEX_POINT('',#34441);
#6875=VERTEX_POINT('',#34450);
#6876=VERTEX_POINT('',#34457);
#6877=VERTEX_POINT('',#34472);
#6878=VERTEX_POINT('',#35168);
#6879=VERTEX_POINT('',#35175);
#6880=VERTEX_POINT('',#35182);
#6881=VERTEX_POINT('',#35197);
#6882=VERTEX_POINT('',#35730);
#6883=VERTEX_POINT('',#35739);
#6884=VERTEX_POINT('',#35746);
#6885=VERTEX_POINT('',#35761);
#6886=VERTEX_POINT('',#36275);
#6887=VERTEX_POINT('',#36288);
#6888=VERTEX_POINT('',#36295);
#6889=VERTEX_POINT('',#36310);
#6890=VERTEX_POINT('',#37009);
#6891=VERTEX_POINT('',#37018);
#6892=VERTEX_POINT('',#37029);
#6893=VERTEX_POINT('',#37044);
#6894=VERTEX_POINT('',#37544);
#6895=VERTEX_POINT('',#37553);
#6896=VERTEX_POINT('',#37560);
#6897=VERTEX_POINT('',#37575);
#6898=VERTEX_POINT('',#38120);
#6899=VERTEX_POINT('',#38127);
#6900=VERTEX_POINT('',#38134);
#6901=VERTEX_POINT('',#38149);
#6902=VERTEX_POINT('',#38591);
#6903=VERTEX_POINT('',#38598);
#6904=VERTEX_POINT('',#38605);
#6905=VERTEX_POINT('',#38620);
#6906=VERTEX_POINT('',#39193);
#6907=VERTEX_POINT('',#39202);
#6908=VERTEX_POINT('',#39209);
#6909=VERTEX_POINT('',#39224);
#6910=VERTEX_POINT('',#39766);
#6911=VERTEX_POINT('',#39775);
#6912=VERTEX_POINT('',#39782);
#6913=VERTEX_POINT('',#39797);
#6914=VERTEX_POINT('',#40442);
#6915=VERTEX_POINT('',#40449);
#6916=VERTEX_POINT('',#40460);
#6917=VERTEX_POINT('',#40475);
#6918=VERTEX_POINT('',#40917);
#6919=VERTEX_POINT('',#40924);
#6920=VERTEX_POINT('',#40931);
#6921=VERTEX_POINT('',#40946);
#6922=VERTEX_POINT('',#41547);
#6923=VERTEX_POINT('',#41554);
#6924=VERTEX_POINT('',#41561);
#6925=VERTEX_POINT('',#41576);
#6926=VERTEX_POINT('',#42032);
#6927=VERTEX_POINT('',#42039);
#6928=VERTEX_POINT('',#42046);
#6929=VERTEX_POINT('',#42061);
#6930=VERTEX_POINT('',#42508);
#6931=VERTEX_POINT('',#42515);
#6932=VERTEX_POINT('',#42522);
#6933=VERTEX_POINT('',#42537);
#6934=VERTEX_POINT('',#42993);
#6935=VERTEX_POINT('',#43004);
#6936=VERTEX_POINT('',#43011);
#6937=VERTEX_POINT('',#43026);
#6938=VERTEX_POINT('',#43543);
#6939=VERTEX_POINT('',#43550);
#6940=VERTEX_POINT('',#43557);
#6941=VERTEX_POINT('',#43572);
#6942=VERTEX_POINT('',#44042);
#6943=VERTEX_POINT('',#44051);
#6944=VERTEX_POINT('',#44058);
#6945=VERTEX_POINT('',#44073);
#6946=VERTEX_POINT('',#44648);
#6947=VERTEX_POINT('',#44655);
#6948=VERTEX_POINT('',#44662);
#6949=VERTEX_POINT('',#44677);
#6950=VERTEX_POINT('',#45105);
#6951=VERTEX_POINT('',#45112);
#6952=VERTEX_POINT('',#45119);
#6953=VERTEX_POINT('',#45134);
#6954=VERTEX_POINT('',#45583);
#6955=VERTEX_POINT('',#45592);
#6956=VERTEX_POINT('',#45603);
#6957=VERTEX_POINT('',#45618);
#6958=VERTEX_POINT('',#46020);
#6959=VERTEX_POINT('',#46029);
#6960=VERTEX_POINT('',#46036);
#6961=VERTEX_POINT('',#46051);
#6962=VERTEX_POINT('',#46512);
#6963=VERTEX_POINT('',#46519);
#6964=VERTEX_POINT('',#46530);
#6965=VERTEX_POINT('',#46545);
#6966=VERTEX_POINT('',#47015);
#6967=VERTEX_POINT('',#47022);
#6968=VERTEX_POINT('',#47029);
#6969=VERTEX_POINT('',#47044);
#6970=VERTEX_POINT('',#47535);
#6971=VERTEX_POINT('',#47542);
#6972=VERTEX_POINT('',#47553);
#6973=VERTEX_POINT('',#47568);
#6974=VERTEX_POINT('',#47900);
#6975=VERTEX_POINT('',#47907);
#6976=VERTEX_POINT('',#47914);
#6977=VERTEX_POINT('',#47929);
#6978=VERTEX_POINT('',#48474);
#6979=VERTEX_POINT('',#48483);
#6980=VERTEX_POINT('',#48494);
#6981=VERTEX_POINT('',#48509);
#6982=VERTEX_POINT('',#48967);
#6983=VERTEX_POINT('',#48978);
#6984=VERTEX_POINT('',#48985);
#6985=VERTEX_POINT('',#49000);
#6986=VERTEX_POINT('',#49531);
#6987=VERTEX_POINT('',#49540);
#6988=VERTEX_POINT('',#49547);
#6989=VERTEX_POINT('',#49562);
#6990=VERTEX_POINT('',#50020);
#6991=VERTEX_POINT('',#50031);
#6992=VERTEX_POINT('',#50038);
#6993=VERTEX_POINT('',#50053);
#6994=VERTEX_POINT('',#50502);
#6995=VERTEX_POINT('',#50509);
#6996=VERTEX_POINT('',#50516);
#6997=VERTEX_POINT('',#50531);
#6998=VERTEX_POINT('',#50959);
#6999=VERTEX_POINT('',#50968);
#7000=VERTEX_POINT('',#50975);
#7001=VERTEX_POINT('',#50990);
#7002=VERTEX_POINT('',#51451);
#7003=VERTEX_POINT('',#51458);
#7004=VERTEX_POINT('',#51465);
#7005=VERTEX_POINT('',#51480);
#7006=VERTEX_POINT('',#51978);
#7007=VERTEX_POINT('',#51987);
#7008=VERTEX_POINT('',#51994);
#7009=VERTEX_POINT('',#52009);
#7010=VERTEX_POINT('',#52668);
#7011=VERTEX_POINT('',#52677);
#7012=VERTEX_POINT('',#52684);
#7013=VERTEX_POINT('',#52699);
#7014=VERTEX_POINT('',#53141);
#7015=VERTEX_POINT('',#53148);
#7016=VERTEX_POINT('',#53155);
#7017=VERTEX_POINT('',#53170);
#7018=VERTEX_POINT('',#53715);
#7019=VERTEX_POINT('',#53722);
#7020=VERTEX_POINT('',#53729);
#7021=VERTEX_POINT('',#53744);
#7022=VERTEX_POINT('',#54214);
#7023=VERTEX_POINT('',#54221);
#7024=VERTEX_POINT('',#54228);
#7025=VERTEX_POINT('',#54243);
#7026=VERTEX_POINT('',#54760);
#7027=VERTEX_POINT('',#54771);
#7028=VERTEX_POINT('',#54778);
#7029=VERTEX_POINT('',#54793);
#7030=VERTEX_POINT('',#55293);
#7031=VERTEX_POINT('',#55300);
#7032=VERTEX_POINT('',#55307);
#7033=VERTEX_POINT('',#55322);
#7034=VERTEX_POINT('',#55839);
#7035=VERTEX_POINT('',#55850);
#7036=VERTEX_POINT('',#55857);
#7037=VERTEX_POINT('',#55872);
#7038=VERTEX_POINT('',#56512);
#7039=VERTEX_POINT('',#56523);
#7040=VERTEX_POINT('',#56530);
#7041=VERTEX_POINT('',#56545);
#7042=VERTEX_POINT('',#57190);
#7043=VERTEX_POINT('',#57199);
#7044=VERTEX_POINT('',#57206);
#7045=VERTEX_POINT('',#57221);
#7046=VERTEX_POINT('',#57761);
#7047=VERTEX_POINT('',#57772);
#7048=VERTEX_POINT('',#57783);
#7049=VERTEX_POINT('',#57798);
#7050=VERTEX_POINT('',#58245);
#7051=VERTEX_POINT('',#58254);
#7052=VERTEX_POINT('',#58261);
#7053=VERTEX_POINT('',#58276);
#7054=VERTEX_POINT('',#58818);
#7055=VERTEX_POINT('',#58829);
#7056=VERTEX_POINT('',#58840);
#7057=VERTEX_POINT('',#58855);
#7058=VERTEX_POINT('',#59596);
#7059=VERTEX_POINT('',#59605);
#7060=VERTEX_POINT('',#59616);
#7061=VERTEX_POINT('',#59631);
#7062=VERTEX_POINT('',#60227);
#7063=VERTEX_POINT('',#60236);
#7064=VERTEX_POINT('',#60243);
#7065=VERTEX_POINT('',#60258);
#7066=VERTEX_POINT('',#60705);
#7067=VERTEX_POINT('',#60714);
#7068=VERTEX_POINT('',#60721);
#7069=VERTEX_POINT('',#60736);
#7070=VERTEX_POINT('',#60754);
#7071=VERTEX_POINT('',#61291);
#7072=VERTEX_POINT('',#61300);
#7073=VERTEX_POINT('',#61307);
#7074=VERTEX_POINT('',#62042);
#7075=VERTEX_POINT('',#62049);
#7076=VERTEX_POINT('',#62056);
#7077=VERTEX_POINT('',#62071);
#7078=VERTEX_POINT('',#62085);
#7079=VERTEX_POINT('',#62096);
#7080=VERTEX_POINT('',#62543);
#7081=VERTEX_POINT('',#62550);
#7082=VERTEX_POINT('',#63084);
#7083=VERTEX_POINT('',#63085);
#7084=VERTEX_POINT('',#63087);
#7085=VERTEX_POINT('',#63089);
#7086=VERTEX_POINT('',#63091);
#7087=VERTEX_POINT('',#63095);
#7088=VERTEX_POINT('',#63101);
#7089=VERTEX_POINT('',#63103);
#7090=VERTEX_POINT('',#63107);
#7091=VERTEX_POINT('',#63109);
#7092=VERTEX_POINT('',#63113);
#7093=VERTEX_POINT('',#63115);
#7094=VERTEX_POINT('',#63121);
#7095=VERTEX_POINT('',#63127);
#7096=VERTEX_POINT('',#63131);
#7097=VERTEX_POINT('',#63135);
#7098=VERTEX_POINT('',#63138);
#7099=VERTEX_POINT('',#63142);
#7100=VERTEX_POINT('',#63146);
#7101=VERTEX_POINT('',#63149);
#7102=VERTEX_POINT('',#63153);
#7103=VERTEX_POINT('',#63156);
#7104=VERTEX_POINT('',#63160);
#7105=VERTEX_POINT('',#63164);
#7106=VERTEX_POINT('',#63167);
#7107=VERTEX_POINT('',#63171);
#7108=VERTEX_POINT('',#63181);
#7109=VERTEX_POINT('',#63183);
#7110=VERTEX_POINT('',#63186);
#7111=VERTEX_POINT('',#63190);
#7112=VERTEX_POINT('',#63194);
#7113=VERTEX_POINT('',#63198);
#7114=VERTEX_POINT('',#63201);
#7115=VERTEX_POINT('',#63205);
#7116=VERTEX_POINT('',#63208);
#7117=VERTEX_POINT('',#63212);
#7118=VERTEX_POINT('',#63216);
#7119=VERTEX_POINT('',#63223);
#7120=VERTEX_POINT('',#63225);
#7121=VERTEX_POINT('',#63229);
#7122=VERTEX_POINT('',#63232);
#7123=VERTEX_POINT('',#63236);
#7124=VERTEX_POINT('',#63239);
#7125=VERTEX_POINT('',#63241);
#7126=VERTEX_POINT('',#63245);
#7127=VERTEX_POINT('',#63248);
#7128=VERTEX_POINT('',#63257);
#7129=VERTEX_POINT('',#63258);
#7130=VERTEX_POINT('',#63260);
#7131=VERTEX_POINT('',#63340);
#7132=VERTEX_POINT('',#63398);
#7133=VERTEX_POINT('',#63399);
#7134=VERTEX_POINT('',#63401);
#7135=VERTEX_POINT('',#63539);
#7136=VERTEX_POINT('',#63675);
#7137=VERTEX_POINT('',#63676);
#7138=VERTEX_POINT('',#63678);
#7139=VERTEX_POINT('',#63816);
#7140=VERTEX_POINT('',#63955);
#7141=VERTEX_POINT('',#63956);
#7142=VERTEX_POINT('',#63958);
#7143=VERTEX_POINT('',#64093);
#7144=VERTEX_POINT('',#64232);
#7145=VERTEX_POINT('',#64233);
#7146=VERTEX_POINT('',#64235);
#7147=VERTEX_POINT('',#64373);
#7148=VERTEX_POINT('',#64512);
#7149=VERTEX_POINT('',#64513);
#7150=VERTEX_POINT('',#64515);
#7151=VERTEX_POINT('',#64653);
#7152=VERTEX_POINT('',#64789);
#7153=VERTEX_POINT('',#64790);
#7154=VERTEX_POINT('',#64837);
#7155=VERTEX_POINT('',#64839);
#7156=VERTEX_POINT('',#64865);
#7157=VERTEX_POINT('',#64999);
#7158=VERTEX_POINT('',#65010);
#7159=VERTEX_POINT('',#65022);
#7160=VERTEX_POINT('',#65033);
#7161=VERTEX_POINT('',#65044);
#7162=VERTEX_POINT('',#65178);
#7163=VERTEX_POINT('',#65180);
#7164=VERTEX_POINT('',#65191);
#7165=VERTEX_POINT('',#65202);
#7166=VERTEX_POINT('',#65213);
#7167=VERTEX_POINT('',#65225);
#7168=VERTEX_POINT('',#65370);
#7169=VERTEX_POINT('',#65405);
#7170=VERTEX_POINT('',#65473);
#7171=VERTEX_POINT('',#65475);
#7172=VERTEX_POINT('',#65557);
#7173=VERTEX_POINT('',#65562);
#7174=VERTEX_POINT('',#65754);
#7175=VERTEX_POINT('',#65891);
#7176=VERTEX_POINT('',#65893);
#7177=VERTEX_POINT('',#66143);
#7178=VERTEX_POINT('',#66217);
#7179=VERTEX_POINT('',#66218);
#7180=VERTEX_POINT('',#66222);
#7181=VERTEX_POINT('',#66226);
#7182=VERTEX_POINT('',#66230);
#7183=VERTEX_POINT('',#66234);
#7184=VERTEX_POINT('',#66238);
#7185=VERTEX_POINT('',#66245);
#7186=VERTEX_POINT('',#66249);
#7187=VERTEX_POINT('',#66251);
#7188=VERTEX_POINT('',#66255);
#7189=VERTEX_POINT('',#66259);
#7190=VERTEX_POINT('',#66263);
#7191=VERTEX_POINT('',#66264);
#7192=VERTEX_POINT('',#66268);
#7193=VERTEX_POINT('',#66272);
#7194=VERTEX_POINT('',#66279);
#7195=VERTEX_POINT('',#66284);
#7196=VERTEX_POINT('',#66288);
#7197=VERTEX_POINT('',#66292);
#7198=VERTEX_POINT('',#66295);
#7199=VERTEX_POINT('',#66299);
#7200=VERTEX_POINT('',#66303);
#7201=VERTEX_POINT('',#66309);
#7202=VERTEX_POINT('',#66311);
#7203=VERTEX_POINT('',#66315);
#7204=VERTEX_POINT('',#66318);
#7205=VERTEX_POINT('',#66322);
#7206=VERTEX_POINT('',#66326);
#7207=VERTEX_POINT('',#66330);
#7208=VERTEX_POINT('',#66333);
#7209=VERTEX_POINT('',#66340);
#7210=VERTEX_POINT('',#66342);
#7211=VERTEX_POINT('',#66346);
#7212=VERTEX_POINT('',#66349);
#7213=VERTEX_POINT('',#66353);
#7214=VERTEX_POINT('',#66357);
#7215=VERTEX_POINT('',#66360);
#7216=VERTEX_POINT('',#66364);
#7217=VERTEX_POINT('',#66368);
#7218=VERTEX_POINT('',#66375);
#7219=VERTEX_POINT('',#66377);
#7220=VERTEX_POINT('',#66381);
#7221=VERTEX_POINT('',#66383);
#7222=VERTEX_POINT('',#66388);
#7223=VERTEX_POINT('',#66390);
#7224=VERTEX_POINT('',#66394);
#7225=VERTEX_POINT('',#66397);
#7226=VERTEX_POINT('',#66401);
#7227=VERTEX_POINT('',#66404);
#7228=VERTEX_POINT('',#66407);
#7229=VERTEX_POINT('',#66409);
#7230=VERTEX_POINT('',#66413);
#7231=VERTEX_POINT('',#66417);
#7232=VERTEX_POINT('',#66420);
#7233=VERTEX_POINT('',#66424);
#7234=VERTEX_POINT('',#66429);
#7235=VERTEX_POINT('',#66433);
#7236=VERTEX_POINT('',#66437);
#7237=VERTEX_POINT('',#66441);
#7238=VERTEX_POINT('',#66446);
#7239=VERTEX_POINT('',#66452);
#7240=VERTEX_POINT('',#66454);
#7241=VERTEX_POINT('',#66458);
#7242=VERTEX_POINT('',#66462);
#7243=VERTEX_POINT('',#66465);
#7244=VERTEX_POINT('',#66469);
#7245=VERTEX_POINT('',#66472);
#7246=VERTEX_POINT('',#66476);
#7247=VERTEX_POINT('',#66479);
#7248=VERTEX_POINT('',#66483);
#7249=VERTEX_POINT('',#66487);
#7250=VERTEX_POINT('',#66491);
#7251=VERTEX_POINT('',#66494);
#7252=VERTEX_POINT('',#66498);
#7253=VERTEX_POINT('',#66501);
#7254=VERTEX_POINT('',#66505);
#7255=VERTEX_POINT('',#66511);
#7256=VERTEX_POINT('',#66513);
#7257=VERTEX_POINT('',#66516);
#7258=VERTEX_POINT('',#66520);
#7259=VERTEX_POINT('',#66524);
#7260=VERTEX_POINT('',#66528);
#7261=VERTEX_POINT('',#66531);
#7262=VERTEX_POINT('',#66535);
#7263=VERTEX_POINT('',#66538);
#7264=VERTEX_POINT('',#66542);
#7265=VERTEX_POINT('',#66546);
#7266=VERTEX_POINT('',#66553);
#7267=VERTEX_POINT('',#66555);
#7268=VERTEX_POINT('',#66559);
#7269=VERTEX_POINT('',#66563);
#7270=VERTEX_POINT('',#66564);
#7271=VERTEX_POINT('',#66566);
#7272=VERTEX_POINT('',#66568);
#7273=VERTEX_POINT('',#66570);
#7274=VERTEX_POINT('',#66572);
#7275=VERTEX_POINT('',#66574);
#7276=VERTEX_POINT('',#66576);
#7277=VERTEX_POINT('',#66579);
#7278=VERTEX_POINT('',#66582);
#7279=VERTEX_POINT('',#66586);
#7280=VERTEX_POINT('',#66587);
#7281=VERTEX_POINT('',#66589);
#7282=VERTEX_POINT('',#66591);
#7283=VERTEX_POINT('',#66593);
#7284=VERTEX_POINT('',#66595);
#7285=VERTEX_POINT('',#66597);
#7286=VERTEX_POINT('',#66599);
#7287=VERTEX_POINT('',#66602);
#7288=VERTEX_POINT('',#66605);
#7289=VERTEX_POINT('',#66609);
#7290=VERTEX_POINT('',#66632);
#7291=VERTEX_POINT('',#66633);
#7292=VERTEX_POINT('',#66635);
#7293=VERTEX_POINT('',#66712);
#7294=VERTEX_POINT('',#66764);
#7295=VERTEX_POINT('',#66765);
#7296=VERTEX_POINT('',#66767);
#7297=VERTEX_POINT('',#66972);
#7298=VERTEX_POINT('',#67164);
#7299=VERTEX_POINT('',#67165);
#7300=VERTEX_POINT('',#67594);
#7301=VERTEX_POINT('',#67595);
#7302=VERTEX_POINT('',#67597);
#7303=VERTEX_POINT('',#67816);
#7304=VERTEX_POINT('',#68110);
#7305=VERTEX_POINT('',#68111);
#7306=VERTEX_POINT('',#68546);
#7307=VERTEX_POINT('',#68547);
#7308=VERTEX_POINT('',#68549);
#7309=VERTEX_POINT('',#68784);
#7310=VERTEX_POINT('',#69038);
#7311=VERTEX_POINT('',#69039);
#7312=VERTEX_POINT('',#69466);
#7313=VERTEX_POINT('',#69467);
#7314=VERTEX_POINT('',#69469);
#7315=VERTEX_POINT('',#69694);
#7316=VERTEX_POINT('',#69974);
#7317=VERTEX_POINT('',#69975);
#7318=VERTEX_POINT('',#70402);
#7319=VERTEX_POINT('',#70403);
#7320=VERTEX_POINT('',#70405);
#7321=VERTEX_POINT('',#70624);
#7322=VERTEX_POINT('',#70860);
#7323=VERTEX_POINT('',#70861);
#7324=VERTEX_POINT('',#71290);
#7325=VERTEX_POINT('',#71291);
#7326=VERTEX_POINT('',#71293);
#7327=VERTEX_POINT('',#71353);
#7328=VERTEX_POINT('',#71563);
#7329=VERTEX_POINT('',#71564);
#7330=VERTEX_POINT('',#71566);
#7331=VERTEX_POINT('',#71884);
#7332=VERTEX_POINT('',#71885);
#7333=VERTEX_POINT('',#71887);
#7334=VERTEX_POINT('',#71925);
#7335=VERTEX_POINT('',#71992);
#7336=VERTEX_POINT('',#71993);
#7337=VERTEX_POINT('',#71995);
#7338=VERTEX_POINT('',#72174);
#7339=VERTEX_POINT('',#72353);
#7340=VERTEX_POINT('',#72354);
#7341=VERTEX_POINT('',#72775);
#7342=VERTEX_POINT('',#72776);
#7343=VERTEX_POINT('',#72778);
#7344=VERTEX_POINT('',#72838);
#7345=VERTEX_POINT('',#72903);
#7346=VERTEX_POINT('',#72904);
#7347=VERTEX_POINT('',#72906);
#7348=VERTEX_POINT('',#73073);
#7349=VERTEX_POINT('',#73168);
#7350=VERTEX_POINT('',#73169);
#7351=VERTEX_POINT('',#73379);
#7352=VERTEX_POINT('',#73581);
#7353=VERTEX_POINT('',#73582);
#7354=VERTEX_POINT('',#73623);
#7355=VERTEX_POINT('',#73625);
#7356=VERTEX_POINT('',#73648);
#7357=VERTEX_POINT('',#73767);
#7358=VERTEX_POINT('',#73778);
#7359=VERTEX_POINT('',#73897);
#7360=VERTEX_POINT('',#74013);
#7361=VERTEX_POINT('',#74024);
#7362=VERTEX_POINT('',#74143);
#7363=VERTEX_POINT('',#74259);
#7364=VERTEX_POINT('',#74270);
#7365=VERTEX_POINT('',#74386);
#7366=VERTEX_POINT('',#74398);
#7367=VERTEX_POINT('',#74409);
#7368=VERTEX_POINT('',#74525);
#7369=VERTEX_POINT('',#74536);
#7370=VERTEX_POINT('',#74655);
#7371=VERTEX_POINT('',#74666);
#7372=VERTEX_POINT('',#74677);
#7373=VERTEX_POINT('',#74793);
#7374=VERTEX_POINT('',#74804);
#7375=VERTEX_POINT('',#74815);
#7376=VERTEX_POINT('',#74817);
#7377=VERTEX_POINT('',#74819);
#7378=VERTEX_POINT('',#74821);
#7379=VERTEX_POINT('',#74831);
#7380=VERTEX_POINT('',#74842);
#7381=VERTEX_POINT('',#74854);
#7382=VERTEX_POINT('',#74970);
#7383=VERTEX_POINT('',#74981);
#7384=VERTEX_POINT('',#74993);
#7385=VERTEX_POINT('',#75109);
#7386=VERTEX_POINT('',#75120);
#7387=VERTEX_POINT('',#75236);
#7388=VERTEX_POINT('',#75248);
#7389=VERTEX_POINT('',#75259);
#7390=VERTEX_POINT('',#75375);
#7391=VERTEX_POINT('',#75387);
#7392=VERTEX_POINT('',#75506);
#7393=VERTEX_POINT('',#75625);
#7394=VERTEX_POINT('',#75637);
#7395=VERTEX_POINT('',#75753);
#7396=VERTEX_POINT('',#75775);
#7397=VERTEX_POINT('',#76008);
#7398=VERTEX_POINT('',#76010);
#7399=VERTEX_POINT('',#76105);
#7400=VERTEX_POINT('',#76162);
#7401=VERTEX_POINT('',#76792);
#7402=VERTEX_POINT('',#76794);
#7403=VERTEX_POINT('',#77360);
#7404=VERTEX_POINT('',#77364);
#7405=VERTEX_POINT('',#77367);
#7406=VERTEX_POINT('',#77368);
#7407=VERTEX_POINT('',#77372);
#7408=VERTEX_POINT('',#77376);
#7409=VERTEX_POINT('',#77380);
#7410=VERTEX_POINT('',#77384);
#7411=VERTEX_POINT('',#77388);
#7412=VERTEX_POINT('',#77395);
#7413=VERTEX_POINT('',#77399);
#7414=VERTEX_POINT('',#77401);
#7415=VERTEX_POINT('',#77405);
#7416=VERTEX_POINT('',#77409);
#7417=VERTEX_POINT('',#77413);
#7418=VERTEX_POINT('',#77414);
#7419=VERTEX_POINT('',#77418);
#7420=VERTEX_POINT('',#77422);
#7421=VERTEX_POINT('',#77429);
#7422=VERTEX_POINT('',#77431);
#7423=VERTEX_POINT('',#77435);
#7424=VERTEX_POINT('',#77440);
#7425=VERTEX_POINT('',#77448);
#7426=VERTEX_POINT('',#77449);
#7427=VERTEX_POINT('',#77451);
#7428=VERTEX_POINT('',#77528);
#7429=VERTEX_POINT('',#77580);
#7430=VERTEX_POINT('',#77581);
#7431=VERTEX_POINT('',#77583);
#7432=VERTEX_POINT('',#77770);
#7433=VERTEX_POINT('',#77809);
#7434=VERTEX_POINT('',#77810);
#7435=VERTEX_POINT('',#78012);
#7436=VERTEX_POINT('',#78181);
#7437=VERTEX_POINT('',#78182);
#7438=VERTEX_POINT('',#78184);
#7439=VERTEX_POINT('',#78592);
#7440=VERTEX_POINT('',#78593);
#7441=VERTEX_POINT('',#78793);
#7442=VERTEX_POINT('',#79041);
#7443=VERTEX_POINT('',#79042);
#7444=VERTEX_POINT('',#79044);
#7445=VERTEX_POINT('',#79448);
#7446=VERTEX_POINT('',#79449);
#7447=VERTEX_POINT('',#79641);
#7448=VERTEX_POINT('',#79777);
#7449=VERTEX_POINT('',#79778);
#7450=VERTEX_POINT('',#79780);
#7451=VERTEX_POINT('',#80013);
#7452=VERTEX_POINT('',#80052);
#7453=VERTEX_POINT('',#80053);
#7454=VERTEX_POINT('',#80247);
#7455=VERTEX_POINT('',#80415);
#7456=VERTEX_POINT('',#80416);
#7457=VERTEX_POINT('',#80418);
#7458=VERTEX_POINT('',#80822);
#7459=VERTEX_POINT('',#80823);
#7460=VERTEX_POINT('',#81023);
#7461=VERTEX_POINT('',#81237);
#7462=VERTEX_POINT('',#81238);
#7463=VERTEX_POINT('',#81240);
#7464=VERTEX_POINT('',#81636);
#7465=VERTEX_POINT('',#81637);
#7466=VERTEX_POINT('',#81829);
#7467=VERTEX_POINT('',#82033);
#7468=VERTEX_POINT('',#82034);
#7469=VERTEX_POINT('',#82036);
#7470=VERTEX_POINT('',#82438);
#7471=VERTEX_POINT('',#82439);
#7472=VERTEX_POINT('',#82639);
#7473=VERTEX_POINT('',#82853);
#7474=VERTEX_POINT('',#82854);
#7475=VERTEX_POINT('',#82861);
#7476=VERTEX_POINT('',#82863);
#7477=VERTEX_POINT('',#82869);
#7478=VERTEX_POINT('',#82988);
#7479=VERTEX_POINT('',#83107);
#7480=VERTEX_POINT('',#83226);
#7481=VERTEX_POINT('',#83342);
#7482=VERTEX_POINT('',#83353);
#7483=VERTEX_POINT('',#83364);
#7484=VERTEX_POINT('',#83376);
#7485=VERTEX_POINT('',#83495);
#7486=VERTEX_POINT('',#83614);
#7487=VERTEX_POINT('',#83730);
#7488=VERTEX_POINT('',#83741);
#7489=VERTEX_POINT('',#83752);
#7490=VERTEX_POINT('',#83764);
#7491=VERTEX_POINT('',#83883);
#7492=VERTEX_POINT('',#83894);
#7493=VERTEX_POINT('',#83896);
#7494=VERTEX_POINT('',#83898);
#7495=VERTEX_POINT('',#83900);
#7496=VERTEX_POINT('',#83910);
#7497=VERTEX_POINT('',#84029);
#7498=VERTEX_POINT('',#84145);
#7499=VERTEX_POINT('',#84261);
#7500=VERTEX_POINT('',#84272);
#7501=VERTEX_POINT('',#84284);
#7502=VERTEX_POINT('',#84295);
#7503=VERTEX_POINT('',#84414);
#7504=VERTEX_POINT('',#84533);
#7505=VERTEX_POINT('',#84649);
#7506=VERTEX_POINT('',#84660);
#7507=VERTEX_POINT('',#84671);
#7508=VERTEX_POINT('',#84683);
#7509=VERTEX_POINT('',#84921);
#7510=VERTEX_POINT('',#85082);
#7511=VERTEX_POINT('',#85084);
#7512=VERTEX_POINT('',#85179);
#7513=VERTEX_POINT('',#85239);
#7514=VERTEX_POINT('',#85769);
#7515=VERTEX_POINT('',#85771);
#7516=VERTEX_POINT('',#86240);
#7517=VERTEX_POINT('',#86244);
#7518=VERTEX_POINT('',#86247);
#7519=VERTEX_POINT('',#86248);
#7520=VERTEX_POINT('',#86252);
#7521=VERTEX_POINT('',#86256);
#7522=VERTEX_POINT('',#86260);
#7523=VERTEX_POINT('',#86264);
#7524=VERTEX_POINT('',#86268);
#7525=VERTEX_POINT('',#86275);
#7526=VERTEX_POINT('',#86279);
#7527=VERTEX_POINT('',#86281);
#7528=VERTEX_POINT('',#86285);
#7529=VERTEX_POINT('',#86289);
#7530=VERTEX_POINT('',#86293);
#7531=VERTEX_POINT('',#86294);
#7532=VERTEX_POINT('',#86298);
#7533=VERTEX_POINT('',#86302);
#7534=VERTEX_POINT('',#86309);
#7535=VERTEX_POINT('',#86311);
#7536=VERTEX_POINT('',#86315);
#7537=VERTEX_POINT('',#86320);
#7538=VERTEX_POINT('',#86328);
#7539=VERTEX_POINT('',#86330);
#7540=VERTEX_POINT('',#86334);
#7541=VERTEX_POINT('',#86337);
#7542=VERTEX_POINT('',#86341);
#7543=VERTEX_POINT('',#86345);
#7544=VERTEX_POINT('',#86348);
#7545=VERTEX_POINT('',#86352);
#7546=VERTEX_POINT('',#86356);
#7547=EDGE_CURVE('',#6001,#6002,#4281,.T.);
#7548=EDGE_CURVE('',#6001,#6003,#4282,.T.);
#7549=EDGE_CURVE('',#6003,#6004,#4283,.T.);
#7550=EDGE_CURVE('',#6002,#6004,#4284,.T.);
#7551=EDGE_CURVE('',#6005,#6001,#4285,.T.);
#7552=EDGE_CURVE('',#6005,#6006,#4286,.T.);
#7553=EDGE_CURVE('',#6006,#6003,#4287,.T.);
#7554=EDGE_CURVE('',#6007,#6005,#4288,.T.);
#7555=EDGE_CURVE('',#6007,#6008,#4289,.T.);
#7556=EDGE_CURVE('',#6008,#6006,#4290,.T.);
#7557=EDGE_CURVE('',#6002,#6007,#4291,.T.);
#7558=EDGE_CURVE('',#6004,#6008,#4292,.T.);
#7559=EDGE_CURVE('',#6009,#6010,#4293,.T.);
#7560=EDGE_CURVE('',#6011,#6009,#4294,.T.);
#7561=EDGE_CURVE('',#6011,#6012,#4295,.T.);
#7562=EDGE_CURVE('',#6012,#6010,#4296,.T.);
#7563=EDGE_CURVE('',#6010,#6013,#4297,.T.);
#7564=EDGE_CURVE('',#6014,#6012,#4298,.T.);
#7565=EDGE_CURVE('',#6015,#6014,#4299,.T.);
#7566=EDGE_CURVE('',#6016,#6015,#4300,.T.);
#7567=EDGE_CURVE('',#6013,#6016,#4301,.T.);
#7568=EDGE_CURVE('',#6017,#6011,#4302,.T.);
#7569=EDGE_CURVE('',#6017,#6014,#4303,.T.);
#7570=EDGE_CURVE('',#6018,#6017,#4304,.T.);
#7571=EDGE_CURVE('',#6018,#6015,#4305,.T.);
#7572=EDGE_CURVE('',#6016,#6019,#4306,.T.);
#7573=EDGE_CURVE('',#6019,#6018,#4307,.T.);
#7574=EDGE_CURVE('',#6020,#6021,#4308,.T.);
#7575=EDGE_CURVE('',#6020,#6022,#4309,.T.);
#7576=EDGE_CURVE('',#6022,#6023,#4310,.T.);
#7577=EDGE_CURVE('',#6021,#6023,#4311,.T.);
#7578=EDGE_CURVE('',#6024,#6020,#4312,.T.);
#7579=EDGE_CURVE('',#6024,#6025,#4313,.T.);
#7580=EDGE_CURVE('',#6025,#6022,#4314,.T.);
#7581=EDGE_CURVE('',#6026,#6024,#4315,.T.);
#7582=EDGE_CURVE('',#6026,#6027,#4316,.T.);
#7583=EDGE_CURVE('',#6027,#6025,#4317,.T.);
#7584=EDGE_CURVE('',#6021,#6026,#4318,.T.);
#7585=EDGE_CURVE('',#6023,#6027,#4319,.T.);
#7586=EDGE_CURVE('',#6028,#6029,#4320,.T.);
#7587=EDGE_CURVE('',#6028,#6030,#4321,.T.);
#7588=EDGE_CURVE('',#6030,#6031,#4322,.T.);
#7589=EDGE_CURVE('',#6029,#6031,#4323,.T.);
#7590=EDGE_CURVE('',#6032,#6028,#4324,.T.);
#7591=EDGE_CURVE('',#6032,#6033,#4325,.T.);
#7592=EDGE_CURVE('',#6033,#6030,#4326,.T.);
#7593=EDGE_CURVE('',#6034,#6032,#4327,.T.);
#7594=EDGE_CURVE('',#6034,#6035,#4328,.T.);
#7595=EDGE_CURVE('',#6035,#6033,#4329,.T.);
#7596=EDGE_CURVE('',#6029,#6034,#4330,.T.);
#7597=EDGE_CURVE('',#6031,#6035,#4331,.T.);
#7598=EDGE_CURVE('',#6036,#6037,#4332,.T.);
#7599=EDGE_CURVE('',#6036,#6038,#4333,.T.);
#7600=EDGE_CURVE('',#6038,#6039,#4334,.T.);
#7601=EDGE_CURVE('',#6037,#6039,#4335,.T.);
#7602=EDGE_CURVE('',#6040,#6036,#4336,.T.);
#7603=EDGE_CURVE('',#6040,#6041,#4337,.T.);
#7604=EDGE_CURVE('',#6041,#6038,#4338,.T.);
#7605=EDGE_CURVE('',#6042,#6040,#4339,.T.);
#7606=EDGE_CURVE('',#6042,#6043,#4340,.T.);
#7607=EDGE_CURVE('',#6043,#6041,#4341,.T.);
#7608=EDGE_CURVE('',#6037,#6042,#4342,.T.);
#7609=EDGE_CURVE('',#6039,#6043,#4343,.T.);
#7610=EDGE_CURVE('',#6044,#6045,#4344,.T.);
#7611=EDGE_CURVE('',#6044,#6046,#4345,.T.);
#7612=EDGE_CURVE('',#6047,#6046,#4346,.T.);
#7613=EDGE_CURVE('',#6045,#6047,#4347,.T.);
#7614=EDGE_CURVE('',#6048,#6049,#4348,.T.);
#7615=EDGE_CURVE('',#6050,#6048,#4349,.T.);
#7616=EDGE_CURVE('',#6050,#6051,#4350,.T.);
#7617=EDGE_CURVE('',#6051,#6049,#4351,.T.);
#7618=EDGE_CURVE('',#6052,#6050,#4352,.T.);
#7619=EDGE_CURVE('',#6052,#6053,#4353,.T.);
#7620=EDGE_CURVE('',#6053,#6051,#4354,.T.);
#7621=EDGE_CURVE('',#6047,#6052,#4355,.T.);
#7622=EDGE_CURVE('',#6046,#6053,#4356,.T.);
#7623=EDGE_CURVE('',#6054,#6044,#4357,.T.);
#7624=EDGE_CURVE('',#6049,#6054,#4358,.T.);
#7625=EDGE_CURVE('',#6013,#6055,#4359,.T.);
#7626=EDGE_CURVE('',#6055,#6056,#4360,.T.);
#7627=EDGE_CURVE('',#6056,#6057,#4361,.T.);
#7628=EDGE_CURVE('',#6009,#6057,#4362,.T.);
#7629=EDGE_CURVE('',#6058,#6019,#4363,.T.);
#7630=EDGE_CURVE('',#6059,#6058,#4364,.T.);
#7631=EDGE_CURVE('',#6055,#6059,#4365,.T.);
#7632=EDGE_CURVE('',#6057,#6060,#4366,.T.);
#7633=EDGE_CURVE('',#6061,#6060,#4367,.T.);
#7634=EDGE_CURVE('',#6062,#6061,#4368,.T.);
#7635=EDGE_CURVE('',#6063,#6062,#4369,.T.);
#7636=EDGE_CURVE('',#6063,#6064,#4370,.T.);
#7637=EDGE_CURVE('',#6064,#6045,#4371,.T.);
#7638=EDGE_CURVE('',#6048,#6065,#4372,.T.);
#7639=EDGE_CURVE('',#6066,#6065,#4373,.T.);
#7640=EDGE_CURVE('',#6067,#6066,#4374,.T.);
#7641=EDGE_CURVE('',#6058,#6067,#4375,.T.);
#7642=EDGE_CURVE('',#6068,#6068,#1754,.T.);
#7643=EDGE_CURVE('',#6069,#6070,#4376,.T.);
#7644=EDGE_CURVE('',#6069,#6071,#4377,.T.);
#7645=EDGE_CURVE('',#6071,#6072,#4378,.T.);
#7646=EDGE_CURVE('',#6070,#6072,#4379,.T.);
#7647=EDGE_CURVE('',#6073,#6069,#4380,.T.);
#7648=EDGE_CURVE('',#6073,#6074,#4381,.T.);
#7649=EDGE_CURVE('',#6074,#6071,#4382,.T.);
#7650=EDGE_CURVE('',#6075,#6073,#4383,.T.);
#7651=EDGE_CURVE('',#6075,#6076,#4384,.T.);
#7652=EDGE_CURVE('',#6076,#6074,#4385,.T.);
#7653=EDGE_CURVE('',#6070,#6075,#4386,.T.);
#7654=EDGE_CURVE('',#6072,#6076,#4387,.T.);
#7655=EDGE_CURVE('',#6077,#6078,#4388,.T.);
#7656=EDGE_CURVE('',#6077,#6079,#4389,.T.);
#7657=EDGE_CURVE('',#6080,#6079,#4390,.T.);
#7658=EDGE_CURVE('',#6078,#6080,#4391,.T.);
#7659=EDGE_CURVE('',#6081,#6082,#4392,.T.);
#7660=EDGE_CURVE('',#6081,#6083,#4393,.T.);
#7661=EDGE_CURVE('',#6083,#6084,#4394,.T.);
#7662=EDGE_CURVE('',#6082,#6084,#4395,.T.);
#7663=EDGE_CURVE('',#6080,#6081,#4396,.T.);
#7664=EDGE_CURVE('',#6079,#6083,#4397,.T.);
#7665=EDGE_CURVE('',#6085,#6086,#4398,.T.);
#7666=EDGE_CURVE('',#6082,#6085,#4399,.T.);
#7667=EDGE_CURVE('',#6084,#6086,#4400,.T.);
#7668=EDGE_CURVE('',#6087,#6077,#4401,.T.);
#7669=EDGE_CURVE('',#6086,#6087,#4402,.T.);
#7670=EDGE_CURVE('',#6088,#6089,#4403,.T.);
#7671=EDGE_CURVE('',#6088,#6090,#4404,.T.);
#7672=EDGE_CURVE('',#6090,#6091,#4405,.T.);
#7673=EDGE_CURVE('',#6089,#6091,#4406,.T.);
#7674=EDGE_CURVE('',#6092,#6088,#4407,.T.);
#7675=EDGE_CURVE('',#6092,#6093,#4408,.T.);
#7676=EDGE_CURVE('',#6093,#6090,#4409,.T.);
#7677=EDGE_CURVE('',#6094,#6092,#4410,.T.);
#7678=EDGE_CURVE('',#6094,#6095,#4411,.T.);
#7679=EDGE_CURVE('',#6095,#6093,#4412,.T.);
#7680=EDGE_CURVE('',#6089,#6094,#4413,.T.);
#7681=EDGE_CURVE('',#6091,#6095,#4414,.T.);
#7682=EDGE_CURVE('',#6096,#6097,#4415,.T.);
#7683=EDGE_CURVE('',#6096,#6098,#4416,.T.);
#7684=EDGE_CURVE('',#6098,#6099,#4417,.T.);
#7685=EDGE_CURVE('',#6097,#6099,#4418,.T.);
#7686=EDGE_CURVE('',#6100,#6096,#4419,.T.);
#7687=EDGE_CURVE('',#6100,#6101,#4420,.T.);
#7688=EDGE_CURVE('',#6101,#6098,#4421,.T.);
#7689=EDGE_CURVE('',#6102,#6100,#4422,.T.);
#7690=EDGE_CURVE('',#6102,#6103,#4423,.T.);
#7691=EDGE_CURVE('',#6103,#6101,#4424,.T.);
#7692=EDGE_CURVE('',#6097,#6102,#4425,.T.);
#7693=EDGE_CURVE('',#6099,#6103,#4426,.T.);
#7694=EDGE_CURVE('',#6104,#6105,#4427,.T.);
#7695=EDGE_CURVE('',#6104,#6106,#4428,.T.);
#7696=EDGE_CURVE('',#6106,#6107,#4429,.T.);
#7697=EDGE_CURVE('',#6105,#6107,#4430,.T.);
#7698=EDGE_CURVE('',#6108,#6104,#4431,.T.);
#7699=EDGE_CURVE('',#6108,#6109,#4432,.T.);
#7700=EDGE_CURVE('',#6109,#6106,#4433,.T.);
#7701=EDGE_CURVE('',#6110,#6108,#4434,.T.);
#7702=EDGE_CURVE('',#6110,#6111,#4435,.T.);
#7703=EDGE_CURVE('',#6111,#6109,#4436,.T.);
#7704=EDGE_CURVE('',#6105,#6110,#4437,.T.);
#7705=EDGE_CURVE('',#6107,#6111,#4438,.T.);
#7706=EDGE_CURVE('',#6112,#6113,#4439,.T.);
#7707=EDGE_CURVE('',#6112,#6114,#4440,.T.);
#7708=EDGE_CURVE('',#6115,#6114,#4441,.T.);
#7709=EDGE_CURVE('',#6113,#6115,#4442,.T.);
#7710=EDGE_CURVE('',#6115,#6116,#4443,.T.);
#7711=EDGE_CURVE('',#6114,#6117,#4444,.T.);
#7712=EDGE_CURVE('',#6116,#6117,#4445,.T.);
#7713=EDGE_CURVE('',#6118,#6119,#4446,.T.);
#7714=EDGE_CURVE('',#6120,#6118,#4447,.T.);
#7715=EDGE_CURVE('',#6120,#6121,#4448,.T.);
#7716=EDGE_CURVE('',#6121,#6119,#4449,.T.);
#7717=EDGE_CURVE('',#6116,#6120,#4450,.T.);
#7718=EDGE_CURVE('',#6117,#6121,#4451,.T.);
#7719=EDGE_CURVE('',#6122,#6112,#4452,.T.);
#7720=EDGE_CURVE('',#6119,#6122,#4453,.T.);
#7721=EDGE_CURVE('',#6123,#6078,#4454,.T.);
#7722=EDGE_CURVE('',#6123,#6124,#4455,.T.);
#7723=EDGE_CURVE('',#6124,#6125,#4456,.T.);
#7724=EDGE_CURVE('',#6125,#6087,#4457,.T.);
#7725=EDGE_CURVE('',#6126,#6113,#4458,.T.);
#7726=EDGE_CURVE('',#6127,#6126,#4459,.T.);
#7727=EDGE_CURVE('',#6128,#6127,#4460,.T.);
#7728=EDGE_CURVE('',#6128,#6122,#4461,.T.);
#7729=EDGE_CURVE('',#6085,#6129,#4462,.T.);
#7730=EDGE_CURVE('',#6130,#6129,#4463,.T.);
#7731=EDGE_CURVE('',#6131,#6130,#4464,.T.);
#7732=EDGE_CURVE('',#6131,#6132,#1755,.T.);
#7733=EDGE_CURVE('',#6132,#6133,#1756,.T.);
#7734=EDGE_CURVE('',#6134,#6133,#4465,.T.);
#7735=EDGE_CURVE('',#6134,#6135,#1757,.T.);
#7736=EDGE_CURVE('',#6135,#6136,#1758,.T.);
#7737=EDGE_CURVE('',#6137,#6136,#4466,.T.);
#7738=EDGE_CURVE('',#6126,#6137,#4467,.T.);
#7739=EDGE_CURVE('',#6118,#6138,#4468,.T.);
#7740=EDGE_CURVE('',#6138,#6139,#4469,.T.);
#7741=EDGE_CURVE('',#6140,#6139,#4470,.T.);
#7742=EDGE_CURVE('',#6141,#6140,#4471,.T.);
#7743=EDGE_CURVE('',#6142,#6141,#4472,.T.);
#7744=EDGE_CURVE('',#6142,#6123,#4473,.T.);
#7745=EDGE_CURVE('',#6143,#6143,#1759,.T.);
#7746=EDGE_CURVE('',#6144,#6144,#1760,.T.);
#7747=EDGE_CURVE('',#6145,#6145,#1761,.T.);
#7748=EDGE_CURVE('',#6146,#6147,#1762,.T.);
#7749=EDGE_CURVE('',#6146,#6148,#4474,.T.);
#7750=EDGE_CURVE('',#6148,#6149,#1763,.T.);
#7751=EDGE_CURVE('',#6147,#6149,#4475,.T.);
#7752=EDGE_CURVE('',#6150,#6146,#1764,.T.);
#7753=EDGE_CURVE('',#6150,#6151,#4476,.T.);
#7754=EDGE_CURVE('',#6151,#6148,#1765,.T.);
#7755=EDGE_CURVE('',#6152,#6150,#4477,.T.);
#7756=EDGE_CURVE('',#6152,#6153,#4478,.T.);
#7757=EDGE_CURVE('',#6153,#6151,#4479,.T.);
#7758=EDGE_CURVE('',#6154,#6152,#4480,.T.);
#7759=EDGE_CURVE('',#6154,#6155,#4481,.T.);
#7760=EDGE_CURVE('',#6155,#6153,#4482,.T.);
#7761=EDGE_CURVE('',#6156,#6154,#4483,.T.);
#7762=EDGE_CURVE('',#6156,#6157,#4484,.T.);
#7763=EDGE_CURVE('',#6157,#6155,#4485,.T.);
#7764=EDGE_CURVE('',#6147,#6156,#1766,.T.);
#7765=EDGE_CURVE('',#6149,#6157,#1767,.T.);
#7766=EDGE_CURVE('',#6158,#6159,#4486,.T.);
#7767=EDGE_CURVE('',#6158,#6160,#4487,.T.);
#7768=EDGE_CURVE('',#6160,#6161,#4488,.T.);
#7769=EDGE_CURVE('',#6159,#6161,#4489,.T.);
#7770=EDGE_CURVE('',#6162,#6158,#4490,.T.);
#7771=EDGE_CURVE('',#6162,#6163,#4491,.T.);
#7772=EDGE_CURVE('',#6163,#6160,#4492,.T.);
#7773=EDGE_CURVE('',#6164,#6162,#4493,.T.);
#7774=EDGE_CURVE('',#6164,#6165,#4494,.T.);
#7775=EDGE_CURVE('',#6165,#6163,#4495,.T.);
#7776=EDGE_CURVE('',#6161,#6166,#1768,.T.);
#7777=EDGE_CURVE('',#6167,#6165,#1769,.T.);
#7778=EDGE_CURVE('',#6166,#6167,#1770,.T.);
#7779=EDGE_CURVE('',#6159,#6168,#1771,.T.);
#7780=EDGE_CURVE('',#6168,#6169,#1772,.T.);
#7781=EDGE_CURVE('',#6169,#6170,#1773,.T.);
#7782=EDGE_CURVE('',#6170,#6127,#4496,.T.);
#7783=EDGE_CURVE('',#6171,#6137,#1774,.T.);
#7784=EDGE_CURVE('',#6171,#6172,#4497,.T.);
#7785=EDGE_CURVE('',#6066,#6172,#1775,.T.);
#7786=EDGE_CURVE('',#6065,#6173,#4498,.T.);
#7787=EDGE_CURVE('',#6173,#6174,#4499,.T.);
#7788=EDGE_CURVE('',#6174,#6175,#1776,.T.);
#7789=EDGE_CURVE('',#6175,#6176,#1777,.T.);
#7790=EDGE_CURVE('',#6176,#6164,#1778,.T.);
#7791=EDGE_CURVE('',#6177,#6178,#1779,.T.);
#7792=EDGE_CURVE('',#6178,#6179,#363,.T.);
#7793=EDGE_CURVE('',#6179,#6180,#1780,.T.);
#7794=EDGE_CURVE('',#6177,#6180,#364,.T.);
#7795=EDGE_CURVE('',#6178,#6181,#1781,.T.);
#7796=EDGE_CURVE('',#6181,#6182,#359,.T.);
#7797=EDGE_CURVE('',#6182,#6179,#1782,.T.);
#7798=EDGE_CURVE('',#6181,#6183,#4500,.T.);
#7799=EDGE_CURVE('',#6183,#6184,#360,.T.);
#7800=EDGE_CURVE('',#6184,#6182,#4501,.T.);
#7801=EDGE_CURVE('',#6183,#6185,#1783,.T.);
#7802=EDGE_CURVE('',#6185,#6186,#365,.T.);
#7803=EDGE_CURVE('',#6186,#6184,#1784,.T.);
#7804=EDGE_CURVE('',#6185,#6187,#1785,.T.);
#7805=EDGE_CURVE('',#6187,#6188,#366,.T.);
#7806=EDGE_CURVE('',#6188,#6186,#1786,.T.);
#7807=EDGE_CURVE('',#6187,#6189,#1787,.T.);
#7808=EDGE_CURVE('',#6189,#6190,#361,.T.);
#7809=EDGE_CURVE('',#6190,#6188,#1788,.T.);
#7810=EDGE_CURVE('',#6189,#6191,#4502,.T.);
#7811=EDGE_CURVE('',#6191,#6192,#362,.T.);
#7812=EDGE_CURVE('',#6192,#6190,#4503,.T.);
#7813=EDGE_CURVE('',#6193,#6192,#1789,.T.);
#7814=EDGE_CURVE('',#6191,#6194,#1790,.T.);
#7815=EDGE_CURVE('',#6194,#6193,#367,.T.);
#7816=EDGE_CURVE('',#6195,#6193,#1791,.T.);
#7817=EDGE_CURVE('',#6194,#6196,#1792,.T.);
#7818=EDGE_CURVE('',#6196,#6195,#368,.T.);
#7819=EDGE_CURVE('',#6197,#6195,#1793,.T.);
#7820=EDGE_CURVE('',#6196,#6198,#1794,.T.);
#7821=EDGE_CURVE('',#6198,#6197,#369,.T.);
#7822=EDGE_CURVE('',#6199,#6197,#1795,.T.);
#7823=EDGE_CURVE('',#6198,#6200,#1796,.T.);
#7824=EDGE_CURVE('',#6200,#6199,#370,.T.);
#7825=EDGE_CURVE('',#6180,#6199,#1797,.T.);
#7826=EDGE_CURVE('',#6200,#6177,#1798,.T.);
#7827=EDGE_CURVE('',#6175,#6193,#4504,.T.);
#7828=EDGE_CURVE('',#6174,#6192,#4505,.T.);
#7829=EDGE_CURVE('',#6176,#6195,#4506,.T.);
#7830=EDGE_CURVE('',#6197,#6167,#4507,.T.);
#7831=EDGE_CURVE('',#6199,#6166,#4508,.T.);
#7832=EDGE_CURVE('',#6168,#6180,#4509,.T.);
#7833=EDGE_CURVE('',#6169,#6179,#4510,.T.);
#7834=EDGE_CURVE('',#6201,#6201,#1799,.T.);
#7835=EDGE_CURVE('',#6202,#6202,#1800,.T.);
#7836=EDGE_CURVE('',#6203,#6203,#1801,.T.);
#7837=EDGE_CURVE('',#6204,#6204,#1802,.T.);
#7838=EDGE_CURVE('',#6205,#6205,#1803,.T.);
#7839=EDGE_CURVE('',#6206,#6207,#371,.T.);
#7840=EDGE_CURVE('',#6207,#6206,#372,.T.);
#7841=EDGE_CURVE('',#6207,#6208,#4511,.T.);
#7842=EDGE_CURVE('',#6208,#6208,#1804,.T.);
#7843=EDGE_CURVE('',#6208,#6209,#4512,.T.);
#7844=EDGE_CURVE('',#6209,#6209,#1805,.T.);
#7845=EDGE_CURVE('',#6210,#6211,#4513,.T.);
#7846=EDGE_CURVE('',#6211,#6211,#1806,.T.);
#7847=EDGE_CURVE('',#6211,#6212,#4514,.T.);
#7848=EDGE_CURVE('',#6213,#6212,#373,.T.);
#7849=EDGE_CURVE('',#6214,#6213,#374,.T.);
#7850=EDGE_CURVE('',#6214,#6215,#4515,.T.);
#7851=EDGE_CURVE('',#6215,#6215,#1807,.T.);
#7852=EDGE_CURVE('',#6212,#6214,#375,.T.);
#7853=EDGE_CURVE('',#6215,#6216,#4516,.T.);
#7854=EDGE_CURVE('',#6217,#6216,#1808,.T.);
#7855=EDGE_CURVE('',#6218,#6217,#376,.T.);
#7856=EDGE_CURVE('',#6216,#6218,#1809,.T.);
#7857=EDGE_CURVE('',#6219,#6218,#4517,.T.);
#7858=EDGE_CURVE('',#6220,#6219,#4518,.T.);
#7859=EDGE_CURVE('',#6221,#6220,#4519,.T.);
#7860=EDGE_CURVE('',#6221,#6222,#1810,.T.);
#7861=EDGE_CURVE('',#6222,#6223,#1811,.T.);
#7862=EDGE_CURVE('',#6224,#6223,#4520,.T.);
#7863=EDGE_CURVE('',#6224,#6225,#1812,.T.);
#7864=EDGE_CURVE('',#6225,#6226,#1813,.T.);
#7865=EDGE_CURVE('',#6172,#6226,#4521,.T.);
#7866=EDGE_CURVE('',#6227,#6171,#4522,.T.);
#7867=EDGE_CURVE('',#6227,#6228,#1814,.T.);
#7868=EDGE_CURVE('',#6228,#6229,#1815,.T.);
#7869=EDGE_CURVE('',#6217,#6229,#4523,.T.);
#7870=EDGE_CURVE('',#6230,#6231,#4524,.T.);
#7871=EDGE_CURVE('',#6231,#6232,#4525,.T.);
#7872=EDGE_CURVE('',#6232,#6233,#4526,.T.);
#7873=EDGE_CURVE('',#6233,#6230,#4527,.T.);
#7874=EDGE_CURVE('',#6234,#6235,#4528,.T.);
#7875=EDGE_CURVE('',#6235,#6236,#4529,.T.);
#7876=EDGE_CURVE('',#6236,#6237,#4530,.T.);
#7877=EDGE_CURVE('',#6237,#6234,#4531,.T.);
#7878=EDGE_CURVE('',#6238,#6239,#4532,.T.);
#7879=EDGE_CURVE('',#6239,#6240,#4533,.T.);
#7880=EDGE_CURVE('',#6240,#6241,#4534,.T.);
#7881=EDGE_CURVE('',#6241,#6238,#4535,.T.);
#7882=EDGE_CURVE('',#6242,#6243,#4536,.T.);
#7883=EDGE_CURVE('',#6243,#6244,#4537,.T.);
#7884=EDGE_CURVE('',#6244,#6245,#4538,.T.);
#7885=EDGE_CURVE('',#6245,#6242,#4539,.T.);
#7886=EDGE_CURVE('',#6246,#6247,#4540,.T.);
#7887=EDGE_CURVE('',#6247,#6248,#4541,.T.);
#7888=EDGE_CURVE('',#6248,#6249,#4542,.T.);
#7889=EDGE_CURVE('',#6249,#6246,#4543,.T.);
#7890=EDGE_CURVE('',#6250,#6251,#4544,.T.);
#7891=EDGE_CURVE('',#6251,#6252,#4545,.T.);
#7892=EDGE_CURVE('',#6252,#6253,#4546,.T.);
#7893=EDGE_CURVE('',#6253,#6250,#4547,.T.);
#7894=EDGE_CURVE('',#6254,#6255,#4548,.T.);
#7895=EDGE_CURVE('',#6255,#6255,#1816,.T.);
#7896=EDGE_CURVE('',#6255,#6256,#4549,.T.);
#7897=EDGE_CURVE('',#6256,#6256,#1817,.T.);
#7898=EDGE_CURVE('',#6257,#6258,#377,.T.);
#7899=EDGE_CURVE('',#6258,#6257,#378,.T.);
#7900=EDGE_CURVE('',#6256,#6228,#4550,.T.);
#7901=EDGE_CURVE('',#6229,#6227,#379,.T.);
#7902=EDGE_CURVE('',#6136,#6134,#380,.T.);
#7903=EDGE_CURVE('',#6133,#6131,#381,.T.);
#7904=EDGE_CURVE('',#6130,#6219,#1818,.T.);
#7905=EDGE_CURVE('',#6259,#6260,#4551,.T.);
#7906=EDGE_CURVE('',#6260,#6260,#1819,.T.);
#7907=EDGE_CURVE('',#6260,#6261,#4552,.T.);
#7908=EDGE_CURVE('',#6261,#6261,#1820,.T.);
#7909=EDGE_CURVE('',#6261,#6222,#4553,.T.);
#7910=EDGE_CURVE('',#6223,#6221,#382,.T.);
#7911=EDGE_CURVE('',#6220,#6067,#1821,.T.);
#7912=EDGE_CURVE('',#6226,#6224,#383,.T.);
#7913=EDGE_CURVE('',#6262,#6263,#4554,.T.);
#7914=EDGE_CURVE('',#6263,#6263,#1822,.T.);
#7915=EDGE_CURVE('',#6263,#6264,#4555,.T.);
#7916=EDGE_CURVE('',#6264,#6264,#1823,.T.);
#7917=EDGE_CURVE('',#6264,#6225,#4556,.T.);
#7918=EDGE_CURVE('',#6265,#6266,#4557,.T.);
#7919=EDGE_CURVE('',#6266,#6266,#1824,.T.);
#7920=EDGE_CURVE('',#6266,#6267,#4558,.T.);
#7921=EDGE_CURVE('',#6267,#6267,#1825,.T.);
#7922=EDGE_CURVE('',#6267,#6205,#4559,.T.);
#7923=EDGE_CURVE('',#6268,#6269,#4560,.T.);
#7924=EDGE_CURVE('',#6269,#6269,#1826,.T.);
#7925=EDGE_CURVE('',#6269,#6270,#4561,.T.);
#7926=EDGE_CURVE('',#6270,#6270,#1827,.T.);
#7927=EDGE_CURVE('',#6270,#6271,#4562,.T.);
#7928=EDGE_CURVE('',#6271,#6271,#1828,.T.);
#7929=EDGE_CURVE('',#6272,#6273,#4563,.T.);
#7930=EDGE_CURVE('',#6273,#6273,#1829,.T.);
#7931=EDGE_CURVE('',#6273,#6274,#4564,.T.);
#7932=EDGE_CURVE('',#6274,#6274,#1830,.T.);
#7933=EDGE_CURVE('',#6274,#6204,#4565,.T.);
#7934=EDGE_CURVE('',#6275,#6276,#4566,.T.);
#7935=EDGE_CURVE('',#6276,#6276,#1831,.T.);
#7936=EDGE_CURVE('',#6276,#6277,#4567,.T.);
#7937=EDGE_CURVE('',#6277,#6277,#1832,.T.);
#7938=EDGE_CURVE('',#6277,#6278,#4568,.T.);
#7939=EDGE_CURVE('',#6278,#6278,#1833,.T.);
#7940=EDGE_CURVE('',#6279,#6280,#4569,.T.);
#7941=EDGE_CURVE('',#6280,#6280,#1834,.T.);
#7942=EDGE_CURVE('',#6280,#6281,#4570,.T.);
#7943=EDGE_CURVE('',#6281,#6281,#1835,.T.);
#7944=EDGE_CURVE('',#6281,#6203,#4571,.T.);
#7945=EDGE_CURVE('',#6282,#6283,#4572,.T.);
#7946=EDGE_CURVE('',#6283,#6283,#1836,.T.);
#7947=EDGE_CURVE('',#6283,#6284,#4573,.T.);
#7948=EDGE_CURVE('',#6284,#6284,#1837,.T.);
#7949=EDGE_CURVE('',#6284,#6285,#4574,.T.);
#7950=EDGE_CURVE('',#6285,#6285,#1838,.T.);
#7951=EDGE_CURVE('',#6286,#6287,#4575,.T.);
#7952=EDGE_CURVE('',#6287,#6287,#1839,.T.);
#7953=EDGE_CURVE('',#6287,#6288,#4576,.T.);
#7954=EDGE_CURVE('',#6288,#6288,#1840,.T.);
#7955=EDGE_CURVE('',#6288,#6202,#4577,.T.);
#7956=EDGE_CURVE('',#6289,#6290,#4578,.T.);
#7957=EDGE_CURVE('',#6290,#6290,#1841,.T.);
#7958=EDGE_CURVE('',#6290,#6291,#4579,.T.);
#7959=EDGE_CURVE('',#6291,#6291,#1842,.T.);
#7960=EDGE_CURVE('',#6291,#6292,#4580,.T.);
#7961=EDGE_CURVE('',#6292,#6292,#1843,.T.);
#7962=EDGE_CURVE('',#6293,#6294,#4581,.T.);
#7963=EDGE_CURVE('',#6294,#6294,#1844,.T.);
#7964=EDGE_CURVE('',#6294,#6295,#4582,.T.);
#7965=EDGE_CURVE('',#6295,#6295,#1845,.T.);
#7966=EDGE_CURVE('',#6295,#6145,#4583,.T.);
#7967=EDGE_CURVE('',#6296,#6297,#4584,.T.);
#7968=EDGE_CURVE('',#6297,#6297,#1846,.T.);
#7969=EDGE_CURVE('',#6297,#6298,#4585,.T.);
#7970=EDGE_CURVE('',#6298,#6298,#1847,.T.);
#7971=EDGE_CURVE('',#6298,#6144,#4586,.T.);
#7972=EDGE_CURVE('',#6299,#6300,#4587,.T.);
#7973=EDGE_CURVE('',#6300,#6300,#1848,.T.);
#7974=EDGE_CURVE('',#6300,#6301,#4588,.T.);
#7975=EDGE_CURVE('',#6301,#6301,#1849,.T.);
#7976=EDGE_CURVE('',#6301,#6132,#4589,.T.);
#7977=EDGE_CURVE('',#6302,#6303,#4590,.T.);
#7978=EDGE_CURVE('',#6303,#6303,#1850,.T.);
#7979=EDGE_CURVE('',#6303,#6257,#4591,.T.);
#7980=EDGE_CURVE('',#6258,#6304,#4592,.T.);
#7981=EDGE_CURVE('',#6304,#6304,#1851,.T.);
#7982=EDGE_CURVE('',#6304,#6135,#4593,.T.);
#7983=EDGE_CURVE('',#6305,#6305,#1852,.T.);
#7984=EDGE_CURVE('',#6305,#6306,#4594,.T.);
#7985=EDGE_CURVE('',#6306,#6306,#1853,.T.);
#7986=EDGE_CURVE('',#6306,#6307,#4595,.T.);
#7987=EDGE_CURVE('',#6307,#6307,#1854,.T.);
#7988=EDGE_CURVE('',#6308,#6308,#1855,.T.);
#7989=EDGE_CURVE('',#6308,#6309,#4596,.T.);
#7990=EDGE_CURVE('',#6309,#6309,#1856,.T.);
#7991=EDGE_CURVE('',#6309,#6310,#4597,.T.);
#7992=EDGE_CURVE('',#6310,#6310,#1857,.T.);
#7993=EDGE_CURVE('',#6311,#6311,#1858,.T.);
#7994=EDGE_CURVE('',#6311,#6312,#4598,.T.);
#7995=EDGE_CURVE('',#6312,#6312,#1859,.T.);
#7996=EDGE_CURVE('',#6312,#6313,#4599,.T.);
#7997=EDGE_CURVE('',#6313,#6313,#1860,.T.);
#7998=EDGE_CURVE('',#6314,#6314,#1861,.T.);
#7999=EDGE_CURVE('',#6314,#6315,#4600,.T.);
#8000=EDGE_CURVE('',#6315,#6315,#1862,.T.);
#8001=EDGE_CURVE('',#6315,#6316,#4601,.T.);
#8002=EDGE_CURVE('',#6316,#6316,#1863,.T.);
#8003=EDGE_CURVE('',#6317,#6059,#4602,.T.);
#8004=EDGE_CURVE('',#6056,#6317,#4603,.T.);
#8005=EDGE_CURVE('',#6060,#6317,#4604,.T.);
#8006=EDGE_CURVE('',#6125,#6318,#4605,.T.);
#8007=EDGE_CURVE('',#6129,#6318,#4606,.T.);
#8008=EDGE_CURVE('',#6318,#6319,#4607,.T.);
#8009=EDGE_CURVE('',#6124,#6319,#4608,.T.);
#8010=EDGE_CURVE('',#6319,#6142,#4609,.T.);
#8011=EDGE_CURVE('',#6320,#6141,#1864,.T.);
#8012=EDGE_CURVE('',#6320,#6321,#4610,.T.);
#8013=EDGE_CURVE('',#6321,#6322,#4611,.T.);
#8014=EDGE_CURVE('',#6322,#6323,#4612,.T.);
#8015=EDGE_CURVE('',#6323,#6324,#4613,.T.);
#8016=EDGE_CURVE('',#6324,#6325,#4614,.T.);
#8017=EDGE_CURVE('',#6061,#6325,#1865,.T.);
#8018=EDGE_CURVE('',#6326,#6326,#1866,.T.);
#8019=EDGE_CURVE('',#6327,#6063,#4615,.T.);
#8020=EDGE_CURVE('',#6328,#6327,#4616,.T.);
#8021=EDGE_CURVE('',#6328,#6064,#4617,.T.);
#8022=EDGE_CURVE('',#6329,#6328,#4618,.T.);
#8023=EDGE_CURVE('',#6054,#6329,#4619,.T.);
#8024=EDGE_CURVE('',#6329,#6173,#4620,.T.);
#8025=EDGE_CURVE('',#6330,#6327,#4621,.T.);
#8026=EDGE_CURVE('',#6190,#6330,#4622,.T.);
#8027=EDGE_CURVE('',#6331,#6184,#4623,.T.);
#8028=EDGE_CURVE('',#6332,#6331,#4624,.T.);
#8029=EDGE_CURVE('',#6333,#6332,#4625,.T.);
#8030=EDGE_CURVE('',#6333,#6128,#4626,.T.);
#8031=EDGE_CURVE('',#6182,#6170,#4627,.T.);
#8032=EDGE_CURVE('',#6139,#6332,#4628,.T.);
#8033=EDGE_CURVE('',#6138,#6333,#4629,.T.);
#8034=EDGE_CURVE('',#6334,#6330,#1867,.T.);
#8035=EDGE_CURVE('',#6334,#6188,#4630,.T.);
#8036=EDGE_CURVE('',#6335,#6186,#4631,.T.);
#8037=EDGE_CURVE('',#6331,#6335,#1868,.T.);
#8038=EDGE_CURVE('',#6336,#6062,#1869,.T.);
#8039=EDGE_CURVE('',#6336,#6337,#4632,.T.);
#8040=EDGE_CURVE('',#6337,#6338,#4633,.T.);
#8041=EDGE_CURVE('',#6338,#6339,#4634,.T.);
#8042=EDGE_CURVE('',#6339,#6340,#4635,.T.);
#8043=EDGE_CURVE('',#6340,#6341,#4636,.T.);
#8044=EDGE_CURVE('',#6140,#6341,#1870,.T.);
#8045=EDGE_CURVE('',#6335,#6334,#1871,.T.);
#8046=EDGE_CURVE('',#6339,#6322,#4637,.T.);
#8047=EDGE_CURVE('',#6340,#6321,#4638,.T.);
#8048=EDGE_CURVE('',#6324,#6337,#4639,.T.);
#8049=EDGE_CURVE('',#6323,#6338,#4640,.T.);
#8050=EDGE_CURVE('',#6325,#6336,#4641,.T.);
#8051=EDGE_CURVE('',#6341,#6320,#4642,.T.);
#8052=EDGE_CURVE('',#6250,#6342,#4643,.T.);
#8053=EDGE_CURVE('',#6342,#6343,#4644,.T.);
#8054=EDGE_CURVE('',#6251,#6343,#4645,.T.);
#8055=EDGE_CURVE('',#6253,#6344,#4646,.T.);
#8056=EDGE_CURVE('',#6344,#6342,#4647,.T.);
#8057=EDGE_CURVE('',#6252,#6345,#4648,.T.);
#8058=EDGE_CURVE('',#6345,#6344,#4649,.T.);
#8059=EDGE_CURVE('',#6343,#6345,#4650,.T.);
#8060=EDGE_CURVE('',#6246,#6346,#4651,.T.);
#8061=EDGE_CURVE('',#6346,#6347,#4652,.T.);
#8062=EDGE_CURVE('',#6247,#6347,#4653,.T.);
#8063=EDGE_CURVE('',#6249,#6348,#4654,.T.);
#8064=EDGE_CURVE('',#6348,#6346,#4655,.T.);
#8065=EDGE_CURVE('',#6248,#6349,#4656,.T.);
#8066=EDGE_CURVE('',#6349,#6348,#4657,.T.);
#8067=EDGE_CURVE('',#6347,#6349,#4658,.T.);
#8068=EDGE_CURVE('',#6242,#6350,#4659,.T.);
#8069=EDGE_CURVE('',#6350,#6351,#4660,.T.);
#8070=EDGE_CURVE('',#6243,#6351,#4661,.T.);
#8071=EDGE_CURVE('',#6245,#6352,#4662,.T.);
#8072=EDGE_CURVE('',#6352,#6350,#4663,.T.);
#8073=EDGE_CURVE('',#6244,#6353,#4664,.T.);
#8074=EDGE_CURVE('',#6353,#6352,#4665,.T.);
#8075=EDGE_CURVE('',#6351,#6353,#4666,.T.);
#8076=EDGE_CURVE('',#6238,#6354,#4667,.T.);
#8077=EDGE_CURVE('',#6354,#6355,#4668,.T.);
#8078=EDGE_CURVE('',#6239,#6355,#4669,.T.);
#8079=EDGE_CURVE('',#6241,#6356,#4670,.T.);
#8080=EDGE_CURVE('',#6356,#6354,#4671,.T.);
#8081=EDGE_CURVE('',#6240,#6357,#4672,.T.);
#8082=EDGE_CURVE('',#6357,#6356,#4673,.T.);
#8083=EDGE_CURVE('',#6355,#6357,#4674,.T.);
#8084=EDGE_CURVE('',#6234,#6358,#4675,.T.);
#8085=EDGE_CURVE('',#6358,#6359,#4676,.T.);
#8086=EDGE_CURVE('',#6235,#6359,#4677,.T.);
#8087=EDGE_CURVE('',#6237,#6360,#4678,.T.);
#8088=EDGE_CURVE('',#6360,#6358,#4679,.T.);
#8089=EDGE_CURVE('',#6236,#6361,#4680,.T.);
#8090=EDGE_CURVE('',#6361,#6360,#4681,.T.);
#8091=EDGE_CURVE('',#6359,#6361,#4682,.T.);
#8092=EDGE_CURVE('',#6230,#6362,#4683,.T.);
#8093=EDGE_CURVE('',#6362,#6363,#4684,.T.);
#8094=EDGE_CURVE('',#6231,#6363,#4685,.T.);
#8095=EDGE_CURVE('',#6233,#6364,#4686,.T.);
#8096=EDGE_CURVE('',#6364,#6362,#4687,.T.);
#8097=EDGE_CURVE('',#6232,#6365,#4688,.T.);
#8098=EDGE_CURVE('',#6365,#6364,#4689,.T.);
#8099=EDGE_CURVE('',#6363,#6365,#4690,.T.);
#8100=EDGE_CURVE('',#6068,#6366,#4691,.T.);
#8101=EDGE_CURVE('',#6366,#6366,#1872,.T.);
#8102=EDGE_CURVE('',#6367,#6367,#1873,.T.);
#8103=EDGE_CURVE('',#6367,#6368,#4692,.T.);
#8104=EDGE_CURVE('',#6368,#6368,#1874,.T.);
#8105=EDGE_CURVE('',#6369,#6369,#1875,.T.);
#8106=EDGE_CURVE('',#6369,#6370,#4693,.T.);
#8107=EDGE_CURVE('',#6370,#6370,#1876,.T.);
#8108=EDGE_CURVE('',#6371,#6371,#1877,.T.);
#8109=EDGE_CURVE('',#6371,#6372,#4694,.T.);
#8110=EDGE_CURVE('',#6373,#6372,#384,.T.);
#8111=EDGE_CURVE('',#6374,#6373,#385,.T.);
#8112=EDGE_CURVE('',#6374,#6375,#4695,.T.);
#8113=EDGE_CURVE('',#6375,#6375,#1878,.T.);
#8114=EDGE_CURVE('',#6372,#6374,#386,.T.);
#8115=EDGE_CURVE('',#6376,#6376,#1879,.T.);
#8116=EDGE_CURVE('',#6376,#6377,#4696,.T.);
#8117=EDGE_CURVE('',#6377,#6377,#1880,.T.);
#8118=EDGE_CURVE('',#6378,#6378,#1881,.T.);
#8119=EDGE_CURVE('',#6378,#6379,#4697,.T.);
#8120=EDGE_CURVE('',#6379,#6379,#1882,.T.);
#8121=EDGE_CURVE('',#6380,#6380,#1883,.T.);
#8122=EDGE_CURVE('',#6380,#6143,#4698,.T.);
#8123=EDGE_CURVE('',#6326,#6381,#4699,.T.);
#8124=EDGE_CURVE('',#6381,#6381,#1884,.T.);
#8125=EDGE_CURVE('',#6382,#6382,#1885,.T.);
#8126=EDGE_CURVE('',#6382,#6383,#4700,.T.);
#8127=EDGE_CURVE('',#6383,#6383,#1886,.T.);
#8128=EDGE_CURVE('',#6384,#6384,#1887,.T.);
#8129=EDGE_CURVE('',#6384,#6385,#4701,.T.);
#8130=EDGE_CURVE('',#6385,#6385,#1888,.T.);
#8131=EDGE_CURVE('',#6385,#6201,#4702,.T.);
#8132=EDGE_CURVE('',#6386,#6386,#1889,.T.);
#8133=EDGE_CURVE('',#6386,#6387,#4703,.T.);
#8134=EDGE_CURVE('',#6387,#6387,#1890,.T.);
#8135=EDGE_CURVE('',#6386,#6388,#4704,.T.);
#8136=EDGE_CURVE('',#6388,#6388,#1891,.T.);
#8137=EDGE_CURVE('',#6389,#6389,#1892,.T.);
#8138=EDGE_CURVE('',#6390,#6391,#1893,.T.);
#8139=EDGE_CURVE('',#6391,#6392,#387,.T.);
#8140=EDGE_CURVE('',#6392,#6393,#1894,.T.);
#8141=EDGE_CURVE('',#6390,#6393,#388,.T.);
#8142=EDGE_CURVE('',#6391,#6394,#1895,.T.);
#8143=EDGE_CURVE('',#6394,#6395,#389,.T.);
#8144=EDGE_CURVE('',#6395,#6392,#1896,.T.);
#8145=EDGE_CURVE('',#6394,#6396,#1897,.T.);
#8146=EDGE_CURVE('',#6396,#6397,#390,.T.);
#8147=EDGE_CURVE('',#6397,#6395,#1898,.T.);
#8148=EDGE_CURVE('',#6396,#6398,#1899,.T.);
#8149=EDGE_CURVE('',#6398,#6399,#391,.T.);
#8150=EDGE_CURVE('',#6399,#6397,#1900,.T.);
#8151=EDGE_CURVE('',#6398,#6400,#1901,.T.);
#8152=EDGE_CURVE('',#6400,#6401,#392,.T.);
#8153=EDGE_CURVE('',#6401,#6399,#1902,.T.);
#8154=EDGE_CURVE('',#6402,#6401,#1903,.T.);
#8155=EDGE_CURVE('',#6400,#6403,#1904,.T.);
#8156=EDGE_CURVE('',#6403,#6402,#393,.T.);
#8157=EDGE_CURVE('',#6404,#6402,#1905,.T.);
#8158=EDGE_CURVE('',#6403,#6405,#1906,.T.);
#8159=EDGE_CURVE('',#6405,#6404,#394,.T.);
#8160=EDGE_CURVE('',#6393,#6404,#1907,.T.);
#8161=EDGE_CURVE('',#6405,#6390,#1908,.T.);
#8162=EDGE_CURVE('',#6406,#6402,#4705,.T.);
#8163=EDGE_CURVE('',#6407,#6406,#1909,.T.);
#8164=EDGE_CURVE('',#6407,#6401,#4706,.T.);
#8165=EDGE_CURVE('',#6408,#6404,#4707,.T.);
#8166=EDGE_CURVE('',#6406,#6408,#1910,.T.);
#8167=EDGE_CURVE('',#6409,#6393,#4708,.T.);
#8168=EDGE_CURVE('',#6408,#6409,#1911,.T.);
#8169=EDGE_CURVE('',#6410,#6392,#4709,.T.);
#8170=EDGE_CURVE('',#6409,#6410,#1912,.T.);
#8171=EDGE_CURVE('',#6411,#6411,#1913,.T.);
#8172=EDGE_CURVE('',#6412,#6412,#1914,.T.);
#8173=EDGE_CURVE('',#6413,#6413,#1915,.T.);
#8174=EDGE_CURVE('',#6414,#6414,#1916,.T.);
#8175=EDGE_CURVE('',#6415,#6415,#1917,.T.);
#8176=EDGE_CURVE('',#6416,#6416,#1918,.T.);
#8177=EDGE_CURVE('',#6416,#6417,#4710,.T.);
#8178=EDGE_CURVE('',#6417,#6417,#1919,.T.);
#8179=EDGE_CURVE('',#6416,#6418,#4711,.T.);
#8180=EDGE_CURVE('',#6418,#6418,#1920,.T.);
#8181=EDGE_CURVE('',#6418,#6419,#4712,.T.);
#8182=EDGE_CURVE('',#6419,#6419,#1921,.T.);
#8183=EDGE_CURVE('',#6420,#6420,#1922,.T.);
#8184=EDGE_CURVE('',#6420,#6415,#4713,.T.);
#8185=EDGE_CURVE('',#6421,#6421,#1923,.T.);
#8186=EDGE_CURVE('',#6421,#6422,#4714,.T.);
#8187=EDGE_CURVE('',#6422,#6422,#1924,.T.);
#8188=EDGE_CURVE('',#6421,#6423,#4715,.T.);
#8189=EDGE_CURVE('',#6423,#6423,#1925,.T.);
#8190=EDGE_CURVE('',#6423,#6424,#4716,.T.);
#8191=EDGE_CURVE('',#6424,#6424,#1926,.T.);
#8192=EDGE_CURVE('',#6425,#6425,#1927,.T.);
#8193=EDGE_CURVE('',#6425,#6414,#4717,.T.);
#8194=EDGE_CURVE('',#6426,#6426,#1928,.T.);
#8195=EDGE_CURVE('',#6426,#6427,#4718,.T.);
#8196=EDGE_CURVE('',#6427,#6427,#1929,.T.);
#8197=EDGE_CURVE('',#6426,#6428,#4719,.T.);
#8198=EDGE_CURVE('',#6428,#6428,#1930,.T.);
#8199=EDGE_CURVE('',#6428,#6429,#4720,.T.);
#8200=EDGE_CURVE('',#6429,#6429,#1931,.T.);
#8201=EDGE_CURVE('',#6430,#6430,#1932,.T.);
#8202=EDGE_CURVE('',#6430,#6413,#4721,.T.);
#8203=EDGE_CURVE('',#6431,#6431,#1933,.T.);
#8204=EDGE_CURVE('',#6431,#6432,#4722,.T.);
#8205=EDGE_CURVE('',#6432,#6432,#1934,.T.);
#8206=EDGE_CURVE('',#6431,#6433,#4723,.T.);
#8207=EDGE_CURVE('',#6433,#6433,#1935,.T.);
#8208=EDGE_CURVE('',#6433,#6434,#4724,.T.);
#8209=EDGE_CURVE('',#6434,#6434,#1936,.T.);
#8210=EDGE_CURVE('',#6435,#6435,#1937,.T.);
#8211=EDGE_CURVE('',#6435,#6412,#4725,.T.);
#8212=EDGE_CURVE('',#6436,#6436,#1938,.T.);
#8213=EDGE_CURVE('',#6436,#6411,#4726,.T.);
#8214=EDGE_CURVE('',#6436,#6437,#4727,.T.);
#8215=EDGE_CURVE('',#6437,#6437,#1939,.T.);
#8216=EDGE_CURVE('',#6438,#6438,#1940,.T.);
#8217=EDGE_CURVE('',#6438,#6389,#4728,.T.);
#8218=EDGE_CURVE('',#6439,#6395,#4729,.T.);
#8219=EDGE_CURVE('',#6410,#6439,#1941,.T.);
#8220=EDGE_CURVE('',#6440,#6397,#4730,.T.);
#8221=EDGE_CURVE('',#6439,#6440,#1942,.T.);
#8222=EDGE_CURVE('',#6441,#6399,#4731,.T.);
#8223=EDGE_CURVE('',#6440,#6441,#1943,.T.);
#8224=EDGE_CURVE('',#6441,#6407,#1944,.T.);
#8225=EDGE_CURVE('',#6442,#6443,#4732,.T.);
#8226=EDGE_CURVE('',#6443,#6444,#4733,.T.);
#8227=EDGE_CURVE('',#6444,#6445,#4734,.T.);
#8228=EDGE_CURVE('',#6442,#6445,#4735,.T.);
#8229=EDGE_CURVE('',#6443,#6446,#4736,.T.);
#8230=EDGE_CURVE('',#6446,#6447,#4737,.T.);
#8231=EDGE_CURVE('',#6447,#6444,#4738,.T.);
#8232=EDGE_CURVE('',#6446,#6448,#4739,.T.);
#8233=EDGE_CURVE('',#6448,#6449,#4740,.T.);
#8234=EDGE_CURVE('',#6449,#6447,#4741,.T.);
#8235=EDGE_CURVE('',#6448,#6450,#4742,.T.);
#8236=EDGE_CURVE('',#6450,#6451,#4743,.T.);
#8237=EDGE_CURVE('',#6451,#6449,#4744,.T.);
#8238=EDGE_CURVE('',#6450,#6452,#4745,.T.);
#8239=EDGE_CURVE('',#6452,#6453,#4746,.T.);
#8240=EDGE_CURVE('',#6453,#6451,#4747,.T.);
#8241=EDGE_CURVE('',#6454,#6453,#4748,.T.);
#8242=EDGE_CURVE('',#6452,#6455,#4749,.T.);
#8243=EDGE_CURVE('',#6455,#6454,#4750,.T.);
#8244=EDGE_CURVE('',#6456,#6454,#4751,.T.);
#8245=EDGE_CURVE('',#6455,#6457,#4752,.T.);
#8246=EDGE_CURVE('',#6457,#6456,#4753,.T.);
#8247=EDGE_CURVE('',#6445,#6456,#4754,.T.);
#8248=EDGE_CURVE('',#6457,#6442,#4755,.T.);
#8249=EDGE_CURVE('',#6458,#6454,#4756,.T.);
#8250=EDGE_CURVE('',#6459,#6458,#4757,.T.);
#8251=EDGE_CURVE('',#6459,#6453,#4758,.T.);
#8252=EDGE_CURVE('',#6460,#6456,#4759,.T.);
#8253=EDGE_CURVE('',#6458,#6460,#4760,.T.);
#8254=EDGE_CURVE('',#6461,#6445,#4761,.T.);
#8255=EDGE_CURVE('',#6460,#6461,#4762,.T.);
#8256=EDGE_CURVE('',#6462,#6444,#4763,.T.);
#8257=EDGE_CURVE('',#6461,#6462,#4764,.T.);
#8258=EDGE_CURVE('',#6463,#6463,#1945,.T.);
#8259=EDGE_CURVE('',#6464,#6465,#4765,.T.);
#8260=EDGE_CURVE('',#6465,#6466,#4766,.T.);
#8261=EDGE_CURVE('',#6466,#6467,#4767,.T.);
#8262=EDGE_CURVE('',#6467,#6464,#4768,.T.);
#8263=EDGE_CURVE('',#6468,#6469,#4769,.T.);
#8264=EDGE_CURVE('',#6469,#6470,#4770,.T.);
#8265=EDGE_CURVE('',#6470,#6471,#4771,.T.);
#8266=EDGE_CURVE('',#6471,#6468,#4772,.T.);
#8267=EDGE_CURVE('',#6472,#6473,#4773,.T.);
#8268=EDGE_CURVE('',#6473,#6474,#4774,.T.);
#8269=EDGE_CURVE('',#6474,#6475,#4775,.T.);
#8270=EDGE_CURVE('',#6475,#6472,#4776,.T.);
#8271=EDGE_CURVE('',#6476,#6477,#4777,.T.);
#8272=EDGE_CURVE('',#6477,#6478,#4778,.T.);
#8273=EDGE_CURVE('',#6478,#6479,#4779,.T.);
#8274=EDGE_CURVE('',#6479,#6476,#4780,.T.);
#8275=EDGE_CURVE('',#6480,#6480,#1946,.T.);
#8276=EDGE_CURVE('',#6481,#6481,#1947,.T.);
#8277=EDGE_CURVE('',#6482,#6482,#1948,.T.);
#8278=EDGE_CURVE('',#6483,#6483,#1949,.T.);
#8279=EDGE_CURVE('',#6484,#6484,#1950,.T.);
#8280=EDGE_CURVE('',#6484,#6485,#4781,.T.);
#8281=EDGE_CURVE('',#6485,#6485,#1951,.T.);
#8282=EDGE_CURVE('',#6484,#6486,#4782,.T.);
#8283=EDGE_CURVE('',#6486,#6486,#1952,.T.);
#8284=EDGE_CURVE('',#6486,#6487,#4783,.T.);
#8285=EDGE_CURVE('',#6487,#6487,#1953,.T.);
#8286=EDGE_CURVE('',#6488,#6488,#1954,.T.);
#8287=EDGE_CURVE('',#6488,#6489,#4784,.T.);
#8288=EDGE_CURVE('',#6489,#6489,#1955,.T.);
#8289=EDGE_CURVE('',#6490,#6490,#1956,.T.);
#8290=EDGE_CURVE('',#6490,#6491,#4785,.T.);
#8291=EDGE_CURVE('',#6491,#6491,#1957,.T.);
#8292=EDGE_CURVE('',#6490,#6492,#4786,.T.);
#8293=EDGE_CURVE('',#6492,#6492,#1958,.T.);
#8294=EDGE_CURVE('',#6492,#6493,#4787,.T.);
#8295=EDGE_CURVE('',#6493,#6493,#1959,.T.);
#8296=EDGE_CURVE('',#6494,#6494,#1960,.T.);
#8297=EDGE_CURVE('',#6494,#6495,#4788,.T.);
#8298=EDGE_CURVE('',#6495,#6495,#1961,.T.);
#8299=EDGE_CURVE('',#6496,#6496,#1962,.T.);
#8300=EDGE_CURVE('',#6496,#6497,#4789,.T.);
#8301=EDGE_CURVE('',#6497,#6497,#1963,.T.);
#8302=EDGE_CURVE('',#6496,#6498,#4790,.T.);
#8303=EDGE_CURVE('',#6498,#6498,#1964,.T.);
#8304=EDGE_CURVE('',#6498,#6499,#4791,.T.);
#8305=EDGE_CURVE('',#6499,#6499,#1965,.T.);
#8306=EDGE_CURVE('',#6500,#6500,#1966,.T.);
#8307=EDGE_CURVE('',#6500,#6501,#4792,.T.);
#8308=EDGE_CURVE('',#6501,#6501,#1967,.T.);
#8309=EDGE_CURVE('',#6502,#6502,#1968,.T.);
#8310=EDGE_CURVE('',#6502,#6503,#4793,.T.);
#8311=EDGE_CURVE('',#6503,#6503,#1969,.T.);
#8312=EDGE_CURVE('',#6502,#6504,#4794,.T.);
#8313=EDGE_CURVE('',#6504,#6504,#1970,.T.);
#8314=EDGE_CURVE('',#6504,#6505,#4795,.T.);
#8315=EDGE_CURVE('',#6505,#6505,#1971,.T.);
#8316=EDGE_CURVE('',#6506,#6506,#1972,.T.);
#8317=EDGE_CURVE('',#6506,#6507,#4796,.T.);
#8318=EDGE_CURVE('',#6507,#6507,#1973,.T.);
#8319=EDGE_CURVE('',#6508,#6508,#1974,.T.);
#8320=EDGE_CURVE('',#6508,#6509,#4797,.T.);
#8321=EDGE_CURVE('',#6509,#6509,#1975,.T.);
#8322=EDGE_CURVE('',#6508,#6510,#4798,.T.);
#8323=EDGE_CURVE('',#6510,#6510,#1976,.T.);
#8324=EDGE_CURVE('',#6510,#6463,#4799,.T.);
#8325=EDGE_CURVE('',#6511,#6511,#1977,.T.);
#8326=EDGE_CURVE('',#6511,#6512,#4800,.T.);
#8327=EDGE_CURVE('',#6512,#6512,#1978,.T.);
#8328=EDGE_CURVE('',#6511,#6513,#4801,.T.);
#8329=EDGE_CURVE('',#6513,#6513,#1979,.T.);
#8330=EDGE_CURVE('',#6513,#6483,#4802,.T.);
#8331=EDGE_CURVE('',#6514,#6514,#1980,.T.);
#8332=EDGE_CURVE('',#6514,#6515,#4803,.T.);
#8333=EDGE_CURVE('',#6515,#6515,#1981,.T.);
#8334=EDGE_CURVE('',#6514,#6516,#4804,.T.);
#8335=EDGE_CURVE('',#6516,#6516,#1982,.T.);
#8336=EDGE_CURVE('',#6516,#6482,#4805,.T.);
#8337=EDGE_CURVE('',#6517,#6517,#1983,.T.);
#8338=EDGE_CURVE('',#6517,#6518,#4806,.T.);
#8339=EDGE_CURVE('',#6518,#6518,#1984,.T.);
#8340=EDGE_CURVE('',#6517,#6519,#4807,.T.);
#8341=EDGE_CURVE('',#6519,#6519,#1985,.T.);
#8342=EDGE_CURVE('',#6519,#6481,#4808,.T.);
#8343=EDGE_CURVE('',#6520,#6521,#4809,.T.);
#8344=EDGE_CURVE('',#6520,#6465,#4810,.T.);
#8345=EDGE_CURVE('',#6521,#6464,#4811,.T.);
#8346=EDGE_CURVE('',#6522,#6520,#4812,.T.);
#8347=EDGE_CURVE('',#6522,#6466,#4813,.T.);
#8348=EDGE_CURVE('',#6523,#6522,#4814,.T.);
#8349=EDGE_CURVE('',#6523,#6467,#4815,.T.);
#8350=EDGE_CURVE('',#6521,#6523,#4816,.T.);
#8351=EDGE_CURVE('',#6524,#6525,#4817,.T.);
#8352=EDGE_CURVE('',#6524,#6469,#4818,.T.);
#8353=EDGE_CURVE('',#6525,#6468,#4819,.T.);
#8354=EDGE_CURVE('',#6526,#6524,#4820,.T.);
#8355=EDGE_CURVE('',#6526,#6470,#4821,.T.);
#8356=EDGE_CURVE('',#6527,#6526,#4822,.T.);
#8357=EDGE_CURVE('',#6527,#6471,#4823,.T.);
#8358=EDGE_CURVE('',#6525,#6527,#4824,.T.);
#8359=EDGE_CURVE('',#6528,#6529,#4825,.T.);
#8360=EDGE_CURVE('',#6528,#6473,#4826,.T.);
#8361=EDGE_CURVE('',#6529,#6472,#4827,.T.);
#8362=EDGE_CURVE('',#6530,#6528,#4828,.T.);
#8363=EDGE_CURVE('',#6530,#6474,#4829,.T.);
#8364=EDGE_CURVE('',#6531,#6530,#4830,.T.);
#8365=EDGE_CURVE('',#6531,#6475,#4831,.T.);
#8366=EDGE_CURVE('',#6529,#6531,#4832,.T.);
#8367=EDGE_CURVE('',#6532,#6533,#4833,.T.);
#8368=EDGE_CURVE('',#6532,#6477,#4834,.T.);
#8369=EDGE_CURVE('',#6533,#6476,#4835,.T.);
#8370=EDGE_CURVE('',#6534,#6532,#4836,.T.);
#8371=EDGE_CURVE('',#6534,#6478,#4837,.T.);
#8372=EDGE_CURVE('',#6535,#6534,#4838,.T.);
#8373=EDGE_CURVE('',#6535,#6479,#4839,.T.);
#8374=EDGE_CURVE('',#6533,#6535,#4840,.T.);
#8375=EDGE_CURVE('',#6536,#6536,#1986,.T.);
#8376=EDGE_CURVE('',#6536,#6537,#4841,.T.);
#8377=EDGE_CURVE('',#6537,#6537,#1987,.T.);
#8378=EDGE_CURVE('',#6480,#6538,#4842,.T.);
#8379=EDGE_CURVE('',#6538,#6538,#1988,.T.);
#8380=EDGE_CURVE('',#6539,#6447,#4843,.T.);
#8381=EDGE_CURVE('',#6462,#6539,#4844,.T.);
#8382=EDGE_CURVE('',#6540,#6449,#4845,.T.);
#8383=EDGE_CURVE('',#6539,#6540,#4846,.T.);
#8384=EDGE_CURVE('',#6541,#6451,#4847,.T.);
#8385=EDGE_CURVE('',#6540,#6541,#4848,.T.);
#8386=EDGE_CURVE('',#6541,#6459,#4849,.T.);
#8387=EDGE_CURVE('',#6542,#6543,#4850,.T.);
#8388=EDGE_CURVE('',#6542,#6544,#395,.T.);
#8389=EDGE_CURVE('',#6544,#6545,#1989,.T.);
#8390=EDGE_CURVE('',#6545,#6546,#4851,.T.);
#8391=EDGE_CURVE('',#6546,#6543,#396,.T.);
#8392=EDGE_CURVE('',#6547,#6548,#4852,.T.);
#8393=EDGE_CURVE('',#6547,#6542,#397,.T.);
#8394=EDGE_CURVE('',#6543,#6548,#398,.T.);
#8395=EDGE_CURVE('',#6549,#6550,#4853,.T.);
#8396=EDGE_CURVE('',#6549,#6547,#399,.T.);
#8397=EDGE_CURVE('',#6548,#6550,#400,.T.);
#8398=EDGE_CURVE('',#6551,#6552,#4854,.T.);
#8399=EDGE_CURVE('',#6551,#6549,#401,.T.);
#8400=EDGE_CURVE('',#6550,#6552,#402,.T.);
#8401=EDGE_CURVE('',#6553,#6554,#4855,.T.);
#8402=EDGE_CURVE('',#6553,#6551,#403,.T.);
#8403=EDGE_CURVE('',#6552,#6554,#404,.T.);
#8404=EDGE_CURVE('',#6555,#6556,#4856,.T.);
#8405=EDGE_CURVE('',#6555,#6553,#405,.T.);
#8406=EDGE_CURVE('',#6554,#6556,#406,.T.);
#8407=EDGE_CURVE('',#6556,#6557,#407,.T.);
#8408=EDGE_CURVE('',#6557,#6558,#1990,.T.);
#8409=EDGE_CURVE('',#6558,#6559,#4857,.T.);
#8410=EDGE_CURVE('',#6559,#6555,#408,.T.);
#8411=EDGE_CURVE('',#6560,#6561,#4858,.T.);
#8412=EDGE_CURVE('',#6560,#6562,#4859,.T.);
#8413=EDGE_CURVE('',#6563,#6562,#4860,.T.);
#8414=EDGE_CURVE('',#6564,#6563,#4861,.T.);
#8415=EDGE_CURVE('',#6561,#6564,#260,.T.);
#8416=EDGE_CURVE('',#6563,#6565,#1991,.T.);
#8417=EDGE_CURVE('',#6562,#6566,#4862,.T.);
#8418=EDGE_CURVE('',#6565,#6566,#4863,.T.);
#8419=EDGE_CURVE('',#6567,#6568,#4864,.T.);
#8420=EDGE_CURVE('',#6569,#6567,#261,.T.);
#8421=EDGE_CURVE('',#6565,#6569,#4865,.T.);
#8422=EDGE_CURVE('',#6566,#6568,#4866,.T.);
#8423=EDGE_CURVE('',#6568,#6560,#4867,.T.);
#8424=EDGE_CURVE('',#6570,#6570,#1992,.T.);
#8425=EDGE_CURVE('',#6570,#6571,#4868,.T.);
#8426=EDGE_CURVE('',#6571,#6564,#1993,.T.);
#8427=EDGE_CURVE('',#6569,#6571,#1994,.T.);
#8428=EDGE_CURVE('',#6561,#6567,#1995,.T.);
#8429=EDGE_CURVE('',#6572,#6570,#4869,.T.);
#8430=EDGE_CURVE('',#6573,#6573,#1996,.T.);
#8431=EDGE_CURVE('',#6573,#6574,#4870,.T.);
#8432=EDGE_CURVE('',#6574,#6574,#1997,.T.);
#8433=EDGE_CURVE('',#6575,#6576,#409,.T.);
#8434=EDGE_CURVE('',#6558,#6575,#4871,.T.);
#8435=EDGE_CURVE('',#6577,#6557,#410,.T.);
#8436=EDGE_CURVE('',#6578,#6577,#411,.T.);
#8437=EDGE_CURVE('',#6576,#6578,#412,.T.);
#8438=EDGE_CURVE('',#6576,#6574,#4872,.T.);
#8439=EDGE_CURVE('',#6579,#6544,#413,.T.);
#8440=EDGE_CURVE('',#6580,#6579,#414,.T.);
#8441=EDGE_CURVE('',#6581,#6580,#415,.T.);
#8442=EDGE_CURVE('',#6545,#6581,#4873,.T.);
#8443=EDGE_CURVE('',#6545,#6582,#4874,.T.);
#8444=EDGE_CURVE('',#6582,#6582,#1998,.T.);
#8445=EDGE_CURVE('',#6582,#6583,#4875,.T.);
#8446=EDGE_CURVE('',#6583,#6583,#1999,.T.);
#8447=EDGE_CURVE('',#6577,#6580,#416,.T.);
#8448=EDGE_CURVE('',#6578,#6579,#417,.T.);
#8449=EDGE_CURVE('',#6559,#6575,#4876,.T.);
#8450=EDGE_CURVE('',#6581,#6546,#4877,.T.);
#8451=EDGE_CURVE('',#6584,#6584,#2000,.T.);
#8452=EDGE_CURVE('',#6585,#6585,#2001,.T.);
#8453=EDGE_CURVE('',#6585,#6584,#4878,.T.);
#8454=EDGE_CURVE('',#6586,#6586,#2002,.T.);
#8455=EDGE_CURVE('',#6586,#6585,#4879,.T.);
#8456=EDGE_CURVE('',#6587,#6587,#2003,.T.);
#8457=EDGE_CURVE('',#6588,#6588,#2004,.T.);
#8458=EDGE_CURVE('',#6588,#6587,#4880,.T.);
#8459=EDGE_CURVE('',#6589,#6589,#2005,.T.);
#8460=EDGE_CURVE('',#6589,#6588,#4881,.T.);
#8461=EDGE_CURVE('',#6590,#6590,#2006,.T.);
#8462=EDGE_CURVE('',#6591,#6591,#2007,.T.);
#8463=EDGE_CURVE('',#6591,#6590,#4882,.T.);
#8464=EDGE_CURVE('',#6591,#6592,#4883,.T.);
#8465=EDGE_CURVE('',#6592,#6592,#2008,.T.);
#8466=EDGE_CURVE('',#6593,#6593,#2009,.T.);
#8467=EDGE_CURVE('',#6594,#6594,#2010,.T.);
#8468=EDGE_CURVE('',#6594,#6593,#4884,.T.);
#8469=EDGE_CURVE('',#6594,#6595,#4885,.T.);
#8470=EDGE_CURVE('',#6595,#6595,#2011,.T.);
#8471=EDGE_CURVE('',#6596,#6597,#2012,.T.);
#8472=EDGE_CURVE('',#6597,#6598,#4886,.T.);
#8473=EDGE_CURVE('',#6598,#6598,#2013,.T.);
#8474=EDGE_CURVE('',#6597,#6596,#2014,.T.);
#8475=EDGE_CURVE('',#6596,#6599,#4887,.T.);
#8476=EDGE_CURVE('',#6600,#6599,#2015,.T.);
#8477=EDGE_CURVE('',#6599,#6600,#2016,.T.);
#8478=EDGE_CURVE('',#6601,#6602,#418,.T.);
#8479=EDGE_CURVE('',#6603,#6602,#2017,.T.);
#8480=EDGE_CURVE('',#6603,#6604,#419,.T.);
#8481=EDGE_CURVE('',#6604,#6605,#4888,.T.);
#8482=EDGE_CURVE('',#6605,#6606,#420,.T.);
#8483=EDGE_CURVE('',#6607,#6606,#2018,.T.);
#8484=EDGE_CURVE('',#6607,#6608,#421,.T.);
#8485=EDGE_CURVE('',#6608,#6609,#4889,.T.);
#8486=EDGE_CURVE('',#6609,#6610,#422,.T.);
#8487=EDGE_CURVE('',#6611,#6610,#2019,.T.);
#8488=EDGE_CURVE('',#6611,#6612,#423,.T.);
#8489=EDGE_CURVE('',#6612,#6613,#4890,.T.);
#8490=EDGE_CURVE('',#6613,#6614,#424,.T.);
#8491=EDGE_CURVE('',#6615,#6614,#2020,.T.);
#8492=EDGE_CURVE('',#6615,#6616,#425,.T.);
#8493=EDGE_CURVE('',#6616,#6617,#4891,.T.);
#8494=EDGE_CURVE('',#6617,#6618,#426,.T.);
#8495=EDGE_CURVE('',#6619,#6618,#2021,.T.);
#8496=EDGE_CURVE('',#6619,#6620,#427,.T.);
#8497=EDGE_CURVE('',#6620,#6621,#4892,.T.);
#8498=EDGE_CURVE('',#6621,#6622,#428,.T.);
#8499=EDGE_CURVE('',#6623,#6622,#2022,.T.);
#8500=EDGE_CURVE('',#6623,#6624,#429,.T.);
#8501=EDGE_CURVE('',#6624,#6625,#4893,.T.);
#8502=EDGE_CURVE('',#6625,#6626,#430,.T.);
#8503=EDGE_CURVE('',#6627,#6626,#2023,.T.);
#8504=EDGE_CURVE('',#6627,#6628,#431,.T.);
#8505=EDGE_CURVE('',#6628,#6629,#4894,.T.);
#8506=EDGE_CURVE('',#6629,#6630,#432,.T.);
#8507=EDGE_CURVE('',#6631,#6630,#2024,.T.);
#8508=EDGE_CURVE('',#6631,#6632,#433,.T.);
#8509=EDGE_CURVE('',#6632,#6633,#4895,.T.);
#8510=EDGE_CURVE('',#6633,#6634,#434,.T.);
#8511=EDGE_CURVE('',#6635,#6634,#2025,.T.);
#8512=EDGE_CURVE('',#6635,#6636,#435,.T.);
#8513=EDGE_CURVE('',#6636,#6637,#4896,.T.);
#8514=EDGE_CURVE('',#6637,#6638,#436,.T.);
#8515=EDGE_CURVE('',#6639,#6638,#2026,.T.);
#8516=EDGE_CURVE('',#6639,#6640,#437,.T.);
#8517=EDGE_CURVE('',#6640,#6641,#4897,.T.);
#8518=EDGE_CURVE('',#6641,#6642,#438,.T.);
#8519=EDGE_CURVE('',#6643,#6642,#2027,.T.);
#8520=EDGE_CURVE('',#6643,#6644,#439,.T.);
#8521=EDGE_CURVE('',#6644,#6645,#4898,.T.);
#8522=EDGE_CURVE('',#6645,#6646,#440,.T.);
#8523=EDGE_CURVE('',#6647,#6646,#2028,.T.);
#8524=EDGE_CURVE('',#6647,#6648,#441,.T.);
#8525=EDGE_CURVE('',#6648,#6649,#4899,.T.);
#8526=EDGE_CURVE('',#6649,#6650,#442,.T.);
#8527=EDGE_CURVE('',#6651,#6650,#2029,.T.);
#8528=EDGE_CURVE('',#6651,#6652,#443,.T.);
#8529=EDGE_CURVE('',#6652,#6653,#4900,.T.);
#8530=EDGE_CURVE('',#6653,#6654,#444,.T.);
#8531=EDGE_CURVE('',#6655,#6654,#2030,.T.);
#8532=EDGE_CURVE('',#6655,#6656,#445,.T.);
#8533=EDGE_CURVE('',#6656,#6657,#4901,.T.);
#8534=EDGE_CURVE('',#6657,#6658,#446,.T.);
#8535=EDGE_CURVE('',#6659,#6658,#2031,.T.);
#8536=EDGE_CURVE('',#6659,#6660,#447,.T.);
#8537=EDGE_CURVE('',#6660,#6661,#4902,.T.);
#8538=EDGE_CURVE('',#6661,#6662,#448,.T.);
#8539=EDGE_CURVE('',#6663,#6662,#2032,.T.);
#8540=EDGE_CURVE('',#6663,#6664,#449,.T.);
#8541=EDGE_CURVE('',#6664,#6665,#4903,.T.);
#8542=EDGE_CURVE('',#6665,#6666,#450,.T.);
#8543=EDGE_CURVE('',#6667,#6666,#2033,.T.);
#8544=EDGE_CURVE('',#6667,#6668,#451,.T.);
#8545=EDGE_CURVE('',#6668,#6669,#4904,.T.);
#8546=EDGE_CURVE('',#6669,#6670,#452,.T.);
#8547=EDGE_CURVE('',#6671,#6670,#2034,.T.);
#8548=EDGE_CURVE('',#6671,#6672,#453,.T.);
#8549=EDGE_CURVE('',#6672,#6673,#4905,.T.);
#8550=EDGE_CURVE('',#6673,#6674,#454,.T.);
#8551=EDGE_CURVE('',#6675,#6674,#2035,.T.);
#8552=EDGE_CURVE('',#6675,#6676,#455,.T.);
#8553=EDGE_CURVE('',#6676,#6677,#4906,.T.);
#8554=EDGE_CURVE('',#6677,#6678,#456,.T.);
#8555=EDGE_CURVE('',#6679,#6678,#2036,.T.);
#8556=EDGE_CURVE('',#6679,#6680,#457,.T.);
#8557=EDGE_CURVE('',#6680,#6681,#4907,.T.);
#8558=EDGE_CURVE('',#6681,#6682,#458,.T.);
#8559=EDGE_CURVE('',#6683,#6682,#2037,.T.);
#8560=EDGE_CURVE('',#6683,#6684,#459,.T.);
#8561=EDGE_CURVE('',#6684,#6685,#4908,.T.);
#8562=EDGE_CURVE('',#6685,#6686,#460,.T.);
#8563=EDGE_CURVE('',#6687,#6686,#2038,.T.);
#8564=EDGE_CURVE('',#6687,#6688,#461,.T.);
#8565=EDGE_CURVE('',#6688,#6689,#4909,.T.);
#8566=EDGE_CURVE('',#6689,#6690,#462,.T.);
#8567=EDGE_CURVE('',#6691,#6690,#2039,.T.);
#8568=EDGE_CURVE('',#6691,#6692,#463,.T.);
#8569=EDGE_CURVE('',#6692,#6693,#4910,.T.);
#8570=EDGE_CURVE('',#6693,#6694,#464,.T.);
#8571=EDGE_CURVE('',#6695,#6694,#2040,.T.);
#8572=EDGE_CURVE('',#6695,#6696,#465,.T.);
#8573=EDGE_CURVE('',#6696,#6697,#4911,.T.);
#8574=EDGE_CURVE('',#6697,#6698,#466,.T.);
#8575=EDGE_CURVE('',#6699,#6698,#2041,.T.);
#8576=EDGE_CURVE('',#6699,#6700,#467,.T.);
#8577=EDGE_CURVE('',#6700,#6701,#4912,.T.);
#8578=EDGE_CURVE('',#6701,#6702,#468,.T.);
#8579=EDGE_CURVE('',#6703,#6702,#2042,.T.);
#8580=EDGE_CURVE('',#6703,#6704,#469,.T.);
#8581=EDGE_CURVE('',#6704,#6705,#4913,.T.);
#8582=EDGE_CURVE('',#6705,#6706,#470,.T.);
#8583=EDGE_CURVE('',#6707,#6706,#2043,.T.);
#8584=EDGE_CURVE('',#6707,#6708,#471,.T.);
#8585=EDGE_CURVE('',#6708,#6709,#4914,.T.);
#8586=EDGE_CURVE('',#6709,#6710,#472,.T.);
#8587=EDGE_CURVE('',#6711,#6710,#2044,.T.);
#8588=EDGE_CURVE('',#6711,#6712,#473,.T.);
#8589=EDGE_CURVE('',#6712,#6713,#4915,.T.);
#8590=EDGE_CURVE('',#6713,#6714,#474,.T.);
#8591=EDGE_CURVE('',#6715,#6714,#2045,.T.);
#8592=EDGE_CURVE('',#6715,#6716,#475,.T.);
#8593=EDGE_CURVE('',#6716,#6717,#4916,.T.);
#8594=EDGE_CURVE('',#6717,#6718,#476,.T.);
#8595=EDGE_CURVE('',#6719,#6718,#2046,.T.);
#8596=EDGE_CURVE('',#6719,#6720,#477,.T.);
#8597=EDGE_CURVE('',#6720,#6601,#4917,.T.);
#8598=EDGE_CURVE('',#6600,#6721,#4918,.T.);
#8599=EDGE_CURVE('',#6721,#6721,#2047,.T.);
#8600=EDGE_CURVE('',#6722,#6723,#478,.T.);
#8601=EDGE_CURVE('',#6723,#6724,#4919,.T.);
#8602=EDGE_CURVE('',#6724,#6725,#479,.T.);
#8603=EDGE_CURVE('',#6725,#6726,#2048,.T.);
#8604=EDGE_CURVE('',#6726,#6727,#480,.T.);
#8605=EDGE_CURVE('',#6727,#6728,#4920,.T.);
#8606=EDGE_CURVE('',#6728,#6729,#481,.T.);
#8607=EDGE_CURVE('',#6729,#6730,#2049,.T.);
#8608=EDGE_CURVE('',#6730,#6731,#482,.T.);
#8609=EDGE_CURVE('',#6731,#6732,#4921,.T.);
#8610=EDGE_CURVE('',#6732,#6733,#483,.T.);
#8611=EDGE_CURVE('',#6733,#6734,#2050,.T.);
#8612=EDGE_CURVE('',#6734,#6735,#484,.T.);
#8613=EDGE_CURVE('',#6735,#6736,#4922,.T.);
#8614=EDGE_CURVE('',#6736,#6737,#485,.T.);
#8615=EDGE_CURVE('',#6737,#6738,#2051,.T.);
#8616=EDGE_CURVE('',#6738,#6739,#486,.T.);
#8617=EDGE_CURVE('',#6739,#6740,#4923,.T.);
#8618=EDGE_CURVE('',#6740,#6741,#487,.T.);
#8619=EDGE_CURVE('',#6741,#6742,#2052,.T.);
#8620=EDGE_CURVE('',#6742,#6743,#488,.T.);
#8621=EDGE_CURVE('',#6743,#6744,#4924,.T.);
#8622=EDGE_CURVE('',#6744,#6745,#489,.T.);
#8623=EDGE_CURVE('',#6745,#6746,#2053,.T.);
#8624=EDGE_CURVE('',#6746,#6747,#490,.T.);
#8625=EDGE_CURVE('',#6747,#6748,#4925,.T.);
#8626=EDGE_CURVE('',#6748,#6749,#491,.T.);
#8627=EDGE_CURVE('',#6749,#6750,#2054,.T.);
#8628=EDGE_CURVE('',#6750,#6751,#492,.T.);
#8629=EDGE_CURVE('',#6751,#6752,#4926,.T.);
#8630=EDGE_CURVE('',#6752,#6753,#493,.T.);
#8631=EDGE_CURVE('',#6753,#6754,#2055,.T.);
#8632=EDGE_CURVE('',#6754,#6755,#494,.T.);
#8633=EDGE_CURVE('',#6755,#6756,#4927,.T.);
#8634=EDGE_CURVE('',#6756,#6757,#495,.T.);
#8635=EDGE_CURVE('',#6757,#6758,#2056,.T.);
#8636=EDGE_CURVE('',#6758,#6759,#496,.T.);
#8637=EDGE_CURVE('',#6759,#6760,#4928,.T.);
#8638=EDGE_CURVE('',#6760,#6761,#497,.T.);
#8639=EDGE_CURVE('',#6761,#6762,#2057,.T.);
#8640=EDGE_CURVE('',#6762,#6763,#498,.T.);
#8641=EDGE_CURVE('',#6763,#6764,#4929,.T.);
#8642=EDGE_CURVE('',#6764,#6765,#499,.T.);
#8643=EDGE_CURVE('',#6765,#6766,#2058,.T.);
#8644=EDGE_CURVE('',#6766,#6767,#500,.T.);
#8645=EDGE_CURVE('',#6767,#6768,#4930,.T.);
#8646=EDGE_CURVE('',#6768,#6769,#501,.T.);
#8647=EDGE_CURVE('',#6769,#6770,#2059,.T.);
#8648=EDGE_CURVE('',#6770,#6771,#502,.T.);
#8649=EDGE_CURVE('',#6771,#6772,#4931,.T.);
#8650=EDGE_CURVE('',#6772,#6773,#503,.T.);
#8651=EDGE_CURVE('',#6773,#6774,#2060,.T.);
#8652=EDGE_CURVE('',#6774,#6775,#504,.T.);
#8653=EDGE_CURVE('',#6775,#6776,#4932,.T.);
#8654=EDGE_CURVE('',#6776,#6777,#505,.T.);
#8655=EDGE_CURVE('',#6777,#6778,#2061,.T.);
#8656=EDGE_CURVE('',#6778,#6779,#506,.T.);
#8657=EDGE_CURVE('',#6779,#6780,#4933,.T.);
#8658=EDGE_CURVE('',#6780,#6781,#507,.T.);
#8659=EDGE_CURVE('',#6781,#6782,#2062,.T.);
#8660=EDGE_CURVE('',#6782,#6783,#508,.T.);
#8661=EDGE_CURVE('',#6783,#6784,#4934,.T.);
#8662=EDGE_CURVE('',#6784,#6785,#509,.T.);
#8663=EDGE_CURVE('',#6785,#6786,#2063,.T.);
#8664=EDGE_CURVE('',#6786,#6787,#510,.T.);
#8665=EDGE_CURVE('',#6787,#6788,#4935,.T.);
#8666=EDGE_CURVE('',#6788,#6789,#511,.T.);
#8667=EDGE_CURVE('',#6789,#6790,#2064,.T.);
#8668=EDGE_CURVE('',#6790,#6791,#512,.T.);
#8669=EDGE_CURVE('',#6791,#6792,#4936,.T.);
#8670=EDGE_CURVE('',#6792,#6793,#513,.T.);
#8671=EDGE_CURVE('',#6793,#6794,#2065,.T.);
#8672=EDGE_CURVE('',#6794,#6795,#514,.T.);
#8673=EDGE_CURVE('',#6795,#6796,#4937,.T.);
#8674=EDGE_CURVE('',#6796,#6797,#515,.T.);
#8675=EDGE_CURVE('',#6797,#6798,#2066,.T.);
#8676=EDGE_CURVE('',#6798,#6799,#516,.T.);
#8677=EDGE_CURVE('',#6799,#6800,#4938,.T.);
#8678=EDGE_CURVE('',#6800,#6801,#517,.T.);
#8679=EDGE_CURVE('',#6801,#6802,#2067,.T.);
#8680=EDGE_CURVE('',#6802,#6803,#518,.T.);
#8681=EDGE_CURVE('',#6803,#6804,#4939,.T.);
#8682=EDGE_CURVE('',#6804,#6805,#519,.T.);
#8683=EDGE_CURVE('',#6805,#6806,#2068,.T.);
#8684=EDGE_CURVE('',#6806,#6807,#520,.T.);
#8685=EDGE_CURVE('',#6807,#6808,#4940,.T.);
#8686=EDGE_CURVE('',#6808,#6809,#521,.T.);
#8687=EDGE_CURVE('',#6809,#6810,#2069,.T.);
#8688=EDGE_CURVE('',#6810,#6811,#522,.T.);
#8689=EDGE_CURVE('',#6811,#6812,#4941,.T.);
#8690=EDGE_CURVE('',#6812,#6813,#523,.T.);
#8691=EDGE_CURVE('',#6813,#6814,#2070,.T.);
#8692=EDGE_CURVE('',#6814,#6815,#524,.T.);
#8693=EDGE_CURVE('',#6815,#6816,#4942,.T.);
#8694=EDGE_CURVE('',#6816,#6817,#525,.T.);
#8695=EDGE_CURVE('',#6817,#6818,#2071,.T.);
#8696=EDGE_CURVE('',#6818,#6819,#526,.T.);
#8697=EDGE_CURVE('',#6819,#6820,#4943,.T.);
#8698=EDGE_CURVE('',#6820,#6821,#527,.T.);
#8699=EDGE_CURVE('',#6821,#6822,#2072,.T.);
#8700=EDGE_CURVE('',#6822,#6823,#528,.T.);
#8701=EDGE_CURVE('',#6823,#6824,#4944,.T.);
#8702=EDGE_CURVE('',#6824,#6825,#529,.T.);
#8703=EDGE_CURVE('',#6825,#6826,#2073,.T.);
#8704=EDGE_CURVE('',#6826,#6827,#530,.T.);
#8705=EDGE_CURVE('',#6827,#6828,#4945,.T.);
#8706=EDGE_CURVE('',#6828,#6829,#531,.T.);
#8707=EDGE_CURVE('',#6829,#6830,#2074,.T.);
#8708=EDGE_CURVE('',#6830,#6831,#532,.T.);
#8709=EDGE_CURVE('',#6831,#6832,#4946,.T.);
#8710=EDGE_CURVE('',#6832,#6833,#533,.T.);
#8711=EDGE_CURVE('',#6833,#6834,#2075,.T.);
#8712=EDGE_CURVE('',#6834,#6835,#534,.T.);
#8713=EDGE_CURVE('',#6835,#6836,#4947,.T.);
#8714=EDGE_CURVE('',#6836,#6837,#535,.T.);
#8715=EDGE_CURVE('',#6837,#6838,#2076,.T.);
#8716=EDGE_CURVE('',#6838,#6839,#536,.T.);
#8717=EDGE_CURVE('',#6839,#6840,#4948,.T.);
#8718=EDGE_CURVE('',#6840,#6841,#537,.T.);
#8719=EDGE_CURVE('',#6841,#6722,#2077,.T.);
#8720=EDGE_CURVE('',#6720,#6724,#538,.T.);
#8721=EDGE_CURVE('',#6842,#6719,#539,.T.);
#8722=EDGE_CURVE('',#6843,#6842,#540,.T.);
#8723=EDGE_CURVE('',#6844,#6843,#541,.T.);
#8724=EDGE_CURVE('',#6845,#6844,#542,.T.);
#8725=EDGE_CURVE('',#6725,#6845,#543,.T.);
#8726=EDGE_CURVE('',#6601,#6723,#544,.T.);
#8727=EDGE_CURVE('',#6846,#6722,#545,.T.);
#8728=EDGE_CURVE('',#6847,#6846,#546,.T.);
#8729=EDGE_CURVE('',#6848,#6847,#547,.T.);
#8730=EDGE_CURVE('',#6849,#6848,#548,.T.);
#8731=EDGE_CURVE('',#6602,#6849,#549,.T.);
#8732=EDGE_CURVE('',#6845,#6850,#2078,.T.);
#8733=EDGE_CURVE('',#6850,#6726,#550,.T.);
#8734=EDGE_CURVE('',#6844,#6851,#2079,.T.);
#8735=EDGE_CURVE('',#6851,#6850,#551,.T.);
#8736=EDGE_CURVE('',#6843,#6852,#2080,.T.);
#8737=EDGE_CURVE('',#6852,#6851,#552,.T.);
#8738=EDGE_CURVE('',#6842,#6853,#2081,.T.);
#8739=EDGE_CURVE('',#6853,#6852,#553,.T.);
#8740=EDGE_CURVE('',#6718,#6853,#554,.T.);
#8741=EDGE_CURVE('',#6604,#6840,#555,.T.);
#8742=EDGE_CURVE('',#6854,#6603,#556,.T.);
#8743=EDGE_CURVE('',#6855,#6854,#557,.T.);
#8744=EDGE_CURVE('',#6856,#6855,#558,.T.);
#8745=EDGE_CURVE('',#6857,#6856,#559,.T.);
#8746=EDGE_CURVE('',#6841,#6857,#560,.T.);
#8747=EDGE_CURVE('',#6605,#6839,#561,.T.);
#8748=EDGE_CURVE('',#6858,#6838,#562,.T.);
#8749=EDGE_CURVE('',#6859,#6858,#563,.T.);
#8750=EDGE_CURVE('',#6860,#6859,#564,.T.);
#8751=EDGE_CURVE('',#6861,#6860,#565,.T.);
#8752=EDGE_CURVE('',#6606,#6861,#566,.T.);
#8753=EDGE_CURVE('',#6857,#6846,#2082,.T.);
#8754=EDGE_CURVE('',#6856,#6847,#2083,.T.);
#8755=EDGE_CURVE('',#6855,#6848,#2084,.T.);
#8756=EDGE_CURVE('',#6854,#6849,#2085,.T.);
#8757=EDGE_CURVE('',#6608,#6836,#567,.T.);
#8758=EDGE_CURVE('',#6862,#6607,#568,.T.);
#8759=EDGE_CURVE('',#6863,#6862,#569,.T.);
#8760=EDGE_CURVE('',#6864,#6863,#570,.T.);
#8761=EDGE_CURVE('',#6865,#6864,#571,.T.);
#8762=EDGE_CURVE('',#6837,#6865,#572,.T.);
#8763=EDGE_CURVE('',#6609,#6835,#573,.T.);
#8764=EDGE_CURVE('',#6866,#6834,#574,.T.);
#8765=EDGE_CURVE('',#6867,#6866,#575,.T.);
#8766=EDGE_CURVE('',#6868,#6867,#576,.T.);
#8767=EDGE_CURVE('',#6869,#6868,#577,.T.);
#8768=EDGE_CURVE('',#6610,#6869,#578,.T.);
#8769=EDGE_CURVE('',#6865,#6858,#2086,.T.);
#8770=EDGE_CURVE('',#6864,#6859,#2087,.T.);
#8771=EDGE_CURVE('',#6863,#6860,#2088,.T.);
#8772=EDGE_CURVE('',#6862,#6861,#2089,.T.);
#8773=EDGE_CURVE('',#6612,#6832,#579,.T.);
#8774=EDGE_CURVE('',#6870,#6611,#580,.T.);
#8775=EDGE_CURVE('',#6871,#6870,#581,.T.);
#8776=EDGE_CURVE('',#6872,#6871,#582,.T.);
#8777=EDGE_CURVE('',#6873,#6872,#583,.T.);
#8778=EDGE_CURVE('',#6833,#6873,#584,.T.);
#8779=EDGE_CURVE('',#6613,#6831,#585,.T.);
#8780=EDGE_CURVE('',#6874,#6830,#586,.T.);
#8781=EDGE_CURVE('',#6875,#6874,#587,.T.);
#8782=EDGE_CURVE('',#6876,#6875,#588,.T.);
#8783=EDGE_CURVE('',#6877,#6876,#589,.T.);
#8784=EDGE_CURVE('',#6614,#6877,#590,.T.);
#8785=EDGE_CURVE('',#6873,#6866,#2090,.T.);
#8786=EDGE_CURVE('',#6872,#6867,#2091,.T.);
#8787=EDGE_CURVE('',#6871,#6868,#2092,.T.);
#8788=EDGE_CURVE('',#6870,#6869,#2093,.T.);
#8789=EDGE_CURVE('',#6616,#6828,#591,.T.);
#8790=EDGE_CURVE('',#6878,#6615,#592,.T.);
#8791=EDGE_CURVE('',#6879,#6878,#593,.T.);
#8792=EDGE_CURVE('',#6880,#6879,#594,.T.);
#8793=EDGE_CURVE('',#6881,#6880,#595,.T.);
#8794=EDGE_CURVE('',#6829,#6881,#596,.T.);
#8795=EDGE_CURVE('',#6617,#6827,#597,.T.);
#8796=EDGE_CURVE('',#6882,#6826,#598,.T.);
#8797=EDGE_CURVE('',#6883,#6882,#599,.T.);
#8798=EDGE_CURVE('',#6884,#6883,#600,.T.);
#8799=EDGE_CURVE('',#6885,#6884,#601,.T.);
#8800=EDGE_CURVE('',#6618,#6885,#602,.T.);
#8801=EDGE_CURVE('',#6881,#6874,#2094,.T.);
#8802=EDGE_CURVE('',#6880,#6875,#2095,.T.);
#8803=EDGE_CURVE('',#6879,#6876,#2096,.T.);
#8804=EDGE_CURVE('',#6878,#6877,#2097,.T.);
#8805=EDGE_CURVE('',#6620,#6824,#603,.T.);
#8806=EDGE_CURVE('',#6886,#6619,#604,.T.);
#8807=EDGE_CURVE('',#6887,#6886,#605,.T.);
#8808=EDGE_CURVE('',#6888,#6887,#606,.T.);
#8809=EDGE_CURVE('',#6889,#6888,#607,.T.);
#8810=EDGE_CURVE('',#6825,#6889,#608,.T.);
#8811=EDGE_CURVE('',#6621,#6823,#609,.T.);
#8812=EDGE_CURVE('',#6890,#6822,#610,.T.);
#8813=EDGE_CURVE('',#6891,#6890,#611,.T.);
#8814=EDGE_CURVE('',#6892,#6891,#612,.T.);
#8815=EDGE_CURVE('',#6893,#6892,#613,.T.);
#8816=EDGE_CURVE('',#6622,#6893,#614,.T.);
#8817=EDGE_CURVE('',#6889,#6882,#2098,.T.);
#8818=EDGE_CURVE('',#6888,#6883,#2099,.T.);
#8819=EDGE_CURVE('',#6887,#6884,#2100,.T.);
#8820=EDGE_CURVE('',#6886,#6885,#2101,.T.);
#8821=EDGE_CURVE('',#6624,#6820,#615,.T.);
#8822=EDGE_CURVE('',#6894,#6623,#616,.T.);
#8823=EDGE_CURVE('',#6895,#6894,#617,.T.);
#8824=EDGE_CURVE('',#6896,#6895,#618,.T.);
#8825=EDGE_CURVE('',#6897,#6896,#619,.T.);
#8826=EDGE_CURVE('',#6821,#6897,#620,.T.);
#8827=EDGE_CURVE('',#6625,#6819,#621,.T.);
#8828=EDGE_CURVE('',#6898,#6818,#622,.T.);
#8829=EDGE_CURVE('',#6899,#6898,#623,.T.);
#8830=EDGE_CURVE('',#6900,#6899,#624,.T.);
#8831=EDGE_CURVE('',#6901,#6900,#625,.T.);
#8832=EDGE_CURVE('',#6626,#6901,#626,.T.);
#8833=EDGE_CURVE('',#6897,#6890,#2102,.T.);
#8834=EDGE_CURVE('',#6896,#6891,#2103,.T.);
#8835=EDGE_CURVE('',#6895,#6892,#2104,.T.);
#8836=EDGE_CURVE('',#6894,#6893,#2105,.T.);
#8837=EDGE_CURVE('',#6628,#6816,#627,.T.);
#8838=EDGE_CURVE('',#6902,#6627,#628,.T.);
#8839=EDGE_CURVE('',#6903,#6902,#629,.T.);
#8840=EDGE_CURVE('',#6904,#6903,#630,.T.);
#8841=EDGE_CURVE('',#6905,#6904,#631,.T.);
#8842=EDGE_CURVE('',#6817,#6905,#632,.T.);
#8843=EDGE_CURVE('',#6629,#6815,#633,.T.);
#8844=EDGE_CURVE('',#6906,#6814,#634,.T.);
#8845=EDGE_CURVE('',#6907,#6906,#635,.T.);
#8846=EDGE_CURVE('',#6908,#6907,#636,.T.);
#8847=EDGE_CURVE('',#6909,#6908,#637,.T.);
#8848=EDGE_CURVE('',#6630,#6909,#638,.T.);
#8849=EDGE_CURVE('',#6905,#6898,#2106,.T.);
#8850=EDGE_CURVE('',#6904,#6899,#2107,.T.);
#8851=EDGE_CURVE('',#6903,#6900,#2108,.T.);
#8852=EDGE_CURVE('',#6902,#6901,#2109,.T.);
#8853=EDGE_CURVE('',#6632,#6812,#639,.T.);
#8854=EDGE_CURVE('',#6910,#6631,#640,.T.);
#8855=EDGE_CURVE('',#6911,#6910,#641,.T.);
#8856=EDGE_CURVE('',#6912,#6911,#642,.T.);
#8857=EDGE_CURVE('',#6913,#6912,#643,.T.);
#8858=EDGE_CURVE('',#6813,#6913,#644,.T.);
#8859=EDGE_CURVE('',#6633,#6811,#645,.T.);
#8860=EDGE_CURVE('',#6914,#6810,#646,.T.);
#8861=EDGE_CURVE('',#6915,#6914,#647,.T.);
#8862=EDGE_CURVE('',#6916,#6915,#648,.T.);
#8863=EDGE_CURVE('',#6917,#6916,#649,.T.);
#8864=EDGE_CURVE('',#6634,#6917,#650,.T.);
#8865=EDGE_CURVE('',#6913,#6906,#2110,.T.);
#8866=EDGE_CURVE('',#6912,#6907,#2111,.T.);
#8867=EDGE_CURVE('',#6911,#6908,#2112,.T.);
#8868=EDGE_CURVE('',#6910,#6909,#2113,.T.);
#8869=EDGE_CURVE('',#6636,#6808,#651,.T.);
#8870=EDGE_CURVE('',#6918,#6635,#652,.T.);
#8871=EDGE_CURVE('',#6919,#6918,#653,.T.);
#8872=EDGE_CURVE('',#6920,#6919,#654,.T.);
#8873=EDGE_CURVE('',#6921,#6920,#655,.T.);
#8874=EDGE_CURVE('',#6809,#6921,#656,.T.);
#8875=EDGE_CURVE('',#6637,#6807,#657,.T.);
#8876=EDGE_CURVE('',#6922,#6806,#658,.T.);
#8877=EDGE_CURVE('',#6923,#6922,#659,.T.);
#8878=EDGE_CURVE('',#6924,#6923,#660,.T.);
#8879=EDGE_CURVE('',#6925,#6924,#661,.T.);
#8880=EDGE_CURVE('',#6638,#6925,#662,.T.);
#8881=EDGE_CURVE('',#6921,#6914,#2114,.T.);
#8882=EDGE_CURVE('',#6920,#6915,#2115,.T.);
#8883=EDGE_CURVE('',#6919,#6916,#2116,.T.);
#8884=EDGE_CURVE('',#6918,#6917,#2117,.T.);
#8885=EDGE_CURVE('',#6640,#6804,#663,.T.);
#8886=EDGE_CURVE('',#6926,#6639,#664,.T.);
#8887=EDGE_CURVE('',#6927,#6926,#665,.T.);
#8888=EDGE_CURVE('',#6928,#6927,#666,.T.);
#8889=EDGE_CURVE('',#6929,#6928,#667,.T.);
#8890=EDGE_CURVE('',#6805,#6929,#668,.T.);
#8891=EDGE_CURVE('',#6641,#6803,#669,.T.);
#8892=EDGE_CURVE('',#6930,#6802,#670,.T.);
#8893=EDGE_CURVE('',#6931,#6930,#671,.T.);
#8894=EDGE_CURVE('',#6932,#6931,#672,.T.);
#8895=EDGE_CURVE('',#6933,#6932,#673,.T.);
#8896=EDGE_CURVE('',#6642,#6933,#674,.T.);
#8897=EDGE_CURVE('',#6929,#6922,#2118,.T.);
#8898=EDGE_CURVE('',#6928,#6923,#2119,.T.);
#8899=EDGE_CURVE('',#6927,#6924,#2120,.T.);
#8900=EDGE_CURVE('',#6926,#6925,#2121,.T.);
#8901=EDGE_CURVE('',#6644,#6800,#675,.T.);
#8902=EDGE_CURVE('',#6934,#6643,#676,.T.);
#8903=EDGE_CURVE('',#6935,#6934,#677,.T.);
#8904=EDGE_CURVE('',#6936,#6935,#678,.T.);
#8905=EDGE_CURVE('',#6937,#6936,#679,.T.);
#8906=EDGE_CURVE('',#6801,#6937,#680,.T.);
#8907=EDGE_CURVE('',#6645,#6799,#681,.T.);
#8908=EDGE_CURVE('',#6938,#6798,#682,.T.);
#8909=EDGE_CURVE('',#6939,#6938,#683,.T.);
#8910=EDGE_CURVE('',#6940,#6939,#684,.T.);
#8911=EDGE_CURVE('',#6941,#6940,#685,.T.);
#8912=EDGE_CURVE('',#6646,#6941,#686,.T.);
#8913=EDGE_CURVE('',#6937,#6930,#2122,.T.);
#8914=EDGE_CURVE('',#6936,#6931,#2123,.T.);
#8915=EDGE_CURVE('',#6935,#6932,#2124,.T.);
#8916=EDGE_CURVE('',#6934,#6933,#2125,.T.);
#8917=EDGE_CURVE('',#6648,#6796,#687,.T.);
#8918=EDGE_CURVE('',#6942,#6647,#688,.T.);
#8919=EDGE_CURVE('',#6943,#6942,#689,.T.);
#8920=EDGE_CURVE('',#6944,#6943,#690,.T.);
#8921=EDGE_CURVE('',#6945,#6944,#691,.T.);
#8922=EDGE_CURVE('',#6797,#6945,#692,.T.);
#8923=EDGE_CURVE('',#6649,#6795,#693,.T.);
#8924=EDGE_CURVE('',#6946,#6794,#694,.T.);
#8925=EDGE_CURVE('',#6947,#6946,#695,.T.);
#8926=EDGE_CURVE('',#6948,#6947,#696,.T.);
#8927=EDGE_CURVE('',#6949,#6948,#697,.T.);
#8928=EDGE_CURVE('',#6650,#6949,#698,.T.);
#8929=EDGE_CURVE('',#6945,#6938,#2126,.T.);
#8930=EDGE_CURVE('',#6944,#6939,#2127,.T.);
#8931=EDGE_CURVE('',#6943,#6940,#2128,.T.);
#8932=EDGE_CURVE('',#6942,#6941,#2129,.T.);
#8933=EDGE_CURVE('',#6652,#6792,#699,.T.);
#8934=EDGE_CURVE('',#6950,#6651,#700,.T.);
#8935=EDGE_CURVE('',#6951,#6950,#701,.T.);
#8936=EDGE_CURVE('',#6952,#6951,#702,.T.);
#8937=EDGE_CURVE('',#6953,#6952,#703,.T.);
#8938=EDGE_CURVE('',#6793,#6953,#704,.T.);
#8939=EDGE_CURVE('',#6653,#6791,#705,.T.);
#8940=EDGE_CURVE('',#6954,#6790,#706,.T.);
#8941=EDGE_CURVE('',#6955,#6954,#707,.T.);
#8942=EDGE_CURVE('',#6956,#6955,#708,.T.);
#8943=EDGE_CURVE('',#6957,#6956,#709,.T.);
#8944=EDGE_CURVE('',#6654,#6957,#710,.T.);
#8945=EDGE_CURVE('',#6953,#6946,#2130,.T.);
#8946=EDGE_CURVE('',#6952,#6947,#2131,.T.);
#8947=EDGE_CURVE('',#6951,#6948,#2132,.T.);
#8948=EDGE_CURVE('',#6950,#6949,#2133,.T.);
#8949=EDGE_CURVE('',#6656,#6788,#711,.T.);
#8950=EDGE_CURVE('',#6958,#6655,#712,.T.);
#8951=EDGE_CURVE('',#6959,#6958,#713,.T.);
#8952=EDGE_CURVE('',#6960,#6959,#714,.T.);
#8953=EDGE_CURVE('',#6961,#6960,#715,.T.);
#8954=EDGE_CURVE('',#6789,#6961,#716,.T.);
#8955=EDGE_CURVE('',#6657,#6787,#717,.T.);
#8956=EDGE_CURVE('',#6962,#6786,#718,.T.);
#8957=EDGE_CURVE('',#6963,#6962,#719,.T.);
#8958=EDGE_CURVE('',#6964,#6963,#720,.T.);
#8959=EDGE_CURVE('',#6965,#6964,#721,.T.);
#8960=EDGE_CURVE('',#6658,#6965,#722,.T.);
#8961=EDGE_CURVE('',#6961,#6954,#2134,.T.);
#8962=EDGE_CURVE('',#6960,#6955,#2135,.T.);
#8963=EDGE_CURVE('',#6959,#6956,#2136,.T.);
#8964=EDGE_CURVE('',#6958,#6957,#2137,.T.);
#8965=EDGE_CURVE('',#6660,#6784,#723,.T.);
#8966=EDGE_CURVE('',#6966,#6659,#724,.T.);
#8967=EDGE_CURVE('',#6967,#6966,#725,.T.);
#8968=EDGE_CURVE('',#6968,#6967,#726,.T.);
#8969=EDGE_CURVE('',#6969,#6968,#727,.T.);
#8970=EDGE_CURVE('',#6785,#6969,#728,.T.);
#8971=EDGE_CURVE('',#6661,#6783,#729,.T.);
#8972=EDGE_CURVE('',#6970,#6782,#730,.T.);
#8973=EDGE_CURVE('',#6971,#6970,#731,.T.);
#8974=EDGE_CURVE('',#6972,#6971,#732,.T.);
#8975=EDGE_CURVE('',#6973,#6972,#733,.T.);
#8976=EDGE_CURVE('',#6662,#6973,#734,.T.);
#8977=EDGE_CURVE('',#6969,#6962,#2138,.T.);
#8978=EDGE_CURVE('',#6968,#6963,#2139,.T.);
#8979=EDGE_CURVE('',#6967,#6964,#2140,.T.);
#8980=EDGE_CURVE('',#6966,#6965,#2141,.T.);
#8981=EDGE_CURVE('',#6664,#6780,#735,.T.);
#8982=EDGE_CURVE('',#6974,#6663,#736,.T.);
#8983=EDGE_CURVE('',#6975,#6974,#737,.T.);
#8984=EDGE_CURVE('',#6976,#6975,#738,.T.);
#8985=EDGE_CURVE('',#6977,#6976,#739,.T.);
#8986=EDGE_CURVE('',#6781,#6977,#740,.T.);
#8987=EDGE_CURVE('',#6665,#6779,#741,.T.);
#8988=EDGE_CURVE('',#6978,#6778,#742,.T.);
#8989=EDGE_CURVE('',#6979,#6978,#743,.T.);
#8990=EDGE_CURVE('',#6980,#6979,#744,.T.);
#8991=EDGE_CURVE('',#6981,#6980,#745,.T.);
#8992=EDGE_CURVE('',#6666,#6981,#746,.T.);
#8993=EDGE_CURVE('',#6977,#6970,#2142,.T.);
#8994=EDGE_CURVE('',#6976,#6971,#2143,.T.);
#8995=EDGE_CURVE('',#6975,#6972,#2144,.T.);
#8996=EDGE_CURVE('',#6974,#6973,#2145,.T.);
#8997=EDGE_CURVE('',#6668,#6776,#747,.T.);
#8998=EDGE_CURVE('',#6982,#6667,#748,.T.);
#8999=EDGE_CURVE('',#6983,#6982,#749,.T.);
#9000=EDGE_CURVE('',#6984,#6983,#750,.T.);
#9001=EDGE_CURVE('',#6985,#6984,#751,.T.);
#9002=EDGE_CURVE('',#6777,#6985,#752,.T.);
#9003=EDGE_CURVE('',#6669,#6775,#753,.T.);
#9004=EDGE_CURVE('',#6986,#6774,#754,.T.);
#9005=EDGE_CURVE('',#6987,#6986,#755,.T.);
#9006=EDGE_CURVE('',#6988,#6987,#756,.T.);
#9007=EDGE_CURVE('',#6989,#6988,#757,.T.);
#9008=EDGE_CURVE('',#6670,#6989,#758,.T.);
#9009=EDGE_CURVE('',#6985,#6978,#2146,.T.);
#9010=EDGE_CURVE('',#6984,#6979,#2147,.T.);
#9011=EDGE_CURVE('',#6983,#6980,#2148,.T.);
#9012=EDGE_CURVE('',#6982,#6981,#2149,.T.);
#9013=EDGE_CURVE('',#6672,#6772,#759,.T.);
#9014=EDGE_CURVE('',#6990,#6671,#760,.T.);
#9015=EDGE_CURVE('',#6991,#6990,#761,.T.);
#9016=EDGE_CURVE('',#6992,#6991,#762,.T.);
#9017=EDGE_CURVE('',#6993,#6992,#763,.T.);
#9018=EDGE_CURVE('',#6773,#6993,#764,.T.);
#9019=EDGE_CURVE('',#6673,#6771,#765,.T.);
#9020=EDGE_CURVE('',#6994,#6770,#766,.T.);
#9021=EDGE_CURVE('',#6995,#6994,#767,.T.);
#9022=EDGE_CURVE('',#6996,#6995,#768,.T.);
#9023=EDGE_CURVE('',#6997,#6996,#769,.T.);
#9024=EDGE_CURVE('',#6674,#6997,#770,.T.);
#9025=EDGE_CURVE('',#6993,#6986,#2150,.T.);
#9026=EDGE_CURVE('',#6992,#6987,#2151,.T.);
#9027=EDGE_CURVE('',#6991,#6988,#2152,.T.);
#9028=EDGE_CURVE('',#6990,#6989,#2153,.T.);
#9029=EDGE_CURVE('',#6676,#6768,#771,.T.);
#9030=EDGE_CURVE('',#6998,#6675,#772,.T.);
#9031=EDGE_CURVE('',#6999,#6998,#773,.T.);
#9032=EDGE_CURVE('',#7000,#6999,#774,.T.);
#9033=EDGE_CURVE('',#7001,#7000,#775,.T.);
#9034=EDGE_CURVE('',#6769,#7001,#776,.T.);
#9035=EDGE_CURVE('',#6677,#6767,#777,.T.);
#9036=EDGE_CURVE('',#7002,#6766,#778,.T.);
#9037=EDGE_CURVE('',#7003,#7002,#779,.T.);
#9038=EDGE_CURVE('',#7004,#7003,#780,.T.);
#9039=EDGE_CURVE('',#7005,#7004,#781,.T.);
#9040=EDGE_CURVE('',#6678,#7005,#782,.T.);
#9041=EDGE_CURVE('',#7001,#6994,#2154,.T.);
#9042=EDGE_CURVE('',#7000,#6995,#2155,.T.);
#9043=EDGE_CURVE('',#6999,#6996,#2156,.T.);
#9044=EDGE_CURVE('',#6998,#6997,#2157,.T.);
#9045=EDGE_CURVE('',#6680,#6764,#783,.T.);
#9046=EDGE_CURVE('',#7006,#6679,#784,.T.);
#9047=EDGE_CURVE('',#7007,#7006,#785,.T.);
#9048=EDGE_CURVE('',#7008,#7007,#786,.T.);
#9049=EDGE_CURVE('',#7009,#7008,#787,.T.);
#9050=EDGE_CURVE('',#6765,#7009,#788,.T.);
#9051=EDGE_CURVE('',#6681,#6763,#789,.T.);
#9052=EDGE_CURVE('',#7010,#6762,#790,.T.);
#9053=EDGE_CURVE('',#7011,#7010,#791,.T.);
#9054=EDGE_CURVE('',#7012,#7011,#792,.T.);
#9055=EDGE_CURVE('',#7013,#7012,#793,.T.);
#9056=EDGE_CURVE('',#6682,#7013,#794,.T.);
#9057=EDGE_CURVE('',#7009,#7002,#2158,.T.);
#9058=EDGE_CURVE('',#7008,#7003,#2159,.T.);
#9059=EDGE_CURVE('',#7007,#7004,#2160,.T.);
#9060=EDGE_CURVE('',#7006,#7005,#2161,.T.);
#9061=EDGE_CURVE('',#6684,#6760,#795,.T.);
#9062=EDGE_CURVE('',#7014,#6683,#796,.T.);
#9063=EDGE_CURVE('',#7015,#7014,#797,.T.);
#9064=EDGE_CURVE('',#7016,#7015,#798,.T.);
#9065=EDGE_CURVE('',#7017,#7016,#799,.T.);
#9066=EDGE_CURVE('',#6761,#7017,#800,.T.);
#9067=EDGE_CURVE('',#6685,#6759,#801,.T.);
#9068=EDGE_CURVE('',#7018,#6758,#802,.T.);
#9069=EDGE_CURVE('',#7019,#7018,#803,.T.);
#9070=EDGE_CURVE('',#7020,#7019,#804,.T.);
#9071=EDGE_CURVE('',#7021,#7020,#805,.T.);
#9072=EDGE_CURVE('',#6686,#7021,#806,.T.);
#9073=EDGE_CURVE('',#7017,#7010,#2162,.T.);
#9074=EDGE_CURVE('',#7016,#7011,#2163,.T.);
#9075=EDGE_CURVE('',#7015,#7012,#2164,.T.);
#9076=EDGE_CURVE('',#7014,#7013,#2165,.T.);
#9077=EDGE_CURVE('',#6688,#6756,#807,.T.);
#9078=EDGE_CURVE('',#7022,#6687,#808,.T.);
#9079=EDGE_CURVE('',#7023,#7022,#809,.T.);
#9080=EDGE_CURVE('',#7024,#7023,#810,.T.);
#9081=EDGE_CURVE('',#7025,#7024,#811,.T.);
#9082=EDGE_CURVE('',#6757,#7025,#812,.T.);
#9083=EDGE_CURVE('',#6689,#6755,#813,.T.);
#9084=EDGE_CURVE('',#7026,#6754,#814,.T.);
#9085=EDGE_CURVE('',#7027,#7026,#815,.T.);
#9086=EDGE_CURVE('',#7028,#7027,#816,.T.);
#9087=EDGE_CURVE('',#7029,#7028,#817,.T.);
#9088=EDGE_CURVE('',#6690,#7029,#818,.T.);
#9089=EDGE_CURVE('',#7025,#7018,#2166,.T.);
#9090=EDGE_CURVE('',#7024,#7019,#2167,.T.);
#9091=EDGE_CURVE('',#7023,#7020,#2168,.T.);
#9092=EDGE_CURVE('',#7022,#7021,#2169,.T.);
#9093=EDGE_CURVE('',#6692,#6752,#819,.T.);
#9094=EDGE_CURVE('',#7030,#6691,#820,.T.);
#9095=EDGE_CURVE('',#7031,#7030,#821,.T.);
#9096=EDGE_CURVE('',#7032,#7031,#822,.T.);
#9097=EDGE_CURVE('',#7033,#7032,#823,.T.);
#9098=EDGE_CURVE('',#6753,#7033,#824,.T.);
#9099=EDGE_CURVE('',#6693,#6751,#825,.T.);
#9100=EDGE_CURVE('',#7034,#6750,#826,.T.);
#9101=EDGE_CURVE('',#7035,#7034,#827,.T.);
#9102=EDGE_CURVE('',#7036,#7035,#828,.T.);
#9103=EDGE_CURVE('',#7037,#7036,#829,.T.);
#9104=EDGE_CURVE('',#6694,#7037,#830,.T.);
#9105=EDGE_CURVE('',#7033,#7026,#2170,.T.);
#9106=EDGE_CURVE('',#7032,#7027,#2171,.T.);
#9107=EDGE_CURVE('',#7031,#7028,#2172,.T.);
#9108=EDGE_CURVE('',#7030,#7029,#2173,.T.);
#9109=EDGE_CURVE('',#6696,#6748,#831,.T.);
#9110=EDGE_CURVE('',#7038,#6695,#832,.T.);
#9111=EDGE_CURVE('',#7039,#7038,#833,.T.);
#9112=EDGE_CURVE('',#7040,#7039,#834,.T.);
#9113=EDGE_CURVE('',#7041,#7040,#835,.T.);
#9114=EDGE_CURVE('',#6749,#7041,#836,.T.);
#9115=EDGE_CURVE('',#6697,#6747,#837,.T.);
#9116=EDGE_CURVE('',#7042,#6746,#838,.T.);
#9117=EDGE_CURVE('',#7043,#7042,#839,.T.);
#9118=EDGE_CURVE('',#7044,#7043,#840,.T.);
#9119=EDGE_CURVE('',#7045,#7044,#841,.T.);
#9120=EDGE_CURVE('',#6698,#7045,#842,.T.);
#9121=EDGE_CURVE('',#7041,#7034,#2174,.T.);
#9122=EDGE_CURVE('',#7040,#7035,#2175,.T.);
#9123=EDGE_CURVE('',#7039,#7036,#2176,.T.);
#9124=EDGE_CURVE('',#7038,#7037,#2177,.T.);
#9125=EDGE_CURVE('',#6700,#6744,#843,.T.);
#9126=EDGE_CURVE('',#7046,#6699,#844,.T.);
#9127=EDGE_CURVE('',#7047,#7046,#845,.T.);
#9128=EDGE_CURVE('',#7048,#7047,#846,.T.);
#9129=EDGE_CURVE('',#7049,#7048,#847,.T.);
#9130=EDGE_CURVE('',#6745,#7049,#848,.T.);
#9131=EDGE_CURVE('',#6701,#6743,#849,.T.);
#9132=EDGE_CURVE('',#7050,#6742,#850,.T.);
#9133=EDGE_CURVE('',#7051,#7050,#851,.T.);
#9134=EDGE_CURVE('',#7052,#7051,#852,.T.);
#9135=EDGE_CURVE('',#7053,#7052,#853,.T.);
#9136=EDGE_CURVE('',#6702,#7053,#854,.T.);
#9137=EDGE_CURVE('',#7049,#7042,#2178,.T.);
#9138=EDGE_CURVE('',#7048,#7043,#2179,.T.);
#9139=EDGE_CURVE('',#7047,#7044,#2180,.T.);
#9140=EDGE_CURVE('',#7046,#7045,#2181,.T.);
#9141=EDGE_CURVE('',#6704,#6740,#855,.T.);
#9142=EDGE_CURVE('',#7054,#6703,#856,.T.);
#9143=EDGE_CURVE('',#7055,#7054,#857,.T.);
#9144=EDGE_CURVE('',#7056,#7055,#858,.T.);
#9145=EDGE_CURVE('',#7057,#7056,#859,.T.);
#9146=EDGE_CURVE('',#6741,#7057,#860,.T.);
#9147=EDGE_CURVE('',#6705,#6739,#861,.T.);
#9148=EDGE_CURVE('',#7058,#6738,#862,.T.);
#9149=EDGE_CURVE('',#7059,#7058,#863,.T.);
#9150=EDGE_CURVE('',#7060,#7059,#864,.T.);
#9151=EDGE_CURVE('',#7061,#7060,#865,.T.);
#9152=EDGE_CURVE('',#6706,#7061,#866,.T.);
#9153=EDGE_CURVE('',#7057,#7050,#2182,.T.);
#9154=EDGE_CURVE('',#7056,#7051,#2183,.T.);
#9155=EDGE_CURVE('',#7055,#7052,#2184,.T.);
#9156=EDGE_CURVE('',#7054,#7053,#2185,.T.);
#9157=EDGE_CURVE('',#6708,#6736,#867,.T.);
#9158=EDGE_CURVE('',#7062,#6707,#868,.T.);
#9159=EDGE_CURVE('',#7063,#7062,#869,.T.);
#9160=EDGE_CURVE('',#7064,#7063,#870,.T.);
#9161=EDGE_CURVE('',#7065,#7064,#871,.T.);
#9162=EDGE_CURVE('',#6737,#7065,#872,.T.);
#9163=EDGE_CURVE('',#6709,#6735,#873,.T.);
#9164=EDGE_CURVE('',#7066,#6734,#874,.T.);
#9165=EDGE_CURVE('',#7067,#7066,#875,.T.);
#9166=EDGE_CURVE('',#7068,#7067,#876,.T.);
#9167=EDGE_CURVE('',#7069,#7068,#877,.T.);
#9168=EDGE_CURVE('',#6710,#7069,#878,.T.);
#9169=EDGE_CURVE('',#7065,#7058,#2186,.T.);
#9170=EDGE_CURVE('',#6733,#7070,#879,.T.);
#9171=EDGE_CURVE('',#7070,#7066,#2187,.T.);
#9172=EDGE_CURVE('',#7064,#7059,#2188,.T.);
#9173=EDGE_CURVE('',#7063,#7060,#2189,.T.);
#9174=EDGE_CURVE('',#7062,#7061,#2190,.T.);
#9175=EDGE_CURVE('',#6712,#6732,#880,.T.);
#9176=EDGE_CURVE('',#7071,#6711,#881,.T.);
#9177=EDGE_CURVE('',#7072,#7071,#882,.T.);
#9178=EDGE_CURVE('',#7073,#7072,#883,.T.);
#9179=EDGE_CURVE('',#7070,#7073,#884,.T.);
#9180=EDGE_CURVE('',#6713,#6731,#885,.T.);
#9181=EDGE_CURVE('',#7074,#6730,#886,.T.);
#9182=EDGE_CURVE('',#7075,#7074,#887,.T.);
#9183=EDGE_CURVE('',#7076,#7075,#888,.T.);
#9184=EDGE_CURVE('',#7077,#7076,#889,.T.);
#9185=EDGE_CURVE('',#6714,#7077,#890,.T.);
#9186=EDGE_CURVE('',#6729,#7078,#891,.T.);
#9187=EDGE_CURVE('',#7078,#7074,#2191,.T.);
#9188=EDGE_CURVE('',#7073,#7067,#2192,.T.);
#9189=EDGE_CURVE('',#7078,#7079,#892,.T.);
#9190=EDGE_CURVE('',#7079,#7075,#2193,.T.);
#9191=EDGE_CURVE('',#7071,#7069,#2194,.T.);
#9192=EDGE_CURVE('',#7072,#7068,#2195,.T.);
#9193=EDGE_CURVE('',#6716,#6728,#893,.T.);
#9194=EDGE_CURVE('',#7080,#6715,#894,.T.);
#9195=EDGE_CURVE('',#7081,#7080,#895,.T.);
#9196=EDGE_CURVE('',#7079,#7081,#896,.T.);
#9197=EDGE_CURVE('',#6717,#6727,#897,.T.);
#9198=EDGE_CURVE('',#7081,#7076,#2196,.T.);
#9199=EDGE_CURVE('',#7080,#7077,#2197,.T.);
#9200=EDGE_CURVE('',#7082,#7083,#4949,.T.);
#9201=EDGE_CURVE('',#7082,#7084,#4950,.T.);
#9202=EDGE_CURVE('',#7085,#7084,#4951,.T.);
#9203=EDGE_CURVE('',#7086,#7085,#262,.T.);
#9204=EDGE_CURVE('',#7087,#7086,#4952,.T.);
#9205=EDGE_CURVE('',#7083,#7087,#263,.T.);
#9206=EDGE_CURVE('',#7088,#7082,#4953,.T.);
#9207=EDGE_CURVE('',#7089,#7088,#4954,.T.);
#9208=EDGE_CURVE('',#7084,#7089,#4955,.T.);
#9209=EDGE_CURVE('',#7090,#7088,#4956,.T.);
#9210=EDGE_CURVE('',#7091,#7090,#264,.T.);
#9211=EDGE_CURVE('',#7092,#7091,#4957,.T.);
#9212=EDGE_CURVE('',#7093,#7092,#265,.T.);
#9213=EDGE_CURVE('',#7089,#7093,#4958,.T.);
#9214=EDGE_CURVE('',#7094,#7094,#2198,.T.);
#9215=EDGE_CURVE('',#7083,#7090,#2199,.T.);
#9216=EDGE_CURVE('',#7087,#7091,#2200,.T.);
#9217=EDGE_CURVE('',#7095,#7095,#2201,.T.);
#9218=EDGE_CURVE('',#7095,#7094,#4959,.T.);
#9219=EDGE_CURVE('',#7096,#7096,#2202,.T.);
#9220=EDGE_CURVE('',#7096,#7095,#4960,.T.);
#9221=EDGE_CURVE('',#7097,#7097,#2203,.T.);
#9222=EDGE_CURVE('',#7098,#7098,#2204,.T.);
#9223=EDGE_CURVE('',#7098,#7097,#4961,.T.);
#9224=EDGE_CURVE('',#7099,#7099,#2205,.T.);
#9225=EDGE_CURVE('',#7099,#7098,#4962,.T.);
#9226=EDGE_CURVE('',#7100,#7100,#2206,.T.);
#9227=EDGE_CURVE('',#7101,#7101,#2207,.T.);
#9228=EDGE_CURVE('',#7101,#7100,#4963,.T.);
#9229=EDGE_CURVE('',#7102,#7102,#2208,.T.);
#9230=EDGE_CURVE('',#7103,#7103,#2209,.T.);
#9231=EDGE_CURVE('',#7103,#7102,#4964,.T.);
#9232=EDGE_CURVE('',#7103,#7104,#4965,.T.);
#9233=EDGE_CURVE('',#7104,#7104,#2210,.T.);
#9234=EDGE_CURVE('',#7105,#7105,#2211,.T.);
#9235=EDGE_CURVE('',#7106,#7106,#2212,.T.);
#9236=EDGE_CURVE('',#7106,#7105,#4966,.T.);
#9237=EDGE_CURVE('',#7106,#7107,#4967,.T.);
#9238=EDGE_CURVE('',#7107,#7107,#2213,.T.);
#9239=EDGE_CURVE('',#7085,#7093,#2214,.T.);
#9240=EDGE_CURVE('',#7086,#7092,#2215,.T.);
#9241=EDGE_CURVE('',#7108,#7108,#2216,.T.);
#9242=EDGE_CURVE('',#7109,#7109,#2217,.T.);
#9243=EDGE_CURVE('',#7110,#7110,#2218,.T.);
#9244=EDGE_CURVE('',#7110,#7108,#4968,.T.);
#9245=EDGE_CURVE('',#7111,#7111,#2219,.T.);
#9246=EDGE_CURVE('',#7111,#7110,#4969,.T.);
#9247=EDGE_CURVE('',#7111,#7112,#4970,.T.);
#9248=EDGE_CURVE('',#7112,#7112,#2220,.T.);
#9249=EDGE_CURVE('',#7113,#7113,#2221,.T.);
#9250=EDGE_CURVE('',#7114,#7114,#2222,.T.);
#9251=EDGE_CURVE('',#7114,#7113,#4971,.T.);
#9252=EDGE_CURVE('',#7115,#7115,#2223,.T.);
#9253=EDGE_CURVE('',#7116,#7116,#2224,.T.);
#9254=EDGE_CURVE('',#7116,#7115,#4972,.T.);
#9255=EDGE_CURVE('',#7117,#7117,#2225,.T.);
#9256=EDGE_CURVE('',#7117,#7116,#4973,.T.);
#9257=EDGE_CURVE('',#7117,#7118,#4974,.T.);
#9258=EDGE_CURVE('',#7118,#7118,#2226,.T.);
#9259=EDGE_CURVE('',#7118,#7109,#4975,.T.);
#9260=EDGE_CURVE('',#7119,#7119,#2227,.T.);
#9261=EDGE_CURVE('',#7119,#7120,#4976,.T.);
#9262=EDGE_CURVE('',#7120,#7120,#2228,.T.);
#9263=EDGE_CURVE('',#7121,#7121,#2229,.T.);
#9264=EDGE_CURVE('',#7121,#7122,#4977,.T.);
#9265=EDGE_CURVE('',#7122,#7122,#2230,.T.);
#9266=EDGE_CURVE('',#7123,#7123,#2231,.T.);
#9267=EDGE_CURVE('',#7124,#7124,#2232,.T.);
#9268=EDGE_CURVE('',#7124,#7125,#4978,.T.);
#9269=EDGE_CURVE('',#7125,#7125,#2233,.T.);
#9270=EDGE_CURVE('',#7126,#7126,#2234,.T.);
#9271=EDGE_CURVE('',#7127,#7127,#2235,.T.);
#9272=EDGE_CURVE('',#7127,#7126,#4979,.T.);
#9273=EDGE_CURVE('',#7127,#7123,#4980,.T.);
#9274=EDGE_CURVE('',#7128,#7129,#4981,.T.);
#9275=EDGE_CURVE('',#7130,#7128,#898,.T.);
#9276=EDGE_CURVE('',#7131,#7130,#2236,.T.);
#9277=EDGE_CURVE('',#7131,#7129,#899,.T.);
#9278=EDGE_CURVE('',#7132,#7133,#4982,.T.);
#9279=EDGE_CURVE('',#7134,#7132,#900,.T.);
#9280=EDGE_CURVE('',#7128,#7134,#901,.T.);
#9281=EDGE_CURVE('',#7129,#7135,#902,.T.);
#9282=EDGE_CURVE('',#7135,#7133,#903,.T.);
#9283=EDGE_CURVE('',#7136,#7137,#4983,.T.);
#9284=EDGE_CURVE('',#7138,#7136,#904,.T.);
#9285=EDGE_CURVE('',#7132,#7138,#905,.T.);
#9286=EDGE_CURVE('',#7133,#7139,#906,.T.);
#9287=EDGE_CURVE('',#7139,#7137,#907,.T.);
#9288=EDGE_CURVE('',#7140,#7141,#4984,.T.);
#9289=EDGE_CURVE('',#7142,#7140,#908,.T.);
#9290=EDGE_CURVE('',#7136,#7142,#909,.T.);
#9291=EDGE_CURVE('',#7137,#7143,#910,.T.);
#9292=EDGE_CURVE('',#7143,#7141,#911,.T.);
#9293=EDGE_CURVE('',#7144,#7145,#4985,.T.);
#9294=EDGE_CURVE('',#7146,#7144,#912,.T.);
#9295=EDGE_CURVE('',#7140,#7146,#913,.T.);
#9296=EDGE_CURVE('',#7141,#7147,#914,.T.);
#9297=EDGE_CURVE('',#7147,#7145,#915,.T.);
#9298=EDGE_CURVE('',#7148,#7149,#4986,.T.);
#9299=EDGE_CURVE('',#7150,#7148,#916,.T.);
#9300=EDGE_CURVE('',#7144,#7150,#917,.T.);
#9301=EDGE_CURVE('',#7145,#7151,#918,.T.);
#9302=EDGE_CURVE('',#7151,#7149,#919,.T.);
#9303=EDGE_CURVE('',#7152,#7153,#920,.T.);
#9304=EDGE_CURVE('',#7153,#7154,#2237,.T.);
#9305=EDGE_CURVE('',#7154,#7155,#921,.T.);
#9306=EDGE_CURVE('',#7155,#7156,#922,.T.);
#9307=EDGE_CURVE('',#7156,#7157,#923,.T.);
#9308=EDGE_CURVE('',#7157,#7158,#924,.T.);
#9309=EDGE_CURVE('',#7158,#7159,#925,.T.);
#9310=EDGE_CURVE('',#7159,#7160,#926,.T.);
#9311=EDGE_CURVE('',#7160,#7161,#927,.T.);
#9312=EDGE_CURVE('',#7162,#7161,#2238,.F.);
#9313=EDGE_CURVE('',#7162,#7163,#928,.T.);
#9314=EDGE_CURVE('',#7163,#7164,#929,.T.);
#9315=EDGE_CURVE('',#7164,#7165,#930,.T.);
#9316=EDGE_CURVE('',#7165,#7166,#931,.T.);
#9317=EDGE_CURVE('',#7166,#7167,#932,.T.);
#9318=EDGE_CURVE('',#7167,#7152,#933,.T.);
#9319=EDGE_CURVE('',#7149,#7168,#934,.T.);
#9320=EDGE_CURVE('',#7168,#7169,#935,.T.);
#9321=EDGE_CURVE('',#7170,#7169,#2239,.T.);
#9322=EDGE_CURVE('',#7171,#7170,#936,.T.);
#9323=EDGE_CURVE('',#7148,#7171,#937,.T.);
#9324=EDGE_CURVE('',#7169,#7172,#938,.T.);
#9325=EDGE_CURVE('',#7173,#7172,#2240,.T.);
#9326=EDGE_CURVE('',#7173,#7170,#939,.T.);
#9327=EDGE_CURVE('',#7174,#7173,#940,.T.);
#9328=EDGE_CURVE('',#7161,#7174,#941,.T.);
#9329=EDGE_CURVE('',#7130,#7154,#942,.T.);
#9330=EDGE_CURVE('',#7154,#7175,#2241,.T.);
#9331=EDGE_CURVE('',#7175,#7176,#2242,.T.);
#9332=EDGE_CURVE('',#7176,#7131,#943,.T.);
#9333=EDGE_CURVE('',#7172,#7177,#944,.T.);
#9334=EDGE_CURVE('',#7176,#7153,#945,.T.);
#9335=EDGE_CURVE('',#7177,#7162,#946,.T.);
#9336=EDGE_CURVE('',#7178,#7179,#266,.T.);
#9337=EDGE_CURVE('',#7180,#7178,#267,.T.);
#9338=EDGE_CURVE('',#7181,#7180,#268,.T.);
#9339=EDGE_CURVE('',#7182,#7181,#269,.T.);
#9340=EDGE_CURVE('',#7183,#7182,#270,.T.);
#9341=EDGE_CURVE('',#7184,#7183,#271,.T.);
#9342=EDGE_CURVE('',#7179,#7184,#272,.T.);
#9343=EDGE_CURVE('',#7179,#7185,#4987,.T.);
#9344=EDGE_CURVE('',#7185,#7185,#2243,.T.);
#9345=EDGE_CURVE('',#7183,#7186,#4988,.T.);
#9346=EDGE_CURVE('',#7186,#7187,#4989,.T.);
#9347=EDGE_CURVE('',#7184,#7187,#4990,.T.);
#9348=EDGE_CURVE('',#7182,#7188,#4991,.T.);
#9349=EDGE_CURVE('',#7188,#7186,#4992,.T.);
#9350=EDGE_CURVE('',#7181,#7189,#4993,.T.);
#9351=EDGE_CURVE('',#7189,#7188,#4994,.T.);
#9352=EDGE_CURVE('',#7190,#7191,#4995,.T.);
#9353=EDGE_CURVE('',#7191,#7191,#2244,.T.);
#9354=EDGE_CURVE('',#7180,#7192,#4996,.T.);
#9355=EDGE_CURVE('',#7192,#7189,#4997,.T.);
#9356=EDGE_CURVE('',#7178,#7193,#4998,.T.);
#9357=EDGE_CURVE('',#7193,#7192,#4999,.T.);
#9358=EDGE_CURVE('',#7187,#7193,#5000,.T.);
#9359=EDGE_CURVE('',#7194,#7194,#2245,.T.);
#9360=EDGE_CURVE('',#7175,#7194,#5001,.T.);
#9361=EDGE_CURVE('',#7195,#7174,#2246,.T.);
#9362=EDGE_CURVE('',#7177,#7195,#2247,.T.);
#9363=EDGE_CURVE('',#7196,#7196,#2248,.T.);
#9364=EDGE_CURVE('',#7196,#7195,#5002,.T.);
#9365=EDGE_CURVE('',#7197,#7197,#2249,.T.);
#9366=EDGE_CURVE('',#7198,#7198,#2250,.T.);
#9367=EDGE_CURVE('',#7198,#7197,#5003,.T.);
#9368=EDGE_CURVE('',#7199,#7199,#2251,.T.);
#9369=EDGE_CURVE('',#7199,#7198,#5004,.T.);
#9370=EDGE_CURVE('',#7199,#7200,#5005,.T.);
#9371=EDGE_CURVE('',#7200,#7200,#2252,.T.);
#9372=EDGE_CURVE('',#7201,#7201,#2253,.T.);
#9373=EDGE_CURVE('',#7201,#7202,#5006,.T.);
#9374=EDGE_CURVE('',#7202,#7202,#2254,.T.);
#9375=EDGE_CURVE('',#7203,#7203,#2255,.T.);
#9376=EDGE_CURVE('',#7204,#7204,#2256,.T.);
#9377=EDGE_CURVE('',#7204,#7203,#5007,.T.);
#9378=EDGE_CURVE('',#7205,#7205,#2257,.T.);
#9379=EDGE_CURVE('',#7205,#7204,#5008,.T.);
#9380=EDGE_CURVE('',#7205,#7206,#5009,.T.);
#9381=EDGE_CURVE('',#7206,#7206,#2258,.T.);
#9382=EDGE_CURVE('',#7207,#7207,#2259,.T.);
#9383=EDGE_CURVE('',#7208,#7208,#2260,.T.);
#9384=EDGE_CURVE('',#7208,#7207,#5010,.T.);
#9385=EDGE_CURVE('',#7201,#7208,#5011,.T.);
#9386=EDGE_CURVE('',#7209,#7209,#2261,.T.);
#9387=EDGE_CURVE('',#7209,#7210,#5012,.T.);
#9388=EDGE_CURVE('',#7210,#7210,#2262,.T.);
#9389=EDGE_CURVE('',#7211,#7211,#2263,.T.);
#9390=EDGE_CURVE('',#7212,#7212,#2264,.T.);
#9391=EDGE_CURVE('',#7212,#7211,#5013,.T.);
#9392=EDGE_CURVE('',#7213,#7213,#2265,.T.);
#9393=EDGE_CURVE('',#7213,#7212,#5014,.T.);
#9394=EDGE_CURVE('',#7214,#7214,#2266,.T.);
#9395=EDGE_CURVE('',#7215,#7215,#2267,.T.);
#9396=EDGE_CURVE('',#7215,#7214,#5015,.T.);
#9397=EDGE_CURVE('',#7216,#7216,#2268,.T.);
#9398=EDGE_CURVE('',#7216,#7215,#5016,.T.);
#9399=EDGE_CURVE('',#7216,#7217,#5017,.T.);
#9400=EDGE_CURVE('',#7217,#7217,#2269,.T.);
#9401=EDGE_CURVE('',#7218,#7218,#2270,.T.);
#9402=EDGE_CURVE('',#7218,#7219,#5018,.T.);
#9403=EDGE_CURVE('',#7219,#7219,#2271,.T.);
#9404=EDGE_CURVE('',#7220,#7220,#2272,.T.);
#9405=EDGE_CURVE('',#7220,#7221,#5019,.T.);
#9406=EDGE_CURVE('',#7221,#7221,#2273,.T.);
#9407=EDGE_CURVE('',#7222,#7222,#2274,.T.);
#9408=EDGE_CURVE('',#7222,#7223,#5020,.T.);
#9409=EDGE_CURVE('',#7223,#7223,#2275,.T.);
#9410=EDGE_CURVE('',#7224,#7224,#2276,.T.);
#9411=EDGE_CURVE('',#7224,#7225,#5021,.T.);
#9412=EDGE_CURVE('',#7225,#7225,#2277,.T.);
#9413=EDGE_CURVE('',#7226,#7226,#2278,.T.);
#9414=EDGE_CURVE('',#7227,#7227,#2279,.T.);
#9415=EDGE_CURVE('',#7228,#7228,#2280,.T.);
#9416=EDGE_CURVE('',#7228,#7229,#5022,.T.);
#9417=EDGE_CURVE('',#7229,#7229,#2281,.T.);
#9418=EDGE_CURVE('',#7228,#7230,#5023,.T.);
#9419=EDGE_CURVE('',#7230,#7230,#2282,.T.);
#9420=EDGE_CURVE('',#7231,#7231,#2283,.T.);
#9421=EDGE_CURVE('',#7231,#7232,#5024,.T.);
#9422=EDGE_CURVE('',#7232,#7232,#2284,.T.);
#9423=EDGE_CURVE('',#7232,#7233,#5025,.T.);
#9424=EDGE_CURVE('',#7233,#7233,#2285,.T.);
#9425=EDGE_CURVE('',#7234,#7234,#2286,.T.);
#9426=EDGE_CURVE('',#7234,#7226,#5026,.T.);
#9427=EDGE_CURVE('',#7235,#7235,#2287,.T.);
#9428=EDGE_CURVE('',#7235,#7234,#5027,.T.);
#9429=EDGE_CURVE('',#7235,#7236,#5028,.T.);
#9430=EDGE_CURVE('',#7236,#7236,#2288,.T.);
#9431=EDGE_CURVE('',#7237,#7237,#2289,.T.);
#9432=EDGE_CURVE('',#7227,#7237,#5029,.T.);
#9433=EDGE_CURVE('',#7238,#7238,#2290,.T.);
#9434=EDGE_CURVE('',#7229,#7238,#5030,.T.);
#9435=EDGE_CURVE('',#7239,#7239,#2291,.T.);
#9436=EDGE_CURVE('',#7239,#7240,#5031,.T.);
#9437=EDGE_CURVE('',#7240,#7240,#2292,.T.);
#9438=EDGE_CURVE('',#7239,#7241,#5032,.T.);
#9439=EDGE_CURVE('',#7241,#7241,#2293,.T.);
#9440=EDGE_CURVE('',#7242,#7242,#2294,.T.);
#9441=EDGE_CURVE('',#7243,#7243,#2295,.T.);
#9442=EDGE_CURVE('',#7243,#7242,#5033,.T.);
#9443=EDGE_CURVE('',#7244,#7244,#2296,.T.);
#9444=EDGE_CURVE('',#7245,#7245,#2297,.T.);
#9445=EDGE_CURVE('',#7245,#7244,#5034,.T.);
#9446=EDGE_CURVE('',#7246,#7246,#2298,.T.);
#9447=EDGE_CURVE('',#7247,#7247,#2299,.T.);
#9448=EDGE_CURVE('',#7247,#7246,#5035,.T.);
#9449=EDGE_CURVE('',#7248,#7248,#2300,.T.);
#9450=EDGE_CURVE('',#7248,#7247,#5036,.T.);
#9451=EDGE_CURVE('',#7248,#7249,#5037,.T.);
#9452=EDGE_CURVE('',#7249,#7249,#2301,.T.);
#9453=EDGE_CURVE('',#7250,#7250,#2302,.T.);
#9454=EDGE_CURVE('',#7251,#7251,#2303,.T.);
#9455=EDGE_CURVE('',#7251,#7250,#5038,.T.);
#9456=EDGE_CURVE('',#7252,#7252,#2304,.T.);
#9457=EDGE_CURVE('',#7253,#7253,#2305,.T.);
#9458=EDGE_CURVE('',#7253,#7252,#5039,.T.);
#9459=EDGE_CURVE('',#7254,#7254,#2306,.T.);
#9460=EDGE_CURVE('',#7240,#7254,#5040,.T.);
#9461=EDGE_CURVE('',#7255,#7255,#2307,.T.);
#9462=EDGE_CURVE('',#7256,#7256,#2308,.T.);
#9463=EDGE_CURVE('',#7257,#7257,#2309,.T.);
#9464=EDGE_CURVE('',#7257,#7255,#5041,.T.);
#9465=EDGE_CURVE('',#7258,#7258,#2310,.T.);
#9466=EDGE_CURVE('',#7258,#7257,#5042,.T.);
#9467=EDGE_CURVE('',#7258,#7259,#5043,.T.);
#9468=EDGE_CURVE('',#7259,#7259,#2311,.T.);
#9469=EDGE_CURVE('',#7260,#7260,#2312,.T.);
#9470=EDGE_CURVE('',#7261,#7261,#2313,.T.);
#9471=EDGE_CURVE('',#7261,#7260,#5044,.T.);
#9472=EDGE_CURVE('',#7262,#7262,#2314,.T.);
#9473=EDGE_CURVE('',#7263,#7263,#2315,.T.);
#9474=EDGE_CURVE('',#7263,#7262,#5045,.T.);
#9475=EDGE_CURVE('',#7264,#7264,#2316,.T.);
#9476=EDGE_CURVE('',#7264,#7263,#5046,.T.);
#9477=EDGE_CURVE('',#7264,#7265,#5047,.T.);
#9478=EDGE_CURVE('',#7265,#7265,#2317,.T.);
#9479=EDGE_CURVE('',#7265,#7256,#5048,.T.);
#9480=EDGE_CURVE('',#7266,#7266,#2318,.T.);
#9481=EDGE_CURVE('',#7266,#7267,#5049,.T.);
#9482=EDGE_CURVE('',#7267,#7267,#2319,.T.);
#9483=EDGE_CURVE('',#7266,#7268,#5050,.T.);
#9484=EDGE_CURVE('',#7268,#7268,#2320,.T.);
#9485=EDGE_CURVE('',#7269,#7270,#5051,.T.);
#9486=EDGE_CURVE('',#7271,#7270,#2321,.T.);
#9487=EDGE_CURVE('',#7271,#7272,#5052,.T.);
#9488=EDGE_CURVE('',#7273,#7272,#2322,.T.);
#9489=EDGE_CURVE('',#7274,#7273,#2323,.T.);
#9490=EDGE_CURVE('',#7275,#7274,#2324,.T.);
#9491=EDGE_CURVE('',#7276,#7275,#2325,.T.);
#9492=EDGE_CURVE('',#7269,#7276,#2326,.T.);
#9493=EDGE_CURVE('',#7277,#7277,#2327,.T.);
#9494=EDGE_CURVE('',#7268,#7278,#5053,.T.);
#9495=EDGE_CURVE('',#7278,#7278,#2328,.T.);
#9496=EDGE_CURVE('',#7279,#7280,#5054,.T.);
#9497=EDGE_CURVE('',#7280,#7281,#2329,.T.);
#9498=EDGE_CURVE('',#7281,#7282,#2330,.T.);
#9499=EDGE_CURVE('',#7282,#7283,#2331,.T.);
#9500=EDGE_CURVE('',#7283,#7284,#2332,.T.);
#9501=EDGE_CURVE('',#7284,#7285,#2333,.T.);
#9502=EDGE_CURVE('',#7285,#7286,#5055,.T.);
#9503=EDGE_CURVE('',#7286,#7279,#2334,.T.);
#9504=EDGE_CURVE('',#7287,#7287,#2335,.T.);
#9505=EDGE_CURVE('',#7288,#7288,#2336,.T.);
#9506=EDGE_CURVE('',#7288,#7277,#5056,.T.);
#9507=EDGE_CURVE('',#7288,#7289,#5057,.T.);
#9508=EDGE_CURVE('',#7289,#7289,#2337,.T.);
#9509=EDGE_CURVE('',#7289,#7287,#5058,.T.);
#9510=EDGE_CURVE('',#7272,#7285,#5059,.T.);
#9511=EDGE_CURVE('',#7286,#7271,#5060,.T.);
#9512=EDGE_CURVE('',#7280,#7269,#5061,.T.);
#9513=EDGE_CURVE('',#7270,#7279,#5062,.T.);
#9514=EDGE_CURVE('',#7273,#7284,#5063,.T.);
#9515=EDGE_CURVE('',#7274,#7283,#5064,.T.);
#9516=EDGE_CURVE('',#7275,#7282,#5065,.T.);
#9517=EDGE_CURVE('',#7276,#7281,#5066,.T.);
#9518=EDGE_CURVE('',#7290,#7291,#5067,.T.);
#9519=EDGE_CURVE('',#7292,#7290,#947,.T.);
#9520=EDGE_CURVE('',#7293,#7292,#2338,.T.);
#9521=EDGE_CURVE('',#7293,#7291,#948,.T.);
#9522=EDGE_CURVE('',#7294,#7295,#5068,.T.);
#9523=EDGE_CURVE('',#7296,#7294,#949,.F.);
#9524=EDGE_CURVE('',#7290,#7296,#950,.T.);
#9525=EDGE_CURVE('',#7291,#7297,#951,.T.);
#9526=EDGE_CURVE('',#7297,#7295,#952,.T.);
#9527=EDGE_CURVE('',#7298,#7299,#5069,.T.);
#9528=EDGE_CURVE('',#7294,#7298,#953,.F.);
#9529=EDGE_CURVE('',#7295,#7299,#954,.T.);
#9530=EDGE_CURVE('',#7300,#7301,#5070,.T.);
#9531=EDGE_CURVE('',#7302,#7300,#955,.F.);
#9532=EDGE_CURVE('',#7298,#7302,#956,.F.);
#9533=EDGE_CURVE('',#7299,#7303,#957,.T.);
#9534=EDGE_CURVE('',#7303,#7301,#958,.T.);
#9535=EDGE_CURVE('',#7304,#7305,#5071,.T.);
#9536=EDGE_CURVE('',#7300,#7304,#959,.F.);
#9537=EDGE_CURVE('',#7301,#7305,#960,.T.);
#9538=EDGE_CURVE('',#7306,#7307,#5072,.T.);
#9539=EDGE_CURVE('',#7308,#7306,#961,.F.);
#9540=EDGE_CURVE('',#7304,#7308,#962,.F.);
#9541=EDGE_CURVE('',#7305,#7309,#963,.T.);
#9542=EDGE_CURVE('',#7309,#7307,#964,.T.);
#9543=EDGE_CURVE('',#7310,#7311,#5073,.T.);
#9544=EDGE_CURVE('',#7306,#7310,#965,.F.);
#9545=EDGE_CURVE('',#7307,#7311,#966,.T.);
#9546=EDGE_CURVE('',#7312,#7313,#5074,.T.);
#9547=EDGE_CURVE('',#7314,#7312,#967,.F.);
#9548=EDGE_CURVE('',#7310,#7314,#968,.F.);
#9549=EDGE_CURVE('',#7311,#7315,#969,.T.);
#9550=EDGE_CURVE('',#7315,#7313,#970,.T.);
#9551=EDGE_CURVE('',#7316,#7317,#5075,.T.);
#9552=EDGE_CURVE('',#7312,#7316,#971,.F.);
#9553=EDGE_CURVE('',#7313,#7317,#972,.T.);
#9554=EDGE_CURVE('',#7318,#7319,#5076,.T.);
#9555=EDGE_CURVE('',#7320,#7318,#973,.F.);
#9556=EDGE_CURVE('',#7316,#7320,#974,.F.);
#9557=EDGE_CURVE('',#7317,#7321,#975,.T.);
#9558=EDGE_CURVE('',#7321,#7319,#976,.T.);
#9559=EDGE_CURVE('',#7322,#7323,#5077,.T.);
#9560=EDGE_CURVE('',#7318,#7322,#977,.F.);
#9561=EDGE_CURVE('',#7319,#7323,#978,.T.);
#9562=EDGE_CURVE('',#7324,#7325,#5078,.T.);
#9563=EDGE_CURVE('',#7326,#7324,#979,.T.);
#9564=EDGE_CURVE('',#7322,#7326,#980,.F.);
#9565=EDGE_CURVE('',#7323,#7327,#981,.T.);
#9566=EDGE_CURVE('',#7327,#7325,#982,.T.);
#9567=EDGE_CURVE('',#7328,#7329,#5079,.T.);
#9568=EDGE_CURVE('',#7330,#7328,#983,.T.);
#9569=EDGE_CURVE('',#7324,#7330,#984,.T.);
#9570=EDGE_CURVE('',#7325,#7329,#985,.T.);
#9571=EDGE_CURVE('',#7331,#7332,#5080,.T.);
#9572=EDGE_CURVE('',#7333,#7331,#986,.T.);
#9573=EDGE_CURVE('',#7328,#7333,#987,.T.);
#9574=EDGE_CURVE('',#7329,#7334,#988,.T.);
#9575=EDGE_CURVE('',#7334,#7332,#989,.T.);
#9576=EDGE_CURVE('',#7335,#7336,#5081,.T.);
#9577=EDGE_CURVE('',#7337,#7335,#990,.F.);
#9578=EDGE_CURVE('',#7331,#7337,#991,.T.);
#9579=EDGE_CURVE('',#7332,#7338,#992,.T.);
#9580=EDGE_CURVE('',#7338,#7336,#993,.T.);
#9581=EDGE_CURVE('',#7339,#7340,#5082,.T.);
#9582=EDGE_CURVE('',#7335,#7339,#994,.F.);
#9583=EDGE_CURVE('',#7336,#7340,#995,.T.);
#9584=EDGE_CURVE('',#7341,#7342,#5083,.T.);
#9585=EDGE_CURVE('',#7343,#7341,#996,.T.);
#9586=EDGE_CURVE('',#7339,#7343,#997,.F.);
#9587=EDGE_CURVE('',#7340,#7344,#998,.T.);
#9588=EDGE_CURVE('',#7344,#7342,#999,.T.);
#9589=EDGE_CURVE('',#7345,#7346,#5084,.T.);
#9590=EDGE_CURVE('',#7347,#7345,#1000,.F.);
#9591=EDGE_CURVE('',#7341,#7347,#1001,.T.);
#9592=EDGE_CURVE('',#7342,#7348,#1002,.T.);
#9593=EDGE_CURVE('',#7348,#7346,#1003,.T.);
#9594=EDGE_CURVE('',#7349,#7350,#5085,.T.);
#9595=EDGE_CURVE('',#7345,#7349,#1004,.F.);
#9596=EDGE_CURVE('',#7346,#7351,#1005,.T.);
#9597=EDGE_CURVE('',#7351,#7350,#1006,.F.);
#9598=EDGE_CURVE('',#7352,#7353,#1007,.T.);
#9599=EDGE_CURVE('',#7353,#7354,#2339,.T.);
#9600=EDGE_CURVE('',#7354,#7355,#1008,.T.);
#9601=EDGE_CURVE('',#7355,#7356,#1009,.T.);
#9602=EDGE_CURVE('',#7356,#7357,#1010,.T.);
#9603=EDGE_CURVE('',#7357,#7358,#1011,.T.);
#9604=EDGE_CURVE('',#7358,#7359,#1012,.T.);
#9605=EDGE_CURVE('',#7359,#7360,#1013,.T.);
#9606=EDGE_CURVE('',#7360,#7361,#1014,.T.);
#9607=EDGE_CURVE('',#7361,#7362,#1015,.T.);
#9608=EDGE_CURVE('',#7362,#7363,#1016,.T.);
#9609=EDGE_CURVE('',#7363,#7364,#1017,.T.);
#9610=EDGE_CURVE('',#7364,#7365,#1018,.T.);
#9611=EDGE_CURVE('',#7365,#7366,#1019,.T.);
#9612=EDGE_CURVE('',#7366,#7367,#1020,.T.);
#9613=EDGE_CURVE('',#7367,#7368,#1021,.T.);
#9614=EDGE_CURVE('',#7368,#7369,#1022,.T.);
#9615=EDGE_CURVE('',#7369,#7370,#1023,.T.);
#9616=EDGE_CURVE('',#7370,#7371,#1024,.T.);
#9617=EDGE_CURVE('',#7371,#7372,#1025,.T.);
#9618=EDGE_CURVE('',#7372,#7373,#1026,.T.);
#9619=EDGE_CURVE('',#7373,#7374,#1027,.T.);
#9620=EDGE_CURVE('',#7374,#7375,#2340,.T.);
#9621=EDGE_CURVE('',#7376,#7375,#2341,.T.);
#9622=EDGE_CURVE('',#7377,#7376,#2342,.T.);
#9623=EDGE_CURVE('',#7377,#7378,#1028,.T.);
#9624=EDGE_CURVE('',#7378,#7379,#1029,.T.);
#9625=EDGE_CURVE('',#7379,#7380,#1030,.T.);
#9626=EDGE_CURVE('',#7380,#7381,#1031,.T.);
#9627=EDGE_CURVE('',#7381,#7382,#1032,.T.);
#9628=EDGE_CURVE('',#7382,#7383,#1033,.T.);
#9629=EDGE_CURVE('',#7383,#7384,#1034,.T.);
#9630=EDGE_CURVE('',#7384,#7385,#1035,.T.);
#9631=EDGE_CURVE('',#7385,#7386,#1036,.T.);
#9632=EDGE_CURVE('',#7386,#7387,#1037,.T.);
#9633=EDGE_CURVE('',#7387,#7388,#1038,.T.);
#9634=EDGE_CURVE('',#7388,#7389,#1039,.T.);
#9635=EDGE_CURVE('',#7389,#7390,#1040,.T.);
#9636=EDGE_CURVE('',#7390,#7391,#1041,.T.);
#9637=EDGE_CURVE('',#7391,#7392,#1042,.T.);
#9638=EDGE_CURVE('',#7392,#7393,#1043,.T.);
#9639=EDGE_CURVE('',#7393,#7394,#1044,.T.);
#9640=EDGE_CURVE('',#7394,#7395,#1045,.T.);
#9641=EDGE_CURVE('',#7395,#7352,#1046,.T.);
#9642=EDGE_CURVE('',#7350,#7396,#1047,.F.);
#9643=EDGE_CURVE('',#7397,#7396,#2343,.T.);
#9644=EDGE_CURVE('',#7398,#7397,#1048,.T.);
#9645=EDGE_CURVE('',#7349,#7398,#1049,.F.);
#9646=EDGE_CURVE('',#7399,#7377,#2344,.T.);
#9647=EDGE_CURVE('',#7399,#7397,#1050,.T.);
#9648=EDGE_CURVE('',#7396,#7400,#1051,.T.);
#9649=EDGE_CURVE('',#7400,#7377,#1052,.T.);
#9650=EDGE_CURVE('',#7375,#7399,#1053,.T.);
#9651=EDGE_CURVE('',#7292,#7354,#1054,.T.);
#9652=EDGE_CURVE('',#7354,#7401,#2345,.T.);
#9653=EDGE_CURVE('',#7401,#7402,#2346,.T.);
#9654=EDGE_CURVE('',#7402,#7293,#1055,.T.);
#9655=EDGE_CURVE('',#7402,#7353,#1056,.T.);
#9656=EDGE_CURVE('',#7403,#7403,#2347,.T.);
#9657=EDGE_CURVE('',#7403,#7376,#2348,.T.);
#9658=EDGE_CURVE('',#7404,#7404,#2349,.T.);
#9659=EDGE_CURVE('',#7405,#7406,#273,.T.);
#9660=EDGE_CURVE('',#7407,#7405,#274,.T.);
#9661=EDGE_CURVE('',#7408,#7407,#275,.T.);
#9662=EDGE_CURVE('',#7409,#7408,#276,.T.);
#9663=EDGE_CURVE('',#7410,#7409,#277,.T.);
#9664=EDGE_CURVE('',#7411,#7410,#278,.T.);
#9665=EDGE_CURVE('',#7406,#7411,#279,.T.);
#9666=EDGE_CURVE('',#7406,#7412,#5086,.T.);
#9667=EDGE_CURVE('',#7412,#7412,#2350,.T.);
#9668=EDGE_CURVE('',#7410,#7413,#5087,.T.);
#9669=EDGE_CURVE('',#7413,#7414,#5088,.T.);
#9670=EDGE_CURVE('',#7411,#7414,#5089,.T.);
#9671=EDGE_CURVE('',#7409,#7415,#5090,.T.);
#9672=EDGE_CURVE('',#7415,#7413,#5091,.T.);
#9673=EDGE_CURVE('',#7408,#7416,#5092,.T.);
#9674=EDGE_CURVE('',#7416,#7415,#5093,.T.);
#9675=EDGE_CURVE('',#7417,#7418,#5094,.T.);
#9676=EDGE_CURVE('',#7418,#7418,#2351,.T.);
#9677=EDGE_CURVE('',#7407,#7419,#5095,.T.);
#9678=EDGE_CURVE('',#7419,#7416,#5096,.T.);
#9679=EDGE_CURVE('',#7405,#7420,#5097,.T.);
#9680=EDGE_CURVE('',#7420,#7419,#5098,.T.);
#9681=EDGE_CURVE('',#7414,#7420,#5099,.T.);
#9682=EDGE_CURVE('',#7421,#7421,#2352,.T.);
#9683=EDGE_CURVE('',#7421,#7422,#2353,.T.);
#9684=EDGE_CURVE('',#7422,#7422,#2354,.T.);
#9685=EDGE_CURVE('',#7422,#7423,#5100,.T.);
#9686=EDGE_CURVE('',#7423,#7423,#2355,.T.);
#9687=EDGE_CURVE('',#7424,#7424,#2356,.T.);
#9688=EDGE_CURVE('',#7401,#7424,#5101,.T.);
#9689=EDGE_CURVE('',#7423,#7404,#5102,.T.);
#9690=EDGE_CURVE('',#7425,#7426,#5103,.T.);
#9691=EDGE_CURVE('',#7427,#7425,#1057,.T.);
#9692=EDGE_CURVE('',#7428,#7427,#2357,.T.);
#9693=EDGE_CURVE('',#7428,#7426,#1058,.T.);
#9694=EDGE_CURVE('',#7429,#7430,#5104,.T.);
#9695=EDGE_CURVE('',#7431,#7429,#1059,.F.);
#9696=EDGE_CURVE('',#7425,#7431,#1060,.T.);
#9697=EDGE_CURVE('',#7426,#7432,#1061,.T.);
#9698=EDGE_CURVE('',#7432,#7430,#1062,.T.);
#9699=EDGE_CURVE('',#7433,#7434,#5105,.T.);
#9700=EDGE_CURVE('',#7429,#7433,#1063,.F.);
#9701=EDGE_CURVE('',#7430,#7435,#1064,.T.);
#9702=EDGE_CURVE('',#7435,#7434,#1065,.T.);
#9703=EDGE_CURVE('',#7436,#7437,#5106,.T.);
#9704=EDGE_CURVE('',#7438,#7436,#1066,.F.);
#9705=EDGE_CURVE('',#7433,#7438,#1067,.F.);
#9706=EDGE_CURVE('',#7434,#7437,#1068,.T.);
#9707=EDGE_CURVE('',#7439,#7440,#5107,.T.);
#9708=EDGE_CURVE('',#7436,#7439,#1069,.F.);
#9709=EDGE_CURVE('',#7437,#7441,#1070,.T.);
#9710=EDGE_CURVE('',#7441,#7440,#1071,.T.);
#9711=EDGE_CURVE('',#7442,#7443,#5108,.T.);
#9712=EDGE_CURVE('',#7444,#7442,#1072,.F.);
#9713=EDGE_CURVE('',#7439,#7444,#1073,.F.);
#9714=EDGE_CURVE('',#7440,#7443,#1074,.T.);
#9715=EDGE_CURVE('',#7445,#7446,#5109,.T.);
#9716=EDGE_CURVE('',#7442,#7445,#1075,.F.);
#9717=EDGE_CURVE('',#7443,#7447,#1076,.T.);
#9718=EDGE_CURVE('',#7447,#7446,#1077,.T.);
#9719=EDGE_CURVE('',#7448,#7449,#5110,.T.);
#9720=EDGE_CURVE('',#7450,#7448,#1078,.F.);
#9721=EDGE_CURVE('',#7445,#7450,#1079,.F.);
#9722=EDGE_CURVE('',#7446,#7451,#1080,.T.);
#9723=EDGE_CURVE('',#7451,#7449,#1081,.T.);
#9724=EDGE_CURVE('',#7452,#7453,#5111,.T.);
#9725=EDGE_CURVE('',#7448,#7452,#1082,.F.);
#9726=EDGE_CURVE('',#7449,#7454,#1083,.T.);
#9727=EDGE_CURVE('',#7454,#7453,#1084,.T.);
#9728=EDGE_CURVE('',#7455,#7456,#5112,.T.);
#9729=EDGE_CURVE('',#7457,#7455,#1085,.F.);
#9730=EDGE_CURVE('',#7452,#7457,#1086,.F.);
#9731=EDGE_CURVE('',#7453,#7456,#1087,.T.);
#9732=EDGE_CURVE('',#7458,#7459,#5113,.T.);
#9733=EDGE_CURVE('',#7455,#7458,#1088,.F.);
#9734=EDGE_CURVE('',#7456,#7460,#1089,.T.);
#9735=EDGE_CURVE('',#7460,#7459,#1090,.T.);
#9736=EDGE_CURVE('',#7461,#7462,#5114,.T.);
#9737=EDGE_CURVE('',#7463,#7461,#1091,.F.);
#9738=EDGE_CURVE('',#7458,#7463,#1092,.F.);
#9739=EDGE_CURVE('',#7459,#7462,#1093,.T.);
#9740=EDGE_CURVE('',#7464,#7465,#5115,.T.);
#9741=EDGE_CURVE('',#7461,#7464,#1094,.F.);
#9742=EDGE_CURVE('',#7462,#7466,#1095,.T.);
#9743=EDGE_CURVE('',#7466,#7465,#1096,.T.);
#9744=EDGE_CURVE('',#7467,#7468,#5116,.T.);
#9745=EDGE_CURVE('',#7469,#7467,#1097,.F.);
#9746=EDGE_CURVE('',#7464,#7469,#1098,.F.);
#9747=EDGE_CURVE('',#7465,#7468,#1099,.T.);
#9748=EDGE_CURVE('',#7470,#7471,#5117,.T.);
#9749=EDGE_CURVE('',#7467,#7470,#1100,.F.);
#9750=EDGE_CURVE('',#7468,#7472,#1101,.T.);
#9751=EDGE_CURVE('',#7472,#7471,#1102,.F.);
#9752=EDGE_CURVE('',#7473,#7474,#1103,.T.);
#9753=EDGE_CURVE('',#7474,#7475,#2358,.T.);
#9754=EDGE_CURVE('',#7475,#7476,#1104,.T.);
#9755=EDGE_CURVE('',#7476,#7477,#1105,.T.);
#9756=EDGE_CURVE('',#7477,#7478,#1106,.T.);
#9757=EDGE_CURVE('',#7478,#7479,#1107,.T.);
#9758=EDGE_CURVE('',#7479,#7480,#1108,.T.);
#9759=EDGE_CURVE('',#7480,#7481,#1109,.T.);
#9760=EDGE_CURVE('',#7481,#7482,#1110,.T.);
#9761=EDGE_CURVE('',#7482,#7483,#1111,.T.);
#9762=EDGE_CURVE('',#7483,#7484,#1112,.T.);
#9763=EDGE_CURVE('',#7484,#7485,#1113,.T.);
#9764=EDGE_CURVE('',#7485,#7486,#1114,.T.);
#9765=EDGE_CURVE('',#7486,#7487,#1115,.T.);
#9766=EDGE_CURVE('',#7487,#7488,#1116,.T.);
#9767=EDGE_CURVE('',#7488,#7489,#1117,.T.);
#9768=EDGE_CURVE('',#7489,#7490,#1118,.T.);
#9769=EDGE_CURVE('',#7490,#7491,#1119,.T.);
#9770=EDGE_CURVE('',#7491,#7492,#2359,.T.);
#9771=EDGE_CURVE('',#7493,#7492,#2360,.T.);
#9772=EDGE_CURVE('',#7494,#7493,#2361,.T.);
#9773=EDGE_CURVE('',#7494,#7495,#1120,.T.);
#9774=EDGE_CURVE('',#7495,#7496,#1121,.T.);
#9775=EDGE_CURVE('',#7496,#7497,#1122,.T.);
#9776=EDGE_CURVE('',#7497,#7498,#1123,.T.);
#9777=EDGE_CURVE('',#7498,#7499,#1124,.T.);
#9778=EDGE_CURVE('',#7499,#7500,#1125,.T.);
#9779=EDGE_CURVE('',#7500,#7501,#1126,.T.);
#9780=EDGE_CURVE('',#7501,#7502,#1127,.T.);
#9781=EDGE_CURVE('',#7502,#7503,#1128,.T.);
#9782=EDGE_CURVE('',#7503,#7504,#1129,.T.);
#9783=EDGE_CURVE('',#7504,#7505,#1130,.T.);
#9784=EDGE_CURVE('',#7505,#7506,#1131,.T.);
#9785=EDGE_CURVE('',#7506,#7507,#1132,.T.);
#9786=EDGE_CURVE('',#7507,#7508,#1133,.T.);
#9787=EDGE_CURVE('',#7508,#7473,#1134,.T.);
#9788=EDGE_CURVE('',#7471,#7509,#1135,.F.);
#9789=EDGE_CURVE('',#7510,#7509,#2362,.T.);
#9790=EDGE_CURVE('',#7511,#7510,#1136,.T.);
#9791=EDGE_CURVE('',#7470,#7511,#1137,.F.);
#9792=EDGE_CURVE('',#7512,#7494,#2363,.T.);
#9793=EDGE_CURVE('',#7512,#7510,#1138,.T.);
#9794=EDGE_CURVE('',#7509,#7513,#1139,.T.);
#9795=EDGE_CURVE('',#7513,#7494,#1140,.T.);
#9796=EDGE_CURVE('',#7492,#7512,#1141,.T.);
#9797=EDGE_CURVE('',#7427,#7475,#1142,.T.);
#9798=EDGE_CURVE('',#7475,#7514,#2364,.T.);
#9799=EDGE_CURVE('',#7514,#7515,#2365,.T.);
#9800=EDGE_CURVE('',#7515,#7428,#1143,.T.);
#9801=EDGE_CURVE('',#7515,#7474,#1144,.T.);
#9802=EDGE_CURVE('',#7516,#7516,#2366,.T.);
#9803=EDGE_CURVE('',#7516,#7493,#2367,.T.);
#9804=EDGE_CURVE('',#7517,#7517,#2368,.T.);
#9805=EDGE_CURVE('',#7518,#7519,#280,.T.);
#9806=EDGE_CURVE('',#7520,#7518,#281,.T.);
#9807=EDGE_CURVE('',#7521,#7520,#282,.T.);
#9808=EDGE_CURVE('',#7522,#7521,#283,.T.);
#9809=EDGE_CURVE('',#7523,#7522,#284,.T.);
#9810=EDGE_CURVE('',#7524,#7523,#285,.T.);
#9811=EDGE_CURVE('',#7519,#7524,#286,.T.);
#9812=EDGE_CURVE('',#7519,#7525,#5118,.T.);
#9813=EDGE_CURVE('',#7525,#7525,#2369,.T.);
#9814=EDGE_CURVE('',#7523,#7526,#5119,.T.);
#9815=EDGE_CURVE('',#7526,#7527,#5120,.T.);
#9816=EDGE_CURVE('',#7524,#7527,#5121,.T.);
#9817=EDGE_CURVE('',#7522,#7528,#5122,.T.);
#9818=EDGE_CURVE('',#7528,#7526,#5123,.T.);
#9819=EDGE_CURVE('',#7521,#7529,#5124,.T.);
#9820=EDGE_CURVE('',#7529,#7528,#5125,.T.);
#9821=EDGE_CURVE('',#7530,#7531,#5126,.T.);
#9822=EDGE_CURVE('',#7531,#7531,#2370,.T.);
#9823=EDGE_CURVE('',#7520,#7532,#5127,.T.);
#9824=EDGE_CURVE('',#7532,#7529,#5128,.T.);
#9825=EDGE_CURVE('',#7518,#7533,#5129,.T.);
#9826=EDGE_CURVE('',#7533,#7532,#5130,.T.);
#9827=EDGE_CURVE('',#7527,#7533,#5131,.T.);
#9828=EDGE_CURVE('',#7534,#7534,#2371,.T.);
#9829=EDGE_CURVE('',#7534,#7535,#2372,.T.);
#9830=EDGE_CURVE('',#7535,#7535,#2373,.T.);
#9831=EDGE_CURVE('',#7535,#7536,#5132,.T.);
#9832=EDGE_CURVE('',#7536,#7536,#2374,.T.);
#9833=EDGE_CURVE('',#7537,#7537,#2375,.T.);
#9834=EDGE_CURVE('',#7514,#7537,#5133,.T.);
#9835=EDGE_CURVE('',#7536,#7517,#5134,.T.);
#9836=EDGE_CURVE('',#7538,#7538,#2376,.T.);
#9837=EDGE_CURVE('',#7538,#7539,#5135,.T.);
#9838=EDGE_CURVE('',#7539,#7539,#2377,.T.);
#9839=EDGE_CURVE('',#7540,#7540,#2378,.T.);
#9840=EDGE_CURVE('',#7541,#7541,#2379,.T.);
#9841=EDGE_CURVE('',#7541,#7540,#5136,.T.);
#9842=EDGE_CURVE('',#7542,#7542,#2380,.T.);
#9843=EDGE_CURVE('',#7542,#7541,#5137,.T.);
#9844=EDGE_CURVE('',#7543,#7543,#2381,.T.);
#9845=EDGE_CURVE('',#7544,#7544,#2382,.T.);
#9846=EDGE_CURVE('',#7544,#7543,#5138,.T.);
#9847=EDGE_CURVE('',#7545,#7545,#2383,.T.);
#9848=EDGE_CURVE('',#7545,#7544,#5139,.T.);
#9849=EDGE_CURVE('',#7545,#7546,#5140,.T.);
#9850=EDGE_CURVE('',#7546,#7546,#2384,.T.);
#9851=ORIENTED_EDGE('',*,*,#7547,.F.);
#9852=ORIENTED_EDGE('',*,*,#7548,.T.);
#9853=ORIENTED_EDGE('',*,*,#7549,.T.);
#9854=ORIENTED_EDGE('',*,*,#7550,.F.);
#9855=ORIENTED_EDGE('',*,*,#7551,.F.);
#9856=ORIENTED_EDGE('',*,*,#7552,.T.);
#9857=ORIENTED_EDGE('',*,*,#7553,.T.);
#9858=ORIENTED_EDGE('',*,*,#7548,.F.);
#9859=ORIENTED_EDGE('',*,*,#7554,.F.);
#9860=ORIENTED_EDGE('',*,*,#7555,.T.);
#9861=ORIENTED_EDGE('',*,*,#7556,.T.);
#9862=ORIENTED_EDGE('',*,*,#7552,.F.);
#9863=ORIENTED_EDGE('',*,*,#7557,.F.);
#9864=ORIENTED_EDGE('',*,*,#7550,.T.);
#9865=ORIENTED_EDGE('',*,*,#7558,.T.);
#9866=ORIENTED_EDGE('',*,*,#7555,.F.);
#9867=ORIENTED_EDGE('',*,*,#7558,.F.);
#9868=ORIENTED_EDGE('',*,*,#7549,.F.);
#9869=ORIENTED_EDGE('',*,*,#7553,.F.);
#9870=ORIENTED_EDGE('',*,*,#7556,.F.);
#9871=ORIENTED_EDGE('',*,*,#7559,.F.);
#9872=ORIENTED_EDGE('',*,*,#7560,.F.);
#9873=ORIENTED_EDGE('',*,*,#7561,.T.);
#9874=ORIENTED_EDGE('',*,*,#7562,.T.);
#9875=ORIENTED_EDGE('',*,*,#7563,.F.);
#9876=ORIENTED_EDGE('',*,*,#7562,.F.);
#9877=ORIENTED_EDGE('',*,*,#7564,.F.);
#9878=ORIENTED_EDGE('',*,*,#7565,.F.);
#9879=ORIENTED_EDGE('',*,*,#7566,.F.);
#9880=ORIENTED_EDGE('',*,*,#7567,.F.);
#9881=ORIENTED_EDGE('',*,*,#7568,.F.);
#9882=ORIENTED_EDGE('',*,*,#7569,.T.);
#9883=ORIENTED_EDGE('',*,*,#7564,.T.);
#9884=ORIENTED_EDGE('',*,*,#7561,.F.);
#9885=ORIENTED_EDGE('',*,*,#7570,.F.);
#9886=ORIENTED_EDGE('',*,*,#7571,.T.);
#9887=ORIENTED_EDGE('',*,*,#7565,.T.);
#9888=ORIENTED_EDGE('',*,*,#7569,.F.);
#9889=ORIENTED_EDGE('',*,*,#7572,.F.);
#9890=ORIENTED_EDGE('',*,*,#7566,.T.);
#9891=ORIENTED_EDGE('',*,*,#7571,.F.);
#9892=ORIENTED_EDGE('',*,*,#7573,.F.);
#9893=ORIENTED_EDGE('',*,*,#7574,.F.);
#9894=ORIENTED_EDGE('',*,*,#7575,.T.);
#9895=ORIENTED_EDGE('',*,*,#7576,.T.);
#9896=ORIENTED_EDGE('',*,*,#7577,.F.);
#9897=ORIENTED_EDGE('',*,*,#7578,.F.);
#9898=ORIENTED_EDGE('',*,*,#7579,.T.);
#9899=ORIENTED_EDGE('',*,*,#7580,.T.);
#9900=ORIENTED_EDGE('',*,*,#7575,.F.);
#9901=ORIENTED_EDGE('',*,*,#7581,.F.);
#9902=ORIENTED_EDGE('',*,*,#7582,.T.);
#9903=ORIENTED_EDGE('',*,*,#7583,.T.);
#9904=ORIENTED_EDGE('',*,*,#7579,.F.);
#9905=ORIENTED_EDGE('',*,*,#7584,.F.);
#9906=ORIENTED_EDGE('',*,*,#7577,.T.);
#9907=ORIENTED_EDGE('',*,*,#7585,.T.);
#9908=ORIENTED_EDGE('',*,*,#7582,.F.);
#9909=ORIENTED_EDGE('',*,*,#7585,.F.);
#9910=ORIENTED_EDGE('',*,*,#7576,.F.);
#9911=ORIENTED_EDGE('',*,*,#7580,.F.);
#9912=ORIENTED_EDGE('',*,*,#7583,.F.);
#9913=ORIENTED_EDGE('',*,*,#7586,.F.);
#9914=ORIENTED_EDGE('',*,*,#7587,.T.);
#9915=ORIENTED_EDGE('',*,*,#7588,.T.);
#9916=ORIENTED_EDGE('',*,*,#7589,.F.);
#9917=ORIENTED_EDGE('',*,*,#7590,.F.);
#9918=ORIENTED_EDGE('',*,*,#7591,.T.);
#9919=ORIENTED_EDGE('',*,*,#7592,.T.);
#9920=ORIENTED_EDGE('',*,*,#7587,.F.);
#9921=ORIENTED_EDGE('',*,*,#7593,.F.);
#9922=ORIENTED_EDGE('',*,*,#7594,.T.);
#9923=ORIENTED_EDGE('',*,*,#7595,.T.);
#9924=ORIENTED_EDGE('',*,*,#7591,.F.);
#9925=ORIENTED_EDGE('',*,*,#7596,.F.);
#9926=ORIENTED_EDGE('',*,*,#7589,.T.);
#9927=ORIENTED_EDGE('',*,*,#7597,.T.);
#9928=ORIENTED_EDGE('',*,*,#7594,.F.);
#9929=ORIENTED_EDGE('',*,*,#7597,.F.);
#9930=ORIENTED_EDGE('',*,*,#7588,.F.);
#9931=ORIENTED_EDGE('',*,*,#7592,.F.);
#9932=ORIENTED_EDGE('',*,*,#7595,.F.);
#9933=ORIENTED_EDGE('',*,*,#7598,.F.);
#9934=ORIENTED_EDGE('',*,*,#7599,.T.);
#9935=ORIENTED_EDGE('',*,*,#7600,.T.);
#9936=ORIENTED_EDGE('',*,*,#7601,.F.);
#9937=ORIENTED_EDGE('',*,*,#7602,.F.);
#9938=ORIENTED_EDGE('',*,*,#7603,.T.);
#9939=ORIENTED_EDGE('',*,*,#7604,.T.);
#9940=ORIENTED_EDGE('',*,*,#7599,.F.);
#9941=ORIENTED_EDGE('',*,*,#7605,.F.);
#9942=ORIENTED_EDGE('',*,*,#7606,.T.);
#9943=ORIENTED_EDGE('',*,*,#7607,.T.);
#9944=ORIENTED_EDGE('',*,*,#7603,.F.);
#9945=ORIENTED_EDGE('',*,*,#7608,.F.);
#9946=ORIENTED_EDGE('',*,*,#7601,.T.);
#9947=ORIENTED_EDGE('',*,*,#7609,.T.);
#9948=ORIENTED_EDGE('',*,*,#7606,.F.);
#9949=ORIENTED_EDGE('',*,*,#7609,.F.);
#9950=ORIENTED_EDGE('',*,*,#7600,.F.);
#9951=ORIENTED_EDGE('',*,*,#7604,.F.);
#9952=ORIENTED_EDGE('',*,*,#7607,.F.);
#9953=ORIENTED_EDGE('',*,*,#7610,.F.);
#9954=ORIENTED_EDGE('',*,*,#7611,.T.);
#9955=ORIENTED_EDGE('',*,*,#7612,.F.);
#9956=ORIENTED_EDGE('',*,*,#7613,.F.);
#9957=ORIENTED_EDGE('',*,*,#7614,.F.);
#9958=ORIENTED_EDGE('',*,*,#7615,.F.);
#9959=ORIENTED_EDGE('',*,*,#7616,.T.);
#9960=ORIENTED_EDGE('',*,*,#7617,.T.);
#9961=ORIENTED_EDGE('',*,*,#7618,.F.);
#9962=ORIENTED_EDGE('',*,*,#7619,.T.);
#9963=ORIENTED_EDGE('',*,*,#7620,.T.);
#9964=ORIENTED_EDGE('',*,*,#7616,.F.);
#9965=ORIENTED_EDGE('',*,*,#7621,.F.);
#9966=ORIENTED_EDGE('',*,*,#7612,.T.);
#9967=ORIENTED_EDGE('',*,*,#7622,.T.);
#9968=ORIENTED_EDGE('',*,*,#7619,.F.);
#9969=ORIENTED_EDGE('',*,*,#7623,.F.);
#9970=ORIENTED_EDGE('',*,*,#7624,.F.);
#9971=ORIENTED_EDGE('',*,*,#7617,.F.);
#9972=ORIENTED_EDGE('',*,*,#7620,.F.);
#9973=ORIENTED_EDGE('',*,*,#7622,.F.);
#9974=ORIENTED_EDGE('',*,*,#7611,.F.);
#9975=ORIENTED_EDGE('',*,*,#7559,.T.);
#9976=ORIENTED_EDGE('',*,*,#7563,.T.);
#9977=ORIENTED_EDGE('',*,*,#7625,.T.);
#9978=ORIENTED_EDGE('',*,*,#7626,.T.);
#9979=ORIENTED_EDGE('',*,*,#7627,.T.);
#9980=ORIENTED_EDGE('',*,*,#7628,.F.);
#9981=ORIENTED_EDGE('',*,*,#7567,.T.);
#9982=ORIENTED_EDGE('',*,*,#7572,.T.);
#9983=ORIENTED_EDGE('',*,*,#7629,.F.);
#9984=ORIENTED_EDGE('',*,*,#7630,.F.);
#9985=ORIENTED_EDGE('',*,*,#7631,.F.);
#9986=ORIENTED_EDGE('',*,*,#7625,.F.);
#9987=ORIENTED_EDGE('',*,*,#7560,.T.);
#9988=ORIENTED_EDGE('',*,*,#7628,.T.);
#9989=ORIENTED_EDGE('',*,*,#7632,.T.);
#9990=ORIENTED_EDGE('',*,*,#7633,.F.);
#9991=ORIENTED_EDGE('',*,*,#7634,.F.);
#9992=ORIENTED_EDGE('',*,*,#7635,.F.);
#9993=ORIENTED_EDGE('',*,*,#7636,.T.);
#9994=ORIENTED_EDGE('',*,*,#7637,.T.);
#9995=ORIENTED_EDGE('',*,*,#7613,.T.);
#9996=ORIENTED_EDGE('',*,*,#7621,.T.);
#9997=ORIENTED_EDGE('',*,*,#7618,.T.);
#9998=ORIENTED_EDGE('',*,*,#7615,.T.);
#9999=ORIENTED_EDGE('',*,*,#7638,.T.);
#10000=ORIENTED_EDGE('',*,*,#7639,.F.);
#10001=ORIENTED_EDGE('',*,*,#7640,.F.);
#10002=ORIENTED_EDGE('',*,*,#7641,.F.);
#10003=ORIENTED_EDGE('',*,*,#7629,.T.);
#10004=ORIENTED_EDGE('',*,*,#7573,.T.);
#10005=ORIENTED_EDGE('',*,*,#7570,.T.);
#10006=ORIENTED_EDGE('',*,*,#7568,.T.);
#10007=ORIENTED_EDGE('',*,*,#7642,.T.);
#10008=ORIENTED_EDGE('',*,*,#7598,.T.);
#10009=ORIENTED_EDGE('',*,*,#7608,.T.);
#10010=ORIENTED_EDGE('',*,*,#7605,.T.);
#10011=ORIENTED_EDGE('',*,*,#7602,.T.);
#10012=ORIENTED_EDGE('',*,*,#7586,.T.);
#10013=ORIENTED_EDGE('',*,*,#7596,.T.);
#10014=ORIENTED_EDGE('',*,*,#7593,.T.);
#10015=ORIENTED_EDGE('',*,*,#7590,.T.);
#10016=ORIENTED_EDGE('',*,*,#7574,.T.);
#10017=ORIENTED_EDGE('',*,*,#7584,.T.);
#10018=ORIENTED_EDGE('',*,*,#7581,.T.);
#10019=ORIENTED_EDGE('',*,*,#7578,.T.);
#10020=ORIENTED_EDGE('',*,*,#7547,.T.);
#10021=ORIENTED_EDGE('',*,*,#7557,.T.);
#10022=ORIENTED_EDGE('',*,*,#7554,.T.);
#10023=ORIENTED_EDGE('',*,*,#7551,.T.);
#10024=ORIENTED_EDGE('',*,*,#7643,.F.);
#10025=ORIENTED_EDGE('',*,*,#7644,.T.);
#10026=ORIENTED_EDGE('',*,*,#7645,.T.);
#10027=ORIENTED_EDGE('',*,*,#7646,.F.);
#10028=ORIENTED_EDGE('',*,*,#7647,.F.);
#10029=ORIENTED_EDGE('',*,*,#7648,.T.);
#10030=ORIENTED_EDGE('',*,*,#7649,.T.);
#10031=ORIENTED_EDGE('',*,*,#7644,.F.);
#10032=ORIENTED_EDGE('',*,*,#7650,.F.);
#10033=ORIENTED_EDGE('',*,*,#7651,.T.);
#10034=ORIENTED_EDGE('',*,*,#7652,.T.);
#10035=ORIENTED_EDGE('',*,*,#7648,.F.);
#10036=ORIENTED_EDGE('',*,*,#7653,.F.);
#10037=ORIENTED_EDGE('',*,*,#7646,.T.);
#10038=ORIENTED_EDGE('',*,*,#7654,.T.);
#10039=ORIENTED_EDGE('',*,*,#7651,.F.);
#10040=ORIENTED_EDGE('',*,*,#7654,.F.);
#10041=ORIENTED_EDGE('',*,*,#7645,.F.);
#10042=ORIENTED_EDGE('',*,*,#7649,.F.);
#10043=ORIENTED_EDGE('',*,*,#7652,.F.);
#10044=ORIENTED_EDGE('',*,*,#7655,.F.);
#10045=ORIENTED_EDGE('',*,*,#7656,.T.);
#10046=ORIENTED_EDGE('',*,*,#7657,.F.);
#10047=ORIENTED_EDGE('',*,*,#7658,.F.);
#10048=ORIENTED_EDGE('',*,*,#7659,.F.);
#10049=ORIENTED_EDGE('',*,*,#7660,.T.);
#10050=ORIENTED_EDGE('',*,*,#7661,.T.);
#10051=ORIENTED_EDGE('',*,*,#7662,.F.);
#10052=ORIENTED_EDGE('',*,*,#7663,.F.);
#10053=ORIENTED_EDGE('',*,*,#7657,.T.);
#10054=ORIENTED_EDGE('',*,*,#7664,.T.);
#10055=ORIENTED_EDGE('',*,*,#7660,.F.);
#10056=ORIENTED_EDGE('',*,*,#7665,.F.);
#10057=ORIENTED_EDGE('',*,*,#7666,.F.);
#10058=ORIENTED_EDGE('',*,*,#7662,.T.);
#10059=ORIENTED_EDGE('',*,*,#7667,.T.);
#10060=ORIENTED_EDGE('',*,*,#7668,.F.);
#10061=ORIENTED_EDGE('',*,*,#7669,.F.);
#10062=ORIENTED_EDGE('',*,*,#7667,.F.);
#10063=ORIENTED_EDGE('',*,*,#7661,.F.);
#10064=ORIENTED_EDGE('',*,*,#7664,.F.);
#10065=ORIENTED_EDGE('',*,*,#7656,.F.);
#10066=ORIENTED_EDGE('',*,*,#7670,.F.);
#10067=ORIENTED_EDGE('',*,*,#7671,.T.);
#10068=ORIENTED_EDGE('',*,*,#7672,.T.);
#10069=ORIENTED_EDGE('',*,*,#7673,.F.);
#10070=ORIENTED_EDGE('',*,*,#7674,.F.);
#10071=ORIENTED_EDGE('',*,*,#7675,.T.);
#10072=ORIENTED_EDGE('',*,*,#7676,.T.);
#10073=ORIENTED_EDGE('',*,*,#7671,.F.);
#10074=ORIENTED_EDGE('',*,*,#7677,.F.);
#10075=ORIENTED_EDGE('',*,*,#7678,.T.);
#10076=ORIENTED_EDGE('',*,*,#7679,.T.);
#10077=ORIENTED_EDGE('',*,*,#7675,.F.);
#10078=ORIENTED_EDGE('',*,*,#7680,.F.);
#10079=ORIENTED_EDGE('',*,*,#7673,.T.);
#10080=ORIENTED_EDGE('',*,*,#7681,.T.);
#10081=ORIENTED_EDGE('',*,*,#7678,.F.);
#10082=ORIENTED_EDGE('',*,*,#7681,.F.);
#10083=ORIENTED_EDGE('',*,*,#7672,.F.);
#10084=ORIENTED_EDGE('',*,*,#7676,.F.);
#10085=ORIENTED_EDGE('',*,*,#7679,.F.);
#10086=ORIENTED_EDGE('',*,*,#7682,.F.);
#10087=ORIENTED_EDGE('',*,*,#7683,.T.);
#10088=ORIENTED_EDGE('',*,*,#7684,.T.);
#10089=ORIENTED_EDGE('',*,*,#7685,.F.);
#10090=ORIENTED_EDGE('',*,*,#7686,.F.);
#10091=ORIENTED_EDGE('',*,*,#7687,.T.);
#10092=ORIENTED_EDGE('',*,*,#7688,.T.);
#10093=ORIENTED_EDGE('',*,*,#7683,.F.);
#10094=ORIENTED_EDGE('',*,*,#7689,.F.);
#10095=ORIENTED_EDGE('',*,*,#7690,.T.);
#10096=ORIENTED_EDGE('',*,*,#7691,.T.);
#10097=ORIENTED_EDGE('',*,*,#7687,.F.);
#10098=ORIENTED_EDGE('',*,*,#7692,.F.);
#10099=ORIENTED_EDGE('',*,*,#7685,.T.);
#10100=ORIENTED_EDGE('',*,*,#7693,.T.);
#10101=ORIENTED_EDGE('',*,*,#7690,.F.);
#10102=ORIENTED_EDGE('',*,*,#7693,.F.);
#10103=ORIENTED_EDGE('',*,*,#7684,.F.);
#10104=ORIENTED_EDGE('',*,*,#7688,.F.);
#10105=ORIENTED_EDGE('',*,*,#7691,.F.);
#10106=ORIENTED_EDGE('',*,*,#7694,.F.);
#10107=ORIENTED_EDGE('',*,*,#7695,.T.);
#10108=ORIENTED_EDGE('',*,*,#7696,.T.);
#10109=ORIENTED_EDGE('',*,*,#7697,.F.);
#10110=ORIENTED_EDGE('',*,*,#7698,.F.);
#10111=ORIENTED_EDGE('',*,*,#7699,.T.);
#10112=ORIENTED_EDGE('',*,*,#7700,.T.);
#10113=ORIENTED_EDGE('',*,*,#7695,.F.);
#10114=ORIENTED_EDGE('',*,*,#7701,.F.);
#10115=ORIENTED_EDGE('',*,*,#7702,.T.);
#10116=ORIENTED_EDGE('',*,*,#7703,.T.);
#10117=ORIENTED_EDGE('',*,*,#7699,.F.);
#10118=ORIENTED_EDGE('',*,*,#7704,.F.);
#10119=ORIENTED_EDGE('',*,*,#7697,.T.);
#10120=ORIENTED_EDGE('',*,*,#7705,.T.);
#10121=ORIENTED_EDGE('',*,*,#7702,.F.);
#10122=ORIENTED_EDGE('',*,*,#7705,.F.);
#10123=ORIENTED_EDGE('',*,*,#7696,.F.);
#10124=ORIENTED_EDGE('',*,*,#7700,.F.);
#10125=ORIENTED_EDGE('',*,*,#7703,.F.);
#10126=ORIENTED_EDGE('',*,*,#7706,.F.);
#10127=ORIENTED_EDGE('',*,*,#7707,.T.);
#10128=ORIENTED_EDGE('',*,*,#7708,.F.);
#10129=ORIENTED_EDGE('',*,*,#7709,.F.);
#10130=ORIENTED_EDGE('',*,*,#7710,.F.);
#10131=ORIENTED_EDGE('',*,*,#7708,.T.);
#10132=ORIENTED_EDGE('',*,*,#7711,.T.);
#10133=ORIENTED_EDGE('',*,*,#7712,.F.);
#10134=ORIENTED_EDGE('',*,*,#7713,.F.);
#10135=ORIENTED_EDGE('',*,*,#7714,.F.);
#10136=ORIENTED_EDGE('',*,*,#7715,.T.);
#10137=ORIENTED_EDGE('',*,*,#7716,.T.);
#10138=ORIENTED_EDGE('',*,*,#7717,.F.);
#10139=ORIENTED_EDGE('',*,*,#7712,.T.);
#10140=ORIENTED_EDGE('',*,*,#7718,.T.);
#10141=ORIENTED_EDGE('',*,*,#7715,.F.);
#10142=ORIENTED_EDGE('',*,*,#7719,.F.);
#10143=ORIENTED_EDGE('',*,*,#7720,.F.);
#10144=ORIENTED_EDGE('',*,*,#7716,.F.);
#10145=ORIENTED_EDGE('',*,*,#7718,.F.);
#10146=ORIENTED_EDGE('',*,*,#7711,.F.);
#10147=ORIENTED_EDGE('',*,*,#7707,.F.);
#10148=ORIENTED_EDGE('',*,*,#7668,.T.);
#10149=ORIENTED_EDGE('',*,*,#7655,.T.);
#10150=ORIENTED_EDGE('',*,*,#7721,.F.);
#10151=ORIENTED_EDGE('',*,*,#7722,.T.);
#10152=ORIENTED_EDGE('',*,*,#7723,.T.);
#10153=ORIENTED_EDGE('',*,*,#7724,.T.);
#10154=ORIENTED_EDGE('',*,*,#7719,.T.);
#10155=ORIENTED_EDGE('',*,*,#7706,.T.);
#10156=ORIENTED_EDGE('',*,*,#7725,.F.);
#10157=ORIENTED_EDGE('',*,*,#7726,.F.);
#10158=ORIENTED_EDGE('',*,*,#7727,.F.);
#10159=ORIENTED_EDGE('',*,*,#7728,.T.);
#10160=ORIENTED_EDGE('',*,*,#7658,.T.);
#10161=ORIENTED_EDGE('',*,*,#7663,.T.);
#10162=ORIENTED_EDGE('',*,*,#7659,.T.);
#10163=ORIENTED_EDGE('',*,*,#7666,.T.);
#10164=ORIENTED_EDGE('',*,*,#7729,.T.);
#10165=ORIENTED_EDGE('',*,*,#7730,.F.);
#10166=ORIENTED_EDGE('',*,*,#7731,.F.);
#10167=ORIENTED_EDGE('',*,*,#7732,.T.);
#10168=ORIENTED_EDGE('',*,*,#7733,.T.);
#10169=ORIENTED_EDGE('',*,*,#7734,.F.);
#10170=ORIENTED_EDGE('',*,*,#7735,.T.);
#10171=ORIENTED_EDGE('',*,*,#7736,.T.);
#10172=ORIENTED_EDGE('',*,*,#7737,.F.);
#10173=ORIENTED_EDGE('',*,*,#7738,.F.);
#10174=ORIENTED_EDGE('',*,*,#7725,.T.);
#10175=ORIENTED_EDGE('',*,*,#7709,.T.);
#10176=ORIENTED_EDGE('',*,*,#7710,.T.);
#10177=ORIENTED_EDGE('',*,*,#7717,.T.);
#10178=ORIENTED_EDGE('',*,*,#7714,.T.);
#10179=ORIENTED_EDGE('',*,*,#7739,.T.);
#10180=ORIENTED_EDGE('',*,*,#7740,.T.);
#10181=ORIENTED_EDGE('',*,*,#7741,.F.);
#10182=ORIENTED_EDGE('',*,*,#7742,.F.);
#10183=ORIENTED_EDGE('',*,*,#7743,.F.);
#10184=ORIENTED_EDGE('',*,*,#7744,.T.);
#10185=ORIENTED_EDGE('',*,*,#7721,.T.);
#10186=ORIENTED_EDGE('',*,*,#7745,.T.);
#10187=ORIENTED_EDGE('',*,*,#7746,.T.);
#10188=ORIENTED_EDGE('',*,*,#7747,.T.);
#10189=ORIENTED_EDGE('',*,*,#7694,.T.);
#10190=ORIENTED_EDGE('',*,*,#7704,.T.);
#10191=ORIENTED_EDGE('',*,*,#7701,.T.);
#10192=ORIENTED_EDGE('',*,*,#7698,.T.);
#10193=ORIENTED_EDGE('',*,*,#7682,.T.);
#10194=ORIENTED_EDGE('',*,*,#7692,.T.);
#10195=ORIENTED_EDGE('',*,*,#7689,.T.);
#10196=ORIENTED_EDGE('',*,*,#7686,.T.);
#10197=ORIENTED_EDGE('',*,*,#7670,.T.);
#10198=ORIENTED_EDGE('',*,*,#7680,.T.);
#10199=ORIENTED_EDGE('',*,*,#7677,.T.);
#10200=ORIENTED_EDGE('',*,*,#7674,.T.);
#10201=ORIENTED_EDGE('',*,*,#7643,.T.);
#10202=ORIENTED_EDGE('',*,*,#7653,.T.);
#10203=ORIENTED_EDGE('',*,*,#7650,.T.);
#10204=ORIENTED_EDGE('',*,*,#7647,.T.);
#10205=ORIENTED_EDGE('',*,*,#7748,.F.);
#10206=ORIENTED_EDGE('',*,*,#7749,.T.);
#10207=ORIENTED_EDGE('',*,*,#7750,.T.);
#10208=ORIENTED_EDGE('',*,*,#7751,.F.);
#10209=ORIENTED_EDGE('',*,*,#7752,.F.);
#10210=ORIENTED_EDGE('',*,*,#7753,.T.);
#10211=ORIENTED_EDGE('',*,*,#7754,.T.);
#10212=ORIENTED_EDGE('',*,*,#7749,.F.);
#10213=ORIENTED_EDGE('',*,*,#7755,.F.);
#10214=ORIENTED_EDGE('',*,*,#7756,.T.);
#10215=ORIENTED_EDGE('',*,*,#7757,.T.);
#10216=ORIENTED_EDGE('',*,*,#7753,.F.);
#10217=ORIENTED_EDGE('',*,*,#7758,.F.);
#10218=ORIENTED_EDGE('',*,*,#7759,.T.);
#10219=ORIENTED_EDGE('',*,*,#7760,.T.);
#10220=ORIENTED_EDGE('',*,*,#7756,.F.);
#10221=ORIENTED_EDGE('',*,*,#7761,.F.);
#10222=ORIENTED_EDGE('',*,*,#7762,.T.);
#10223=ORIENTED_EDGE('',*,*,#7763,.T.);
#10224=ORIENTED_EDGE('',*,*,#7759,.F.);
#10225=ORIENTED_EDGE('',*,*,#7764,.F.);
#10226=ORIENTED_EDGE('',*,*,#7751,.T.);
#10227=ORIENTED_EDGE('',*,*,#7765,.T.);
#10228=ORIENTED_EDGE('',*,*,#7762,.F.);
#10229=ORIENTED_EDGE('',*,*,#7765,.F.);
#10230=ORIENTED_EDGE('',*,*,#7750,.F.);
#10231=ORIENTED_EDGE('',*,*,#7754,.F.);
#10232=ORIENTED_EDGE('',*,*,#7757,.F.);
#10233=ORIENTED_EDGE('',*,*,#7760,.F.);
#10234=ORIENTED_EDGE('',*,*,#7763,.F.);
#10235=ORIENTED_EDGE('',*,*,#7766,.F.);
#10236=ORIENTED_EDGE('',*,*,#7767,.T.);
#10237=ORIENTED_EDGE('',*,*,#7768,.T.);
#10238=ORIENTED_EDGE('',*,*,#7769,.F.);
#10239=ORIENTED_EDGE('',*,*,#7770,.F.);
#10240=ORIENTED_EDGE('',*,*,#7771,.T.);
#10241=ORIENTED_EDGE('',*,*,#7772,.T.);
#10242=ORIENTED_EDGE('',*,*,#7767,.F.);
#10243=ORIENTED_EDGE('',*,*,#7773,.F.);
#10244=ORIENTED_EDGE('',*,*,#7774,.T.);
#10245=ORIENTED_EDGE('',*,*,#7775,.T.);
#10246=ORIENTED_EDGE('',*,*,#7771,.F.);
#10247=ORIENTED_EDGE('',*,*,#7776,.F.);
#10248=ORIENTED_EDGE('',*,*,#7768,.F.);
#10249=ORIENTED_EDGE('',*,*,#7772,.F.);
#10250=ORIENTED_EDGE('',*,*,#7775,.F.);
#10251=ORIENTED_EDGE('',*,*,#7777,.F.);
#10252=ORIENTED_EDGE('',*,*,#7778,.F.);
#10253=ORIENTED_EDGE('',*,*,#7773,.T.);
#10254=ORIENTED_EDGE('',*,*,#7770,.T.);
#10255=ORIENTED_EDGE('',*,*,#7766,.T.);
#10256=ORIENTED_EDGE('',*,*,#7779,.T.);
#10257=ORIENTED_EDGE('',*,*,#7780,.T.);
#10258=ORIENTED_EDGE('',*,*,#7781,.T.);
#10259=ORIENTED_EDGE('',*,*,#7782,.T.);
#10260=ORIENTED_EDGE('',*,*,#7726,.T.);
#10261=ORIENTED_EDGE('',*,*,#7738,.T.);
#10262=ORIENTED_EDGE('',*,*,#7783,.F.);
#10263=ORIENTED_EDGE('',*,*,#7784,.T.);
#10264=ORIENTED_EDGE('',*,*,#7785,.F.);
#10265=ORIENTED_EDGE('',*,*,#7639,.T.);
#10266=ORIENTED_EDGE('',*,*,#7786,.T.);
#10267=ORIENTED_EDGE('',*,*,#7787,.T.);
#10268=ORIENTED_EDGE('',*,*,#7788,.T.);
#10269=ORIENTED_EDGE('',*,*,#7789,.T.);
#10270=ORIENTED_EDGE('',*,*,#7790,.T.);
#10271=ORIENTED_EDGE('',*,*,#7791,.T.);
#10272=ORIENTED_EDGE('',*,*,#7792,.T.);
#10273=ORIENTED_EDGE('',*,*,#7793,.T.);
#10274=ORIENTED_EDGE('',*,*,#7794,.F.);
#10275=ORIENTED_EDGE('',*,*,#7795,.T.);
#10276=ORIENTED_EDGE('',*,*,#7796,.T.);
#10277=ORIENTED_EDGE('',*,*,#7797,.T.);
#10278=ORIENTED_EDGE('',*,*,#7792,.F.);
#10279=ORIENTED_EDGE('',*,*,#7798,.T.);
#10280=ORIENTED_EDGE('',*,*,#7799,.T.);
#10281=ORIENTED_EDGE('',*,*,#7800,.T.);
#10282=ORIENTED_EDGE('',*,*,#7796,.F.);
#10283=ORIENTED_EDGE('',*,*,#7801,.T.);
#10284=ORIENTED_EDGE('',*,*,#7802,.T.);
#10285=ORIENTED_EDGE('',*,*,#7803,.T.);
#10286=ORIENTED_EDGE('',*,*,#7799,.F.);
#10287=ORIENTED_EDGE('',*,*,#7804,.T.);
#10288=ORIENTED_EDGE('',*,*,#7805,.T.);
#10289=ORIENTED_EDGE('',*,*,#7806,.T.);
#10290=ORIENTED_EDGE('',*,*,#7802,.F.);
#10291=ORIENTED_EDGE('',*,*,#7807,.T.);
#10292=ORIENTED_EDGE('',*,*,#7808,.T.);
#10293=ORIENTED_EDGE('',*,*,#7809,.T.);
#10294=ORIENTED_EDGE('',*,*,#7805,.F.);
#10295=ORIENTED_EDGE('',*,*,#7810,.T.);
#10296=ORIENTED_EDGE('',*,*,#7811,.T.);
#10297=ORIENTED_EDGE('',*,*,#7812,.T.);
#10298=ORIENTED_EDGE('',*,*,#7808,.F.);
#10299=ORIENTED_EDGE('',*,*,#7813,.T.);
#10300=ORIENTED_EDGE('',*,*,#7811,.F.);
#10301=ORIENTED_EDGE('',*,*,#7814,.T.);
#10302=ORIENTED_EDGE('',*,*,#7815,.T.);
#10303=ORIENTED_EDGE('',*,*,#7816,.T.);
#10304=ORIENTED_EDGE('',*,*,#7815,.F.);
#10305=ORIENTED_EDGE('',*,*,#7817,.T.);
#10306=ORIENTED_EDGE('',*,*,#7818,.T.);
#10307=ORIENTED_EDGE('',*,*,#7819,.T.);
#10308=ORIENTED_EDGE('',*,*,#7818,.F.);
#10309=ORIENTED_EDGE('',*,*,#7820,.T.);
#10310=ORIENTED_EDGE('',*,*,#7821,.T.);
#10311=ORIENTED_EDGE('',*,*,#7822,.T.);
#10312=ORIENTED_EDGE('',*,*,#7821,.F.);
#10313=ORIENTED_EDGE('',*,*,#7823,.T.);
#10314=ORIENTED_EDGE('',*,*,#7824,.T.);
#10315=ORIENTED_EDGE('',*,*,#7825,.T.);
#10316=ORIENTED_EDGE('',*,*,#7824,.F.);
#10317=ORIENTED_EDGE('',*,*,#7826,.T.);
#10318=ORIENTED_EDGE('',*,*,#7794,.T.);
#10319=ORIENTED_EDGE('',*,*,#7813,.F.);
#10320=ORIENTED_EDGE('',*,*,#7827,.F.);
#10321=ORIENTED_EDGE('',*,*,#7788,.F.);
#10322=ORIENTED_EDGE('',*,*,#7828,.T.);
#10323=ORIENTED_EDGE('',*,*,#7816,.F.);
#10324=ORIENTED_EDGE('',*,*,#7829,.F.);
#10325=ORIENTED_EDGE('',*,*,#7789,.F.);
#10326=ORIENTED_EDGE('',*,*,#7827,.T.);
#10327=ORIENTED_EDGE('',*,*,#7819,.F.);
#10328=ORIENTED_EDGE('',*,*,#7830,.T.);
#10329=ORIENTED_EDGE('',*,*,#7777,.T.);
#10330=ORIENTED_EDGE('',*,*,#7774,.F.);
#10331=ORIENTED_EDGE('',*,*,#7790,.F.);
#10332=ORIENTED_EDGE('',*,*,#7829,.T.);
#10333=ORIENTED_EDGE('',*,*,#7822,.F.);
#10334=ORIENTED_EDGE('',*,*,#7831,.T.);
#10335=ORIENTED_EDGE('',*,*,#7778,.T.);
#10336=ORIENTED_EDGE('',*,*,#7830,.F.);
#10337=ORIENTED_EDGE('',*,*,#7825,.F.);
#10338=ORIENTED_EDGE('',*,*,#7832,.F.);
#10339=ORIENTED_EDGE('',*,*,#7779,.F.);
#10340=ORIENTED_EDGE('',*,*,#7769,.T.);
#10341=ORIENTED_EDGE('',*,*,#7776,.T.);
#10342=ORIENTED_EDGE('',*,*,#7831,.F.);
#10343=ORIENTED_EDGE('',*,*,#7793,.F.);
#10344=ORIENTED_EDGE('',*,*,#7833,.F.);
#10345=ORIENTED_EDGE('',*,*,#7780,.F.);
#10346=ORIENTED_EDGE('',*,*,#7832,.T.);
#10347=ORIENTED_EDGE('',*,*,#7791,.F.);
#10348=ORIENTED_EDGE('',*,*,#7826,.F.);
#10349=ORIENTED_EDGE('',*,*,#7823,.F.);
#10350=ORIENTED_EDGE('',*,*,#7820,.F.);
#10351=ORIENTED_EDGE('',*,*,#7817,.F.);
#10352=ORIENTED_EDGE('',*,*,#7814,.F.);
#10353=ORIENTED_EDGE('',*,*,#7810,.F.);
#10354=ORIENTED_EDGE('',*,*,#7807,.F.);
#10355=ORIENTED_EDGE('',*,*,#7804,.F.);
#10356=ORIENTED_EDGE('',*,*,#7801,.F.);
#10357=ORIENTED_EDGE('',*,*,#7798,.F.);
#10358=ORIENTED_EDGE('',*,*,#7795,.F.);
#10359=ORIENTED_EDGE('',*,*,#7834,.T.);
#10360=ORIENTED_EDGE('',*,*,#7835,.T.);
#10361=ORIENTED_EDGE('',*,*,#7836,.T.);
#10362=ORIENTED_EDGE('',*,*,#7837,.T.);
#10363=ORIENTED_EDGE('',*,*,#7838,.T.);
#10364=ORIENTED_EDGE('',*,*,#7839,.F.);
#10365=ORIENTED_EDGE('',*,*,#7840,.F.);
#10366=ORIENTED_EDGE('',*,*,#7841,.T.);
#10367=ORIENTED_EDGE('',*,*,#7842,.T.);
#10368=ORIENTED_EDGE('',*,*,#7841,.F.);
#10369=ORIENTED_EDGE('',*,*,#7842,.F.);
#10370=ORIENTED_EDGE('',*,*,#7843,.T.);
#10371=ORIENTED_EDGE('',*,*,#7844,.F.);
#10372=ORIENTED_EDGE('',*,*,#7843,.F.);
#10373=ORIENTED_EDGE('',*,*,#7845,.T.);
#10374=ORIENTED_EDGE('',*,*,#7846,.T.);
#10375=ORIENTED_EDGE('',*,*,#7845,.F.);
#10376=ORIENTED_EDGE('',*,*,#7846,.F.);
#10377=ORIENTED_EDGE('',*,*,#7847,.T.);
#10378=ORIENTED_EDGE('',*,*,#7848,.F.);
#10379=ORIENTED_EDGE('',*,*,#7849,.F.);
#10380=ORIENTED_EDGE('',*,*,#7850,.T.);
#10381=ORIENTED_EDGE('',*,*,#7851,.T.);
#10382=ORIENTED_EDGE('',*,*,#7850,.F.);
#10383=ORIENTED_EDGE('',*,*,#7852,.F.);
#10384=ORIENTED_EDGE('',*,*,#7847,.F.);
#10385=ORIENTED_EDGE('',*,*,#7851,.F.);
#10386=ORIENTED_EDGE('',*,*,#7853,.T.);
#10387=ORIENTED_EDGE('',*,*,#7854,.F.);
#10388=ORIENTED_EDGE('',*,*,#7855,.F.);
#10389=ORIENTED_EDGE('',*,*,#7856,.F.);
#10390=ORIENTED_EDGE('',*,*,#7853,.F.);
#10391=ORIENTED_EDGE('',*,*,#7854,.T.);
#10392=ORIENTED_EDGE('',*,*,#7856,.T.);
#10393=ORIENTED_EDGE('',*,*,#7857,.F.);
#10394=ORIENTED_EDGE('',*,*,#7858,.F.);
#10395=ORIENTED_EDGE('',*,*,#7859,.F.);
#10396=ORIENTED_EDGE('',*,*,#7860,.T.);
#10397=ORIENTED_EDGE('',*,*,#7861,.T.);
#10398=ORIENTED_EDGE('',*,*,#7862,.F.);
#10399=ORIENTED_EDGE('',*,*,#7863,.T.);
#10400=ORIENTED_EDGE('',*,*,#7864,.T.);
#10401=ORIENTED_EDGE('',*,*,#7865,.F.);
#10402=ORIENTED_EDGE('',*,*,#7784,.F.);
#10403=ORIENTED_EDGE('',*,*,#7866,.F.);
#10404=ORIENTED_EDGE('',*,*,#7867,.T.);
#10405=ORIENTED_EDGE('',*,*,#7868,.T.);
#10406=ORIENTED_EDGE('',*,*,#7869,.F.);
#10407=ORIENTED_EDGE('',*,*,#7844,.T.);
#10408=ORIENTED_EDGE('',*,*,#7870,.T.);
#10409=ORIENTED_EDGE('',*,*,#7871,.T.);
#10410=ORIENTED_EDGE('',*,*,#7872,.T.);
#10411=ORIENTED_EDGE('',*,*,#7873,.T.);
#10412=ORIENTED_EDGE('',*,*,#7874,.T.);
#10413=ORIENTED_EDGE('',*,*,#7875,.T.);
#10414=ORIENTED_EDGE('',*,*,#7876,.T.);
#10415=ORIENTED_EDGE('',*,*,#7877,.T.);
#10416=ORIENTED_EDGE('',*,*,#7878,.T.);
#10417=ORIENTED_EDGE('',*,*,#7879,.T.);
#10418=ORIENTED_EDGE('',*,*,#7880,.T.);
#10419=ORIENTED_EDGE('',*,*,#7881,.T.);
#10420=ORIENTED_EDGE('',*,*,#7882,.T.);
#10421=ORIENTED_EDGE('',*,*,#7883,.T.);
#10422=ORIENTED_EDGE('',*,*,#7884,.T.);
#10423=ORIENTED_EDGE('',*,*,#7885,.T.);
#10424=ORIENTED_EDGE('',*,*,#7886,.T.);
#10425=ORIENTED_EDGE('',*,*,#7887,.T.);
#10426=ORIENTED_EDGE('',*,*,#7888,.T.);
#10427=ORIENTED_EDGE('',*,*,#7889,.T.);
#10428=ORIENTED_EDGE('',*,*,#7890,.T.);
#10429=ORIENTED_EDGE('',*,*,#7891,.T.);
#10430=ORIENTED_EDGE('',*,*,#7892,.T.);
#10431=ORIENTED_EDGE('',*,*,#7893,.T.);
#10432=ORIENTED_EDGE('',*,*,#7894,.T.);
#10433=ORIENTED_EDGE('',*,*,#7895,.T.);
#10434=ORIENTED_EDGE('',*,*,#7894,.F.);
#10435=ORIENTED_EDGE('',*,*,#7895,.F.);
#10436=ORIENTED_EDGE('',*,*,#7896,.T.);
#10437=ORIENTED_EDGE('',*,*,#7897,.T.);
#10438=ORIENTED_EDGE('',*,*,#7896,.F.);
#10439=ORIENTED_EDGE('',*,*,#7898,.F.);
#10440=ORIENTED_EDGE('',*,*,#7899,.F.);
#10441=ORIENTED_EDGE('',*,*,#7897,.F.);
#10442=ORIENTED_EDGE('',*,*,#7900,.T.);
#10443=ORIENTED_EDGE('',*,*,#7867,.F.);
#10444=ORIENTED_EDGE('',*,*,#7901,.F.);
#10445=ORIENTED_EDGE('',*,*,#7868,.F.);
#10446=ORIENTED_EDGE('',*,*,#7900,.F.);
#10447=ORIENTED_EDGE('',*,*,#7855,.T.);
#10448=ORIENTED_EDGE('',*,*,#7869,.T.);
#10449=ORIENTED_EDGE('',*,*,#7901,.T.);
#10450=ORIENTED_EDGE('',*,*,#7866,.T.);
#10451=ORIENTED_EDGE('',*,*,#7783,.T.);
#10452=ORIENTED_EDGE('',*,*,#7737,.T.);
#10453=ORIENTED_EDGE('',*,*,#7902,.T.);
#10454=ORIENTED_EDGE('',*,*,#7734,.T.);
#10455=ORIENTED_EDGE('',*,*,#7903,.T.);
#10456=ORIENTED_EDGE('',*,*,#7731,.T.);
#10457=ORIENTED_EDGE('',*,*,#7904,.T.);
#10458=ORIENTED_EDGE('',*,*,#7857,.T.);
#10459=ORIENTED_EDGE('',*,*,#7905,.T.);
#10460=ORIENTED_EDGE('',*,*,#7906,.T.);
#10461=ORIENTED_EDGE('',*,*,#7905,.F.);
#10462=ORIENTED_EDGE('',*,*,#7906,.F.);
#10463=ORIENTED_EDGE('',*,*,#7907,.T.);
#10464=ORIENTED_EDGE('',*,*,#7908,.T.);
#10465=ORIENTED_EDGE('',*,*,#7907,.F.);
#10466=ORIENTED_EDGE('',*,*,#7908,.F.);
#10467=ORIENTED_EDGE('',*,*,#7909,.T.);
#10468=ORIENTED_EDGE('',*,*,#7860,.F.);
#10469=ORIENTED_EDGE('',*,*,#7910,.F.);
#10470=ORIENTED_EDGE('',*,*,#7861,.F.);
#10471=ORIENTED_EDGE('',*,*,#7909,.F.);
#10472=ORIENTED_EDGE('',*,*,#7910,.T.);
#10473=ORIENTED_EDGE('',*,*,#7859,.T.);
#10474=ORIENTED_EDGE('',*,*,#7911,.T.);
#10475=ORIENTED_EDGE('',*,*,#7640,.T.);
#10476=ORIENTED_EDGE('',*,*,#7785,.T.);
#10477=ORIENTED_EDGE('',*,*,#7865,.T.);
#10478=ORIENTED_EDGE('',*,*,#7912,.T.);
#10479=ORIENTED_EDGE('',*,*,#7862,.T.);
#10480=ORIENTED_EDGE('',*,*,#7913,.T.);
#10481=ORIENTED_EDGE('',*,*,#7914,.T.);
#10482=ORIENTED_EDGE('',*,*,#7913,.F.);
#10483=ORIENTED_EDGE('',*,*,#7914,.F.);
#10484=ORIENTED_EDGE('',*,*,#7915,.T.);
#10485=ORIENTED_EDGE('',*,*,#7916,.T.);
#10486=ORIENTED_EDGE('',*,*,#7915,.F.);
#10487=ORIENTED_EDGE('',*,*,#7916,.F.);
#10488=ORIENTED_EDGE('',*,*,#7917,.T.);
#10489=ORIENTED_EDGE('',*,*,#7863,.F.);
#10490=ORIENTED_EDGE('',*,*,#7912,.F.);
#10491=ORIENTED_EDGE('',*,*,#7864,.F.);
#10492=ORIENTED_EDGE('',*,*,#7917,.F.);
#10493=ORIENTED_EDGE('',*,*,#7918,.T.);
#10494=ORIENTED_EDGE('',*,*,#7919,.T.);
#10495=ORIENTED_EDGE('',*,*,#7918,.F.);
#10496=ORIENTED_EDGE('',*,*,#7919,.F.);
#10497=ORIENTED_EDGE('',*,*,#7920,.T.);
#10498=ORIENTED_EDGE('',*,*,#7921,.T.);
#10499=ORIENTED_EDGE('',*,*,#7920,.F.);
#10500=ORIENTED_EDGE('',*,*,#7921,.F.);
#10501=ORIENTED_EDGE('',*,*,#7922,.T.);
#10502=ORIENTED_EDGE('',*,*,#7838,.F.);
#10503=ORIENTED_EDGE('',*,*,#7922,.F.);
#10504=ORIENTED_EDGE('',*,*,#7923,.T.);
#10505=ORIENTED_EDGE('',*,*,#7924,.T.);
#10506=ORIENTED_EDGE('',*,*,#7923,.F.);
#10507=ORIENTED_EDGE('',*,*,#7924,.F.);
#10508=ORIENTED_EDGE('',*,*,#7925,.T.);
#10509=ORIENTED_EDGE('',*,*,#7926,.T.);
#10510=ORIENTED_EDGE('',*,*,#7925,.F.);
#10511=ORIENTED_EDGE('',*,*,#7926,.F.);
#10512=ORIENTED_EDGE('',*,*,#7927,.T.);
#10513=ORIENTED_EDGE('',*,*,#7928,.F.);
#10514=ORIENTED_EDGE('',*,*,#7927,.F.);
#10515=ORIENTED_EDGE('',*,*,#7929,.T.);
#10516=ORIENTED_EDGE('',*,*,#7930,.T.);
#10517=ORIENTED_EDGE('',*,*,#7929,.F.);
#10518=ORIENTED_EDGE('',*,*,#7930,.F.);
#10519=ORIENTED_EDGE('',*,*,#7931,.T.);
#10520=ORIENTED_EDGE('',*,*,#7932,.T.);
#10521=ORIENTED_EDGE('',*,*,#7931,.F.);
#10522=ORIENTED_EDGE('',*,*,#7932,.F.);
#10523=ORIENTED_EDGE('',*,*,#7933,.T.);
#10524=ORIENTED_EDGE('',*,*,#7837,.F.);
#10525=ORIENTED_EDGE('',*,*,#7933,.F.);
#10526=ORIENTED_EDGE('',*,*,#7934,.T.);
#10527=ORIENTED_EDGE('',*,*,#7935,.T.);
#10528=ORIENTED_EDGE('',*,*,#7934,.F.);
#10529=ORIENTED_EDGE('',*,*,#7935,.F.);
#10530=ORIENTED_EDGE('',*,*,#7936,.T.);
#10531=ORIENTED_EDGE('',*,*,#7937,.T.);
#10532=ORIENTED_EDGE('',*,*,#7936,.F.);
#10533=ORIENTED_EDGE('',*,*,#7937,.F.);
#10534=ORIENTED_EDGE('',*,*,#7938,.T.);
#10535=ORIENTED_EDGE('',*,*,#7939,.F.);
#10536=ORIENTED_EDGE('',*,*,#7938,.F.);
#10537=ORIENTED_EDGE('',*,*,#7940,.T.);
#10538=ORIENTED_EDGE('',*,*,#7941,.T.);
#10539=ORIENTED_EDGE('',*,*,#7940,.F.);
#10540=ORIENTED_EDGE('',*,*,#7941,.F.);
#10541=ORIENTED_EDGE('',*,*,#7942,.T.);
#10542=ORIENTED_EDGE('',*,*,#7943,.T.);
#10543=ORIENTED_EDGE('',*,*,#7942,.F.);
#10544=ORIENTED_EDGE('',*,*,#7943,.F.);
#10545=ORIENTED_EDGE('',*,*,#7944,.T.);
#10546=ORIENTED_EDGE('',*,*,#7836,.F.);
#10547=ORIENTED_EDGE('',*,*,#7944,.F.);
#10548=ORIENTED_EDGE('',*,*,#7945,.T.);
#10549=ORIENTED_EDGE('',*,*,#7946,.T.);
#10550=ORIENTED_EDGE('',*,*,#7945,.F.);
#10551=ORIENTED_EDGE('',*,*,#7946,.F.);
#10552=ORIENTED_EDGE('',*,*,#7947,.T.);
#10553=ORIENTED_EDGE('',*,*,#7948,.T.);
#10554=ORIENTED_EDGE('',*,*,#7947,.F.);
#10555=ORIENTED_EDGE('',*,*,#7948,.F.);
#10556=ORIENTED_EDGE('',*,*,#7949,.T.);
#10557=ORIENTED_EDGE('',*,*,#7950,.F.);
#10558=ORIENTED_EDGE('',*,*,#7949,.F.);
#10559=ORIENTED_EDGE('',*,*,#7951,.T.);
#10560=ORIENTED_EDGE('',*,*,#7952,.T.);
#10561=ORIENTED_EDGE('',*,*,#7951,.F.);
#10562=ORIENTED_EDGE('',*,*,#7952,.F.);
#10563=ORIENTED_EDGE('',*,*,#7953,.T.);
#10564=ORIENTED_EDGE('',*,*,#7954,.T.);
#10565=ORIENTED_EDGE('',*,*,#7953,.F.);
#10566=ORIENTED_EDGE('',*,*,#7954,.F.);
#10567=ORIENTED_EDGE('',*,*,#7955,.T.);
#10568=ORIENTED_EDGE('',*,*,#7835,.F.);
#10569=ORIENTED_EDGE('',*,*,#7955,.F.);
#10570=ORIENTED_EDGE('',*,*,#7956,.T.);
#10571=ORIENTED_EDGE('',*,*,#7957,.T.);
#10572=ORIENTED_EDGE('',*,*,#7956,.F.);
#10573=ORIENTED_EDGE('',*,*,#7957,.F.);
#10574=ORIENTED_EDGE('',*,*,#7958,.T.);
#10575=ORIENTED_EDGE('',*,*,#7959,.T.);
#10576=ORIENTED_EDGE('',*,*,#7958,.F.);
#10577=ORIENTED_EDGE('',*,*,#7959,.F.);
#10578=ORIENTED_EDGE('',*,*,#7960,.T.);
#10579=ORIENTED_EDGE('',*,*,#7961,.F.);
#10580=ORIENTED_EDGE('',*,*,#7960,.F.);
#10581=ORIENTED_EDGE('',*,*,#7962,.T.);
#10582=ORIENTED_EDGE('',*,*,#7963,.T.);
#10583=ORIENTED_EDGE('',*,*,#7962,.F.);
#10584=ORIENTED_EDGE('',*,*,#7963,.F.);
#10585=ORIENTED_EDGE('',*,*,#7964,.T.);
#10586=ORIENTED_EDGE('',*,*,#7965,.T.);
#10587=ORIENTED_EDGE('',*,*,#7964,.F.);
#10588=ORIENTED_EDGE('',*,*,#7965,.F.);
#10589=ORIENTED_EDGE('',*,*,#7966,.T.);
#10590=ORIENTED_EDGE('',*,*,#7747,.F.);
#10591=ORIENTED_EDGE('',*,*,#7966,.F.);
#10592=ORIENTED_EDGE('',*,*,#7967,.T.);
#10593=ORIENTED_EDGE('',*,*,#7968,.T.);
#10594=ORIENTED_EDGE('',*,*,#7967,.F.);
#10595=ORIENTED_EDGE('',*,*,#7968,.F.);
#10596=ORIENTED_EDGE('',*,*,#7969,.T.);
#10597=ORIENTED_EDGE('',*,*,#7970,.T.);
#10598=ORIENTED_EDGE('',*,*,#7969,.F.);
#10599=ORIENTED_EDGE('',*,*,#7970,.F.);
#10600=ORIENTED_EDGE('',*,*,#7971,.T.);
#10601=ORIENTED_EDGE('',*,*,#7746,.F.);
#10602=ORIENTED_EDGE('',*,*,#7971,.F.);
#10603=ORIENTED_EDGE('',*,*,#7972,.T.);
#10604=ORIENTED_EDGE('',*,*,#7973,.T.);
#10605=ORIENTED_EDGE('',*,*,#7972,.F.);
#10606=ORIENTED_EDGE('',*,*,#7973,.F.);
#10607=ORIENTED_EDGE('',*,*,#7974,.T.);
#10608=ORIENTED_EDGE('',*,*,#7975,.T.);
#10609=ORIENTED_EDGE('',*,*,#7974,.F.);
#10610=ORIENTED_EDGE('',*,*,#7848,.T.);
#10611=ORIENTED_EDGE('',*,*,#7852,.T.);
#10612=ORIENTED_EDGE('',*,*,#7849,.T.);
#10613=ORIENTED_EDGE('',*,*,#7975,.F.);
#10614=ORIENTED_EDGE('',*,*,#7976,.T.);
#10615=ORIENTED_EDGE('',*,*,#7732,.F.);
#10616=ORIENTED_EDGE('',*,*,#7903,.F.);
#10617=ORIENTED_EDGE('',*,*,#7733,.F.);
#10618=ORIENTED_EDGE('',*,*,#7976,.F.);
#10619=ORIENTED_EDGE('',*,*,#7977,.T.);
#10620=ORIENTED_EDGE('',*,*,#7978,.T.);
#10621=ORIENTED_EDGE('',*,*,#7977,.F.);
#10622=ORIENTED_EDGE('',*,*,#7978,.F.);
#10623=ORIENTED_EDGE('',*,*,#7979,.T.);
#10624=ORIENTED_EDGE('',*,*,#7898,.T.);
#10625=ORIENTED_EDGE('',*,*,#7980,.T.);
#10626=ORIENTED_EDGE('',*,*,#7981,.T.);
#10627=ORIENTED_EDGE('',*,*,#7980,.F.);
#10628=ORIENTED_EDGE('',*,*,#7899,.T.);
#10629=ORIENTED_EDGE('',*,*,#7979,.F.);
#10630=ORIENTED_EDGE('',*,*,#7981,.F.);
#10631=ORIENTED_EDGE('',*,*,#7982,.T.);
#10632=ORIENTED_EDGE('',*,*,#7735,.F.);
#10633=ORIENTED_EDGE('',*,*,#7902,.F.);
#10634=ORIENTED_EDGE('',*,*,#7736,.F.);
#10635=ORIENTED_EDGE('',*,*,#7982,.F.);
#10636=ORIENTED_EDGE('',*,*,#7983,.F.);
#10637=ORIENTED_EDGE('',*,*,#7984,.T.);
#10638=ORIENTED_EDGE('',*,*,#7985,.T.);
#10639=ORIENTED_EDGE('',*,*,#7984,.F.);
#10640=ORIENTED_EDGE('',*,*,#7985,.F.);
#10641=ORIENTED_EDGE('',*,*,#7986,.T.);
#10642=ORIENTED_EDGE('',*,*,#7987,.F.);
#10643=ORIENTED_EDGE('',*,*,#7986,.F.);
#10644=ORIENTED_EDGE('',*,*,#7988,.F.);
#10645=ORIENTED_EDGE('',*,*,#7989,.T.);
#10646=ORIENTED_EDGE('',*,*,#7990,.T.);
#10647=ORIENTED_EDGE('',*,*,#7989,.F.);
#10648=ORIENTED_EDGE('',*,*,#7990,.F.);
#10649=ORIENTED_EDGE('',*,*,#7991,.T.);
#10650=ORIENTED_EDGE('',*,*,#7992,.F.);
#10651=ORIENTED_EDGE('',*,*,#7991,.F.);
#10652=ORIENTED_EDGE('',*,*,#7993,.F.);
#10653=ORIENTED_EDGE('',*,*,#7994,.T.);
#10654=ORIENTED_EDGE('',*,*,#7995,.T.);
#10655=ORIENTED_EDGE('',*,*,#7994,.F.);
#10656=ORIENTED_EDGE('',*,*,#7995,.F.);
#10657=ORIENTED_EDGE('',*,*,#7996,.T.);
#10658=ORIENTED_EDGE('',*,*,#7997,.F.);
#10659=ORIENTED_EDGE('',*,*,#7996,.F.);
#10660=ORIENTED_EDGE('',*,*,#7998,.F.);
#10661=ORIENTED_EDGE('',*,*,#7999,.T.);
#10662=ORIENTED_EDGE('',*,*,#8000,.T.);
#10663=ORIENTED_EDGE('',*,*,#7999,.F.);
#10664=ORIENTED_EDGE('',*,*,#8000,.F.);
#10665=ORIENTED_EDGE('',*,*,#8001,.T.);
#10666=ORIENTED_EDGE('',*,*,#8002,.F.);
#10667=ORIENTED_EDGE('',*,*,#8001,.F.);
#10668=ORIENTED_EDGE('',*,*,#8003,.F.);
#10669=ORIENTED_EDGE('',*,*,#8004,.F.);
#10670=ORIENTED_EDGE('',*,*,#7626,.F.);
#10671=ORIENTED_EDGE('',*,*,#7631,.T.);
#10672=ORIENTED_EDGE('',*,*,#8005,.F.);
#10673=ORIENTED_EDGE('',*,*,#7632,.F.);
#10674=ORIENTED_EDGE('',*,*,#7627,.F.);
#10675=ORIENTED_EDGE('',*,*,#8004,.T.);
#10676=ORIENTED_EDGE('',*,*,#7993,.T.);
#10677=ORIENTED_EDGE('',*,*,#7669,.T.);
#10678=ORIENTED_EDGE('',*,*,#7724,.F.);
#10679=ORIENTED_EDGE('',*,*,#8006,.T.);
#10680=ORIENTED_EDGE('',*,*,#8007,.F.);
#10681=ORIENTED_EDGE('',*,*,#7729,.F.);
#10682=ORIENTED_EDGE('',*,*,#7665,.T.);
#10683=ORIENTED_EDGE('',*,*,#8008,.F.);
#10684=ORIENTED_EDGE('',*,*,#8006,.F.);
#10685=ORIENTED_EDGE('',*,*,#7723,.F.);
#10686=ORIENTED_EDGE('',*,*,#8009,.T.);
#10687=ORIENTED_EDGE('',*,*,#7744,.F.);
#10688=ORIENTED_EDGE('',*,*,#8010,.F.);
#10689=ORIENTED_EDGE('',*,*,#8009,.F.);
#10690=ORIENTED_EDGE('',*,*,#7722,.F.);
#10691=ORIENTED_EDGE('',*,*,#7983,.T.);
#10692=ORIENTED_EDGE('',*,*,#8005,.T.);
#10693=ORIENTED_EDGE('',*,*,#8003,.T.);
#10694=ORIENTED_EDGE('',*,*,#7630,.T.);
#10695=ORIENTED_EDGE('',*,*,#7641,.T.);
#10696=ORIENTED_EDGE('',*,*,#7911,.F.);
#10697=ORIENTED_EDGE('',*,*,#7858,.T.);
#10698=ORIENTED_EDGE('',*,*,#7904,.F.);
#10699=ORIENTED_EDGE('',*,*,#7730,.T.);
#10700=ORIENTED_EDGE('',*,*,#8007,.T.);
#10701=ORIENTED_EDGE('',*,*,#8008,.T.);
#10702=ORIENTED_EDGE('',*,*,#8010,.T.);
#10703=ORIENTED_EDGE('',*,*,#7743,.T.);
#10704=ORIENTED_EDGE('',*,*,#8011,.F.);
#10705=ORIENTED_EDGE('',*,*,#8012,.T.);
#10706=ORIENTED_EDGE('',*,*,#8013,.T.);
#10707=ORIENTED_EDGE('',*,*,#8014,.T.);
#10708=ORIENTED_EDGE('',*,*,#8015,.T.);
#10709=ORIENTED_EDGE('',*,*,#8016,.T.);
#10710=ORIENTED_EDGE('',*,*,#8017,.F.);
#10711=ORIENTED_EDGE('',*,*,#7633,.T.);
#10712=ORIENTED_EDGE('',*,*,#7748,.T.);
#10713=ORIENTED_EDGE('',*,*,#7764,.T.);
#10714=ORIENTED_EDGE('',*,*,#7761,.T.);
#10715=ORIENTED_EDGE('',*,*,#7758,.T.);
#10716=ORIENTED_EDGE('',*,*,#7755,.T.);
#10717=ORIENTED_EDGE('',*,*,#7752,.T.);
#10718=ORIENTED_EDGE('',*,*,#7928,.T.);
#10719=ORIENTED_EDGE('',*,*,#7939,.T.);
#10720=ORIENTED_EDGE('',*,*,#7950,.T.);
#10721=ORIENTED_EDGE('',*,*,#7961,.T.);
#10722=ORIENTED_EDGE('',*,*,#8018,.T.);
#10723=ORIENTED_EDGE('',*,*,#8019,.F.);
#10724=ORIENTED_EDGE('',*,*,#8020,.F.);
#10725=ORIENTED_EDGE('',*,*,#8021,.T.);
#10726=ORIENTED_EDGE('',*,*,#7636,.F.);
#10727=ORIENTED_EDGE('',*,*,#7998,.T.);
#10728=ORIENTED_EDGE('',*,*,#7610,.T.);
#10729=ORIENTED_EDGE('',*,*,#7637,.F.);
#10730=ORIENTED_EDGE('',*,*,#8021,.F.);
#10731=ORIENTED_EDGE('',*,*,#8022,.F.);
#10732=ORIENTED_EDGE('',*,*,#8023,.F.);
#10733=ORIENTED_EDGE('',*,*,#7623,.T.);
#10734=ORIENTED_EDGE('',*,*,#7812,.F.);
#10735=ORIENTED_EDGE('',*,*,#7828,.F.);
#10736=ORIENTED_EDGE('',*,*,#7787,.F.);
#10737=ORIENTED_EDGE('',*,*,#8024,.F.);
#10738=ORIENTED_EDGE('',*,*,#8022,.T.);
#10739=ORIENTED_EDGE('',*,*,#8020,.T.);
#10740=ORIENTED_EDGE('',*,*,#8025,.F.);
#10741=ORIENTED_EDGE('',*,*,#8026,.F.);
#10742=ORIENTED_EDGE('',*,*,#7624,.T.);
#10743=ORIENTED_EDGE('',*,*,#8023,.T.);
#10744=ORIENTED_EDGE('',*,*,#8024,.T.);
#10745=ORIENTED_EDGE('',*,*,#7786,.F.);
#10746=ORIENTED_EDGE('',*,*,#7638,.F.);
#10747=ORIENTED_EDGE('',*,*,#7614,.T.);
#10748=ORIENTED_EDGE('',*,*,#7800,.F.);
#10749=ORIENTED_EDGE('',*,*,#8027,.F.);
#10750=ORIENTED_EDGE('',*,*,#8028,.F.);
#10751=ORIENTED_EDGE('',*,*,#8029,.F.);
#10752=ORIENTED_EDGE('',*,*,#8030,.T.);
#10753=ORIENTED_EDGE('',*,*,#7727,.T.);
#10754=ORIENTED_EDGE('',*,*,#7782,.F.);
#10755=ORIENTED_EDGE('',*,*,#8031,.F.);
#10756=ORIENTED_EDGE('',*,*,#8032,.F.);
#10757=ORIENTED_EDGE('',*,*,#7740,.F.);
#10758=ORIENTED_EDGE('',*,*,#8033,.T.);
#10759=ORIENTED_EDGE('',*,*,#8029,.T.);
#10760=ORIENTED_EDGE('',*,*,#7988,.T.);
#10761=ORIENTED_EDGE('',*,*,#7720,.T.);
#10762=ORIENTED_EDGE('',*,*,#7728,.F.);
#10763=ORIENTED_EDGE('',*,*,#8030,.F.);
#10764=ORIENTED_EDGE('',*,*,#8033,.F.);
#10765=ORIENTED_EDGE('',*,*,#7739,.F.);
#10766=ORIENTED_EDGE('',*,*,#7713,.T.);
#10767=ORIENTED_EDGE('',*,*,#7809,.F.);
#10768=ORIENTED_EDGE('',*,*,#8026,.T.);
#10769=ORIENTED_EDGE('',*,*,#8034,.F.);
#10770=ORIENTED_EDGE('',*,*,#8035,.T.);
#10771=ORIENTED_EDGE('',*,*,#7797,.F.);
#10772=ORIENTED_EDGE('',*,*,#8031,.T.);
#10773=ORIENTED_EDGE('',*,*,#7781,.F.);
#10774=ORIENTED_EDGE('',*,*,#7833,.T.);
#10775=ORIENTED_EDGE('',*,*,#7803,.F.);
#10776=ORIENTED_EDGE('',*,*,#8036,.F.);
#10777=ORIENTED_EDGE('',*,*,#8037,.F.);
#10778=ORIENTED_EDGE('',*,*,#8027,.T.);
#10779=ORIENTED_EDGE('',*,*,#8025,.T.);
#10780=ORIENTED_EDGE('',*,*,#8019,.T.);
#10781=ORIENTED_EDGE('',*,*,#7635,.T.);
#10782=ORIENTED_EDGE('',*,*,#8038,.F.);
#10783=ORIENTED_EDGE('',*,*,#8039,.T.);
#10784=ORIENTED_EDGE('',*,*,#8040,.T.);
#10785=ORIENTED_EDGE('',*,*,#8041,.T.);
#10786=ORIENTED_EDGE('',*,*,#8042,.T.);
#10787=ORIENTED_EDGE('',*,*,#8043,.T.);
#10788=ORIENTED_EDGE('',*,*,#8044,.F.);
#10789=ORIENTED_EDGE('',*,*,#7741,.T.);
#10790=ORIENTED_EDGE('',*,*,#8032,.T.);
#10791=ORIENTED_EDGE('',*,*,#8028,.T.);
#10792=ORIENTED_EDGE('',*,*,#8037,.T.);
#10793=ORIENTED_EDGE('',*,*,#8045,.T.);
#10794=ORIENTED_EDGE('',*,*,#8034,.T.);
#10795=ORIENTED_EDGE('',*,*,#8042,.F.);
#10796=ORIENTED_EDGE('',*,*,#8046,.T.);
#10797=ORIENTED_EDGE('',*,*,#8013,.F.);
#10798=ORIENTED_EDGE('',*,*,#8047,.F.);
#10799=ORIENTED_EDGE('',*,*,#8040,.F.);
#10800=ORIENTED_EDGE('',*,*,#8048,.F.);
#10801=ORIENTED_EDGE('',*,*,#8015,.F.);
#10802=ORIENTED_EDGE('',*,*,#8049,.T.);
#10803=ORIENTED_EDGE('',*,*,#8041,.F.);
#10804=ORIENTED_EDGE('',*,*,#8049,.F.);
#10805=ORIENTED_EDGE('',*,*,#8014,.F.);
#10806=ORIENTED_EDGE('',*,*,#8046,.F.);
#10807=ORIENTED_EDGE('',*,*,#8048,.T.);
#10808=ORIENTED_EDGE('',*,*,#8039,.F.);
#10809=ORIENTED_EDGE('',*,*,#8050,.F.);
#10810=ORIENTED_EDGE('',*,*,#8016,.F.);
#10811=ORIENTED_EDGE('',*,*,#7997,.T.);
#10812=ORIENTED_EDGE('',*,*,#8002,.T.);
#10813=ORIENTED_EDGE('',*,*,#8047,.T.);
#10814=ORIENTED_EDGE('',*,*,#8012,.F.);
#10815=ORIENTED_EDGE('',*,*,#8051,.F.);
#10816=ORIENTED_EDGE('',*,*,#8043,.F.);
#10817=ORIENTED_EDGE('',*,*,#7987,.T.);
#10818=ORIENTED_EDGE('',*,*,#7992,.T.);
#10819=ORIENTED_EDGE('',*,*,#7890,.F.);
#10820=ORIENTED_EDGE('',*,*,#8052,.T.);
#10821=ORIENTED_EDGE('',*,*,#8053,.T.);
#10822=ORIENTED_EDGE('',*,*,#8054,.F.);
#10823=ORIENTED_EDGE('',*,*,#7893,.F.);
#10824=ORIENTED_EDGE('',*,*,#8055,.T.);
#10825=ORIENTED_EDGE('',*,*,#8056,.T.);
#10826=ORIENTED_EDGE('',*,*,#8052,.F.);
#10827=ORIENTED_EDGE('',*,*,#7892,.F.);
#10828=ORIENTED_EDGE('',*,*,#8057,.T.);
#10829=ORIENTED_EDGE('',*,*,#8058,.T.);
#10830=ORIENTED_EDGE('',*,*,#8055,.F.);
#10831=ORIENTED_EDGE('',*,*,#7891,.F.);
#10832=ORIENTED_EDGE('',*,*,#8054,.T.);
#10833=ORIENTED_EDGE('',*,*,#8059,.T.);
#10834=ORIENTED_EDGE('',*,*,#8057,.F.);
#10835=ORIENTED_EDGE('',*,*,#8059,.F.);
#10836=ORIENTED_EDGE('',*,*,#8053,.F.);
#10837=ORIENTED_EDGE('',*,*,#8056,.F.);
#10838=ORIENTED_EDGE('',*,*,#8058,.F.);
#10839=ORIENTED_EDGE('',*,*,#7886,.F.);
#10840=ORIENTED_EDGE('',*,*,#8060,.T.);
#10841=ORIENTED_EDGE('',*,*,#8061,.T.);
#10842=ORIENTED_EDGE('',*,*,#8062,.F.);
#10843=ORIENTED_EDGE('',*,*,#7889,.F.);
#10844=ORIENTED_EDGE('',*,*,#8063,.T.);
#10845=ORIENTED_EDGE('',*,*,#8064,.T.);
#10846=ORIENTED_EDGE('',*,*,#8060,.F.);
#10847=ORIENTED_EDGE('',*,*,#7888,.F.);
#10848=ORIENTED_EDGE('',*,*,#8065,.T.);
#10849=ORIENTED_EDGE('',*,*,#8066,.T.);
#10850=ORIENTED_EDGE('',*,*,#8063,.F.);
#10851=ORIENTED_EDGE('',*,*,#7887,.F.);
#10852=ORIENTED_EDGE('',*,*,#8062,.T.);
#10853=ORIENTED_EDGE('',*,*,#8067,.T.);
#10854=ORIENTED_EDGE('',*,*,#8065,.F.);
#10855=ORIENTED_EDGE('',*,*,#8067,.F.);
#10856=ORIENTED_EDGE('',*,*,#8061,.F.);
#10857=ORIENTED_EDGE('',*,*,#8064,.F.);
#10858=ORIENTED_EDGE('',*,*,#8066,.F.);
#10859=ORIENTED_EDGE('',*,*,#7882,.F.);
#10860=ORIENTED_EDGE('',*,*,#8068,.T.);
#10861=ORIENTED_EDGE('',*,*,#8069,.T.);
#10862=ORIENTED_EDGE('',*,*,#8070,.F.);
#10863=ORIENTED_EDGE('',*,*,#7885,.F.);
#10864=ORIENTED_EDGE('',*,*,#8071,.T.);
#10865=ORIENTED_EDGE('',*,*,#8072,.T.);
#10866=ORIENTED_EDGE('',*,*,#8068,.F.);
#10867=ORIENTED_EDGE('',*,*,#7884,.F.);
#10868=ORIENTED_EDGE('',*,*,#8073,.T.);
#10869=ORIENTED_EDGE('',*,*,#8074,.T.);
#10870=ORIENTED_EDGE('',*,*,#8071,.F.);
#10871=ORIENTED_EDGE('',*,*,#7883,.F.);
#10872=ORIENTED_EDGE('',*,*,#8070,.T.);
#10873=ORIENTED_EDGE('',*,*,#8075,.T.);
#10874=ORIENTED_EDGE('',*,*,#8073,.F.);
#10875=ORIENTED_EDGE('',*,*,#8075,.F.);
#10876=ORIENTED_EDGE('',*,*,#8069,.F.);
#10877=ORIENTED_EDGE('',*,*,#8072,.F.);
#10878=ORIENTED_EDGE('',*,*,#8074,.F.);
#10879=ORIENTED_EDGE('',*,*,#7878,.F.);
#10880=ORIENTED_EDGE('',*,*,#8076,.T.);
#10881=ORIENTED_EDGE('',*,*,#8077,.T.);
#10882=ORIENTED_EDGE('',*,*,#8078,.F.);
#10883=ORIENTED_EDGE('',*,*,#7881,.F.);
#10884=ORIENTED_EDGE('',*,*,#8079,.T.);
#10885=ORIENTED_EDGE('',*,*,#8080,.T.);
#10886=ORIENTED_EDGE('',*,*,#8076,.F.);
#10887=ORIENTED_EDGE('',*,*,#7880,.F.);
#10888=ORIENTED_EDGE('',*,*,#8081,.T.);
#10889=ORIENTED_EDGE('',*,*,#8082,.T.);
#10890=ORIENTED_EDGE('',*,*,#8079,.F.);
#10891=ORIENTED_EDGE('',*,*,#7879,.F.);
#10892=ORIENTED_EDGE('',*,*,#8078,.T.);
#10893=ORIENTED_EDGE('',*,*,#8083,.T.);
#10894=ORIENTED_EDGE('',*,*,#8081,.F.);
#10895=ORIENTED_EDGE('',*,*,#8083,.F.);
#10896=ORIENTED_EDGE('',*,*,#8077,.F.);
#10897=ORIENTED_EDGE('',*,*,#8080,.F.);
#10898=ORIENTED_EDGE('',*,*,#8082,.F.);
#10899=ORIENTED_EDGE('',*,*,#7874,.F.);
#10900=ORIENTED_EDGE('',*,*,#8084,.T.);
#10901=ORIENTED_EDGE('',*,*,#8085,.T.);
#10902=ORIENTED_EDGE('',*,*,#8086,.F.);
#10903=ORIENTED_EDGE('',*,*,#7877,.F.);
#10904=ORIENTED_EDGE('',*,*,#8087,.T.);
#10905=ORIENTED_EDGE('',*,*,#8088,.T.);
#10906=ORIENTED_EDGE('',*,*,#8084,.F.);
#10907=ORIENTED_EDGE('',*,*,#7876,.F.);
#10908=ORIENTED_EDGE('',*,*,#8089,.T.);
#10909=ORIENTED_EDGE('',*,*,#8090,.T.);
#10910=ORIENTED_EDGE('',*,*,#8087,.F.);
#10911=ORIENTED_EDGE('',*,*,#7875,.F.);
#10912=ORIENTED_EDGE('',*,*,#8086,.T.);
#10913=ORIENTED_EDGE('',*,*,#8091,.T.);
#10914=ORIENTED_EDGE('',*,*,#8089,.F.);
#10915=ORIENTED_EDGE('',*,*,#8091,.F.);
#10916=ORIENTED_EDGE('',*,*,#8085,.F.);
#10917=ORIENTED_EDGE('',*,*,#8088,.F.);
#10918=ORIENTED_EDGE('',*,*,#8090,.F.);
#10919=ORIENTED_EDGE('',*,*,#7870,.F.);
#10920=ORIENTED_EDGE('',*,*,#8092,.T.);
#10921=ORIENTED_EDGE('',*,*,#8093,.T.);
#10922=ORIENTED_EDGE('',*,*,#8094,.F.);
#10923=ORIENTED_EDGE('',*,*,#7873,.F.);
#10924=ORIENTED_EDGE('',*,*,#8095,.T.);
#10925=ORIENTED_EDGE('',*,*,#8096,.T.);
#10926=ORIENTED_EDGE('',*,*,#8092,.F.);
#10927=ORIENTED_EDGE('',*,*,#7872,.F.);
#10928=ORIENTED_EDGE('',*,*,#8097,.T.);
#10929=ORIENTED_EDGE('',*,*,#8098,.T.);
#10930=ORIENTED_EDGE('',*,*,#8095,.F.);
#10931=ORIENTED_EDGE('',*,*,#7871,.F.);
#10932=ORIENTED_EDGE('',*,*,#8094,.T.);
#10933=ORIENTED_EDGE('',*,*,#8099,.T.);
#10934=ORIENTED_EDGE('',*,*,#8097,.F.);
#10935=ORIENTED_EDGE('',*,*,#8099,.F.);
#10936=ORIENTED_EDGE('',*,*,#8093,.F.);
#10937=ORIENTED_EDGE('',*,*,#8096,.F.);
#10938=ORIENTED_EDGE('',*,*,#8098,.F.);
#10939=ORIENTED_EDGE('',*,*,#7642,.F.);
#10940=ORIENTED_EDGE('',*,*,#8100,.T.);
#10941=ORIENTED_EDGE('',*,*,#8101,.T.);
#10942=ORIENTED_EDGE('',*,*,#8100,.F.);
#10943=ORIENTED_EDGE('',*,*,#8102,.T.);
#10944=ORIENTED_EDGE('',*,*,#8101,.F.);
#10945=ORIENTED_EDGE('',*,*,#8102,.F.);
#10946=ORIENTED_EDGE('',*,*,#8103,.T.);
#10947=ORIENTED_EDGE('',*,*,#8104,.T.);
#10948=ORIENTED_EDGE('',*,*,#8103,.F.);
#10949=ORIENTED_EDGE('',*,*,#8104,.F.);
#10950=ORIENTED_EDGE('',*,*,#8105,.T.);
#10951=ORIENTED_EDGE('',*,*,#8105,.F.);
#10952=ORIENTED_EDGE('',*,*,#8106,.T.);
#10953=ORIENTED_EDGE('',*,*,#8107,.T.);
#10954=ORIENTED_EDGE('',*,*,#8106,.F.);
#10955=ORIENTED_EDGE('',*,*,#8107,.F.);
#10956=ORIENTED_EDGE('',*,*,#8108,.T.);
#10957=ORIENTED_EDGE('',*,*,#8108,.F.);
#10958=ORIENTED_EDGE('',*,*,#8109,.T.);
#10959=ORIENTED_EDGE('',*,*,#8110,.F.);
#10960=ORIENTED_EDGE('',*,*,#8111,.F.);
#10961=ORIENTED_EDGE('',*,*,#8112,.T.);
#10962=ORIENTED_EDGE('',*,*,#8113,.T.);
#10963=ORIENTED_EDGE('',*,*,#8112,.F.);
#10964=ORIENTED_EDGE('',*,*,#8114,.F.);
#10965=ORIENTED_EDGE('',*,*,#8109,.F.);
#10966=ORIENTED_EDGE('',*,*,#7839,.T.);
#10967=ORIENTED_EDGE('',*,*,#7840,.T.);
#10968=ORIENTED_EDGE('',*,*,#8115,.T.);
#10969=ORIENTED_EDGE('',*,*,#8113,.F.);
#10970=ORIENTED_EDGE('',*,*,#8115,.F.);
#10971=ORIENTED_EDGE('',*,*,#8116,.T.);
#10972=ORIENTED_EDGE('',*,*,#8117,.T.);
#10973=ORIENTED_EDGE('',*,*,#8116,.F.);
#10974=ORIENTED_EDGE('',*,*,#8118,.T.);
#10975=ORIENTED_EDGE('',*,*,#8117,.F.);
#10976=ORIENTED_EDGE('',*,*,#8118,.F.);
#10977=ORIENTED_EDGE('',*,*,#8119,.T.);
#10978=ORIENTED_EDGE('',*,*,#8120,.T.);
#10979=ORIENTED_EDGE('',*,*,#8119,.F.);
#10980=ORIENTED_EDGE('',*,*,#8120,.F.);
#10981=ORIENTED_EDGE('',*,*,#8121,.T.);
#10982=ORIENTED_EDGE('',*,*,#8121,.F.);
#10983=ORIENTED_EDGE('',*,*,#8122,.T.);
#10984=ORIENTED_EDGE('',*,*,#7745,.F.);
#10985=ORIENTED_EDGE('',*,*,#8122,.F.);
#10986=ORIENTED_EDGE('',*,*,#8018,.F.);
#10987=ORIENTED_EDGE('',*,*,#8123,.T.);
#10988=ORIENTED_EDGE('',*,*,#8124,.T.);
#10989=ORIENTED_EDGE('',*,*,#8123,.F.);
#10990=ORIENTED_EDGE('',*,*,#8110,.T.);
#10991=ORIENTED_EDGE('',*,*,#8114,.T.);
#10992=ORIENTED_EDGE('',*,*,#8111,.T.);
#10993=ORIENTED_EDGE('',*,*,#8124,.F.);
#10994=ORIENTED_EDGE('',*,*,#8125,.T.);
#10995=ORIENTED_EDGE('',*,*,#8125,.F.);
#10996=ORIENTED_EDGE('',*,*,#8126,.T.);
#10997=ORIENTED_EDGE('',*,*,#8127,.T.);
#10998=ORIENTED_EDGE('',*,*,#8126,.F.);
#10999=ORIENTED_EDGE('',*,*,#8127,.F.);
#11000=ORIENTED_EDGE('',*,*,#8128,.T.);
#11001=ORIENTED_EDGE('',*,*,#8128,.F.);
#11002=ORIENTED_EDGE('',*,*,#8129,.T.);
#11003=ORIENTED_EDGE('',*,*,#8130,.T.);
#11004=ORIENTED_EDGE('',*,*,#8129,.F.);
#11005=ORIENTED_EDGE('',*,*,#8130,.F.);
#11006=ORIENTED_EDGE('',*,*,#8131,.T.);
#11007=ORIENTED_EDGE('',*,*,#7834,.F.);
#11008=ORIENTED_EDGE('',*,*,#8131,.F.);
#11009=ORIENTED_EDGE('',*,*,#7806,.F.);
#11010=ORIENTED_EDGE('',*,*,#8035,.F.);
#11011=ORIENTED_EDGE('',*,*,#8045,.F.);
#11012=ORIENTED_EDGE('',*,*,#8036,.T.);
#11013=ORIENTED_EDGE('',*,*,#8038,.T.);
#11014=ORIENTED_EDGE('',*,*,#7634,.T.);
#11015=ORIENTED_EDGE('',*,*,#8017,.T.);
#11016=ORIENTED_EDGE('',*,*,#8050,.T.);
#11017=ORIENTED_EDGE('',*,*,#8044,.T.);
#11018=ORIENTED_EDGE('',*,*,#8051,.T.);
#11019=ORIENTED_EDGE('',*,*,#8011,.T.);
#11020=ORIENTED_EDGE('',*,*,#7742,.T.);
#11021=ORIENTED_EDGE('',*,*,#8132,.T.);
#11022=ORIENTED_EDGE('',*,*,#8133,.T.);
#11023=ORIENTED_EDGE('',*,*,#8134,.T.);
#11024=ORIENTED_EDGE('',*,*,#8133,.F.);
#11025=ORIENTED_EDGE('',*,*,#8132,.F.);
#11026=ORIENTED_EDGE('',*,*,#8135,.T.);
#11027=ORIENTED_EDGE('',*,*,#8136,.F.);
#11028=ORIENTED_EDGE('',*,*,#8135,.F.);
#11029=ORIENTED_EDGE('',*,*,#8134,.F.);
#11030=ORIENTED_EDGE('',*,*,#8137,.T.);
#11031=ORIENTED_EDGE('',*,*,#8138,.T.);
#11032=ORIENTED_EDGE('',*,*,#8139,.T.);
#11033=ORIENTED_EDGE('',*,*,#8140,.T.);
#11034=ORIENTED_EDGE('',*,*,#8141,.F.);
#11035=ORIENTED_EDGE('',*,*,#8142,.T.);
#11036=ORIENTED_EDGE('',*,*,#8143,.T.);
#11037=ORIENTED_EDGE('',*,*,#8144,.T.);
#11038=ORIENTED_EDGE('',*,*,#8139,.F.);
#11039=ORIENTED_EDGE('',*,*,#8145,.T.);
#11040=ORIENTED_EDGE('',*,*,#8146,.T.);
#11041=ORIENTED_EDGE('',*,*,#8147,.T.);
#11042=ORIENTED_EDGE('',*,*,#8143,.F.);
#11043=ORIENTED_EDGE('',*,*,#8148,.T.);
#11044=ORIENTED_EDGE('',*,*,#8149,.T.);
#11045=ORIENTED_EDGE('',*,*,#8150,.T.);
#11046=ORIENTED_EDGE('',*,*,#8146,.F.);
#11047=ORIENTED_EDGE('',*,*,#8151,.T.);
#11048=ORIENTED_EDGE('',*,*,#8152,.T.);
#11049=ORIENTED_EDGE('',*,*,#8153,.T.);
#11050=ORIENTED_EDGE('',*,*,#8149,.F.);
#11051=ORIENTED_EDGE('',*,*,#8154,.T.);
#11052=ORIENTED_EDGE('',*,*,#8152,.F.);
#11053=ORIENTED_EDGE('',*,*,#8155,.T.);
#11054=ORIENTED_EDGE('',*,*,#8156,.T.);
#11055=ORIENTED_EDGE('',*,*,#8157,.T.);
#11056=ORIENTED_EDGE('',*,*,#8156,.F.);
#11057=ORIENTED_EDGE('',*,*,#8158,.T.);
#11058=ORIENTED_EDGE('',*,*,#8159,.T.);
#11059=ORIENTED_EDGE('',*,*,#8160,.T.);
#11060=ORIENTED_EDGE('',*,*,#8159,.F.);
#11061=ORIENTED_EDGE('',*,*,#8161,.T.);
#11062=ORIENTED_EDGE('',*,*,#8141,.T.);
#11063=ORIENTED_EDGE('',*,*,#8154,.F.);
#11064=ORIENTED_EDGE('',*,*,#8162,.F.);
#11065=ORIENTED_EDGE('',*,*,#8163,.F.);
#11066=ORIENTED_EDGE('',*,*,#8164,.T.);
#11067=ORIENTED_EDGE('',*,*,#8157,.F.);
#11068=ORIENTED_EDGE('',*,*,#8165,.F.);
#11069=ORIENTED_EDGE('',*,*,#8166,.F.);
#11070=ORIENTED_EDGE('',*,*,#8162,.T.);
#11071=ORIENTED_EDGE('',*,*,#8160,.F.);
#11072=ORIENTED_EDGE('',*,*,#8167,.F.);
#11073=ORIENTED_EDGE('',*,*,#8168,.F.);
#11074=ORIENTED_EDGE('',*,*,#8165,.T.);
#11075=ORIENTED_EDGE('',*,*,#8140,.F.);
#11076=ORIENTED_EDGE('',*,*,#8169,.F.);
#11077=ORIENTED_EDGE('',*,*,#8170,.F.);
#11078=ORIENTED_EDGE('',*,*,#8167,.T.);
#11079=ORIENTED_EDGE('',*,*,#8138,.F.);
#11080=ORIENTED_EDGE('',*,*,#8161,.F.);
#11081=ORIENTED_EDGE('',*,*,#8158,.F.);
#11082=ORIENTED_EDGE('',*,*,#8155,.F.);
#11083=ORIENTED_EDGE('',*,*,#8151,.F.);
#11084=ORIENTED_EDGE('',*,*,#8148,.F.);
#11085=ORIENTED_EDGE('',*,*,#8145,.F.);
#11086=ORIENTED_EDGE('',*,*,#8142,.F.);
#11087=ORIENTED_EDGE('',*,*,#8171,.T.);
#11088=ORIENTED_EDGE('',*,*,#8172,.T.);
#11089=ORIENTED_EDGE('',*,*,#8173,.T.);
#11090=ORIENTED_EDGE('',*,*,#8174,.T.);
#11091=ORIENTED_EDGE('',*,*,#8175,.T.);
#11092=ORIENTED_EDGE('',*,*,#8176,.T.);
#11093=ORIENTED_EDGE('',*,*,#8177,.T.);
#11094=ORIENTED_EDGE('',*,*,#8178,.F.);
#11095=ORIENTED_EDGE('',*,*,#8177,.F.);
#11096=ORIENTED_EDGE('',*,*,#8176,.F.);
#11097=ORIENTED_EDGE('',*,*,#8179,.T.);
#11098=ORIENTED_EDGE('',*,*,#8180,.T.);
#11099=ORIENTED_EDGE('',*,*,#8179,.F.);
#11100=ORIENTED_EDGE('',*,*,#8180,.F.);
#11101=ORIENTED_EDGE('',*,*,#8181,.T.);
#11102=ORIENTED_EDGE('',*,*,#8182,.T.);
#11103=ORIENTED_EDGE('',*,*,#8181,.F.);
#11104=ORIENTED_EDGE('',*,*,#8183,.T.);
#11105=ORIENTED_EDGE('',*,*,#8182,.F.);
#11106=ORIENTED_EDGE('',*,*,#8183,.F.);
#11107=ORIENTED_EDGE('',*,*,#8184,.T.);
#11108=ORIENTED_EDGE('',*,*,#8175,.F.);
#11109=ORIENTED_EDGE('',*,*,#8184,.F.);
#11110=ORIENTED_EDGE('',*,*,#8185,.T.);
#11111=ORIENTED_EDGE('',*,*,#8186,.T.);
#11112=ORIENTED_EDGE('',*,*,#8187,.F.);
#11113=ORIENTED_EDGE('',*,*,#8186,.F.);
#11114=ORIENTED_EDGE('',*,*,#8185,.F.);
#11115=ORIENTED_EDGE('',*,*,#8188,.T.);
#11116=ORIENTED_EDGE('',*,*,#8189,.T.);
#11117=ORIENTED_EDGE('',*,*,#8188,.F.);
#11118=ORIENTED_EDGE('',*,*,#8189,.F.);
#11119=ORIENTED_EDGE('',*,*,#8190,.T.);
#11120=ORIENTED_EDGE('',*,*,#8191,.T.);
#11121=ORIENTED_EDGE('',*,*,#8190,.F.);
#11122=ORIENTED_EDGE('',*,*,#8192,.T.);
#11123=ORIENTED_EDGE('',*,*,#8191,.F.);
#11124=ORIENTED_EDGE('',*,*,#8192,.F.);
#11125=ORIENTED_EDGE('',*,*,#8193,.T.);
#11126=ORIENTED_EDGE('',*,*,#8174,.F.);
#11127=ORIENTED_EDGE('',*,*,#8193,.F.);
#11128=ORIENTED_EDGE('',*,*,#8194,.T.);
#11129=ORIENTED_EDGE('',*,*,#8195,.T.);
#11130=ORIENTED_EDGE('',*,*,#8196,.F.);
#11131=ORIENTED_EDGE('',*,*,#8195,.F.);
#11132=ORIENTED_EDGE('',*,*,#8194,.F.);
#11133=ORIENTED_EDGE('',*,*,#8197,.T.);
#11134=ORIENTED_EDGE('',*,*,#8198,.T.);
#11135=ORIENTED_EDGE('',*,*,#8197,.F.);
#11136=ORIENTED_EDGE('',*,*,#8198,.F.);
#11137=ORIENTED_EDGE('',*,*,#8199,.T.);
#11138=ORIENTED_EDGE('',*,*,#8200,.T.);
#11139=ORIENTED_EDGE('',*,*,#8199,.F.);
#11140=ORIENTED_EDGE('',*,*,#8201,.T.);
#11141=ORIENTED_EDGE('',*,*,#8200,.F.);
#11142=ORIENTED_EDGE('',*,*,#8201,.F.);
#11143=ORIENTED_EDGE('',*,*,#8202,.T.);
#11144=ORIENTED_EDGE('',*,*,#8173,.F.);
#11145=ORIENTED_EDGE('',*,*,#8202,.F.);
#11146=ORIENTED_EDGE('',*,*,#8203,.T.);
#11147=ORIENTED_EDGE('',*,*,#8204,.T.);
#11148=ORIENTED_EDGE('',*,*,#8205,.F.);
#11149=ORIENTED_EDGE('',*,*,#8204,.F.);
#11150=ORIENTED_EDGE('',*,*,#8203,.F.);
#11151=ORIENTED_EDGE('',*,*,#8206,.T.);
#11152=ORIENTED_EDGE('',*,*,#8207,.T.);
#11153=ORIENTED_EDGE('',*,*,#8206,.F.);
#11154=ORIENTED_EDGE('',*,*,#8207,.F.);
#11155=ORIENTED_EDGE('',*,*,#8208,.T.);
#11156=ORIENTED_EDGE('',*,*,#8209,.T.);
#11157=ORIENTED_EDGE('',*,*,#8208,.F.);
#11158=ORIENTED_EDGE('',*,*,#8210,.T.);
#11159=ORIENTED_EDGE('',*,*,#8209,.F.);
#11160=ORIENTED_EDGE('',*,*,#8210,.F.);
#11161=ORIENTED_EDGE('',*,*,#8211,.T.);
#11162=ORIENTED_EDGE('',*,*,#8172,.F.);
#11163=ORIENTED_EDGE('',*,*,#8211,.F.);
#11164=ORIENTED_EDGE('',*,*,#8212,.T.);
#11165=ORIENTED_EDGE('',*,*,#8213,.T.);
#11166=ORIENTED_EDGE('',*,*,#8171,.F.);
#11167=ORIENTED_EDGE('',*,*,#8213,.F.);
#11168=ORIENTED_EDGE('',*,*,#8212,.F.);
#11169=ORIENTED_EDGE('',*,*,#8214,.T.);
#11170=ORIENTED_EDGE('',*,*,#8215,.T.);
#11171=ORIENTED_EDGE('',*,*,#8214,.F.);
#11172=ORIENTED_EDGE('',*,*,#8216,.T.);
#11173=ORIENTED_EDGE('',*,*,#8215,.F.);
#11174=ORIENTED_EDGE('',*,*,#8216,.F.);
#11175=ORIENTED_EDGE('',*,*,#8217,.T.);
#11176=ORIENTED_EDGE('',*,*,#8137,.F.);
#11177=ORIENTED_EDGE('',*,*,#8217,.F.);
#11178=ORIENTED_EDGE('',*,*,#8144,.F.);
#11179=ORIENTED_EDGE('',*,*,#8218,.F.);
#11180=ORIENTED_EDGE('',*,*,#8219,.F.);
#11181=ORIENTED_EDGE('',*,*,#8169,.T.);
#11182=ORIENTED_EDGE('',*,*,#8147,.F.);
#11183=ORIENTED_EDGE('',*,*,#8220,.F.);
#11184=ORIENTED_EDGE('',*,*,#8221,.F.);
#11185=ORIENTED_EDGE('',*,*,#8218,.T.);
#11186=ORIENTED_EDGE('',*,*,#8150,.F.);
#11187=ORIENTED_EDGE('',*,*,#8222,.F.);
#11188=ORIENTED_EDGE('',*,*,#8223,.F.);
#11189=ORIENTED_EDGE('',*,*,#8220,.T.);
#11190=ORIENTED_EDGE('',*,*,#8153,.F.);
#11191=ORIENTED_EDGE('',*,*,#8164,.F.);
#11192=ORIENTED_EDGE('',*,*,#8224,.F.);
#11193=ORIENTED_EDGE('',*,*,#8222,.T.);
#11194=ORIENTED_EDGE('',*,*,#8224,.T.);
#11195=ORIENTED_EDGE('',*,*,#8163,.T.);
#11196=ORIENTED_EDGE('',*,*,#8166,.T.);
#11197=ORIENTED_EDGE('',*,*,#8168,.T.);
#11198=ORIENTED_EDGE('',*,*,#8170,.T.);
#11199=ORIENTED_EDGE('',*,*,#8219,.T.);
#11200=ORIENTED_EDGE('',*,*,#8221,.T.);
#11201=ORIENTED_EDGE('',*,*,#8223,.T.);
#11202=ORIENTED_EDGE('',*,*,#8178,.T.);
#11203=ORIENTED_EDGE('',*,*,#8187,.T.);
#11204=ORIENTED_EDGE('',*,*,#8196,.T.);
#11205=ORIENTED_EDGE('',*,*,#8205,.T.);
#11206=ORIENTED_EDGE('',*,*,#8136,.T.);
#11207=ORIENTED_EDGE('',*,*,#8225,.T.);
#11208=ORIENTED_EDGE('',*,*,#8226,.T.);
#11209=ORIENTED_EDGE('',*,*,#8227,.T.);
#11210=ORIENTED_EDGE('',*,*,#8228,.F.);
#11211=ORIENTED_EDGE('',*,*,#8229,.T.);
#11212=ORIENTED_EDGE('',*,*,#8230,.T.);
#11213=ORIENTED_EDGE('',*,*,#8231,.T.);
#11214=ORIENTED_EDGE('',*,*,#8226,.F.);
#11215=ORIENTED_EDGE('',*,*,#8232,.T.);
#11216=ORIENTED_EDGE('',*,*,#8233,.T.);
#11217=ORIENTED_EDGE('',*,*,#8234,.T.);
#11218=ORIENTED_EDGE('',*,*,#8230,.F.);
#11219=ORIENTED_EDGE('',*,*,#8235,.T.);
#11220=ORIENTED_EDGE('',*,*,#8236,.T.);
#11221=ORIENTED_EDGE('',*,*,#8237,.T.);
#11222=ORIENTED_EDGE('',*,*,#8233,.F.);
#11223=ORIENTED_EDGE('',*,*,#8238,.T.);
#11224=ORIENTED_EDGE('',*,*,#8239,.T.);
#11225=ORIENTED_EDGE('',*,*,#8240,.T.);
#11226=ORIENTED_EDGE('',*,*,#8236,.F.);
#11227=ORIENTED_EDGE('',*,*,#8241,.T.);
#11228=ORIENTED_EDGE('',*,*,#8239,.F.);
#11229=ORIENTED_EDGE('',*,*,#8242,.T.);
#11230=ORIENTED_EDGE('',*,*,#8243,.T.);
#11231=ORIENTED_EDGE('',*,*,#8244,.T.);
#11232=ORIENTED_EDGE('',*,*,#8243,.F.);
#11233=ORIENTED_EDGE('',*,*,#8245,.T.);
#11234=ORIENTED_EDGE('',*,*,#8246,.T.);
#11235=ORIENTED_EDGE('',*,*,#8247,.T.);
#11236=ORIENTED_EDGE('',*,*,#8246,.F.);
#11237=ORIENTED_EDGE('',*,*,#8248,.T.);
#11238=ORIENTED_EDGE('',*,*,#8228,.T.);
#11239=ORIENTED_EDGE('',*,*,#8241,.F.);
#11240=ORIENTED_EDGE('',*,*,#8249,.F.);
#11241=ORIENTED_EDGE('',*,*,#8250,.F.);
#11242=ORIENTED_EDGE('',*,*,#8251,.T.);
#11243=ORIENTED_EDGE('',*,*,#8244,.F.);
#11244=ORIENTED_EDGE('',*,*,#8252,.F.);
#11245=ORIENTED_EDGE('',*,*,#8253,.F.);
#11246=ORIENTED_EDGE('',*,*,#8249,.T.);
#11247=ORIENTED_EDGE('',*,*,#8247,.F.);
#11248=ORIENTED_EDGE('',*,*,#8254,.F.);
#11249=ORIENTED_EDGE('',*,*,#8255,.F.);
#11250=ORIENTED_EDGE('',*,*,#8252,.T.);
#11251=ORIENTED_EDGE('',*,*,#8227,.F.);
#11252=ORIENTED_EDGE('',*,*,#8256,.F.);
#11253=ORIENTED_EDGE('',*,*,#8257,.F.);
#11254=ORIENTED_EDGE('',*,*,#8254,.T.);
#11255=ORIENTED_EDGE('',*,*,#8225,.F.);
#11256=ORIENTED_EDGE('',*,*,#8248,.F.);
#11257=ORIENTED_EDGE('',*,*,#8245,.F.);
#11258=ORIENTED_EDGE('',*,*,#8242,.F.);
#11259=ORIENTED_EDGE('',*,*,#8238,.F.);
#11260=ORIENTED_EDGE('',*,*,#8235,.F.);
#11261=ORIENTED_EDGE('',*,*,#8232,.F.);
#11262=ORIENTED_EDGE('',*,*,#8229,.F.);
#11263=ORIENTED_EDGE('',*,*,#8258,.T.);
#11264=ORIENTED_EDGE('',*,*,#8259,.T.);
#11265=ORIENTED_EDGE('',*,*,#8260,.T.);
#11266=ORIENTED_EDGE('',*,*,#8261,.T.);
#11267=ORIENTED_EDGE('',*,*,#8262,.T.);
#11268=ORIENTED_EDGE('',*,*,#8263,.T.);
#11269=ORIENTED_EDGE('',*,*,#8264,.T.);
#11270=ORIENTED_EDGE('',*,*,#8265,.T.);
#11271=ORIENTED_EDGE('',*,*,#8266,.T.);
#11272=ORIENTED_EDGE('',*,*,#8267,.T.);
#11273=ORIENTED_EDGE('',*,*,#8268,.T.);
#11274=ORIENTED_EDGE('',*,*,#8269,.T.);
#11275=ORIENTED_EDGE('',*,*,#8270,.T.);
#11276=ORIENTED_EDGE('',*,*,#8271,.T.);
#11277=ORIENTED_EDGE('',*,*,#8272,.T.);
#11278=ORIENTED_EDGE('',*,*,#8273,.T.);
#11279=ORIENTED_EDGE('',*,*,#8274,.T.);
#11280=ORIENTED_EDGE('',*,*,#8275,.T.);
#11281=ORIENTED_EDGE('',*,*,#8276,.T.);
#11282=ORIENTED_EDGE('',*,*,#8277,.T.);
#11283=ORIENTED_EDGE('',*,*,#8278,.T.);
#11284=ORIENTED_EDGE('',*,*,#8279,.T.);
#11285=ORIENTED_EDGE('',*,*,#8280,.T.);
#11286=ORIENTED_EDGE('',*,*,#8281,.F.);
#11287=ORIENTED_EDGE('',*,*,#8280,.F.);
#11288=ORIENTED_EDGE('',*,*,#8279,.F.);
#11289=ORIENTED_EDGE('',*,*,#8282,.T.);
#11290=ORIENTED_EDGE('',*,*,#8283,.T.);
#11291=ORIENTED_EDGE('',*,*,#8282,.F.);
#11292=ORIENTED_EDGE('',*,*,#8283,.F.);
#11293=ORIENTED_EDGE('',*,*,#8284,.T.);
#11294=ORIENTED_EDGE('',*,*,#8285,.T.);
#11295=ORIENTED_EDGE('',*,*,#8284,.F.);
#11296=ORIENTED_EDGE('',*,*,#8286,.T.);
#11297=ORIENTED_EDGE('',*,*,#8285,.F.);
#11298=ORIENTED_EDGE('',*,*,#8286,.F.);
#11299=ORIENTED_EDGE('',*,*,#8287,.T.);
#11300=ORIENTED_EDGE('',*,*,#8288,.F.);
#11301=ORIENTED_EDGE('',*,*,#8287,.F.);
#11302=ORIENTED_EDGE('',*,*,#8289,.T.);
#11303=ORIENTED_EDGE('',*,*,#8290,.T.);
#11304=ORIENTED_EDGE('',*,*,#8291,.F.);
#11305=ORIENTED_EDGE('',*,*,#8290,.F.);
#11306=ORIENTED_EDGE('',*,*,#8289,.F.);
#11307=ORIENTED_EDGE('',*,*,#8292,.T.);
#11308=ORIENTED_EDGE('',*,*,#8293,.T.);
#11309=ORIENTED_EDGE('',*,*,#8292,.F.);
#11310=ORIENTED_EDGE('',*,*,#8293,.F.);
#11311=ORIENTED_EDGE('',*,*,#8294,.T.);
#11312=ORIENTED_EDGE('',*,*,#8295,.T.);
#11313=ORIENTED_EDGE('',*,*,#8294,.F.);
#11314=ORIENTED_EDGE('',*,*,#8296,.T.);
#11315=ORIENTED_EDGE('',*,*,#8295,.F.);
#11316=ORIENTED_EDGE('',*,*,#8296,.F.);
#11317=ORIENTED_EDGE('',*,*,#8297,.T.);
#11318=ORIENTED_EDGE('',*,*,#8298,.F.);
#11319=ORIENTED_EDGE('',*,*,#8297,.F.);
#11320=ORIENTED_EDGE('',*,*,#8299,.T.);
#11321=ORIENTED_EDGE('',*,*,#8300,.T.);
#11322=ORIENTED_EDGE('',*,*,#8301,.F.);
#11323=ORIENTED_EDGE('',*,*,#8300,.F.);
#11324=ORIENTED_EDGE('',*,*,#8299,.F.);
#11325=ORIENTED_EDGE('',*,*,#8302,.T.);
#11326=ORIENTED_EDGE('',*,*,#8303,.T.);
#11327=ORIENTED_EDGE('',*,*,#8302,.F.);
#11328=ORIENTED_EDGE('',*,*,#8303,.F.);
#11329=ORIENTED_EDGE('',*,*,#8304,.T.);
#11330=ORIENTED_EDGE('',*,*,#8305,.T.);
#11331=ORIENTED_EDGE('',*,*,#8304,.F.);
#11332=ORIENTED_EDGE('',*,*,#8306,.T.);
#11333=ORIENTED_EDGE('',*,*,#8305,.F.);
#11334=ORIENTED_EDGE('',*,*,#8306,.F.);
#11335=ORIENTED_EDGE('',*,*,#8307,.T.);
#11336=ORIENTED_EDGE('',*,*,#8308,.F.);
#11337=ORIENTED_EDGE('',*,*,#8307,.F.);
#11338=ORIENTED_EDGE('',*,*,#8309,.T.);
#11339=ORIENTED_EDGE('',*,*,#8310,.T.);
#11340=ORIENTED_EDGE('',*,*,#8311,.F.);
#11341=ORIENTED_EDGE('',*,*,#8310,.F.);
#11342=ORIENTED_EDGE('',*,*,#8309,.F.);
#11343=ORIENTED_EDGE('',*,*,#8312,.T.);
#11344=ORIENTED_EDGE('',*,*,#8313,.T.);
#11345=ORIENTED_EDGE('',*,*,#8312,.F.);
#11346=ORIENTED_EDGE('',*,*,#8313,.F.);
#11347=ORIENTED_EDGE('',*,*,#8314,.T.);
#11348=ORIENTED_EDGE('',*,*,#8315,.T.);
#11349=ORIENTED_EDGE('',*,*,#8314,.F.);
#11350=ORIENTED_EDGE('',*,*,#8316,.T.);
#11351=ORIENTED_EDGE('',*,*,#8315,.F.);
#11352=ORIENTED_EDGE('',*,*,#8316,.F.);
#11353=ORIENTED_EDGE('',*,*,#8317,.T.);
#11354=ORIENTED_EDGE('',*,*,#8318,.F.);
#11355=ORIENTED_EDGE('',*,*,#8317,.F.);
#11356=ORIENTED_EDGE('',*,*,#8319,.T.);
#11357=ORIENTED_EDGE('',*,*,#8320,.T.);
#11358=ORIENTED_EDGE('',*,*,#8321,.F.);
#11359=ORIENTED_EDGE('',*,*,#8320,.F.);
#11360=ORIENTED_EDGE('',*,*,#8319,.F.);
#11361=ORIENTED_EDGE('',*,*,#8322,.T.);
#11362=ORIENTED_EDGE('',*,*,#8323,.T.);
#11363=ORIENTED_EDGE('',*,*,#8322,.F.);
#11364=ORIENTED_EDGE('',*,*,#8323,.F.);
#11365=ORIENTED_EDGE('',*,*,#8324,.T.);
#11366=ORIENTED_EDGE('',*,*,#8258,.F.);
#11367=ORIENTED_EDGE('',*,*,#8324,.F.);
#11368=ORIENTED_EDGE('',*,*,#8325,.T.);
#11369=ORIENTED_EDGE('',*,*,#8326,.T.);
#11370=ORIENTED_EDGE('',*,*,#8327,.F.);
#11371=ORIENTED_EDGE('',*,*,#8326,.F.);
#11372=ORIENTED_EDGE('',*,*,#8325,.F.);
#11373=ORIENTED_EDGE('',*,*,#8328,.T.);
#11374=ORIENTED_EDGE('',*,*,#8329,.T.);
#11375=ORIENTED_EDGE('',*,*,#8328,.F.);
#11376=ORIENTED_EDGE('',*,*,#8329,.F.);
#11377=ORIENTED_EDGE('',*,*,#8330,.T.);
#11378=ORIENTED_EDGE('',*,*,#8278,.F.);
#11379=ORIENTED_EDGE('',*,*,#8330,.F.);
#11380=ORIENTED_EDGE('',*,*,#8331,.T.);
#11381=ORIENTED_EDGE('',*,*,#8332,.T.);
#11382=ORIENTED_EDGE('',*,*,#8333,.F.);
#11383=ORIENTED_EDGE('',*,*,#8332,.F.);
#11384=ORIENTED_EDGE('',*,*,#8331,.F.);
#11385=ORIENTED_EDGE('',*,*,#8334,.T.);
#11386=ORIENTED_EDGE('',*,*,#8335,.T.);
#11387=ORIENTED_EDGE('',*,*,#8334,.F.);
#11388=ORIENTED_EDGE('',*,*,#8335,.F.);
#11389=ORIENTED_EDGE('',*,*,#8336,.T.);
#11390=ORIENTED_EDGE('',*,*,#8277,.F.);
#11391=ORIENTED_EDGE('',*,*,#8336,.F.);
#11392=ORIENTED_EDGE('',*,*,#8337,.T.);
#11393=ORIENTED_EDGE('',*,*,#8338,.T.);
#11394=ORIENTED_EDGE('',*,*,#8339,.F.);
#11395=ORIENTED_EDGE('',*,*,#8338,.F.);
#11396=ORIENTED_EDGE('',*,*,#8337,.F.);
#11397=ORIENTED_EDGE('',*,*,#8340,.T.);
#11398=ORIENTED_EDGE('',*,*,#8341,.T.);
#11399=ORIENTED_EDGE('',*,*,#8340,.F.);
#11400=ORIENTED_EDGE('',*,*,#8341,.F.);
#11401=ORIENTED_EDGE('',*,*,#8342,.T.);
#11402=ORIENTED_EDGE('',*,*,#8276,.F.);
#11403=ORIENTED_EDGE('',*,*,#8342,.F.);
#11404=ORIENTED_EDGE('',*,*,#8343,.F.);
#11405=ORIENTED_EDGE('',*,*,#8344,.T.);
#11406=ORIENTED_EDGE('',*,*,#8259,.F.);
#11407=ORIENTED_EDGE('',*,*,#8345,.F.);
#11408=ORIENTED_EDGE('',*,*,#8346,.F.);
#11409=ORIENTED_EDGE('',*,*,#8347,.T.);
#11410=ORIENTED_EDGE('',*,*,#8260,.F.);
#11411=ORIENTED_EDGE('',*,*,#8344,.F.);
#11412=ORIENTED_EDGE('',*,*,#8348,.F.);
#11413=ORIENTED_EDGE('',*,*,#8349,.T.);
#11414=ORIENTED_EDGE('',*,*,#8261,.F.);
#11415=ORIENTED_EDGE('',*,*,#8347,.F.);
#11416=ORIENTED_EDGE('',*,*,#8350,.F.);
#11417=ORIENTED_EDGE('',*,*,#8345,.T.);
#11418=ORIENTED_EDGE('',*,*,#8262,.F.);
#11419=ORIENTED_EDGE('',*,*,#8349,.F.);
#11420=ORIENTED_EDGE('',*,*,#8351,.F.);
#11421=ORIENTED_EDGE('',*,*,#8352,.T.);
#11422=ORIENTED_EDGE('',*,*,#8263,.F.);
#11423=ORIENTED_EDGE('',*,*,#8353,.F.);
#11424=ORIENTED_EDGE('',*,*,#8354,.F.);
#11425=ORIENTED_EDGE('',*,*,#8355,.T.);
#11426=ORIENTED_EDGE('',*,*,#8264,.F.);
#11427=ORIENTED_EDGE('',*,*,#8352,.F.);
#11428=ORIENTED_EDGE('',*,*,#8356,.F.);
#11429=ORIENTED_EDGE('',*,*,#8357,.T.);
#11430=ORIENTED_EDGE('',*,*,#8265,.F.);
#11431=ORIENTED_EDGE('',*,*,#8355,.F.);
#11432=ORIENTED_EDGE('',*,*,#8358,.F.);
#11433=ORIENTED_EDGE('',*,*,#8353,.T.);
#11434=ORIENTED_EDGE('',*,*,#8266,.F.);
#11435=ORIENTED_EDGE('',*,*,#8357,.F.);
#11436=ORIENTED_EDGE('',*,*,#8359,.F.);
#11437=ORIENTED_EDGE('',*,*,#8360,.T.);
#11438=ORIENTED_EDGE('',*,*,#8267,.F.);
#11439=ORIENTED_EDGE('',*,*,#8361,.F.);
#11440=ORIENTED_EDGE('',*,*,#8362,.F.);
#11441=ORIENTED_EDGE('',*,*,#8363,.T.);
#11442=ORIENTED_EDGE('',*,*,#8268,.F.);
#11443=ORIENTED_EDGE('',*,*,#8360,.F.);
#11444=ORIENTED_EDGE('',*,*,#8364,.F.);
#11445=ORIENTED_EDGE('',*,*,#8365,.T.);
#11446=ORIENTED_EDGE('',*,*,#8269,.F.);
#11447=ORIENTED_EDGE('',*,*,#8363,.F.);
#11448=ORIENTED_EDGE('',*,*,#8366,.F.);
#11449=ORIENTED_EDGE('',*,*,#8361,.T.);
#11450=ORIENTED_EDGE('',*,*,#8270,.F.);
#11451=ORIENTED_EDGE('',*,*,#8365,.F.);
#11452=ORIENTED_EDGE('',*,*,#8367,.F.);
#11453=ORIENTED_EDGE('',*,*,#8368,.T.);
#11454=ORIENTED_EDGE('',*,*,#8271,.F.);
#11455=ORIENTED_EDGE('',*,*,#8369,.F.);
#11456=ORIENTED_EDGE('',*,*,#8370,.F.);
#11457=ORIENTED_EDGE('',*,*,#8371,.T.);
#11458=ORIENTED_EDGE('',*,*,#8272,.F.);
#11459=ORIENTED_EDGE('',*,*,#8368,.F.);
#11460=ORIENTED_EDGE('',*,*,#8372,.F.);
#11461=ORIENTED_EDGE('',*,*,#8373,.T.);
#11462=ORIENTED_EDGE('',*,*,#8273,.F.);
#11463=ORIENTED_EDGE('',*,*,#8371,.F.);
#11464=ORIENTED_EDGE('',*,*,#8374,.F.);
#11465=ORIENTED_EDGE('',*,*,#8369,.T.);
#11466=ORIENTED_EDGE('',*,*,#8274,.F.);
#11467=ORIENTED_EDGE('',*,*,#8373,.F.);
#11468=ORIENTED_EDGE('',*,*,#8375,.F.);
#11469=ORIENTED_EDGE('',*,*,#8376,.T.);
#11470=ORIENTED_EDGE('',*,*,#8377,.F.);
#11471=ORIENTED_EDGE('',*,*,#8376,.F.);
#11472=ORIENTED_EDGE('',*,*,#8275,.F.);
#11473=ORIENTED_EDGE('',*,*,#8378,.T.);
#11474=ORIENTED_EDGE('',*,*,#8379,.T.);
#11475=ORIENTED_EDGE('',*,*,#8378,.F.);
#11476=ORIENTED_EDGE('',*,*,#8379,.F.);
#11477=ORIENTED_EDGE('',*,*,#8288,.T.);
#11478=ORIENTED_EDGE('',*,*,#8298,.T.);
#11479=ORIENTED_EDGE('',*,*,#8308,.T.);
#11480=ORIENTED_EDGE('',*,*,#8318,.T.);
#11481=ORIENTED_EDGE('',*,*,#8377,.T.);
#11482=ORIENTED_EDGE('',*,*,#8231,.F.);
#11483=ORIENTED_EDGE('',*,*,#8380,.F.);
#11484=ORIENTED_EDGE('',*,*,#8381,.F.);
#11485=ORIENTED_EDGE('',*,*,#8256,.T.);
#11486=ORIENTED_EDGE('',*,*,#8234,.F.);
#11487=ORIENTED_EDGE('',*,*,#8382,.F.);
#11488=ORIENTED_EDGE('',*,*,#8383,.F.);
#11489=ORIENTED_EDGE('',*,*,#8380,.T.);
#11490=ORIENTED_EDGE('',*,*,#8237,.F.);
#11491=ORIENTED_EDGE('',*,*,#8384,.F.);
#11492=ORIENTED_EDGE('',*,*,#8385,.F.);
#11493=ORIENTED_EDGE('',*,*,#8382,.T.);
#11494=ORIENTED_EDGE('',*,*,#8240,.F.);
#11495=ORIENTED_EDGE('',*,*,#8251,.F.);
#11496=ORIENTED_EDGE('',*,*,#8386,.F.);
#11497=ORIENTED_EDGE('',*,*,#8384,.T.);
#11498=ORIENTED_EDGE('',*,*,#8386,.T.);
#11499=ORIENTED_EDGE('',*,*,#8250,.T.);
#11500=ORIENTED_EDGE('',*,*,#8253,.T.);
#11501=ORIENTED_EDGE('',*,*,#8255,.T.);
#11502=ORIENTED_EDGE('',*,*,#8257,.T.);
#11503=ORIENTED_EDGE('',*,*,#8381,.T.);
#11504=ORIENTED_EDGE('',*,*,#8383,.T.);
#11505=ORIENTED_EDGE('',*,*,#8385,.T.);
#11506=ORIENTED_EDGE('',*,*,#8291,.T.);
#11507=ORIENTED_EDGE('',*,*,#8311,.T.);
#11508=ORIENTED_EDGE('',*,*,#8327,.T.);
#11509=ORIENTED_EDGE('',*,*,#8333,.T.);
#11510=ORIENTED_EDGE('',*,*,#8339,.T.);
#11511=ORIENTED_EDGE('',*,*,#8375,.T.);
#11512=ORIENTED_EDGE('',*,*,#8367,.T.);
#11513=ORIENTED_EDGE('',*,*,#8374,.T.);
#11514=ORIENTED_EDGE('',*,*,#8372,.T.);
#11515=ORIENTED_EDGE('',*,*,#8370,.T.);
#11516=ORIENTED_EDGE('',*,*,#8359,.T.);
#11517=ORIENTED_EDGE('',*,*,#8366,.T.);
#11518=ORIENTED_EDGE('',*,*,#8364,.T.);
#11519=ORIENTED_EDGE('',*,*,#8362,.T.);
#11520=ORIENTED_EDGE('',*,*,#8351,.T.);
#11521=ORIENTED_EDGE('',*,*,#8358,.T.);
#11522=ORIENTED_EDGE('',*,*,#8356,.T.);
#11523=ORIENTED_EDGE('',*,*,#8354,.T.);
#11524=ORIENTED_EDGE('',*,*,#8343,.T.);
#11525=ORIENTED_EDGE('',*,*,#8350,.T.);
#11526=ORIENTED_EDGE('',*,*,#8348,.T.);
#11527=ORIENTED_EDGE('',*,*,#8346,.T.);
#11528=ORIENTED_EDGE('',*,*,#8321,.T.);
#11529=ORIENTED_EDGE('',*,*,#8301,.T.);
#11530=ORIENTED_EDGE('',*,*,#8281,.T.);
#11531=ORIENTED_EDGE('',*,*,#8387,.F.);
#11532=ORIENTED_EDGE('',*,*,#8388,.T.);
#11533=ORIENTED_EDGE('',*,*,#8389,.T.);
#11534=ORIENTED_EDGE('',*,*,#8390,.T.);
#11535=ORIENTED_EDGE('',*,*,#8391,.T.);
#11536=ORIENTED_EDGE('',*,*,#8392,.F.);
#11537=ORIENTED_EDGE('',*,*,#8393,.T.);
#11538=ORIENTED_EDGE('',*,*,#8387,.T.);
#11539=ORIENTED_EDGE('',*,*,#8394,.T.);
#11540=ORIENTED_EDGE('',*,*,#8395,.F.);
#11541=ORIENTED_EDGE('',*,*,#8396,.T.);
#11542=ORIENTED_EDGE('',*,*,#8392,.T.);
#11543=ORIENTED_EDGE('',*,*,#8397,.T.);
#11544=ORIENTED_EDGE('',*,*,#8398,.F.);
#11545=ORIENTED_EDGE('',*,*,#8399,.T.);
#11546=ORIENTED_EDGE('',*,*,#8395,.T.);
#11547=ORIENTED_EDGE('',*,*,#8400,.T.);
#11548=ORIENTED_EDGE('',*,*,#8401,.F.);
#11549=ORIENTED_EDGE('',*,*,#8402,.T.);
#11550=ORIENTED_EDGE('',*,*,#8398,.T.);
#11551=ORIENTED_EDGE('',*,*,#8403,.T.);
#11552=ORIENTED_EDGE('',*,*,#8404,.F.);
#11553=ORIENTED_EDGE('',*,*,#8405,.T.);
#11554=ORIENTED_EDGE('',*,*,#8401,.T.);
#11555=ORIENTED_EDGE('',*,*,#8406,.T.);
#11556=ORIENTED_EDGE('',*,*,#8404,.T.);
#11557=ORIENTED_EDGE('',*,*,#8407,.T.);
#11558=ORIENTED_EDGE('',*,*,#8408,.T.);
#11559=ORIENTED_EDGE('',*,*,#8409,.T.);
#11560=ORIENTED_EDGE('',*,*,#8410,.T.);
#11561=ORIENTED_EDGE('',*,*,#8411,.F.);
#11562=ORIENTED_EDGE('',*,*,#8412,.T.);
#11563=ORIENTED_EDGE('',*,*,#8413,.F.);
#11564=ORIENTED_EDGE('',*,*,#8414,.F.);
#11565=ORIENTED_EDGE('',*,*,#8415,.F.);
#11566=ORIENTED_EDGE('',*,*,#8416,.F.);
#11567=ORIENTED_EDGE('',*,*,#8413,.T.);
#11568=ORIENTED_EDGE('',*,*,#8417,.T.);
#11569=ORIENTED_EDGE('',*,*,#8418,.F.);
#11570=ORIENTED_EDGE('',*,*,#8419,.F.);
#11571=ORIENTED_EDGE('',*,*,#8420,.F.);
#11572=ORIENTED_EDGE('',*,*,#8421,.F.);
#11573=ORIENTED_EDGE('',*,*,#8418,.T.);
#11574=ORIENTED_EDGE('',*,*,#8422,.T.);
#11575=ORIENTED_EDGE('',*,*,#8423,.F.);
#11576=ORIENTED_EDGE('',*,*,#8422,.F.);
#11577=ORIENTED_EDGE('',*,*,#8417,.F.);
#11578=ORIENTED_EDGE('',*,*,#8412,.F.);
#11579=ORIENTED_EDGE('',*,*,#8424,.F.);
#11580=ORIENTED_EDGE('',*,*,#8425,.T.);
#11581=ORIENTED_EDGE('',*,*,#8426,.T.);
#11582=ORIENTED_EDGE('',*,*,#8414,.T.);
#11583=ORIENTED_EDGE('',*,*,#8416,.T.);
#11584=ORIENTED_EDGE('',*,*,#8421,.T.);
#11585=ORIENTED_EDGE('',*,*,#8427,.T.);
#11586=ORIENTED_EDGE('',*,*,#8425,.F.);
#11587=ORIENTED_EDGE('',*,*,#8415,.T.);
#11588=ORIENTED_EDGE('',*,*,#8426,.F.);
#11589=ORIENTED_EDGE('',*,*,#8427,.F.);
#11590=ORIENTED_EDGE('',*,*,#8420,.T.);
#11591=ORIENTED_EDGE('',*,*,#8428,.F.);
#11592=ORIENTED_EDGE('',*,*,#8429,.T.);
#11593=ORIENTED_EDGE('',*,*,#8424,.T.);
#11594=ORIENTED_EDGE('',*,*,#8429,.F.);
#11595=ORIENTED_EDGE('',*,*,#8430,.F.);
#11596=ORIENTED_EDGE('',*,*,#8431,.T.);
#11597=ORIENTED_EDGE('',*,*,#8432,.T.);
#11598=ORIENTED_EDGE('',*,*,#8431,.F.);
#11599=ORIENTED_EDGE('',*,*,#8433,.F.);
#11600=ORIENTED_EDGE('',*,*,#8434,.F.);
#11601=ORIENTED_EDGE('',*,*,#8408,.F.);
#11602=ORIENTED_EDGE('',*,*,#8435,.F.);
#11603=ORIENTED_EDGE('',*,*,#8436,.F.);
#11604=ORIENTED_EDGE('',*,*,#8437,.F.);
#11605=ORIENTED_EDGE('',*,*,#8438,.T.);
#11606=ORIENTED_EDGE('',*,*,#8432,.F.);
#11607=ORIENTED_EDGE('',*,*,#8438,.F.);
#11608=ORIENTED_EDGE('',*,*,#8389,.F.);
#11609=ORIENTED_EDGE('',*,*,#8439,.F.);
#11610=ORIENTED_EDGE('',*,*,#8440,.F.);
#11611=ORIENTED_EDGE('',*,*,#8441,.F.);
#11612=ORIENTED_EDGE('',*,*,#8442,.F.);
#11613=ORIENTED_EDGE('',*,*,#8443,.T.);
#11614=ORIENTED_EDGE('',*,*,#8444,.T.);
#11615=ORIENTED_EDGE('',*,*,#8443,.F.);
#11616=ORIENTED_EDGE('',*,*,#8444,.F.);
#11617=ORIENTED_EDGE('',*,*,#8445,.T.);
#11618=ORIENTED_EDGE('',*,*,#8446,.T.);
#11619=ORIENTED_EDGE('',*,*,#8445,.F.);
#11620=ORIENTED_EDGE('',*,*,#8436,.T.);
#11621=ORIENTED_EDGE('',*,*,#8447,.T.);
#11622=ORIENTED_EDGE('',*,*,#8440,.T.);
#11623=ORIENTED_EDGE('',*,*,#8448,.F.);
#11624=ORIENTED_EDGE('',*,*,#8433,.T.);
#11625=ORIENTED_EDGE('',*,*,#8437,.T.);
#11626=ORIENTED_EDGE('',*,*,#8448,.T.);
#11627=ORIENTED_EDGE('',*,*,#8439,.T.);
#11628=ORIENTED_EDGE('',*,*,#8388,.F.);
#11629=ORIENTED_EDGE('',*,*,#8393,.F.);
#11630=ORIENTED_EDGE('',*,*,#8396,.F.);
#11631=ORIENTED_EDGE('',*,*,#8399,.F.);
#11632=ORIENTED_EDGE('',*,*,#8402,.F.);
#11633=ORIENTED_EDGE('',*,*,#8405,.F.);
#11634=ORIENTED_EDGE('',*,*,#8410,.F.);
#11635=ORIENTED_EDGE('',*,*,#8449,.T.);
#11636=ORIENTED_EDGE('',*,*,#8434,.T.);
#11637=ORIENTED_EDGE('',*,*,#8449,.F.);
#11638=ORIENTED_EDGE('',*,*,#8409,.F.);
#11639=ORIENTED_EDGE('',*,*,#8435,.T.);
#11640=ORIENTED_EDGE('',*,*,#8407,.F.);
#11641=ORIENTED_EDGE('',*,*,#8406,.F.);
#11642=ORIENTED_EDGE('',*,*,#8403,.F.);
#11643=ORIENTED_EDGE('',*,*,#8400,.F.);
#11644=ORIENTED_EDGE('',*,*,#8397,.F.);
#11645=ORIENTED_EDGE('',*,*,#8394,.F.);
#11646=ORIENTED_EDGE('',*,*,#8391,.F.);
#11647=ORIENTED_EDGE('',*,*,#8450,.F.);
#11648=ORIENTED_EDGE('',*,*,#8441,.T.);
#11649=ORIENTED_EDGE('',*,*,#8447,.F.);
#11650=ORIENTED_EDGE('',*,*,#8442,.T.);
#11651=ORIENTED_EDGE('',*,*,#8450,.T.);
#11652=ORIENTED_EDGE('',*,*,#8390,.F.);
#11653=ORIENTED_EDGE('',*,*,#8451,.F.);
#11654=ORIENTED_EDGE('',*,*,#8452,.F.);
#11655=ORIENTED_EDGE('',*,*,#8453,.T.);
#11656=ORIENTED_EDGE('',*,*,#8451,.T.);
#11657=ORIENTED_EDGE('',*,*,#8453,.F.);
#11658=ORIENTED_EDGE('',*,*,#8454,.F.);
#11659=ORIENTED_EDGE('',*,*,#8455,.T.);
#11660=ORIENTED_EDGE('',*,*,#8452,.T.);
#11661=ORIENTED_EDGE('',*,*,#8455,.F.);
#11662=ORIENTED_EDGE('',*,*,#8456,.F.);
#11663=ORIENTED_EDGE('',*,*,#8454,.T.);
#11664=ORIENTED_EDGE('',*,*,#8457,.F.);
#11665=ORIENTED_EDGE('',*,*,#8458,.T.);
#11666=ORIENTED_EDGE('',*,*,#8456,.T.);
#11667=ORIENTED_EDGE('',*,*,#8458,.F.);
#11668=ORIENTED_EDGE('',*,*,#8459,.F.);
#11669=ORIENTED_EDGE('',*,*,#8460,.T.);
#11670=ORIENTED_EDGE('',*,*,#8457,.T.);
#11671=ORIENTED_EDGE('',*,*,#8460,.F.);
#11672=ORIENTED_EDGE('',*,*,#8459,.T.);
#11673=ORIENTED_EDGE('',*,*,#8446,.F.);
#11674=ORIENTED_EDGE('',*,*,#8461,.F.);
#11675=ORIENTED_EDGE('',*,*,#8430,.T.);
#11676=ORIENTED_EDGE('',*,*,#8462,.F.);
#11677=ORIENTED_EDGE('',*,*,#8463,.T.);
#11678=ORIENTED_EDGE('',*,*,#8461,.T.);
#11679=ORIENTED_EDGE('',*,*,#8463,.F.);
#11680=ORIENTED_EDGE('',*,*,#8462,.T.);
#11681=ORIENTED_EDGE('',*,*,#8464,.T.);
#11682=ORIENTED_EDGE('',*,*,#8465,.F.);
#11683=ORIENTED_EDGE('',*,*,#8464,.F.);
#11684=ORIENTED_EDGE('',*,*,#8465,.T.);
#11685=ORIENTED_EDGE('',*,*,#8466,.F.);
#11686=ORIENTED_EDGE('',*,*,#8467,.F.);
#11687=ORIENTED_EDGE('',*,*,#8468,.T.);
#11688=ORIENTED_EDGE('',*,*,#8466,.T.);
#11689=ORIENTED_EDGE('',*,*,#8468,.F.);
#11690=ORIENTED_EDGE('',*,*,#8467,.T.);
#11691=ORIENTED_EDGE('',*,*,#8469,.T.);
#11692=ORIENTED_EDGE('',*,*,#8470,.F.);
#11693=ORIENTED_EDGE('',*,*,#8469,.F.);
#11694=ORIENTED_EDGE('',*,*,#8470,.T.);
#11695=ORIENTED_EDGE('',*,*,#8411,.T.);
#11696=ORIENTED_EDGE('',*,*,#8428,.T.);
#11697=ORIENTED_EDGE('',*,*,#8419,.T.);
#11698=ORIENTED_EDGE('',*,*,#8423,.T.);
#11699=ORIENTED_EDGE('',*,*,#8471,.T.);
#11700=ORIENTED_EDGE('',*,*,#8472,.T.);
#11701=ORIENTED_EDGE('',*,*,#8473,.T.);
#11702=ORIENTED_EDGE('',*,*,#8472,.F.);
#11703=ORIENTED_EDGE('',*,*,#8474,.T.);
#11704=ORIENTED_EDGE('',*,*,#8471,.F.);
#11705=ORIENTED_EDGE('',*,*,#8475,.T.);
#11706=ORIENTED_EDGE('',*,*,#8476,.F.);
#11707=ORIENTED_EDGE('',*,*,#8477,.F.);
#11708=ORIENTED_EDGE('',*,*,#8475,.F.);
#11709=ORIENTED_EDGE('',*,*,#8474,.F.);
#11710=ORIENTED_EDGE('',*,*,#8478,.T.);
#11711=ORIENTED_EDGE('',*,*,#8479,.F.);
#11712=ORIENTED_EDGE('',*,*,#8480,.T.);
#11713=ORIENTED_EDGE('',*,*,#8481,.T.);
#11714=ORIENTED_EDGE('',*,*,#8482,.T.);
#11715=ORIENTED_EDGE('',*,*,#8483,.F.);
#11716=ORIENTED_EDGE('',*,*,#8484,.T.);
#11717=ORIENTED_EDGE('',*,*,#8485,.T.);
#11718=ORIENTED_EDGE('',*,*,#8486,.T.);
#11719=ORIENTED_EDGE('',*,*,#8487,.F.);
#11720=ORIENTED_EDGE('',*,*,#8488,.T.);
#11721=ORIENTED_EDGE('',*,*,#8489,.T.);
#11722=ORIENTED_EDGE('',*,*,#8490,.T.);
#11723=ORIENTED_EDGE('',*,*,#8491,.F.);
#11724=ORIENTED_EDGE('',*,*,#8492,.T.);
#11725=ORIENTED_EDGE('',*,*,#8493,.T.);
#11726=ORIENTED_EDGE('',*,*,#8494,.T.);
#11727=ORIENTED_EDGE('',*,*,#8495,.F.);
#11728=ORIENTED_EDGE('',*,*,#8496,.T.);
#11729=ORIENTED_EDGE('',*,*,#8497,.T.);
#11730=ORIENTED_EDGE('',*,*,#8498,.T.);
#11731=ORIENTED_EDGE('',*,*,#8499,.F.);
#11732=ORIENTED_EDGE('',*,*,#8500,.T.);
#11733=ORIENTED_EDGE('',*,*,#8501,.T.);
#11734=ORIENTED_EDGE('',*,*,#8502,.T.);
#11735=ORIENTED_EDGE('',*,*,#8503,.F.);
#11736=ORIENTED_EDGE('',*,*,#8504,.T.);
#11737=ORIENTED_EDGE('',*,*,#8505,.T.);
#11738=ORIENTED_EDGE('',*,*,#8506,.T.);
#11739=ORIENTED_EDGE('',*,*,#8507,.F.);
#11740=ORIENTED_EDGE('',*,*,#8508,.T.);
#11741=ORIENTED_EDGE('',*,*,#8509,.T.);
#11742=ORIENTED_EDGE('',*,*,#8510,.T.);
#11743=ORIENTED_EDGE('',*,*,#8511,.F.);
#11744=ORIENTED_EDGE('',*,*,#8512,.T.);
#11745=ORIENTED_EDGE('',*,*,#8513,.T.);
#11746=ORIENTED_EDGE('',*,*,#8514,.T.);
#11747=ORIENTED_EDGE('',*,*,#8515,.F.);
#11748=ORIENTED_EDGE('',*,*,#8516,.T.);
#11749=ORIENTED_EDGE('',*,*,#8517,.T.);
#11750=ORIENTED_EDGE('',*,*,#8518,.T.);
#11751=ORIENTED_EDGE('',*,*,#8519,.F.);
#11752=ORIENTED_EDGE('',*,*,#8520,.T.);
#11753=ORIENTED_EDGE('',*,*,#8521,.T.);
#11754=ORIENTED_EDGE('',*,*,#8522,.T.);
#11755=ORIENTED_EDGE('',*,*,#8523,.F.);
#11756=ORIENTED_EDGE('',*,*,#8524,.T.);
#11757=ORIENTED_EDGE('',*,*,#8525,.T.);
#11758=ORIENTED_EDGE('',*,*,#8526,.T.);
#11759=ORIENTED_EDGE('',*,*,#8527,.F.);
#11760=ORIENTED_EDGE('',*,*,#8528,.T.);
#11761=ORIENTED_EDGE('',*,*,#8529,.T.);
#11762=ORIENTED_EDGE('',*,*,#8530,.T.);
#11763=ORIENTED_EDGE('',*,*,#8531,.F.);
#11764=ORIENTED_EDGE('',*,*,#8532,.T.);
#11765=ORIENTED_EDGE('',*,*,#8533,.T.);
#11766=ORIENTED_EDGE('',*,*,#8534,.T.);
#11767=ORIENTED_EDGE('',*,*,#8535,.F.);
#11768=ORIENTED_EDGE('',*,*,#8536,.T.);
#11769=ORIENTED_EDGE('',*,*,#8537,.T.);
#11770=ORIENTED_EDGE('',*,*,#8538,.T.);
#11771=ORIENTED_EDGE('',*,*,#8539,.F.);
#11772=ORIENTED_EDGE('',*,*,#8540,.T.);
#11773=ORIENTED_EDGE('',*,*,#8541,.T.);
#11774=ORIENTED_EDGE('',*,*,#8542,.T.);
#11775=ORIENTED_EDGE('',*,*,#8543,.F.);
#11776=ORIENTED_EDGE('',*,*,#8544,.T.);
#11777=ORIENTED_EDGE('',*,*,#8545,.T.);
#11778=ORIENTED_EDGE('',*,*,#8546,.T.);
#11779=ORIENTED_EDGE('',*,*,#8547,.F.);
#11780=ORIENTED_EDGE('',*,*,#8548,.T.);
#11781=ORIENTED_EDGE('',*,*,#8549,.T.);
#11782=ORIENTED_EDGE('',*,*,#8550,.T.);
#11783=ORIENTED_EDGE('',*,*,#8551,.F.);
#11784=ORIENTED_EDGE('',*,*,#8552,.T.);
#11785=ORIENTED_EDGE('',*,*,#8553,.T.);
#11786=ORIENTED_EDGE('',*,*,#8554,.T.);
#11787=ORIENTED_EDGE('',*,*,#8555,.F.);
#11788=ORIENTED_EDGE('',*,*,#8556,.T.);
#11789=ORIENTED_EDGE('',*,*,#8557,.T.);
#11790=ORIENTED_EDGE('',*,*,#8558,.T.);
#11791=ORIENTED_EDGE('',*,*,#8559,.F.);
#11792=ORIENTED_EDGE('',*,*,#8560,.T.);
#11793=ORIENTED_EDGE('',*,*,#8561,.T.);
#11794=ORIENTED_EDGE('',*,*,#8562,.T.);
#11795=ORIENTED_EDGE('',*,*,#8563,.F.);
#11796=ORIENTED_EDGE('',*,*,#8564,.T.);
#11797=ORIENTED_EDGE('',*,*,#8565,.T.);
#11798=ORIENTED_EDGE('',*,*,#8566,.T.);
#11799=ORIENTED_EDGE('',*,*,#8567,.F.);
#11800=ORIENTED_EDGE('',*,*,#8568,.T.);
#11801=ORIENTED_EDGE('',*,*,#8569,.T.);
#11802=ORIENTED_EDGE('',*,*,#8570,.T.);
#11803=ORIENTED_EDGE('',*,*,#8571,.F.);
#11804=ORIENTED_EDGE('',*,*,#8572,.T.);
#11805=ORIENTED_EDGE('',*,*,#8573,.T.);
#11806=ORIENTED_EDGE('',*,*,#8574,.T.);
#11807=ORIENTED_EDGE('',*,*,#8575,.F.);
#11808=ORIENTED_EDGE('',*,*,#8576,.T.);
#11809=ORIENTED_EDGE('',*,*,#8577,.T.);
#11810=ORIENTED_EDGE('',*,*,#8578,.T.);
#11811=ORIENTED_EDGE('',*,*,#8579,.F.);
#11812=ORIENTED_EDGE('',*,*,#8580,.T.);
#11813=ORIENTED_EDGE('',*,*,#8581,.T.);
#11814=ORIENTED_EDGE('',*,*,#8582,.T.);
#11815=ORIENTED_EDGE('',*,*,#8583,.F.);
#11816=ORIENTED_EDGE('',*,*,#8584,.T.);
#11817=ORIENTED_EDGE('',*,*,#8585,.T.);
#11818=ORIENTED_EDGE('',*,*,#8586,.T.);
#11819=ORIENTED_EDGE('',*,*,#8587,.F.);
#11820=ORIENTED_EDGE('',*,*,#8588,.T.);
#11821=ORIENTED_EDGE('',*,*,#8589,.T.);
#11822=ORIENTED_EDGE('',*,*,#8590,.T.);
#11823=ORIENTED_EDGE('',*,*,#8591,.F.);
#11824=ORIENTED_EDGE('',*,*,#8592,.T.);
#11825=ORIENTED_EDGE('',*,*,#8593,.T.);
#11826=ORIENTED_EDGE('',*,*,#8594,.T.);
#11827=ORIENTED_EDGE('',*,*,#8595,.F.);
#11828=ORIENTED_EDGE('',*,*,#8596,.T.);
#11829=ORIENTED_EDGE('',*,*,#8597,.T.);
#11830=ORIENTED_EDGE('',*,*,#8473,.F.);
#11831=ORIENTED_EDGE('',*,*,#8476,.T.);
#11832=ORIENTED_EDGE('',*,*,#8477,.T.);
#11833=ORIENTED_EDGE('',*,*,#8598,.T.);
#11834=ORIENTED_EDGE('',*,*,#8599,.T.);
#11835=ORIENTED_EDGE('',*,*,#8598,.F.);
#11836=ORIENTED_EDGE('',*,*,#8600,.T.);
#11837=ORIENTED_EDGE('',*,*,#8601,.T.);
#11838=ORIENTED_EDGE('',*,*,#8602,.T.);
#11839=ORIENTED_EDGE('',*,*,#8603,.T.);
#11840=ORIENTED_EDGE('',*,*,#8604,.T.);
#11841=ORIENTED_EDGE('',*,*,#8605,.T.);
#11842=ORIENTED_EDGE('',*,*,#8606,.T.);
#11843=ORIENTED_EDGE('',*,*,#8607,.T.);
#11844=ORIENTED_EDGE('',*,*,#8608,.T.);
#11845=ORIENTED_EDGE('',*,*,#8609,.T.);
#11846=ORIENTED_EDGE('',*,*,#8610,.T.);
#11847=ORIENTED_EDGE('',*,*,#8611,.T.);
#11848=ORIENTED_EDGE('',*,*,#8612,.T.);
#11849=ORIENTED_EDGE('',*,*,#8613,.T.);
#11850=ORIENTED_EDGE('',*,*,#8614,.T.);
#11851=ORIENTED_EDGE('',*,*,#8615,.T.);
#11852=ORIENTED_EDGE('',*,*,#8616,.T.);
#11853=ORIENTED_EDGE('',*,*,#8617,.T.);
#11854=ORIENTED_EDGE('',*,*,#8618,.T.);
#11855=ORIENTED_EDGE('',*,*,#8619,.T.);
#11856=ORIENTED_EDGE('',*,*,#8620,.T.);
#11857=ORIENTED_EDGE('',*,*,#8621,.T.);
#11858=ORIENTED_EDGE('',*,*,#8622,.T.);
#11859=ORIENTED_EDGE('',*,*,#8623,.T.);
#11860=ORIENTED_EDGE('',*,*,#8624,.T.);
#11861=ORIENTED_EDGE('',*,*,#8625,.T.);
#11862=ORIENTED_EDGE('',*,*,#8626,.T.);
#11863=ORIENTED_EDGE('',*,*,#8627,.T.);
#11864=ORIENTED_EDGE('',*,*,#8628,.T.);
#11865=ORIENTED_EDGE('',*,*,#8629,.T.);
#11866=ORIENTED_EDGE('',*,*,#8630,.T.);
#11867=ORIENTED_EDGE('',*,*,#8631,.T.);
#11868=ORIENTED_EDGE('',*,*,#8632,.T.);
#11869=ORIENTED_EDGE('',*,*,#8633,.T.);
#11870=ORIENTED_EDGE('',*,*,#8634,.T.);
#11871=ORIENTED_EDGE('',*,*,#8635,.T.);
#11872=ORIENTED_EDGE('',*,*,#8636,.T.);
#11873=ORIENTED_EDGE('',*,*,#8637,.T.);
#11874=ORIENTED_EDGE('',*,*,#8638,.T.);
#11875=ORIENTED_EDGE('',*,*,#8639,.T.);
#11876=ORIENTED_EDGE('',*,*,#8640,.T.);
#11877=ORIENTED_EDGE('',*,*,#8641,.T.);
#11878=ORIENTED_EDGE('',*,*,#8642,.T.);
#11879=ORIENTED_EDGE('',*,*,#8643,.T.);
#11880=ORIENTED_EDGE('',*,*,#8644,.T.);
#11881=ORIENTED_EDGE('',*,*,#8645,.T.);
#11882=ORIENTED_EDGE('',*,*,#8646,.T.);
#11883=ORIENTED_EDGE('',*,*,#8647,.T.);
#11884=ORIENTED_EDGE('',*,*,#8648,.T.);
#11885=ORIENTED_EDGE('',*,*,#8649,.T.);
#11886=ORIENTED_EDGE('',*,*,#8650,.T.);
#11887=ORIENTED_EDGE('',*,*,#8651,.T.);
#11888=ORIENTED_EDGE('',*,*,#8652,.T.);
#11889=ORIENTED_EDGE('',*,*,#8653,.T.);
#11890=ORIENTED_EDGE('',*,*,#8654,.T.);
#11891=ORIENTED_EDGE('',*,*,#8655,.T.);
#11892=ORIENTED_EDGE('',*,*,#8656,.T.);
#11893=ORIENTED_EDGE('',*,*,#8657,.T.);
#11894=ORIENTED_EDGE('',*,*,#8658,.T.);
#11895=ORIENTED_EDGE('',*,*,#8659,.T.);
#11896=ORIENTED_EDGE('',*,*,#8660,.T.);
#11897=ORIENTED_EDGE('',*,*,#8661,.T.);
#11898=ORIENTED_EDGE('',*,*,#8662,.T.);
#11899=ORIENTED_EDGE('',*,*,#8663,.T.);
#11900=ORIENTED_EDGE('',*,*,#8664,.T.);
#11901=ORIENTED_EDGE('',*,*,#8665,.T.);
#11902=ORIENTED_EDGE('',*,*,#8666,.T.);
#11903=ORIENTED_EDGE('',*,*,#8667,.T.);
#11904=ORIENTED_EDGE('',*,*,#8668,.T.);
#11905=ORIENTED_EDGE('',*,*,#8669,.T.);
#11906=ORIENTED_EDGE('',*,*,#8670,.T.);
#11907=ORIENTED_EDGE('',*,*,#8671,.T.);
#11908=ORIENTED_EDGE('',*,*,#8672,.T.);
#11909=ORIENTED_EDGE('',*,*,#8673,.T.);
#11910=ORIENTED_EDGE('',*,*,#8674,.T.);
#11911=ORIENTED_EDGE('',*,*,#8675,.T.);
#11912=ORIENTED_EDGE('',*,*,#8676,.T.);
#11913=ORIENTED_EDGE('',*,*,#8677,.T.);
#11914=ORIENTED_EDGE('',*,*,#8678,.T.);
#11915=ORIENTED_EDGE('',*,*,#8679,.T.);
#11916=ORIENTED_EDGE('',*,*,#8680,.T.);
#11917=ORIENTED_EDGE('',*,*,#8681,.T.);
#11918=ORIENTED_EDGE('',*,*,#8682,.T.);
#11919=ORIENTED_EDGE('',*,*,#8683,.T.);
#11920=ORIENTED_EDGE('',*,*,#8684,.T.);
#11921=ORIENTED_EDGE('',*,*,#8685,.T.);
#11922=ORIENTED_EDGE('',*,*,#8686,.T.);
#11923=ORIENTED_EDGE('',*,*,#8687,.T.);
#11924=ORIENTED_EDGE('',*,*,#8688,.T.);
#11925=ORIENTED_EDGE('',*,*,#8689,.T.);
#11926=ORIENTED_EDGE('',*,*,#8690,.T.);
#11927=ORIENTED_EDGE('',*,*,#8691,.T.);
#11928=ORIENTED_EDGE('',*,*,#8692,.T.);
#11929=ORIENTED_EDGE('',*,*,#8693,.T.);
#11930=ORIENTED_EDGE('',*,*,#8694,.T.);
#11931=ORIENTED_EDGE('',*,*,#8695,.T.);
#11932=ORIENTED_EDGE('',*,*,#8696,.T.);
#11933=ORIENTED_EDGE('',*,*,#8697,.T.);
#11934=ORIENTED_EDGE('',*,*,#8698,.T.);
#11935=ORIENTED_EDGE('',*,*,#8699,.T.);
#11936=ORIENTED_EDGE('',*,*,#8700,.T.);
#11937=ORIENTED_EDGE('',*,*,#8701,.T.);
#11938=ORIENTED_EDGE('',*,*,#8702,.T.);
#11939=ORIENTED_EDGE('',*,*,#8703,.T.);
#11940=ORIENTED_EDGE('',*,*,#8704,.T.);
#11941=ORIENTED_EDGE('',*,*,#8705,.T.);
#11942=ORIENTED_EDGE('',*,*,#8706,.T.);
#11943=ORIENTED_EDGE('',*,*,#8707,.T.);
#11944=ORIENTED_EDGE('',*,*,#8708,.T.);
#11945=ORIENTED_EDGE('',*,*,#8709,.T.);
#11946=ORIENTED_EDGE('',*,*,#8710,.T.);
#11947=ORIENTED_EDGE('',*,*,#8711,.T.);
#11948=ORIENTED_EDGE('',*,*,#8712,.T.);
#11949=ORIENTED_EDGE('',*,*,#8713,.T.);
#11950=ORIENTED_EDGE('',*,*,#8714,.T.);
#11951=ORIENTED_EDGE('',*,*,#8715,.T.);
#11952=ORIENTED_EDGE('',*,*,#8716,.T.);
#11953=ORIENTED_EDGE('',*,*,#8717,.T.);
#11954=ORIENTED_EDGE('',*,*,#8718,.T.);
#11955=ORIENTED_EDGE('',*,*,#8719,.T.);
#11956=ORIENTED_EDGE('',*,*,#8599,.F.);
#11957=ORIENTED_EDGE('',*,*,#8602,.F.);
#11958=ORIENTED_EDGE('',*,*,#8720,.F.);
#11959=ORIENTED_EDGE('',*,*,#8596,.F.);
#11960=ORIENTED_EDGE('',*,*,#8721,.F.);
#11961=ORIENTED_EDGE('',*,*,#8722,.F.);
#11962=ORIENTED_EDGE('',*,*,#8723,.F.);
#11963=ORIENTED_EDGE('',*,*,#8724,.F.);
#11964=ORIENTED_EDGE('',*,*,#8725,.F.);
#11965=ORIENTED_EDGE('',*,*,#8601,.F.);
#11966=ORIENTED_EDGE('',*,*,#8726,.F.);
#11967=ORIENTED_EDGE('',*,*,#8597,.F.);
#11968=ORIENTED_EDGE('',*,*,#8720,.T.);
#11969=ORIENTED_EDGE('',*,*,#8600,.F.);
#11970=ORIENTED_EDGE('',*,*,#8727,.F.);
#11971=ORIENTED_EDGE('',*,*,#8728,.F.);
#11972=ORIENTED_EDGE('',*,*,#8729,.F.);
#11973=ORIENTED_EDGE('',*,*,#8730,.F.);
#11974=ORIENTED_EDGE('',*,*,#8731,.F.);
#11975=ORIENTED_EDGE('',*,*,#8478,.F.);
#11976=ORIENTED_EDGE('',*,*,#8726,.T.);
#11977=ORIENTED_EDGE('',*,*,#8725,.T.);
#11978=ORIENTED_EDGE('',*,*,#8732,.T.);
#11979=ORIENTED_EDGE('',*,*,#8733,.T.);
#11980=ORIENTED_EDGE('',*,*,#8603,.F.);
#11981=ORIENTED_EDGE('',*,*,#8724,.T.);
#11982=ORIENTED_EDGE('',*,*,#8734,.T.);
#11983=ORIENTED_EDGE('',*,*,#8735,.T.);
#11984=ORIENTED_EDGE('',*,*,#8732,.F.);
#11985=ORIENTED_EDGE('',*,*,#8723,.T.);
#11986=ORIENTED_EDGE('',*,*,#8736,.T.);
#11987=ORIENTED_EDGE('',*,*,#8737,.T.);
#11988=ORIENTED_EDGE('',*,*,#8734,.F.);
#11989=ORIENTED_EDGE('',*,*,#8722,.T.);
#11990=ORIENTED_EDGE('',*,*,#8738,.T.);
#11991=ORIENTED_EDGE('',*,*,#8739,.T.);
#11992=ORIENTED_EDGE('',*,*,#8736,.F.);
#11993=ORIENTED_EDGE('',*,*,#8721,.T.);
#11994=ORIENTED_EDGE('',*,*,#8595,.T.);
#11995=ORIENTED_EDGE('',*,*,#8740,.T.);
#11996=ORIENTED_EDGE('',*,*,#8738,.F.);
#11997=ORIENTED_EDGE('',*,*,#8718,.F.);
#11998=ORIENTED_EDGE('',*,*,#8741,.F.);
#11999=ORIENTED_EDGE('',*,*,#8480,.F.);
#12000=ORIENTED_EDGE('',*,*,#8742,.F.);
#12001=ORIENTED_EDGE('',*,*,#8743,.F.);
#12002=ORIENTED_EDGE('',*,*,#8744,.F.);
#12003=ORIENTED_EDGE('',*,*,#8745,.F.);
#12004=ORIENTED_EDGE('',*,*,#8746,.F.);
#12005=ORIENTED_EDGE('',*,*,#8717,.F.);
#12006=ORIENTED_EDGE('',*,*,#8747,.F.);
#12007=ORIENTED_EDGE('',*,*,#8481,.F.);
#12008=ORIENTED_EDGE('',*,*,#8741,.T.);
#12009=ORIENTED_EDGE('',*,*,#8716,.F.);
#12010=ORIENTED_EDGE('',*,*,#8748,.F.);
#12011=ORIENTED_EDGE('',*,*,#8749,.F.);
#12012=ORIENTED_EDGE('',*,*,#8750,.F.);
#12013=ORIENTED_EDGE('',*,*,#8751,.F.);
#12014=ORIENTED_EDGE('',*,*,#8752,.F.);
#12015=ORIENTED_EDGE('',*,*,#8482,.F.);
#12016=ORIENTED_EDGE('',*,*,#8747,.T.);
#12017=ORIENTED_EDGE('',*,*,#8727,.T.);
#12018=ORIENTED_EDGE('',*,*,#8719,.F.);
#12019=ORIENTED_EDGE('',*,*,#8746,.T.);
#12020=ORIENTED_EDGE('',*,*,#8753,.T.);
#12021=ORIENTED_EDGE('',*,*,#8728,.T.);
#12022=ORIENTED_EDGE('',*,*,#8753,.F.);
#12023=ORIENTED_EDGE('',*,*,#8745,.T.);
#12024=ORIENTED_EDGE('',*,*,#8754,.T.);
#12025=ORIENTED_EDGE('',*,*,#8729,.T.);
#12026=ORIENTED_EDGE('',*,*,#8754,.F.);
#12027=ORIENTED_EDGE('',*,*,#8744,.T.);
#12028=ORIENTED_EDGE('',*,*,#8755,.T.);
#12029=ORIENTED_EDGE('',*,*,#8730,.T.);
#12030=ORIENTED_EDGE('',*,*,#8755,.F.);
#12031=ORIENTED_EDGE('',*,*,#8743,.T.);
#12032=ORIENTED_EDGE('',*,*,#8756,.T.);
#12033=ORIENTED_EDGE('',*,*,#8731,.T.);
#12034=ORIENTED_EDGE('',*,*,#8756,.F.);
#12035=ORIENTED_EDGE('',*,*,#8742,.T.);
#12036=ORIENTED_EDGE('',*,*,#8479,.T.);
#12037=ORIENTED_EDGE('',*,*,#8714,.F.);
#12038=ORIENTED_EDGE('',*,*,#8757,.F.);
#12039=ORIENTED_EDGE('',*,*,#8484,.F.);
#12040=ORIENTED_EDGE('',*,*,#8758,.F.);
#12041=ORIENTED_EDGE('',*,*,#8759,.F.);
#12042=ORIENTED_EDGE('',*,*,#8760,.F.);
#12043=ORIENTED_EDGE('',*,*,#8761,.F.);
#12044=ORIENTED_EDGE('',*,*,#8762,.F.);
#12045=ORIENTED_EDGE('',*,*,#8713,.F.);
#12046=ORIENTED_EDGE('',*,*,#8763,.F.);
#12047=ORIENTED_EDGE('',*,*,#8485,.F.);
#12048=ORIENTED_EDGE('',*,*,#8757,.T.);
#12049=ORIENTED_EDGE('',*,*,#8712,.F.);
#12050=ORIENTED_EDGE('',*,*,#8764,.F.);
#12051=ORIENTED_EDGE('',*,*,#8765,.F.);
#12052=ORIENTED_EDGE('',*,*,#8766,.F.);
#12053=ORIENTED_EDGE('',*,*,#8767,.F.);
#12054=ORIENTED_EDGE('',*,*,#8768,.F.);
#12055=ORIENTED_EDGE('',*,*,#8486,.F.);
#12056=ORIENTED_EDGE('',*,*,#8763,.T.);
#12057=ORIENTED_EDGE('',*,*,#8748,.T.);
#12058=ORIENTED_EDGE('',*,*,#8715,.F.);
#12059=ORIENTED_EDGE('',*,*,#8762,.T.);
#12060=ORIENTED_EDGE('',*,*,#8769,.T.);
#12061=ORIENTED_EDGE('',*,*,#8749,.T.);
#12062=ORIENTED_EDGE('',*,*,#8769,.F.);
#12063=ORIENTED_EDGE('',*,*,#8761,.T.);
#12064=ORIENTED_EDGE('',*,*,#8770,.T.);
#12065=ORIENTED_EDGE('',*,*,#8750,.T.);
#12066=ORIENTED_EDGE('',*,*,#8770,.F.);
#12067=ORIENTED_EDGE('',*,*,#8760,.T.);
#12068=ORIENTED_EDGE('',*,*,#8771,.T.);
#12069=ORIENTED_EDGE('',*,*,#8751,.T.);
#12070=ORIENTED_EDGE('',*,*,#8771,.F.);
#12071=ORIENTED_EDGE('',*,*,#8759,.T.);
#12072=ORIENTED_EDGE('',*,*,#8772,.T.);
#12073=ORIENTED_EDGE('',*,*,#8752,.T.);
#12074=ORIENTED_EDGE('',*,*,#8772,.F.);
#12075=ORIENTED_EDGE('',*,*,#8758,.T.);
#12076=ORIENTED_EDGE('',*,*,#8483,.T.);
#12077=ORIENTED_EDGE('',*,*,#8710,.F.);
#12078=ORIENTED_EDGE('',*,*,#8773,.F.);
#12079=ORIENTED_EDGE('',*,*,#8488,.F.);
#12080=ORIENTED_EDGE('',*,*,#8774,.F.);
#12081=ORIENTED_EDGE('',*,*,#8775,.F.);
#12082=ORIENTED_EDGE('',*,*,#8776,.F.);
#12083=ORIENTED_EDGE('',*,*,#8777,.F.);
#12084=ORIENTED_EDGE('',*,*,#8778,.F.);
#12085=ORIENTED_EDGE('',*,*,#8709,.F.);
#12086=ORIENTED_EDGE('',*,*,#8779,.F.);
#12087=ORIENTED_EDGE('',*,*,#8489,.F.);
#12088=ORIENTED_EDGE('',*,*,#8773,.T.);
#12089=ORIENTED_EDGE('',*,*,#8708,.F.);
#12090=ORIENTED_EDGE('',*,*,#8780,.F.);
#12091=ORIENTED_EDGE('',*,*,#8781,.F.);
#12092=ORIENTED_EDGE('',*,*,#8782,.F.);
#12093=ORIENTED_EDGE('',*,*,#8783,.F.);
#12094=ORIENTED_EDGE('',*,*,#8784,.F.);
#12095=ORIENTED_EDGE('',*,*,#8490,.F.);
#12096=ORIENTED_EDGE('',*,*,#8779,.T.);
#12097=ORIENTED_EDGE('',*,*,#8764,.T.);
#12098=ORIENTED_EDGE('',*,*,#8711,.F.);
#12099=ORIENTED_EDGE('',*,*,#8778,.T.);
#12100=ORIENTED_EDGE('',*,*,#8785,.T.);
#12101=ORIENTED_EDGE('',*,*,#8765,.T.);
#12102=ORIENTED_EDGE('',*,*,#8785,.F.);
#12103=ORIENTED_EDGE('',*,*,#8777,.T.);
#12104=ORIENTED_EDGE('',*,*,#8786,.T.);
#12105=ORIENTED_EDGE('',*,*,#8766,.T.);
#12106=ORIENTED_EDGE('',*,*,#8786,.F.);
#12107=ORIENTED_EDGE('',*,*,#8776,.T.);
#12108=ORIENTED_EDGE('',*,*,#8787,.T.);
#12109=ORIENTED_EDGE('',*,*,#8767,.T.);
#12110=ORIENTED_EDGE('',*,*,#8787,.F.);
#12111=ORIENTED_EDGE('',*,*,#8775,.T.);
#12112=ORIENTED_EDGE('',*,*,#8788,.T.);
#12113=ORIENTED_EDGE('',*,*,#8768,.T.);
#12114=ORIENTED_EDGE('',*,*,#8788,.F.);
#12115=ORIENTED_EDGE('',*,*,#8774,.T.);
#12116=ORIENTED_EDGE('',*,*,#8487,.T.);
#12117=ORIENTED_EDGE('',*,*,#8706,.F.);
#12118=ORIENTED_EDGE('',*,*,#8789,.F.);
#12119=ORIENTED_EDGE('',*,*,#8492,.F.);
#12120=ORIENTED_EDGE('',*,*,#8790,.F.);
#12121=ORIENTED_EDGE('',*,*,#8791,.F.);
#12122=ORIENTED_EDGE('',*,*,#8792,.F.);
#12123=ORIENTED_EDGE('',*,*,#8793,.F.);
#12124=ORIENTED_EDGE('',*,*,#8794,.F.);
#12125=ORIENTED_EDGE('',*,*,#8705,.F.);
#12126=ORIENTED_EDGE('',*,*,#8795,.F.);
#12127=ORIENTED_EDGE('',*,*,#8493,.F.);
#12128=ORIENTED_EDGE('',*,*,#8789,.T.);
#12129=ORIENTED_EDGE('',*,*,#8704,.F.);
#12130=ORIENTED_EDGE('',*,*,#8796,.F.);
#12131=ORIENTED_EDGE('',*,*,#8797,.F.);
#12132=ORIENTED_EDGE('',*,*,#8798,.F.);
#12133=ORIENTED_EDGE('',*,*,#8799,.F.);
#12134=ORIENTED_EDGE('',*,*,#8800,.F.);
#12135=ORIENTED_EDGE('',*,*,#8494,.F.);
#12136=ORIENTED_EDGE('',*,*,#8795,.T.);
#12137=ORIENTED_EDGE('',*,*,#8780,.T.);
#12138=ORIENTED_EDGE('',*,*,#8707,.F.);
#12139=ORIENTED_EDGE('',*,*,#8794,.T.);
#12140=ORIENTED_EDGE('',*,*,#8801,.T.);
#12141=ORIENTED_EDGE('',*,*,#8781,.T.);
#12142=ORIENTED_EDGE('',*,*,#8801,.F.);
#12143=ORIENTED_EDGE('',*,*,#8793,.T.);
#12144=ORIENTED_EDGE('',*,*,#8802,.T.);
#12145=ORIENTED_EDGE('',*,*,#8782,.T.);
#12146=ORIENTED_EDGE('',*,*,#8802,.F.);
#12147=ORIENTED_EDGE('',*,*,#8792,.T.);
#12148=ORIENTED_EDGE('',*,*,#8803,.T.);
#12149=ORIENTED_EDGE('',*,*,#8783,.T.);
#12150=ORIENTED_EDGE('',*,*,#8803,.F.);
#12151=ORIENTED_EDGE('',*,*,#8791,.T.);
#12152=ORIENTED_EDGE('',*,*,#8804,.T.);
#12153=ORIENTED_EDGE('',*,*,#8784,.T.);
#12154=ORIENTED_EDGE('',*,*,#8804,.F.);
#12155=ORIENTED_EDGE('',*,*,#8790,.T.);
#12156=ORIENTED_EDGE('',*,*,#8491,.T.);
#12157=ORIENTED_EDGE('',*,*,#8702,.F.);
#12158=ORIENTED_EDGE('',*,*,#8805,.F.);
#12159=ORIENTED_EDGE('',*,*,#8496,.F.);
#12160=ORIENTED_EDGE('',*,*,#8806,.F.);
#12161=ORIENTED_EDGE('',*,*,#8807,.F.);
#12162=ORIENTED_EDGE('',*,*,#8808,.F.);
#12163=ORIENTED_EDGE('',*,*,#8809,.F.);
#12164=ORIENTED_EDGE('',*,*,#8810,.F.);
#12165=ORIENTED_EDGE('',*,*,#8701,.F.);
#12166=ORIENTED_EDGE('',*,*,#8811,.F.);
#12167=ORIENTED_EDGE('',*,*,#8497,.F.);
#12168=ORIENTED_EDGE('',*,*,#8805,.T.);
#12169=ORIENTED_EDGE('',*,*,#8700,.F.);
#12170=ORIENTED_EDGE('',*,*,#8812,.F.);
#12171=ORIENTED_EDGE('',*,*,#8813,.F.);
#12172=ORIENTED_EDGE('',*,*,#8814,.F.);
#12173=ORIENTED_EDGE('',*,*,#8815,.F.);
#12174=ORIENTED_EDGE('',*,*,#8816,.F.);
#12175=ORIENTED_EDGE('',*,*,#8498,.F.);
#12176=ORIENTED_EDGE('',*,*,#8811,.T.);
#12177=ORIENTED_EDGE('',*,*,#8796,.T.);
#12178=ORIENTED_EDGE('',*,*,#8703,.F.);
#12179=ORIENTED_EDGE('',*,*,#8810,.T.);
#12180=ORIENTED_EDGE('',*,*,#8817,.T.);
#12181=ORIENTED_EDGE('',*,*,#8797,.T.);
#12182=ORIENTED_EDGE('',*,*,#8817,.F.);
#12183=ORIENTED_EDGE('',*,*,#8809,.T.);
#12184=ORIENTED_EDGE('',*,*,#8818,.T.);
#12185=ORIENTED_EDGE('',*,*,#8798,.T.);
#12186=ORIENTED_EDGE('',*,*,#8818,.F.);
#12187=ORIENTED_EDGE('',*,*,#8808,.T.);
#12188=ORIENTED_EDGE('',*,*,#8819,.T.);
#12189=ORIENTED_EDGE('',*,*,#8799,.T.);
#12190=ORIENTED_EDGE('',*,*,#8819,.F.);
#12191=ORIENTED_EDGE('',*,*,#8807,.T.);
#12192=ORIENTED_EDGE('',*,*,#8820,.T.);
#12193=ORIENTED_EDGE('',*,*,#8800,.T.);
#12194=ORIENTED_EDGE('',*,*,#8820,.F.);
#12195=ORIENTED_EDGE('',*,*,#8806,.T.);
#12196=ORIENTED_EDGE('',*,*,#8495,.T.);
#12197=ORIENTED_EDGE('',*,*,#8698,.F.);
#12198=ORIENTED_EDGE('',*,*,#8821,.F.);
#12199=ORIENTED_EDGE('',*,*,#8500,.F.);
#12200=ORIENTED_EDGE('',*,*,#8822,.F.);
#12201=ORIENTED_EDGE('',*,*,#8823,.F.);
#12202=ORIENTED_EDGE('',*,*,#8824,.F.);
#12203=ORIENTED_EDGE('',*,*,#8825,.F.);
#12204=ORIENTED_EDGE('',*,*,#8826,.F.);
#12205=ORIENTED_EDGE('',*,*,#8697,.F.);
#12206=ORIENTED_EDGE('',*,*,#8827,.F.);
#12207=ORIENTED_EDGE('',*,*,#8501,.F.);
#12208=ORIENTED_EDGE('',*,*,#8821,.T.);
#12209=ORIENTED_EDGE('',*,*,#8696,.F.);
#12210=ORIENTED_EDGE('',*,*,#8828,.F.);
#12211=ORIENTED_EDGE('',*,*,#8829,.F.);
#12212=ORIENTED_EDGE('',*,*,#8830,.F.);
#12213=ORIENTED_EDGE('',*,*,#8831,.F.);
#12214=ORIENTED_EDGE('',*,*,#8832,.F.);
#12215=ORIENTED_EDGE('',*,*,#8502,.F.);
#12216=ORIENTED_EDGE('',*,*,#8827,.T.);
#12217=ORIENTED_EDGE('',*,*,#8812,.T.);
#12218=ORIENTED_EDGE('',*,*,#8699,.F.);
#12219=ORIENTED_EDGE('',*,*,#8826,.T.);
#12220=ORIENTED_EDGE('',*,*,#8833,.T.);
#12221=ORIENTED_EDGE('',*,*,#8813,.T.);
#12222=ORIENTED_EDGE('',*,*,#8833,.F.);
#12223=ORIENTED_EDGE('',*,*,#8825,.T.);
#12224=ORIENTED_EDGE('',*,*,#8834,.T.);
#12225=ORIENTED_EDGE('',*,*,#8814,.T.);
#12226=ORIENTED_EDGE('',*,*,#8834,.F.);
#12227=ORIENTED_EDGE('',*,*,#8824,.T.);
#12228=ORIENTED_EDGE('',*,*,#8835,.T.);
#12229=ORIENTED_EDGE('',*,*,#8815,.T.);
#12230=ORIENTED_EDGE('',*,*,#8835,.F.);
#12231=ORIENTED_EDGE('',*,*,#8823,.T.);
#12232=ORIENTED_EDGE('',*,*,#8836,.T.);
#12233=ORIENTED_EDGE('',*,*,#8816,.T.);
#12234=ORIENTED_EDGE('',*,*,#8836,.F.);
#12235=ORIENTED_EDGE('',*,*,#8822,.T.);
#12236=ORIENTED_EDGE('',*,*,#8499,.T.);
#12237=ORIENTED_EDGE('',*,*,#8694,.F.);
#12238=ORIENTED_EDGE('',*,*,#8837,.F.);
#12239=ORIENTED_EDGE('',*,*,#8504,.F.);
#12240=ORIENTED_EDGE('',*,*,#8838,.F.);
#12241=ORIENTED_EDGE('',*,*,#8839,.F.);
#12242=ORIENTED_EDGE('',*,*,#8840,.F.);
#12243=ORIENTED_EDGE('',*,*,#8841,.F.);
#12244=ORIENTED_EDGE('',*,*,#8842,.F.);
#12245=ORIENTED_EDGE('',*,*,#8693,.F.);
#12246=ORIENTED_EDGE('',*,*,#8843,.F.);
#12247=ORIENTED_EDGE('',*,*,#8505,.F.);
#12248=ORIENTED_EDGE('',*,*,#8837,.T.);
#12249=ORIENTED_EDGE('',*,*,#8692,.F.);
#12250=ORIENTED_EDGE('',*,*,#8844,.F.);
#12251=ORIENTED_EDGE('',*,*,#8845,.F.);
#12252=ORIENTED_EDGE('',*,*,#8846,.F.);
#12253=ORIENTED_EDGE('',*,*,#8847,.F.);
#12254=ORIENTED_EDGE('',*,*,#8848,.F.);
#12255=ORIENTED_EDGE('',*,*,#8506,.F.);
#12256=ORIENTED_EDGE('',*,*,#8843,.T.);
#12257=ORIENTED_EDGE('',*,*,#8828,.T.);
#12258=ORIENTED_EDGE('',*,*,#8695,.F.);
#12259=ORIENTED_EDGE('',*,*,#8842,.T.);
#12260=ORIENTED_EDGE('',*,*,#8849,.T.);
#12261=ORIENTED_EDGE('',*,*,#8829,.T.);
#12262=ORIENTED_EDGE('',*,*,#8849,.F.);
#12263=ORIENTED_EDGE('',*,*,#8841,.T.);
#12264=ORIENTED_EDGE('',*,*,#8850,.T.);
#12265=ORIENTED_EDGE('',*,*,#8830,.T.);
#12266=ORIENTED_EDGE('',*,*,#8850,.F.);
#12267=ORIENTED_EDGE('',*,*,#8840,.T.);
#12268=ORIENTED_EDGE('',*,*,#8851,.T.);
#12269=ORIENTED_EDGE('',*,*,#8831,.T.);
#12270=ORIENTED_EDGE('',*,*,#8851,.F.);
#12271=ORIENTED_EDGE('',*,*,#8839,.T.);
#12272=ORIENTED_EDGE('',*,*,#8852,.T.);
#12273=ORIENTED_EDGE('',*,*,#8832,.T.);
#12274=ORIENTED_EDGE('',*,*,#8852,.F.);
#12275=ORIENTED_EDGE('',*,*,#8838,.T.);
#12276=ORIENTED_EDGE('',*,*,#8503,.T.);
#12277=ORIENTED_EDGE('',*,*,#8690,.F.);
#12278=ORIENTED_EDGE('',*,*,#8853,.F.);
#12279=ORIENTED_EDGE('',*,*,#8508,.F.);
#12280=ORIENTED_EDGE('',*,*,#8854,.F.);
#12281=ORIENTED_EDGE('',*,*,#8855,.F.);
#12282=ORIENTED_EDGE('',*,*,#8856,.F.);
#12283=ORIENTED_EDGE('',*,*,#8857,.F.);
#12284=ORIENTED_EDGE('',*,*,#8858,.F.);
#12285=ORIENTED_EDGE('',*,*,#8689,.F.);
#12286=ORIENTED_EDGE('',*,*,#8859,.F.);
#12287=ORIENTED_EDGE('',*,*,#8509,.F.);
#12288=ORIENTED_EDGE('',*,*,#8853,.T.);
#12289=ORIENTED_EDGE('',*,*,#8688,.F.);
#12290=ORIENTED_EDGE('',*,*,#8860,.F.);
#12291=ORIENTED_EDGE('',*,*,#8861,.F.);
#12292=ORIENTED_EDGE('',*,*,#8862,.F.);
#12293=ORIENTED_EDGE('',*,*,#8863,.F.);
#12294=ORIENTED_EDGE('',*,*,#8864,.F.);
#12295=ORIENTED_EDGE('',*,*,#8510,.F.);
#12296=ORIENTED_EDGE('',*,*,#8859,.T.);
#12297=ORIENTED_EDGE('',*,*,#8844,.T.);
#12298=ORIENTED_EDGE('',*,*,#8691,.F.);
#12299=ORIENTED_EDGE('',*,*,#8858,.T.);
#12300=ORIENTED_EDGE('',*,*,#8865,.T.);
#12301=ORIENTED_EDGE('',*,*,#8845,.T.);
#12302=ORIENTED_EDGE('',*,*,#8865,.F.);
#12303=ORIENTED_EDGE('',*,*,#8857,.T.);
#12304=ORIENTED_EDGE('',*,*,#8866,.T.);
#12305=ORIENTED_EDGE('',*,*,#8846,.T.);
#12306=ORIENTED_EDGE('',*,*,#8866,.F.);
#12307=ORIENTED_EDGE('',*,*,#8856,.T.);
#12308=ORIENTED_EDGE('',*,*,#8867,.T.);
#12309=ORIENTED_EDGE('',*,*,#8847,.T.);
#12310=ORIENTED_EDGE('',*,*,#8867,.F.);
#12311=ORIENTED_EDGE('',*,*,#8855,.T.);
#12312=ORIENTED_EDGE('',*,*,#8868,.T.);
#12313=ORIENTED_EDGE('',*,*,#8848,.T.);
#12314=ORIENTED_EDGE('',*,*,#8868,.F.);
#12315=ORIENTED_EDGE('',*,*,#8854,.T.);
#12316=ORIENTED_EDGE('',*,*,#8507,.T.);
#12317=ORIENTED_EDGE('',*,*,#8686,.F.);
#12318=ORIENTED_EDGE('',*,*,#8869,.F.);
#12319=ORIENTED_EDGE('',*,*,#8512,.F.);
#12320=ORIENTED_EDGE('',*,*,#8870,.F.);
#12321=ORIENTED_EDGE('',*,*,#8871,.F.);
#12322=ORIENTED_EDGE('',*,*,#8872,.F.);
#12323=ORIENTED_EDGE('',*,*,#8873,.F.);
#12324=ORIENTED_EDGE('',*,*,#8874,.F.);
#12325=ORIENTED_EDGE('',*,*,#8685,.F.);
#12326=ORIENTED_EDGE('',*,*,#8875,.F.);
#12327=ORIENTED_EDGE('',*,*,#8513,.F.);
#12328=ORIENTED_EDGE('',*,*,#8869,.T.);
#12329=ORIENTED_EDGE('',*,*,#8684,.F.);
#12330=ORIENTED_EDGE('',*,*,#8876,.F.);
#12331=ORIENTED_EDGE('',*,*,#8877,.F.);
#12332=ORIENTED_EDGE('',*,*,#8878,.F.);
#12333=ORIENTED_EDGE('',*,*,#8879,.F.);
#12334=ORIENTED_EDGE('',*,*,#8880,.F.);
#12335=ORIENTED_EDGE('',*,*,#8514,.F.);
#12336=ORIENTED_EDGE('',*,*,#8875,.T.);
#12337=ORIENTED_EDGE('',*,*,#8860,.T.);
#12338=ORIENTED_EDGE('',*,*,#8687,.F.);
#12339=ORIENTED_EDGE('',*,*,#8874,.T.);
#12340=ORIENTED_EDGE('',*,*,#8881,.T.);
#12341=ORIENTED_EDGE('',*,*,#8861,.T.);
#12342=ORIENTED_EDGE('',*,*,#8881,.F.);
#12343=ORIENTED_EDGE('',*,*,#8873,.T.);
#12344=ORIENTED_EDGE('',*,*,#8882,.T.);
#12345=ORIENTED_EDGE('',*,*,#8862,.T.);
#12346=ORIENTED_EDGE('',*,*,#8882,.F.);
#12347=ORIENTED_EDGE('',*,*,#8872,.T.);
#12348=ORIENTED_EDGE('',*,*,#8883,.T.);
#12349=ORIENTED_EDGE('',*,*,#8863,.T.);
#12350=ORIENTED_EDGE('',*,*,#8883,.F.);
#12351=ORIENTED_EDGE('',*,*,#8871,.T.);
#12352=ORIENTED_EDGE('',*,*,#8884,.T.);
#12353=ORIENTED_EDGE('',*,*,#8864,.T.);
#12354=ORIENTED_EDGE('',*,*,#8884,.F.);
#12355=ORIENTED_EDGE('',*,*,#8870,.T.);
#12356=ORIENTED_EDGE('',*,*,#8511,.T.);
#12357=ORIENTED_EDGE('',*,*,#8682,.F.);
#12358=ORIENTED_EDGE('',*,*,#8885,.F.);
#12359=ORIENTED_EDGE('',*,*,#8516,.F.);
#12360=ORIENTED_EDGE('',*,*,#8886,.F.);
#12361=ORIENTED_EDGE('',*,*,#8887,.F.);
#12362=ORIENTED_EDGE('',*,*,#8888,.F.);
#12363=ORIENTED_EDGE('',*,*,#8889,.F.);
#12364=ORIENTED_EDGE('',*,*,#8890,.F.);
#12365=ORIENTED_EDGE('',*,*,#8681,.F.);
#12366=ORIENTED_EDGE('',*,*,#8891,.F.);
#12367=ORIENTED_EDGE('',*,*,#8517,.F.);
#12368=ORIENTED_EDGE('',*,*,#8885,.T.);
#12369=ORIENTED_EDGE('',*,*,#8680,.F.);
#12370=ORIENTED_EDGE('',*,*,#8892,.F.);
#12371=ORIENTED_EDGE('',*,*,#8893,.F.);
#12372=ORIENTED_EDGE('',*,*,#8894,.F.);
#12373=ORIENTED_EDGE('',*,*,#8895,.F.);
#12374=ORIENTED_EDGE('',*,*,#8896,.F.);
#12375=ORIENTED_EDGE('',*,*,#8518,.F.);
#12376=ORIENTED_EDGE('',*,*,#8891,.T.);
#12377=ORIENTED_EDGE('',*,*,#8876,.T.);
#12378=ORIENTED_EDGE('',*,*,#8683,.F.);
#12379=ORIENTED_EDGE('',*,*,#8890,.T.);
#12380=ORIENTED_EDGE('',*,*,#8897,.T.);
#12381=ORIENTED_EDGE('',*,*,#8877,.T.);
#12382=ORIENTED_EDGE('',*,*,#8897,.F.);
#12383=ORIENTED_EDGE('',*,*,#8889,.T.);
#12384=ORIENTED_EDGE('',*,*,#8898,.T.);
#12385=ORIENTED_EDGE('',*,*,#8878,.T.);
#12386=ORIENTED_EDGE('',*,*,#8898,.F.);
#12387=ORIENTED_EDGE('',*,*,#8888,.T.);
#12388=ORIENTED_EDGE('',*,*,#8899,.T.);
#12389=ORIENTED_EDGE('',*,*,#8879,.T.);
#12390=ORIENTED_EDGE('',*,*,#8899,.F.);
#12391=ORIENTED_EDGE('',*,*,#8887,.T.);
#12392=ORIENTED_EDGE('',*,*,#8900,.T.);
#12393=ORIENTED_EDGE('',*,*,#8880,.T.);
#12394=ORIENTED_EDGE('',*,*,#8900,.F.);
#12395=ORIENTED_EDGE('',*,*,#8886,.T.);
#12396=ORIENTED_EDGE('',*,*,#8515,.T.);
#12397=ORIENTED_EDGE('',*,*,#8678,.F.);
#12398=ORIENTED_EDGE('',*,*,#8901,.F.);
#12399=ORIENTED_EDGE('',*,*,#8520,.F.);
#12400=ORIENTED_EDGE('',*,*,#8902,.F.);
#12401=ORIENTED_EDGE('',*,*,#8903,.F.);
#12402=ORIENTED_EDGE('',*,*,#8904,.F.);
#12403=ORIENTED_EDGE('',*,*,#8905,.F.);
#12404=ORIENTED_EDGE('',*,*,#8906,.F.);
#12405=ORIENTED_EDGE('',*,*,#8677,.F.);
#12406=ORIENTED_EDGE('',*,*,#8907,.F.);
#12407=ORIENTED_EDGE('',*,*,#8521,.F.);
#12408=ORIENTED_EDGE('',*,*,#8901,.T.);
#12409=ORIENTED_EDGE('',*,*,#8676,.F.);
#12410=ORIENTED_EDGE('',*,*,#8908,.F.);
#12411=ORIENTED_EDGE('',*,*,#8909,.F.);
#12412=ORIENTED_EDGE('',*,*,#8910,.F.);
#12413=ORIENTED_EDGE('',*,*,#8911,.F.);
#12414=ORIENTED_EDGE('',*,*,#8912,.F.);
#12415=ORIENTED_EDGE('',*,*,#8522,.F.);
#12416=ORIENTED_EDGE('',*,*,#8907,.T.);
#12417=ORIENTED_EDGE('',*,*,#8892,.T.);
#12418=ORIENTED_EDGE('',*,*,#8679,.F.);
#12419=ORIENTED_EDGE('',*,*,#8906,.T.);
#12420=ORIENTED_EDGE('',*,*,#8913,.T.);
#12421=ORIENTED_EDGE('',*,*,#8893,.T.);
#12422=ORIENTED_EDGE('',*,*,#8913,.F.);
#12423=ORIENTED_EDGE('',*,*,#8905,.T.);
#12424=ORIENTED_EDGE('',*,*,#8914,.T.);
#12425=ORIENTED_EDGE('',*,*,#8894,.T.);
#12426=ORIENTED_EDGE('',*,*,#8914,.F.);
#12427=ORIENTED_EDGE('',*,*,#8904,.T.);
#12428=ORIENTED_EDGE('',*,*,#8915,.T.);
#12429=ORIENTED_EDGE('',*,*,#8895,.T.);
#12430=ORIENTED_EDGE('',*,*,#8915,.F.);
#12431=ORIENTED_EDGE('',*,*,#8903,.T.);
#12432=ORIENTED_EDGE('',*,*,#8916,.T.);
#12433=ORIENTED_EDGE('',*,*,#8896,.T.);
#12434=ORIENTED_EDGE('',*,*,#8916,.F.);
#12435=ORIENTED_EDGE('',*,*,#8902,.T.);
#12436=ORIENTED_EDGE('',*,*,#8519,.T.);
#12437=ORIENTED_EDGE('',*,*,#8674,.F.);
#12438=ORIENTED_EDGE('',*,*,#8917,.F.);
#12439=ORIENTED_EDGE('',*,*,#8524,.F.);
#12440=ORIENTED_EDGE('',*,*,#8918,.F.);
#12441=ORIENTED_EDGE('',*,*,#8919,.F.);
#12442=ORIENTED_EDGE('',*,*,#8920,.F.);
#12443=ORIENTED_EDGE('',*,*,#8921,.F.);
#12444=ORIENTED_EDGE('',*,*,#8922,.F.);
#12445=ORIENTED_EDGE('',*,*,#8673,.F.);
#12446=ORIENTED_EDGE('',*,*,#8923,.F.);
#12447=ORIENTED_EDGE('',*,*,#8525,.F.);
#12448=ORIENTED_EDGE('',*,*,#8917,.T.);
#12449=ORIENTED_EDGE('',*,*,#8672,.F.);
#12450=ORIENTED_EDGE('',*,*,#8924,.F.);
#12451=ORIENTED_EDGE('',*,*,#8925,.F.);
#12452=ORIENTED_EDGE('',*,*,#8926,.F.);
#12453=ORIENTED_EDGE('',*,*,#8927,.F.);
#12454=ORIENTED_EDGE('',*,*,#8928,.F.);
#12455=ORIENTED_EDGE('',*,*,#8526,.F.);
#12456=ORIENTED_EDGE('',*,*,#8923,.T.);
#12457=ORIENTED_EDGE('',*,*,#8908,.T.);
#12458=ORIENTED_EDGE('',*,*,#8675,.F.);
#12459=ORIENTED_EDGE('',*,*,#8922,.T.);
#12460=ORIENTED_EDGE('',*,*,#8929,.T.);
#12461=ORIENTED_EDGE('',*,*,#8909,.T.);
#12462=ORIENTED_EDGE('',*,*,#8929,.F.);
#12463=ORIENTED_EDGE('',*,*,#8921,.T.);
#12464=ORIENTED_EDGE('',*,*,#8930,.T.);
#12465=ORIENTED_EDGE('',*,*,#8910,.T.);
#12466=ORIENTED_EDGE('',*,*,#8930,.F.);
#12467=ORIENTED_EDGE('',*,*,#8920,.T.);
#12468=ORIENTED_EDGE('',*,*,#8931,.T.);
#12469=ORIENTED_EDGE('',*,*,#8911,.T.);
#12470=ORIENTED_EDGE('',*,*,#8931,.F.);
#12471=ORIENTED_EDGE('',*,*,#8919,.T.);
#12472=ORIENTED_EDGE('',*,*,#8932,.T.);
#12473=ORIENTED_EDGE('',*,*,#8912,.T.);
#12474=ORIENTED_EDGE('',*,*,#8932,.F.);
#12475=ORIENTED_EDGE('',*,*,#8918,.T.);
#12476=ORIENTED_EDGE('',*,*,#8523,.T.);
#12477=ORIENTED_EDGE('',*,*,#8670,.F.);
#12478=ORIENTED_EDGE('',*,*,#8933,.F.);
#12479=ORIENTED_EDGE('',*,*,#8528,.F.);
#12480=ORIENTED_EDGE('',*,*,#8934,.F.);
#12481=ORIENTED_EDGE('',*,*,#8935,.F.);
#12482=ORIENTED_EDGE('',*,*,#8936,.F.);
#12483=ORIENTED_EDGE('',*,*,#8937,.F.);
#12484=ORIENTED_EDGE('',*,*,#8938,.F.);
#12485=ORIENTED_EDGE('',*,*,#8669,.F.);
#12486=ORIENTED_EDGE('',*,*,#8939,.F.);
#12487=ORIENTED_EDGE('',*,*,#8529,.F.);
#12488=ORIENTED_EDGE('',*,*,#8933,.T.);
#12489=ORIENTED_EDGE('',*,*,#8668,.F.);
#12490=ORIENTED_EDGE('',*,*,#8940,.F.);
#12491=ORIENTED_EDGE('',*,*,#8941,.F.);
#12492=ORIENTED_EDGE('',*,*,#8942,.F.);
#12493=ORIENTED_EDGE('',*,*,#8943,.F.);
#12494=ORIENTED_EDGE('',*,*,#8944,.F.);
#12495=ORIENTED_EDGE('',*,*,#8530,.F.);
#12496=ORIENTED_EDGE('',*,*,#8939,.T.);
#12497=ORIENTED_EDGE('',*,*,#8924,.T.);
#12498=ORIENTED_EDGE('',*,*,#8671,.F.);
#12499=ORIENTED_EDGE('',*,*,#8938,.T.);
#12500=ORIENTED_EDGE('',*,*,#8945,.T.);
#12501=ORIENTED_EDGE('',*,*,#8925,.T.);
#12502=ORIENTED_EDGE('',*,*,#8945,.F.);
#12503=ORIENTED_EDGE('',*,*,#8937,.T.);
#12504=ORIENTED_EDGE('',*,*,#8946,.T.);
#12505=ORIENTED_EDGE('',*,*,#8926,.T.);
#12506=ORIENTED_EDGE('',*,*,#8946,.F.);
#12507=ORIENTED_EDGE('',*,*,#8936,.T.);
#12508=ORIENTED_EDGE('',*,*,#8947,.T.);
#12509=ORIENTED_EDGE('',*,*,#8927,.T.);
#12510=ORIENTED_EDGE('',*,*,#8947,.F.);
#12511=ORIENTED_EDGE('',*,*,#8935,.T.);
#12512=ORIENTED_EDGE('',*,*,#8948,.T.);
#12513=ORIENTED_EDGE('',*,*,#8928,.T.);
#12514=ORIENTED_EDGE('',*,*,#8948,.F.);
#12515=ORIENTED_EDGE('',*,*,#8934,.T.);
#12516=ORIENTED_EDGE('',*,*,#8527,.T.);
#12517=ORIENTED_EDGE('',*,*,#8666,.F.);
#12518=ORIENTED_EDGE('',*,*,#8949,.F.);
#12519=ORIENTED_EDGE('',*,*,#8532,.F.);
#12520=ORIENTED_EDGE('',*,*,#8950,.F.);
#12521=ORIENTED_EDGE('',*,*,#8951,.F.);
#12522=ORIENTED_EDGE('',*,*,#8952,.F.);
#12523=ORIENTED_EDGE('',*,*,#8953,.F.);
#12524=ORIENTED_EDGE('',*,*,#8954,.F.);
#12525=ORIENTED_EDGE('',*,*,#8665,.F.);
#12526=ORIENTED_EDGE('',*,*,#8955,.F.);
#12527=ORIENTED_EDGE('',*,*,#8533,.F.);
#12528=ORIENTED_EDGE('',*,*,#8949,.T.);
#12529=ORIENTED_EDGE('',*,*,#8664,.F.);
#12530=ORIENTED_EDGE('',*,*,#8956,.F.);
#12531=ORIENTED_EDGE('',*,*,#8957,.F.);
#12532=ORIENTED_EDGE('',*,*,#8958,.F.);
#12533=ORIENTED_EDGE('',*,*,#8959,.F.);
#12534=ORIENTED_EDGE('',*,*,#8960,.F.);
#12535=ORIENTED_EDGE('',*,*,#8534,.F.);
#12536=ORIENTED_EDGE('',*,*,#8955,.T.);
#12537=ORIENTED_EDGE('',*,*,#8940,.T.);
#12538=ORIENTED_EDGE('',*,*,#8667,.F.);
#12539=ORIENTED_EDGE('',*,*,#8954,.T.);
#12540=ORIENTED_EDGE('',*,*,#8961,.T.);
#12541=ORIENTED_EDGE('',*,*,#8941,.T.);
#12542=ORIENTED_EDGE('',*,*,#8961,.F.);
#12543=ORIENTED_EDGE('',*,*,#8953,.T.);
#12544=ORIENTED_EDGE('',*,*,#8962,.T.);
#12545=ORIENTED_EDGE('',*,*,#8942,.T.);
#12546=ORIENTED_EDGE('',*,*,#8962,.F.);
#12547=ORIENTED_EDGE('',*,*,#8952,.T.);
#12548=ORIENTED_EDGE('',*,*,#8963,.T.);
#12549=ORIENTED_EDGE('',*,*,#8943,.T.);
#12550=ORIENTED_EDGE('',*,*,#8963,.F.);
#12551=ORIENTED_EDGE('',*,*,#8951,.T.);
#12552=ORIENTED_EDGE('',*,*,#8964,.T.);
#12553=ORIENTED_EDGE('',*,*,#8944,.T.);
#12554=ORIENTED_EDGE('',*,*,#8964,.F.);
#12555=ORIENTED_EDGE('',*,*,#8950,.T.);
#12556=ORIENTED_EDGE('',*,*,#8531,.T.);
#12557=ORIENTED_EDGE('',*,*,#8662,.F.);
#12558=ORIENTED_EDGE('',*,*,#8965,.F.);
#12559=ORIENTED_EDGE('',*,*,#8536,.F.);
#12560=ORIENTED_EDGE('',*,*,#8966,.F.);
#12561=ORIENTED_EDGE('',*,*,#8967,.F.);
#12562=ORIENTED_EDGE('',*,*,#8968,.F.);
#12563=ORIENTED_EDGE('',*,*,#8969,.F.);
#12564=ORIENTED_EDGE('',*,*,#8970,.F.);
#12565=ORIENTED_EDGE('',*,*,#8661,.F.);
#12566=ORIENTED_EDGE('',*,*,#8971,.F.);
#12567=ORIENTED_EDGE('',*,*,#8537,.F.);
#12568=ORIENTED_EDGE('',*,*,#8965,.T.);
#12569=ORIENTED_EDGE('',*,*,#8660,.F.);
#12570=ORIENTED_EDGE('',*,*,#8972,.F.);
#12571=ORIENTED_EDGE('',*,*,#8973,.F.);
#12572=ORIENTED_EDGE('',*,*,#8974,.F.);
#12573=ORIENTED_EDGE('',*,*,#8975,.F.);
#12574=ORIENTED_EDGE('',*,*,#8976,.F.);
#12575=ORIENTED_EDGE('',*,*,#8538,.F.);
#12576=ORIENTED_EDGE('',*,*,#8971,.T.);
#12577=ORIENTED_EDGE('',*,*,#8956,.T.);
#12578=ORIENTED_EDGE('',*,*,#8663,.F.);
#12579=ORIENTED_EDGE('',*,*,#8970,.T.);
#12580=ORIENTED_EDGE('',*,*,#8977,.T.);
#12581=ORIENTED_EDGE('',*,*,#8957,.T.);
#12582=ORIENTED_EDGE('',*,*,#8977,.F.);
#12583=ORIENTED_EDGE('',*,*,#8969,.T.);
#12584=ORIENTED_EDGE('',*,*,#8978,.T.);
#12585=ORIENTED_EDGE('',*,*,#8958,.T.);
#12586=ORIENTED_EDGE('',*,*,#8978,.F.);
#12587=ORIENTED_EDGE('',*,*,#8968,.T.);
#12588=ORIENTED_EDGE('',*,*,#8979,.T.);
#12589=ORIENTED_EDGE('',*,*,#8959,.T.);
#12590=ORIENTED_EDGE('',*,*,#8979,.F.);
#12591=ORIENTED_EDGE('',*,*,#8967,.T.);
#12592=ORIENTED_EDGE('',*,*,#8980,.T.);
#12593=ORIENTED_EDGE('',*,*,#8960,.T.);
#12594=ORIENTED_EDGE('',*,*,#8980,.F.);
#12595=ORIENTED_EDGE('',*,*,#8966,.T.);
#12596=ORIENTED_EDGE('',*,*,#8535,.T.);
#12597=ORIENTED_EDGE('',*,*,#8658,.F.);
#12598=ORIENTED_EDGE('',*,*,#8981,.F.);
#12599=ORIENTED_EDGE('',*,*,#8540,.F.);
#12600=ORIENTED_EDGE('',*,*,#8982,.F.);
#12601=ORIENTED_EDGE('',*,*,#8983,.F.);
#12602=ORIENTED_EDGE('',*,*,#8984,.F.);
#12603=ORIENTED_EDGE('',*,*,#8985,.F.);
#12604=ORIENTED_EDGE('',*,*,#8986,.F.);
#12605=ORIENTED_EDGE('',*,*,#8657,.F.);
#12606=ORIENTED_EDGE('',*,*,#8987,.F.);
#12607=ORIENTED_EDGE('',*,*,#8541,.F.);
#12608=ORIENTED_EDGE('',*,*,#8981,.T.);
#12609=ORIENTED_EDGE('',*,*,#8656,.F.);
#12610=ORIENTED_EDGE('',*,*,#8988,.F.);
#12611=ORIENTED_EDGE('',*,*,#8989,.F.);
#12612=ORIENTED_EDGE('',*,*,#8990,.F.);
#12613=ORIENTED_EDGE('',*,*,#8991,.F.);
#12614=ORIENTED_EDGE('',*,*,#8992,.F.);
#12615=ORIENTED_EDGE('',*,*,#8542,.F.);
#12616=ORIENTED_EDGE('',*,*,#8987,.T.);
#12617=ORIENTED_EDGE('',*,*,#8972,.T.);
#12618=ORIENTED_EDGE('',*,*,#8659,.F.);
#12619=ORIENTED_EDGE('',*,*,#8986,.T.);
#12620=ORIENTED_EDGE('',*,*,#8993,.T.);
#12621=ORIENTED_EDGE('',*,*,#8973,.T.);
#12622=ORIENTED_EDGE('',*,*,#8993,.F.);
#12623=ORIENTED_EDGE('',*,*,#8985,.T.);
#12624=ORIENTED_EDGE('',*,*,#8994,.T.);
#12625=ORIENTED_EDGE('',*,*,#8974,.T.);
#12626=ORIENTED_EDGE('',*,*,#8994,.F.);
#12627=ORIENTED_EDGE('',*,*,#8984,.T.);
#12628=ORIENTED_EDGE('',*,*,#8995,.T.);
#12629=ORIENTED_EDGE('',*,*,#8975,.T.);
#12630=ORIENTED_EDGE('',*,*,#8995,.F.);
#12631=ORIENTED_EDGE('',*,*,#8983,.T.);
#12632=ORIENTED_EDGE('',*,*,#8996,.T.);
#12633=ORIENTED_EDGE('',*,*,#8976,.T.);
#12634=ORIENTED_EDGE('',*,*,#8996,.F.);
#12635=ORIENTED_EDGE('',*,*,#8982,.T.);
#12636=ORIENTED_EDGE('',*,*,#8539,.T.);
#12637=ORIENTED_EDGE('',*,*,#8654,.F.);
#12638=ORIENTED_EDGE('',*,*,#8997,.F.);
#12639=ORIENTED_EDGE('',*,*,#8544,.F.);
#12640=ORIENTED_EDGE('',*,*,#8998,.F.);
#12641=ORIENTED_EDGE('',*,*,#8999,.F.);
#12642=ORIENTED_EDGE('',*,*,#9000,.F.);
#12643=ORIENTED_EDGE('',*,*,#9001,.F.);
#12644=ORIENTED_EDGE('',*,*,#9002,.F.);
#12645=ORIENTED_EDGE('',*,*,#8653,.F.);
#12646=ORIENTED_EDGE('',*,*,#9003,.F.);
#12647=ORIENTED_EDGE('',*,*,#8545,.F.);
#12648=ORIENTED_EDGE('',*,*,#8997,.T.);
#12649=ORIENTED_EDGE('',*,*,#8652,.F.);
#12650=ORIENTED_EDGE('',*,*,#9004,.F.);
#12651=ORIENTED_EDGE('',*,*,#9005,.F.);
#12652=ORIENTED_EDGE('',*,*,#9006,.F.);
#12653=ORIENTED_EDGE('',*,*,#9007,.F.);
#12654=ORIENTED_EDGE('',*,*,#9008,.F.);
#12655=ORIENTED_EDGE('',*,*,#8546,.F.);
#12656=ORIENTED_EDGE('',*,*,#9003,.T.);
#12657=ORIENTED_EDGE('',*,*,#8988,.T.);
#12658=ORIENTED_EDGE('',*,*,#8655,.F.);
#12659=ORIENTED_EDGE('',*,*,#9002,.T.);
#12660=ORIENTED_EDGE('',*,*,#9009,.T.);
#12661=ORIENTED_EDGE('',*,*,#8989,.T.);
#12662=ORIENTED_EDGE('',*,*,#9009,.F.);
#12663=ORIENTED_EDGE('',*,*,#9001,.T.);
#12664=ORIENTED_EDGE('',*,*,#9010,.T.);
#12665=ORIENTED_EDGE('',*,*,#8990,.T.);
#12666=ORIENTED_EDGE('',*,*,#9010,.F.);
#12667=ORIENTED_EDGE('',*,*,#9000,.T.);
#12668=ORIENTED_EDGE('',*,*,#9011,.T.);
#12669=ORIENTED_EDGE('',*,*,#8991,.T.);
#12670=ORIENTED_EDGE('',*,*,#9011,.F.);
#12671=ORIENTED_EDGE('',*,*,#8999,.T.);
#12672=ORIENTED_EDGE('',*,*,#9012,.T.);
#12673=ORIENTED_EDGE('',*,*,#8992,.T.);
#12674=ORIENTED_EDGE('',*,*,#9012,.F.);
#12675=ORIENTED_EDGE('',*,*,#8998,.T.);
#12676=ORIENTED_EDGE('',*,*,#8543,.T.);
#12677=ORIENTED_EDGE('',*,*,#8650,.F.);
#12678=ORIENTED_EDGE('',*,*,#9013,.F.);
#12679=ORIENTED_EDGE('',*,*,#8548,.F.);
#12680=ORIENTED_EDGE('',*,*,#9014,.F.);
#12681=ORIENTED_EDGE('',*,*,#9015,.F.);
#12682=ORIENTED_EDGE('',*,*,#9016,.F.);
#12683=ORIENTED_EDGE('',*,*,#9017,.F.);
#12684=ORIENTED_EDGE('',*,*,#9018,.F.);
#12685=ORIENTED_EDGE('',*,*,#8649,.F.);
#12686=ORIENTED_EDGE('',*,*,#9019,.F.);
#12687=ORIENTED_EDGE('',*,*,#8549,.F.);
#12688=ORIENTED_EDGE('',*,*,#9013,.T.);
#12689=ORIENTED_EDGE('',*,*,#8648,.F.);
#12690=ORIENTED_EDGE('',*,*,#9020,.F.);
#12691=ORIENTED_EDGE('',*,*,#9021,.F.);
#12692=ORIENTED_EDGE('',*,*,#9022,.F.);
#12693=ORIENTED_EDGE('',*,*,#9023,.F.);
#12694=ORIENTED_EDGE('',*,*,#9024,.F.);
#12695=ORIENTED_EDGE('',*,*,#8550,.F.);
#12696=ORIENTED_EDGE('',*,*,#9019,.T.);
#12697=ORIENTED_EDGE('',*,*,#9004,.T.);
#12698=ORIENTED_EDGE('',*,*,#8651,.F.);
#12699=ORIENTED_EDGE('',*,*,#9018,.T.);
#12700=ORIENTED_EDGE('',*,*,#9025,.T.);
#12701=ORIENTED_EDGE('',*,*,#9005,.T.);
#12702=ORIENTED_EDGE('',*,*,#9025,.F.);
#12703=ORIENTED_EDGE('',*,*,#9017,.T.);
#12704=ORIENTED_EDGE('',*,*,#9026,.T.);
#12705=ORIENTED_EDGE('',*,*,#9006,.T.);
#12706=ORIENTED_EDGE('',*,*,#9026,.F.);
#12707=ORIENTED_EDGE('',*,*,#9016,.T.);
#12708=ORIENTED_EDGE('',*,*,#9027,.T.);
#12709=ORIENTED_EDGE('',*,*,#9007,.T.);
#12710=ORIENTED_EDGE('',*,*,#9027,.F.);
#12711=ORIENTED_EDGE('',*,*,#9015,.T.);
#12712=ORIENTED_EDGE('',*,*,#9028,.T.);
#12713=ORIENTED_EDGE('',*,*,#9008,.T.);
#12714=ORIENTED_EDGE('',*,*,#9028,.F.);
#12715=ORIENTED_EDGE('',*,*,#9014,.T.);
#12716=ORIENTED_EDGE('',*,*,#8547,.T.);
#12717=ORIENTED_EDGE('',*,*,#8646,.F.);
#12718=ORIENTED_EDGE('',*,*,#9029,.F.);
#12719=ORIENTED_EDGE('',*,*,#8552,.F.);
#12720=ORIENTED_EDGE('',*,*,#9030,.F.);
#12721=ORIENTED_EDGE('',*,*,#9031,.F.);
#12722=ORIENTED_EDGE('',*,*,#9032,.F.);
#12723=ORIENTED_EDGE('',*,*,#9033,.F.);
#12724=ORIENTED_EDGE('',*,*,#9034,.F.);
#12725=ORIENTED_EDGE('',*,*,#8645,.F.);
#12726=ORIENTED_EDGE('',*,*,#9035,.F.);
#12727=ORIENTED_EDGE('',*,*,#8553,.F.);
#12728=ORIENTED_EDGE('',*,*,#9029,.T.);
#12729=ORIENTED_EDGE('',*,*,#8644,.F.);
#12730=ORIENTED_EDGE('',*,*,#9036,.F.);
#12731=ORIENTED_EDGE('',*,*,#9037,.F.);
#12732=ORIENTED_EDGE('',*,*,#9038,.F.);
#12733=ORIENTED_EDGE('',*,*,#9039,.F.);
#12734=ORIENTED_EDGE('',*,*,#9040,.F.);
#12735=ORIENTED_EDGE('',*,*,#8554,.F.);
#12736=ORIENTED_EDGE('',*,*,#9035,.T.);
#12737=ORIENTED_EDGE('',*,*,#9020,.T.);
#12738=ORIENTED_EDGE('',*,*,#8647,.F.);
#12739=ORIENTED_EDGE('',*,*,#9034,.T.);
#12740=ORIENTED_EDGE('',*,*,#9041,.T.);
#12741=ORIENTED_EDGE('',*,*,#9021,.T.);
#12742=ORIENTED_EDGE('',*,*,#9041,.F.);
#12743=ORIENTED_EDGE('',*,*,#9033,.T.);
#12744=ORIENTED_EDGE('',*,*,#9042,.T.);
#12745=ORIENTED_EDGE('',*,*,#9022,.T.);
#12746=ORIENTED_EDGE('',*,*,#9042,.F.);
#12747=ORIENTED_EDGE('',*,*,#9032,.T.);
#12748=ORIENTED_EDGE('',*,*,#9043,.T.);
#12749=ORIENTED_EDGE('',*,*,#9023,.T.);
#12750=ORIENTED_EDGE('',*,*,#9043,.F.);
#12751=ORIENTED_EDGE('',*,*,#9031,.T.);
#12752=ORIENTED_EDGE('',*,*,#9044,.T.);
#12753=ORIENTED_EDGE('',*,*,#9024,.T.);
#12754=ORIENTED_EDGE('',*,*,#9044,.F.);
#12755=ORIENTED_EDGE('',*,*,#9030,.T.);
#12756=ORIENTED_EDGE('',*,*,#8551,.T.);
#12757=ORIENTED_EDGE('',*,*,#8642,.F.);
#12758=ORIENTED_EDGE('',*,*,#9045,.F.);
#12759=ORIENTED_EDGE('',*,*,#8556,.F.);
#12760=ORIENTED_EDGE('',*,*,#9046,.F.);
#12761=ORIENTED_EDGE('',*,*,#9047,.F.);
#12762=ORIENTED_EDGE('',*,*,#9048,.F.);
#12763=ORIENTED_EDGE('',*,*,#9049,.F.);
#12764=ORIENTED_EDGE('',*,*,#9050,.F.);
#12765=ORIENTED_EDGE('',*,*,#8641,.F.);
#12766=ORIENTED_EDGE('',*,*,#9051,.F.);
#12767=ORIENTED_EDGE('',*,*,#8557,.F.);
#12768=ORIENTED_EDGE('',*,*,#9045,.T.);
#12769=ORIENTED_EDGE('',*,*,#8640,.F.);
#12770=ORIENTED_EDGE('',*,*,#9052,.F.);
#12771=ORIENTED_EDGE('',*,*,#9053,.F.);
#12772=ORIENTED_EDGE('',*,*,#9054,.F.);
#12773=ORIENTED_EDGE('',*,*,#9055,.F.);
#12774=ORIENTED_EDGE('',*,*,#9056,.F.);
#12775=ORIENTED_EDGE('',*,*,#8558,.F.);
#12776=ORIENTED_EDGE('',*,*,#9051,.T.);
#12777=ORIENTED_EDGE('',*,*,#9036,.T.);
#12778=ORIENTED_EDGE('',*,*,#8643,.F.);
#12779=ORIENTED_EDGE('',*,*,#9050,.T.);
#12780=ORIENTED_EDGE('',*,*,#9057,.T.);
#12781=ORIENTED_EDGE('',*,*,#9037,.T.);
#12782=ORIENTED_EDGE('',*,*,#9057,.F.);
#12783=ORIENTED_EDGE('',*,*,#9049,.T.);
#12784=ORIENTED_EDGE('',*,*,#9058,.T.);
#12785=ORIENTED_EDGE('',*,*,#9038,.T.);
#12786=ORIENTED_EDGE('',*,*,#9058,.F.);
#12787=ORIENTED_EDGE('',*,*,#9048,.T.);
#12788=ORIENTED_EDGE('',*,*,#9059,.T.);
#12789=ORIENTED_EDGE('',*,*,#9039,.T.);
#12790=ORIENTED_EDGE('',*,*,#9059,.F.);
#12791=ORIENTED_EDGE('',*,*,#9047,.T.);
#12792=ORIENTED_EDGE('',*,*,#9060,.T.);
#12793=ORIENTED_EDGE('',*,*,#9040,.T.);
#12794=ORIENTED_EDGE('',*,*,#9060,.F.);
#12795=ORIENTED_EDGE('',*,*,#9046,.T.);
#12796=ORIENTED_EDGE('',*,*,#8555,.T.);
#12797=ORIENTED_EDGE('',*,*,#8638,.F.);
#12798=ORIENTED_EDGE('',*,*,#9061,.F.);
#12799=ORIENTED_EDGE('',*,*,#8560,.F.);
#12800=ORIENTED_EDGE('',*,*,#9062,.F.);
#12801=ORIENTED_EDGE('',*,*,#9063,.F.);
#12802=ORIENTED_EDGE('',*,*,#9064,.F.);
#12803=ORIENTED_EDGE('',*,*,#9065,.F.);
#12804=ORIENTED_EDGE('',*,*,#9066,.F.);
#12805=ORIENTED_EDGE('',*,*,#8637,.F.);
#12806=ORIENTED_EDGE('',*,*,#9067,.F.);
#12807=ORIENTED_EDGE('',*,*,#8561,.F.);
#12808=ORIENTED_EDGE('',*,*,#9061,.T.);
#12809=ORIENTED_EDGE('',*,*,#8636,.F.);
#12810=ORIENTED_EDGE('',*,*,#9068,.F.);
#12811=ORIENTED_EDGE('',*,*,#9069,.F.);
#12812=ORIENTED_EDGE('',*,*,#9070,.F.);
#12813=ORIENTED_EDGE('',*,*,#9071,.F.);
#12814=ORIENTED_EDGE('',*,*,#9072,.F.);
#12815=ORIENTED_EDGE('',*,*,#8562,.F.);
#12816=ORIENTED_EDGE('',*,*,#9067,.T.);
#12817=ORIENTED_EDGE('',*,*,#9052,.T.);
#12818=ORIENTED_EDGE('',*,*,#8639,.F.);
#12819=ORIENTED_EDGE('',*,*,#9066,.T.);
#12820=ORIENTED_EDGE('',*,*,#9073,.T.);
#12821=ORIENTED_EDGE('',*,*,#9053,.T.);
#12822=ORIENTED_EDGE('',*,*,#9073,.F.);
#12823=ORIENTED_EDGE('',*,*,#9065,.T.);
#12824=ORIENTED_EDGE('',*,*,#9074,.T.);
#12825=ORIENTED_EDGE('',*,*,#9054,.T.);
#12826=ORIENTED_EDGE('',*,*,#9074,.F.);
#12827=ORIENTED_EDGE('',*,*,#9064,.T.);
#12828=ORIENTED_EDGE('',*,*,#9075,.T.);
#12829=ORIENTED_EDGE('',*,*,#9055,.T.);
#12830=ORIENTED_EDGE('',*,*,#9075,.F.);
#12831=ORIENTED_EDGE('',*,*,#9063,.T.);
#12832=ORIENTED_EDGE('',*,*,#9076,.T.);
#12833=ORIENTED_EDGE('',*,*,#9056,.T.);
#12834=ORIENTED_EDGE('',*,*,#9076,.F.);
#12835=ORIENTED_EDGE('',*,*,#9062,.T.);
#12836=ORIENTED_EDGE('',*,*,#8559,.T.);
#12837=ORIENTED_EDGE('',*,*,#8634,.F.);
#12838=ORIENTED_EDGE('',*,*,#9077,.F.);
#12839=ORIENTED_EDGE('',*,*,#8564,.F.);
#12840=ORIENTED_EDGE('',*,*,#9078,.F.);
#12841=ORIENTED_EDGE('',*,*,#9079,.F.);
#12842=ORIENTED_EDGE('',*,*,#9080,.F.);
#12843=ORIENTED_EDGE('',*,*,#9081,.F.);
#12844=ORIENTED_EDGE('',*,*,#9082,.F.);
#12845=ORIENTED_EDGE('',*,*,#8633,.F.);
#12846=ORIENTED_EDGE('',*,*,#9083,.F.);
#12847=ORIENTED_EDGE('',*,*,#8565,.F.);
#12848=ORIENTED_EDGE('',*,*,#9077,.T.);
#12849=ORIENTED_EDGE('',*,*,#8632,.F.);
#12850=ORIENTED_EDGE('',*,*,#9084,.F.);
#12851=ORIENTED_EDGE('',*,*,#9085,.F.);
#12852=ORIENTED_EDGE('',*,*,#9086,.F.);
#12853=ORIENTED_EDGE('',*,*,#9087,.F.);
#12854=ORIENTED_EDGE('',*,*,#9088,.F.);
#12855=ORIENTED_EDGE('',*,*,#8566,.F.);
#12856=ORIENTED_EDGE('',*,*,#9083,.T.);
#12857=ORIENTED_EDGE('',*,*,#9068,.T.);
#12858=ORIENTED_EDGE('',*,*,#8635,.F.);
#12859=ORIENTED_EDGE('',*,*,#9082,.T.);
#12860=ORIENTED_EDGE('',*,*,#9089,.T.);
#12861=ORIENTED_EDGE('',*,*,#9069,.T.);
#12862=ORIENTED_EDGE('',*,*,#9089,.F.);
#12863=ORIENTED_EDGE('',*,*,#9081,.T.);
#12864=ORIENTED_EDGE('',*,*,#9090,.T.);
#12865=ORIENTED_EDGE('',*,*,#9070,.T.);
#12866=ORIENTED_EDGE('',*,*,#9090,.F.);
#12867=ORIENTED_EDGE('',*,*,#9080,.T.);
#12868=ORIENTED_EDGE('',*,*,#9091,.T.);
#12869=ORIENTED_EDGE('',*,*,#9071,.T.);
#12870=ORIENTED_EDGE('',*,*,#9091,.F.);
#12871=ORIENTED_EDGE('',*,*,#9079,.T.);
#12872=ORIENTED_EDGE('',*,*,#9092,.T.);
#12873=ORIENTED_EDGE('',*,*,#9072,.T.);
#12874=ORIENTED_EDGE('',*,*,#9092,.F.);
#12875=ORIENTED_EDGE('',*,*,#9078,.T.);
#12876=ORIENTED_EDGE('',*,*,#8563,.T.);
#12877=ORIENTED_EDGE('',*,*,#8630,.F.);
#12878=ORIENTED_EDGE('',*,*,#9093,.F.);
#12879=ORIENTED_EDGE('',*,*,#8568,.F.);
#12880=ORIENTED_EDGE('',*,*,#9094,.F.);
#12881=ORIENTED_EDGE('',*,*,#9095,.F.);
#12882=ORIENTED_EDGE('',*,*,#9096,.F.);
#12883=ORIENTED_EDGE('',*,*,#9097,.F.);
#12884=ORIENTED_EDGE('',*,*,#9098,.F.);
#12885=ORIENTED_EDGE('',*,*,#8629,.F.);
#12886=ORIENTED_EDGE('',*,*,#9099,.F.);
#12887=ORIENTED_EDGE('',*,*,#8569,.F.);
#12888=ORIENTED_EDGE('',*,*,#9093,.T.);
#12889=ORIENTED_EDGE('',*,*,#8628,.F.);
#12890=ORIENTED_EDGE('',*,*,#9100,.F.);
#12891=ORIENTED_EDGE('',*,*,#9101,.F.);
#12892=ORIENTED_EDGE('',*,*,#9102,.F.);
#12893=ORIENTED_EDGE('',*,*,#9103,.F.);
#12894=ORIENTED_EDGE('',*,*,#9104,.F.);
#12895=ORIENTED_EDGE('',*,*,#8570,.F.);
#12896=ORIENTED_EDGE('',*,*,#9099,.T.);
#12897=ORIENTED_EDGE('',*,*,#9084,.T.);
#12898=ORIENTED_EDGE('',*,*,#8631,.F.);
#12899=ORIENTED_EDGE('',*,*,#9098,.T.);
#12900=ORIENTED_EDGE('',*,*,#9105,.T.);
#12901=ORIENTED_EDGE('',*,*,#9085,.T.);
#12902=ORIENTED_EDGE('',*,*,#9105,.F.);
#12903=ORIENTED_EDGE('',*,*,#9097,.T.);
#12904=ORIENTED_EDGE('',*,*,#9106,.T.);
#12905=ORIENTED_EDGE('',*,*,#9086,.T.);
#12906=ORIENTED_EDGE('',*,*,#9106,.F.);
#12907=ORIENTED_EDGE('',*,*,#9096,.T.);
#12908=ORIENTED_EDGE('',*,*,#9107,.T.);
#12909=ORIENTED_EDGE('',*,*,#9087,.T.);
#12910=ORIENTED_EDGE('',*,*,#9107,.F.);
#12911=ORIENTED_EDGE('',*,*,#9095,.T.);
#12912=ORIENTED_EDGE('',*,*,#9108,.T.);
#12913=ORIENTED_EDGE('',*,*,#9088,.T.);
#12914=ORIENTED_EDGE('',*,*,#9108,.F.);
#12915=ORIENTED_EDGE('',*,*,#9094,.T.);
#12916=ORIENTED_EDGE('',*,*,#8567,.T.);
#12917=ORIENTED_EDGE('',*,*,#8626,.F.);
#12918=ORIENTED_EDGE('',*,*,#9109,.F.);
#12919=ORIENTED_EDGE('',*,*,#8572,.F.);
#12920=ORIENTED_EDGE('',*,*,#9110,.F.);
#12921=ORIENTED_EDGE('',*,*,#9111,.F.);
#12922=ORIENTED_EDGE('',*,*,#9112,.F.);
#12923=ORIENTED_EDGE('',*,*,#9113,.F.);
#12924=ORIENTED_EDGE('',*,*,#9114,.F.);
#12925=ORIENTED_EDGE('',*,*,#8625,.F.);
#12926=ORIENTED_EDGE('',*,*,#9115,.F.);
#12927=ORIENTED_EDGE('',*,*,#8573,.F.);
#12928=ORIENTED_EDGE('',*,*,#9109,.T.);
#12929=ORIENTED_EDGE('',*,*,#8624,.F.);
#12930=ORIENTED_EDGE('',*,*,#9116,.F.);
#12931=ORIENTED_EDGE('',*,*,#9117,.F.);
#12932=ORIENTED_EDGE('',*,*,#9118,.F.);
#12933=ORIENTED_EDGE('',*,*,#9119,.F.);
#12934=ORIENTED_EDGE('',*,*,#9120,.F.);
#12935=ORIENTED_EDGE('',*,*,#8574,.F.);
#12936=ORIENTED_EDGE('',*,*,#9115,.T.);
#12937=ORIENTED_EDGE('',*,*,#9100,.T.);
#12938=ORIENTED_EDGE('',*,*,#8627,.F.);
#12939=ORIENTED_EDGE('',*,*,#9114,.T.);
#12940=ORIENTED_EDGE('',*,*,#9121,.T.);
#12941=ORIENTED_EDGE('',*,*,#9101,.T.);
#12942=ORIENTED_EDGE('',*,*,#9121,.F.);
#12943=ORIENTED_EDGE('',*,*,#9113,.T.);
#12944=ORIENTED_EDGE('',*,*,#9122,.T.);
#12945=ORIENTED_EDGE('',*,*,#9102,.T.);
#12946=ORIENTED_EDGE('',*,*,#9122,.F.);
#12947=ORIENTED_EDGE('',*,*,#9112,.T.);
#12948=ORIENTED_EDGE('',*,*,#9123,.T.);
#12949=ORIENTED_EDGE('',*,*,#9103,.T.);
#12950=ORIENTED_EDGE('',*,*,#9123,.F.);
#12951=ORIENTED_EDGE('',*,*,#9111,.T.);
#12952=ORIENTED_EDGE('',*,*,#9124,.T.);
#12953=ORIENTED_EDGE('',*,*,#9104,.T.);
#12954=ORIENTED_EDGE('',*,*,#9124,.F.);
#12955=ORIENTED_EDGE('',*,*,#9110,.T.);
#12956=ORIENTED_EDGE('',*,*,#8571,.T.);
#12957=ORIENTED_EDGE('',*,*,#8622,.F.);
#12958=ORIENTED_EDGE('',*,*,#9125,.F.);
#12959=ORIENTED_EDGE('',*,*,#8576,.F.);
#12960=ORIENTED_EDGE('',*,*,#9126,.F.);
#12961=ORIENTED_EDGE('',*,*,#9127,.F.);
#12962=ORIENTED_EDGE('',*,*,#9128,.F.);
#12963=ORIENTED_EDGE('',*,*,#9129,.F.);
#12964=ORIENTED_EDGE('',*,*,#9130,.F.);
#12965=ORIENTED_EDGE('',*,*,#8621,.F.);
#12966=ORIENTED_EDGE('',*,*,#9131,.F.);
#12967=ORIENTED_EDGE('',*,*,#8577,.F.);
#12968=ORIENTED_EDGE('',*,*,#9125,.T.);
#12969=ORIENTED_EDGE('',*,*,#8620,.F.);
#12970=ORIENTED_EDGE('',*,*,#9132,.F.);
#12971=ORIENTED_EDGE('',*,*,#9133,.F.);
#12972=ORIENTED_EDGE('',*,*,#9134,.F.);
#12973=ORIENTED_EDGE('',*,*,#9135,.F.);
#12974=ORIENTED_EDGE('',*,*,#9136,.F.);
#12975=ORIENTED_EDGE('',*,*,#8578,.F.);
#12976=ORIENTED_EDGE('',*,*,#9131,.T.);
#12977=ORIENTED_EDGE('',*,*,#9116,.T.);
#12978=ORIENTED_EDGE('',*,*,#8623,.F.);
#12979=ORIENTED_EDGE('',*,*,#9130,.T.);
#12980=ORIENTED_EDGE('',*,*,#9137,.T.);
#12981=ORIENTED_EDGE('',*,*,#9117,.T.);
#12982=ORIENTED_EDGE('',*,*,#9137,.F.);
#12983=ORIENTED_EDGE('',*,*,#9129,.T.);
#12984=ORIENTED_EDGE('',*,*,#9138,.T.);
#12985=ORIENTED_EDGE('',*,*,#9118,.T.);
#12986=ORIENTED_EDGE('',*,*,#9138,.F.);
#12987=ORIENTED_EDGE('',*,*,#9128,.T.);
#12988=ORIENTED_EDGE('',*,*,#9139,.T.);
#12989=ORIENTED_EDGE('',*,*,#9119,.T.);
#12990=ORIENTED_EDGE('',*,*,#9139,.F.);
#12991=ORIENTED_EDGE('',*,*,#9127,.T.);
#12992=ORIENTED_EDGE('',*,*,#9140,.T.);
#12993=ORIENTED_EDGE('',*,*,#9120,.T.);
#12994=ORIENTED_EDGE('',*,*,#9140,.F.);
#12995=ORIENTED_EDGE('',*,*,#9126,.T.);
#12996=ORIENTED_EDGE('',*,*,#8575,.T.);
#12997=ORIENTED_EDGE('',*,*,#8618,.F.);
#12998=ORIENTED_EDGE('',*,*,#9141,.F.);
#12999=ORIENTED_EDGE('',*,*,#8580,.F.);
#13000=ORIENTED_EDGE('',*,*,#9142,.F.);
#13001=ORIENTED_EDGE('',*,*,#9143,.F.);
#13002=ORIENTED_EDGE('',*,*,#9144,.F.);
#13003=ORIENTED_EDGE('',*,*,#9145,.F.);
#13004=ORIENTED_EDGE('',*,*,#9146,.F.);
#13005=ORIENTED_EDGE('',*,*,#8617,.F.);
#13006=ORIENTED_EDGE('',*,*,#9147,.F.);
#13007=ORIENTED_EDGE('',*,*,#8581,.F.);
#13008=ORIENTED_EDGE('',*,*,#9141,.T.);
#13009=ORIENTED_EDGE('',*,*,#8616,.F.);
#13010=ORIENTED_EDGE('',*,*,#9148,.F.);
#13011=ORIENTED_EDGE('',*,*,#9149,.F.);
#13012=ORIENTED_EDGE('',*,*,#9150,.F.);
#13013=ORIENTED_EDGE('',*,*,#9151,.F.);
#13014=ORIENTED_EDGE('',*,*,#9152,.F.);
#13015=ORIENTED_EDGE('',*,*,#8582,.F.);
#13016=ORIENTED_EDGE('',*,*,#9147,.T.);
#13017=ORIENTED_EDGE('',*,*,#9132,.T.);
#13018=ORIENTED_EDGE('',*,*,#8619,.F.);
#13019=ORIENTED_EDGE('',*,*,#9146,.T.);
#13020=ORIENTED_EDGE('',*,*,#9153,.T.);
#13021=ORIENTED_EDGE('',*,*,#9133,.T.);
#13022=ORIENTED_EDGE('',*,*,#9153,.F.);
#13023=ORIENTED_EDGE('',*,*,#9145,.T.);
#13024=ORIENTED_EDGE('',*,*,#9154,.T.);
#13025=ORIENTED_EDGE('',*,*,#9134,.T.);
#13026=ORIENTED_EDGE('',*,*,#9154,.F.);
#13027=ORIENTED_EDGE('',*,*,#9144,.T.);
#13028=ORIENTED_EDGE('',*,*,#9155,.T.);
#13029=ORIENTED_EDGE('',*,*,#9135,.T.);
#13030=ORIENTED_EDGE('',*,*,#9155,.F.);
#13031=ORIENTED_EDGE('',*,*,#9143,.T.);
#13032=ORIENTED_EDGE('',*,*,#9156,.T.);
#13033=ORIENTED_EDGE('',*,*,#9136,.T.);
#13034=ORIENTED_EDGE('',*,*,#9156,.F.);
#13035=ORIENTED_EDGE('',*,*,#9142,.T.);
#13036=ORIENTED_EDGE('',*,*,#8579,.T.);
#13037=ORIENTED_EDGE('',*,*,#8614,.F.);
#13038=ORIENTED_EDGE('',*,*,#9157,.F.);
#13039=ORIENTED_EDGE('',*,*,#8584,.F.);
#13040=ORIENTED_EDGE('',*,*,#9158,.F.);
#13041=ORIENTED_EDGE('',*,*,#9159,.F.);
#13042=ORIENTED_EDGE('',*,*,#9160,.F.);
#13043=ORIENTED_EDGE('',*,*,#9161,.F.);
#13044=ORIENTED_EDGE('',*,*,#9162,.F.);
#13045=ORIENTED_EDGE('',*,*,#8613,.F.);
#13046=ORIENTED_EDGE('',*,*,#9163,.F.);
#13047=ORIENTED_EDGE('',*,*,#8585,.F.);
#13048=ORIENTED_EDGE('',*,*,#9157,.T.);
#13049=ORIENTED_EDGE('',*,*,#8612,.F.);
#13050=ORIENTED_EDGE('',*,*,#9164,.F.);
#13051=ORIENTED_EDGE('',*,*,#9165,.F.);
#13052=ORIENTED_EDGE('',*,*,#9166,.F.);
#13053=ORIENTED_EDGE('',*,*,#9167,.F.);
#13054=ORIENTED_EDGE('',*,*,#9168,.F.);
#13055=ORIENTED_EDGE('',*,*,#8586,.F.);
#13056=ORIENTED_EDGE('',*,*,#9163,.T.);
#13057=ORIENTED_EDGE('',*,*,#9148,.T.);
#13058=ORIENTED_EDGE('',*,*,#8615,.F.);
#13059=ORIENTED_EDGE('',*,*,#9162,.T.);
#13060=ORIENTED_EDGE('',*,*,#9169,.T.);
#13061=ORIENTED_EDGE('',*,*,#9164,.T.);
#13062=ORIENTED_EDGE('',*,*,#8611,.F.);
#13063=ORIENTED_EDGE('',*,*,#9170,.T.);
#13064=ORIENTED_EDGE('',*,*,#9171,.T.);
#13065=ORIENTED_EDGE('',*,*,#9149,.T.);
#13066=ORIENTED_EDGE('',*,*,#9169,.F.);
#13067=ORIENTED_EDGE('',*,*,#9161,.T.);
#13068=ORIENTED_EDGE('',*,*,#9172,.T.);
#13069=ORIENTED_EDGE('',*,*,#9150,.T.);
#13070=ORIENTED_EDGE('',*,*,#9172,.F.);
#13071=ORIENTED_EDGE('',*,*,#9160,.T.);
#13072=ORIENTED_EDGE('',*,*,#9173,.T.);
#13073=ORIENTED_EDGE('',*,*,#9151,.T.);
#13074=ORIENTED_EDGE('',*,*,#9173,.F.);
#13075=ORIENTED_EDGE('',*,*,#9159,.T.);
#13076=ORIENTED_EDGE('',*,*,#9174,.T.);
#13077=ORIENTED_EDGE('',*,*,#9152,.T.);
#13078=ORIENTED_EDGE('',*,*,#9174,.F.);
#13079=ORIENTED_EDGE('',*,*,#9158,.T.);
#13080=ORIENTED_EDGE('',*,*,#8583,.T.);
#13081=ORIENTED_EDGE('',*,*,#8610,.F.);
#13082=ORIENTED_EDGE('',*,*,#9175,.F.);
#13083=ORIENTED_EDGE('',*,*,#8588,.F.);
#13084=ORIENTED_EDGE('',*,*,#9176,.F.);
#13085=ORIENTED_EDGE('',*,*,#9177,.F.);
#13086=ORIENTED_EDGE('',*,*,#9178,.F.);
#13087=ORIENTED_EDGE('',*,*,#9179,.F.);
#13088=ORIENTED_EDGE('',*,*,#9170,.F.);
#13089=ORIENTED_EDGE('',*,*,#8609,.F.);
#13090=ORIENTED_EDGE('',*,*,#9180,.F.);
#13091=ORIENTED_EDGE('',*,*,#8589,.F.);
#13092=ORIENTED_EDGE('',*,*,#9175,.T.);
#13093=ORIENTED_EDGE('',*,*,#8608,.F.);
#13094=ORIENTED_EDGE('',*,*,#9181,.F.);
#13095=ORIENTED_EDGE('',*,*,#9182,.F.);
#13096=ORIENTED_EDGE('',*,*,#9183,.F.);
#13097=ORIENTED_EDGE('',*,*,#9184,.F.);
#13098=ORIENTED_EDGE('',*,*,#9185,.F.);
#13099=ORIENTED_EDGE('',*,*,#8590,.F.);
#13100=ORIENTED_EDGE('',*,*,#9180,.T.);
#13101=ORIENTED_EDGE('',*,*,#9181,.T.);
#13102=ORIENTED_EDGE('',*,*,#8607,.F.);
#13103=ORIENTED_EDGE('',*,*,#9186,.T.);
#13104=ORIENTED_EDGE('',*,*,#9187,.T.);
#13105=ORIENTED_EDGE('',*,*,#9165,.T.);
#13106=ORIENTED_EDGE('',*,*,#9171,.F.);
#13107=ORIENTED_EDGE('',*,*,#9179,.T.);
#13108=ORIENTED_EDGE('',*,*,#9188,.T.);
#13109=ORIENTED_EDGE('',*,*,#9182,.T.);
#13110=ORIENTED_EDGE('',*,*,#9187,.F.);
#13111=ORIENTED_EDGE('',*,*,#9189,.T.);
#13112=ORIENTED_EDGE('',*,*,#9190,.T.);
#13113=ORIENTED_EDGE('',*,*,#9168,.T.);
#13114=ORIENTED_EDGE('',*,*,#9191,.F.);
#13115=ORIENTED_EDGE('',*,*,#9176,.T.);
#13116=ORIENTED_EDGE('',*,*,#8587,.T.);
#13117=ORIENTED_EDGE('',*,*,#9166,.T.);
#13118=ORIENTED_EDGE('',*,*,#9188,.F.);
#13119=ORIENTED_EDGE('',*,*,#9178,.T.);
#13120=ORIENTED_EDGE('',*,*,#9192,.T.);
#13121=ORIENTED_EDGE('',*,*,#9167,.T.);
#13122=ORIENTED_EDGE('',*,*,#9192,.F.);
#13123=ORIENTED_EDGE('',*,*,#9177,.T.);
#13124=ORIENTED_EDGE('',*,*,#9191,.T.);
#13125=ORIENTED_EDGE('',*,*,#8606,.F.);
#13126=ORIENTED_EDGE('',*,*,#9193,.F.);
#13127=ORIENTED_EDGE('',*,*,#8592,.F.);
#13128=ORIENTED_EDGE('',*,*,#9194,.F.);
#13129=ORIENTED_EDGE('',*,*,#9195,.F.);
#13130=ORIENTED_EDGE('',*,*,#9196,.F.);
#13131=ORIENTED_EDGE('',*,*,#9189,.F.);
#13132=ORIENTED_EDGE('',*,*,#9186,.F.);
#13133=ORIENTED_EDGE('',*,*,#8605,.F.);
#13134=ORIENTED_EDGE('',*,*,#9197,.F.);
#13135=ORIENTED_EDGE('',*,*,#8593,.F.);
#13136=ORIENTED_EDGE('',*,*,#9193,.T.);
#13137=ORIENTED_EDGE('',*,*,#8604,.F.);
#13138=ORIENTED_EDGE('',*,*,#8733,.F.);
#13139=ORIENTED_EDGE('',*,*,#8735,.F.);
#13140=ORIENTED_EDGE('',*,*,#8737,.F.);
#13141=ORIENTED_EDGE('',*,*,#8739,.F.);
#13142=ORIENTED_EDGE('',*,*,#8740,.F.);
#13143=ORIENTED_EDGE('',*,*,#8594,.F.);
#13144=ORIENTED_EDGE('',*,*,#9197,.T.);
#13145=ORIENTED_EDGE('',*,*,#9184,.T.);
#13146=ORIENTED_EDGE('',*,*,#9198,.F.);
#13147=ORIENTED_EDGE('',*,*,#9195,.T.);
#13148=ORIENTED_EDGE('',*,*,#9199,.T.);
#13149=ORIENTED_EDGE('',*,*,#9183,.T.);
#13150=ORIENTED_EDGE('',*,*,#9190,.F.);
#13151=ORIENTED_EDGE('',*,*,#9196,.T.);
#13152=ORIENTED_EDGE('',*,*,#9198,.T.);
#13153=ORIENTED_EDGE('',*,*,#9185,.T.);
#13154=ORIENTED_EDGE('',*,*,#9199,.F.);
#13155=ORIENTED_EDGE('',*,*,#9194,.T.);
#13156=ORIENTED_EDGE('',*,*,#8591,.T.);
#13157=ORIENTED_EDGE('',*,*,#9200,.F.);
#13158=ORIENTED_EDGE('',*,*,#9201,.T.);
#13159=ORIENTED_EDGE('',*,*,#9202,.F.);
#13160=ORIENTED_EDGE('',*,*,#9203,.F.);
#13161=ORIENTED_EDGE('',*,*,#9204,.F.);
#13162=ORIENTED_EDGE('',*,*,#9205,.F.);
#13163=ORIENTED_EDGE('',*,*,#9206,.F.);
#13164=ORIENTED_EDGE('',*,*,#9207,.F.);
#13165=ORIENTED_EDGE('',*,*,#9208,.F.);
#13166=ORIENTED_EDGE('',*,*,#9201,.F.);
#13167=ORIENTED_EDGE('',*,*,#9209,.F.);
#13168=ORIENTED_EDGE('',*,*,#9210,.F.);
#13169=ORIENTED_EDGE('',*,*,#9211,.F.);
#13170=ORIENTED_EDGE('',*,*,#9212,.F.);
#13171=ORIENTED_EDGE('',*,*,#9213,.F.);
#13172=ORIENTED_EDGE('',*,*,#9207,.T.);
#13173=ORIENTED_EDGE('',*,*,#9214,.F.);
#13174=ORIENTED_EDGE('',*,*,#9209,.T.);
#13175=ORIENTED_EDGE('',*,*,#9206,.T.);
#13176=ORIENTED_EDGE('',*,*,#9200,.T.);
#13177=ORIENTED_EDGE('',*,*,#9215,.T.);
#13178=ORIENTED_EDGE('',*,*,#9210,.T.);
#13179=ORIENTED_EDGE('',*,*,#9215,.F.);
#13180=ORIENTED_EDGE('',*,*,#9205,.T.);
#13181=ORIENTED_EDGE('',*,*,#9216,.T.);
#13182=ORIENTED_EDGE('',*,*,#9217,.F.);
#13183=ORIENTED_EDGE('',*,*,#9218,.T.);
#13184=ORIENTED_EDGE('',*,*,#9214,.T.);
#13185=ORIENTED_EDGE('',*,*,#9218,.F.);
#13186=ORIENTED_EDGE('',*,*,#9219,.F.);
#13187=ORIENTED_EDGE('',*,*,#9220,.T.);
#13188=ORIENTED_EDGE('',*,*,#9217,.T.);
#13189=ORIENTED_EDGE('',*,*,#9220,.F.);
#13190=ORIENTED_EDGE('',*,*,#9221,.F.);
#13191=ORIENTED_EDGE('',*,*,#9219,.T.);
#13192=ORIENTED_EDGE('',*,*,#9222,.F.);
#13193=ORIENTED_EDGE('',*,*,#9223,.T.);
#13194=ORIENTED_EDGE('',*,*,#9221,.T.);
#13195=ORIENTED_EDGE('',*,*,#9223,.F.);
#13196=ORIENTED_EDGE('',*,*,#9224,.F.);
#13197=ORIENTED_EDGE('',*,*,#9225,.T.);
#13198=ORIENTED_EDGE('',*,*,#9222,.T.);
#13199=ORIENTED_EDGE('',*,*,#9225,.F.);
#13200=ORIENTED_EDGE('',*,*,#9226,.F.);
#13201=ORIENTED_EDGE('',*,*,#9224,.T.);
#13202=ORIENTED_EDGE('',*,*,#9227,.F.);
#13203=ORIENTED_EDGE('',*,*,#9228,.T.);
#13204=ORIENTED_EDGE('',*,*,#9226,.T.);
#13205=ORIENTED_EDGE('',*,*,#9228,.F.);
#13206=ORIENTED_EDGE('',*,*,#9227,.T.);
#13207=ORIENTED_EDGE('',*,*,#9229,.F.);
#13208=ORIENTED_EDGE('',*,*,#9230,.F.);
#13209=ORIENTED_EDGE('',*,*,#9231,.T.);
#13210=ORIENTED_EDGE('',*,*,#9229,.T.);
#13211=ORIENTED_EDGE('',*,*,#9231,.F.);
#13212=ORIENTED_EDGE('',*,*,#9230,.T.);
#13213=ORIENTED_EDGE('',*,*,#9232,.T.);
#13214=ORIENTED_EDGE('',*,*,#9233,.F.);
#13215=ORIENTED_EDGE('',*,*,#9232,.F.);
#13216=ORIENTED_EDGE('',*,*,#9233,.T.);
#13217=ORIENTED_EDGE('',*,*,#9234,.F.);
#13218=ORIENTED_EDGE('',*,*,#9235,.F.);
#13219=ORIENTED_EDGE('',*,*,#9236,.T.);
#13220=ORIENTED_EDGE('',*,*,#9234,.T.);
#13221=ORIENTED_EDGE('',*,*,#9236,.F.);
#13222=ORIENTED_EDGE('',*,*,#9235,.T.);
#13223=ORIENTED_EDGE('',*,*,#9237,.T.);
#13224=ORIENTED_EDGE('',*,*,#9238,.F.);
#13225=ORIENTED_EDGE('',*,*,#9237,.F.);
#13226=ORIENTED_EDGE('',*,*,#9238,.T.);
#13227=ORIENTED_EDGE('',*,*,#9213,.T.);
#13228=ORIENTED_EDGE('',*,*,#9239,.F.);
#13229=ORIENTED_EDGE('',*,*,#9202,.T.);
#13230=ORIENTED_EDGE('',*,*,#9208,.T.);
#13231=ORIENTED_EDGE('',*,*,#9212,.T.);
#13232=ORIENTED_EDGE('',*,*,#9240,.F.);
#13233=ORIENTED_EDGE('',*,*,#9203,.T.);
#13234=ORIENTED_EDGE('',*,*,#9239,.T.);
#13235=ORIENTED_EDGE('',*,*,#9211,.T.);
#13236=ORIENTED_EDGE('',*,*,#9216,.F.);
#13237=ORIENTED_EDGE('',*,*,#9204,.T.);
#13238=ORIENTED_EDGE('',*,*,#9240,.T.);
#13239=ORIENTED_EDGE('',*,*,#9241,.F.);
#13240=ORIENTED_EDGE('',*,*,#9242,.T.);
#13241=ORIENTED_EDGE('',*,*,#9243,.F.);
#13242=ORIENTED_EDGE('',*,*,#9244,.T.);
#13243=ORIENTED_EDGE('',*,*,#9241,.T.);
#13244=ORIENTED_EDGE('',*,*,#9244,.F.);
#13245=ORIENTED_EDGE('',*,*,#9245,.F.);
#13246=ORIENTED_EDGE('',*,*,#9246,.T.);
#13247=ORIENTED_EDGE('',*,*,#9243,.T.);
#13248=ORIENTED_EDGE('',*,*,#9246,.F.);
#13249=ORIENTED_EDGE('',*,*,#9245,.T.);
#13250=ORIENTED_EDGE('',*,*,#9247,.T.);
#13251=ORIENTED_EDGE('',*,*,#9248,.F.);
#13252=ORIENTED_EDGE('',*,*,#9247,.F.);
#13253=ORIENTED_EDGE('',*,*,#9248,.T.);
#13254=ORIENTED_EDGE('',*,*,#9249,.F.);
#13255=ORIENTED_EDGE('',*,*,#9250,.F.);
#13256=ORIENTED_EDGE('',*,*,#9251,.T.);
#13257=ORIENTED_EDGE('',*,*,#9249,.T.);
#13258=ORIENTED_EDGE('',*,*,#9251,.F.);
#13259=ORIENTED_EDGE('',*,*,#9250,.T.);
#13260=ORIENTED_EDGE('',*,*,#9252,.F.);
#13261=ORIENTED_EDGE('',*,*,#9253,.F.);
#13262=ORIENTED_EDGE('',*,*,#9254,.T.);
#13263=ORIENTED_EDGE('',*,*,#9252,.T.);
#13264=ORIENTED_EDGE('',*,*,#9254,.F.);
#13265=ORIENTED_EDGE('',*,*,#9255,.F.);
#13266=ORIENTED_EDGE('',*,*,#9256,.T.);
#13267=ORIENTED_EDGE('',*,*,#9253,.T.);
#13268=ORIENTED_EDGE('',*,*,#9256,.F.);
#13269=ORIENTED_EDGE('',*,*,#9255,.T.);
#13270=ORIENTED_EDGE('',*,*,#9257,.T.);
#13271=ORIENTED_EDGE('',*,*,#9258,.F.);
#13272=ORIENTED_EDGE('',*,*,#9257,.F.);
#13273=ORIENTED_EDGE('',*,*,#9258,.T.);
#13274=ORIENTED_EDGE('',*,*,#9259,.T.);
#13275=ORIENTED_EDGE('',*,*,#9242,.F.);
#13276=ORIENTED_EDGE('',*,*,#9259,.F.);
#13277=ORIENTED_EDGE('',*,*,#9260,.F.);
#13278=ORIENTED_EDGE('',*,*,#9261,.T.);
#13279=ORIENTED_EDGE('',*,*,#9262,.T.);
#13280=ORIENTED_EDGE('',*,*,#9261,.F.);
#13281=ORIENTED_EDGE('',*,*,#9263,.T.);
#13282=ORIENTED_EDGE('',*,*,#9262,.F.);
#13283=ORIENTED_EDGE('',*,*,#9263,.F.);
#13284=ORIENTED_EDGE('',*,*,#9264,.T.);
#13285=ORIENTED_EDGE('',*,*,#9265,.F.);
#13286=ORIENTED_EDGE('',*,*,#9264,.F.);
#13287=ORIENTED_EDGE('',*,*,#9266,.T.);
#13288=ORIENTED_EDGE('',*,*,#9265,.T.);
#13289=ORIENTED_EDGE('',*,*,#9267,.F.);
#13290=ORIENTED_EDGE('',*,*,#9268,.T.);
#13291=ORIENTED_EDGE('',*,*,#9269,.T.);
#13292=ORIENTED_EDGE('',*,*,#9268,.F.);
#13293=ORIENTED_EDGE('',*,*,#9270,.F.);
#13294=ORIENTED_EDGE('',*,*,#9267,.T.);
#13295=ORIENTED_EDGE('',*,*,#9271,.F.);
#13296=ORIENTED_EDGE('',*,*,#9272,.T.);
#13297=ORIENTED_EDGE('',*,*,#9270,.T.);
#13298=ORIENTED_EDGE('',*,*,#9272,.F.);
#13299=ORIENTED_EDGE('',*,*,#9271,.T.);
#13300=ORIENTED_EDGE('',*,*,#9273,.T.);
#13301=ORIENTED_EDGE('',*,*,#9266,.F.);
#13302=ORIENTED_EDGE('',*,*,#9273,.F.);
#13303=ORIENTED_EDGE('',*,*,#9260,.T.);
#13304=ORIENTED_EDGE('',*,*,#9269,.F.);
#13305=ORIENTED_EDGE('',*,*,#9274,.F.);
#13306=ORIENTED_EDGE('',*,*,#9275,.F.);
#13307=ORIENTED_EDGE('',*,*,#9276,.F.);
#13308=ORIENTED_EDGE('',*,*,#9277,.T.);
#13309=ORIENTED_EDGE('',*,*,#9278,.F.);
#13310=ORIENTED_EDGE('',*,*,#9279,.F.);
#13311=ORIENTED_EDGE('',*,*,#9280,.F.);
#13312=ORIENTED_EDGE('',*,*,#9274,.T.);
#13313=ORIENTED_EDGE('',*,*,#9281,.T.);
#13314=ORIENTED_EDGE('',*,*,#9282,.T.);
#13315=ORIENTED_EDGE('',*,*,#9283,.F.);
#13316=ORIENTED_EDGE('',*,*,#9284,.F.);
#13317=ORIENTED_EDGE('',*,*,#9285,.F.);
#13318=ORIENTED_EDGE('',*,*,#9278,.T.);
#13319=ORIENTED_EDGE('',*,*,#9286,.T.);
#13320=ORIENTED_EDGE('',*,*,#9287,.T.);
#13321=ORIENTED_EDGE('',*,*,#9288,.F.);
#13322=ORIENTED_EDGE('',*,*,#9289,.F.);
#13323=ORIENTED_EDGE('',*,*,#9290,.F.);
#13324=ORIENTED_EDGE('',*,*,#9283,.T.);
#13325=ORIENTED_EDGE('',*,*,#9291,.T.);
#13326=ORIENTED_EDGE('',*,*,#9292,.T.);
#13327=ORIENTED_EDGE('',*,*,#9293,.F.);
#13328=ORIENTED_EDGE('',*,*,#9294,.F.);
#13329=ORIENTED_EDGE('',*,*,#9295,.F.);
#13330=ORIENTED_EDGE('',*,*,#9288,.T.);
#13331=ORIENTED_EDGE('',*,*,#9296,.T.);
#13332=ORIENTED_EDGE('',*,*,#9297,.T.);
#13333=ORIENTED_EDGE('',*,*,#9298,.F.);
#13334=ORIENTED_EDGE('',*,*,#9299,.F.);
#13335=ORIENTED_EDGE('',*,*,#9300,.F.);
#13336=ORIENTED_EDGE('',*,*,#9293,.T.);
#13337=ORIENTED_EDGE('',*,*,#9301,.T.);
#13338=ORIENTED_EDGE('',*,*,#9302,.T.);
#13339=ORIENTED_EDGE('',*,*,#9303,.T.);
#13340=ORIENTED_EDGE('',*,*,#9304,.T.);
#13341=ORIENTED_EDGE('',*,*,#9305,.T.);
#13342=ORIENTED_EDGE('',*,*,#9306,.T.);
#13343=ORIENTED_EDGE('',*,*,#9307,.T.);
#13344=ORIENTED_EDGE('',*,*,#9308,.T.);
#13345=ORIENTED_EDGE('',*,*,#9309,.T.);
#13346=ORIENTED_EDGE('',*,*,#9310,.T.);
#13347=ORIENTED_EDGE('',*,*,#9311,.T.);
#13348=ORIENTED_EDGE('',*,*,#9312,.F.);
#13349=ORIENTED_EDGE('',*,*,#9313,.T.);
#13350=ORIENTED_EDGE('',*,*,#9314,.T.);
#13351=ORIENTED_EDGE('',*,*,#9315,.T.);
#13352=ORIENTED_EDGE('',*,*,#9316,.T.);
#13353=ORIENTED_EDGE('',*,*,#9317,.T.);
#13354=ORIENTED_EDGE('',*,*,#9318,.T.);
#13355=ORIENTED_EDGE('',*,*,#9298,.T.);
#13356=ORIENTED_EDGE('',*,*,#9319,.T.);
#13357=ORIENTED_EDGE('',*,*,#9320,.T.);
#13358=ORIENTED_EDGE('',*,*,#9321,.F.);
#13359=ORIENTED_EDGE('',*,*,#9322,.F.);
#13360=ORIENTED_EDGE('',*,*,#9323,.F.);
#13361=ORIENTED_EDGE('',*,*,#9324,.T.);
#13362=ORIENTED_EDGE('',*,*,#9325,.F.);
#13363=ORIENTED_EDGE('',*,*,#9326,.T.);
#13364=ORIENTED_EDGE('',*,*,#9321,.T.);
#13365=ORIENTED_EDGE('',*,*,#9327,.F.);
#13366=ORIENTED_EDGE('',*,*,#9328,.F.);
#13367=ORIENTED_EDGE('',*,*,#9311,.F.);
#13368=ORIENTED_EDGE('',*,*,#9310,.F.);
#13369=ORIENTED_EDGE('',*,*,#9309,.F.);
#13370=ORIENTED_EDGE('',*,*,#9308,.F.);
#13371=ORIENTED_EDGE('',*,*,#9307,.F.);
#13372=ORIENTED_EDGE('',*,*,#9306,.F.);
#13373=ORIENTED_EDGE('',*,*,#9305,.F.);
#13374=ORIENTED_EDGE('',*,*,#9329,.F.);
#13375=ORIENTED_EDGE('',*,*,#9275,.T.);
#13376=ORIENTED_EDGE('',*,*,#9280,.T.);
#13377=ORIENTED_EDGE('',*,*,#9279,.T.);
#13378=ORIENTED_EDGE('',*,*,#9285,.T.);
#13379=ORIENTED_EDGE('',*,*,#9284,.T.);
#13380=ORIENTED_EDGE('',*,*,#9290,.T.);
#13381=ORIENTED_EDGE('',*,*,#9289,.T.);
#13382=ORIENTED_EDGE('',*,*,#9295,.T.);
#13383=ORIENTED_EDGE('',*,*,#9294,.T.);
#13384=ORIENTED_EDGE('',*,*,#9300,.T.);
#13385=ORIENTED_EDGE('',*,*,#9299,.T.);
#13386=ORIENTED_EDGE('',*,*,#9323,.T.);
#13387=ORIENTED_EDGE('',*,*,#9322,.T.);
#13388=ORIENTED_EDGE('',*,*,#9326,.F.);
#13389=ORIENTED_EDGE('',*,*,#9330,.T.);
#13390=ORIENTED_EDGE('',*,*,#9331,.T.);
#13391=ORIENTED_EDGE('',*,*,#9332,.T.);
#13392=ORIENTED_EDGE('',*,*,#9276,.T.);
#13393=ORIENTED_EDGE('',*,*,#9329,.T.);
#13394=ORIENTED_EDGE('',*,*,#9333,.F.);
#13395=ORIENTED_EDGE('',*,*,#9324,.F.);
#13396=ORIENTED_EDGE('',*,*,#9320,.F.);
#13397=ORIENTED_EDGE('',*,*,#9319,.F.);
#13398=ORIENTED_EDGE('',*,*,#9302,.F.);
#13399=ORIENTED_EDGE('',*,*,#9301,.F.);
#13400=ORIENTED_EDGE('',*,*,#9297,.F.);
#13401=ORIENTED_EDGE('',*,*,#9296,.F.);
#13402=ORIENTED_EDGE('',*,*,#9292,.F.);
#13403=ORIENTED_EDGE('',*,*,#9291,.F.);
#13404=ORIENTED_EDGE('',*,*,#9287,.F.);
#13405=ORIENTED_EDGE('',*,*,#9286,.F.);
#13406=ORIENTED_EDGE('',*,*,#9282,.F.);
#13407=ORIENTED_EDGE('',*,*,#9281,.F.);
#13408=ORIENTED_EDGE('',*,*,#9277,.F.);
#13409=ORIENTED_EDGE('',*,*,#9332,.F.);
#13410=ORIENTED_EDGE('',*,*,#9334,.T.);
#13411=ORIENTED_EDGE('',*,*,#9303,.F.);
#13412=ORIENTED_EDGE('',*,*,#9318,.F.);
#13413=ORIENTED_EDGE('',*,*,#9317,.F.);
#13414=ORIENTED_EDGE('',*,*,#9316,.F.);
#13415=ORIENTED_EDGE('',*,*,#9315,.F.);
#13416=ORIENTED_EDGE('',*,*,#9314,.F.);
#13417=ORIENTED_EDGE('',*,*,#9313,.F.);
#13418=ORIENTED_EDGE('',*,*,#9335,.F.);
#13419=ORIENTED_EDGE('',*,*,#9336,.F.);
#13420=ORIENTED_EDGE('',*,*,#9337,.F.);
#13421=ORIENTED_EDGE('',*,*,#9338,.F.);
#13422=ORIENTED_EDGE('',*,*,#9339,.F.);
#13423=ORIENTED_EDGE('',*,*,#9340,.F.);
#13424=ORIENTED_EDGE('',*,*,#9341,.F.);
#13425=ORIENTED_EDGE('',*,*,#9342,.F.);
#13426=ORIENTED_EDGE('',*,*,#9343,.T.);
#13427=ORIENTED_EDGE('',*,*,#9344,.F.);
#13428=ORIENTED_EDGE('',*,*,#9343,.F.);
#13429=ORIENTED_EDGE('',*,*,#9341,.T.);
#13430=ORIENTED_EDGE('',*,*,#9345,.T.);
#13431=ORIENTED_EDGE('',*,*,#9346,.T.);
#13432=ORIENTED_EDGE('',*,*,#9347,.F.);
#13433=ORIENTED_EDGE('',*,*,#9340,.T.);
#13434=ORIENTED_EDGE('',*,*,#9348,.T.);
#13435=ORIENTED_EDGE('',*,*,#9349,.T.);
#13436=ORIENTED_EDGE('',*,*,#9345,.F.);
#13437=ORIENTED_EDGE('',*,*,#9339,.T.);
#13438=ORIENTED_EDGE('',*,*,#9350,.T.);
#13439=ORIENTED_EDGE('',*,*,#9351,.T.);
#13440=ORIENTED_EDGE('',*,*,#9348,.F.);
#13441=ORIENTED_EDGE('',*,*,#9352,.T.);
#13442=ORIENTED_EDGE('',*,*,#9353,.F.);
#13443=ORIENTED_EDGE('',*,*,#9352,.F.);
#13444=ORIENTED_EDGE('',*,*,#9338,.T.);
#13445=ORIENTED_EDGE('',*,*,#9354,.T.);
#13446=ORIENTED_EDGE('',*,*,#9355,.T.);
#13447=ORIENTED_EDGE('',*,*,#9350,.F.);
#13448=ORIENTED_EDGE('',*,*,#9337,.T.);
#13449=ORIENTED_EDGE('',*,*,#9356,.T.);
#13450=ORIENTED_EDGE('',*,*,#9357,.T.);
#13451=ORIENTED_EDGE('',*,*,#9354,.F.);
#13452=ORIENTED_EDGE('',*,*,#9336,.T.);
#13453=ORIENTED_EDGE('',*,*,#9342,.T.);
#13454=ORIENTED_EDGE('',*,*,#9347,.T.);
#13455=ORIENTED_EDGE('',*,*,#9358,.T.);
#13456=ORIENTED_EDGE('',*,*,#9356,.F.);
#13457=ORIENTED_EDGE('',*,*,#9351,.F.);
#13458=ORIENTED_EDGE('',*,*,#9355,.F.);
#13459=ORIENTED_EDGE('',*,*,#9357,.F.);
#13460=ORIENTED_EDGE('',*,*,#9358,.F.);
#13461=ORIENTED_EDGE('',*,*,#9346,.F.);
#13462=ORIENTED_EDGE('',*,*,#9349,.F.);
#13463=ORIENTED_EDGE('',*,*,#9353,.T.);
#13464=ORIENTED_EDGE('',*,*,#9359,.F.);
#13465=ORIENTED_EDGE('',*,*,#9334,.F.);
#13466=ORIENTED_EDGE('',*,*,#9331,.F.);
#13467=ORIENTED_EDGE('',*,*,#9360,.T.);
#13468=ORIENTED_EDGE('',*,*,#9359,.T.);
#13469=ORIENTED_EDGE('',*,*,#9360,.F.);
#13470=ORIENTED_EDGE('',*,*,#9330,.F.);
#13471=ORIENTED_EDGE('',*,*,#9304,.F.);
#13472=ORIENTED_EDGE('',*,*,#9328,.T.);
#13473=ORIENTED_EDGE('',*,*,#9361,.F.);
#13474=ORIENTED_EDGE('',*,*,#9362,.F.);
#13475=ORIENTED_EDGE('',*,*,#9335,.T.);
#13476=ORIENTED_EDGE('',*,*,#9312,.T.);
#13477=ORIENTED_EDGE('',*,*,#9363,.F.);
#13478=ORIENTED_EDGE('',*,*,#9364,.T.);
#13479=ORIENTED_EDGE('',*,*,#9361,.T.);
#13480=ORIENTED_EDGE('',*,*,#9327,.T.);
#13481=ORIENTED_EDGE('',*,*,#9325,.T.);
#13482=ORIENTED_EDGE('',*,*,#9333,.T.);
#13483=ORIENTED_EDGE('',*,*,#9362,.T.);
#13484=ORIENTED_EDGE('',*,*,#9364,.F.);
#13485=ORIENTED_EDGE('',*,*,#9365,.F.);
#13486=ORIENTED_EDGE('',*,*,#9363,.T.);
#13487=ORIENTED_EDGE('',*,*,#9366,.F.);
#13488=ORIENTED_EDGE('',*,*,#9367,.T.);
#13489=ORIENTED_EDGE('',*,*,#9365,.T.);
#13490=ORIENTED_EDGE('',*,*,#9367,.F.);
#13491=ORIENTED_EDGE('',*,*,#9368,.F.);
#13492=ORIENTED_EDGE('',*,*,#9369,.T.);
#13493=ORIENTED_EDGE('',*,*,#9366,.T.);
#13494=ORIENTED_EDGE('',*,*,#9369,.F.);
#13495=ORIENTED_EDGE('',*,*,#9368,.T.);
#13496=ORIENTED_EDGE('',*,*,#9370,.T.);
#13497=ORIENTED_EDGE('',*,*,#9371,.F.);
#13498=ORIENTED_EDGE('',*,*,#9370,.F.);
#13499=ORIENTED_EDGE('',*,*,#9371,.T.);
#13500=ORIENTED_EDGE('',*,*,#9344,.T.);
#13501=ORIENTED_EDGE('',*,*,#9372,.T.);
#13502=ORIENTED_EDGE('',*,*,#9373,.T.);
#13503=ORIENTED_EDGE('',*,*,#9374,.F.);
#13504=ORIENTED_EDGE('',*,*,#9373,.F.);
#13505=ORIENTED_EDGE('',*,*,#9375,.F.);
#13506=ORIENTED_EDGE('',*,*,#9374,.T.);
#13507=ORIENTED_EDGE('',*,*,#9376,.F.);
#13508=ORIENTED_EDGE('',*,*,#9377,.T.);
#13509=ORIENTED_EDGE('',*,*,#9375,.T.);
#13510=ORIENTED_EDGE('',*,*,#9377,.F.);
#13511=ORIENTED_EDGE('',*,*,#9378,.F.);
#13512=ORIENTED_EDGE('',*,*,#9379,.T.);
#13513=ORIENTED_EDGE('',*,*,#9376,.T.);
#13514=ORIENTED_EDGE('',*,*,#9379,.F.);
#13515=ORIENTED_EDGE('',*,*,#9378,.T.);
#13516=ORIENTED_EDGE('',*,*,#9380,.T.);
#13517=ORIENTED_EDGE('',*,*,#9381,.F.);
#13518=ORIENTED_EDGE('',*,*,#9380,.F.);
#13519=ORIENTED_EDGE('',*,*,#9381,.T.);
#13520=ORIENTED_EDGE('',*,*,#9382,.F.);
#13521=ORIENTED_EDGE('',*,*,#9383,.F.);
#13522=ORIENTED_EDGE('',*,*,#9384,.T.);
#13523=ORIENTED_EDGE('',*,*,#9382,.T.);
#13524=ORIENTED_EDGE('',*,*,#9384,.F.);
#13525=ORIENTED_EDGE('',*,*,#9372,.F.);
#13526=ORIENTED_EDGE('',*,*,#9385,.T.);
#13527=ORIENTED_EDGE('',*,*,#9383,.T.);
#13528=ORIENTED_EDGE('',*,*,#9385,.F.);
#13529=ORIENTED_EDGE('',*,*,#9386,.F.);
#13530=ORIENTED_EDGE('',*,*,#9387,.T.);
#13531=ORIENTED_EDGE('',*,*,#9388,.T.);
#13532=ORIENTED_EDGE('',*,*,#9387,.F.);
#13533=ORIENTED_EDGE('',*,*,#9389,.F.);
#13534=ORIENTED_EDGE('',*,*,#9386,.T.);
#13535=ORIENTED_EDGE('',*,*,#9390,.F.);
#13536=ORIENTED_EDGE('',*,*,#9391,.T.);
#13537=ORIENTED_EDGE('',*,*,#9389,.T.);
#13538=ORIENTED_EDGE('',*,*,#9391,.F.);
#13539=ORIENTED_EDGE('',*,*,#9392,.F.);
#13540=ORIENTED_EDGE('',*,*,#9393,.T.);
#13541=ORIENTED_EDGE('',*,*,#9390,.T.);
#13542=ORIENTED_EDGE('',*,*,#9393,.F.);
#13543=ORIENTED_EDGE('',*,*,#9394,.F.);
#13544=ORIENTED_EDGE('',*,*,#9392,.T.);
#13545=ORIENTED_EDGE('',*,*,#9395,.F.);
#13546=ORIENTED_EDGE('',*,*,#9396,.T.);
#13547=ORIENTED_EDGE('',*,*,#9394,.T.);
#13548=ORIENTED_EDGE('',*,*,#9396,.F.);
#13549=ORIENTED_EDGE('',*,*,#9397,.F.);
#13550=ORIENTED_EDGE('',*,*,#9398,.T.);
#13551=ORIENTED_EDGE('',*,*,#9395,.T.);
#13552=ORIENTED_EDGE('',*,*,#9398,.F.);
#13553=ORIENTED_EDGE('',*,*,#9397,.T.);
#13554=ORIENTED_EDGE('',*,*,#9399,.T.);
#13555=ORIENTED_EDGE('',*,*,#9400,.F.);
#13556=ORIENTED_EDGE('',*,*,#9399,.F.);
#13557=ORIENTED_EDGE('',*,*,#9400,.T.);
#13558=ORIENTED_EDGE('',*,*,#9388,.F.);
#13559=ORIENTED_EDGE('',*,*,#9401,.F.);
#13560=ORIENTED_EDGE('',*,*,#9402,.T.);
#13561=ORIENTED_EDGE('',*,*,#9403,.F.);
#13562=ORIENTED_EDGE('',*,*,#9402,.F.);
#13563=ORIENTED_EDGE('',*,*,#9404,.F.);
#13564=ORIENTED_EDGE('',*,*,#9405,.T.);
#13565=ORIENTED_EDGE('',*,*,#9406,.T.);
#13566=ORIENTED_EDGE('',*,*,#9405,.F.);
#13567=ORIENTED_EDGE('',*,*,#9406,.F.);
#13568=ORIENTED_EDGE('',*,*,#9401,.T.);
#13569=ORIENTED_EDGE('',*,*,#9407,.F.);
#13570=ORIENTED_EDGE('',*,*,#9408,.T.);
#13571=ORIENTED_EDGE('',*,*,#9409,.T.);
#13572=ORIENTED_EDGE('',*,*,#9408,.F.);
#13573=ORIENTED_EDGE('',*,*,#9410,.T.);
#13574=ORIENTED_EDGE('',*,*,#9409,.F.);
#13575=ORIENTED_EDGE('',*,*,#9410,.F.);
#13576=ORIENTED_EDGE('',*,*,#9411,.T.);
#13577=ORIENTED_EDGE('',*,*,#9412,.F.);
#13578=ORIENTED_EDGE('',*,*,#9411,.F.);
#13579=ORIENTED_EDGE('',*,*,#9413,.F.);
#13580=ORIENTED_EDGE('',*,*,#9404,.T.);
#13581=ORIENTED_EDGE('',*,*,#9414,.T.);
#13582=ORIENTED_EDGE('',*,*,#9412,.T.);
#13583=ORIENTED_EDGE('',*,*,#9415,.F.);
#13584=ORIENTED_EDGE('',*,*,#9416,.T.);
#13585=ORIENTED_EDGE('',*,*,#9417,.T.);
#13586=ORIENTED_EDGE('',*,*,#9416,.F.);
#13587=ORIENTED_EDGE('',*,*,#9415,.T.);
#13588=ORIENTED_EDGE('',*,*,#9418,.T.);
#13589=ORIENTED_EDGE('',*,*,#9419,.F.);
#13590=ORIENTED_EDGE('',*,*,#9418,.F.);
#13591=ORIENTED_EDGE('',*,*,#9420,.F.);
#13592=ORIENTED_EDGE('',*,*,#9419,.T.);
#13593=ORIENTED_EDGE('',*,*,#9420,.T.);
#13594=ORIENTED_EDGE('',*,*,#9421,.T.);
#13595=ORIENTED_EDGE('',*,*,#9422,.F.);
#13596=ORIENTED_EDGE('',*,*,#9421,.F.);
#13597=ORIENTED_EDGE('',*,*,#9422,.T.);
#13598=ORIENTED_EDGE('',*,*,#9423,.T.);
#13599=ORIENTED_EDGE('',*,*,#9424,.F.);
#13600=ORIENTED_EDGE('',*,*,#9423,.F.);
#13601=ORIENTED_EDGE('',*,*,#9403,.T.);
#13602=ORIENTED_EDGE('',*,*,#9424,.T.);
#13603=ORIENTED_EDGE('',*,*,#9425,.F.);
#13604=ORIENTED_EDGE('',*,*,#9426,.T.);
#13605=ORIENTED_EDGE('',*,*,#9413,.T.);
#13606=ORIENTED_EDGE('',*,*,#9426,.F.);
#13607=ORIENTED_EDGE('',*,*,#9427,.F.);
#13608=ORIENTED_EDGE('',*,*,#9428,.T.);
#13609=ORIENTED_EDGE('',*,*,#9425,.T.);
#13610=ORIENTED_EDGE('',*,*,#9428,.F.);
#13611=ORIENTED_EDGE('',*,*,#9427,.T.);
#13612=ORIENTED_EDGE('',*,*,#9429,.T.);
#13613=ORIENTED_EDGE('',*,*,#9430,.F.);
#13614=ORIENTED_EDGE('',*,*,#9429,.F.);
#13615=ORIENTED_EDGE('',*,*,#9430,.T.);
#13616=ORIENTED_EDGE('',*,*,#9431,.F.);
#13617=ORIENTED_EDGE('',*,*,#9414,.F.);
#13618=ORIENTED_EDGE('',*,*,#9432,.T.);
#13619=ORIENTED_EDGE('',*,*,#9431,.T.);
#13620=ORIENTED_EDGE('',*,*,#9432,.F.);
#13621=ORIENTED_EDGE('',*,*,#9407,.T.);
#13622=ORIENTED_EDGE('',*,*,#9433,.F.);
#13623=ORIENTED_EDGE('',*,*,#9417,.F.);
#13624=ORIENTED_EDGE('',*,*,#9434,.T.);
#13625=ORIENTED_EDGE('',*,*,#9433,.T.);
#13626=ORIENTED_EDGE('',*,*,#9434,.F.);
#13627=ORIENTED_EDGE('',*,*,#9435,.F.);
#13628=ORIENTED_EDGE('',*,*,#9436,.T.);
#13629=ORIENTED_EDGE('',*,*,#9437,.T.);
#13630=ORIENTED_EDGE('',*,*,#9436,.F.);
#13631=ORIENTED_EDGE('',*,*,#9435,.T.);
#13632=ORIENTED_EDGE('',*,*,#9438,.T.);
#13633=ORIENTED_EDGE('',*,*,#9439,.F.);
#13634=ORIENTED_EDGE('',*,*,#9438,.F.);
#13635=ORIENTED_EDGE('',*,*,#9440,.F.);
#13636=ORIENTED_EDGE('',*,*,#9439,.T.);
#13637=ORIENTED_EDGE('',*,*,#9441,.F.);
#13638=ORIENTED_EDGE('',*,*,#9442,.T.);
#13639=ORIENTED_EDGE('',*,*,#9440,.T.);
#13640=ORIENTED_EDGE('',*,*,#9442,.F.);
#13641=ORIENTED_EDGE('',*,*,#9443,.F.);
#13642=ORIENTED_EDGE('',*,*,#9441,.T.);
#13643=ORIENTED_EDGE('',*,*,#9444,.F.);
#13644=ORIENTED_EDGE('',*,*,#9445,.T.);
#13645=ORIENTED_EDGE('',*,*,#9443,.T.);
#13646=ORIENTED_EDGE('',*,*,#9445,.F.);
#13647=ORIENTED_EDGE('',*,*,#9446,.F.);
#13648=ORIENTED_EDGE('',*,*,#9444,.T.);
#13649=ORIENTED_EDGE('',*,*,#9447,.F.);
#13650=ORIENTED_EDGE('',*,*,#9448,.T.);
#13651=ORIENTED_EDGE('',*,*,#9446,.T.);
#13652=ORIENTED_EDGE('',*,*,#9448,.F.);
#13653=ORIENTED_EDGE('',*,*,#9449,.F.);
#13654=ORIENTED_EDGE('',*,*,#9450,.T.);
#13655=ORIENTED_EDGE('',*,*,#9447,.T.);
#13656=ORIENTED_EDGE('',*,*,#9450,.F.);
#13657=ORIENTED_EDGE('',*,*,#9449,.T.);
#13658=ORIENTED_EDGE('',*,*,#9451,.T.);
#13659=ORIENTED_EDGE('',*,*,#9452,.F.);
#13660=ORIENTED_EDGE('',*,*,#9451,.F.);
#13661=ORIENTED_EDGE('',*,*,#9452,.T.);
#13662=ORIENTED_EDGE('',*,*,#9453,.F.);
#13663=ORIENTED_EDGE('',*,*,#9454,.F.);
#13664=ORIENTED_EDGE('',*,*,#9455,.T.);
#13665=ORIENTED_EDGE('',*,*,#9453,.T.);
#13666=ORIENTED_EDGE('',*,*,#9455,.F.);
#13667=ORIENTED_EDGE('',*,*,#9454,.T.);
#13668=ORIENTED_EDGE('',*,*,#9456,.F.);
#13669=ORIENTED_EDGE('',*,*,#9457,.F.);
#13670=ORIENTED_EDGE('',*,*,#9458,.T.);
#13671=ORIENTED_EDGE('',*,*,#9456,.T.);
#13672=ORIENTED_EDGE('',*,*,#9458,.F.);
#13673=ORIENTED_EDGE('',*,*,#9457,.T.);
#13674=ORIENTED_EDGE('',*,*,#9459,.F.);
#13675=ORIENTED_EDGE('',*,*,#9437,.F.);
#13676=ORIENTED_EDGE('',*,*,#9460,.T.);
#13677=ORIENTED_EDGE('',*,*,#9459,.T.);
#13678=ORIENTED_EDGE('',*,*,#9460,.F.);
#13679=ORIENTED_EDGE('',*,*,#9461,.F.);
#13680=ORIENTED_EDGE('',*,*,#9462,.T.);
#13681=ORIENTED_EDGE('',*,*,#9463,.F.);
#13682=ORIENTED_EDGE('',*,*,#9464,.T.);
#13683=ORIENTED_EDGE('',*,*,#9461,.T.);
#13684=ORIENTED_EDGE('',*,*,#9464,.F.);
#13685=ORIENTED_EDGE('',*,*,#9465,.F.);
#13686=ORIENTED_EDGE('',*,*,#9466,.T.);
#13687=ORIENTED_EDGE('',*,*,#9463,.T.);
#13688=ORIENTED_EDGE('',*,*,#9466,.F.);
#13689=ORIENTED_EDGE('',*,*,#9465,.T.);
#13690=ORIENTED_EDGE('',*,*,#9467,.T.);
#13691=ORIENTED_EDGE('',*,*,#9468,.F.);
#13692=ORIENTED_EDGE('',*,*,#9467,.F.);
#13693=ORIENTED_EDGE('',*,*,#9468,.T.);
#13694=ORIENTED_EDGE('',*,*,#9469,.F.);
#13695=ORIENTED_EDGE('',*,*,#9470,.F.);
#13696=ORIENTED_EDGE('',*,*,#9471,.T.);
#13697=ORIENTED_EDGE('',*,*,#9469,.T.);
#13698=ORIENTED_EDGE('',*,*,#9471,.F.);
#13699=ORIENTED_EDGE('',*,*,#9470,.T.);
#13700=ORIENTED_EDGE('',*,*,#9472,.F.);
#13701=ORIENTED_EDGE('',*,*,#9473,.F.);
#13702=ORIENTED_EDGE('',*,*,#9474,.T.);
#13703=ORIENTED_EDGE('',*,*,#9472,.T.);
#13704=ORIENTED_EDGE('',*,*,#9474,.F.);
#13705=ORIENTED_EDGE('',*,*,#9475,.F.);
#13706=ORIENTED_EDGE('',*,*,#9476,.T.);
#13707=ORIENTED_EDGE('',*,*,#9473,.T.);
#13708=ORIENTED_EDGE('',*,*,#9476,.F.);
#13709=ORIENTED_EDGE('',*,*,#9475,.T.);
#13710=ORIENTED_EDGE('',*,*,#9477,.T.);
#13711=ORIENTED_EDGE('',*,*,#9478,.F.);
#13712=ORIENTED_EDGE('',*,*,#9477,.F.);
#13713=ORIENTED_EDGE('',*,*,#9478,.T.);
#13714=ORIENTED_EDGE('',*,*,#9479,.T.);
#13715=ORIENTED_EDGE('',*,*,#9462,.F.);
#13716=ORIENTED_EDGE('',*,*,#9479,.F.);
#13717=ORIENTED_EDGE('',*,*,#9480,.T.);
#13718=ORIENTED_EDGE('',*,*,#9481,.T.);
#13719=ORIENTED_EDGE('',*,*,#9482,.T.);
#13720=ORIENTED_EDGE('',*,*,#9481,.F.);
#13721=ORIENTED_EDGE('',*,*,#9480,.F.);
#13722=ORIENTED_EDGE('',*,*,#9483,.T.);
#13723=ORIENTED_EDGE('',*,*,#9484,.F.);
#13724=ORIENTED_EDGE('',*,*,#9483,.F.);
#13725=ORIENTED_EDGE('',*,*,#9485,.T.);
#13726=ORIENTED_EDGE('',*,*,#9486,.F.);
#13727=ORIENTED_EDGE('',*,*,#9487,.T.);
#13728=ORIENTED_EDGE('',*,*,#9488,.F.);
#13729=ORIENTED_EDGE('',*,*,#9489,.F.);
#13730=ORIENTED_EDGE('',*,*,#9490,.F.);
#13731=ORIENTED_EDGE('',*,*,#9491,.F.);
#13732=ORIENTED_EDGE('',*,*,#9492,.F.);
#13733=ORIENTED_EDGE('',*,*,#9493,.F.);
#13734=ORIENTED_EDGE('',*,*,#9482,.F.);
#13735=ORIENTED_EDGE('',*,*,#9484,.T.);
#13736=ORIENTED_EDGE('',*,*,#9494,.T.);
#13737=ORIENTED_EDGE('',*,*,#9495,.T.);
#13738=ORIENTED_EDGE('',*,*,#9494,.F.);
#13739=ORIENTED_EDGE('',*,*,#9496,.T.);
#13740=ORIENTED_EDGE('',*,*,#9497,.T.);
#13741=ORIENTED_EDGE('',*,*,#9498,.T.);
#13742=ORIENTED_EDGE('',*,*,#9499,.T.);
#13743=ORIENTED_EDGE('',*,*,#9500,.T.);
#13744=ORIENTED_EDGE('',*,*,#9501,.T.);
#13745=ORIENTED_EDGE('',*,*,#9502,.T.);
#13746=ORIENTED_EDGE('',*,*,#9503,.T.);
#13747=ORIENTED_EDGE('',*,*,#9504,.F.);
#13748=ORIENTED_EDGE('',*,*,#9495,.F.);
#13749=ORIENTED_EDGE('',*,*,#9505,.T.);
#13750=ORIENTED_EDGE('',*,*,#9506,.T.);
#13751=ORIENTED_EDGE('',*,*,#9493,.T.);
#13752=ORIENTED_EDGE('',*,*,#9506,.F.);
#13753=ORIENTED_EDGE('',*,*,#9505,.F.);
#13754=ORIENTED_EDGE('',*,*,#9507,.T.);
#13755=ORIENTED_EDGE('',*,*,#9508,.F.);
#13756=ORIENTED_EDGE('',*,*,#9507,.F.);
#13757=ORIENTED_EDGE('',*,*,#9508,.T.);
#13758=ORIENTED_EDGE('',*,*,#9509,.T.);
#13759=ORIENTED_EDGE('',*,*,#9504,.T.);
#13760=ORIENTED_EDGE('',*,*,#9509,.F.);
#13761=ORIENTED_EDGE('',*,*,#9510,.F.);
#13762=ORIENTED_EDGE('',*,*,#9487,.F.);
#13763=ORIENTED_EDGE('',*,*,#9511,.F.);
#13764=ORIENTED_EDGE('',*,*,#9502,.F.);
#13765=ORIENTED_EDGE('',*,*,#9512,.F.);
#13766=ORIENTED_EDGE('',*,*,#9496,.F.);
#13767=ORIENTED_EDGE('',*,*,#9513,.F.);
#13768=ORIENTED_EDGE('',*,*,#9485,.F.);
#13769=ORIENTED_EDGE('',*,*,#9510,.T.);
#13770=ORIENTED_EDGE('',*,*,#9501,.F.);
#13771=ORIENTED_EDGE('',*,*,#9514,.F.);
#13772=ORIENTED_EDGE('',*,*,#9488,.T.);
#13773=ORIENTED_EDGE('',*,*,#9489,.T.);
#13774=ORIENTED_EDGE('',*,*,#9514,.T.);
#13775=ORIENTED_EDGE('',*,*,#9500,.F.);
#13776=ORIENTED_EDGE('',*,*,#9515,.F.);
#13777=ORIENTED_EDGE('',*,*,#9490,.T.);
#13778=ORIENTED_EDGE('',*,*,#9515,.T.);
#13779=ORIENTED_EDGE('',*,*,#9499,.F.);
#13780=ORIENTED_EDGE('',*,*,#9516,.F.);
#13781=ORIENTED_EDGE('',*,*,#9491,.T.);
#13782=ORIENTED_EDGE('',*,*,#9516,.T.);
#13783=ORIENTED_EDGE('',*,*,#9498,.F.);
#13784=ORIENTED_EDGE('',*,*,#9517,.F.);
#13785=ORIENTED_EDGE('',*,*,#9512,.T.);
#13786=ORIENTED_EDGE('',*,*,#9492,.T.);
#13787=ORIENTED_EDGE('',*,*,#9517,.T.);
#13788=ORIENTED_EDGE('',*,*,#9497,.F.);
#13789=ORIENTED_EDGE('',*,*,#9513,.T.);
#13790=ORIENTED_EDGE('',*,*,#9503,.F.);
#13791=ORIENTED_EDGE('',*,*,#9511,.T.);
#13792=ORIENTED_EDGE('',*,*,#9486,.T.);
#13793=ORIENTED_EDGE('',*,*,#9518,.F.);
#13794=ORIENTED_EDGE('',*,*,#9519,.F.);
#13795=ORIENTED_EDGE('',*,*,#9520,.F.);
#13796=ORIENTED_EDGE('',*,*,#9521,.T.);
#13797=ORIENTED_EDGE('',*,*,#9522,.F.);
#13798=ORIENTED_EDGE('',*,*,#9523,.F.);
#13799=ORIENTED_EDGE('',*,*,#9524,.F.);
#13800=ORIENTED_EDGE('',*,*,#9518,.T.);
#13801=ORIENTED_EDGE('',*,*,#9525,.T.);
#13802=ORIENTED_EDGE('',*,*,#9526,.T.);
#13803=ORIENTED_EDGE('',*,*,#9527,.F.);
#13804=ORIENTED_EDGE('',*,*,#9528,.F.);
#13805=ORIENTED_EDGE('',*,*,#9522,.T.);
#13806=ORIENTED_EDGE('',*,*,#9529,.T.);
#13807=ORIENTED_EDGE('',*,*,#9530,.F.);
#13808=ORIENTED_EDGE('',*,*,#9531,.F.);
#13809=ORIENTED_EDGE('',*,*,#9532,.F.);
#13810=ORIENTED_EDGE('',*,*,#9527,.T.);
#13811=ORIENTED_EDGE('',*,*,#9533,.T.);
#13812=ORIENTED_EDGE('',*,*,#9534,.T.);
#13813=ORIENTED_EDGE('',*,*,#9535,.F.);
#13814=ORIENTED_EDGE('',*,*,#9536,.F.);
#13815=ORIENTED_EDGE('',*,*,#9530,.T.);
#13816=ORIENTED_EDGE('',*,*,#9537,.T.);
#13817=ORIENTED_EDGE('',*,*,#9538,.F.);
#13818=ORIENTED_EDGE('',*,*,#9539,.F.);
#13819=ORIENTED_EDGE('',*,*,#9540,.F.);
#13820=ORIENTED_EDGE('',*,*,#9535,.T.);
#13821=ORIENTED_EDGE('',*,*,#9541,.T.);
#13822=ORIENTED_EDGE('',*,*,#9542,.T.);
#13823=ORIENTED_EDGE('',*,*,#9543,.F.);
#13824=ORIENTED_EDGE('',*,*,#9544,.F.);
#13825=ORIENTED_EDGE('',*,*,#9538,.T.);
#13826=ORIENTED_EDGE('',*,*,#9545,.T.);
#13827=ORIENTED_EDGE('',*,*,#9546,.F.);
#13828=ORIENTED_EDGE('',*,*,#9547,.F.);
#13829=ORIENTED_EDGE('',*,*,#9548,.F.);
#13830=ORIENTED_EDGE('',*,*,#9543,.T.);
#13831=ORIENTED_EDGE('',*,*,#9549,.T.);
#13832=ORIENTED_EDGE('',*,*,#9550,.T.);
#13833=ORIENTED_EDGE('',*,*,#9551,.F.);
#13834=ORIENTED_EDGE('',*,*,#9552,.F.);
#13835=ORIENTED_EDGE('',*,*,#9546,.T.);
#13836=ORIENTED_EDGE('',*,*,#9553,.T.);
#13837=ORIENTED_EDGE('',*,*,#9554,.F.);
#13838=ORIENTED_EDGE('',*,*,#9555,.F.);
#13839=ORIENTED_EDGE('',*,*,#9556,.F.);
#13840=ORIENTED_EDGE('',*,*,#9551,.T.);
#13841=ORIENTED_EDGE('',*,*,#9557,.T.);
#13842=ORIENTED_EDGE('',*,*,#9558,.T.);
#13843=ORIENTED_EDGE('',*,*,#9559,.F.);
#13844=ORIENTED_EDGE('',*,*,#9560,.F.);
#13845=ORIENTED_EDGE('',*,*,#9554,.T.);
#13846=ORIENTED_EDGE('',*,*,#9561,.T.);
#13847=ORIENTED_EDGE('',*,*,#9562,.F.);
#13848=ORIENTED_EDGE('',*,*,#9563,.F.);
#13849=ORIENTED_EDGE('',*,*,#9564,.F.);
#13850=ORIENTED_EDGE('',*,*,#9559,.T.);
#13851=ORIENTED_EDGE('',*,*,#9565,.T.);
#13852=ORIENTED_EDGE('',*,*,#9566,.T.);
#13853=ORIENTED_EDGE('',*,*,#9567,.F.);
#13854=ORIENTED_EDGE('',*,*,#9568,.F.);
#13855=ORIENTED_EDGE('',*,*,#9569,.F.);
#13856=ORIENTED_EDGE('',*,*,#9562,.T.);
#13857=ORIENTED_EDGE('',*,*,#9570,.T.);
#13858=ORIENTED_EDGE('',*,*,#9571,.F.);
#13859=ORIENTED_EDGE('',*,*,#9572,.F.);
#13860=ORIENTED_EDGE('',*,*,#9573,.F.);
#13861=ORIENTED_EDGE('',*,*,#9567,.T.);
#13862=ORIENTED_EDGE('',*,*,#9574,.T.);
#13863=ORIENTED_EDGE('',*,*,#9575,.T.);
#13864=ORIENTED_EDGE('',*,*,#9576,.F.);
#13865=ORIENTED_EDGE('',*,*,#9577,.F.);
#13866=ORIENTED_EDGE('',*,*,#9578,.F.);
#13867=ORIENTED_EDGE('',*,*,#9571,.T.);
#13868=ORIENTED_EDGE('',*,*,#9579,.T.);
#13869=ORIENTED_EDGE('',*,*,#9580,.T.);
#13870=ORIENTED_EDGE('',*,*,#9581,.F.);
#13871=ORIENTED_EDGE('',*,*,#9582,.F.);
#13872=ORIENTED_EDGE('',*,*,#9576,.T.);
#13873=ORIENTED_EDGE('',*,*,#9583,.T.);
#13874=ORIENTED_EDGE('',*,*,#9584,.F.);
#13875=ORIENTED_EDGE('',*,*,#9585,.F.);
#13876=ORIENTED_EDGE('',*,*,#9586,.F.);
#13877=ORIENTED_EDGE('',*,*,#9581,.T.);
#13878=ORIENTED_EDGE('',*,*,#9587,.T.);
#13879=ORIENTED_EDGE('',*,*,#9588,.T.);
#13880=ORIENTED_EDGE('',*,*,#9589,.F.);
#13881=ORIENTED_EDGE('',*,*,#9590,.F.);
#13882=ORIENTED_EDGE('',*,*,#9591,.F.);
#13883=ORIENTED_EDGE('',*,*,#9584,.T.);
#13884=ORIENTED_EDGE('',*,*,#9592,.T.);
#13885=ORIENTED_EDGE('',*,*,#9593,.T.);
#13886=ORIENTED_EDGE('',*,*,#9594,.F.);
#13887=ORIENTED_EDGE('',*,*,#9595,.F.);
#13888=ORIENTED_EDGE('',*,*,#9589,.T.);
#13889=ORIENTED_EDGE('',*,*,#9596,.T.);
#13890=ORIENTED_EDGE('',*,*,#9597,.T.);
#13891=ORIENTED_EDGE('',*,*,#9598,.T.);
#13892=ORIENTED_EDGE('',*,*,#9599,.T.);
#13893=ORIENTED_EDGE('',*,*,#9600,.T.);
#13894=ORIENTED_EDGE('',*,*,#9601,.T.);
#13895=ORIENTED_EDGE('',*,*,#9602,.T.);
#13896=ORIENTED_EDGE('',*,*,#9603,.T.);
#13897=ORIENTED_EDGE('',*,*,#9604,.T.);
#13898=ORIENTED_EDGE('',*,*,#9605,.T.);
#13899=ORIENTED_EDGE('',*,*,#9606,.T.);
#13900=ORIENTED_EDGE('',*,*,#9607,.T.);
#13901=ORIENTED_EDGE('',*,*,#9608,.T.);
#13902=ORIENTED_EDGE('',*,*,#9609,.T.);
#13903=ORIENTED_EDGE('',*,*,#9610,.T.);
#13904=ORIENTED_EDGE('',*,*,#9611,.T.);
#13905=ORIENTED_EDGE('',*,*,#9612,.T.);
#13906=ORIENTED_EDGE('',*,*,#9613,.T.);
#13907=ORIENTED_EDGE('',*,*,#9614,.T.);
#13908=ORIENTED_EDGE('',*,*,#9615,.T.);
#13909=ORIENTED_EDGE('',*,*,#9616,.T.);
#13910=ORIENTED_EDGE('',*,*,#9617,.T.);
#13911=ORIENTED_EDGE('',*,*,#9618,.T.);
#13912=ORIENTED_EDGE('',*,*,#9619,.T.);
#13913=ORIENTED_EDGE('',*,*,#9620,.T.);
#13914=ORIENTED_EDGE('',*,*,#9621,.F.);
#13915=ORIENTED_EDGE('',*,*,#9622,.F.);
#13916=ORIENTED_EDGE('',*,*,#9623,.T.);
#13917=ORIENTED_EDGE('',*,*,#9624,.T.);
#13918=ORIENTED_EDGE('',*,*,#9625,.T.);
#13919=ORIENTED_EDGE('',*,*,#9626,.T.);
#13920=ORIENTED_EDGE('',*,*,#9627,.T.);
#13921=ORIENTED_EDGE('',*,*,#9628,.T.);
#13922=ORIENTED_EDGE('',*,*,#9629,.T.);
#13923=ORIENTED_EDGE('',*,*,#9630,.T.);
#13924=ORIENTED_EDGE('',*,*,#9631,.T.);
#13925=ORIENTED_EDGE('',*,*,#9632,.T.);
#13926=ORIENTED_EDGE('',*,*,#9633,.T.);
#13927=ORIENTED_EDGE('',*,*,#9634,.T.);
#13928=ORIENTED_EDGE('',*,*,#9635,.T.);
#13929=ORIENTED_EDGE('',*,*,#9636,.T.);
#13930=ORIENTED_EDGE('',*,*,#9637,.T.);
#13931=ORIENTED_EDGE('',*,*,#9638,.T.);
#13932=ORIENTED_EDGE('',*,*,#9639,.T.);
#13933=ORIENTED_EDGE('',*,*,#9640,.T.);
#13934=ORIENTED_EDGE('',*,*,#9641,.T.);
#13935=ORIENTED_EDGE('',*,*,#9594,.T.);
#13936=ORIENTED_EDGE('',*,*,#9642,.T.);
#13937=ORIENTED_EDGE('',*,*,#9643,.F.);
#13938=ORIENTED_EDGE('',*,*,#9644,.F.);
#13939=ORIENTED_EDGE('',*,*,#9645,.F.);
#13940=ORIENTED_EDGE('',*,*,#9646,.F.);
#13941=ORIENTED_EDGE('',*,*,#9647,.T.);
#13942=ORIENTED_EDGE('',*,*,#9643,.T.);
#13943=ORIENTED_EDGE('',*,*,#9648,.T.);
#13944=ORIENTED_EDGE('',*,*,#9649,.T.);
#13945=ORIENTED_EDGE('',*,*,#9647,.F.);
#13946=ORIENTED_EDGE('',*,*,#9650,.F.);
#13947=ORIENTED_EDGE('',*,*,#9620,.F.);
#13948=ORIENTED_EDGE('',*,*,#9619,.F.);
#13949=ORIENTED_EDGE('',*,*,#9618,.F.);
#13950=ORIENTED_EDGE('',*,*,#9617,.F.);
#13951=ORIENTED_EDGE('',*,*,#9616,.F.);
#13952=ORIENTED_EDGE('',*,*,#9615,.F.);
#13953=ORIENTED_EDGE('',*,*,#9614,.F.);
#13954=ORIENTED_EDGE('',*,*,#9613,.F.);
#13955=ORIENTED_EDGE('',*,*,#9612,.F.);
#13956=ORIENTED_EDGE('',*,*,#9611,.F.);
#13957=ORIENTED_EDGE('',*,*,#9610,.F.);
#13958=ORIENTED_EDGE('',*,*,#9609,.F.);
#13959=ORIENTED_EDGE('',*,*,#9608,.F.);
#13960=ORIENTED_EDGE('',*,*,#9607,.F.);
#13961=ORIENTED_EDGE('',*,*,#9606,.F.);
#13962=ORIENTED_EDGE('',*,*,#9605,.F.);
#13963=ORIENTED_EDGE('',*,*,#9604,.F.);
#13964=ORIENTED_EDGE('',*,*,#9603,.F.);
#13965=ORIENTED_EDGE('',*,*,#9602,.F.);
#13966=ORIENTED_EDGE('',*,*,#9601,.F.);
#13967=ORIENTED_EDGE('',*,*,#9600,.F.);
#13968=ORIENTED_EDGE('',*,*,#9651,.F.);
#13969=ORIENTED_EDGE('',*,*,#9519,.T.);
#13970=ORIENTED_EDGE('',*,*,#9524,.T.);
#13971=ORIENTED_EDGE('',*,*,#9523,.T.);
#13972=ORIENTED_EDGE('',*,*,#9528,.T.);
#13973=ORIENTED_EDGE('',*,*,#9532,.T.);
#13974=ORIENTED_EDGE('',*,*,#9531,.T.);
#13975=ORIENTED_EDGE('',*,*,#9536,.T.);
#13976=ORIENTED_EDGE('',*,*,#9540,.T.);
#13977=ORIENTED_EDGE('',*,*,#9539,.T.);
#13978=ORIENTED_EDGE('',*,*,#9544,.T.);
#13979=ORIENTED_EDGE('',*,*,#9548,.T.);
#13980=ORIENTED_EDGE('',*,*,#9547,.T.);
#13981=ORIENTED_EDGE('',*,*,#9552,.T.);
#13982=ORIENTED_EDGE('',*,*,#9556,.T.);
#13983=ORIENTED_EDGE('',*,*,#9555,.T.);
#13984=ORIENTED_EDGE('',*,*,#9560,.T.);
#13985=ORIENTED_EDGE('',*,*,#9564,.T.);
#13986=ORIENTED_EDGE('',*,*,#9563,.T.);
#13987=ORIENTED_EDGE('',*,*,#9569,.T.);
#13988=ORIENTED_EDGE('',*,*,#9568,.T.);
#13989=ORIENTED_EDGE('',*,*,#9573,.T.);
#13990=ORIENTED_EDGE('',*,*,#9572,.T.);
#13991=ORIENTED_EDGE('',*,*,#9578,.T.);
#13992=ORIENTED_EDGE('',*,*,#9577,.T.);
#13993=ORIENTED_EDGE('',*,*,#9582,.T.);
#13994=ORIENTED_EDGE('',*,*,#9586,.T.);
#13995=ORIENTED_EDGE('',*,*,#9585,.T.);
#13996=ORIENTED_EDGE('',*,*,#9591,.T.);
#13997=ORIENTED_EDGE('',*,*,#9590,.T.);
#13998=ORIENTED_EDGE('',*,*,#9595,.T.);
#13999=ORIENTED_EDGE('',*,*,#9645,.T.);
#14000=ORIENTED_EDGE('',*,*,#9644,.T.);
#14001=ORIENTED_EDGE('',*,*,#9652,.T.);
#14002=ORIENTED_EDGE('',*,*,#9653,.T.);
#14003=ORIENTED_EDGE('',*,*,#9654,.T.);
#14004=ORIENTED_EDGE('',*,*,#9520,.T.);
#14005=ORIENTED_EDGE('',*,*,#9651,.T.);
#14006=ORIENTED_EDGE('',*,*,#9649,.F.);
#14007=ORIENTED_EDGE('',*,*,#9648,.F.);
#14008=ORIENTED_EDGE('',*,*,#9642,.F.);
#14009=ORIENTED_EDGE('',*,*,#9597,.F.);
#14010=ORIENTED_EDGE('',*,*,#9596,.F.);
#14011=ORIENTED_EDGE('',*,*,#9593,.F.);
#14012=ORIENTED_EDGE('',*,*,#9592,.F.);
#14013=ORIENTED_EDGE('',*,*,#9588,.F.);
#14014=ORIENTED_EDGE('',*,*,#9587,.F.);
#14015=ORIENTED_EDGE('',*,*,#9583,.F.);
#14016=ORIENTED_EDGE('',*,*,#9580,.F.);
#14017=ORIENTED_EDGE('',*,*,#9579,.F.);
#14018=ORIENTED_EDGE('',*,*,#9575,.F.);
#14019=ORIENTED_EDGE('',*,*,#9574,.F.);
#14020=ORIENTED_EDGE('',*,*,#9570,.F.);
#14021=ORIENTED_EDGE('',*,*,#9566,.F.);
#14022=ORIENTED_EDGE('',*,*,#9565,.F.);
#14023=ORIENTED_EDGE('',*,*,#9561,.F.);
#14024=ORIENTED_EDGE('',*,*,#9558,.F.);
#14025=ORIENTED_EDGE('',*,*,#9557,.F.);
#14026=ORIENTED_EDGE('',*,*,#9553,.F.);
#14027=ORIENTED_EDGE('',*,*,#9550,.F.);
#14028=ORIENTED_EDGE('',*,*,#9549,.F.);
#14029=ORIENTED_EDGE('',*,*,#9545,.F.);
#14030=ORIENTED_EDGE('',*,*,#9542,.F.);
#14031=ORIENTED_EDGE('',*,*,#9541,.F.);
#14032=ORIENTED_EDGE('',*,*,#9537,.F.);
#14033=ORIENTED_EDGE('',*,*,#9534,.F.);
#14034=ORIENTED_EDGE('',*,*,#9533,.F.);
#14035=ORIENTED_EDGE('',*,*,#9529,.F.);
#14036=ORIENTED_EDGE('',*,*,#9526,.F.);
#14037=ORIENTED_EDGE('',*,*,#9525,.F.);
#14038=ORIENTED_EDGE('',*,*,#9521,.F.);
#14039=ORIENTED_EDGE('',*,*,#9654,.F.);
#14040=ORIENTED_EDGE('',*,*,#9655,.T.);
#14041=ORIENTED_EDGE('',*,*,#9598,.F.);
#14042=ORIENTED_EDGE('',*,*,#9641,.F.);
#14043=ORIENTED_EDGE('',*,*,#9640,.F.);
#14044=ORIENTED_EDGE('',*,*,#9639,.F.);
#14045=ORIENTED_EDGE('',*,*,#9638,.F.);
#14046=ORIENTED_EDGE('',*,*,#9637,.F.);
#14047=ORIENTED_EDGE('',*,*,#9636,.F.);
#14048=ORIENTED_EDGE('',*,*,#9635,.F.);
#14049=ORIENTED_EDGE('',*,*,#9634,.F.);
#14050=ORIENTED_EDGE('',*,*,#9633,.F.);
#14051=ORIENTED_EDGE('',*,*,#9632,.F.);
#14052=ORIENTED_EDGE('',*,*,#9631,.F.);
#14053=ORIENTED_EDGE('',*,*,#9630,.F.);
#14054=ORIENTED_EDGE('',*,*,#9629,.F.);
#14055=ORIENTED_EDGE('',*,*,#9628,.F.);
#14056=ORIENTED_EDGE('',*,*,#9627,.F.);
#14057=ORIENTED_EDGE('',*,*,#9626,.F.);
#14058=ORIENTED_EDGE('',*,*,#9625,.F.);
#14059=ORIENTED_EDGE('',*,*,#9624,.F.);
#14060=ORIENTED_EDGE('',*,*,#9623,.F.);
#14061=ORIENTED_EDGE('',*,*,#9656,.T.);
#14062=ORIENTED_EDGE('',*,*,#9657,.T.);
#14063=ORIENTED_EDGE('',*,*,#9621,.T.);
#14064=ORIENTED_EDGE('',*,*,#9650,.T.);
#14065=ORIENTED_EDGE('',*,*,#9646,.T.);
#14066=ORIENTED_EDGE('',*,*,#9622,.T.);
#14067=ORIENTED_EDGE('',*,*,#9657,.F.);
#14068=ORIENTED_EDGE('',*,*,#9658,.F.);
#14069=ORIENTED_EDGE('',*,*,#9656,.F.);
#14070=ORIENTED_EDGE('',*,*,#9659,.F.);
#14071=ORIENTED_EDGE('',*,*,#9660,.F.);
#14072=ORIENTED_EDGE('',*,*,#9661,.F.);
#14073=ORIENTED_EDGE('',*,*,#9662,.F.);
#14074=ORIENTED_EDGE('',*,*,#9663,.F.);
#14075=ORIENTED_EDGE('',*,*,#9664,.F.);
#14076=ORIENTED_EDGE('',*,*,#9665,.F.);
#14077=ORIENTED_EDGE('',*,*,#9666,.T.);
#14078=ORIENTED_EDGE('',*,*,#9667,.F.);
#14079=ORIENTED_EDGE('',*,*,#9666,.F.);
#14080=ORIENTED_EDGE('',*,*,#9664,.T.);
#14081=ORIENTED_EDGE('',*,*,#9668,.T.);
#14082=ORIENTED_EDGE('',*,*,#9669,.T.);
#14083=ORIENTED_EDGE('',*,*,#9670,.F.);
#14084=ORIENTED_EDGE('',*,*,#9663,.T.);
#14085=ORIENTED_EDGE('',*,*,#9671,.T.);
#14086=ORIENTED_EDGE('',*,*,#9672,.T.);
#14087=ORIENTED_EDGE('',*,*,#9668,.F.);
#14088=ORIENTED_EDGE('',*,*,#9662,.T.);
#14089=ORIENTED_EDGE('',*,*,#9673,.T.);
#14090=ORIENTED_EDGE('',*,*,#9674,.T.);
#14091=ORIENTED_EDGE('',*,*,#9671,.F.);
#14092=ORIENTED_EDGE('',*,*,#9675,.T.);
#14093=ORIENTED_EDGE('',*,*,#9676,.F.);
#14094=ORIENTED_EDGE('',*,*,#9675,.F.);
#14095=ORIENTED_EDGE('',*,*,#9661,.T.);
#14096=ORIENTED_EDGE('',*,*,#9677,.T.);
#14097=ORIENTED_EDGE('',*,*,#9678,.T.);
#14098=ORIENTED_EDGE('',*,*,#9673,.F.);
#14099=ORIENTED_EDGE('',*,*,#9660,.T.);
#14100=ORIENTED_EDGE('',*,*,#9679,.T.);
#14101=ORIENTED_EDGE('',*,*,#9680,.T.);
#14102=ORIENTED_EDGE('',*,*,#9677,.F.);
#14103=ORIENTED_EDGE('',*,*,#9659,.T.);
#14104=ORIENTED_EDGE('',*,*,#9665,.T.);
#14105=ORIENTED_EDGE('',*,*,#9670,.T.);
#14106=ORIENTED_EDGE('',*,*,#9681,.T.);
#14107=ORIENTED_EDGE('',*,*,#9679,.F.);
#14108=ORIENTED_EDGE('',*,*,#9674,.F.);
#14109=ORIENTED_EDGE('',*,*,#9678,.F.);
#14110=ORIENTED_EDGE('',*,*,#9680,.F.);
#14111=ORIENTED_EDGE('',*,*,#9681,.F.);
#14112=ORIENTED_EDGE('',*,*,#9669,.F.);
#14113=ORIENTED_EDGE('',*,*,#9672,.F.);
#14114=ORIENTED_EDGE('',*,*,#9676,.T.);
#14115=ORIENTED_EDGE('',*,*,#9682,.T.);
#14116=ORIENTED_EDGE('',*,*,#9683,.T.);
#14117=ORIENTED_EDGE('',*,*,#9684,.T.);
#14118=ORIENTED_EDGE('',*,*,#9683,.F.);
#14119=ORIENTED_EDGE('',*,*,#9684,.F.);
#14120=ORIENTED_EDGE('',*,*,#9685,.T.);
#14121=ORIENTED_EDGE('',*,*,#9686,.T.);
#14122=ORIENTED_EDGE('',*,*,#9685,.F.);
#14123=ORIENTED_EDGE('',*,*,#9682,.F.);
#14124=ORIENTED_EDGE('',*,*,#9667,.T.);
#14125=ORIENTED_EDGE('',*,*,#9687,.F.);
#14126=ORIENTED_EDGE('',*,*,#9655,.F.);
#14127=ORIENTED_EDGE('',*,*,#9653,.F.);
#14128=ORIENTED_EDGE('',*,*,#9688,.T.);
#14129=ORIENTED_EDGE('',*,*,#9687,.T.);
#14130=ORIENTED_EDGE('',*,*,#9688,.F.);
#14131=ORIENTED_EDGE('',*,*,#9652,.F.);
#14132=ORIENTED_EDGE('',*,*,#9599,.F.);
#14133=ORIENTED_EDGE('',*,*,#9686,.F.);
#14134=ORIENTED_EDGE('',*,*,#9689,.T.);
#14135=ORIENTED_EDGE('',*,*,#9658,.T.);
#14136=ORIENTED_EDGE('',*,*,#9689,.F.);
#14137=ORIENTED_EDGE('',*,*,#9690,.F.);
#14138=ORIENTED_EDGE('',*,*,#9691,.F.);
#14139=ORIENTED_EDGE('',*,*,#9692,.F.);
#14140=ORIENTED_EDGE('',*,*,#9693,.T.);
#14141=ORIENTED_EDGE('',*,*,#9694,.F.);
#14142=ORIENTED_EDGE('',*,*,#9695,.F.);
#14143=ORIENTED_EDGE('',*,*,#9696,.F.);
#14144=ORIENTED_EDGE('',*,*,#9690,.T.);
#14145=ORIENTED_EDGE('',*,*,#9697,.T.);
#14146=ORIENTED_EDGE('',*,*,#9698,.T.);
#14147=ORIENTED_EDGE('',*,*,#9699,.F.);
#14148=ORIENTED_EDGE('',*,*,#9700,.F.);
#14149=ORIENTED_EDGE('',*,*,#9694,.T.);
#14150=ORIENTED_EDGE('',*,*,#9701,.T.);
#14151=ORIENTED_EDGE('',*,*,#9702,.T.);
#14152=ORIENTED_EDGE('',*,*,#9703,.F.);
#14153=ORIENTED_EDGE('',*,*,#9704,.F.);
#14154=ORIENTED_EDGE('',*,*,#9705,.F.);
#14155=ORIENTED_EDGE('',*,*,#9699,.T.);
#14156=ORIENTED_EDGE('',*,*,#9706,.T.);
#14157=ORIENTED_EDGE('',*,*,#9707,.F.);
#14158=ORIENTED_EDGE('',*,*,#9708,.F.);
#14159=ORIENTED_EDGE('',*,*,#9703,.T.);
#14160=ORIENTED_EDGE('',*,*,#9709,.T.);
#14161=ORIENTED_EDGE('',*,*,#9710,.T.);
#14162=ORIENTED_EDGE('',*,*,#9711,.F.);
#14163=ORIENTED_EDGE('',*,*,#9712,.F.);
#14164=ORIENTED_EDGE('',*,*,#9713,.F.);
#14165=ORIENTED_EDGE('',*,*,#9707,.T.);
#14166=ORIENTED_EDGE('',*,*,#9714,.T.);
#14167=ORIENTED_EDGE('',*,*,#9715,.F.);
#14168=ORIENTED_EDGE('',*,*,#9716,.F.);
#14169=ORIENTED_EDGE('',*,*,#9711,.T.);
#14170=ORIENTED_EDGE('',*,*,#9717,.T.);
#14171=ORIENTED_EDGE('',*,*,#9718,.T.);
#14172=ORIENTED_EDGE('',*,*,#9719,.F.);
#14173=ORIENTED_EDGE('',*,*,#9720,.F.);
#14174=ORIENTED_EDGE('',*,*,#9721,.F.);
#14175=ORIENTED_EDGE('',*,*,#9715,.T.);
#14176=ORIENTED_EDGE('',*,*,#9722,.T.);
#14177=ORIENTED_EDGE('',*,*,#9723,.T.);
#14178=ORIENTED_EDGE('',*,*,#9724,.F.);
#14179=ORIENTED_EDGE('',*,*,#9725,.F.);
#14180=ORIENTED_EDGE('',*,*,#9719,.T.);
#14181=ORIENTED_EDGE('',*,*,#9726,.T.);
#14182=ORIENTED_EDGE('',*,*,#9727,.T.);
#14183=ORIENTED_EDGE('',*,*,#9728,.F.);
#14184=ORIENTED_EDGE('',*,*,#9729,.F.);
#14185=ORIENTED_EDGE('',*,*,#9730,.F.);
#14186=ORIENTED_EDGE('',*,*,#9724,.T.);
#14187=ORIENTED_EDGE('',*,*,#9731,.T.);
#14188=ORIENTED_EDGE('',*,*,#9732,.F.);
#14189=ORIENTED_EDGE('',*,*,#9733,.F.);
#14190=ORIENTED_EDGE('',*,*,#9728,.T.);
#14191=ORIENTED_EDGE('',*,*,#9734,.T.);
#14192=ORIENTED_EDGE('',*,*,#9735,.T.);
#14193=ORIENTED_EDGE('',*,*,#9736,.F.);
#14194=ORIENTED_EDGE('',*,*,#9737,.F.);
#14195=ORIENTED_EDGE('',*,*,#9738,.F.);
#14196=ORIENTED_EDGE('',*,*,#9732,.T.);
#14197=ORIENTED_EDGE('',*,*,#9739,.T.);
#14198=ORIENTED_EDGE('',*,*,#9740,.F.);
#14199=ORIENTED_EDGE('',*,*,#9741,.F.);
#14200=ORIENTED_EDGE('',*,*,#9736,.T.);
#14201=ORIENTED_EDGE('',*,*,#9742,.T.);
#14202=ORIENTED_EDGE('',*,*,#9743,.T.);
#14203=ORIENTED_EDGE('',*,*,#9744,.F.);
#14204=ORIENTED_EDGE('',*,*,#9745,.F.);
#14205=ORIENTED_EDGE('',*,*,#9746,.F.);
#14206=ORIENTED_EDGE('',*,*,#9740,.T.);
#14207=ORIENTED_EDGE('',*,*,#9747,.T.);
#14208=ORIENTED_EDGE('',*,*,#9748,.F.);
#14209=ORIENTED_EDGE('',*,*,#9749,.F.);
#14210=ORIENTED_EDGE('',*,*,#9744,.T.);
#14211=ORIENTED_EDGE('',*,*,#9750,.T.);
#14212=ORIENTED_EDGE('',*,*,#9751,.T.);
#14213=ORIENTED_EDGE('',*,*,#9752,.T.);
#14214=ORIENTED_EDGE('',*,*,#9753,.T.);
#14215=ORIENTED_EDGE('',*,*,#9754,.T.);
#14216=ORIENTED_EDGE('',*,*,#9755,.T.);
#14217=ORIENTED_EDGE('',*,*,#9756,.T.);
#14218=ORIENTED_EDGE('',*,*,#9757,.T.);
#14219=ORIENTED_EDGE('',*,*,#9758,.T.);
#14220=ORIENTED_EDGE('',*,*,#9759,.T.);
#14221=ORIENTED_EDGE('',*,*,#9760,.T.);
#14222=ORIENTED_EDGE('',*,*,#9761,.T.);
#14223=ORIENTED_EDGE('',*,*,#9762,.T.);
#14224=ORIENTED_EDGE('',*,*,#9763,.T.);
#14225=ORIENTED_EDGE('',*,*,#9764,.T.);
#14226=ORIENTED_EDGE('',*,*,#9765,.T.);
#14227=ORIENTED_EDGE('',*,*,#9766,.T.);
#14228=ORIENTED_EDGE('',*,*,#9767,.T.);
#14229=ORIENTED_EDGE('',*,*,#9768,.T.);
#14230=ORIENTED_EDGE('',*,*,#9769,.T.);
#14231=ORIENTED_EDGE('',*,*,#9770,.T.);
#14232=ORIENTED_EDGE('',*,*,#9771,.F.);
#14233=ORIENTED_EDGE('',*,*,#9772,.F.);
#14234=ORIENTED_EDGE('',*,*,#9773,.T.);
#14235=ORIENTED_EDGE('',*,*,#9774,.T.);
#14236=ORIENTED_EDGE('',*,*,#9775,.T.);
#14237=ORIENTED_EDGE('',*,*,#9776,.T.);
#14238=ORIENTED_EDGE('',*,*,#9777,.T.);
#14239=ORIENTED_EDGE('',*,*,#9778,.T.);
#14240=ORIENTED_EDGE('',*,*,#9779,.T.);
#14241=ORIENTED_EDGE('',*,*,#9780,.T.);
#14242=ORIENTED_EDGE('',*,*,#9781,.T.);
#14243=ORIENTED_EDGE('',*,*,#9782,.T.);
#14244=ORIENTED_EDGE('',*,*,#9783,.T.);
#14245=ORIENTED_EDGE('',*,*,#9784,.T.);
#14246=ORIENTED_EDGE('',*,*,#9785,.T.);
#14247=ORIENTED_EDGE('',*,*,#9786,.T.);
#14248=ORIENTED_EDGE('',*,*,#9787,.T.);
#14249=ORIENTED_EDGE('',*,*,#9748,.T.);
#14250=ORIENTED_EDGE('',*,*,#9788,.T.);
#14251=ORIENTED_EDGE('',*,*,#9789,.F.);
#14252=ORIENTED_EDGE('',*,*,#9790,.F.);
#14253=ORIENTED_EDGE('',*,*,#9791,.F.);
#14254=ORIENTED_EDGE('',*,*,#9792,.F.);
#14255=ORIENTED_EDGE('',*,*,#9793,.T.);
#14256=ORIENTED_EDGE('',*,*,#9789,.T.);
#14257=ORIENTED_EDGE('',*,*,#9794,.T.);
#14258=ORIENTED_EDGE('',*,*,#9795,.T.);
#14259=ORIENTED_EDGE('',*,*,#9793,.F.);
#14260=ORIENTED_EDGE('',*,*,#9796,.F.);
#14261=ORIENTED_EDGE('',*,*,#9770,.F.);
#14262=ORIENTED_EDGE('',*,*,#9769,.F.);
#14263=ORIENTED_EDGE('',*,*,#9768,.F.);
#14264=ORIENTED_EDGE('',*,*,#9767,.F.);
#14265=ORIENTED_EDGE('',*,*,#9766,.F.);
#14266=ORIENTED_EDGE('',*,*,#9765,.F.);
#14267=ORIENTED_EDGE('',*,*,#9764,.F.);
#14268=ORIENTED_EDGE('',*,*,#9763,.F.);
#14269=ORIENTED_EDGE('',*,*,#9762,.F.);
#14270=ORIENTED_EDGE('',*,*,#9761,.F.);
#14271=ORIENTED_EDGE('',*,*,#9760,.F.);
#14272=ORIENTED_EDGE('',*,*,#9759,.F.);
#14273=ORIENTED_EDGE('',*,*,#9758,.F.);
#14274=ORIENTED_EDGE('',*,*,#9757,.F.);
#14275=ORIENTED_EDGE('',*,*,#9756,.F.);
#14276=ORIENTED_EDGE('',*,*,#9755,.F.);
#14277=ORIENTED_EDGE('',*,*,#9754,.F.);
#14278=ORIENTED_EDGE('',*,*,#9797,.F.);
#14279=ORIENTED_EDGE('',*,*,#9691,.T.);
#14280=ORIENTED_EDGE('',*,*,#9696,.T.);
#14281=ORIENTED_EDGE('',*,*,#9695,.T.);
#14282=ORIENTED_EDGE('',*,*,#9700,.T.);
#14283=ORIENTED_EDGE('',*,*,#9705,.T.);
#14284=ORIENTED_EDGE('',*,*,#9704,.T.);
#14285=ORIENTED_EDGE('',*,*,#9708,.T.);
#14286=ORIENTED_EDGE('',*,*,#9713,.T.);
#14287=ORIENTED_EDGE('',*,*,#9712,.T.);
#14288=ORIENTED_EDGE('',*,*,#9716,.T.);
#14289=ORIENTED_EDGE('',*,*,#9721,.T.);
#14290=ORIENTED_EDGE('',*,*,#9720,.T.);
#14291=ORIENTED_EDGE('',*,*,#9725,.T.);
#14292=ORIENTED_EDGE('',*,*,#9730,.T.);
#14293=ORIENTED_EDGE('',*,*,#9729,.T.);
#14294=ORIENTED_EDGE('',*,*,#9733,.T.);
#14295=ORIENTED_EDGE('',*,*,#9738,.T.);
#14296=ORIENTED_EDGE('',*,*,#9737,.T.);
#14297=ORIENTED_EDGE('',*,*,#9741,.T.);
#14298=ORIENTED_EDGE('',*,*,#9746,.T.);
#14299=ORIENTED_EDGE('',*,*,#9745,.T.);
#14300=ORIENTED_EDGE('',*,*,#9749,.T.);
#14301=ORIENTED_EDGE('',*,*,#9791,.T.);
#14302=ORIENTED_EDGE('',*,*,#9790,.T.);
#14303=ORIENTED_EDGE('',*,*,#9798,.T.);
#14304=ORIENTED_EDGE('',*,*,#9799,.T.);
#14305=ORIENTED_EDGE('',*,*,#9800,.T.);
#14306=ORIENTED_EDGE('',*,*,#9692,.T.);
#14307=ORIENTED_EDGE('',*,*,#9797,.T.);
#14308=ORIENTED_EDGE('',*,*,#9795,.F.);
#14309=ORIENTED_EDGE('',*,*,#9794,.F.);
#14310=ORIENTED_EDGE('',*,*,#9788,.F.);
#14311=ORIENTED_EDGE('',*,*,#9751,.F.);
#14312=ORIENTED_EDGE('',*,*,#9750,.F.);
#14313=ORIENTED_EDGE('',*,*,#9747,.F.);
#14314=ORIENTED_EDGE('',*,*,#9743,.F.);
#14315=ORIENTED_EDGE('',*,*,#9742,.F.);
#14316=ORIENTED_EDGE('',*,*,#9739,.F.);
#14317=ORIENTED_EDGE('',*,*,#9735,.F.);
#14318=ORIENTED_EDGE('',*,*,#9734,.F.);
#14319=ORIENTED_EDGE('',*,*,#9731,.F.);
#14320=ORIENTED_EDGE('',*,*,#9727,.F.);
#14321=ORIENTED_EDGE('',*,*,#9726,.F.);
#14322=ORIENTED_EDGE('',*,*,#9723,.F.);
#14323=ORIENTED_EDGE('',*,*,#9722,.F.);
#14324=ORIENTED_EDGE('',*,*,#9718,.F.);
#14325=ORIENTED_EDGE('',*,*,#9717,.F.);
#14326=ORIENTED_EDGE('',*,*,#9714,.F.);
#14327=ORIENTED_EDGE('',*,*,#9710,.F.);
#14328=ORIENTED_EDGE('',*,*,#9709,.F.);
#14329=ORIENTED_EDGE('',*,*,#9706,.F.);
#14330=ORIENTED_EDGE('',*,*,#9702,.F.);
#14331=ORIENTED_EDGE('',*,*,#9701,.F.);
#14332=ORIENTED_EDGE('',*,*,#9698,.F.);
#14333=ORIENTED_EDGE('',*,*,#9697,.F.);
#14334=ORIENTED_EDGE('',*,*,#9693,.F.);
#14335=ORIENTED_EDGE('',*,*,#9800,.F.);
#14336=ORIENTED_EDGE('',*,*,#9801,.T.);
#14337=ORIENTED_EDGE('',*,*,#9752,.F.);
#14338=ORIENTED_EDGE('',*,*,#9787,.F.);
#14339=ORIENTED_EDGE('',*,*,#9786,.F.);
#14340=ORIENTED_EDGE('',*,*,#9785,.F.);
#14341=ORIENTED_EDGE('',*,*,#9784,.F.);
#14342=ORIENTED_EDGE('',*,*,#9783,.F.);
#14343=ORIENTED_EDGE('',*,*,#9782,.F.);
#14344=ORIENTED_EDGE('',*,*,#9781,.F.);
#14345=ORIENTED_EDGE('',*,*,#9780,.F.);
#14346=ORIENTED_EDGE('',*,*,#9779,.F.);
#14347=ORIENTED_EDGE('',*,*,#9778,.F.);
#14348=ORIENTED_EDGE('',*,*,#9777,.F.);
#14349=ORIENTED_EDGE('',*,*,#9776,.F.);
#14350=ORIENTED_EDGE('',*,*,#9775,.F.);
#14351=ORIENTED_EDGE('',*,*,#9774,.F.);
#14352=ORIENTED_EDGE('',*,*,#9773,.F.);
#14353=ORIENTED_EDGE('',*,*,#9802,.T.);
#14354=ORIENTED_EDGE('',*,*,#9803,.T.);
#14355=ORIENTED_EDGE('',*,*,#9771,.T.);
#14356=ORIENTED_EDGE('',*,*,#9796,.T.);
#14357=ORIENTED_EDGE('',*,*,#9792,.T.);
#14358=ORIENTED_EDGE('',*,*,#9772,.T.);
#14359=ORIENTED_EDGE('',*,*,#9803,.F.);
#14360=ORIENTED_EDGE('',*,*,#9804,.F.);
#14361=ORIENTED_EDGE('',*,*,#9802,.F.);
#14362=ORIENTED_EDGE('',*,*,#9805,.F.);
#14363=ORIENTED_EDGE('',*,*,#9806,.F.);
#14364=ORIENTED_EDGE('',*,*,#9807,.F.);
#14365=ORIENTED_EDGE('',*,*,#9808,.F.);
#14366=ORIENTED_EDGE('',*,*,#9809,.F.);
#14367=ORIENTED_EDGE('',*,*,#9810,.F.);
#14368=ORIENTED_EDGE('',*,*,#9811,.F.);
#14369=ORIENTED_EDGE('',*,*,#9812,.T.);
#14370=ORIENTED_EDGE('',*,*,#9813,.F.);
#14371=ORIENTED_EDGE('',*,*,#9812,.F.);
#14372=ORIENTED_EDGE('',*,*,#9810,.T.);
#14373=ORIENTED_EDGE('',*,*,#9814,.T.);
#14374=ORIENTED_EDGE('',*,*,#9815,.T.);
#14375=ORIENTED_EDGE('',*,*,#9816,.F.);
#14376=ORIENTED_EDGE('',*,*,#9809,.T.);
#14377=ORIENTED_EDGE('',*,*,#9817,.T.);
#14378=ORIENTED_EDGE('',*,*,#9818,.T.);
#14379=ORIENTED_EDGE('',*,*,#9814,.F.);
#14380=ORIENTED_EDGE('',*,*,#9808,.T.);
#14381=ORIENTED_EDGE('',*,*,#9819,.T.);
#14382=ORIENTED_EDGE('',*,*,#9820,.T.);
#14383=ORIENTED_EDGE('',*,*,#9817,.F.);
#14384=ORIENTED_EDGE('',*,*,#9821,.T.);
#14385=ORIENTED_EDGE('',*,*,#9822,.F.);
#14386=ORIENTED_EDGE('',*,*,#9821,.F.);
#14387=ORIENTED_EDGE('',*,*,#9807,.T.);
#14388=ORIENTED_EDGE('',*,*,#9823,.T.);
#14389=ORIENTED_EDGE('',*,*,#9824,.T.);
#14390=ORIENTED_EDGE('',*,*,#9819,.F.);
#14391=ORIENTED_EDGE('',*,*,#9806,.T.);
#14392=ORIENTED_EDGE('',*,*,#9825,.T.);
#14393=ORIENTED_EDGE('',*,*,#9826,.T.);
#14394=ORIENTED_EDGE('',*,*,#9823,.F.);
#14395=ORIENTED_EDGE('',*,*,#9805,.T.);
#14396=ORIENTED_EDGE('',*,*,#9811,.T.);
#14397=ORIENTED_EDGE('',*,*,#9816,.T.);
#14398=ORIENTED_EDGE('',*,*,#9827,.T.);
#14399=ORIENTED_EDGE('',*,*,#9825,.F.);
#14400=ORIENTED_EDGE('',*,*,#9820,.F.);
#14401=ORIENTED_EDGE('',*,*,#9824,.F.);
#14402=ORIENTED_EDGE('',*,*,#9826,.F.);
#14403=ORIENTED_EDGE('',*,*,#9827,.F.);
#14404=ORIENTED_EDGE('',*,*,#9815,.F.);
#14405=ORIENTED_EDGE('',*,*,#9818,.F.);
#14406=ORIENTED_EDGE('',*,*,#9822,.T.);
#14407=ORIENTED_EDGE('',*,*,#9828,.T.);
#14408=ORIENTED_EDGE('',*,*,#9829,.T.);
#14409=ORIENTED_EDGE('',*,*,#9830,.T.);
#14410=ORIENTED_EDGE('',*,*,#9829,.F.);
#14411=ORIENTED_EDGE('',*,*,#9830,.F.);
#14412=ORIENTED_EDGE('',*,*,#9831,.T.);
#14413=ORIENTED_EDGE('',*,*,#9832,.T.);
#14414=ORIENTED_EDGE('',*,*,#9831,.F.);
#14415=ORIENTED_EDGE('',*,*,#9828,.F.);
#14416=ORIENTED_EDGE('',*,*,#9813,.T.);
#14417=ORIENTED_EDGE('',*,*,#9833,.F.);
#14418=ORIENTED_EDGE('',*,*,#9801,.F.);
#14419=ORIENTED_EDGE('',*,*,#9799,.F.);
#14420=ORIENTED_EDGE('',*,*,#9834,.T.);
#14421=ORIENTED_EDGE('',*,*,#9833,.T.);
#14422=ORIENTED_EDGE('',*,*,#9834,.F.);
#14423=ORIENTED_EDGE('',*,*,#9798,.F.);
#14424=ORIENTED_EDGE('',*,*,#9753,.F.);
#14425=ORIENTED_EDGE('',*,*,#9832,.F.);
#14426=ORIENTED_EDGE('',*,*,#9835,.T.);
#14427=ORIENTED_EDGE('',*,*,#9804,.T.);
#14428=ORIENTED_EDGE('',*,*,#9835,.F.);
#14429=ORIENTED_EDGE('',*,*,#9836,.F.);
#14430=ORIENTED_EDGE('',*,*,#9837,.T.);
#14431=ORIENTED_EDGE('',*,*,#9838,.T.);
#14432=ORIENTED_EDGE('',*,*,#9837,.F.);
#14433=ORIENTED_EDGE('',*,*,#9839,.F.);
#14434=ORIENTED_EDGE('',*,*,#9836,.T.);
#14435=ORIENTED_EDGE('',*,*,#9840,.F.);
#14436=ORIENTED_EDGE('',*,*,#9841,.T.);
#14437=ORIENTED_EDGE('',*,*,#9839,.T.);
#14438=ORIENTED_EDGE('',*,*,#9841,.F.);
#14439=ORIENTED_EDGE('',*,*,#9842,.F.);
#14440=ORIENTED_EDGE('',*,*,#9843,.T.);
#14441=ORIENTED_EDGE('',*,*,#9840,.T.);
#14442=ORIENTED_EDGE('',*,*,#9843,.F.);
#14443=ORIENTED_EDGE('',*,*,#9844,.F.);
#14444=ORIENTED_EDGE('',*,*,#9842,.T.);
#14445=ORIENTED_EDGE('',*,*,#9845,.F.);
#14446=ORIENTED_EDGE('',*,*,#9846,.T.);
#14447=ORIENTED_EDGE('',*,*,#9844,.T.);
#14448=ORIENTED_EDGE('',*,*,#9846,.F.);
#14449=ORIENTED_EDGE('',*,*,#9847,.F.);
#14450=ORIENTED_EDGE('',*,*,#9848,.T.);
#14451=ORIENTED_EDGE('',*,*,#9845,.T.);
#14452=ORIENTED_EDGE('',*,*,#9848,.F.);
#14453=ORIENTED_EDGE('',*,*,#9847,.T.);
#14454=ORIENTED_EDGE('',*,*,#9849,.T.);
#14455=ORIENTED_EDGE('',*,*,#9850,.F.);
#14456=ORIENTED_EDGE('',*,*,#9849,.F.);
#14457=ORIENTED_EDGE('',*,*,#9850,.T.);
#14458=ORIENTED_EDGE('',*,*,#9838,.F.);
#14459=PLANE('',#15832);
#14460=PLANE('',#15833);
#14461=PLANE('',#15834);
#14462=PLANE('',#15835);
#14463=PLANE('',#15836);
#14464=PLANE('',#15837);
#14465=PLANE('',#15838);
#14466=PLANE('',#15839);
#14467=PLANE('',#15840);
#14468=PLANE('',#15841);
#14469=PLANE('',#15842);
#14470=PLANE('',#15843);
#14471=PLANE('',#15844);
#14472=PLANE('',#15845);
#14473=PLANE('',#15846);
#14474=PLANE('',#15847);
#14475=PLANE('',#15848);
#14476=PLANE('',#15849);
#14477=PLANE('',#15850);
#14478=PLANE('',#15851);
#14479=PLANE('',#15852);
#14480=PLANE('',#15853);
#14481=PLANE('',#15854);
#14482=PLANE('',#15855);
#14483=PLANE('',#15856);
#14484=PLANE('',#15857);
#14485=PLANE('',#15858);
#14486=PLANE('',#15859);
#14487=PLANE('',#15860);
#14488=PLANE('',#15861);
#14489=PLANE('',#15862);
#14490=PLANE('',#15863);
#14491=PLANE('',#15864);
#14492=PLANE('',#15866);
#14493=PLANE('',#15867);
#14494=PLANE('',#15868);
#14495=PLANE('',#15869);
#14496=PLANE('',#15870);
#14497=PLANE('',#15871);
#14498=PLANE('',#15872);
#14499=PLANE('',#15873);
#14500=PLANE('',#15874);
#14501=PLANE('',#15875);
#14502=PLANE('',#15876);
#14503=PLANE('',#15877);
#14504=PLANE('',#15878);
#14505=PLANE('',#15879);
#14506=PLANE('',#15880);
#14507=PLANE('',#15881);
#14508=PLANE('',#15882);
#14509=PLANE('',#15883);
#14510=PLANE('',#15884);
#14511=PLANE('',#15885);
#14512=PLANE('',#15886);
#14513=PLANE('',#15887);
#14514=PLANE('',#15888);
#14515=PLANE('',#15889);
#14516=PLANE('',#15890);
#14517=PLANE('',#15891);
#14518=PLANE('',#15892);
#14519=PLANE('',#15893);
#14520=PLANE('',#15894);
#14521=PLANE('',#15895);
#14522=PLANE('',#15896);
#14523=PLANE('',#15897);
#14524=PLANE('',#15898);
#14525=PLANE('',#15912);
#14526=PLANE('',#15913);
#14527=PLANE('',#15914);
#14528=PLANE('',#15918);
#14529=PLANE('',#15919);
#14530=PLANE('',#15920);
#14531=PLANE('',#15921);
#14532=PLANE('',#15922);
#14533=PLANE('',#15926);
#14534=PLANE('',#15942);
#14535=PLANE('',#15954);
#14536=PLANE('',#15977);
#14537=PLANE('',#15994);
#14538=PLANE('',#16104);
#14539=PLANE('',#16105);
#14540=PLANE('',#16106);
#14541=PLANE('',#16107);
#14542=PLANE('',#16108);
#14543=PLANE('',#16109);
#14544=PLANE('',#16113);
#14545=PLANE('',#16114);
#14546=PLANE('',#16115);
#14547=PLANE('',#16116);
#14548=PLANE('',#16117);
#14549=PLANE('',#16118);
#14550=PLANE('',#16119);
#14551=PLANE('',#16125);
#14552=PLANE('',#16129);
#14553=PLANE('',#16130);
#14554=PLANE('',#16131);
#14555=PLANE('',#16132);
#14556=PLANE('',#16133);
#14557=PLANE('',#16134);
#14558=PLANE('',#16135);
#14559=PLANE('',#16136);
#14560=PLANE('',#16137);
#14561=PLANE('',#16138);
#14562=PLANE('',#16139);
#14563=PLANE('',#16140);
#14564=PLANE('',#16141);
#14565=PLANE('',#16142);
#14566=PLANE('',#16143);
#14567=PLANE('',#16144);
#14568=PLANE('',#16145);
#14569=PLANE('',#16146);
#14570=PLANE('',#16147);
#14571=PLANE('',#16148);
#14572=PLANE('',#16149);
#14573=PLANE('',#16150);
#14574=PLANE('',#16151);
#14575=PLANE('',#16152);
#14576=PLANE('',#16153);
#14577=PLANE('',#16154);
#14578=PLANE('',#16155);
#14579=PLANE('',#16156);
#14580=PLANE('',#16157);
#14581=PLANE('',#16158);
#14582=PLANE('',#16159);
#14583=PLANE('',#16160);
#14584=PLANE('',#16161);
#14585=PLANE('',#16162);
#14586=PLANE('',#16163);
#14587=PLANE('',#16166);
#14588=PLANE('',#16170);
#14589=PLANE('',#16174);
#14590=PLANE('',#16178);
#14591=PLANE('',#16182);
#14592=PLANE('',#16186);
#14593=PLANE('',#16191);
#14594=PLANE('',#16195);
#14595=PLANE('',#16209);
#14596=PLANE('',#16243);
#14597=PLANE('',#16256);
#14598=PLANE('',#16266);
#14599=PLANE('',#16276);
#14600=PLANE('',#16286);
#14601=PLANE('',#16293);
#14602=PLANE('',#16304);
#14603=PLANE('',#16306);
#14604=PLANE('',#16307);
#14605=PLANE('',#16308);
#14606=PLANE('',#16309);
#14607=PLANE('',#16310);
#14608=PLANE('',#16311);
#14609=PLANE('',#16312);
#14610=PLANE('',#16313);
#14611=PLANE('',#16314);
#14612=PLANE('',#16315);
#14613=PLANE('',#16316);
#14614=PLANE('',#16317);
#14615=PLANE('',#16318);
#14616=PLANE('',#16331);
#14617=PLANE('',#16342);
#14618=PLANE('',#16353);
#14619=PLANE('',#16364);
#14620=PLANE('',#16392);
#14621=PLANE('',#16393);
#14622=PLANE('',#16394);
#14623=PLANE('',#16395);
#14624=PLANE('',#16396);
#14625=PLANE('',#16397);
#14626=PLANE('',#16398);
#14627=PLANE('',#16399);
#14628=PLANE('',#16400);
#14629=PLANE('',#16401);
#14630=PLANE('',#16402);
#14631=PLANE('',#16403);
#14632=PLANE('',#16404);
#14633=PLANE('',#16405);
#14634=PLANE('',#16406);
#14635=PLANE('',#16407);
#14636=PLANE('',#16413);
#14637=PLANE('',#16414);
#14638=PLANE('',#16415);
#14639=PLANE('',#16416);
#14640=PLANE('',#16417);
#14641=PLANE('',#16418);
#14642=PLANE('',#16429);
#14643=PLANE('',#16430);
#14644=PLANE('',#16432);
#14645=PLANE('',#16433);
#14646=PLANE('',#16449);
#14647=PLANE('',#16450);
#14648=PLANE('',#16451);
#14649=PLANE('',#16457);
#14650=PLANE('',#16463);
#14651=PLANE('',#16464);
#14652=PLANE('',#16470);
#14653=PLANE('',#16476);
#14654=PLANE('',#16485);
#14655=PLANE('',#16518);
#14656=PLANE('',#16820);
#14657=PLANE('',#16821);
#14658=PLANE('',#16822);
#14659=PLANE('',#16823);
#14660=PLANE('',#16832);
#14661=PLANE('',#16838);
#14662=PLANE('',#16842);
#14663=PLANE('',#16848);
#14664=PLANE('',#16854);
#14665=PLANE('',#16860);
#14666=PLANE('',#16869);
#14667=PLANE('',#16873);
#14668=PLANE('',#16886);
#14669=PLANE('',#16890);
#14670=PLANE('',#16895);
#14671=PLANE('',#16900);
#14672=PLANE('',#16901);
#14673=PLANE('',#16915);
#14674=PLANE('',#16917);
#14675=PLANE('',#16922);
#14676=PLANE('',#16923);
#14677=PLANE('',#16924);
#14678=PLANE('',#16927);
#14679=PLANE('',#16928);
#14680=PLANE('',#16929);
#14681=PLANE('',#16930);
#14682=PLANE('',#16931);
#14683=PLANE('',#16934);
#14684=PLANE('',#16939);
#14685=PLANE('',#16947);
#14686=PLANE('',#16952);
#14687=PLANE('',#16960);
#14688=PLANE('',#16969);
#14689=PLANE('',#16975);
#14690=PLANE('',#16983);
#14691=PLANE('',#16984);
#14692=PLANE('',#16992);
#14693=PLANE('',#16996);
#14694=PLANE('',#17000);
#14695=PLANE('',#17002);
#14696=PLANE('',#17009);
#14697=PLANE('',#17015);
#14698=PLANE('',#17022);
#14699=PLANE('',#17025);
#14700=PLANE('',#17034);
#14701=PLANE('',#17038);
#14702=PLANE('',#17042);
#14703=PLANE('',#17050);
#14704=PLANE('',#17054);
#14705=PLANE('',#17058);
#14706=PLANE('',#17062);
#14707=PLANE('',#17071);
#14708=PLANE('',#17075);
#14709=PLANE('',#17090);
#14710=PLANE('',#17100);
#14711=PLANE('',#17113);
#14712=PLANE('',#17114);
#14713=PLANE('',#17149);
#14714=PLANE('',#17151);
#14715=PLANE('',#17157);
#14716=PLANE('',#17161);
#14717=PLANE('',#17162);
#14718=PLANE('',#17163);
#14719=PLANE('',#17166);
#14720=PLANE('',#17167);
#14721=PLANE('',#17168);
#14722=PLANE('',#17169);
#14723=PLANE('',#17176);
#14724=PLANE('',#17177);
#14725=PLANE('',#17205);
#14726=PLANE('',#17207);
#14727=PLANE('',#17213);
#14728=PLANE('',#17217);
#14729=PLANE('',#17218);
#14730=PLANE('',#17219);
#14731=PLANE('',#17222);
#14732=PLANE('',#17223);
#14733=PLANE('',#17224);
#14734=PLANE('',#17225);
#14735=PLANE('',#17232);
#14736=PLANE('',#17233);
#14737=PLANE('',#17241);
#14738=PLANE('',#17247);
#14739=PLANE('',#17255);
#14740=PLANE('',#17256);
#14741=ADVANCED_FACE('',(#2385),#14459,.F.);
#14742=ADVANCED_FACE('',(#2386),#14460,.F.);
#14743=ADVANCED_FACE('',(#2387),#14461,.F.);
#14744=ADVANCED_FACE('',(#2388),#14462,.F.);
#14745=ADVANCED_FACE('',(#2389),#14463,.F.);
#14746=ADVANCED_FACE('',(#2390),#14464,.F.);
#14747=ADVANCED_FACE('',(#2391),#14465,.F.);
#14748=ADVANCED_FACE('',(#2392),#14466,.F.);
#14749=ADVANCED_FACE('',(#2393),#14467,.F.);
#14750=ADVANCED_FACE('',(#2394),#14468,.F.);
#14751=ADVANCED_FACE('',(#2395),#14469,.F.);
#14752=ADVANCED_FACE('',(#2396),#14470,.F.);
#14753=ADVANCED_FACE('',(#2397),#14471,.F.);
#14754=ADVANCED_FACE('',(#2398),#14472,.F.);
#14755=ADVANCED_FACE('',(#2399),#14473,.F.);
#14756=ADVANCED_FACE('',(#2400),#14474,.F.);
#14757=ADVANCED_FACE('',(#2401),#14475,.F.);
#14758=ADVANCED_FACE('',(#2402),#14476,.F.);
#14759=ADVANCED_FACE('',(#2403),#14477,.F.);
#14760=ADVANCED_FACE('',(#2404),#14478,.F.);
#14761=ADVANCED_FACE('',(#2405),#14479,.F.);
#14762=ADVANCED_FACE('',(#2406),#14480,.F.);
#14763=ADVANCED_FACE('',(#2407),#14481,.F.);
#14764=ADVANCED_FACE('',(#2408),#14482,.F.);
#14765=ADVANCED_FACE('',(#2409),#14483,.F.);
#14766=ADVANCED_FACE('',(#2410),#14484,.F.);
#14767=ADVANCED_FACE('',(#2411),#14485,.F.);
#14768=ADVANCED_FACE('',(#2412),#14486,.F.);
#14769=ADVANCED_FACE('',(#2413),#14487,.F.);
#14770=ADVANCED_FACE('',(#2414),#14488,.F.);
#14771=ADVANCED_FACE('',(#2415),#14489,.F.);
#14772=ADVANCED_FACE('',(#2416),#14490,.F.);
#14773=ADVANCED_FACE('',(#2417,#1602,#1603,#1604,#1605,#1606),#14491,.T.);
#14774=ADVANCED_FACE('',(#2418),#14492,.F.);
#14775=ADVANCED_FACE('',(#2419),#14493,.F.);
#14776=ADVANCED_FACE('',(#2420),#14494,.F.);
#14777=ADVANCED_FACE('',(#2421),#14495,.F.);
#14778=ADVANCED_FACE('',(#2422),#14496,.F.);
#14779=ADVANCED_FACE('',(#2423),#14497,.F.);
#14780=ADVANCED_FACE('',(#2424),#14498,.F.);
#14781=ADVANCED_FACE('',(#2425),#14499,.F.);
#14782=ADVANCED_FACE('',(#2426),#14500,.F.);
#14783=ADVANCED_FACE('',(#2427),#14501,.F.);
#14784=ADVANCED_FACE('',(#2428),#14502,.F.);
#14785=ADVANCED_FACE('',(#2429),#14503,.F.);
#14786=ADVANCED_FACE('',(#2430),#14504,.F.);
#14787=ADVANCED_FACE('',(#2431),#14505,.F.);
#14788=ADVANCED_FACE('',(#2432),#14506,.F.);
#14789=ADVANCED_FACE('',(#2433),#14507,.F.);
#14790=ADVANCED_FACE('',(#2434),#14508,.F.);
#14791=ADVANCED_FACE('',(#2435),#14509,.F.);
#14792=ADVANCED_FACE('',(#2436),#14510,.F.);
#14793=ADVANCED_FACE('',(#2437),#14511,.F.);
#14794=ADVANCED_FACE('',(#2438),#14512,.F.);
#14795=ADVANCED_FACE('',(#2439),#14513,.F.);
#14796=ADVANCED_FACE('',(#2440),#14514,.F.);
#14797=ADVANCED_FACE('',(#2441),#14515,.F.);
#14798=ADVANCED_FACE('',(#2442),#14516,.F.);
#14799=ADVANCED_FACE('',(#2443),#14517,.F.);
#14800=ADVANCED_FACE('',(#2444),#14518,.F.);
#14801=ADVANCED_FACE('',(#2445),#14519,.F.);
#14802=ADVANCED_FACE('',(#2446),#14520,.F.);
#14803=ADVANCED_FACE('',(#2447),#14521,.F.);
#14804=ADVANCED_FACE('',(#2448),#14522,.F.);
#14805=ADVANCED_FACE('',(#2449),#14523,.F.);
#14806=ADVANCED_FACE('',(#2450,#1607,#1608,#1609,#1610,#1611,#1612,#1613),
#14524,.T.);
#14807=ADVANCED_FACE('',(#2451),#1351,.T.);
#14808=ADVANCED_FACE('',(#2452),#1352,.T.);
#14809=ADVANCED_FACE('',(#2453),#14525,.F.);
#14810=ADVANCED_FACE('',(#2454),#14526,.F.);
#14811=ADVANCED_FACE('',(#2455),#14527,.F.);
#14812=ADVANCED_FACE('',(#2456),#1353,.T.);
#14813=ADVANCED_FACE('',(#2457),#14528,.F.);
#14814=ADVANCED_FACE('',(#2458),#14529,.F.);
#14815=ADVANCED_FACE('',(#2459),#14530,.F.);
#14816=ADVANCED_FACE('',(#2460),#14531,.F.);
#14817=ADVANCED_FACE('',(#2461),#14532,.T.);
#14818=ADVANCED_FACE('',(#2462),#14533,.T.);
#14819=ADVANCED_FACE('',(#2463),#1145,.T.);
#14820=ADVANCED_FACE('',(#2464),#1146,.T.);
#14821=ADVANCED_FACE('',(#2465),#14534,.T.);
#14822=ADVANCED_FACE('',(#2466),#1147,.T.);
#14823=ADVANCED_FACE('',(#2467),#1148,.T.);
#14824=ADVANCED_FACE('',(#2468),#1149,.T.);
#14825=ADVANCED_FACE('',(#2469),#14535,.T.);
#14826=ADVANCED_FACE('',(#2470),#1150,.T.);
#14827=ADVANCED_FACE('',(#2471),#1151,.T.);
#14828=ADVANCED_FACE('',(#2472),#1152,.T.);
#14829=ADVANCED_FACE('',(#2473),#1153,.T.);
#14830=ADVANCED_FACE('',(#2474),#1154,.T.);
#14831=ADVANCED_FACE('',(#2475),#1354,.T.);
#14832=ADVANCED_FACE('',(#2476),#1355,.T.);
#14833=ADVANCED_FACE('',(#2477),#1356,.T.);
#14834=ADVANCED_FACE('',(#2478),#1357,.T.);
#14835=ADVANCED_FACE('',(#2479),#1358,.T.);
#14836=ADVANCED_FACE('',(#2480),#1359,.T.);
#14837=ADVANCED_FACE('',(#2481,#1614,#1615,#1616,#1617,#1618),#14536,.T.);
#14838=ADVANCED_FACE('',(#2482),#1360,.F.);
#14839=ADVANCED_FACE('',(#2483),#1155,.F.);
#14840=ADVANCED_FACE('',(#2484),#1156,.F.);
#14841=ADVANCED_FACE('',(#2485),#1361,.F.);
#14842=ADVANCED_FACE('',(#2486),#1157,.F.);
#14843=ADVANCED_FACE('',(#2487,#1619,#1620,#1621,#1622,#1623,#1624,#1625),
#14537,.T.);
#14844=ADVANCED_FACE('',(#2488),#1158,.F.);
#14845=ADVANCED_FACE('',(#2489,#1626),#1362,.F.);
#14846=ADVANCED_FACE('',(#2490),#1159,.F.);
#14847=ADVANCED_FACE('',(#2491),#1363,.T.);
#14848=ADVANCED_FACE('',(#2492),#1160,.F.);
#14849=ADVANCED_FACE('',(#2493),#1364,.F.);
#14850=ADVANCED_FACE('',(#2494),#1161,.F.);
#14851=ADVANCED_FACE('',(#2495),#1365,.T.);
#14852=ADVANCED_FACE('',(#2496),#1162,.F.);
#14853=ADVANCED_FACE('',(#2497),#1366,.F.);
#14854=ADVANCED_FACE('',(#2498),#1163,.F.);
#14855=ADVANCED_FACE('',(#2499),#1164,.F.);
#14856=ADVANCED_FACE('',(#2500),#1367,.F.);
#14857=ADVANCED_FACE('',(#2501),#1165,.F.);
#14858=ADVANCED_FACE('',(#2502),#1166,.F.);
#14859=ADVANCED_FACE('',(#2503),#1368,.F.);
#14860=ADVANCED_FACE('',(#2504),#1167,.F.);
#14861=ADVANCED_FACE('',(#2505),#1168,.F.);
#14862=ADVANCED_FACE('',(#2506),#1369,.F.);
#14863=ADVANCED_FACE('',(#2507),#1169,.F.);
#14864=ADVANCED_FACE('',(#2508),#1170,.F.);
#14865=ADVANCED_FACE('',(#2509),#1370,.F.);
#14866=ADVANCED_FACE('',(#2510),#1171,.F.);
#14867=ADVANCED_FACE('',(#2511),#1172,.F.);
#14868=ADVANCED_FACE('',(#2512),#1371,.F.);
#14869=ADVANCED_FACE('',(#2513),#1173,.F.);
#14870=ADVANCED_FACE('',(#2514),#1174,.F.);
#14871=ADVANCED_FACE('',(#2515),#1372,.F.);
#14872=ADVANCED_FACE('',(#2516),#1175,.F.);
#14873=ADVANCED_FACE('',(#2517),#1176,.F.);
#14874=ADVANCED_FACE('',(#2518),#1373,.F.);
#14875=ADVANCED_FACE('',(#2519),#1177,.F.);
#14876=ADVANCED_FACE('',(#2520),#1178,.F.);
#14877=ADVANCED_FACE('',(#2521),#1374,.F.);
#14878=ADVANCED_FACE('',(#2522),#1179,.F.);
#14879=ADVANCED_FACE('',(#2523),#1180,.F.);
#14880=ADVANCED_FACE('',(#2524),#1375,.F.);
#14881=ADVANCED_FACE('',(#2525),#1181,.F.);
#14882=ADVANCED_FACE('',(#2526),#1182,.F.);
#14883=ADVANCED_FACE('',(#2527),#1376,.F.);
#14884=ADVANCED_FACE('',(#2528),#1183,.F.);
#14885=ADVANCED_FACE('',(#2529),#1184,.F.);
#14886=ADVANCED_FACE('',(#2530,#1627),#1377,.F.);
#14887=ADVANCED_FACE('',(#2531),#1185,.F.);
#14888=ADVANCED_FACE('',(#2532),#1186,.F.);
#14889=ADVANCED_FACE('',(#2533),#1378,.F.);
#14890=ADVANCED_FACE('',(#2534),#1187,.F.);
#14891=ADVANCED_FACE('',(#2535),#1379,.F.);
#14892=ADVANCED_FACE('',(#2536),#1188,.F.);
#14893=ADVANCED_FACE('',(#2537),#1380,.F.);
#14894=ADVANCED_FACE('',(#2538),#1189,.F.);
#14895=ADVANCED_FACE('',(#2539),#1381,.F.);
#14896=ADVANCED_FACE('',(#2540),#1190,.F.);
#14897=ADVANCED_FACE('',(#2541),#1382,.F.);
#14898=ADVANCED_FACE('',(#2542),#1191,.F.);
#14899=ADVANCED_FACE('',(#2543),#14538,.F.);
#14900=ADVANCED_FACE('',(#2544,#1628),#14539,.F.);
#14901=ADVANCED_FACE('',(#2545),#14540,.F.);
#14902=ADVANCED_FACE('',(#2546),#14541,.F.);
#14903=ADVANCED_FACE('',(#2547,#1629),#14542,.F.);
#14904=ADVANCED_FACE('',(#2548,#1630,#1631,#1632,#1633,#1634,#1635),#14543,
 .T.);
#14905=ADVANCED_FACE('',(#2549,#1636),#14544,.F.);
#14906=ADVANCED_FACE('',(#2550),#14545,.T.);
#14907=ADVANCED_FACE('',(#2551),#14546,.F.);
#14908=ADVANCED_FACE('',(#2552),#14547,.F.);
#14909=ADVANCED_FACE('',(#2553),#14548,.F.);
#14910=ADVANCED_FACE('',(#2554,#1637),#14549,.F.);
#14911=ADVANCED_FACE('',(#2555),#14550,.T.);
#14912=ADVANCED_FACE('',(#2556),#1383,.T.);
#14913=ADVANCED_FACE('',(#2557),#1384,.T.);
#14914=ADVANCED_FACE('',(#2558),#1385,.T.);
#14915=ADVANCED_FACE('',(#2559),#14551,.T.);
#14916=ADVANCED_FACE('',(#2560),#14552,.F.);
#14917=ADVANCED_FACE('',(#2561),#14553,.F.);
#14918=ADVANCED_FACE('',(#2562),#14554,.F.);
#14919=ADVANCED_FACE('',(#2563,#1638,#1639),#14555,.T.);
#14920=ADVANCED_FACE('',(#2564,#1640,#1641),#14556,.T.);
#14921=ADVANCED_FACE('',(#2565),#14557,.F.);
#14922=ADVANCED_FACE('',(#2566),#14558,.F.);
#14923=ADVANCED_FACE('',(#2567),#14559,.F.);
#14924=ADVANCED_FACE('',(#2568),#14560,.F.);
#14925=ADVANCED_FACE('',(#2569),#14561,.F.);
#14926=ADVANCED_FACE('',(#2570),#14562,.F.);
#14927=ADVANCED_FACE('',(#2571),#14563,.F.);
#14928=ADVANCED_FACE('',(#2572),#14564,.F.);
#14929=ADVANCED_FACE('',(#2573),#14565,.F.);
#14930=ADVANCED_FACE('',(#2574),#14566,.F.);
#14931=ADVANCED_FACE('',(#2575),#14567,.F.);
#14932=ADVANCED_FACE('',(#2576),#14568,.F.);
#14933=ADVANCED_FACE('',(#2577),#14569,.F.);
#14934=ADVANCED_FACE('',(#2578),#14570,.F.);
#14935=ADVANCED_FACE('',(#2579),#14571,.F.);
#14936=ADVANCED_FACE('',(#2580),#14572,.F.);
#14937=ADVANCED_FACE('',(#2581),#14573,.F.);
#14938=ADVANCED_FACE('',(#2582),#14574,.F.);
#14939=ADVANCED_FACE('',(#2583),#14575,.F.);
#14940=ADVANCED_FACE('',(#2584),#14576,.F.);
#14941=ADVANCED_FACE('',(#2585),#14577,.F.);
#14942=ADVANCED_FACE('',(#2586),#14578,.F.);
#14943=ADVANCED_FACE('',(#2587),#14579,.F.);
#14944=ADVANCED_FACE('',(#2588),#14580,.F.);
#14945=ADVANCED_FACE('',(#2589),#14581,.F.);
#14946=ADVANCED_FACE('',(#2590),#14582,.F.);
#14947=ADVANCED_FACE('',(#2591),#14583,.F.);
#14948=ADVANCED_FACE('',(#2592),#14584,.F.);
#14949=ADVANCED_FACE('',(#2593),#14585,.F.);
#14950=ADVANCED_FACE('',(#2594),#14586,.F.);
#14951=ADVANCED_FACE('',(#2595),#1386,.F.);
#14952=ADVANCED_FACE('',(#2596,#1642),#14587,.F.);
#14953=ADVANCED_FACE('',(#2597),#1387,.F.);
#14954=ADVANCED_FACE('',(#2598,#1643),#14588,.F.);
#14955=ADVANCED_FACE('',(#2599),#1388,.F.);
#14956=ADVANCED_FACE('',(#2600,#1644),#14589,.F.);
#14957=ADVANCED_FACE('',(#2601,#1645),#1389,.F.);
#14958=ADVANCED_FACE('',(#2602,#1646),#14590,.F.);
#14959=ADVANCED_FACE('',(#2603),#1390,.F.);
#14960=ADVANCED_FACE('',(#2604,#1647),#14591,.F.);
#14961=ADVANCED_FACE('',(#2605),#1391,.F.);
#14962=ADVANCED_FACE('',(#2606,#1648),#14592,.F.);
#14963=ADVANCED_FACE('',(#2607),#1392,.F.);
#14964=ADVANCED_FACE('',(#2608,#1649),#1393,.F.);
#14965=ADVANCED_FACE('',(#2609,#1650),#14593,.F.);
#14966=ADVANCED_FACE('',(#2610),#1394,.F.);
#14967=ADVANCED_FACE('',(#2611,#1651),#14594,.F.);
#14968=ADVANCED_FACE('',(#2612),#1395,.F.);
#14969=ADVANCED_FACE('',(#2613),#1192,.F.);
#14970=ADVANCED_FACE('',(#2614),#1396,.T.);
#14971=ADVANCED_FACE('',(#2615),#1397,.T.);
#14972=ADVANCED_FACE('',(#2616),#1398,.T.);
#14973=ADVANCED_FACE('',(#2617),#1193,.T.);
#14974=ADVANCED_FACE('',(#2618),#1399,.T.);
#14975=ADVANCED_FACE('',(#2619,#1652),#14595,.T.);
#14976=ADVANCED_FACE('',(#2620),#1194,.T.);
#14977=ADVANCED_FACE('',(#2621),#1195,.T.);
#14978=ADVANCED_FACE('',(#2622),#1196,.T.);
#14979=ADVANCED_FACE('',(#2623),#1197,.T.);
#14980=ADVANCED_FACE('',(#2624),#1198,.T.);
#14981=ADVANCED_FACE('',(#2625),#1199,.T.);
#14982=ADVANCED_FACE('',(#2626),#1200,.T.);
#14983=ADVANCED_FACE('',(#2627),#1201,.T.);
#14984=ADVANCED_FACE('',(#2628),#1400,.T.);
#14985=ADVANCED_FACE('',(#2629),#1401,.T.);
#14986=ADVANCED_FACE('',(#2630),#1402,.T.);
#14987=ADVANCED_FACE('',(#2631),#1403,.T.);
#14988=ADVANCED_FACE('',(#2632,#1653,#1654,#1655,#1656,#1657),#14596,.F.);
#14989=ADVANCED_FACE('',(#2633),#1202,.F.);
#14990=ADVANCED_FACE('',(#2634),#1404,.F.);
#14991=ADVANCED_FACE('',(#2635),#1203,.F.);
#14992=ADVANCED_FACE('',(#2636,#1658),#14597,.F.);
#14993=ADVANCED_FACE('',(#2637),#1405,.F.);
#14994=ADVANCED_FACE('',(#2638),#1204,.F.);
#14995=ADVANCED_FACE('',(#2639),#1406,.F.);
#14996=ADVANCED_FACE('',(#2640),#1205,.F.);
#14997=ADVANCED_FACE('',(#2641,#1659),#14598,.F.);
#14998=ADVANCED_FACE('',(#2642),#1407,.F.);
#14999=ADVANCED_FACE('',(#2643),#1206,.F.);
#15000=ADVANCED_FACE('',(#2644),#1408,.F.);
#15001=ADVANCED_FACE('',(#2645),#1207,.F.);
#15002=ADVANCED_FACE('',(#2646,#1660),#14599,.F.);
#15003=ADVANCED_FACE('',(#2647),#1409,.F.);
#15004=ADVANCED_FACE('',(#2648),#1208,.F.);
#15005=ADVANCED_FACE('',(#2649),#1410,.F.);
#15006=ADVANCED_FACE('',(#2650),#1209,.F.);
#15007=ADVANCED_FACE('',(#2651,#1661),#14600,.F.);
#15008=ADVANCED_FACE('',(#2652),#1411,.F.);
#15009=ADVANCED_FACE('',(#2653),#1210,.F.);
#15010=ADVANCED_FACE('',(#2654),#1412,.F.);
#15011=ADVANCED_FACE('',(#2655,#1662),#14601,.F.);
#15012=ADVANCED_FACE('',(#2656),#1413,.F.);
#15013=ADVANCED_FACE('',(#2657),#1414,.T.);
#15014=ADVANCED_FACE('',(#2658),#1415,.T.);
#15015=ADVANCED_FACE('',(#2659),#1416,.T.);
#15016=ADVANCED_FACE('',(#2660),#1417,.T.);
#15017=ADVANCED_FACE('',(#2661,#1663,#1664,#1665,#1666,#1667),#14602,.T.);
#15018=ADVANCED_FACE('',(#2662),#14603,.T.);
#15019=ADVANCED_FACE('',(#2663),#14604,.T.);
#15020=ADVANCED_FACE('',(#2664),#14605,.T.);
#15021=ADVANCED_FACE('',(#2665),#14606,.T.);
#15022=ADVANCED_FACE('',(#2666),#14607,.T.);
#15023=ADVANCED_FACE('',(#2667),#14608,.T.);
#15024=ADVANCED_FACE('',(#2668),#14609,.T.);
#15025=ADVANCED_FACE('',(#2669),#14610,.T.);
#15026=ADVANCED_FACE('',(#2670),#14611,.T.);
#15027=ADVANCED_FACE('',(#2671),#14612,.T.);
#15028=ADVANCED_FACE('',(#2672),#14613,.T.);
#15029=ADVANCED_FACE('',(#2673),#14614,.T.);
#15030=ADVANCED_FACE('',(#2674,#1668,#1669,#1670,#1671,#1672,#1673,#1674,
#1675,#1676),#14615,.T.);
#15031=ADVANCED_FACE('',(#2675),#1211,.F.);
#15032=ADVANCED_FACE('',(#2676),#1418,.F.);
#15033=ADVANCED_FACE('',(#2677),#1212,.F.);
#15034=ADVANCED_FACE('',(#2678,#1677),#14616,.F.);
#15035=ADVANCED_FACE('',(#2679),#1419,.F.);
#15036=ADVANCED_FACE('',(#2680),#1213,.F.);
#15037=ADVANCED_FACE('',(#2681),#1420,.F.);
#15038=ADVANCED_FACE('',(#2682),#1214,.F.);
#15039=ADVANCED_FACE('',(#2683,#1678),#14617,.F.);
#15040=ADVANCED_FACE('',(#2684),#1421,.F.);
#15041=ADVANCED_FACE('',(#2685),#1215,.F.);
#15042=ADVANCED_FACE('',(#2686),#1422,.F.);
#15043=ADVANCED_FACE('',(#2687),#1216,.F.);
#15044=ADVANCED_FACE('',(#2688,#1679),#14618,.F.);
#15045=ADVANCED_FACE('',(#2689),#1423,.F.);
#15046=ADVANCED_FACE('',(#2690),#1217,.F.);
#15047=ADVANCED_FACE('',(#2691),#1424,.F.);
#15048=ADVANCED_FACE('',(#2692),#1218,.F.);
#15049=ADVANCED_FACE('',(#2693,#1680),#14619,.F.);
#15050=ADVANCED_FACE('',(#2694),#1425,.F.);
#15051=ADVANCED_FACE('',(#2695),#1219,.F.);
#15052=ADVANCED_FACE('',(#2696),#1426,.F.);
#15053=ADVANCED_FACE('',(#2697),#1220,.F.);
#15054=ADVANCED_FACE('',(#2698),#1221,.F.);
#15055=ADVANCED_FACE('',(#2699),#1427,.F.);
#15056=ADVANCED_FACE('',(#2700),#1222,.F.);
#15057=ADVANCED_FACE('',(#2701),#1223,.F.);
#15058=ADVANCED_FACE('',(#2702),#1428,.F.);
#15059=ADVANCED_FACE('',(#2703),#1224,.F.);
#15060=ADVANCED_FACE('',(#2704),#1225,.F.);
#15061=ADVANCED_FACE('',(#2705),#1429,.F.);
#15062=ADVANCED_FACE('',(#2706),#1226,.F.);
#15063=ADVANCED_FACE('',(#2707),#14620,.F.);
#15064=ADVANCED_FACE('',(#2708),#14621,.F.);
#15065=ADVANCED_FACE('',(#2709),#14622,.F.);
#15066=ADVANCED_FACE('',(#2710),#14623,.F.);
#15067=ADVANCED_FACE('',(#2711),#14624,.F.);
#15068=ADVANCED_FACE('',(#2712),#14625,.F.);
#15069=ADVANCED_FACE('',(#2713),#14626,.F.);
#15070=ADVANCED_FACE('',(#2714),#14627,.F.);
#15071=ADVANCED_FACE('',(#2715),#14628,.F.);
#15072=ADVANCED_FACE('',(#2716),#14629,.F.);
#15073=ADVANCED_FACE('',(#2717),#14630,.F.);
#15074=ADVANCED_FACE('',(#2718),#14631,.F.);
#15075=ADVANCED_FACE('',(#2719),#14632,.F.);
#15076=ADVANCED_FACE('',(#2720),#14633,.F.);
#15077=ADVANCED_FACE('',(#2721),#14634,.F.);
#15078=ADVANCED_FACE('',(#2722),#14635,.F.);
#15079=ADVANCED_FACE('',(#2723),#1430,.F.);
#15080=ADVANCED_FACE('',(#2724),#1431,.F.);
#15081=ADVANCED_FACE('',(#2725,#1681,#1682,#1683,#1684,#1685),#14636,.F.);
#15082=ADVANCED_FACE('',(#2726),#14637,.T.);
#15083=ADVANCED_FACE('',(#2727),#14638,.T.);
#15084=ADVANCED_FACE('',(#2728),#14639,.T.);
#15085=ADVANCED_FACE('',(#2729),#14640,.T.);
#15086=ADVANCED_FACE('',(#2730,#1686,#1687,#1688,#1689,#1690,#1691,#1692,
#1693,#1694,#1695,#1696,#1697,#1698),#14641,.T.);
#15087=ADVANCED_FACE('',(#2731),#1432,.T.);
#15088=ADVANCED_FACE('',(#2732),#1433,.T.);
#15089=ADVANCED_FACE('',(#2733),#1434,.T.);
#15090=ADVANCED_FACE('',(#2734),#1435,.T.);
#15091=ADVANCED_FACE('',(#2735),#1436,.T.);
#15092=ADVANCED_FACE('',(#2736),#1437,.T.);
#15093=ADVANCED_FACE('',(#2737),#1438,.T.);
#15094=ADVANCED_FACE('',(#2738),#14642,.F.);
#15095=ADVANCED_FACE('',(#2739),#14643,.F.);
#15096=ADVANCED_FACE('',(#2740),#14644,.F.);
#15097=ADVANCED_FACE('',(#2741),#14645,.F.);
#15098=ADVANCED_FACE('',(#2742),#1439,.F.);
#15099=ADVANCED_FACE('',(#2743),#1227,.F.);
#15100=ADVANCED_FACE('',(#2744),#1228,.F.);
#15101=ADVANCED_FACE('',(#2745),#1440,.T.);
#15102=ADVANCED_FACE('',(#2746),#1229,.T.);
#15103=ADVANCED_FACE('',(#2747),#1230,.T.);
#15104=ADVANCED_FACE('',(#2748),#1441,.T.);
#15105=ADVANCED_FACE('',(#2749),#161,.T.);
#15106=ADVANCED_FACE('',(#2750),#162,.T.);
#15107=ADVANCED_FACE('',(#2751),#14646,.T.);
#15108=ADVANCED_FACE('',(#2752),#163,.T.);
#15109=ADVANCED_FACE('',(#2753),#14647,.T.);
#15110=ADVANCED_FACE('',(#2754),#14648,.T.);
#15111=ADVANCED_FACE('',(#2755),#1231,.T.);
#15112=ADVANCED_FACE('',(#2756),#1442,.T.);
#15113=ADVANCED_FACE('',(#2757,#1699),#14649,.T.);
#15114=ADVANCED_FACE('',(#2758),#1232,.T.);
#15115=ADVANCED_FACE('',(#2759),#1443,.T.);
#15116=ADVANCED_FACE('',(#2760,#1700),#14650,.T.);
#15117=ADVANCED_FACE('',(#2761,#1701),#14651,.T.);
#15118=ADVANCED_FACE('',(#2762),#1444,.T.);
#15119=ADVANCED_FACE('',(#2763),#1233,.T.);
#15120=ADVANCED_FACE('',(#2764,#1702),#14652,.T.);
#15121=ADVANCED_FACE('',(#2765),#1445,.T.);
#15122=ADVANCED_FACE('',(#2766),#1234,.T.);
#15123=ADVANCED_FACE('',(#2767,#1703),#14653,.T.);
#15124=ADVANCED_FACE('',(#2768),#1235,.F.);
#15125=ADVANCED_FACE('',(#2769),#1446,.F.);
#15126=ADVANCED_FACE('',(#2770,#1704),#14654,.T.);
#15127=ADVANCED_FACE('',(#2771),#1236,.F.);
#15128=ADVANCED_FACE('',(#2772,#1705),#14655,.T.);
#15129=ADVANCED_FACE('',(#2773),#164,.F.);
#15130=ADVANCED_FACE('',(#2774),#165,.F.);
#15131=ADVANCED_FACE('',(#2775),#166,.F.);
#15132=ADVANCED_FACE('',(#2776),#1237,.T.);
#15133=ADVANCED_FACE('',(#2777),#1447,.T.);
#15134=ADVANCED_FACE('',(#2778),#127,.F.);
#15135=ADVANCED_FACE('',(#2779),#1448,.T.);
#15136=ADVANCED_FACE('',(#2780),#1238,.T.);
#15137=ADVANCED_FACE('',(#2781),#167,.F.);
#15138=ADVANCED_FACE('',(#2782),#168,.F.);
#15139=ADVANCED_FACE('',(#2783),#169,.F.);
#15140=ADVANCED_FACE('',(#2784),#1239,.T.);
#15141=ADVANCED_FACE('',(#2785),#1449,.T.);
#15142=ADVANCED_FACE('',(#2786),#128,.F.);
#15143=ADVANCED_FACE('',(#2787),#1450,.T.);
#15144=ADVANCED_FACE('',(#2788),#1240,.T.);
#15145=ADVANCED_FACE('',(#2789),#170,.F.);
#15146=ADVANCED_FACE('',(#2790),#171,.F.);
#15147=ADVANCED_FACE('',(#2791),#172,.F.);
#15148=ADVANCED_FACE('',(#2792),#1241,.T.);
#15149=ADVANCED_FACE('',(#2793),#1451,.T.);
#15150=ADVANCED_FACE('',(#2794),#129,.F.);
#15151=ADVANCED_FACE('',(#2795),#1452,.T.);
#15152=ADVANCED_FACE('',(#2796),#1242,.T.);
#15153=ADVANCED_FACE('',(#2797),#173,.F.);
#15154=ADVANCED_FACE('',(#2798),#174,.F.);
#15155=ADVANCED_FACE('',(#2799),#175,.F.);
#15156=ADVANCED_FACE('',(#2800),#1243,.T.);
#15157=ADVANCED_FACE('',(#2801),#1453,.T.);
#15158=ADVANCED_FACE('',(#2802),#130,.F.);
#15159=ADVANCED_FACE('',(#2803),#1454,.T.);
#15160=ADVANCED_FACE('',(#2804),#1244,.T.);
#15161=ADVANCED_FACE('',(#2805),#176,.F.);
#15162=ADVANCED_FACE('',(#2806),#177,.F.);
#15163=ADVANCED_FACE('',(#2807),#178,.F.);
#15164=ADVANCED_FACE('',(#2808),#1245,.T.);
#15165=ADVANCED_FACE('',(#2809),#1455,.T.);
#15166=ADVANCED_FACE('',(#2810),#131,.F.);
#15167=ADVANCED_FACE('',(#2811),#1456,.T.);
#15168=ADVANCED_FACE('',(#2812),#1246,.T.);
#15169=ADVANCED_FACE('',(#2813),#179,.F.);
#15170=ADVANCED_FACE('',(#2814),#180,.F.);
#15171=ADVANCED_FACE('',(#2815),#181,.F.);
#15172=ADVANCED_FACE('',(#2816),#1247,.T.);
#15173=ADVANCED_FACE('',(#2817),#1457,.T.);
#15174=ADVANCED_FACE('',(#2818),#132,.F.);
#15175=ADVANCED_FACE('',(#2819),#1458,.T.);
#15176=ADVANCED_FACE('',(#2820),#1248,.T.);
#15177=ADVANCED_FACE('',(#2821),#182,.F.);
#15178=ADVANCED_FACE('',(#2822),#183,.F.);
#15179=ADVANCED_FACE('',(#2823),#184,.F.);
#15180=ADVANCED_FACE('',(#2824),#1249,.T.);
#15181=ADVANCED_FACE('',(#2825),#1459,.T.);
#15182=ADVANCED_FACE('',(#2826),#133,.F.);
#15183=ADVANCED_FACE('',(#2827),#1460,.T.);
#15184=ADVANCED_FACE('',(#2828),#1250,.T.);
#15185=ADVANCED_FACE('',(#2829),#185,.F.);
#15186=ADVANCED_FACE('',(#2830),#186,.F.);
#15187=ADVANCED_FACE('',(#2831),#187,.F.);
#15188=ADVANCED_FACE('',(#2832),#1251,.T.);
#15189=ADVANCED_FACE('',(#2833),#1461,.T.);
#15190=ADVANCED_FACE('',(#2834),#134,.F.);
#15191=ADVANCED_FACE('',(#2835),#1462,.T.);
#15192=ADVANCED_FACE('',(#2836),#1252,.T.);
#15193=ADVANCED_FACE('',(#2837),#188,.F.);
#15194=ADVANCED_FACE('',(#2838),#189,.F.);
#15195=ADVANCED_FACE('',(#2839),#190,.F.);
#15196=ADVANCED_FACE('',(#2840),#1253,.T.);
#15197=ADVANCED_FACE('',(#2841),#1463,.T.);
#15198=ADVANCED_FACE('',(#2842),#135,.F.);
#15199=ADVANCED_FACE('',(#2843),#1464,.T.);
#15200=ADVANCED_FACE('',(#2844),#1254,.T.);
#15201=ADVANCED_FACE('',(#2845),#191,.F.);
#15202=ADVANCED_FACE('',(#2846),#192,.F.);
#15203=ADVANCED_FACE('',(#2847),#193,.F.);
#15204=ADVANCED_FACE('',(#2848),#1255,.T.);
#15205=ADVANCED_FACE('',(#2849),#1465,.T.);
#15206=ADVANCED_FACE('',(#2850),#136,.F.);
#15207=ADVANCED_FACE('',(#2851),#1466,.T.);
#15208=ADVANCED_FACE('',(#2852),#1256,.T.);
#15209=ADVANCED_FACE('',(#2853),#194,.F.);
#15210=ADVANCED_FACE('',(#2854),#195,.F.);
#15211=ADVANCED_FACE('',(#2855),#196,.F.);
#15212=ADVANCED_FACE('',(#2856),#1257,.T.);
#15213=ADVANCED_FACE('',(#2857),#1467,.T.);
#15214=ADVANCED_FACE('',(#2858),#137,.F.);
#15215=ADVANCED_FACE('',(#2859),#1468,.T.);
#15216=ADVANCED_FACE('',(#2860),#1258,.T.);
#15217=ADVANCED_FACE('',(#2861),#197,.F.);
#15218=ADVANCED_FACE('',(#2862),#198,.F.);
#15219=ADVANCED_FACE('',(#2863),#199,.F.);
#15220=ADVANCED_FACE('',(#2864),#1259,.T.);
#15221=ADVANCED_FACE('',(#2865),#1469,.T.);
#15222=ADVANCED_FACE('',(#2866),#138,.F.);
#15223=ADVANCED_FACE('',(#2867),#1470,.T.);
#15224=ADVANCED_FACE('',(#2868),#1260,.T.);
#15225=ADVANCED_FACE('',(#2869),#200,.F.);
#15226=ADVANCED_FACE('',(#2870),#201,.F.);
#15227=ADVANCED_FACE('',(#2871),#202,.F.);
#15228=ADVANCED_FACE('',(#2872),#1261,.T.);
#15229=ADVANCED_FACE('',(#2873),#1471,.T.);
#15230=ADVANCED_FACE('',(#2874),#139,.F.);
#15231=ADVANCED_FACE('',(#2875),#1472,.T.);
#15232=ADVANCED_FACE('',(#2876),#1262,.T.);
#15233=ADVANCED_FACE('',(#2877),#203,.F.);
#15234=ADVANCED_FACE('',(#2878),#204,.F.);
#15235=ADVANCED_FACE('',(#2879),#205,.F.);
#15236=ADVANCED_FACE('',(#2880),#1263,.T.);
#15237=ADVANCED_FACE('',(#2881),#1473,.T.);
#15238=ADVANCED_FACE('',(#2882),#140,.F.);
#15239=ADVANCED_FACE('',(#2883),#1474,.T.);
#15240=ADVANCED_FACE('',(#2884),#1264,.T.);
#15241=ADVANCED_FACE('',(#2885),#206,.F.);
#15242=ADVANCED_FACE('',(#2886),#207,.F.);
#15243=ADVANCED_FACE('',(#2887),#208,.F.);
#15244=ADVANCED_FACE('',(#2888),#1265,.T.);
#15245=ADVANCED_FACE('',(#2889),#1475,.T.);
#15246=ADVANCED_FACE('',(#2890),#141,.F.);
#15247=ADVANCED_FACE('',(#2891),#1476,.T.);
#15248=ADVANCED_FACE('',(#2892),#1266,.T.);
#15249=ADVANCED_FACE('',(#2893),#209,.F.);
#15250=ADVANCED_FACE('',(#2894),#210,.F.);
#15251=ADVANCED_FACE('',(#2895),#211,.F.);
#15252=ADVANCED_FACE('',(#2896),#1267,.T.);
#15253=ADVANCED_FACE('',(#2897),#1477,.T.);
#15254=ADVANCED_FACE('',(#2898),#142,.F.);
#15255=ADVANCED_FACE('',(#2899),#1478,.T.);
#15256=ADVANCED_FACE('',(#2900),#1268,.T.);
#15257=ADVANCED_FACE('',(#2901),#212,.F.);
#15258=ADVANCED_FACE('',(#2902),#213,.F.);
#15259=ADVANCED_FACE('',(#2903),#214,.F.);
#15260=ADVANCED_FACE('',(#2904),#1269,.T.);
#15261=ADVANCED_FACE('',(#2905),#1479,.T.);
#15262=ADVANCED_FACE('',(#2906),#143,.F.);
#15263=ADVANCED_FACE('',(#2907),#1480,.T.);
#15264=ADVANCED_FACE('',(#2908),#1270,.T.);
#15265=ADVANCED_FACE('',(#2909),#215,.F.);
#15266=ADVANCED_FACE('',(#2910),#216,.F.);
#15267=ADVANCED_FACE('',(#2911),#217,.F.);
#15268=ADVANCED_FACE('',(#2912),#1271,.T.);
#15269=ADVANCED_FACE('',(#2913),#1481,.T.);
#15270=ADVANCED_FACE('',(#2914),#144,.F.);
#15271=ADVANCED_FACE('',(#2915),#1482,.T.);
#15272=ADVANCED_FACE('',(#2916),#1272,.T.);
#15273=ADVANCED_FACE('',(#2917),#218,.F.);
#15274=ADVANCED_FACE('',(#2918),#219,.F.);
#15275=ADVANCED_FACE('',(#2919),#220,.F.);
#15276=ADVANCED_FACE('',(#2920),#1273,.T.);
#15277=ADVANCED_FACE('',(#2921),#1483,.T.);
#15278=ADVANCED_FACE('',(#2922),#145,.F.);
#15279=ADVANCED_FACE('',(#2923),#1484,.T.);
#15280=ADVANCED_FACE('',(#2924),#1274,.T.);
#15281=ADVANCED_FACE('',(#2925),#221,.F.);
#15282=ADVANCED_FACE('',(#2926),#222,.F.);
#15283=ADVANCED_FACE('',(#2927),#223,.F.);
#15284=ADVANCED_FACE('',(#2928),#1275,.T.);
#15285=ADVANCED_FACE('',(#2929),#1485,.T.);
#15286=ADVANCED_FACE('',(#2930),#146,.F.);
#15287=ADVANCED_FACE('',(#2931),#1486,.T.);
#15288=ADVANCED_FACE('',(#2932),#1276,.T.);
#15289=ADVANCED_FACE('',(#2933),#224,.F.);
#15290=ADVANCED_FACE('',(#2934),#225,.F.);
#15291=ADVANCED_FACE('',(#2935),#226,.F.);
#15292=ADVANCED_FACE('',(#2936),#1277,.T.);
#15293=ADVANCED_FACE('',(#2937),#1487,.T.);
#15294=ADVANCED_FACE('',(#2938),#147,.F.);
#15295=ADVANCED_FACE('',(#2939),#1488,.T.);
#15296=ADVANCED_FACE('',(#2940),#1278,.T.);
#15297=ADVANCED_FACE('',(#2941),#227,.F.);
#15298=ADVANCED_FACE('',(#2942),#228,.F.);
#15299=ADVANCED_FACE('',(#2943),#229,.F.);
#15300=ADVANCED_FACE('',(#2944),#1279,.T.);
#15301=ADVANCED_FACE('',(#2945),#1489,.T.);
#15302=ADVANCED_FACE('',(#2946),#148,.F.);
#15303=ADVANCED_FACE('',(#2947),#1490,.T.);
#15304=ADVANCED_FACE('',(#2948),#1280,.T.);
#15305=ADVANCED_FACE('',(#2949),#230,.F.);
#15306=ADVANCED_FACE('',(#2950),#231,.F.);
#15307=ADVANCED_FACE('',(#2951),#232,.F.);
#15308=ADVANCED_FACE('',(#2952),#1281,.T.);
#15309=ADVANCED_FACE('',(#2953),#1491,.T.);
#15310=ADVANCED_FACE('',(#2954),#149,.F.);
#15311=ADVANCED_FACE('',(#2955),#1492,.T.);
#15312=ADVANCED_FACE('',(#2956),#1282,.T.);
#15313=ADVANCED_FACE('',(#2957),#233,.F.);
#15314=ADVANCED_FACE('',(#2958),#234,.F.);
#15315=ADVANCED_FACE('',(#2959),#235,.F.);
#15316=ADVANCED_FACE('',(#2960),#1283,.T.);
#15317=ADVANCED_FACE('',(#2961),#1493,.T.);
#15318=ADVANCED_FACE('',(#2962),#150,.F.);
#15319=ADVANCED_FACE('',(#2963),#1494,.T.);
#15320=ADVANCED_FACE('',(#2964),#1284,.T.);
#15321=ADVANCED_FACE('',(#2965),#236,.F.);
#15322=ADVANCED_FACE('',(#2966),#237,.F.);
#15323=ADVANCED_FACE('',(#2967),#238,.F.);
#15324=ADVANCED_FACE('',(#2968),#1285,.T.);
#15325=ADVANCED_FACE('',(#2969),#1495,.T.);
#15326=ADVANCED_FACE('',(#2970),#151,.F.);
#15327=ADVANCED_FACE('',(#2971),#1496,.T.);
#15328=ADVANCED_FACE('',(#2972),#1286,.T.);
#15329=ADVANCED_FACE('',(#2973),#239,.F.);
#15330=ADVANCED_FACE('',(#2974),#240,.F.);
#15331=ADVANCED_FACE('',(#2975),#241,.F.);
#15332=ADVANCED_FACE('',(#2976),#1287,.T.);
#15333=ADVANCED_FACE('',(#2977),#1497,.T.);
#15334=ADVANCED_FACE('',(#2978),#152,.F.);
#15335=ADVANCED_FACE('',(#2979),#1498,.T.);
#15336=ADVANCED_FACE('',(#2980),#1288,.T.);
#15337=ADVANCED_FACE('',(#2981),#242,.F.);
#15338=ADVANCED_FACE('',(#2982),#243,.F.);
#15339=ADVANCED_FACE('',(#2983),#244,.F.);
#15340=ADVANCED_FACE('',(#2984),#1289,.T.);
#15341=ADVANCED_FACE('',(#2985),#1499,.T.);
#15342=ADVANCED_FACE('',(#2986),#153,.F.);
#15343=ADVANCED_FACE('',(#2987),#1500,.T.);
#15344=ADVANCED_FACE('',(#2988),#1290,.T.);
#15345=ADVANCED_FACE('',(#2989),#245,.F.);
#15346=ADVANCED_FACE('',(#2990),#246,.F.);
#15347=ADVANCED_FACE('',(#2991),#247,.F.);
#15348=ADVANCED_FACE('',(#2992),#1291,.T.);
#15349=ADVANCED_FACE('',(#2993),#1292,.T.);
#15350=ADVANCED_FACE('',(#2994),#1501,.T.);
#15351=ADVANCED_FACE('',(#2995),#154,.F.);
#15352=ADVANCED_FACE('',(#2996),#1502,.T.);
#15353=ADVANCED_FACE('',(#2997),#1293,.T.);
#15354=ADVANCED_FACE('',(#2998),#248,.F.);
#15355=ADVANCED_FACE('',(#2999),#249,.F.);
#15356=ADVANCED_FACE('',(#3000),#250,.F.);
#15357=ADVANCED_FACE('',(#3001),#1294,.T.);
#15358=ADVANCED_FACE('',(#3002),#1503,.T.);
#15359=ADVANCED_FACE('',(#3003),#1504,.T.);
#15360=ADVANCED_FACE('',(#3004),#1295,.T.);
#15361=ADVANCED_FACE('',(#3005),#155,.F.);
#15362=ADVANCED_FACE('',(#3006),#1505,.T.);
#15363=ADVANCED_FACE('',(#3007),#251,.F.);
#15364=ADVANCED_FACE('',(#3008),#252,.F.);
#15365=ADVANCED_FACE('',(#3009),#253,.F.);
#15366=ADVANCED_FACE('',(#3010),#1506,.T.);
#15367=ADVANCED_FACE('',(#3011),#156,.F.);
#15368=ADVANCED_FACE('',(#3012),#1296,.T.);
#15369=ADVANCED_FACE('',(#3013),#14656,.F.);
#15370=ADVANCED_FACE('',(#3014),#14657,.F.);
#15371=ADVANCED_FACE('',(#3015),#14658,.F.);
#15372=ADVANCED_FACE('',(#3016,#1706),#14659,.T.);
#15373=ADVANCED_FACE('',(#3017),#1297,.F.);
#15374=ADVANCED_FACE('',(#3018),#1298,.T.);
#15375=ADVANCED_FACE('',(#3019),#1507,.T.);
#15376=ADVANCED_FACE('',(#3020,#1707),#14660,.T.);
#15377=ADVANCED_FACE('',(#3021),#1299,.T.);
#15378=ADVANCED_FACE('',(#3022),#1508,.T.);
#15379=ADVANCED_FACE('',(#3023,#1708),#14661,.T.);
#15380=ADVANCED_FACE('',(#3024),#1509,.T.);
#15381=ADVANCED_FACE('',(#3025,#1709),#14662,.T.);
#15382=ADVANCED_FACE('',(#3026),#1510,.T.);
#15383=ADVANCED_FACE('',(#3027),#1300,.T.);
#15384=ADVANCED_FACE('',(#3028,#1710),#14663,.T.);
#15385=ADVANCED_FACE('',(#3029),#1511,.T.);
#15386=ADVANCED_FACE('',(#3030),#1301,.T.);
#15387=ADVANCED_FACE('',(#3031,#1711),#14664,.T.);
#15388=ADVANCED_FACE('',(#3032),#1302,.F.);
#15389=ADVANCED_FACE('',(#3033),#1512,.F.);
#15390=ADVANCED_FACE('',(#3034,#1712),#14665,.T.);
#15391=ADVANCED_FACE('',(#3035),#1303,.T.);
#15392=ADVANCED_FACE('',(#3036),#1513,.T.);
#15393=ADVANCED_FACE('',(#3037),#1304,.T.);
#15394=ADVANCED_FACE('',(#3038,#1713),#14666,.T.);
#15395=ADVANCED_FACE('',(#3039),#1514,.F.);
#15396=ADVANCED_FACE('',(#3040,#1714),#14667,.T.);
#15397=ADVANCED_FACE('',(#3041),#1305,.F.);
#15398=ADVANCED_FACE('',(#3042),#1515,.F.);
#15399=ADVANCED_FACE('',(#3043),#1306,.F.);
#15400=ADVANCED_FACE('',(#3044),#1307,.F.);
#15401=ADVANCED_FACE('',(#3045),#1516,.T.);
#15402=ADVANCED_FACE('',(#3046,#1715),#14668,.F.);
#15403=ADVANCED_FACE('',(#3047),#1517,.F.);
#15404=ADVANCED_FACE('',(#3048,#1716),#14669,.T.);
#15405=ADVANCED_FACE('',(#3049),#1518,.F.);
#15406=ADVANCED_FACE('',(#3050,#1717),#14670,.T.);
#15407=ADVANCED_FACE('',(#3051),#1519,.T.);
#15408=ADVANCED_FACE('',(#3052),#1308,.T.);
#15409=ADVANCED_FACE('',(#3053),#14671,.T.);
#15410=ADVANCED_FACE('',(#3054),#14672,.T.);
#15411=ADVANCED_FACE('',(#3055),#1520,.T.);
#15412=ADVANCED_FACE('',(#3056),#1521,.T.);
#15413=ADVANCED_FACE('',(#3057),#1522,.T.);
#15414=ADVANCED_FACE('',(#3058),#1523,.T.);
#15415=ADVANCED_FACE('',(#3059),#1524,.T.);
#15416=ADVANCED_FACE('',(#3060),#1525,.T.);
#15417=ADVANCED_FACE('',(#3061),#1526,.T.);
#15418=ADVANCED_FACE('',(#3062),#1527,.T.);
#15419=ADVANCED_FACE('',(#3063),#14673,.F.);
#15420=ADVANCED_FACE('',(#3064),#254,.F.);
#15421=ADVANCED_FACE('',(#3065),#14674,.T.);
#15422=ADVANCED_FACE('',(#3066),#255,.F.);
#15423=ADVANCED_FACE('',(#3067),#1309,.F.);
#15424=ADVANCED_FACE('',(#3068),#14675,.F.);
#15425=ADVANCED_FACE('',(#3069),#14676,.F.);
#15426=ADVANCED_FACE('',(#3070),#14677,.F.);
#15427=ADVANCED_FACE('',(#3071),#1310,.F.);
#15428=ADVANCED_FACE('',(#3072),#14678,.F.);
#15429=ADVANCED_FACE('',(#3073),#14679,.F.);
#15430=ADVANCED_FACE('',(#3074),#14680,.F.);
#15431=ADVANCED_FACE('',(#3075,#1718),#14681,.F.);
#15432=ADVANCED_FACE('',(#3076),#14682,.T.);
#15433=ADVANCED_FACE('',(#3077),#1311,.T.);
#15434=ADVANCED_FACE('',(#3078),#14683,.T.);
#15435=ADVANCED_FACE('',(#3079),#1528,.T.);
#15436=ADVANCED_FACE('',(#3080,#1719),#14684,.T.);
#15437=ADVANCED_FACE('',(#3081),#1312,.T.);
#15438=ADVANCED_FACE('',(#3082),#1529,.T.);
#15439=ADVANCED_FACE('',(#3083),#1313,.T.);
#15440=ADVANCED_FACE('',(#3084,#1720),#14685,.T.);
#15441=ADVANCED_FACE('',(#3085),#1314,.F.);
#15442=ADVANCED_FACE('',(#3086,#1721),#14686,.T.);
#15443=ADVANCED_FACE('',(#3087),#1315,.T.);
#15444=ADVANCED_FACE('',(#3088),#1530,.T.);
#15445=ADVANCED_FACE('',(#3089),#1316,.T.);
#15446=ADVANCED_FACE('',(#3090,#1722),#14687,.T.);
#15447=ADVANCED_FACE('',(#3091),#1317,.F.);
#15448=ADVANCED_FACE('',(#3092),#1531,.F.);
#15449=ADVANCED_FACE('',(#3093),#1532,.F.);
#15450=ADVANCED_FACE('',(#3094,#1723),#14688,.T.);
#15451=ADVANCED_FACE('',(#3095),#1318,.T.);
#15452=ADVANCED_FACE('',(#3096),#1533,.T.);
#15453=ADVANCED_FACE('',(#3097,#1724),#14689,.T.);
#15454=ADVANCED_FACE('',(#3098),#1319,.T.);
#15455=ADVANCED_FACE('',(#3099),#1534,.T.);
#15456=ADVANCED_FACE('',(#3100),#1320,.T.);
#15457=ADVANCED_FACE('',(#3101),#14690,.T.);
#15458=ADVANCED_FACE('',(#3102),#14691,.T.);
#15459=ADVANCED_FACE('',(#3103),#1535,.T.);
#15460=ADVANCED_FACE('',(#3104),#1536,.F.);
#15461=ADVANCED_FACE('',(#3105,#1725),#14692,.F.);
#15462=ADVANCED_FACE('',(#3106),#1537,.T.);
#15463=ADVANCED_FACE('',(#3107,#1726),#14693,.F.);
#15464=ADVANCED_FACE('',(#3108),#1538,.F.);
#15465=ADVANCED_FACE('',(#3109,#1727),#14694,.T.);
#15466=ADVANCED_FACE('',(#3110,#1728),#14695,.T.);
#15467=ADVANCED_FACE('',(#3111),#1539,.F.);
#15468=ADVANCED_FACE('',(#3112),#1321,.F.);
#15469=ADVANCED_FACE('',(#3113,#1729),#14696,.T.);
#15470=ADVANCED_FACE('',(#3114),#1322,.F.);
#15471=ADVANCED_FACE('',(#3115),#1323,.F.);
#15472=ADVANCED_FACE('',(#3116,#1730),#14697,.T.);
#15473=ADVANCED_FACE('',(#3117),#1324,.T.);
#15474=ADVANCED_FACE('',(#3118),#1540,.T.);
#15475=ADVANCED_FACE('',(#3119),#1325,.T.);
#15476=ADVANCED_FACE('',(#3120,#1731),#14698,.T.);
#15477=ADVANCED_FACE('',(#3121),#1541,.T.);
#15478=ADVANCED_FACE('',(#3122,#1732),#14699,.T.);
#15479=ADVANCED_FACE('',(#3123),#1326,.F.);
#15480=ADVANCED_FACE('',(#3124),#1542,.F.);
#15481=ADVANCED_FACE('',(#3125),#1327,.F.);
#15482=ADVANCED_FACE('',(#3126,#1733),#14700,.T.);
#15483=ADVANCED_FACE('',(#3127),#1543,.T.);
#15484=ADVANCED_FACE('',(#3128,#1734),#14701,.T.);
#15485=ADVANCED_FACE('',(#3129),#1544,.F.);
#15486=ADVANCED_FACE('',(#3130,#1735),#14702,.T.);
#15487=ADVANCED_FACE('',(#3131),#1328,.T.);
#15488=ADVANCED_FACE('',(#3132),#1545,.T.);
#15489=ADVANCED_FACE('',(#3133),#1329,.T.);
#15490=ADVANCED_FACE('',(#3134,#1736),#14703,.T.);
#15491=ADVANCED_FACE('',(#3135),#1546,.F.);
#15492=ADVANCED_FACE('',(#3136,#1737),#14704,.T.);
#15493=ADVANCED_FACE('',(#3137),#1547,.T.);
#15494=ADVANCED_FACE('',(#3138,#1738),#14705,.T.);
#15495=ADVANCED_FACE('',(#3139),#1330,.F.);
#15496=ADVANCED_FACE('',(#3140,#1739),#14706,.T.);
#15497=ADVANCED_FACE('',(#3141),#1331,.T.);
#15498=ADVANCED_FACE('',(#3142),#1548,.T.);
#15499=ADVANCED_FACE('',(#3143),#1332,.T.);
#15500=ADVANCED_FACE('',(#3144,#1740),#14707,.T.);
#15501=ADVANCED_FACE('',(#3145),#1549,.F.);
#15502=ADVANCED_FACE('',(#3146,#1741),#14708,.T.);
#15503=ADVANCED_FACE('',(#3147),#1333,.F.);
#15504=ADVANCED_FACE('',(#3148),#1550,.F.);
#15505=ADVANCED_FACE('',(#3149),#1334,.F.);
#15506=ADVANCED_FACE('',(#3150),#1335,.F.);
#15507=ADVANCED_FACE('',(#3151),#1336,.F.);
#15508=ADVANCED_FACE('',(#3152),#1551,.F.);
#15509=ADVANCED_FACE('',(#3153,#1742,#1743),#14709,.F.);
#15510=ADVANCED_FACE('',(#3154),#1337,.F.);
#15511=ADVANCED_FACE('',(#3155,#1744,#1745),#14710,.T.);
#15512=ADVANCED_FACE('',(#3156),#1338,.F.);
#15513=ADVANCED_FACE('',(#3157),#1552,.F.);
#15514=ADVANCED_FACE('',(#3158),#1339,.F.);
#15515=ADVANCED_FACE('',(#3159),#14711,.F.);
#15516=ADVANCED_FACE('',(#3160),#14712,.F.);
#15517=ADVANCED_FACE('',(#3161),#1553,.F.);
#15518=ADVANCED_FACE('',(#3162),#1554,.T.);
#15519=ADVANCED_FACE('',(#3163),#1555,.F.);
#15520=ADVANCED_FACE('',(#3164),#1556,.T.);
#15521=ADVANCED_FACE('',(#3165),#1557,.F.);
#15522=ADVANCED_FACE('',(#3166),#1558,.T.);
#15523=ADVANCED_FACE('',(#3167),#1559,.T.);
#15524=ADVANCED_FACE('',(#3168),#1560,.T.);
#15525=ADVANCED_FACE('',(#3169),#1561,.T.);
#15526=ADVANCED_FACE('',(#3170),#1562,.T.);
#15527=ADVANCED_FACE('',(#3171),#1563,.T.);
#15528=ADVANCED_FACE('',(#3172),#1564,.T.);
#15529=ADVANCED_FACE('',(#3173),#1565,.T.);
#15530=ADVANCED_FACE('',(#3174),#1566,.T.);
#15531=ADVANCED_FACE('',(#3175),#1567,.T.);
#15532=ADVANCED_FACE('',(#3176),#1568,.T.);
#15533=ADVANCED_FACE('',(#3177),#1569,.T.);
#15534=ADVANCED_FACE('',(#3178),#1570,.T.);
#15535=ADVANCED_FACE('',(#3179),#1571,.T.);
#15536=ADVANCED_FACE('',(#3180),#1572,.T.);
#15537=ADVANCED_FACE('',(#3181),#1573,.T.);
#15538=ADVANCED_FACE('',(#3182),#1574,.T.);
#15539=ADVANCED_FACE('',(#3183),#1575,.T.);
#15540=ADVANCED_FACE('',(#3184),#1576,.T.);
#15541=ADVANCED_FACE('',(#3185),#1577,.T.);
#15542=ADVANCED_FACE('',(#3186),#1578,.T.);
#15543=ADVANCED_FACE('',(#3187),#1579,.T.);
#15544=ADVANCED_FACE('',(#3188),#14713,.F.);
#15545=ADVANCED_FACE('',(#3189),#256,.F.);
#15546=ADVANCED_FACE('',(#3190),#14714,.T.);
#15547=ADVANCED_FACE('',(#3191),#257,.F.);
#15548=ADVANCED_FACE('',(#3192),#157,.F.);
#15549=ADVANCED_FACE('',(#3193,#1746),#14715,.T.);
#15550=ADVANCED_FACE('',(#3194),#1340,.F.);
#15551=ADVANCED_FACE('',(#3195),#14716,.F.);
#15552=ADVANCED_FACE('',(#3196),#14717,.F.);
#15553=ADVANCED_FACE('',(#3197),#14718,.F.);
#15554=ADVANCED_FACE('',(#3198),#1341,.F.);
#15555=ADVANCED_FACE('',(#3199),#14719,.F.);
#15556=ADVANCED_FACE('',(#3200),#14720,.F.);
#15557=ADVANCED_FACE('',(#3201),#14721,.F.);
#15558=ADVANCED_FACE('',(#3202,#1747),#14722,.F.);
#15559=ADVANCED_FACE('',(#3203),#158,.T.);
#15560=ADVANCED_FACE('',(#3204),#1580,.T.);
#15561=ADVANCED_FACE('',(#3205,#1748),#14723,.T.);
#15562=ADVANCED_FACE('',(#3206),#14724,.T.);
#15563=ADVANCED_FACE('',(#3207),#1342,.T.);
#15564=ADVANCED_FACE('',(#3208),#1343,.T.);
#15565=ADVANCED_FACE('',(#3209),#1581,.T.);
#15566=ADVANCED_FACE('',(#3210),#1582,.T.);
#15567=ADVANCED_FACE('',(#3211),#1583,.T.);
#15568=ADVANCED_FACE('',(#3212),#1584,.T.);
#15569=ADVANCED_FACE('',(#3213),#1585,.T.);
#15570=ADVANCED_FACE('',(#3214),#1586,.T.);
#15571=ADVANCED_FACE('',(#3215),#1587,.T.);
#15572=ADVANCED_FACE('',(#3216),#1588,.T.);
#15573=ADVANCED_FACE('',(#3217),#1589,.T.);
#15574=ADVANCED_FACE('',(#3218),#1590,.T.);
#15575=ADVANCED_FACE('',(#3219),#1591,.T.);
#15576=ADVANCED_FACE('',(#3220),#1592,.T.);
#15577=ADVANCED_FACE('',(#3221),#1593,.T.);
#15578=ADVANCED_FACE('',(#3222),#1594,.T.);
#15579=ADVANCED_FACE('',(#3223),#1595,.T.);
#15580=ADVANCED_FACE('',(#3224),#1596,.T.);
#15581=ADVANCED_FACE('',(#3225),#1597,.T.);
#15582=ADVANCED_FACE('',(#3226),#14725,.F.);
#15583=ADVANCED_FACE('',(#3227),#258,.F.);
#15584=ADVANCED_FACE('',(#3228),#14726,.T.);
#15585=ADVANCED_FACE('',(#3229),#259,.F.);
#15586=ADVANCED_FACE('',(#3230),#159,.F.);
#15587=ADVANCED_FACE('',(#3231,#1749),#14727,.T.);
#15588=ADVANCED_FACE('',(#3232),#1344,.F.);
#15589=ADVANCED_FACE('',(#3233),#14728,.F.);
#15590=ADVANCED_FACE('',(#3234),#14729,.F.);
#15591=ADVANCED_FACE('',(#3235),#14730,.F.);
#15592=ADVANCED_FACE('',(#3236),#1345,.F.);
#15593=ADVANCED_FACE('',(#3237),#14731,.F.);
#15594=ADVANCED_FACE('',(#3238),#14732,.F.);
#15595=ADVANCED_FACE('',(#3239),#14733,.F.);
#15596=ADVANCED_FACE('',(#3240,#1750),#14734,.F.);
#15597=ADVANCED_FACE('',(#3241),#160,.T.);
#15598=ADVANCED_FACE('',(#3242),#1598,.T.);
#15599=ADVANCED_FACE('',(#3243,#1751),#14735,.T.);
#15600=ADVANCED_FACE('',(#3244),#14736,.T.);
#15601=ADVANCED_FACE('',(#3245),#1346,.T.);
#15602=ADVANCED_FACE('',(#3246),#1347,.T.);
#15603=ADVANCED_FACE('',(#3247),#1599,.F.);
#15604=ADVANCED_FACE('',(#3248,#1752),#14737,.T.);
#15605=ADVANCED_FACE('',(#3249),#1348,.T.);
#15606=ADVANCED_FACE('',(#3250),#1600,.T.);
#15607=ADVANCED_FACE('',(#3251,#1753),#14738,.T.);
#15608=ADVANCED_FACE('',(#3252),#1349,.T.);
#15609=ADVANCED_FACE('',(#3253),#1601,.T.);
#15610=ADVANCED_FACE('',(#3254),#1350,.T.);
#15611=ADVANCED_FACE('',(#3255),#14739,.T.);
#15612=ADVANCED_FACE('',(#3256),#14740,.T.);
#15613=CLOSED_SHELL('',(#14741,#14742,#14743,#14744,#14745,#14746,#14747,
#14748,#14749,#14750,#14751,#14752,#14753,#14754,#14755,#14756,#14757,#14758,
#14759,#14760,#14761,#14762,#14763,#14764,#14765,#14766,#14767,#14768,#14769,
#14770,#14771,#14772,#14773,#14774,#14775,#14776,#14777,#14778,#14779,#14780,
#14781,#14782,#14783,#14784,#14785,#14786,#14787,#14788,#14789,#14790,#14791,
#14792,#14793,#14794,#14795,#14796,#14797,#14798,#14799,#14800,#14801,#14802,
#14803,#14804,#14805,#14806,#14807,#14808,#14809,#14810,#14811,#14812,#14813,
#14814,#14815,#14816,#14817,#14818,#14819,#14820,#14821,#14822,#14823,#14824,
#14825,#14826,#14827,#14828,#14829,#14830,#14831,#14832,#14833,#14834,#14835,
#14836,#14837,#14838,#14839,#14840,#14841,#14842,#14843,#14844,#14845,#14846,
#14847,#14848,#14849,#14850,#14851,#14852,#14853,#14854,#14855,#14856,#14857,
#14858,#14859,#14860,#14861,#14862,#14863,#14864,#14865,#14866,#14867,#14868,
#14869,#14870,#14871,#14872,#14873,#14874,#14875,#14876,#14877,#14878,#14879,
#14880,#14881,#14882,#14883,#14884,#14885,#14886,#14887,#14888,#14889,#14890,
#14891,#14892,#14893,#14894,#14895,#14896,#14897,#14898,#14899,#14900,#14901,
#14902,#14903,#14904,#14905,#14906,#14907,#14908,#14909,#14910,#14911,#14912,
#14913,#14914,#14915,#14916,#14917,#14918,#14919,#14920,#14921,#14922,#14923,
#14924,#14925,#14926,#14927,#14928,#14929,#14930,#14931,#14932,#14933,#14934,
#14935,#14936,#14937,#14938,#14939,#14940,#14941,#14942,#14943,#14944,#14945,
#14946,#14947,#14948,#14949,#14950,#14951,#14952,#14953,#14954,#14955,#14956,
#14957,#14958,#14959,#14960,#14961,#14962,#14963,#14964,#14965,#14966,#14967,
#14968,#14969,#14970,#14971,#14972));
#15614=CLOSED_SHELL('',(#14973,#14974,#14975,#14976,#14977,#14978,#14979,
#14980,#14981,#14982,#14983,#14984,#14985,#14986,#14987,#14988,#14989,#14990,
#14991,#14992,#14993,#14994,#14995,#14996,#14997,#14998,#14999,#15000,#15001,
#15002,#15003,#15004,#15005,#15006,#15007,#15008,#15009,#15010,#15011,#15012,
#15013,#15014,#15015,#15016,#15017));
#15615=CLOSED_SHELL('',(#15018,#15019,#15020,#15021,#15022,#15023,#15024,
#15025,#15026,#15027,#15028,#15029,#15030,#15031,#15032,#15033,#15034,#15035,
#15036,#15037,#15038,#15039,#15040,#15041,#15042,#15043,#15044,#15045,#15046,
#15047,#15048,#15049,#15050,#15051,#15052,#15053,#15054,#15055,#15056,#15057,
#15058,#15059,#15060,#15061,#15062,#15063,#15064,#15065,#15066,#15067,#15068,
#15069,#15070,#15071,#15072,#15073,#15074,#15075,#15076,#15077,#15078,#15079,
#15080,#15081,#15082,#15083,#15084,#15085,#15086));
#15616=CLOSED_SHELL('',(#15087,#15088,#15089,#15090,#15091,#15092,#15093,
#15094,#15095,#15096,#15097,#15098,#15099,#15100,#15101,#15102,#15103,#15104,
#15105,#15106,#15107,#15108,#15109,#15110,#15111,#15112,#15113,#15114,#15115,
#15116,#15117,#15118,#15119,#15120,#15121,#15122,#15123));
#15617=CLOSED_SHELL('',(#15124,#15125,#15126,#15127,#15128,#15129,#15130,
#15131,#15132,#15133,#15134,#15135,#15136,#15137,#15138,#15139,#15140,#15141,
#15142,#15143,#15144,#15145,#15146,#15147,#15148,#15149,#15150,#15151,#15152,
#15153,#15154,#15155,#15156,#15157,#15158,#15159,#15160,#15161,#15162,#15163,
#15164,#15165,#15166,#15167,#15168,#15169,#15170,#15171,#15172,#15173,#15174,
#15175,#15176,#15177,#15178,#15179,#15180,#15181,#15182,#15183,#15184,#15185,
#15186,#15187,#15188,#15189,#15190,#15191,#15192,#15193,#15194,#15195,#15196,
#15197,#15198,#15199,#15200,#15201,#15202,#15203,#15204,#15205,#15206,#15207,
#15208,#15209,#15210,#15211,#15212,#15213,#15214,#15215,#15216,#15217,#15218,
#15219,#15220,#15221,#15222,#15223,#15224,#15225,#15226,#15227,#15228,#15229,
#15230,#15231,#15232,#15233,#15234,#15235,#15236,#15237,#15238,#15239,#15240,
#15241,#15242,#15243,#15244,#15245,#15246,#15247,#15248,#15249,#15250,#15251,
#15252,#15253,#15254,#15255,#15256,#15257,#15258,#15259,#15260,#15261,#15262,
#15263,#15264,#15265,#15266,#15267,#15268,#15269,#15270,#15271,#15272,#15273,
#15274,#15275,#15276,#15277,#15278,#15279,#15280,#15281,#15282,#15283,#15284,
#15285,#15286,#15287,#15288,#15289,#15290,#15291,#15292,#15293,#15294,#15295,
#15296,#15297,#15298,#15299,#15300,#15301,#15302,#15303,#15304,#15305,#15306,
#15307,#15308,#15309,#15310,#15311,#15312,#15313,#15314,#15315,#15316,#15317,
#15318,#15319,#15320,#15321,#15322,#15323,#15324,#15325,#15326,#15327,#15328,
#15329,#15330,#15331,#15332,#15333,#15334,#15335,#15336,#15337,#15338,#15339,
#15340,#15341,#15342,#15343,#15344,#15345,#15346,#15347,#15348,#15349,#15350,
#15351,#15352,#15353,#15354,#15355,#15356,#15357,#15358,#15359,#15360,#15361,
#15362,#15363,#15364,#15365,#15366,#15367,#15368));
#15618=CLOSED_SHELL('',(#15369,#15370,#15371,#15372,#15373,#15374,#15375,
#15376,#15377,#15378,#15379,#15380,#15381,#15382,#15383,#15384,#15385,#15386,
#15387,#15388,#15389));
#15619=CLOSED_SHELL('',(#15390,#15391,#15392,#15393,#15394,#15395,#15396,
#15397,#15398,#15399,#15400));
#15620=CLOSED_SHELL('',(#15401,#15402,#15403,#15404,#15405,#15406,#15407,
#15408,#15409,#15410));
#15621=CLOSED_SHELL('',(#15411,#15412,#15413,#15414,#15415,#15416,#15417,
#15418,#15419,#15420,#15421,#15422,#15423,#15424,#15425,#15426,#15427,#15428,
#15429,#15430,#15431,#15432,#15433,#15434,#15435,#15436,#15437,#15438,#15439,
#15440));
#15622=CLOSED_SHELL('',(#15441,#15442,#15443,#15444,#15445,#15446,#15447,
#15448));
#15623=CLOSED_SHELL('',(#15449,#15450,#15451,#15452,#15453,#15454,#15455,
#15456,#15457,#15458));
#15624=CLOSED_SHELL('',(#15459,#15460,#15461,#15462,#15463,#15464,#15465,
#15466,#15467,#15468,#15469,#15470,#15471,#15472,#15473,#15474,#15475,#15476,
#15477,#15478,#15479));
#15625=CLOSED_SHELL('',(#15480,#15481,#15482,#15483,#15484,#15485,#15486,
#15487,#15488,#15489,#15490,#15491,#15492,#15493,#15494,#15495));
#15626=CLOSED_SHELL('',(#15496,#15497,#15498,#15499,#15500,#15501,#15502,
#15503,#15504,#15505,#15506));
#15627=CLOSED_SHELL('',(#15507,#15508,#15509,#15510,#15511,#15512,#15513,
#15514,#15515,#15516,#15517,#15518,#15519,#15520,#15521,#15522));
#15628=CLOSED_SHELL('',(#15523,#15524,#15525,#15526,#15527,#15528,#15529,
#15530,#15531,#15532,#15533,#15534,#15535,#15536,#15537,#15538,#15539,#15540,
#15541,#15542,#15543,#15544,#15545,#15546,#15547,#15548,#15549,#15550,#15551,
#15552,#15553,#15554,#15555,#15556,#15557,#15558,#15559,#15560,#15561,#15562,
#15563,#15564));
#15629=CLOSED_SHELL('',(#15565,#15566,#15567,#15568,#15569,#15570,#15571,
#15572,#15573,#15574,#15575,#15576,#15577,#15578,#15579,#15580,#15581,#15582,
#15583,#15584,#15585,#15586,#15587,#15588,#15589,#15590,#15591,#15592,#15593,
#15594,#15595,#15596,#15597,#15598,#15599,#15600,#15601,#15602));
#15630=CLOSED_SHELL('',(#15603,#15604,#15605,#15606,#15607,#15608,#15609,
#15610,#15611,#15612));
#15631=DERIVED_UNIT_ELEMENT(#15667,1.);
#15632=DERIVED_UNIT_ELEMENT(#86431,-3.);
#15633=DERIVED_UNIT_ELEMENT(#15667,1.);
#15634=DERIVED_UNIT_ELEMENT(#86431,-3.);
#15635=DERIVED_UNIT_ELEMENT(#15667,1.);
#15636=DERIVED_UNIT_ELEMENT(#86431,-3.);
#15637=DERIVED_UNIT_ELEMENT(#15667,1.);
#15638=DERIVED_UNIT_ELEMENT(#86431,-3.);
#15639=DERIVED_UNIT_ELEMENT(#15667,1.);
#15640=DERIVED_UNIT_ELEMENT(#86431,-3.);
#15641=DERIVED_UNIT_ELEMENT(#15667,1.);
#15642=DERIVED_UNIT_ELEMENT(#86431,-3.);
#15643=DERIVED_UNIT_ELEMENT(#15667,1.);
#15644=DERIVED_UNIT_ELEMENT(#86431,-3.);
#15645=DERIVED_UNIT_ELEMENT(#15667,1.);
#15646=DERIVED_UNIT_ELEMENT(#86431,-3.);
#15647=DERIVED_UNIT_ELEMENT(#15667,1.);
#15648=DERIVED_UNIT_ELEMENT(#86431,-3.);
#15649=DERIVED_UNIT_ELEMENT(#15667,1.);
#15650=DERIVED_UNIT_ELEMENT(#86431,-3.);
#15651=DERIVED_UNIT_ELEMENT(#15667,1.);
#15652=DERIVED_UNIT_ELEMENT(#86431,-3.);
#15653=DERIVED_UNIT_ELEMENT(#15667,1.);
#15654=DERIVED_UNIT_ELEMENT(#86431,-3.);
#15655=DERIVED_UNIT_ELEMENT(#15667,1.);
#15656=DERIVED_UNIT_ELEMENT(#86431,-3.);
#15657=DERIVED_UNIT_ELEMENT(#15667,1.);
#15658=DERIVED_UNIT_ELEMENT(#86431,-3.);
#15659=DERIVED_UNIT_ELEMENT(#15667,1.);
#15660=DERIVED_UNIT_ELEMENT(#86431,-3.);
#15661=DERIVED_UNIT_ELEMENT(#15667,1.);
#15662=DERIVED_UNIT_ELEMENT(#86431,-3.);
#15663=DERIVED_UNIT_ELEMENT(#15667,1.);
#15664=DERIVED_UNIT_ELEMENT(#86431,-3.);
#15665=DERIVED_UNIT_ELEMENT(#15667,1.);
#15666=DERIVED_UNIT_ELEMENT(#86431,-3.);
#15667=(
MASS_UNIT()
NAMED_UNIT(*)
SI_UNIT(.KILO.,.GRAM.)
);
#15668=DERIVED_UNIT((#15631,#15632));
#15669=DERIVED_UNIT((#15633,#15634));
#15670=DERIVED_UNIT((#15635,#15636));
#15671=DERIVED_UNIT((#15637,#15638));
#15672=DERIVED_UNIT((#15639,#15640));
#15673=DERIVED_UNIT((#15641,#15642));
#15674=DERIVED_UNIT((#15643,#15644));
#15675=DERIVED_UNIT((#15645,#15646));
#15676=DERIVED_UNIT((#15647,#15648));
#15677=DERIVED_UNIT((#15649,#15650));
#15678=DERIVED_UNIT((#15651,#15652));
#15679=DERIVED_UNIT((#15653,#15654));
#15680=DERIVED_UNIT((#15655,#15656));
#15681=DERIVED_UNIT((#15657,#15658));
#15682=DERIVED_UNIT((#15659,#15660));
#15683=DERIVED_UNIT((#15661,#15662));
#15684=DERIVED_UNIT((#15663,#15664));
#15685=DERIVED_UNIT((#15665,#15666));
#15686=MEASURE_REPRESENTATION_ITEM('density measure',
POSITIVE_RATIO_MEASURE(2670.),#15668);
#15687=MEASURE_REPRESENTATION_ITEM('density measure',
POSITIVE_RATIO_MEASURE(2670.),#15669);
#15688=MEASURE_REPRESENTATION_ITEM('density measure',
POSITIVE_RATIO_MEASURE(2670.),#15670);
#15689=MEASURE_REPRESENTATION_ITEM('density measure',
POSITIVE_RATIO_MEASURE(7850.),#15671);
#15690=MEASURE_REPRESENTATION_ITEM('density measure',
POSITIVE_RATIO_MEASURE(8870.),#15672);
#15691=MEASURE_REPRESENTATION_ITEM('density measure',
POSITIVE_RATIO_MEASURE(7395.3),#15673);
#15692=MEASURE_REPRESENTATION_ITEM('density measure',
POSITIVE_RATIO_MEASURE(1250.),#15674);
#15693=MEASURE_REPRESENTATION_ITEM('density measure',
POSITIVE_RATIO_MEASURE(7850.),#15675);
#15694=MEASURE_REPRESENTATION_ITEM('density measure',
POSITIVE_RATIO_MEASURE(7850.),#15676);
#15695=MEASURE_REPRESENTATION_ITEM('density measure',
POSITIVE_RATIO_MEASURE(8940.),#15677);
#15696=MEASURE_REPRESENTATION_ITEM('density measure',
POSITIVE_RATIO_MEASURE(894.),#15678);
#15697=MEASURE_REPRESENTATION_ITEM('density measure',
POSITIVE_RATIO_MEASURE(7810.),#15679);
#15698=MEASURE_REPRESENTATION_ITEM('density measure',
POSITIVE_RATIO_MEASURE(7810.),#15680);
#15699=MEASURE_REPRESENTATION_ITEM('density measure',
POSITIVE_RATIO_MEASURE(1250.),#15681);
#15700=MEASURE_REPRESENTATION_ITEM('density measure',
POSITIVE_RATIO_MEASURE(7850.),#15682);
#15701=MEASURE_REPRESENTATION_ITEM('density measure',
POSITIVE_RATIO_MEASURE(7850.),#15683);
#15702=MEASURE_REPRESENTATION_ITEM('density measure',
POSITIVE_RATIO_MEASURE(7850.),#15684);
#15703=MEASURE_REPRESENTATION_ITEM('density measure',
POSITIVE_RATIO_MEASURE(894.),#15685);
#15704=PROPERTY_DEFINITION_REPRESENTATION(#15794,#15740);
#15705=PROPERTY_DEFINITION_REPRESENTATION(#15795,#15741);
#15706=PROPERTY_DEFINITION_REPRESENTATION(#15796,#15742);
#15707=PROPERTY_DEFINITION_REPRESENTATION(#15797,#15743);
#15708=PROPERTY_DEFINITION_REPRESENTATION(#15798,#15744);
#15709=PROPERTY_DEFINITION_REPRESENTATION(#15799,#15745);
#15710=PROPERTY_DEFINITION_REPRESENTATION(#15800,#15746);
#15711=PROPERTY_DEFINITION_REPRESENTATION(#15801,#15747);
#15712=PROPERTY_DEFINITION_REPRESENTATION(#15802,#15748);
#15713=PROPERTY_DEFINITION_REPRESENTATION(#15803,#15749);
#15714=PROPERTY_DEFINITION_REPRESENTATION(#15804,#15750);
#15715=PROPERTY_DEFINITION_REPRESENTATION(#15805,#15751);
#15716=PROPERTY_DEFINITION_REPRESENTATION(#15806,#15752);
#15717=PROPERTY_DEFINITION_REPRESENTATION(#15807,#15753);
#15718=PROPERTY_DEFINITION_REPRESENTATION(#15808,#15754);
#15719=PROPERTY_DEFINITION_REPRESENTATION(#15809,#15755);
#15720=PROPERTY_DEFINITION_REPRESENTATION(#15810,#15756);
#15721=PROPERTY_DEFINITION_REPRESENTATION(#15811,#15757);
#15722=PROPERTY_DEFINITION_REPRESENTATION(#15812,#15758);
#15723=PROPERTY_DEFINITION_REPRESENTATION(#15813,#15759);
#15724=PROPERTY_DEFINITION_REPRESENTATION(#15814,#15760);
#15725=PROPERTY_DEFINITION_REPRESENTATION(#15815,#15761);
#15726=PROPERTY_DEFINITION_REPRESENTATION(#15816,#15762);
#15727=PROPERTY_DEFINITION_REPRESENTATION(#15817,#15763);
#15728=PROPERTY_DEFINITION_REPRESENTATION(#15818,#15764);
#15729=PROPERTY_DEFINITION_REPRESENTATION(#15819,#15765);
#15730=PROPERTY_DEFINITION_REPRESENTATION(#15820,#15766);
#15731=PROPERTY_DEFINITION_REPRESENTATION(#15821,#15767);
#15732=PROPERTY_DEFINITION_REPRESENTATION(#15822,#15768);
#15733=PROPERTY_DEFINITION_REPRESENTATION(#15823,#15769);
#15734=PROPERTY_DEFINITION_REPRESENTATION(#15824,#15770);
#15735=PROPERTY_DEFINITION_REPRESENTATION(#15825,#15771);
#15736=PROPERTY_DEFINITION_REPRESENTATION(#15826,#15772);
#15737=PROPERTY_DEFINITION_REPRESENTATION(#15827,#15773);
#15738=PROPERTY_DEFINITION_REPRESENTATION(#15828,#15774);
#15739=PROPERTY_DEFINITION_REPRESENTATION(#15829,#15775);
#15740=REPRESENTATION('material name',(#15776),#86411);
#15741=REPRESENTATION('density',(#15686),#86411);
#15742=REPRESENTATION('material name',(#15777),#86412);
#15743=REPRESENTATION('density',(#15687),#86412);
#15744=REPRESENTATION('material name',(#15778),#86413);
#15745=REPRESENTATION('density',(#15688),#86413);
#15746=REPRESENTATION('material name',(#15779),#86414);
#15747=REPRESENTATION('density',(#15689),#86414);
#15748=REPRESENTATION('material name',(#15780),#86415);
#15749=REPRESENTATION('density',(#15690),#86415);
#15750=REPRESENTATION('material name',(#15781),#86416);
#15751=REPRESENTATION('density',(#15691),#86416);
#15752=REPRESENTATION('material name',(#15782),#86417);
#15753=REPRESENTATION('density',(#15692),#86417);
#15754=REPRESENTATION('material name',(#15783),#86418);
#15755=REPRESENTATION('density',(#15693),#86418);
#15756=REPRESENTATION('material name',(#15784),#86419);
#15757=REPRESENTATION('density',(#15694),#86419);
#15758=REPRESENTATION('material name',(#15785),#86420);
#15759=REPRESENTATION('density',(#15695),#86420);
#15760=REPRESENTATION('material name',(#15786),#86421);
#15761=REPRESENTATION('density',(#15696),#86421);
#15762=REPRESENTATION('material name',(#15787),#86422);
#15763=REPRESENTATION('density',(#15697),#86422);
#15764=REPRESENTATION('material name',(#15788),#86423);
#15765=REPRESENTATION('density',(#15698),#86423);
#15766=REPRESENTATION('material name',(#15789),#86424);
#15767=REPRESENTATION('density',(#15699),#86424);
#15768=REPRESENTATION('material name',(#15790),#86425);
#15769=REPRESENTATION('density',(#15700),#86425);
#15770=REPRESENTATION('material name',(#15791),#86426);
#15771=REPRESENTATION('density',(#15701),#86426);
#15772=REPRESENTATION('material name',(#15792),#86427);
#15773=REPRESENTATION('density',(#15702),#86427);
#15774=REPRESENTATION('material name',(#15793),#86428);
#15775=REPRESENTATION('density',(#15703),#86428);
#15776=DESCRIPTIVE_REPRESENTATION_ITEM('Aluminum A356 T6',
'Aluminum A356 T6');
#15777=DESCRIPTIVE_REPRESENTATION_ITEM('Aluminum A356 T6',
'Aluminum A356 T6');
#15778=DESCRIPTIVE_REPRESENTATION_ITEM('Aluminum A356 T6',
'Aluminum A356 T6');
#15779=DESCRIPTIVE_REPRESENTATION_ITEM('Steel AISI 4340 350A QT',
'Steel AISI 4340 350A QT');
#15780=DESCRIPTIVE_REPRESENTATION_ITEM('Bronze, Cast','Bronze, Cast');
#15781=DESCRIPTIVE_REPRESENTATION_ITEM(
'Iron, Gray Cast ASTM A48 Grade 30','Iron, Gray Cast ASTM A48 Grade 30');
#15782=DESCRIPTIVE_REPRESENTATION_ITEM('Rubber, Silicone',
'Rubber, Silicone');
#15783=DESCRIPTIVE_REPRESENTATION_ITEM('Steel, Mild','Steel, Mild');
#15784=DESCRIPTIVE_REPRESENTATION_ITEM('Steel, Galvanized',
'Steel, Galvanized');
#15785=DESCRIPTIVE_REPRESENTATION_ITEM('Copper','Copper');
#15786=DESCRIPTIVE_REPRESENTATION_ITEM('Polyethylene, Low Density',
'Polyethylene, Low Density');
#15787=DESCRIPTIVE_REPRESENTATION_ITEM('Steel AISI 5210 517 H',
'Steel AISI 5210 517 H');
#15788=DESCRIPTIVE_REPRESENTATION_ITEM('Steel AISI 5210 517 H',
'Steel AISI 5210 517 H');
#15789=DESCRIPTIVE_REPRESENTATION_ITEM('Rubber, Silicone',
'Rubber, Silicone');
#15790=DESCRIPTIVE_REPRESENTATION_ITEM('Steel AISI 1060',
'Steel AISI 1060');
#15791=DESCRIPTIVE_REPRESENTATION_ITEM('Steel, Galvanized',
'Steel, Galvanized');
#15792=DESCRIPTIVE_REPRESENTATION_ITEM('Steel, Galvanized',
'Steel, Galvanized');
#15793=DESCRIPTIVE_REPRESENTATION_ITEM('Polyethylene, Low Density',
'Polyethylene, Low Density');
#15794=PROPERTY_DEFINITION('material property','material name',#86522);
#15795=PROPERTY_DEFINITION('material property','density of part',#86522);
#15796=PROPERTY_DEFINITION('material property','material name',#86523);
#15797=PROPERTY_DEFINITION('material property','density of part',#86523);
#15798=PROPERTY_DEFINITION('material property','material name',#86524);
#15799=PROPERTY_DEFINITION('material property','density of part',#86524);
#15800=PROPERTY_DEFINITION('material property','material name',#86525);
#15801=PROPERTY_DEFINITION('material property','density of part',#86525);
#15802=PROPERTY_DEFINITION('material property','material name',#86526);
#15803=PROPERTY_DEFINITION('material property','density of part',#86526);
#15804=PROPERTY_DEFINITION('material property','material name',#86527);
#15805=PROPERTY_DEFINITION('material property','density of part',#86527);
#15806=PROPERTY_DEFINITION('material property','material name',#86528);
#15807=PROPERTY_DEFINITION('material property','density of part',#86528);
#15808=PROPERTY_DEFINITION('material property','material name',#86529);
#15809=PROPERTY_DEFINITION('material property','density of part',#86529);
#15810=PROPERTY_DEFINITION('material property','material name',#86530);
#15811=PROPERTY_DEFINITION('material property','density of part',#86530);
#15812=PROPERTY_DEFINITION('material property','material name',#86531);
#15813=PROPERTY_DEFINITION('material property','density of part',#86531);
#15814=PROPERTY_DEFINITION('material property','material name',#86532);
#15815=PROPERTY_DEFINITION('material property','density of part',#86532);
#15816=PROPERTY_DEFINITION('material property','material name',#86533);
#15817=PROPERTY_DEFINITION('material property','density of part',#86533);
#15818=PROPERTY_DEFINITION('material property','material name',#86534);
#15819=PROPERTY_DEFINITION('material property','density of part',#86534);
#15820=PROPERTY_DEFINITION('material property','material name',#86535);
#15821=PROPERTY_DEFINITION('material property','density of part',#86535);
#15822=PROPERTY_DEFINITION('material property','material name',#86536);
#15823=PROPERTY_DEFINITION('material property','density of part',#86536);
#15824=PROPERTY_DEFINITION('material property','material name',#86537);
#15825=PROPERTY_DEFINITION('material property','density of part',#86537);
#15826=PROPERTY_DEFINITION('material property','material name',#86538);
#15827=PROPERTY_DEFINITION('material property','density of part',#86538);
#15828=PROPERTY_DEFINITION('material property','material name',#86539);
#15829=PROPERTY_DEFINITION('material property','density of part',#86539);
#15830=AXIS2_PLACEMENT_3D('',#21058,#17286,#17287);
#15831=AXIS2_PLACEMENT_3D('',#21059,#17288,#17289);
#15832=AXIS2_PLACEMENT_3D('',#21060,#17290,#17291);
#15833=AXIS2_PLACEMENT_3D('',#21069,#17296,#17297);
#15834=AXIS2_PLACEMENT_3D('',#21075,#17301,#17302);
#15835=AXIS2_PLACEMENT_3D('',#21081,#17306,#17307);
#15836=AXIS2_PLACEMENT_3D('',#21084,#17310,#17311);
#15837=AXIS2_PLACEMENT_3D('',#21085,#17312,#17313);
#15838=AXIS2_PLACEMENT_3D('',#21094,#17318,#17319);
#15839=AXIS2_PLACEMENT_3D('',#21104,#17325,#17326);
#15840=AXIS2_PLACEMENT_3D('',#21108,#17329,#17330);
#15841=AXIS2_PLACEMENT_3D('',#21112,#17333,#17334);
#15842=AXIS2_PLACEMENT_3D('',#21116,#17337,#17338);
#15843=AXIS2_PLACEMENT_3D('',#21125,#17343,#17344);
#15844=AXIS2_PLACEMENT_3D('',#21131,#17348,#17349);
#15845=AXIS2_PLACEMENT_3D('',#21137,#17353,#17354);
#15846=AXIS2_PLACEMENT_3D('',#21140,#17357,#17358);
#15847=AXIS2_PLACEMENT_3D('',#21141,#17359,#17360);
#15848=AXIS2_PLACEMENT_3D('',#21150,#17365,#17366);
#15849=AXIS2_PLACEMENT_3D('',#21156,#17370,#17371);
#15850=AXIS2_PLACEMENT_3D('',#21162,#17375,#17376);
#15851=AXIS2_PLACEMENT_3D('',#21165,#17379,#17380);
#15852=AXIS2_PLACEMENT_3D('',#21166,#17381,#17382);
#15853=AXIS2_PLACEMENT_3D('',#21175,#17387,#17388);
#15854=AXIS2_PLACEMENT_3D('',#21181,#17392,#17393);
#15855=AXIS2_PLACEMENT_3D('',#21187,#17397,#17398);
#15856=AXIS2_PLACEMENT_3D('',#21190,#17401,#17402);
#15857=AXIS2_PLACEMENT_3D('',#21191,#17403,#17404);
#15858=AXIS2_PLACEMENT_3D('',#21200,#17409,#17410);
#15859=AXIS2_PLACEMENT_3D('',#21209,#17415,#17416);
#15860=AXIS2_PLACEMENT_3D('',#21215,#17420,#17421);
#15861=AXIS2_PLACEMENT_3D('',#21218,#17424,#17425);
#15862=AXIS2_PLACEMENT_3D('',#21222,#17428,#17429);
#15863=AXIS2_PLACEMENT_3D('',#21230,#17434,#17435);
#15864=AXIS2_PLACEMENT_3D('',#21236,#17439,#17440);
#15865=AXIS2_PLACEMENT_3D('',#21256,#17451,#17452);
#15866=AXIS2_PLACEMENT_3D('',#21257,#17453,#17454);
#15867=AXIS2_PLACEMENT_3D('',#21266,#17459,#17460);
#15868=AXIS2_PLACEMENT_3D('',#21272,#17464,#17465);
#15869=AXIS2_PLACEMENT_3D('',#21278,#17469,#17470);
#15870=AXIS2_PLACEMENT_3D('',#21281,#17473,#17474);
#15871=AXIS2_PLACEMENT_3D('',#21282,#17475,#17476);
#15872=AXIS2_PLACEMENT_3D('',#21291,#17481,#17482);
#15873=AXIS2_PLACEMENT_3D('',#21300,#17487,#17488);
#15874=AXIS2_PLACEMENT_3D('',#21303,#17491,#17492);
#15875=AXIS2_PLACEMENT_3D('',#21309,#17496,#17497);
#15876=AXIS2_PLACEMENT_3D('',#21313,#17500,#17501);
#15877=AXIS2_PLACEMENT_3D('',#21322,#17506,#17507);
#15878=AXIS2_PLACEMENT_3D('',#21328,#17511,#17512);
#15879=AXIS2_PLACEMENT_3D('',#21334,#17516,#17517);
#15880=AXIS2_PLACEMENT_3D('',#21337,#17520,#17521);
#15881=AXIS2_PLACEMENT_3D('',#21338,#17522,#17523);
#15882=AXIS2_PLACEMENT_3D('',#21347,#17528,#17529);
#15883=AXIS2_PLACEMENT_3D('',#21353,#17533,#17534);
#15884=AXIS2_PLACEMENT_3D('',#21359,#17538,#17539);
#15885=AXIS2_PLACEMENT_3D('',#21362,#17542,#17543);
#15886=AXIS2_PLACEMENT_3D('',#21363,#17544,#17545);
#15887=AXIS2_PLACEMENT_3D('',#21372,#17550,#17551);
#15888=AXIS2_PLACEMENT_3D('',#21378,#17555,#17556);
#15889=AXIS2_PLACEMENT_3D('',#21384,#17560,#17561);
#15890=AXIS2_PLACEMENT_3D('',#21387,#17564,#17565);
#15891=AXIS2_PLACEMENT_3D('',#21388,#17566,#17567);
#15892=AXIS2_PLACEMENT_3D('',#21397,#17572,#17573);
#15893=AXIS2_PLACEMENT_3D('',#21403,#17577,#17578);
#15894=AXIS2_PLACEMENT_3D('',#21412,#17583,#17584);
#15895=AXIS2_PLACEMENT_3D('',#21415,#17587,#17588);
#15896=AXIS2_PLACEMENT_3D('',#21419,#17591,#17592);
#15897=AXIS2_PLACEMENT_3D('',#21427,#17597,#17598);
#15898=AXIS2_PLACEMENT_3D('',#21435,#17603,#17604);
#15899=AXIS2_PLACEMENT_3D('',#21443,#17608,#17609);
#15900=AXIS2_PLACEMENT_3D('',#21445,#17610,#17611);
#15901=AXIS2_PLACEMENT_3D('',#21449,#17613,#17614);
#15902=AXIS2_PLACEMENT_3D('',#21451,#17615,#17616);
#15903=AXIS2_PLACEMENT_3D('',#21467,#17625,#17626);
#15904=AXIS2_PLACEMENT_3D('',#21469,#17627,#17628);
#15905=AXIS2_PLACEMENT_3D('',#21471,#17629,#17630);
#15906=AXIS2_PLACEMENT_3D('',#21472,#17631,#17632);
#15907=AXIS2_PLACEMENT_3D('',#21475,#17633,#17634);
#15908=AXIS2_PLACEMENT_3D('',#21479,#17636,#17637);
#15909=AXIS2_PLACEMENT_3D('',#21481,#17639,#17640);
#15910=AXIS2_PLACEMENT_3D('',#21483,#17641,#17642);
#15911=AXIS2_PLACEMENT_3D('',#21486,#17644,#17645);
#15912=AXIS2_PLACEMENT_3D('',#21487,#17646,#17647);
#15913=AXIS2_PLACEMENT_3D('',#21493,#17651,#17652);
#15914=AXIS2_PLACEMENT_3D('',#21499,#17656,#17657);
#15915=AXIS2_PLACEMENT_3D('',#21505,#17661,#17662);
#15916=AXIS2_PLACEMENT_3D('',#21506,#17663,#17664);
#15917=AXIS2_PLACEMENT_3D('',#21507,#17665,#17666);
#15918=AXIS2_PLACEMENT_3D('',#21508,#17667,#17668);
#15919=AXIS2_PLACEMENT_3D('',#21509,#17669,#17670);
#15920=AXIS2_PLACEMENT_3D('',#21518,#17675,#17676);
#15921=AXIS2_PLACEMENT_3D('',#21524,#17680,#17681);
#15922=AXIS2_PLACEMENT_3D('',#21530,#17685,#17686);
#15923=AXIS2_PLACEMENT_3D('',#21532,#17687,#17688);
#15924=AXIS2_PLACEMENT_3D('',#21534,#17689,#17690);
#15925=AXIS2_PLACEMENT_3D('',#21535,#17691,#17692);
#15926=AXIS2_PLACEMENT_3D('',#21536,#17693,#17694);
#15927=AXIS2_PLACEMENT_3D('',#21538,#17695,#17696);
#15928=AXIS2_PLACEMENT_3D('',#21540,#17697,#17698);
#15929=AXIS2_PLACEMENT_3D('',#21542,#17699,#17700);
#15930=AXIS2_PLACEMENT_3D('',#21545,#17702,#17703);
#15931=AXIS2_PLACEMENT_3D('',#21548,#17705,#17706);
#15932=AXIS2_PLACEMENT_3D('',#21554,#17709,#17710);
#15933=AXIS2_PLACEMENT_3D('',#21556,#17711,#17712);
#15934=AXIS2_PLACEMENT_3D('',#21557,#17713,#17714);
#15935=AXIS2_PLACEMENT_3D('',#21558,#17715,#17716);
#15936=AXIS2_PLACEMENT_3D('',#21561,#17717,#17718);
#15937=AXIS2_PLACEMENT_3D('',#21568,#17719,#17720);
#15938=AXIS2_PLACEMENT_3D('',#21573,#17721,#17722);
#15939=AXIS2_PLACEMENT_3D('',#21575,#17723,#17724);
#15940=AXIS2_PLACEMENT_3D('',#21577,#17725,#17726);
#15941=AXIS2_PLACEMENT_3D('',#21578,#17727,#17728);
#15942=AXIS2_PLACEMENT_3D('',#21579,#17729,#17730);
#15943=AXIS2_PLACEMENT_3D('',#21583,#17732,#17733);
#15944=AXIS2_PLACEMENT_3D('',#21585,#17735,#17736);
#15945=AXIS2_PLACEMENT_3D('',#21587,#17737,#17738);
#15946=AXIS2_PLACEMENT_3D('',#21593,#17739,#17740);
#15947=AXIS2_PLACEMENT_3D('',#21594,#17741,#17742);
#15948=AXIS2_PLACEMENT_3D('',#21596,#17743,#17744);
#15949=AXIS2_PLACEMENT_3D('',#21602,#17745,#17746);
#15950=AXIS2_PLACEMENT_3D('',#21603,#17747,#17748);
#15951=AXIS2_PLACEMENT_3D('',#21605,#17749,#17750);
#15952=AXIS2_PLACEMENT_3D('',#21607,#17751,#17752);
#15953=AXIS2_PLACEMENT_3D('',#21608,#17753,#17754);
#15954=AXIS2_PLACEMENT_3D('',#21609,#17755,#17756);
#15955=AXIS2_PLACEMENT_3D('',#21613,#17758,#17759);
#15956=AXIS2_PLACEMENT_3D('',#21615,#17761,#17762);
#15957=AXIS2_PLACEMENT_3D('',#21617,#17763,#17764);
#15958=AXIS2_PLACEMENT_3D('',#21619,#17765,#17766);
#15959=AXIS2_PLACEMENT_3D('',#21624,#17767,#17768);
#15960=AXIS2_PLACEMENT_3D('',#21626,#17769,#17770);
#15961=AXIS2_PLACEMENT_3D('',#21628,#17771,#17772);
#15962=AXIS2_PLACEMENT_3D('',#21633,#17773,#17774);
#15963=AXIS2_PLACEMENT_3D('',#21635,#17775,#17776);
#15964=AXIS2_PLACEMENT_3D('',#21637,#17777,#17778);
#15965=AXIS2_PLACEMENT_3D('',#21642,#17779,#17780);
#15966=AXIS2_PLACEMENT_3D('',#21644,#17781,#17782);
#15967=AXIS2_PLACEMENT_3D('',#21646,#17783,#17784);
#15968=AXIS2_PLACEMENT_3D('',#21651,#17785,#17786);
#15969=AXIS2_PLACEMENT_3D('',#21652,#17787,#17788);
#15970=AXIS2_PLACEMENT_3D('',#21653,#17789,#17790);
#15971=AXIS2_PLACEMENT_3D('',#21654,#17791,#17792);
#15972=AXIS2_PLACEMENT_3D('',#21657,#17795,#17796);
#15973=AXIS2_PLACEMENT_3D('',#21659,#17798,#17799);
#15974=AXIS2_PLACEMENT_3D('',#21661,#17801,#17802);
#15975=AXIS2_PLACEMENT_3D('',#21663,#17804,#17805);
#15976=AXIS2_PLACEMENT_3D('',#21665,#17807,#17808);
#15977=AXIS2_PLACEMENT_3D('',#21667,#17810,#17811);
#15978=AXIS2_PLACEMENT_3D('',#21669,#17812,#17813);
#15979=AXIS2_PLACEMENT_3D('',#21671,#17814,#17815);
#15980=AXIS2_PLACEMENT_3D('',#21673,#17816,#17817);
#15981=AXIS2_PLACEMENT_3D('',#21675,#17818,#17819);
#15982=AXIS2_PLACEMENT_3D('',#21677,#17820,#17821);
#15983=AXIS2_PLACEMENT_3D('',#21678,#17822,#17823);
#15984=AXIS2_PLACEMENT_3D('',#21719,#17825,#17826);
#15985=AXIS2_PLACEMENT_3D('',#21720,#17827,#17828);
#15986=AXIS2_PLACEMENT_3D('',#21723,#17830,#17831);
#15987=AXIS2_PLACEMENT_3D('',#21724,#17832,#17833);
#15988=AXIS2_PLACEMENT_3D('',#21728,#17835,#17836);
#15989=AXIS2_PLACEMENT_3D('',#21729,#17837,#17838);
#15990=AXIS2_PLACEMENT_3D('',#21764,#17841,#17842);
#15991=AXIS2_PLACEMENT_3D('',#21792,#17843,#17844);
#15992=AXIS2_PLACEMENT_3D('',#21796,#17846,#17847);
#15993=AXIS2_PLACEMENT_3D('',#21808,#17848,#17849);
#15994=AXIS2_PLACEMENT_3D('',#21809,#17850,#17851);
#15995=AXIS2_PLACEMENT_3D('',#21817,#17855,#17856);
#15996=AXIS2_PLACEMENT_3D('',#21819,#17857,#17858);
#15997=AXIS2_PLACEMENT_3D('',#21823,#17860,#17861);
#15998=AXIS2_PLACEMENT_3D('',#21825,#17862,#17863);
#15999=AXIS2_PLACEMENT_3D('',#21830,#17866,#17867);
#16000=AXIS2_PLACEMENT_3D('',#21832,#17868,#17869);
#16001=AXIS2_PLACEMENT_3D('',#21882,#17895,#17896);
#16002=AXIS2_PLACEMENT_3D('',#21886,#17898,#17899);
#16003=AXIS2_PLACEMENT_3D('',#21887,#17900,#17901);
#16004=AXIS2_PLACEMENT_3D('',#21890,#17903,#17904);
#16005=AXIS2_PLACEMENT_3D('',#21945,#17905,#17906);
#16006=AXIS2_PLACEMENT_3D('',#21957,#17908,#17909);
#16007=AXIS2_PLACEMENT_3D('',#22004,#17910,#17911);
#16008=AXIS2_PLACEMENT_3D('',#22005,#17912,#17913);
#16009=AXIS2_PLACEMENT_3D('',#22009,#17915,#17916);
#16010=AXIS2_PLACEMENT_3D('',#22010,#17917,#17918);
#16011=AXIS2_PLACEMENT_3D('',#22013,#17920,#17921);
#16012=AXIS2_PLACEMENT_3D('',#22014,#17922,#17923);
#16013=AXIS2_PLACEMENT_3D('',#22026,#17925,#17926);
#16014=AXIS2_PLACEMENT_3D('',#22027,#17927,#17928);
#16015=AXIS2_PLACEMENT_3D('',#22038,#17929,#17930);
#16016=AXIS2_PLACEMENT_3D('',#22042,#17932,#17933);
#16017=AXIS2_PLACEMENT_3D('',#22043,#17934,#17935);
#16018=AXIS2_PLACEMENT_3D('',#22046,#17937,#17938);
#16019=AXIS2_PLACEMENT_3D('',#22047,#17939,#17940);
#16020=AXIS2_PLACEMENT_3D('',#22049,#17942,#17943);
#16021=AXIS2_PLACEMENT_3D('',#22053,#17945,#17946);
#16022=AXIS2_PLACEMENT_3D('',#22054,#17947,#17948);
#16023=AXIS2_PLACEMENT_3D('',#22057,#17950,#17951);
#16024=AXIS2_PLACEMENT_3D('',#22058,#17952,#17953);
#16025=AXIS2_PLACEMENT_3D('',#22060,#17955,#17956);
#16026=AXIS2_PLACEMENT_3D('',#22064,#17958,#17959);
#16027=AXIS2_PLACEMENT_3D('',#22065,#17960,#17961);
#16028=AXIS2_PLACEMENT_3D('',#22068,#17963,#17964);
#16029=AXIS2_PLACEMENT_3D('',#22069,#17965,#17966);
#16030=AXIS2_PLACEMENT_3D('',#22072,#17968,#17969);
#16031=AXIS2_PLACEMENT_3D('',#22073,#17970,#17971);
#16032=AXIS2_PLACEMENT_3D('',#22077,#17973,#17974);
#16033=AXIS2_PLACEMENT_3D('',#22078,#17975,#17976);
#16034=AXIS2_PLACEMENT_3D('',#22081,#17978,#17979);
#16035=AXIS2_PLACEMENT_3D('',#22082,#17980,#17981);
#16036=AXIS2_PLACEMENT_3D('',#22084,#17983,#17984);
#16037=AXIS2_PLACEMENT_3D('',#22088,#17986,#17987);
#16038=AXIS2_PLACEMENT_3D('',#22089,#17988,#17989);
#16039=AXIS2_PLACEMENT_3D('',#22092,#17991,#17992);
#16040=AXIS2_PLACEMENT_3D('',#22093,#17993,#17994);
#16041=AXIS2_PLACEMENT_3D('',#22096,#17996,#17997);
#16042=AXIS2_PLACEMENT_3D('',#22097,#17998,#17999);
#16043=AXIS2_PLACEMENT_3D('',#22101,#18001,#18002);
#16044=AXIS2_PLACEMENT_3D('',#22102,#18003,#18004);
#16045=AXIS2_PLACEMENT_3D('',#22105,#18006,#18007);
#16046=AXIS2_PLACEMENT_3D('',#22106,#18008,#18009);
#16047=AXIS2_PLACEMENT_3D('',#22108,#18011,#18012);
#16048=AXIS2_PLACEMENT_3D('',#22112,#18014,#18015);
#16049=AXIS2_PLACEMENT_3D('',#22113,#18016,#18017);
#16050=AXIS2_PLACEMENT_3D('',#22116,#18019,#18020);
#16051=AXIS2_PLACEMENT_3D('',#22117,#18021,#18022);
#16052=AXIS2_PLACEMENT_3D('',#22120,#18024,#18025);
#16053=AXIS2_PLACEMENT_3D('',#22121,#18026,#18027);
#16054=AXIS2_PLACEMENT_3D('',#22125,#18029,#18030);
#16055=AXIS2_PLACEMENT_3D('',#22126,#18031,#18032);
#16056=AXIS2_PLACEMENT_3D('',#22129,#18034,#18035);
#16057=AXIS2_PLACEMENT_3D('',#22130,#18036,#18037);
#16058=AXIS2_PLACEMENT_3D('',#22132,#18039,#18040);
#16059=AXIS2_PLACEMENT_3D('',#22136,#18042,#18043);
#16060=AXIS2_PLACEMENT_3D('',#22137,#18044,#18045);
#16061=AXIS2_PLACEMENT_3D('',#22140,#18047,#18048);
#16062=AXIS2_PLACEMENT_3D('',#22141,#18049,#18050);
#16063=AXIS2_PLACEMENT_3D('',#22144,#18052,#18053);
#16064=AXIS2_PLACEMENT_3D('',#22145,#18054,#18055);
#16065=AXIS2_PLACEMENT_3D('',#22149,#18057,#18058);
#16066=AXIS2_PLACEMENT_3D('',#22150,#18059,#18060);
#16067=AXIS2_PLACEMENT_3D('',#22153,#18062,#18063);
#16068=AXIS2_PLACEMENT_3D('',#22154,#18064,#18065);
#16069=AXIS2_PLACEMENT_3D('',#22156,#18067,#18068);
#16070=AXIS2_PLACEMENT_3D('',#22160,#18070,#18071);
#16071=AXIS2_PLACEMENT_3D('',#22161,#18072,#18073);
#16072=AXIS2_PLACEMENT_3D('',#22164,#18075,#18076);
#16073=AXIS2_PLACEMENT_3D('',#22165,#18077,#18078);
#16074=AXIS2_PLACEMENT_3D('',#22167,#18080,#18081);
#16075=AXIS2_PLACEMENT_3D('',#22171,#18083,#18084);
#16076=AXIS2_PLACEMENT_3D('',#22172,#18085,#18086);
#16077=AXIS2_PLACEMENT_3D('',#22175,#18088,#18089);
#16078=AXIS2_PLACEMENT_3D('',#22176,#18090,#18091);
#16079=AXIS2_PLACEMENT_3D('',#22178,#18093,#18094);
#16080=AXIS2_PLACEMENT_3D('',#22182,#18096,#18097);
#16081=AXIS2_PLACEMENT_3D('',#22183,#18098,#18099);
#16082=AXIS2_PLACEMENT_3D('',#22187,#18102,#18103);
#16083=AXIS2_PLACEMENT_3D('',#22188,#18104,#18105);
#16084=AXIS2_PLACEMENT_3D('',#22190,#18107,#18108);
#16085=AXIS2_PLACEMENT_3D('',#22192,#18109,#18110);
#16086=AXIS2_PLACEMENT_3D('',#22195,#18112,#18113);
#16087=AXIS2_PLACEMENT_3D('',#22196,#18114,#18115);
#16088=AXIS2_PLACEMENT_3D('',#22199,#18117,#18118);
#16089=AXIS2_PLACEMENT_3D('',#22200,#18119,#18120);
#16090=AXIS2_PLACEMENT_3D('',#22202,#18121,#18122);
#16091=AXIS2_PLACEMENT_3D('',#22205,#18124,#18125);
#16092=AXIS2_PLACEMENT_3D('',#22206,#18126,#18127);
#16093=AXIS2_PLACEMENT_3D('',#22209,#18129,#18130);
#16094=AXIS2_PLACEMENT_3D('',#22210,#18131,#18132);
#16095=AXIS2_PLACEMENT_3D('',#22212,#18133,#18134);
#16096=AXIS2_PLACEMENT_3D('',#22215,#18136,#18137);
#16097=AXIS2_PLACEMENT_3D('',#22216,#18138,#18139);
#16098=AXIS2_PLACEMENT_3D('',#22219,#18141,#18142);
#16099=AXIS2_PLACEMENT_3D('',#22220,#18143,#18144);
#16100=AXIS2_PLACEMENT_3D('',#22222,#18145,#18146);
#16101=AXIS2_PLACEMENT_3D('',#22225,#18148,#18149);
#16102=AXIS2_PLACEMENT_3D('',#22226,#18150,#18151);
#16103=AXIS2_PLACEMENT_3D('',#22229,#18153,#18154);
#16104=AXIS2_PLACEMENT_3D('',#22230,#18155,#18156);
#16105=AXIS2_PLACEMENT_3D('',#22234,#18159,#18160);
#16106=AXIS2_PLACEMENT_3D('',#22236,#18162,#18163);
#16107=AXIS2_PLACEMENT_3D('',#22240,#18166,#18167);
#16108=AXIS2_PLACEMENT_3D('',#22244,#18170,#18171);
#16109=AXIS2_PLACEMENT_3D('',#22246,#18173,#18174);
#16110=AXIS2_PLACEMENT_3D('',#22248,#18175,#18176);
#16111=AXIS2_PLACEMENT_3D('',#22259,#18182,#18183);
#16112=AXIS2_PLACEMENT_3D('',#22261,#18184,#18185);
#16113=AXIS2_PLACEMENT_3D('',#22262,#18186,#18187);
#16114=AXIS2_PLACEMENT_3D('',#22268,#18191,#18192);
#16115=AXIS2_PLACEMENT_3D('',#22272,#18195,#18196);
#16116=AXIS2_PLACEMENT_3D('',#22277,#18200,#18201);
#16117=AXIS2_PLACEMENT_3D('',#22278,#18202,#18203);
#16118=AXIS2_PLACEMENT_3D('',#22287,#18209,#18210);
#16119=AXIS2_PLACEMENT_3D('',#22290,#18213,#18214);
#16120=AXIS2_PLACEMENT_3D('',#22291,#18215,#18216);
#16121=AXIS2_PLACEMENT_3D('',#22293,#18217,#18218);
#16122=AXIS2_PLACEMENT_3D('',#22295,#18220,#18221);
#16123=AXIS2_PLACEMENT_3D('',#22296,#18222,#18223);
#16124=AXIS2_PLACEMENT_3D('',#22299,#18225,#18226);
#16125=AXIS2_PLACEMENT_3D('',#22300,#18227,#18228);
#16126=AXIS2_PLACEMENT_3D('',#22302,#18229,#18230);
#16127=AXIS2_PLACEMENT_3D('',#22313,#18236,#18237);
#16128=AXIS2_PLACEMENT_3D('',#22314,#18238,#18239);
#16129=AXIS2_PLACEMENT_3D('',#22315,#18240,#18241);
#16130=AXIS2_PLACEMENT_3D('',#22318,#18244,#18245);
#16131=AXIS2_PLACEMENT_3D('',#22321,#18248,#18249);
#16132=AXIS2_PLACEMENT_3D('',#22322,#18250,#18251);
#16133=AXIS2_PLACEMENT_3D('',#22324,#18253,#18254);
#16134=AXIS2_PLACEMENT_3D('',#22326,#18256,#18257);
#16135=AXIS2_PLACEMENT_3D('',#22332,#18261,#18262);
#16136=AXIS2_PLACEMENT_3D('',#22336,#18265,#18266);
#16137=AXIS2_PLACEMENT_3D('',#22340,#18269,#18270);
#16138=AXIS2_PLACEMENT_3D('',#22342,#18272,#18273);
#16139=AXIS2_PLACEMENT_3D('',#22343,#18274,#18275);
#16140=AXIS2_PLACEMENT_3D('',#22349,#18279,#18280);
#16141=AXIS2_PLACEMENT_3D('',#22353,#18283,#18284);
#16142=AXIS2_PLACEMENT_3D('',#22357,#18287,#18288);
#16143=AXIS2_PLACEMENT_3D('',#22359,#18290,#18291);
#16144=AXIS2_PLACEMENT_3D('',#22360,#18292,#18293);
#16145=AXIS2_PLACEMENT_3D('',#22366,#18297,#18298);
#16146=AXIS2_PLACEMENT_3D('',#22370,#18301,#18302);
#16147=AXIS2_PLACEMENT_3D('',#22374,#18305,#18306);
#16148=AXIS2_PLACEMENT_3D('',#22376,#18308,#18309);
#16149=AXIS2_PLACEMENT_3D('',#22377,#18310,#18311);
#16150=AXIS2_PLACEMENT_3D('',#22383,#18315,#18316);
#16151=AXIS2_PLACEMENT_3D('',#22387,#18319,#18320);
#16152=AXIS2_PLACEMENT_3D('',#22391,#18323,#18324);
#16153=AXIS2_PLACEMENT_3D('',#22393,#18326,#18327);
#16154=AXIS2_PLACEMENT_3D('',#22394,#18328,#18329);
#16155=AXIS2_PLACEMENT_3D('',#22400,#18333,#18334);
#16156=AXIS2_PLACEMENT_3D('',#22404,#18337,#18338);
#16157=AXIS2_PLACEMENT_3D('',#22408,#18341,#18342);
#16158=AXIS2_PLACEMENT_3D('',#22410,#18344,#18345);
#16159=AXIS2_PLACEMENT_3D('',#22411,#18346,#18347);
#16160=AXIS2_PLACEMENT_3D('',#22417,#18351,#18352);
#16161=AXIS2_PLACEMENT_3D('',#22421,#18355,#18356);
#16162=AXIS2_PLACEMENT_3D('',#22425,#18359,#18360);
#16163=AXIS2_PLACEMENT_3D('',#22427,#18362,#18363);
#16164=AXIS2_PLACEMENT_3D('',#22428,#18364,#18365);
#16165=AXIS2_PLACEMENT_3D('',#22431,#18367,#18368);
#16166=AXIS2_PLACEMENT_3D('',#22432,#18369,#18370);
#16167=AXIS2_PLACEMENT_3D('',#22434,#18371,#18372);
#16168=AXIS2_PLACEMENT_3D('',#22435,#18373,#18374);
#16169=AXIS2_PLACEMENT_3D('',#22438,#18376,#18377);
#16170=AXIS2_PLACEMENT_3D('',#22439,#18378,#18379);
#16171=AXIS2_PLACEMENT_3D('',#22441,#18380,#18381);
#16172=AXIS2_PLACEMENT_3D('',#22442,#18382,#18383);
#16173=AXIS2_PLACEMENT_3D('',#22445,#18385,#18386);
#16174=AXIS2_PLACEMENT_3D('',#22446,#18387,#18388);
#16175=AXIS2_PLACEMENT_3D('',#22448,#18389,#18390);
#16176=AXIS2_PLACEMENT_3D('',#22449,#18391,#18392);
#16177=AXIS2_PLACEMENT_3D('',#22492,#18395,#18396);
#16178=AXIS2_PLACEMENT_3D('',#22528,#18397,#18398);
#16179=AXIS2_PLACEMENT_3D('',#22530,#18399,#18400);
#16180=AXIS2_PLACEMENT_3D('',#22531,#18401,#18402);
#16181=AXIS2_PLACEMENT_3D('',#22534,#18404,#18405);
#16182=AXIS2_PLACEMENT_3D('',#22535,#18406,#18407);
#16183=AXIS2_PLACEMENT_3D('',#22537,#18408,#18409);
#16184=AXIS2_PLACEMENT_3D('',#22538,#18410,#18411);
#16185=AXIS2_PLACEMENT_3D('',#22541,#18413,#18414);
#16186=AXIS2_PLACEMENT_3D('',#22542,#18415,#18416);
#16187=AXIS2_PLACEMENT_3D('',#22544,#18417,#18418);
#16188=AXIS2_PLACEMENT_3D('',#22545,#18419,#18420);
#16189=AXIS2_PLACEMENT_3D('',#22547,#18422,#18423);
#16190=AXIS2_PLACEMENT_3D('',#22550,#18425,#18426);
#16191=AXIS2_PLACEMENT_3D('',#22551,#18427,#18428);
#16192=AXIS2_PLACEMENT_3D('',#22553,#18429,#18430);
#16193=AXIS2_PLACEMENT_3D('',#22554,#18431,#18432);
#16194=AXIS2_PLACEMENT_3D('',#22557,#18434,#18435);
#16195=AXIS2_PLACEMENT_3D('',#22558,#18436,#18437);
#16196=AXIS2_PLACEMENT_3D('',#22560,#18438,#18439);
#16197=AXIS2_PLACEMENT_3D('',#22561,#18440,#18441);
#16198=AXIS2_PLACEMENT_3D('',#22564,#18443,#18444);
#16199=AXIS2_PLACEMENT_3D('',#22565,#18445,#18446);
#16200=AXIS2_PLACEMENT_3D('',#22567,#18448,#18449);
#16201=AXIS2_PLACEMENT_3D('',#22568,#18450,#18451);
#16202=AXIS2_PLACEMENT_3D('',#22569,#18452,#18453);
#16203=AXIS2_PLACEMENT_3D('',#22570,#18454,#18455);
#16204=AXIS2_PLACEMENT_3D('',#22571,#18456,#18457);
#16205=AXIS2_PLACEMENT_3D('',#22573,#18458,#18459);
#16206=AXIS2_PLACEMENT_3D('',#22576,#18461,#18462);
#16207=AXIS2_PLACEMENT_3D('',#22577,#18463,#18464);
#16208=AXIS2_PLACEMENT_3D('',#22580,#18466,#18467);
#16209=AXIS2_PLACEMENT_3D('',#22581,#18468,#18469);
#16210=AXIS2_PLACEMENT_3D('',#22583,#18470,#18471);
#16211=AXIS2_PLACEMENT_3D('',#22584,#18472,#18473);
#16212=AXIS2_PLACEMENT_3D('',#22587,#18474,#18475);
#16213=AXIS2_PLACEMENT_3D('',#22594,#18476,#18477);
#16214=AXIS2_PLACEMENT_3D('',#22599,#18478,#18479);
#16215=AXIS2_PLACEMENT_3D('',#22601,#18480,#18481);
#16216=AXIS2_PLACEMENT_3D('',#22607,#18482,#18483);
#16217=AXIS2_PLACEMENT_3D('',#22608,#18484,#18485);
#16218=AXIS2_PLACEMENT_3D('',#22610,#18486,#18487);
#16219=AXIS2_PLACEMENT_3D('',#22616,#18488,#18489);
#16220=AXIS2_PLACEMENT_3D('',#22617,#18490,#18491);
#16221=AXIS2_PLACEMENT_3D('',#22619,#18492,#18493);
#16222=AXIS2_PLACEMENT_3D('',#22625,#18494,#18495);
#16223=AXIS2_PLACEMENT_3D('',#22626,#18496,#18497);
#16224=AXIS2_PLACEMENT_3D('',#22628,#18498,#18499);
#16225=AXIS2_PLACEMENT_3D('',#22634,#18500,#18501);
#16226=AXIS2_PLACEMENT_3D('',#22635,#18502,#18503);
#16227=AXIS2_PLACEMENT_3D('',#22637,#18504,#18505);
#16228=AXIS2_PLACEMENT_3D('',#22639,#18506,#18507);
#16229=AXIS2_PLACEMENT_3D('',#22644,#18508,#18509);
#16230=AXIS2_PLACEMENT_3D('',#22646,#18510,#18511);
#16231=AXIS2_PLACEMENT_3D('',#22648,#18512,#18513);
#16232=AXIS2_PLACEMENT_3D('',#22653,#18514,#18515);
#16233=AXIS2_PLACEMENT_3D('',#22654,#18516,#18517);
#16234=AXIS2_PLACEMENT_3D('',#22655,#18518,#18519);
#16235=AXIS2_PLACEMENT_3D('',#22656,#18520,#18521);
#16236=AXIS2_PLACEMENT_3D('',#22660,#18523,#18524);
#16237=AXIS2_PLACEMENT_3D('',#22662,#18526,#18527);
#16238=AXIS2_PLACEMENT_3D('',#22665,#18529,#18530);
#16239=AXIS2_PLACEMENT_3D('',#22666,#18531,#18532);
#16240=AXIS2_PLACEMENT_3D('',#22669,#18534,#18535);
#16241=AXIS2_PLACEMENT_3D('',#22670,#18536,#18537);
#16242=AXIS2_PLACEMENT_3D('',#22673,#18539,#18540);
#16243=AXIS2_PLACEMENT_3D('',#22674,#18541,#18542);
#16244=AXIS2_PLACEMENT_3D('',#22676,#18543,#18544);
#16245=AXIS2_PLACEMENT_3D('',#22678,#18545,#18546);
#16246=AXIS2_PLACEMENT_3D('',#22680,#18547,#18548);
#16247=AXIS2_PLACEMENT_3D('',#22682,#18549,#18550);
#16248=AXIS2_PLACEMENT_3D('',#22684,#18551,#18552);
#16249=AXIS2_PLACEMENT_3D('',#22685,#18553,#18554);
#16250=AXIS2_PLACEMENT_3D('',#22687,#18555,#18556);
#16251=AXIS2_PLACEMENT_3D('',#22690,#18558,#18559);
#16252=AXIS2_PLACEMENT_3D('',#22691,#18560,#18561);
#16253=AXIS2_PLACEMENT_3D('',#22694,#18563,#18564);
#16254=AXIS2_PLACEMENT_3D('',#22695,#18565,#18566);
#16255=AXIS2_PLACEMENT_3D('',#22698,#18568,#18569);
#16256=AXIS2_PLACEMENT_3D('',#22699,#18570,#18571);
#16257=AXIS2_PLACEMENT_3D('',#22701,#18572,#18573);
#16258=AXIS2_PLACEMENT_3D('',#22702,#18574,#18575);
#16259=AXIS2_PLACEMENT_3D('',#22704,#18577,#18578);
#16260=AXIS2_PLACEMENT_3D('',#22706,#18579,#18580);
#16261=AXIS2_PLACEMENT_3D('',#22709,#18582,#18583);
#16262=AXIS2_PLACEMENT_3D('',#22710,#18584,#18585);
#16263=AXIS2_PLACEMENT_3D('',#22713,#18587,#18588);
#16264=AXIS2_PLACEMENT_3D('',#22714,#18589,#18590);
#16265=AXIS2_PLACEMENT_3D('',#22717,#18592,#18593);
#16266=AXIS2_PLACEMENT_3D('',#22718,#18594,#18595);
#16267=AXIS2_PLACEMENT_3D('',#22720,#18596,#18597);
#16268=AXIS2_PLACEMENT_3D('',#22721,#18598,#18599);
#16269=AXIS2_PLACEMENT_3D('',#22723,#18601,#18602);
#16270=AXIS2_PLACEMENT_3D('',#22725,#18603,#18604);
#16271=AXIS2_PLACEMENT_3D('',#22728,#18606,#18607);
#16272=AXIS2_PLACEMENT_3D('',#22729,#18608,#18609);
#16273=AXIS2_PLACEMENT_3D('',#22732,#18611,#18612);
#16274=AXIS2_PLACEMENT_3D('',#22733,#18613,#18614);
#16275=AXIS2_PLACEMENT_3D('',#22736,#18616,#18617);
#16276=AXIS2_PLACEMENT_3D('',#22737,#18618,#18619);
#16277=AXIS2_PLACEMENT_3D('',#22739,#18620,#18621);
#16278=AXIS2_PLACEMENT_3D('',#22740,#18622,#18623);
#16279=AXIS2_PLACEMENT_3D('',#22742,#18625,#18626);
#16280=AXIS2_PLACEMENT_3D('',#22744,#18627,#18628);
#16281=AXIS2_PLACEMENT_3D('',#22747,#18630,#18631);
#16282=AXIS2_PLACEMENT_3D('',#22748,#18632,#18633);
#16283=AXIS2_PLACEMENT_3D('',#22751,#18635,#18636);
#16284=AXIS2_PLACEMENT_3D('',#22752,#18637,#18638);
#16285=AXIS2_PLACEMENT_3D('',#22755,#18640,#18641);
#16286=AXIS2_PLACEMENT_3D('',#22756,#18642,#18643);
#16287=AXIS2_PLACEMENT_3D('',#22758,#18644,#18645);
#16288=AXIS2_PLACEMENT_3D('',#22759,#18646,#18647);
#16289=AXIS2_PLACEMENT_3D('',#22761,#18649,#18650);
#16290=AXIS2_PLACEMENT_3D('',#22763,#18651,#18652);
#16291=AXIS2_PLACEMENT_3D('',#22765,#18654,#18655);
#16292=AXIS2_PLACEMENT_3D('',#22768,#18657,#18658);
#16293=AXIS2_PLACEMENT_3D('',#22769,#18659,#18660);
#16294=AXIS2_PLACEMENT_3D('',#22771,#18661,#18662);
#16295=AXIS2_PLACEMENT_3D('',#22772,#18663,#18664);
#16296=AXIS2_PLACEMENT_3D('',#22774,#18666,#18667);
#16297=AXIS2_PLACEMENT_3D('',#22777,#18669,#18670);
#16298=AXIS2_PLACEMENT_3D('',#22778,#18671,#18672);
#16299=AXIS2_PLACEMENT_3D('',#22781,#18674,#18675);
#16300=AXIS2_PLACEMENT_3D('',#22782,#18676,#18677);
#16301=AXIS2_PLACEMENT_3D('',#22785,#18679,#18680);
#16302=AXIS2_PLACEMENT_3D('',#22786,#18681,#18682);
#16303=AXIS2_PLACEMENT_3D('',#22787,#18683,#18684);
#16304=AXIS2_PLACEMENT_3D('',#22788,#18685,#18686);
#16305=AXIS2_PLACEMENT_3D('',#22789,#18687,#18688);
#16306=AXIS2_PLACEMENT_3D('',#22790,#18689,#18690);
#16307=AXIS2_PLACEMENT_3D('',#22799,#18695,#18696);
#16308=AXIS2_PLACEMENT_3D('',#22805,#18700,#18701);
#16309=AXIS2_PLACEMENT_3D('',#22811,#18705,#18706);
#16310=AXIS2_PLACEMENT_3D('',#22817,#18710,#18711);
#16311=AXIS2_PLACEMENT_3D('',#22823,#18715,#18716);
#16312=AXIS2_PLACEMENT_3D('',#22829,#18720,#18721);
#16313=AXIS2_PLACEMENT_3D('',#22835,#18725,#18726);
#16314=AXIS2_PLACEMENT_3D('',#22838,#18729,#18730);
#16315=AXIS2_PLACEMENT_3D('',#22844,#18734,#18735);
#16316=AXIS2_PLACEMENT_3D('',#22848,#18738,#18739);
#16317=AXIS2_PLACEMENT_3D('',#22852,#18742,#18743);
#16318=AXIS2_PLACEMENT_3D('',#22856,#18746,#18747);
#16319=AXIS2_PLACEMENT_3D('',#22858,#18748,#18749);
#16320=AXIS2_PLACEMENT_3D('',#22892,#18766,#18767);
#16321=AXIS2_PLACEMENT_3D('',#22894,#18768,#18769);
#16322=AXIS2_PLACEMENT_3D('',#22896,#18770,#18771);
#16323=AXIS2_PLACEMENT_3D('',#22898,#18772,#18773);
#16324=AXIS2_PLACEMENT_3D('',#22899,#18774,#18775);
#16325=AXIS2_PLACEMENT_3D('',#22901,#18776,#18777);
#16326=AXIS2_PLACEMENT_3D('',#22904,#18779,#18780);
#16327=AXIS2_PLACEMENT_3D('',#22905,#18781,#18782);
#16328=AXIS2_PLACEMENT_3D('',#22908,#18784,#18785);
#16329=AXIS2_PLACEMENT_3D('',#22909,#18786,#18787);
#16330=AXIS2_PLACEMENT_3D('',#22912,#18789,#18790);
#16331=AXIS2_PLACEMENT_3D('',#22913,#18791,#18792);
#16332=AXIS2_PLACEMENT_3D('',#22915,#18793,#18794);
#16333=AXIS2_PLACEMENT_3D('',#22916,#18795,#18796);
#16334=AXIS2_PLACEMENT_3D('',#22919,#18798,#18799);
#16335=AXIS2_PLACEMENT_3D('',#22920,#18800,#18801);
#16336=AXIS2_PLACEMENT_3D('',#22922,#18802,#18803);
#16337=AXIS2_PLACEMENT_3D('',#22925,#18805,#18806);
#16338=AXIS2_PLACEMENT_3D('',#22926,#18807,#18808);
#16339=AXIS2_PLACEMENT_3D('',#22929,#18810,#18811);
#16340=AXIS2_PLACEMENT_3D('',#22930,#18812,#18813);
#16341=AXIS2_PLACEMENT_3D('',#22933,#18815,#18816);
#16342=AXIS2_PLACEMENT_3D('',#22934,#18817,#18818);
#16343=AXIS2_PLACEMENT_3D('',#22936,#18819,#18820);
#16344=AXIS2_PLACEMENT_3D('',#22937,#18821,#18822);
#16345=AXIS2_PLACEMENT_3D('',#22940,#18824,#18825);
#16346=AXIS2_PLACEMENT_3D('',#22941,#18826,#18827);
#16347=AXIS2_PLACEMENT_3D('',#22943,#18828,#18829);
#16348=AXIS2_PLACEMENT_3D('',#22946,#18831,#18832);
#16349=AXIS2_PLACEMENT_3D('',#22947,#18833,#18834);
#16350=AXIS2_PLACEMENT_3D('',#22950,#18836,#18837);
#16351=AXIS2_PLACEMENT_3D('',#22951,#18838,#18839);
#16352=AXIS2_PLACEMENT_3D('',#22954,#18841,#18842);
#16353=AXIS2_PLACEMENT_3D('',#22955,#18843,#18844);
#16354=AXIS2_PLACEMENT_3D('',#22957,#18845,#18846);
#16355=AXIS2_PLACEMENT_3D('',#22958,#18847,#18848);
#16356=AXIS2_PLACEMENT_3D('',#22961,#18850,#18851);
#16357=AXIS2_PLACEMENT_3D('',#22962,#18852,#18853);
#16358=AXIS2_PLACEMENT_3D('',#22964,#18854,#18855);
#16359=AXIS2_PLACEMENT_3D('',#22967,#18857,#18858);
#16360=AXIS2_PLACEMENT_3D('',#22968,#18859,#18860);
#16361=AXIS2_PLACEMENT_3D('',#22971,#18862,#18863);
#16362=AXIS2_PLACEMENT_3D('',#22972,#18864,#18865);
#16363=AXIS2_PLACEMENT_3D('',#22975,#18867,#18868);
#16364=AXIS2_PLACEMENT_3D('',#22976,#18869,#18870);
#16365=AXIS2_PLACEMENT_3D('',#22978,#18871,#18872);
#16366=AXIS2_PLACEMENT_3D('',#22979,#18873,#18874);
#16367=AXIS2_PLACEMENT_3D('',#22982,#18876,#18877);
#16368=AXIS2_PLACEMENT_3D('',#22983,#18878,#18879);
#16369=AXIS2_PLACEMENT_3D('',#22985,#18880,#18881);
#16370=AXIS2_PLACEMENT_3D('',#22988,#18883,#18884);
#16371=AXIS2_PLACEMENT_3D('',#22989,#18885,#18886);
#16372=AXIS2_PLACEMENT_3D('',#22992,#18888,#18889);
#16373=AXIS2_PLACEMENT_3D('',#22993,#18890,#18891);
#16374=AXIS2_PLACEMENT_3D('',#22995,#18893,#18894);
#16375=AXIS2_PLACEMENT_3D('',#22997,#18895,#18896);
#16376=AXIS2_PLACEMENT_3D('',#23000,#18898,#18899);
#16377=AXIS2_PLACEMENT_3D('',#23001,#18900,#18901);
#16378=AXIS2_PLACEMENT_3D('',#23004,#18903,#18904);
#16379=AXIS2_PLACEMENT_3D('',#23005,#18905,#18906);
#16380=AXIS2_PLACEMENT_3D('',#23007,#18908,#18909);
#16381=AXIS2_PLACEMENT_3D('',#23009,#18910,#18911);
#16382=AXIS2_PLACEMENT_3D('',#23012,#18913,#18914);
#16383=AXIS2_PLACEMENT_3D('',#23013,#18915,#18916);
#16384=AXIS2_PLACEMENT_3D('',#23016,#18918,#18919);
#16385=AXIS2_PLACEMENT_3D('',#23017,#18920,#18921);
#16386=AXIS2_PLACEMENT_3D('',#23019,#18923,#18924);
#16387=AXIS2_PLACEMENT_3D('',#23021,#18925,#18926);
#16388=AXIS2_PLACEMENT_3D('',#23024,#18928,#18929);
#16389=AXIS2_PLACEMENT_3D('',#23025,#18930,#18931);
#16390=AXIS2_PLACEMENT_3D('',#23028,#18933,#18934);
#16391=AXIS2_PLACEMENT_3D('',#23029,#18935,#18936);
#16392=AXIS2_PLACEMENT_3D('',#23031,#18938,#18939);
#16393=AXIS2_PLACEMENT_3D('',#23037,#18943,#18944);
#16394=AXIS2_PLACEMENT_3D('',#23041,#18947,#18948);
#16395=AXIS2_PLACEMENT_3D('',#23045,#18951,#18952);
#16396=AXIS2_PLACEMENT_3D('',#23047,#18954,#18955);
#16397=AXIS2_PLACEMENT_3D('',#23053,#18959,#18960);
#16398=AXIS2_PLACEMENT_3D('',#23057,#18963,#18964);
#16399=AXIS2_PLACEMENT_3D('',#23061,#18967,#18968);
#16400=AXIS2_PLACEMENT_3D('',#23063,#18970,#18971);
#16401=AXIS2_PLACEMENT_3D('',#23069,#18975,#18976);
#16402=AXIS2_PLACEMENT_3D('',#23073,#18979,#18980);
#16403=AXIS2_PLACEMENT_3D('',#23077,#18983,#18984);
#16404=AXIS2_PLACEMENT_3D('',#23079,#18986,#18987);
#16405=AXIS2_PLACEMENT_3D('',#23085,#18991,#18992);
#16406=AXIS2_PLACEMENT_3D('',#23089,#18995,#18996);
#16407=AXIS2_PLACEMENT_3D('',#23093,#18999,#19000);
#16408=AXIS2_PLACEMENT_3D('',#23095,#19002,#19003);
#16409=AXIS2_PLACEMENT_3D('',#23097,#19004,#19005);
#16410=AXIS2_PLACEMENT_3D('',#23100,#19007,#19008);
#16411=AXIS2_PLACEMENT_3D('',#23101,#19009,#19010);
#16412=AXIS2_PLACEMENT_3D('',#23104,#19012,#19013);
#16413=AXIS2_PLACEMENT_3D('',#23105,#19014,#19015);
#16414=AXIS2_PLACEMENT_3D('',#23106,#19016,#19017);
#16415=AXIS2_PLACEMENT_3D('',#23110,#19020,#19021);
#16416=AXIS2_PLACEMENT_3D('',#23114,#19024,#19025);
#16417=AXIS2_PLACEMENT_3D('',#23118,#19028,#19029);
#16418=AXIS2_PLACEMENT_3D('',#23120,#19031,#19032);
#16419=AXIS2_PLACEMENT_3D('',#23121,#19033,#19034);
#16420=AXIS2_PLACEMENT_3D('',#23122,#19035,#19036);
#16421=AXIS2_PLACEMENT_3D('',#23190,#19038,#19039);
#16422=AXIS2_PLACEMENT_3D('',#23199,#19041,#19042);
#16423=AXIS2_PLACEMENT_3D('',#23319,#19044,#19045);
#16424=AXIS2_PLACEMENT_3D('',#23449,#19047,#19048);
#16425=AXIS2_PLACEMENT_3D('',#23589,#19050,#19051);
#16426=AXIS2_PLACEMENT_3D('',#23719,#19053,#19054);
#16427=AXIS2_PLACEMENT_3D('',#23843,#19056,#19057);
#16428=AXIS2_PLACEMENT_3D('',#23904,#19058,#19059);
#16429=AXIS2_PLACEMENT_3D('',#23933,#19061,#19062);
#16430=AXIS2_PLACEMENT_3D('',#23946,#19067,#19068);
#16431=AXIS2_PLACEMENT_3D('',#23948,#19069,#19070);
#16432=AXIS2_PLACEMENT_3D('',#23952,#19073,#19074);
#16433=AXIS2_PLACEMENT_3D('',#23962,#19078,#19079);
#16434=AXIS2_PLACEMENT_3D('',#23964,#19081,#19082);
#16435=AXIS2_PLACEMENT_3D('',#23966,#19083,#19084);
#16436=AXIS2_PLACEMENT_3D('',#23969,#19086,#19087);
#16437=AXIS2_PLACEMENT_3D('',#23970,#19088,#19089);
#16438=AXIS2_PLACEMENT_3D('',#23971,#19090,#19091);
#16439=AXIS2_PLACEMENT_3D('',#23972,#19092,#19093);
#16440=AXIS2_PLACEMENT_3D('',#23973,#19094,#19095);
#16441=AXIS2_PLACEMENT_3D('',#23976,#19097,#19098);
#16442=AXIS2_PLACEMENT_3D('',#23978,#19099,#19100);
#16443=AXIS2_PLACEMENT_3D('',#23981,#19102,#19103);
#16444=AXIS2_PLACEMENT_3D('',#23982,#19104,#19105);
#16445=AXIS2_PLACEMENT_3D('',#24205,#19108,#19109);
#16446=AXIS2_PLACEMENT_3D('',#24270,#19112,#19113);
#16447=AXIS2_PLACEMENT_3D('',#24271,#19114,#19115);
#16448=AXIS2_PLACEMENT_3D('',#24274,#19117,#19118);
#16449=AXIS2_PLACEMENT_3D('',#26137,#19120,#19121);
#16450=AXIS2_PLACEMENT_3D('',#26763,#19123,#19124);
#16451=AXIS2_PLACEMENT_3D('',#26764,#19125,#19126);
#16452=AXIS2_PLACEMENT_3D('',#26766,#19127,#19128);
#16453=AXIS2_PLACEMENT_3D('',#26767,#19129,#19130);
#16454=AXIS2_PLACEMENT_3D('',#26769,#19131,#19132);
#16455=AXIS2_PLACEMENT_3D('',#26771,#19134,#19135);
#16456=AXIS2_PLACEMENT_3D('',#26773,#19136,#19137);
#16457=AXIS2_PLACEMENT_3D('',#26775,#19139,#19140);
#16458=AXIS2_PLACEMENT_3D('',#26777,#19141,#19142);
#16459=AXIS2_PLACEMENT_3D('',#26778,#19143,#19144);
#16460=AXIS2_PLACEMENT_3D('',#26780,#19145,#19146);
#16461=AXIS2_PLACEMENT_3D('',#26782,#19148,#19149);
#16462=AXIS2_PLACEMENT_3D('',#26784,#19150,#19151);
#16463=AXIS2_PLACEMENT_3D('',#26786,#19153,#19154);
#16464=AXIS2_PLACEMENT_3D('',#26787,#19155,#19156);
#16465=AXIS2_PLACEMENT_3D('',#26789,#19157,#19158);
#16466=AXIS2_PLACEMENT_3D('',#26790,#19159,#19160);
#16467=AXIS2_PLACEMENT_3D('',#26792,#19161,#19162);
#16468=AXIS2_PLACEMENT_3D('',#26794,#19164,#19165);
#16469=AXIS2_PLACEMENT_3D('',#26797,#19167,#19168);
#16470=AXIS2_PLACEMENT_3D('',#26798,#19169,#19170);
#16471=AXIS2_PLACEMENT_3D('',#26800,#19171,#19172);
#16472=AXIS2_PLACEMENT_3D('',#26801,#19173,#19174);
#16473=AXIS2_PLACEMENT_3D('',#26803,#19175,#19176);
#16474=AXIS2_PLACEMENT_3D('',#26805,#19178,#19179);
#16475=AXIS2_PLACEMENT_3D('',#26808,#19181,#19182);
#16476=AXIS2_PLACEMENT_3D('',#26809,#19183,#19184);
#16477=AXIS2_PLACEMENT_3D('',#26810,#19185,#19186);
#16478=AXIS2_PLACEMENT_3D('',#26811,#19187,#19188);
#16479=AXIS2_PLACEMENT_3D('',#26814,#19189,#19190);
#16480=AXIS2_PLACEMENT_3D('',#26817,#19192,#19193);
#16481=AXIS2_PLACEMENT_3D('',#26818,#19194,#19195);
#16482=AXIS2_PLACEMENT_3D('',#26819,#19196,#19197);
#16483=AXIS2_PLACEMENT_3D('',#26823,#19199,#19200);
#16484=AXIS2_PLACEMENT_3D('',#26824,#19201,#19202);
#16485=AXIS2_PLACEMENT_3D('',#26825,#19203,#19204);
#16486=AXIS2_PLACEMENT_3D('',#26848,#19205,#19206);
#16487=AXIS2_PLACEMENT_3D('',#26891,#19208,#19209);
#16488=AXIS2_PLACEMENT_3D('',#26937,#19211,#19212);
#16489=AXIS2_PLACEMENT_3D('',#26980,#19214,#19215);
#16490=AXIS2_PLACEMENT_3D('',#27026,#19217,#19218);
#16491=AXIS2_PLACEMENT_3D('',#27069,#19220,#19221);
#16492=AXIS2_PLACEMENT_3D('',#27112,#19223,#19224);
#16493=AXIS2_PLACEMENT_3D('',#27155,#19226,#19227);
#16494=AXIS2_PLACEMENT_3D('',#27195,#19229,#19230);
#16495=AXIS2_PLACEMENT_3D('',#27237,#19232,#19233);
#16496=AXIS2_PLACEMENT_3D('',#27276,#19235,#19236);
#16497=AXIS2_PLACEMENT_3D('',#27315,#19238,#19239);
#16498=AXIS2_PLACEMENT_3D('',#27356,#19241,#19242);
#16499=AXIS2_PLACEMENT_3D('',#27393,#19244,#19245);
#16500=AXIS2_PLACEMENT_3D('',#27429,#19247,#19248);
#16501=AXIS2_PLACEMENT_3D('',#27468,#19250,#19251);
#16502=AXIS2_PLACEMENT_3D('',#27506,#19253,#19254);
#16503=AXIS2_PLACEMENT_3D('',#27544,#19256,#19257);
#16504=AXIS2_PLACEMENT_3D('',#27605,#19259,#19260);
#16505=AXIS2_PLACEMENT_3D('',#27643,#19262,#19263);
#16506=AXIS2_PLACEMENT_3D('',#27683,#19265,#19266);
#16507=AXIS2_PLACEMENT_3D('',#27714,#19268,#19269);
#16508=AXIS2_PLACEMENT_3D('',#27758,#19271,#19272);
#16509=AXIS2_PLACEMENT_3D('',#27801,#19274,#19275);
#16510=AXIS2_PLACEMENT_3D('',#27848,#19277,#19278);
#16511=AXIS2_PLACEMENT_3D('',#27891,#19280,#19281);
#16512=AXIS2_PLACEMENT_3D('',#27937,#19283,#19284);
#16513=AXIS2_PLACEMENT_3D('',#27978,#19286,#19287);
#16514=AXIS2_PLACEMENT_3D('',#28021,#19289,#19290);
#16515=AXIS2_PLACEMENT_3D('',#28051,#19292,#19293);
#16516=AXIS2_PLACEMENT_3D('',#28112,#19295,#19296);
#16517=AXIS2_PLACEMENT_3D('',#28115,#19298,#19299);
#16518=AXIS2_PLACEMENT_3D('',#28116,#19300,#19301);
#16519=AXIS2_PLACEMENT_3D('',#28149,#19303,#19304);
#16520=AXIS2_PLACEMENT_3D('',#28191,#19306,#19307);
#16521=AXIS2_PLACEMENT_3D('',#28270,#19309,#19310);
#16522=AXIS2_PLACEMENT_3D('',#28300,#19312,#19313);
#16523=AXIS2_PLACEMENT_3D('',#28380,#19315,#19316);
#16524=AXIS2_PLACEMENT_3D('',#28411,#19318,#19319);
#16525=AXIS2_PLACEMENT_3D('',#28446,#19321,#19322);
#16526=AXIS2_PLACEMENT_3D('',#28517,#19324,#19325);
#16527=AXIS2_PLACEMENT_3D('',#28561,#19327,#19328);
#16528=AXIS2_PLACEMENT_3D('',#28601,#19330,#19331);
#16529=AXIS2_PLACEMENT_3D('',#28630,#19333,#19334);
#16530=AXIS2_PLACEMENT_3D('',#28659,#19336,#19337);
#16531=AXIS2_PLACEMENT_3D('',#28688,#19339,#19340);
#16532=AXIS2_PLACEMENT_3D('',#28717,#19342,#19343);
#16533=AXIS2_PLACEMENT_3D('',#28745,#19345,#19346);
#16534=AXIS2_PLACEMENT_3D('',#28806,#19348,#19349);
#16535=AXIS2_PLACEMENT_3D('',#28836,#19351,#19352);
#16536=AXIS2_PLACEMENT_3D('',#28863,#19354,#19355);
#16537=AXIS2_PLACEMENT_3D('',#28936,#19357,#19358);
#16538=AXIS2_PLACEMENT_3D('',#28999,#19360,#19361);
#16539=AXIS2_PLACEMENT_3D('',#29029,#19363,#19364);
#16540=AXIS2_PLACEMENT_3D('',#29060,#19366,#19367);
#16541=AXIS2_PLACEMENT_3D('',#29089,#19369,#19370);
#16542=AXIS2_PLACEMENT_3D('',#29120,#19372,#19373);
#16543=AXIS2_PLACEMENT_3D('',#29193,#19375,#19376);
#16544=AXIS2_PLACEMENT_3D('',#29266,#19378,#19379);
#16545=AXIS2_PLACEMENT_3D('',#29301,#19381,#19382);
#16546=AXIS2_PLACEMENT_3D('',#29333,#19384,#19385);
#16547=AXIS2_PLACEMENT_3D('',#29413,#19387,#19388);
#16548=AXIS2_PLACEMENT_3D('',#29445,#19390,#19391);
#16549=AXIS2_PLACEMENT_3D('',#30616,#19392,#19393);
#16550=AXIS2_PLACEMENT_3D('',#30618,#19394,#19395);
#16551=AXIS2_PLACEMENT_3D('',#30625,#19396,#19397);
#16552=AXIS2_PLACEMENT_3D('',#30627,#19398,#19399);
#16553=AXIS2_PLACEMENT_3D('',#30636,#19400,#19401);
#16554=AXIS2_PLACEMENT_3D('',#30638,#19402,#19403);
#16555=AXIS2_PLACEMENT_3D('',#30653,#19404,#19405);
#16556=AXIS2_PLACEMENT_3D('',#30655,#19406,#19407);
#16557=AXIS2_PLACEMENT_3D('',#30662,#19408,#19409);
#16558=AXIS2_PLACEMENT_3D('',#31931,#19410,#19411);
#16559=AXIS2_PLACEMENT_3D('',#31932,#19412,#19413);
#16560=AXIS2_PLACEMENT_3D('',#31933,#19414,#19415);
#16561=AXIS2_PLACEMENT_3D('',#31934,#19416,#19417);
#16562=AXIS2_PLACEMENT_3D('',#31935,#19418,#19419);
#16563=AXIS2_PLACEMENT_3D('',#31936,#19420,#19421);
#16564=AXIS2_PLACEMENT_3D('',#31937,#19422,#19423);
#16565=AXIS2_PLACEMENT_3D('',#31938,#19424,#19425);
#16566=AXIS2_PLACEMENT_3D('',#31939,#19426,#19427);
#16567=AXIS2_PLACEMENT_3D('',#33296,#19428,#19429);
#16568=AXIS2_PLACEMENT_3D('',#33297,#19430,#19431);
#16569=AXIS2_PLACEMENT_3D('',#33298,#19432,#19433);
#16570=AXIS2_PLACEMENT_3D('',#33299,#19434,#19435);
#16571=AXIS2_PLACEMENT_3D('',#33300,#19436,#19437);
#16572=AXIS2_PLACEMENT_3D('',#33301,#19438,#19439);
#16573=AXIS2_PLACEMENT_3D('',#33302,#19440,#19441);
#16574=AXIS2_PLACEMENT_3D('',#33303,#19442,#19443);
#16575=AXIS2_PLACEMENT_3D('',#33304,#19444,#19445);
#16576=AXIS2_PLACEMENT_3D('',#34487,#19446,#19447);
#16577=AXIS2_PLACEMENT_3D('',#34488,#19448,#19449);
#16578=AXIS2_PLACEMENT_3D('',#34489,#19450,#19451);
#16579=AXIS2_PLACEMENT_3D('',#34490,#19452,#19453);
#16580=AXIS2_PLACEMENT_3D('',#34491,#19454,#19455);
#16581=AXIS2_PLACEMENT_3D('',#34492,#19456,#19457);
#16582=AXIS2_PLACEMENT_3D('',#34493,#19458,#19459);
#16583=AXIS2_PLACEMENT_3D('',#34494,#19460,#19461);
#16584=AXIS2_PLACEMENT_3D('',#34495,#19462,#19463);
#16585=AXIS2_PLACEMENT_3D('',#35776,#19464,#19465);
#16586=AXIS2_PLACEMENT_3D('',#35777,#19466,#19467);
#16587=AXIS2_PLACEMENT_3D('',#35778,#19468,#19469);
#16588=AXIS2_PLACEMENT_3D('',#35779,#19470,#19471);
#16589=AXIS2_PLACEMENT_3D('',#35780,#19472,#19473);
#16590=AXIS2_PLACEMENT_3D('',#35781,#19474,#19475);
#16591=AXIS2_PLACEMENT_3D('',#35782,#19476,#19477);
#16592=AXIS2_PLACEMENT_3D('',#35783,#19478,#19479);
#16593=AXIS2_PLACEMENT_3D('',#35784,#19480,#19481);
#16594=AXIS2_PLACEMENT_3D('',#37059,#19482,#19483);
#16595=AXIS2_PLACEMENT_3D('',#37060,#19484,#19485);
#16596=AXIS2_PLACEMENT_3D('',#37061,#19486,#19487);
#16597=AXIS2_PLACEMENT_3D('',#37062,#19488,#19489);
#16598=AXIS2_PLACEMENT_3D('',#37063,#19490,#19491);
#16599=AXIS2_PLACEMENT_3D('',#37064,#19492,#19493);
#16600=AXIS2_PLACEMENT_3D('',#37065,#19494,#19495);
#16601=AXIS2_PLACEMENT_3D('',#37066,#19496,#19497);
#16602=AXIS2_PLACEMENT_3D('',#37067,#19498,#19499);
#16603=AXIS2_PLACEMENT_3D('',#38162,#19500,#19501);
#16604=AXIS2_PLACEMENT_3D('',#38163,#19502,#19503);
#16605=AXIS2_PLACEMENT_3D('',#38164,#19504,#19505);
#16606=AXIS2_PLACEMENT_3D('',#38165,#19506,#19507);
#16607=AXIS2_PLACEMENT_3D('',#38166,#19508,#19509);
#16608=AXIS2_PLACEMENT_3D('',#38167,#19510,#19511);
#16609=AXIS2_PLACEMENT_3D('',#38168,#19512,#19513);
#16610=AXIS2_PLACEMENT_3D('',#38169,#19514,#19515);
#16611=AXIS2_PLACEMENT_3D('',#38170,#19516,#19517);
#16612=AXIS2_PLACEMENT_3D('',#39239,#19518,#19519);
#16613=AXIS2_PLACEMENT_3D('',#39240,#19520,#19521);
#16614=AXIS2_PLACEMENT_3D('',#39241,#19522,#19523);
#16615=AXIS2_PLACEMENT_3D('',#39242,#19524,#19525);
#16616=AXIS2_PLACEMENT_3D('',#39243,#19526,#19527);
#16617=AXIS2_PLACEMENT_3D('',#39244,#19528,#19529);
#16618=AXIS2_PLACEMENT_3D('',#39245,#19530,#19531);
#16619=AXIS2_PLACEMENT_3D('',#39246,#19532,#19533);
#16620=AXIS2_PLACEMENT_3D('',#39247,#19534,#19535);
#16621=AXIS2_PLACEMENT_3D('',#40488,#19536,#19537);
#16622=AXIS2_PLACEMENT_3D('',#40489,#19538,#19539);
#16623=AXIS2_PLACEMENT_3D('',#40490,#19540,#19541);
#16624=AXIS2_PLACEMENT_3D('',#40491,#19542,#19543);
#16625=AXIS2_PLACEMENT_3D('',#40492,#19544,#19545);
#16626=AXIS2_PLACEMENT_3D('',#40493,#19546,#19547);
#16627=AXIS2_PLACEMENT_3D('',#40494,#19548,#19549);
#16628=AXIS2_PLACEMENT_3D('',#40495,#19550,#19551);
#16629=AXIS2_PLACEMENT_3D('',#40496,#19552,#19553);
#16630=AXIS2_PLACEMENT_3D('',#41589,#19554,#19555);
#16631=AXIS2_PLACEMENT_3D('',#41590,#19556,#19557);
#16632=AXIS2_PLACEMENT_3D('',#41591,#19558,#19559);
#16633=AXIS2_PLACEMENT_3D('',#41592,#19560,#19561);
#16634=AXIS2_PLACEMENT_3D('',#41593,#19562,#19563);
#16635=AXIS2_PLACEMENT_3D('',#41594,#19564,#19565);
#16636=AXIS2_PLACEMENT_3D('',#41595,#19566,#19567);
#16637=AXIS2_PLACEMENT_3D('',#41596,#19568,#19569);
#16638=AXIS2_PLACEMENT_3D('',#41597,#19570,#19571);
#16639=AXIS2_PLACEMENT_3D('',#42550,#19572,#19573);
#16640=AXIS2_PLACEMENT_3D('',#42551,#19574,#19575);
#16641=AXIS2_PLACEMENT_3D('',#42552,#19576,#19577);
#16642=AXIS2_PLACEMENT_3D('',#42553,#19578,#19579);
#16643=AXIS2_PLACEMENT_3D('',#42554,#19580,#19581);
#16644=AXIS2_PLACEMENT_3D('',#42555,#19582,#19583);
#16645=AXIS2_PLACEMENT_3D('',#42556,#19584,#19585);
#16646=AXIS2_PLACEMENT_3D('',#42557,#19586,#19587);
#16647=AXIS2_PLACEMENT_3D('',#42558,#19588,#19589);
#16648=AXIS2_PLACEMENT_3D('',#43585,#19590,#19591);
#16649=AXIS2_PLACEMENT_3D('',#43586,#19592,#19593);
#16650=AXIS2_PLACEMENT_3D('',#43587,#19594,#19595);
#16651=AXIS2_PLACEMENT_3D('',#43588,#19596,#19597);
#16652=AXIS2_PLACEMENT_3D('',#43589,#19598,#19599);
#16653=AXIS2_PLACEMENT_3D('',#43590,#19600,#19601);
#16654=AXIS2_PLACEMENT_3D('',#43591,#19602,#19603);
#16655=AXIS2_PLACEMENT_3D('',#43592,#19604,#19605);
#16656=AXIS2_PLACEMENT_3D('',#43593,#19606,#19607);
#16657=AXIS2_PLACEMENT_3D('',#44690,#19608,#19609);
#16658=AXIS2_PLACEMENT_3D('',#44691,#19610,#19611);
#16659=AXIS2_PLACEMENT_3D('',#44692,#19612,#19613);
#16660=AXIS2_PLACEMENT_3D('',#44693,#19614,#19615);
#16661=AXIS2_PLACEMENT_3D('',#44694,#19616,#19617);
#16662=AXIS2_PLACEMENT_3D('',#44695,#19618,#19619);
#16663=AXIS2_PLACEMENT_3D('',#44696,#19620,#19621);
#16664=AXIS2_PLACEMENT_3D('',#44697,#19622,#19623);
#16665=AXIS2_PLACEMENT_3D('',#44698,#19624,#19625);
#16666=AXIS2_PLACEMENT_3D('',#45633,#19626,#19627);
#16667=AXIS2_PLACEMENT_3D('',#45634,#19628,#19629);
#16668=AXIS2_PLACEMENT_3D('',#45635,#19630,#19631);
#16669=AXIS2_PLACEMENT_3D('',#45636,#19632,#19633);
#16670=AXIS2_PLACEMENT_3D('',#45637,#19634,#19635);
#16671=AXIS2_PLACEMENT_3D('',#45638,#19636,#19637);
#16672=AXIS2_PLACEMENT_3D('',#45639,#19638,#19639);
#16673=AXIS2_PLACEMENT_3D('',#45640,#19640,#19641);
#16674=AXIS2_PLACEMENT_3D('',#45641,#19642,#19643);
#16675=AXIS2_PLACEMENT_3D('',#46558,#19644,#19645);
#16676=AXIS2_PLACEMENT_3D('',#46559,#19646,#19647);
#16677=AXIS2_PLACEMENT_3D('',#46560,#19648,#19649);
#16678=AXIS2_PLACEMENT_3D('',#46561,#19650,#19651);
#16679=AXIS2_PLACEMENT_3D('',#46562,#19652,#19653);
#16680=AXIS2_PLACEMENT_3D('',#46563,#19654,#19655);
#16681=AXIS2_PLACEMENT_3D('',#46564,#19656,#19657);
#16682=AXIS2_PLACEMENT_3D('',#46565,#19658,#19659);
#16683=AXIS2_PLACEMENT_3D('',#46566,#19660,#19661);
#16684=AXIS2_PLACEMENT_3D('',#47583,#19662,#19663);
#16685=AXIS2_PLACEMENT_3D('',#47584,#19664,#19665);
#16686=AXIS2_PLACEMENT_3D('',#47585,#19666,#19667);
#16687=AXIS2_PLACEMENT_3D('',#47586,#19668,#19669);
#16688=AXIS2_PLACEMENT_3D('',#47587,#19670,#19671);
#16689=AXIS2_PLACEMENT_3D('',#47588,#19672,#19673);
#16690=AXIS2_PLACEMENT_3D('',#47589,#19674,#19675);
#16691=AXIS2_PLACEMENT_3D('',#47590,#19676,#19677);
#16692=AXIS2_PLACEMENT_3D('',#47591,#19678,#19679);
#16693=AXIS2_PLACEMENT_3D('',#48524,#19680,#19681);
#16694=AXIS2_PLACEMENT_3D('',#48525,#19682,#19683);
#16695=AXIS2_PLACEMENT_3D('',#48526,#19684,#19685);
#16696=AXIS2_PLACEMENT_3D('',#48527,#19686,#19687);
#16697=AXIS2_PLACEMENT_3D('',#48528,#19688,#19689);
#16698=AXIS2_PLACEMENT_3D('',#48529,#19690,#19691);
#16699=AXIS2_PLACEMENT_3D('',#48530,#19692,#19693);
#16700=AXIS2_PLACEMENT_3D('',#48531,#19694,#19695);
#16701=AXIS2_PLACEMENT_3D('',#48532,#19696,#19697);
#16702=AXIS2_PLACEMENT_3D('',#49577,#19698,#19699);
#16703=AXIS2_PLACEMENT_3D('',#49578,#19700,#19701);
#16704=AXIS2_PLACEMENT_3D('',#49579,#19702,#19703);
#16705=AXIS2_PLACEMENT_3D('',#49580,#19704,#19705);
#16706=AXIS2_PLACEMENT_3D('',#49581,#19706,#19707);
#16707=AXIS2_PLACEMENT_3D('',#49582,#19708,#19709);
#16708=AXIS2_PLACEMENT_3D('',#49583,#19710,#19711);
#16709=AXIS2_PLACEMENT_3D('',#49584,#19712,#19713);
#16710=AXIS2_PLACEMENT_3D('',#49585,#19714,#19715);
#16711=AXIS2_PLACEMENT_3D('',#50544,#19716,#19717);
#16712=AXIS2_PLACEMENT_3D('',#50545,#19718,#19719);
#16713=AXIS2_PLACEMENT_3D('',#50546,#19720,#19721);
#16714=AXIS2_PLACEMENT_3D('',#50547,#19722,#19723);
#16715=AXIS2_PLACEMENT_3D('',#50548,#19724,#19725);
#16716=AXIS2_PLACEMENT_3D('',#50549,#19726,#19727);
#16717=AXIS2_PLACEMENT_3D('',#50550,#19728,#19729);
#16718=AXIS2_PLACEMENT_3D('',#50551,#19730,#19731);
#16719=AXIS2_PLACEMENT_3D('',#50552,#19732,#19733);
#16720=AXIS2_PLACEMENT_3D('',#51493,#19734,#19735);
#16721=AXIS2_PLACEMENT_3D('',#51494,#19736,#19737);
#16722=AXIS2_PLACEMENT_3D('',#51495,#19738,#19739);
#16723=AXIS2_PLACEMENT_3D('',#51496,#19740,#19741);
#16724=AXIS2_PLACEMENT_3D('',#51497,#19742,#19743);
#16725=AXIS2_PLACEMENT_3D('',#51498,#19744,#19745);
#16726=AXIS2_PLACEMENT_3D('',#51499,#19746,#19747);
#16727=AXIS2_PLACEMENT_3D('',#51500,#19748,#19749);
#16728=AXIS2_PLACEMENT_3D('',#51501,#19750,#19751);
#16729=AXIS2_PLACEMENT_3D('',#52712,#19752,#19753);
#16730=AXIS2_PLACEMENT_3D('',#52713,#19754,#19755);
#16731=AXIS2_PLACEMENT_3D('',#52714,#19756,#19757);
#16732=AXIS2_PLACEMENT_3D('',#52715,#19758,#19759);
#16733=AXIS2_PLACEMENT_3D('',#52716,#19760,#19761);
#16734=AXIS2_PLACEMENT_3D('',#52717,#19762,#19763);
#16735=AXIS2_PLACEMENT_3D('',#52718,#19764,#19765);
#16736=AXIS2_PLACEMENT_3D('',#52719,#19766,#19767);
#16737=AXIS2_PLACEMENT_3D('',#52720,#19768,#19769);
#16738=AXIS2_PLACEMENT_3D('',#53757,#19770,#19771);
#16739=AXIS2_PLACEMENT_3D('',#53758,#19772,#19773);
#16740=AXIS2_PLACEMENT_3D('',#53759,#19774,#19775);
#16741=AXIS2_PLACEMENT_3D('',#53760,#19776,#19777);
#16742=AXIS2_PLACEMENT_3D('',#53761,#19778,#19779);
#16743=AXIS2_PLACEMENT_3D('',#53762,#19780,#19781);
#16744=AXIS2_PLACEMENT_3D('',#53763,#19782,#19783);
#16745=AXIS2_PLACEMENT_3D('',#53764,#19784,#19785);
#16746=AXIS2_PLACEMENT_3D('',#53765,#19786,#19787);
#16747=AXIS2_PLACEMENT_3D('',#54808,#19788,#19789);
#16748=AXIS2_PLACEMENT_3D('',#54809,#19790,#19791);
#16749=AXIS2_PLACEMENT_3D('',#54810,#19792,#19793);
#16750=AXIS2_PLACEMENT_3D('',#54811,#19794,#19795);
#16751=AXIS2_PLACEMENT_3D('',#54812,#19796,#19797);
#16752=AXIS2_PLACEMENT_3D('',#54813,#19798,#19799);
#16753=AXIS2_PLACEMENT_3D('',#54814,#19800,#19801);
#16754=AXIS2_PLACEMENT_3D('',#54815,#19802,#19803);
#16755=AXIS2_PLACEMENT_3D('',#54816,#19804,#19805);
#16756=AXIS2_PLACEMENT_3D('',#55887,#19806,#19807);
#16757=AXIS2_PLACEMENT_3D('',#55888,#19808,#19809);
#16758=AXIS2_PLACEMENT_3D('',#55889,#19810,#19811);
#16759=AXIS2_PLACEMENT_3D('',#55890,#19812,#19813);
#16760=AXIS2_PLACEMENT_3D('',#55891,#19814,#19815);
#16761=AXIS2_PLACEMENT_3D('',#55892,#19816,#19817);
#16762=AXIS2_PLACEMENT_3D('',#55893,#19818,#19819);
#16763=AXIS2_PLACEMENT_3D('',#55894,#19820,#19821);
#16764=AXIS2_PLACEMENT_3D('',#55895,#19822,#19823);
#16765=AXIS2_PLACEMENT_3D('',#57234,#19824,#19825);
#16766=AXIS2_PLACEMENT_3D('',#57235,#19826,#19827);
#16767=AXIS2_PLACEMENT_3D('',#57236,#19828,#19829);
#16768=AXIS2_PLACEMENT_3D('',#57237,#19830,#19831);
#16769=AXIS2_PLACEMENT_3D('',#57238,#19832,#19833);
#16770=AXIS2_PLACEMENT_3D('',#57239,#19834,#19835);
#16771=AXIS2_PLACEMENT_3D('',#57240,#19836,#19837);
#16772=AXIS2_PLACEMENT_3D('',#57241,#19838,#19839);
#16773=AXIS2_PLACEMENT_3D('',#57242,#19840,#19841);
#16774=AXIS2_PLACEMENT_3D('',#58291,#19842,#19843);
#16775=AXIS2_PLACEMENT_3D('',#58292,#19844,#19845);
#16776=AXIS2_PLACEMENT_3D('',#58293,#19846,#19847);
#16777=AXIS2_PLACEMENT_3D('',#58294,#19848,#19849);
#16778=AXIS2_PLACEMENT_3D('',#58295,#19850,#19851);
#16779=AXIS2_PLACEMENT_3D('',#58296,#19852,#19853);
#16780=AXIS2_PLACEMENT_3D('',#58297,#19854,#19855);
#16781=AXIS2_PLACEMENT_3D('',#58298,#19856,#19857);
#16782=AXIS2_PLACEMENT_3D('',#58299,#19858,#19859);
#16783=AXIS2_PLACEMENT_3D('',#59644,#19860,#19861);
#16784=AXIS2_PLACEMENT_3D('',#59645,#19862,#19863);
#16785=AXIS2_PLACEMENT_3D('',#59646,#19864,#19865);
#16786=AXIS2_PLACEMENT_3D('',#59647,#19866,#19867);
#16787=AXIS2_PLACEMENT_3D('',#59648,#19868,#19869);
#16788=AXIS2_PLACEMENT_3D('',#59649,#19870,#19871);
#16789=AXIS2_PLACEMENT_3D('',#59650,#19872,#19873);
#16790=AXIS2_PLACEMENT_3D('',#59651,#19874,#19875);
#16791=AXIS2_PLACEMENT_3D('',#59652,#19876,#19877);
#16792=AXIS2_PLACEMENT_3D('',#60751,#19878,#19879);
#16793=AXIS2_PLACEMENT_3D('',#60752,#19880,#19881);
#16794=AXIS2_PLACEMENT_3D('',#60753,#19882,#19883);
#16795=AXIS2_PLACEMENT_3D('',#60765,#19884,#19885);
#16796=AXIS2_PLACEMENT_3D('',#60766,#19886,#19887);
#16797=AXIS2_PLACEMENT_3D('',#60767,#19888,#19889);
#16798=AXIS2_PLACEMENT_3D('',#60768,#19890,#19891);
#16799=AXIS2_PLACEMENT_3D('',#60769,#19892,#19893);
#16800=AXIS2_PLACEMENT_3D('',#60770,#19894,#19895);
#16801=AXIS2_PLACEMENT_3D('',#60771,#19896,#19897);
#16802=AXIS2_PLACEMENT_3D('',#60772,#19898,#19899);
#16803=AXIS2_PLACEMENT_3D('',#62084,#19900,#19901);
#16804=AXIS2_PLACEMENT_3D('',#62092,#19902,#19903);
#16805=AXIS2_PLACEMENT_3D('',#62093,#19904,#19905);
#16806=AXIS2_PLACEMENT_3D('',#62094,#19906,#19907);
#16807=AXIS2_PLACEMENT_3D('',#62095,#19908,#19909);
#16808=AXIS2_PLACEMENT_3D('',#62103,#19910,#19911);
#16809=AXIS2_PLACEMENT_3D('',#62104,#19912,#19913);
#16810=AXIS2_PLACEMENT_3D('',#62105,#19914,#19915);
#16811=AXIS2_PLACEMENT_3D('',#62106,#19916,#19917);
#16812=AXIS2_PLACEMENT_3D('',#62107,#19918,#19919);
#16813=AXIS2_PLACEMENT_3D('',#62108,#19920,#19921);
#16814=AXIS2_PLACEMENT_3D('',#63077,#19922,#19923);
#16815=AXIS2_PLACEMENT_3D('',#63078,#19924,#19925);
#16816=AXIS2_PLACEMENT_3D('',#63079,#19926,#19927);
#16817=AXIS2_PLACEMENT_3D('',#63080,#19928,#19929);
#16818=AXIS2_PLACEMENT_3D('',#63081,#19930,#19931);
#16819=AXIS2_PLACEMENT_3D('',#63082,#19932,#19933);
#16820=AXIS2_PLACEMENT_3D('',#63083,#19934,#19935);
#16821=AXIS2_PLACEMENT_3D('',#63100,#19940,#19941);
#16822=AXIS2_PLACEMENT_3D('',#63106,#19945,#19946);
#16823=AXIS2_PLACEMENT_3D('',#63120,#19950,#19951);
#16824=AXIS2_PLACEMENT_3D('',#63122,#19952,#19953);
#16825=AXIS2_PLACEMENT_3D('',#63123,#19954,#19955);
#16826=AXIS2_PLACEMENT_3D('',#63124,#19956,#19957);
#16827=AXIS2_PLACEMENT_3D('',#63125,#19958,#19959);
#16828=AXIS2_PLACEMENT_3D('',#63126,#19960,#19961);
#16829=AXIS2_PLACEMENT_3D('',#63128,#19962,#19963);
#16830=AXIS2_PLACEMENT_3D('',#63130,#19965,#19966);
#16831=AXIS2_PLACEMENT_3D('',#63132,#19967,#19968);
#16832=AXIS2_PLACEMENT_3D('',#63134,#19970,#19971);
#16833=AXIS2_PLACEMENT_3D('',#63136,#19972,#19973);
#16834=AXIS2_PLACEMENT_3D('',#63137,#19974,#19975);
#16835=AXIS2_PLACEMENT_3D('',#63139,#19976,#19977);
#16836=AXIS2_PLACEMENT_3D('',#63141,#19979,#19980);
#16837=AXIS2_PLACEMENT_3D('',#63143,#19981,#19982);
#16838=AXIS2_PLACEMENT_3D('',#63145,#19984,#19985);
#16839=AXIS2_PLACEMENT_3D('',#63147,#19986,#19987);
#16840=AXIS2_PLACEMENT_3D('',#63148,#19988,#19989);
#16841=AXIS2_PLACEMENT_3D('',#63150,#19990,#19991);
#16842=AXIS2_PLACEMENT_3D('',#63152,#19993,#19994);
#16843=AXIS2_PLACEMENT_3D('',#63154,#19995,#19996);
#16844=AXIS2_PLACEMENT_3D('',#63155,#19997,#19998);
#16845=AXIS2_PLACEMENT_3D('',#63157,#19999,#20000);
#16846=AXIS2_PLACEMENT_3D('',#63159,#20002,#20003);
#16847=AXIS2_PLACEMENT_3D('',#63162,#20005,#20006);
#16848=AXIS2_PLACEMENT_3D('',#63163,#20007,#20008);
#16849=AXIS2_PLACEMENT_3D('',#63165,#20009,#20010);
#16850=AXIS2_PLACEMENT_3D('',#63166,#20011,#20012);
#16851=AXIS2_PLACEMENT_3D('',#63168,#20013,#20014);
#16852=AXIS2_PLACEMENT_3D('',#63170,#20016,#20017);
#16853=AXIS2_PLACEMENT_3D('',#63173,#20019,#20020);
#16854=AXIS2_PLACEMENT_3D('',#63174,#20021,#20022);
#16855=AXIS2_PLACEMENT_3D('',#63175,#20023,#20024);
#16856=AXIS2_PLACEMENT_3D('',#63176,#20025,#20026);
#16857=AXIS2_PLACEMENT_3D('',#63177,#20027,#20028);
#16858=AXIS2_PLACEMENT_3D('',#63178,#20029,#20030);
#16859=AXIS2_PLACEMENT_3D('',#63179,#20031,#20032);
#16860=AXIS2_PLACEMENT_3D('',#63180,#20033,#20034);
#16861=AXIS2_PLACEMENT_3D('',#63182,#20035,#20036);
#16862=AXIS2_PLACEMENT_3D('',#63184,#20037,#20038);
#16863=AXIS2_PLACEMENT_3D('',#63185,#20039,#20040);
#16864=AXIS2_PLACEMENT_3D('',#63187,#20041,#20042);
#16865=AXIS2_PLACEMENT_3D('',#63189,#20044,#20045);
#16866=AXIS2_PLACEMENT_3D('',#63191,#20046,#20047);
#16867=AXIS2_PLACEMENT_3D('',#63193,#20049,#20050);
#16868=AXIS2_PLACEMENT_3D('',#63196,#20052,#20053);
#16869=AXIS2_PLACEMENT_3D('',#63197,#20054,#20055);
#16870=AXIS2_PLACEMENT_3D('',#63199,#20056,#20057);
#16871=AXIS2_PLACEMENT_3D('',#63200,#20058,#20059);
#16872=AXIS2_PLACEMENT_3D('',#63202,#20060,#20061);
#16873=AXIS2_PLACEMENT_3D('',#63204,#20063,#20064);
#16874=AXIS2_PLACEMENT_3D('',#63206,#20065,#20066);
#16875=AXIS2_PLACEMENT_3D('',#63207,#20067,#20068);
#16876=AXIS2_PLACEMENT_3D('',#63209,#20069,#20070);
#16877=AXIS2_PLACEMENT_3D('',#63211,#20072,#20073);
#16878=AXIS2_PLACEMENT_3D('',#63213,#20074,#20075);
#16879=AXIS2_PLACEMENT_3D('',#63215,#20077,#20078);
#16880=AXIS2_PLACEMENT_3D('',#63218,#20080,#20081);
#16881=AXIS2_PLACEMENT_3D('',#63219,#20082,#20083);
#16882=AXIS2_PLACEMENT_3D('',#63221,#20085,#20086);
#16883=AXIS2_PLACEMENT_3D('',#63222,#20087,#20088);
#16884=AXIS2_PLACEMENT_3D('',#63224,#20089,#20090);
#16885=AXIS2_PLACEMENT_3D('',#63227,#20092,#20093);
#16886=AXIS2_PLACEMENT_3D('',#63228,#20094,#20095);
#16887=AXIS2_PLACEMENT_3D('',#63230,#20096,#20097);
#16888=AXIS2_PLACEMENT_3D('',#63231,#20098,#20099);
#16889=AXIS2_PLACEMENT_3D('',#63234,#20101,#20102);
#16890=AXIS2_PLACEMENT_3D('',#63235,#20103,#20104);
#16891=AXIS2_PLACEMENT_3D('',#63237,#20105,#20106);
#16892=AXIS2_PLACEMENT_3D('',#63238,#20107,#20108);
#16893=AXIS2_PLACEMENT_3D('',#63240,#20109,#20110);
#16894=AXIS2_PLACEMENT_3D('',#63243,#20112,#20113);
#16895=AXIS2_PLACEMENT_3D('',#63244,#20114,#20115);
#16896=AXIS2_PLACEMENT_3D('',#63246,#20116,#20117);
#16897=AXIS2_PLACEMENT_3D('',#63247,#20118,#20119);
#16898=AXIS2_PLACEMENT_3D('',#63249,#20120,#20121);
#16899=AXIS2_PLACEMENT_3D('',#63251,#20123,#20124);
#16900=AXIS2_PLACEMENT_3D('',#63253,#20126,#20127);
#16901=AXIS2_PLACEMENT_3D('',#63254,#20128,#20129);
#16902=AXIS2_PLACEMENT_3D('',#63255,#20130,#20131);
#16903=AXIS2_PLACEMENT_3D('',#63256,#20132,#20133);
#16904=AXIS2_PLACEMENT_3D('',#63341,#20135,#20136);
#16905=AXIS2_PLACEMENT_3D('',#63397,#20137,#20138);
#16906=AXIS2_PLACEMENT_3D('',#63674,#20140,#20141);
#16907=AXIS2_PLACEMENT_3D('',#63954,#20143,#20144);
#16908=AXIS2_PLACEMENT_3D('',#64231,#20146,#20147);
#16909=AXIS2_PLACEMENT_3D('',#64511,#20149,#20150);
#16910=AXIS2_PLACEMENT_3D('',#64788,#20152,#20153);
#16911=AXIS2_PLACEMENT_3D('',#64838,#20154,#20155);
#16912=AXIS2_PLACEMENT_3D('',#65179,#20156,#20157);
#16913=AXIS2_PLACEMENT_3D('',#65369,#20158,#20159);
#16914=AXIS2_PLACEMENT_3D('',#65474,#20160,#20161);
#16915=AXIS2_PLACEMENT_3D('',#65556,#20162,#20163);
#16916=AXIS2_PLACEMENT_3D('',#65563,#20164,#20165);
#16917=AXIS2_PLACEMENT_3D('',#65890,#20166,#20167);
#16918=AXIS2_PLACEMENT_3D('',#65892,#20168,#20169);
#16919=AXIS2_PLACEMENT_3D('',#65894,#20170,#20171);
#16920=AXIS2_PLACEMENT_3D('',#66216,#20172,#20173);
#16921=AXIS2_PLACEMENT_3D('',#66247,#20175,#20176);
#16922=AXIS2_PLACEMENT_3D('',#66248,#20177,#20178);
#16923=AXIS2_PLACEMENT_3D('',#66254,#20182,#20183);
#16924=AXIS2_PLACEMENT_3D('',#66258,#20186,#20187);
#16925=AXIS2_PLACEMENT_3D('',#66262,#20190,#20191);
#16926=AXIS2_PLACEMENT_3D('',#66266,#20193,#20194);
#16927=AXIS2_PLACEMENT_3D('',#66267,#20195,#20196);
#16928=AXIS2_PLACEMENT_3D('',#66271,#20199,#20200);
#16929=AXIS2_PLACEMENT_3D('',#66275,#20203,#20204);
#16930=AXIS2_PLACEMENT_3D('',#66277,#20206,#20207);
#16931=AXIS2_PLACEMENT_3D('',#66278,#20208,#20209);
#16932=AXIS2_PLACEMENT_3D('',#66280,#20210,#20211);
#16933=AXIS2_PLACEMENT_3D('',#66281,#20212,#20213);
#16934=AXIS2_PLACEMENT_3D('',#66283,#20215,#20216);
#16935=AXIS2_PLACEMENT_3D('',#66285,#20217,#20218);
#16936=AXIS2_PLACEMENT_3D('',#66286,#20219,#20220);
#16937=AXIS2_PLACEMENT_3D('',#66287,#20221,#20222);
#16938=AXIS2_PLACEMENT_3D('',#66289,#20223,#20224);
#16939=AXIS2_PLACEMENT_3D('',#66291,#20226,#20227);
#16940=AXIS2_PLACEMENT_3D('',#66293,#20228,#20229);
#16941=AXIS2_PLACEMENT_3D('',#66294,#20230,#20231);
#16942=AXIS2_PLACEMENT_3D('',#66296,#20232,#20233);
#16943=AXIS2_PLACEMENT_3D('',#66298,#20235,#20236);
#16944=AXIS2_PLACEMENT_3D('',#66300,#20237,#20238);
#16945=AXIS2_PLACEMENT_3D('',#66302,#20240,#20241);
#16946=AXIS2_PLACEMENT_3D('',#66305,#20243,#20244);
#16947=AXIS2_PLACEMENT_3D('',#66306,#20245,#20246);
#16948=AXIS2_PLACEMENT_3D('',#66307,#20247,#20248);
#16949=AXIS2_PLACEMENT_3D('',#66308,#20249,#20250);
#16950=AXIS2_PLACEMENT_3D('',#66310,#20251,#20252);
#16951=AXIS2_PLACEMENT_3D('',#66313,#20254,#20255);
#16952=AXIS2_PLACEMENT_3D('',#66314,#20256,#20257);
#16953=AXIS2_PLACEMENT_3D('',#66316,#20258,#20259);
#16954=AXIS2_PLACEMENT_3D('',#66317,#20260,#20261);
#16955=AXIS2_PLACEMENT_3D('',#66319,#20262,#20263);
#16956=AXIS2_PLACEMENT_3D('',#66321,#20265,#20266);
#16957=AXIS2_PLACEMENT_3D('',#66323,#20267,#20268);
#16958=AXIS2_PLACEMENT_3D('',#66325,#20270,#20271);
#16959=AXIS2_PLACEMENT_3D('',#66328,#20273,#20274);
#16960=AXIS2_PLACEMENT_3D('',#66329,#20275,#20276);
#16961=AXIS2_PLACEMENT_3D('',#66331,#20277,#20278);
#16962=AXIS2_PLACEMENT_3D('',#66332,#20279,#20280);
#16963=AXIS2_PLACEMENT_3D('',#66334,#20281,#20282);
#16964=AXIS2_PLACEMENT_3D('',#66336,#20284,#20285);
#16965=AXIS2_PLACEMENT_3D('',#66338,#20287,#20288);
#16966=AXIS2_PLACEMENT_3D('',#66339,#20289,#20290);
#16967=AXIS2_PLACEMENT_3D('',#66341,#20291,#20292);
#16968=AXIS2_PLACEMENT_3D('',#66344,#20294,#20295);
#16969=AXIS2_PLACEMENT_3D('',#66345,#20296,#20297);
#16970=AXIS2_PLACEMENT_3D('',#66347,#20298,#20299);
#16971=AXIS2_PLACEMENT_3D('',#66348,#20300,#20301);
#16972=AXIS2_PLACEMENT_3D('',#66350,#20302,#20303);
#16973=AXIS2_PLACEMENT_3D('',#66352,#20305,#20306);
#16974=AXIS2_PLACEMENT_3D('',#66354,#20307,#20308);
#16975=AXIS2_PLACEMENT_3D('',#66356,#20310,#20311);
#16976=AXIS2_PLACEMENT_3D('',#66358,#20312,#20313);
#16977=AXIS2_PLACEMENT_3D('',#66359,#20314,#20315);
#16978=AXIS2_PLACEMENT_3D('',#66361,#20316,#20317);
#16979=AXIS2_PLACEMENT_3D('',#66363,#20319,#20320);
#16980=AXIS2_PLACEMENT_3D('',#66365,#20321,#20322);
#16981=AXIS2_PLACEMENT_3D('',#66367,#20324,#20325);
#16982=AXIS2_PLACEMENT_3D('',#66370,#20327,#20328);
#16983=AXIS2_PLACEMENT_3D('',#66371,#20329,#20330);
#16984=AXIS2_PLACEMENT_3D('',#66372,#20331,#20332);
#16985=AXIS2_PLACEMENT_3D('',#66373,#20333,#20334);
#16986=AXIS2_PLACEMENT_3D('',#66374,#20335,#20336);
#16987=AXIS2_PLACEMENT_3D('',#66376,#20337,#20338);
#16988=AXIS2_PLACEMENT_3D('',#66379,#20340,#20341);
#16989=AXIS2_PLACEMENT_3D('',#66380,#20342,#20343);
#16990=AXIS2_PLACEMENT_3D('',#66382,#20344,#20345);
#16991=AXIS2_PLACEMENT_3D('',#66385,#20347,#20348);
#16992=AXIS2_PLACEMENT_3D('',#66386,#20349,#20350);
#16993=AXIS2_PLACEMENT_3D('',#66387,#20351,#20352);
#16994=AXIS2_PLACEMENT_3D('',#66389,#20353,#20354);
#16995=AXIS2_PLACEMENT_3D('',#66392,#20356,#20357);
#16996=AXIS2_PLACEMENT_3D('',#66393,#20358,#20359);
#16997=AXIS2_PLACEMENT_3D('',#66395,#20360,#20361);
#16998=AXIS2_PLACEMENT_3D('',#66396,#20362,#20363);
#16999=AXIS2_PLACEMENT_3D('',#66399,#20365,#20366);
#17000=AXIS2_PLACEMENT_3D('',#66400,#20367,#20368);
#17001=AXIS2_PLACEMENT_3D('',#66402,#20369,#20370);
#17002=AXIS2_PLACEMENT_3D('',#66403,#20371,#20372);
#17003=AXIS2_PLACEMENT_3D('',#66405,#20373,#20374);
#17004=AXIS2_PLACEMENT_3D('',#66406,#20375,#20376);
#17005=AXIS2_PLACEMENT_3D('',#66408,#20377,#20378);
#17006=AXIS2_PLACEMENT_3D('',#66411,#20380,#20381);
#17007=AXIS2_PLACEMENT_3D('',#66412,#20382,#20383);
#17008=AXIS2_PLACEMENT_3D('',#66415,#20385,#20386);
#17009=AXIS2_PLACEMENT_3D('',#66416,#20387,#20388);
#17010=AXIS2_PLACEMENT_3D('',#66418,#20389,#20390);
#17011=AXIS2_PLACEMENT_3D('',#66419,#20391,#20392);
#17012=AXIS2_PLACEMENT_3D('',#66422,#20394,#20395);
#17013=AXIS2_PLACEMENT_3D('',#66423,#20396,#20397);
#17014=AXIS2_PLACEMENT_3D('',#66426,#20399,#20400);
#17015=AXIS2_PLACEMENT_3D('',#66427,#20401,#20402);
#17016=AXIS2_PLACEMENT_3D('',#66428,#20403,#20404);
#17017=AXIS2_PLACEMENT_3D('',#66430,#20405,#20406);
#17018=AXIS2_PLACEMENT_3D('',#66432,#20408,#20409);
#17019=AXIS2_PLACEMENT_3D('',#66434,#20410,#20411);
#17020=AXIS2_PLACEMENT_3D('',#66436,#20413,#20414);
#17021=AXIS2_PLACEMENT_3D('',#66439,#20416,#20417);
#17022=AXIS2_PLACEMENT_3D('',#66440,#20418,#20419);
#17023=AXIS2_PLACEMENT_3D('',#66442,#20420,#20421);
#17024=AXIS2_PLACEMENT_3D('',#66443,#20422,#20423);
#17025=AXIS2_PLACEMENT_3D('',#66445,#20425,#20426);
#17026=AXIS2_PLACEMENT_3D('',#66447,#20427,#20428);
#17027=AXIS2_PLACEMENT_3D('',#66448,#20429,#20430);
#17028=AXIS2_PLACEMENT_3D('',#66450,#20432,#20433);
#17029=AXIS2_PLACEMENT_3D('',#66451,#20434,#20435);
#17030=AXIS2_PLACEMENT_3D('',#66453,#20436,#20437);
#17031=AXIS2_PLACEMENT_3D('',#66456,#20439,#20440);
#17032=AXIS2_PLACEMENT_3D('',#66457,#20441,#20442);
#17033=AXIS2_PLACEMENT_3D('',#66460,#20444,#20445);
#17034=AXIS2_PLACEMENT_3D('',#66461,#20446,#20447);
#17035=AXIS2_PLACEMENT_3D('',#66463,#20448,#20449);
#17036=AXIS2_PLACEMENT_3D('',#66464,#20450,#20451);
#17037=AXIS2_PLACEMENT_3D('',#66466,#20452,#20453);
#17038=AXIS2_PLACEMENT_3D('',#66468,#20455,#20456);
#17039=AXIS2_PLACEMENT_3D('',#66470,#20457,#20458);
#17040=AXIS2_PLACEMENT_3D('',#66471,#20459,#20460);
#17041=AXIS2_PLACEMENT_3D('',#66473,#20461,#20462);
#17042=AXIS2_PLACEMENT_3D('',#66475,#20464,#20465);
#17043=AXIS2_PLACEMENT_3D('',#66477,#20466,#20467);
#17044=AXIS2_PLACEMENT_3D('',#66478,#20468,#20469);
#17045=AXIS2_PLACEMENT_3D('',#66480,#20470,#20471);
#17046=AXIS2_PLACEMENT_3D('',#66482,#20473,#20474);
#17047=AXIS2_PLACEMENT_3D('',#66484,#20475,#20476);
#17048=AXIS2_PLACEMENT_3D('',#66486,#20478,#20479);
#17049=AXIS2_PLACEMENT_3D('',#66489,#20481,#20482);
#17050=AXIS2_PLACEMENT_3D('',#66490,#20483,#20484);
#17051=AXIS2_PLACEMENT_3D('',#66492,#20485,#20486);
#17052=AXIS2_PLACEMENT_3D('',#66493,#20487,#20488);
#17053=AXIS2_PLACEMENT_3D('',#66495,#20489,#20490);
#17054=AXIS2_PLACEMENT_3D('',#66497,#20492,#20493);
#17055=AXIS2_PLACEMENT_3D('',#66499,#20494,#20495);
#17056=AXIS2_PLACEMENT_3D('',#66500,#20496,#20497);
#17057=AXIS2_PLACEMENT_3D('',#66502,#20498,#20499);
#17058=AXIS2_PLACEMENT_3D('',#66504,#20501,#20502);
#17059=AXIS2_PLACEMENT_3D('',#66506,#20503,#20504);
#17060=AXIS2_PLACEMENT_3D('',#66507,#20505,#20506);
#17061=AXIS2_PLACEMENT_3D('',#66509,#20508,#20509);
#17062=AXIS2_PLACEMENT_3D('',#66510,#20510,#20511);
#17063=AXIS2_PLACEMENT_3D('',#66512,#20512,#20513);
#17064=AXIS2_PLACEMENT_3D('',#66514,#20514,#20515);
#17065=AXIS2_PLACEMENT_3D('',#66515,#20516,#20517);
#17066=AXIS2_PLACEMENT_3D('',#66517,#20518,#20519);
#17067=AXIS2_PLACEMENT_3D('',#66519,#20521,#20522);
#17068=AXIS2_PLACEMENT_3D('',#66521,#20523,#20524);
#17069=AXIS2_PLACEMENT_3D('',#66523,#20526,#20527);
#17070=AXIS2_PLACEMENT_3D('',#66526,#20529,#20530);
#17071=AXIS2_PLACEMENT_3D('',#66527,#20531,#20532);
#17072=AXIS2_PLACEMENT_3D('',#66529,#20533,#20534);
#17073=AXIS2_PLACEMENT_3D('',#66530,#20535,#20536);
#17074=AXIS2_PLACEMENT_3D('',#66532,#20537,#20538);
#17075=AXIS2_PLACEMENT_3D('',#66534,#20540,#20541);
#17076=AXIS2_PLACEMENT_3D('',#66536,#20542,#20543);
#17077=AXIS2_PLACEMENT_3D('',#66537,#20544,#20545);
#17078=AXIS2_PLACEMENT_3D('',#66539,#20546,#20547);
#17079=AXIS2_PLACEMENT_3D('',#66541,#20549,#20550);
#17080=AXIS2_PLACEMENT_3D('',#66543,#20551,#20552);
#17081=AXIS2_PLACEMENT_3D('',#66545,#20554,#20555);
#17082=AXIS2_PLACEMENT_3D('',#66548,#20557,#20558);
#17083=AXIS2_PLACEMENT_3D('',#66549,#20559,#20560);
#17084=AXIS2_PLACEMENT_3D('',#66551,#20562,#20563);
#17085=AXIS2_PLACEMENT_3D('',#66552,#20564,#20565);
#17086=AXIS2_PLACEMENT_3D('',#66554,#20566,#20567);
#17087=AXIS2_PLACEMENT_3D('',#66557,#20569,#20570);
#17088=AXIS2_PLACEMENT_3D('',#66558,#20571,#20572);
#17089=AXIS2_PLACEMENT_3D('',#66561,#20574,#20575);
#17090=AXIS2_PLACEMENT_3D('',#66562,#20576,#20577);
#17091=AXIS2_PLACEMENT_3D('',#66567,#20579,#20580);
#17092=AXIS2_PLACEMENT_3D('',#66571,#20582,#20583);
#17093=AXIS2_PLACEMENT_3D('',#66573,#20584,#20585);
#17094=AXIS2_PLACEMENT_3D('',#66575,#20586,#20587);
#17095=AXIS2_PLACEMENT_3D('',#66577,#20588,#20589);
#17096=AXIS2_PLACEMENT_3D('',#66578,#20590,#20591);
#17097=AXIS2_PLACEMENT_3D('',#66580,#20592,#20593);
#17098=AXIS2_PLACEMENT_3D('',#66581,#20594,#20595);
#17099=AXIS2_PLACEMENT_3D('',#66584,#20597,#20598);
#17100=AXIS2_PLACEMENT_3D('',#66585,#20599,#20600);
#17101=AXIS2_PLACEMENT_3D('',#66590,#20602,#20603);
#17102=AXIS2_PLACEMENT_3D('',#66592,#20604,#20605);
#17103=AXIS2_PLACEMENT_3D('',#66594,#20606,#20607);
#17104=AXIS2_PLACEMENT_3D('',#66596,#20608,#20609);
#17105=AXIS2_PLACEMENT_3D('',#66598,#20610,#20611);
#17106=AXIS2_PLACEMENT_3D('',#66601,#20613,#20614);
#17107=AXIS2_PLACEMENT_3D('',#66603,#20615,#20616);
#17108=AXIS2_PLACEMENT_3D('',#66604,#20617,#20618);
#17109=AXIS2_PLACEMENT_3D('',#66606,#20619,#20620);
#17110=AXIS2_PLACEMENT_3D('',#66608,#20622,#20623);
#17111=AXIS2_PLACEMENT_3D('',#66611,#20625,#20626);
#17112=AXIS2_PLACEMENT_3D('',#66612,#20627,#20628);
#17113=AXIS2_PLACEMENT_3D('',#66614,#20630,#20631);
#17114=AXIS2_PLACEMENT_3D('',#66617,#20634,#20635);
#17115=AXIS2_PLACEMENT_3D('',#66620,#20638,#20639);
#17116=AXIS2_PLACEMENT_3D('',#66622,#20641,#20642);
#17117=AXIS2_PLACEMENT_3D('',#66624,#20644,#20645);
#17118=AXIS2_PLACEMENT_3D('',#66626,#20647,#20648);
#17119=AXIS2_PLACEMENT_3D('',#66628,#20650,#20651);
#17120=AXIS2_PLACEMENT_3D('',#66629,#20652,#20653);
#17121=AXIS2_PLACEMENT_3D('',#66630,#20654,#20655);
#17122=AXIS2_PLACEMENT_3D('',#66631,#20656,#20657);
#17123=AXIS2_PLACEMENT_3D('',#66713,#20659,#20660);
#17124=AXIS2_PLACEMENT_3D('',#66763,#20661,#20662);
#17125=AXIS2_PLACEMENT_3D('',#67163,#20664,#20665);
#17126=AXIS2_PLACEMENT_3D('',#67593,#20667,#20668);
#17127=AXIS2_PLACEMENT_3D('',#68109,#20670,#20671);
#17128=AXIS2_PLACEMENT_3D('',#68545,#20673,#20674);
#17129=AXIS2_PLACEMENT_3D('',#69037,#20676,#20677);
#17130=AXIS2_PLACEMENT_3D('',#69465,#20679,#20680);
#17131=AXIS2_PLACEMENT_3D('',#69973,#20682,#20683);
#17132=AXIS2_PLACEMENT_3D('',#70401,#20685,#20686);
#17133=AXIS2_PLACEMENT_3D('',#70859,#20688,#20689);
#17134=AXIS2_PLACEMENT_3D('',#71289,#20691,#20692);
#17135=AXIS2_PLACEMENT_3D('',#71562,#20694,#20695);
#17136=AXIS2_PLACEMENT_3D('',#71883,#20697,#20698);
#17137=AXIS2_PLACEMENT_3D('',#71991,#20700,#20701);
#17138=AXIS2_PLACEMENT_3D('',#72352,#20703,#20704);
#17139=AXIS2_PLACEMENT_3D('',#72774,#20706,#20707);
#17140=AXIS2_PLACEMENT_3D('',#72902,#20709,#20710);
#17141=AXIS2_PLACEMENT_3D('',#73167,#20712,#20713);
#17142=AXIS2_PLACEMENT_3D('',#73580,#20715,#20716);
#17143=AXIS2_PLACEMENT_3D('',#73624,#20717,#20718);
#17144=AXIS2_PLACEMENT_3D('',#74816,#20719,#20720);
#17145=AXIS2_PLACEMENT_3D('',#74818,#20721,#20722);
#17146=AXIS2_PLACEMENT_3D('',#74820,#20723,#20724);
#17147=AXIS2_PLACEMENT_3D('',#75774,#20725,#20726);
#17148=AXIS2_PLACEMENT_3D('',#76009,#20727,#20728);
#17149=AXIS2_PLACEMENT_3D('',#76104,#20729,#20730);
#17150=AXIS2_PLACEMENT_3D('',#76106,#20731,#20732);
#17151=AXIS2_PLACEMENT_3D('',#76791,#20733,#20734);
#17152=AXIS2_PLACEMENT_3D('',#76793,#20735,#20736);
#17153=AXIS2_PLACEMENT_3D('',#76795,#20737,#20738);
#17154=AXIS2_PLACEMENT_3D('',#77359,#20739,#20740);
#17155=AXIS2_PLACEMENT_3D('',#77361,#20741,#20742);
#17156=AXIS2_PLACEMENT_3D('',#77362,#20743,#20744);
#17157=AXIS2_PLACEMENT_3D('',#77363,#20745,#20746);
#17158=AXIS2_PLACEMENT_3D('',#77365,#20747,#20748);
#17159=AXIS2_PLACEMENT_3D('',#77366,#20749,#20750);
#17160=AXIS2_PLACEMENT_3D('',#77397,#20752,#20753);
#17161=AXIS2_PLACEMENT_3D('',#77398,#20754,#20755);
#17162=AXIS2_PLACEMENT_3D('',#77404,#20759,#20760);
#17163=AXIS2_PLACEMENT_3D('',#77408,#20763,#20764);
#17164=AXIS2_PLACEMENT_3D('',#77412,#20767,#20768);
#17165=AXIS2_PLACEMENT_3D('',#77416,#20770,#20771);
#17166=AXIS2_PLACEMENT_3D('',#77417,#20772,#20773);
#17167=AXIS2_PLACEMENT_3D('',#77421,#20776,#20777);
#17168=AXIS2_PLACEMENT_3D('',#77425,#20780,#20781);
#17169=AXIS2_PLACEMENT_3D('',#77427,#20783,#20784);
#17170=AXIS2_PLACEMENT_3D('',#77428,#20785,#20786);
#17171=AXIS2_PLACEMENT_3D('',#77430,#20787,#20788);
#17172=AXIS2_PLACEMENT_3D('',#77432,#20789,#20790);
#17173=AXIS2_PLACEMENT_3D('',#77433,#20791,#20792);
#17174=AXIS2_PLACEMENT_3D('',#77434,#20793,#20794);
#17175=AXIS2_PLACEMENT_3D('',#77437,#20796,#20797);
#17176=AXIS2_PLACEMENT_3D('',#77438,#20798,#20799);
#17177=AXIS2_PLACEMENT_3D('',#77439,#20800,#20801);
#17178=AXIS2_PLACEMENT_3D('',#77441,#20802,#20803);
#17179=AXIS2_PLACEMENT_3D('',#77442,#20804,#20805);
#17180=AXIS2_PLACEMENT_3D('',#77444,#20807,#20808);
#17181=AXIS2_PLACEMENT_3D('',#77446,#20810,#20811);
#17182=AXIS2_PLACEMENT_3D('',#77447,#20812,#20813);
#17183=AXIS2_PLACEMENT_3D('',#77529,#20815,#20816);
#17184=AXIS2_PLACEMENT_3D('',#77579,#20817,#20818);
#17185=AXIS2_PLACEMENT_3D('',#77808,#20820,#20821);
#17186=AXIS2_PLACEMENT_3D('',#78180,#20823,#20824);
#17187=AXIS2_PLACEMENT_3D('',#78591,#20826,#20827);
#17188=AXIS2_PLACEMENT_3D('',#79040,#20829,#20830);
#17189=AXIS2_PLACEMENT_3D('',#79447,#20832,#20833);
#17190=AXIS2_PLACEMENT_3D('',#79776,#20835,#20836);
#17191=AXIS2_PLACEMENT_3D('',#80051,#20838,#20839);
#17192=AXIS2_PLACEMENT_3D('',#80414,#20841,#20842);
#17193=AXIS2_PLACEMENT_3D('',#80821,#20844,#20845);
#17194=AXIS2_PLACEMENT_3D('',#81236,#20847,#20848);
#17195=AXIS2_PLACEMENT_3D('',#81635,#20850,#20851);
#17196=AXIS2_PLACEMENT_3D('',#82032,#20853,#20854);
#17197=AXIS2_PLACEMENT_3D('',#82437,#20856,#20857);
#17198=AXIS2_PLACEMENT_3D('',#82852,#20859,#20860);
#17199=AXIS2_PLACEMENT_3D('',#82862,#20861,#20862);
#17200=AXIS2_PLACEMENT_3D('',#83895,#20863,#20864);
#17201=AXIS2_PLACEMENT_3D('',#83897,#20865,#20866);
#17202=AXIS2_PLACEMENT_3D('',#83899,#20867,#20868);
#17203=AXIS2_PLACEMENT_3D('',#84920,#20869,#20870);
#17204=AXIS2_PLACEMENT_3D('',#85083,#20871,#20872);
#17205=AXIS2_PLACEMENT_3D('',#85178,#20873,#20874);
#17206=AXIS2_PLACEMENT_3D('',#85180,#20875,#20876);
#17207=AXIS2_PLACEMENT_3D('',#85768,#20877,#20878);
#17208=AXIS2_PLACEMENT_3D('',#85770,#20879,#20880);
#17209=AXIS2_PLACEMENT_3D('',#85772,#20881,#20882);
#17210=AXIS2_PLACEMENT_3D('',#86239,#20883,#20884);
#17211=AXIS2_PLACEMENT_3D('',#86241,#20885,#20886);
#17212=AXIS2_PLACEMENT_3D('',#86242,#20887,#20888);
#17213=AXIS2_PLACEMENT_3D('',#86243,#20889,#20890);
#17214=AXIS2_PLACEMENT_3D('',#86245,#20891,#20892);
#17215=AXIS2_PLACEMENT_3D('',#86246,#20893,#20894);
#17216=AXIS2_PLACEMENT_3D('',#86277,#20896,#20897);
#17217=AXIS2_PLACEMENT_3D('',#86278,#20898,#20899);
#17218=AXIS2_PLACEMENT_3D('',#86284,#20903,#20904);
#17219=AXIS2_PLACEMENT_3D('',#86288,#20907,#20908);
#17220=AXIS2_PLACEMENT_3D('',#86292,#20911,#20912);
#17221=AXIS2_PLACEMENT_3D('',#86296,#20914,#20915);
#17222=AXIS2_PLACEMENT_3D('',#86297,#20916,#20917);
#17223=AXIS2_PLACEMENT_3D('',#86301,#20920,#20921);
#17224=AXIS2_PLACEMENT_3D('',#86305,#20924,#20925);
#17225=AXIS2_PLACEMENT_3D('',#86307,#20927,#20928);
#17226=AXIS2_PLACEMENT_3D('',#86308,#20929,#20930);
#17227=AXIS2_PLACEMENT_3D('',#86310,#20931,#20932);
#17228=AXIS2_PLACEMENT_3D('',#86312,#20933,#20934);
#17229=AXIS2_PLACEMENT_3D('',#86313,#20935,#20936);
#17230=AXIS2_PLACEMENT_3D('',#86314,#20937,#20938);
#17231=AXIS2_PLACEMENT_3D('',#86317,#20940,#20941);
#17232=AXIS2_PLACEMENT_3D('',#86318,#20942,#20943);
#17233=AXIS2_PLACEMENT_3D('',#86319,#20944,#20945);
#17234=AXIS2_PLACEMENT_3D('',#86321,#20946,#20947);
#17235=AXIS2_PLACEMENT_3D('',#86322,#20948,#20949);
#17236=AXIS2_PLACEMENT_3D('',#86324,#20951,#20952);
#17237=AXIS2_PLACEMENT_3D('',#86326,#20954,#20955);
#17238=AXIS2_PLACEMENT_3D('',#86327,#20956,#20957);
#17239=AXIS2_PLACEMENT_3D('',#86329,#20958,#20959);
#17240=AXIS2_PLACEMENT_3D('',#86332,#20961,#20962);
#17241=AXIS2_PLACEMENT_3D('',#86333,#20963,#20964);
#17242=AXIS2_PLACEMENT_3D('',#86335,#20965,#20966);
#17243=AXIS2_PLACEMENT_3D('',#86336,#20967,#20968);
#17244=AXIS2_PLACEMENT_3D('',#86338,#20969,#20970);
#17245=AXIS2_PLACEMENT_3D('',#86340,#20972,#20973);
#17246=AXIS2_PLACEMENT_3D('',#86342,#20974,#20975);
#17247=AXIS2_PLACEMENT_3D('',#86344,#20977,#20978);
#17248=AXIS2_PLACEMENT_3D('',#86346,#20979,#20980);
#17249=AXIS2_PLACEMENT_3D('',#86347,#20981,#20982);
#17250=AXIS2_PLACEMENT_3D('',#86349,#20983,#20984);
#17251=AXIS2_PLACEMENT_3D('',#86351,#20986,#20987);
#17252=AXIS2_PLACEMENT_3D('',#86353,#20988,#20989);
#17253=AXIS2_PLACEMENT_3D('',#86355,#20991,#20992);
#17254=AXIS2_PLACEMENT_3D('',#86358,#20994,#20995);
#17255=AXIS2_PLACEMENT_3D('',#86359,#20996,#20997);
#17256=AXIS2_PLACEMENT_3D('',#86360,#20998,#20999);
#17257=AXIS2_PLACEMENT_3D('',#86361,#21000,#21001);
#17258=AXIS2_PLACEMENT_3D('',#86362,#21002,#21003);
#17259=AXIS2_PLACEMENT_3D('',#86363,#21004,#21005);
#17260=AXIS2_PLACEMENT_3D('',#86364,#21006,#21007);
#17261=AXIS2_PLACEMENT_3D('',#86365,#21008,#21009);
#17262=AXIS2_PLACEMENT_3D('',#86366,#21010,#21011);
#17263=AXIS2_PLACEMENT_3D('',#86367,#21012,#21013);
#17264=AXIS2_PLACEMENT_3D('',#86368,#21014,#21015);
#17265=AXIS2_PLACEMENT_3D('',#86369,#21016,#21017);
#17266=AXIS2_PLACEMENT_3D('',#86370,#21018,#21019);
#17267=AXIS2_PLACEMENT_3D('',#86371,#21020,#21021);
#17268=AXIS2_PLACEMENT_3D('',#86372,#21022,#21023);
#17269=AXIS2_PLACEMENT_3D('',#86373,#21024,#21025);
#17270=AXIS2_PLACEMENT_3D('',#86374,#21026,#21027);
#17271=AXIS2_PLACEMENT_3D('',#86375,#21028,#21029);
#17272=AXIS2_PLACEMENT_3D('',#86376,#21030,#21031);
#17273=AXIS2_PLACEMENT_3D('',#86377,#21032,#21033);
#17274=AXIS2_PLACEMENT_3D('',#86378,#21034,#21035);
#17275=AXIS2_PLACEMENT_3D('',#86379,#21036,#21037);
#17276=AXIS2_PLACEMENT_3D('',#86380,#21038,#21039);
#17277=AXIS2_PLACEMENT_3D('',#86381,#21040,#21041);
#17278=AXIS2_PLACEMENT_3D('',#86382,#21042,#21043);
#17279=AXIS2_PLACEMENT_3D('',#86383,#21044,#21045);
#17280=AXIS2_PLACEMENT_3D('',#86384,#21046,#21047);
#17281=AXIS2_PLACEMENT_3D('',#86385,#21048,#21049);
#17282=AXIS2_PLACEMENT_3D('',#86386,#21050,#21051);
#17283=AXIS2_PLACEMENT_3D('',#86387,#21052,#21053);
#17284=AXIS2_PLACEMENT_3D('',#86388,#21054,#21055);
#17285=AXIS2_PLACEMENT_3D('',#86389,#21056,#21057);
#17286=DIRECTION('axis',(0.,0.,1.));
#17287=DIRECTION('refdir',(1.,0.,0.));
#17288=DIRECTION('axis',(0.,0.,1.));
#17289=DIRECTION('refdir',(1.,0.,0.));
#17290=DIRECTION('center_axis',(0.,0.,-1.));
#17291=DIRECTION('ref_axis',(0.,-1.,0.));
#17292=DIRECTION('',(0.,-1.,0.));
#17293=DIRECTION('',(-1.,0.,0.));
#17294=DIRECTION('',(0.,-1.,0.));
#17295=DIRECTION('',(-1.,0.,0.));
#17296=DIRECTION('center_axis',(0.,1.,0.));
#17297=DIRECTION('ref_axis',(0.,0.,-1.));
#17298=DIRECTION('',(0.,0.,-1.));
#17299=DIRECTION('',(-1.,0.,0.));
#17300=DIRECTION('',(0.,0.,-1.));
#17301=DIRECTION('center_axis',(0.,0.,1.));
#17302=DIRECTION('ref_axis',(0.,1.,0.));
#17303=DIRECTION('',(0.,1.,0.));
#17304=DIRECTION('',(-1.,0.,0.));
#17305=DIRECTION('',(0.,1.,0.));
#17306=DIRECTION('center_axis',(0.,-1.,0.));
#17307=DIRECTION('ref_axis',(0.,0.,1.));
#17308=DIRECTION('',(0.,0.,1.));
#17309=DIRECTION('',(0.,0.,1.));
#17310=DIRECTION('center_axis',(-1.,0.,0.));
#17311=DIRECTION('ref_axis',(0.,0.,1.));
#17312=DIRECTION('center_axis',(0.,0.,-1.));
#17313=DIRECTION('ref_axis',(0.,-1.,0.));
#17314=DIRECTION('',(-1.,0.,0.));
#17315=DIRECTION('',(0.,-1.,0.));
#17316=DIRECTION('',(-1.,0.,0.));
#17317=DIRECTION('',(0.,-1.,0.));
#17318=DIRECTION('center_axis',(-1.,0.,0.));
#17319=DIRECTION('ref_axis',(0.,0.,1.));
#17320=DIRECTION('',(0.,0.,1.));
#17321=DIRECTION('',(0.,0.,-1.));
#17322=DIRECTION('',(0.,1.,0.));
#17323=DIRECTION('',(0.,0.,1.));
#17324=DIRECTION('',(0.,-1.,0.));
#17325=DIRECTION('center_axis',(0.,1.,0.));
#17326=DIRECTION('ref_axis',(0.,0.,-1.));
#17327=DIRECTION('',(0.,0.,-1.));
#17328=DIRECTION('',(-1.,0.,0.));
#17329=DIRECTION('center_axis',(0.,0.,1.));
#17330=DIRECTION('ref_axis',(0.,1.,0.));
#17331=DIRECTION('',(0.,1.,0.));
#17332=DIRECTION('',(-1.,0.,0.));
#17333=DIRECTION('center_axis',(0.,-1.,0.));
#17334=DIRECTION('ref_axis',(0.,0.,1.));
#17335=DIRECTION('',(1.,0.,0.));
#17336=DIRECTION('',(0.,0.,1.));
#17337=DIRECTION('center_axis',(0.,0.,-1.));
#17338=DIRECTION('ref_axis',(0.,-1.,0.));
#17339=DIRECTION('',(0.,-1.,0.));
#17340=DIRECTION('',(-1.,0.,0.));
#17341=DIRECTION('',(0.,-1.,0.));
#17342=DIRECTION('',(-1.,0.,0.));
#17343=DIRECTION('center_axis',(0.,1.,0.));
#17344=DIRECTION('ref_axis',(0.,0.,-1.));
#17345=DIRECTION('',(0.,0.,-1.));
#17346=DIRECTION('',(-1.,0.,0.));
#17347=DIRECTION('',(0.,0.,-1.));
#17348=DIRECTION('center_axis',(0.,0.,1.));
#17349=DIRECTION('ref_axis',(0.,1.,0.));
#17350=DIRECTION('',(0.,1.,0.));
#17351=DIRECTION('',(-1.,0.,0.));
#17352=DIRECTION('',(0.,1.,0.));
#17353=DIRECTION('center_axis',(0.,-1.,0.));
#17354=DIRECTION('ref_axis',(0.,0.,1.));
#17355=DIRECTION('',(0.,0.,1.));
#17356=DIRECTION('',(0.,0.,1.));
#17357=DIRECTION('center_axis',(-1.,0.,0.));
#17358=DIRECTION('ref_axis',(0.,0.,1.));
#17359=DIRECTION('center_axis',(0.,0.,-1.));
#17360=DIRECTION('ref_axis',(0.,-1.,0.));
#17361=DIRECTION('',(0.,-1.,0.));
#17362=DIRECTION('',(-1.,0.,0.));
#17363=DIRECTION('',(0.,-1.,0.));
#17364=DIRECTION('',(-1.,0.,0.));
#17365=DIRECTION('center_axis',(0.,1.,0.));
#17366=DIRECTION('ref_axis',(0.,0.,-1.));
#17367=DIRECTION('',(0.,0.,-1.));
#17368=DIRECTION('',(-1.,0.,0.));
#17369=DIRECTION('',(0.,0.,-1.));
#17370=DIRECTION('center_axis',(0.,0.,1.));
#17371=DIRECTION('ref_axis',(0.,1.,0.));
#17372=DIRECTION('',(0.,1.,0.));
#17373=DIRECTION('',(-1.,0.,0.));
#17374=DIRECTION('',(0.,1.,0.));
#17375=DIRECTION('center_axis',(0.,-1.,0.));
#17376=DIRECTION('ref_axis',(0.,0.,1.));
#17377=DIRECTION('',(0.,0.,1.));
#17378=DIRECTION('',(0.,0.,1.));
#17379=DIRECTION('center_axis',(-1.,0.,0.));
#17380=DIRECTION('ref_axis',(0.,0.,1.));
#17381=DIRECTION('center_axis',(0.,0.,-1.));
#17382=DIRECTION('ref_axis',(0.,-1.,0.));
#17383=DIRECTION('',(0.,-1.,0.));
#17384=DIRECTION('',(-1.,0.,0.));
#17385=DIRECTION('',(0.,-1.,0.));
#17386=DIRECTION('',(-1.,0.,0.));
#17387=DIRECTION('center_axis',(0.,1.,0.));
#17388=DIRECTION('ref_axis',(0.,0.,-1.));
#17389=DIRECTION('',(0.,0.,-1.));
#17390=DIRECTION('',(-1.,0.,0.));
#17391=DIRECTION('',(0.,0.,-1.));
#17392=DIRECTION('center_axis',(0.,0.,1.));
#17393=DIRECTION('ref_axis',(0.,1.,0.));
#17394=DIRECTION('',(0.,1.,0.));
#17395=DIRECTION('',(-1.,0.,0.));
#17396=DIRECTION('',(0.,1.,0.));
#17397=DIRECTION('center_axis',(0.,-1.,0.));
#17398=DIRECTION('ref_axis',(0.,0.,1.));
#17399=DIRECTION('',(0.,0.,1.));
#17400=DIRECTION('',(0.,0.,1.));
#17401=DIRECTION('center_axis',(-1.,0.,0.));
#17402=DIRECTION('ref_axis',(0.,0.,1.));
#17403=DIRECTION('center_axis',(0.,0.,-1.));
#17404=DIRECTION('ref_axis',(0.,-1.,0.));
#17405=DIRECTION('',(1.,0.,0.));
#17406=DIRECTION('',(0.,-1.,0.));
#17407=DIRECTION('',(-1.,0.,0.));
#17408=DIRECTION('',(0.,-1.,0.));
#17409=DIRECTION('center_axis',(0.,1.,0.));
#17410=DIRECTION('ref_axis',(0.,0.,-1.));
#17411=DIRECTION('',(-1.,0.,0.));
#17412=DIRECTION('',(0.,0.,-1.));
#17413=DIRECTION('',(-1.,0.,0.));
#17414=DIRECTION('',(0.,0.,-1.));
#17415=DIRECTION('center_axis',(0.,0.,1.));
#17416=DIRECTION('ref_axis',(0.,1.,0.));
#17417=DIRECTION('',(0.,1.,0.));
#17418=DIRECTION('',(-1.,0.,0.));
#17419=DIRECTION('',(0.,1.,0.));
#17420=DIRECTION('center_axis',(0.,-1.,0.));
#17421=DIRECTION('ref_axis',(0.,0.,1.));
#17422=DIRECTION('',(0.,0.,1.));
#17423=DIRECTION('',(0.,0.,1.));
#17424=DIRECTION('center_axis',(-1.,0.,0.));
#17425=DIRECTION('ref_axis',(0.,0.,1.));
#17426=DIRECTION('',(0.,0.,-1.));
#17427=DIRECTION('',(0.,-1.,0.));
#17428=DIRECTION('center_axis',(0.,1.,0.));
#17429=DIRECTION('ref_axis',(1.,0.,0.));
#17430=DIRECTION('',(-1.,0.,0.));
#17431=DIRECTION('',(0.,0.,-1.));
#17432=DIRECTION('',(1.,0.,0.));
#17433=DIRECTION('',(0.,0.,-1.));
#17434=DIRECTION('center_axis',(0.,0.,1.));
#17435=DIRECTION('ref_axis',(-1.,0.,0.));
#17436=DIRECTION('',(0.,1.,0.));
#17437=DIRECTION('',(1.,0.,0.));
#17438=DIRECTION('',(0.,-1.,0.));
#17439=DIRECTION('center_axis',(1.,0.,0.));
#17440=DIRECTION('ref_axis',(0.,0.,-1.));
#17441=DIRECTION('',(0.,-1.,0.));
#17442=DIRECTION('',(0.,0.,1.));
#17443=DIRECTION('',(0.,-1.,0.));
#17444=DIRECTION('',(0.,0.,-1.));
#17445=DIRECTION('',(0.,-1.,0.));
#17446=DIRECTION('',(0.,0.,1.));
#17447=DIRECTION('',(0.,1.,0.));
#17448=DIRECTION('',(0.,0.,-1.));
#17449=DIRECTION('',(0.,1.,0.));
#17450=DIRECTION('',(0.,0.,1.));
#17451=DIRECTION('center_axis',(-1.,0.,0.));
#17452=DIRECTION('ref_axis',(0.,0.,1.));
#17453=DIRECTION('center_axis',(0.,0.,1.));
#17454=DIRECTION('ref_axis',(0.,-1.,0.));
#17455=DIRECTION('',(0.,-1.,0.));
#17456=DIRECTION('',(1.,0.,0.));
#17457=DIRECTION('',(0.,-1.,0.));
#17458=DIRECTION('',(1.,0.,0.));
#17459=DIRECTION('center_axis',(0.,1.,0.));
#17460=DIRECTION('ref_axis',(0.,0.,1.));
#17461=DIRECTION('',(0.,0.,1.));
#17462=DIRECTION('',(1.,0.,0.));
#17463=DIRECTION('',(0.,0.,1.));
#17464=DIRECTION('center_axis',(0.,0.,-1.));
#17465=DIRECTION('ref_axis',(0.,1.,0.));
#17466=DIRECTION('',(0.,1.,0.));
#17467=DIRECTION('',(1.,0.,0.));
#17468=DIRECTION('',(0.,1.,0.));
#17469=DIRECTION('center_axis',(0.,-1.,0.));
#17470=DIRECTION('ref_axis',(0.,0.,-1.));
#17471=DIRECTION('',(0.,0.,-1.));
#17472=DIRECTION('',(0.,0.,-1.));
#17473=DIRECTION('center_axis',(1.,0.,0.));
#17474=DIRECTION('ref_axis',(0.,0.,-1.));
#17475=DIRECTION('center_axis',(0.,0.,-1.));
#17476=DIRECTION('ref_axis',(0.,1.,0.));
#17477=DIRECTION('',(-1.,0.,0.));
#17478=DIRECTION('',(0.,1.,0.));
#17479=DIRECTION('',(1.,0.,0.));
#17480=DIRECTION('',(0.,1.,0.));
#17481=DIRECTION('center_axis',(0.,0.,1.));
#17482=DIRECTION('ref_axis',(0.,-1.,0.));
#17483=DIRECTION('',(0.,-1.,0.));
#17484=DIRECTION('',(1.,0.,0.));
#17485=DIRECTION('',(0.,-1.,0.));
#17486=DIRECTION('',(1.,0.,0.));
#17487=DIRECTION('center_axis',(0.,1.,0.));
#17488=DIRECTION('ref_axis',(0.,0.,1.));
#17489=DIRECTION('',(0.,0.,1.));
#17490=DIRECTION('',(0.,0.,1.));
#17491=DIRECTION('center_axis',(0.,-1.,0.));
#17492=DIRECTION('ref_axis',(0.,0.,-1.));
#17493=DIRECTION('',(1.,0.,0.));
#17494=DIRECTION('',(0.,0.,-1.));
#17495=DIRECTION('',(0.,0.,-1.));
#17496=DIRECTION('center_axis',(1.,0.,0.));
#17497=DIRECTION('ref_axis',(0.,0.,-1.));
#17498=DIRECTION('',(0.,0.,-1.));
#17499=DIRECTION('',(0.,1.,0.));
#17500=DIRECTION('center_axis',(0.,0.,1.));
#17501=DIRECTION('ref_axis',(0.,-1.,0.));
#17502=DIRECTION('',(0.,-1.,0.));
#17503=DIRECTION('',(1.,0.,0.));
#17504=DIRECTION('',(0.,-1.,0.));
#17505=DIRECTION('',(1.,0.,0.));
#17506=DIRECTION('center_axis',(0.,1.,0.));
#17507=DIRECTION('ref_axis',(0.,0.,1.));
#17508=DIRECTION('',(0.,0.,1.));
#17509=DIRECTION('',(1.,0.,0.));
#17510=DIRECTION('',(0.,0.,1.));
#17511=DIRECTION('center_axis',(0.,0.,-1.));
#17512=DIRECTION('ref_axis',(0.,1.,0.));
#17513=DIRECTION('',(0.,1.,0.));
#17514=DIRECTION('',(1.,0.,0.));
#17515=DIRECTION('',(0.,1.,0.));
#17516=DIRECTION('center_axis',(0.,-1.,0.));
#17517=DIRECTION('ref_axis',(0.,0.,-1.));
#17518=DIRECTION('',(0.,0.,-1.));
#17519=DIRECTION('',(0.,0.,-1.));
#17520=DIRECTION('center_axis',(1.,0.,0.));
#17521=DIRECTION('ref_axis',(0.,0.,-1.));
#17522=DIRECTION('center_axis',(0.,0.,1.));
#17523=DIRECTION('ref_axis',(0.,-1.,0.));
#17524=DIRECTION('',(0.,-1.,0.));
#17525=DIRECTION('',(1.,0.,0.));
#17526=DIRECTION('',(0.,-1.,0.));
#17527=DIRECTION('',(1.,0.,0.));
#17528=DIRECTION('center_axis',(0.,1.,0.));
#17529=DIRECTION('ref_axis',(0.,0.,1.));
#17530=DIRECTION('',(0.,0.,1.));
#17531=DIRECTION('',(1.,0.,0.));
#17532=DIRECTION('',(0.,0.,1.));
#17533=DIRECTION('center_axis',(0.,0.,-1.));
#17534=DIRECTION('ref_axis',(0.,1.,0.));
#17535=DIRECTION('',(0.,1.,0.));
#17536=DIRECTION('',(1.,0.,0.));
#17537=DIRECTION('',(0.,1.,0.));
#17538=DIRECTION('center_axis',(0.,-1.,0.));
#17539=DIRECTION('ref_axis',(0.,0.,-1.));
#17540=DIRECTION('',(0.,0.,-1.));
#17541=DIRECTION('',(0.,0.,-1.));
#17542=DIRECTION('center_axis',(1.,0.,0.));
#17543=DIRECTION('ref_axis',(0.,0.,-1.));
#17544=DIRECTION('center_axis',(0.,0.,1.));
#17545=DIRECTION('ref_axis',(0.,-1.,0.));
#17546=DIRECTION('',(0.,-1.,0.));
#17547=DIRECTION('',(1.,0.,0.));
#17548=DIRECTION('',(0.,-1.,0.));
#17549=DIRECTION('',(1.,0.,0.));
#17550=DIRECTION('center_axis',(0.,1.,0.));
#17551=DIRECTION('ref_axis',(0.,0.,1.));
#17552=DIRECTION('',(0.,0.,1.));
#17553=DIRECTION('',(1.,0.,0.));
#17554=DIRECTION('',(0.,0.,1.));
#17555=DIRECTION('center_axis',(0.,0.,-1.));
#17556=DIRECTION('ref_axis',(0.,1.,0.));
#17557=DIRECTION('',(0.,1.,0.));
#17558=DIRECTION('',(1.,0.,0.));
#17559=DIRECTION('',(0.,1.,0.));
#17560=DIRECTION('center_axis',(0.,-1.,0.));
#17561=DIRECTION('ref_axis',(0.,0.,-1.));
#17562=DIRECTION('',(0.,0.,-1.));
#17563=DIRECTION('',(0.,0.,-1.));
#17564=DIRECTION('center_axis',(1.,0.,0.));
#17565=DIRECTION('ref_axis',(0.,0.,-1.));
#17566=DIRECTION('center_axis',(0.,1.,0.));
#17567=DIRECTION('ref_axis',(0.,0.,1.));
#17568=DIRECTION('',(-1.,0.,0.));
#17569=DIRECTION('',(0.,0.,1.));
#17570=DIRECTION('',(1.,0.,0.));
#17571=DIRECTION('',(0.,0.,1.));
#17572=DIRECTION('center_axis',(0.,0.,1.));
#17573=DIRECTION('ref_axis',(0.,-1.,0.));
#17574=DIRECTION('',(0.,-1.,0.));
#17575=DIRECTION('',(0.,-1.,0.));
#17576=DIRECTION('',(1.,0.,0.));
#17577=DIRECTION('center_axis',(0.,0.,-1.));
#17578=DIRECTION('ref_axis',(0.,1.,0.));
#17579=DIRECTION('',(1.,0.,0.));
#17580=DIRECTION('',(0.,1.,0.));
#17581=DIRECTION('',(1.,0.,0.));
#17582=DIRECTION('',(0.,1.,0.));
#17583=DIRECTION('center_axis',(0.,-1.,0.));
#17584=DIRECTION('ref_axis',(0.,0.,-1.));
#17585=DIRECTION('',(0.,0.,-1.));
#17586=DIRECTION('',(0.,0.,-1.));
#17587=DIRECTION('center_axis',(1.,0.,0.));
#17588=DIRECTION('ref_axis',(0.,0.,-1.));
#17589=DIRECTION('',(0.,1.,0.));
#17590=DIRECTION('',(0.,0.,1.));
#17591=DIRECTION('center_axis',(0.,1.,0.));
#17592=DIRECTION('ref_axis',(1.,0.,0.));
#17593=DIRECTION('',(0.,0.,1.));
#17594=DIRECTION('',(1.,0.,0.));
#17595=DIRECTION('',(0.,0.,1.));
#17596=DIRECTION('',(-1.,0.,0.));
#17597=DIRECTION('center_axis',(0.,0.,1.));
#17598=DIRECTION('ref_axis',(1.,0.,0.));
#17599=DIRECTION('',(0.,-1.,0.));
#17600=DIRECTION('',(-1.,0.,0.));
#17601=DIRECTION('',(0.,1.,0.));
#17602=DIRECTION('',(-1.,0.,0.));
#17603=DIRECTION('center_axis',(-1.,0.,0.));
#17604=DIRECTION('ref_axis',(0.,0.,1.));
#17605=DIRECTION('',(0.,-1.,0.));
#17606=DIRECTION('',(0.,0.,-1.));
#17607=DIRECTION('',(0.,-1.,0.));
#17608=DIRECTION('center_axis',(1.,0.,0.));
#17609=DIRECTION('ref_axis',(0.,-1.,0.));
#17610=DIRECTION('center_axis',(1.,0.,0.));
#17611=DIRECTION('ref_axis',(0.,-1.,0.));
#17612=DIRECTION('',(0.,-1.,0.));
#17613=DIRECTION('center_axis',(1.,0.,0.));
#17614=DIRECTION('ref_axis',(0.,-1.,0.));
#17615=DIRECTION('center_axis',(1.,0.,0.));
#17616=DIRECTION('ref_axis',(0.,-1.,0.));
#17617=DIRECTION('',(0.,-1.,0.));
#17618=DIRECTION('',(0.,0.,1.));
#17619=DIRECTION('',(0.,0.,-1.));
#17620=DIRECTION('',(0.,1.,0.));
#17621=DIRECTION('',(0.,0.,1.));
#17622=DIRECTION('',(0.,1.,0.));
#17623=DIRECTION('',(0.,0.,-1.));
#17624=DIRECTION('',(0.,1.,0.));
#17625=DIRECTION('center_axis',(1.,0.,0.));
#17626=DIRECTION('ref_axis',(0.,0.,1.));
#17627=DIRECTION('center_axis',(1.,0.,0.));
#17628=DIRECTION('ref_axis',(0.,-1.,0.));
#17629=DIRECTION('center_axis',(1.,0.,0.));
#17630=DIRECTION('ref_axis',(0.,-1.,0.));
#17631=DIRECTION('center_axis',(0.,1.,0.));
#17632=DIRECTION('ref_axis',(1.,0.,0.));
#17633=DIRECTION('center_axis',(0.,-1.,0.));
#17634=DIRECTION('ref_axis',(1.,0.,0.));
#17635=DIRECTION('',(0.,1.,0.));
#17636=DIRECTION('center_axis',(0.,-1.,0.));
#17637=DIRECTION('ref_axis',(1.,0.,0.));
#17638=DIRECTION('',(0.,1.,0.));
#17639=DIRECTION('center_axis',(0.,1.,0.));
#17640=DIRECTION('ref_axis',(1.,0.,0.));
#17641=DIRECTION('center_axis',(0.,-1.,0.));
#17642=DIRECTION('ref_axis',(1.,0.,0.));
#17643=DIRECTION('',(0.,1.,0.));
#17644=DIRECTION('center_axis',(0.,-1.,0.));
#17645=DIRECTION('ref_axis',(1.,0.,0.));
#17646=DIRECTION('center_axis',(1.,0.,0.));
#17647=DIRECTION('ref_axis',(0.,0.,-1.));
#17648=DIRECTION('',(0.,0.,-1.));
#17649=DIRECTION('',(0.,1.,0.));
#17650=DIRECTION('',(0.,0.,-1.));
#17651=DIRECTION('center_axis',(0.,0.,1.));
#17652=DIRECTION('ref_axis',(1.,0.,0.));
#17653=DIRECTION('',(1.,0.,0.));
#17654=DIRECTION('',(0.,1.,0.));
#17655=DIRECTION('',(1.,0.,0.));
#17656=DIRECTION('center_axis',(-1.,0.,0.));
#17657=DIRECTION('ref_axis',(0.,0.,1.));
#17658=DIRECTION('',(0.,0.,1.));
#17659=DIRECTION('',(0.,1.,0.));
#17660=DIRECTION('',(0.,0.,1.));
#17661=DIRECTION('center_axis',(0.,1.,0.));
#17662=DIRECTION('ref_axis',(1.,0.,0.));
#17663=DIRECTION('center_axis',(0.,-1.,0.));
#17664=DIRECTION('ref_axis',(1.,0.,0.));
#17665=DIRECTION('center_axis',(0.,-1.,0.));
#17666=DIRECTION('ref_axis',(1.,0.,0.));
#17667=DIRECTION('center_axis',(0.,1.,0.));
#17668=DIRECTION('ref_axis',(1.,0.,0.));
#17669=DIRECTION('center_axis',(-1.,0.,0.));
#17670=DIRECTION('ref_axis',(0.,0.,-1.));
#17671=DIRECTION('',(0.,0.,-1.));
#17672=DIRECTION('',(0.,-1.,0.));
#17673=DIRECTION('',(0.,0.,-1.));
#17674=DIRECTION('',(0.,-1.,0.));
#17675=DIRECTION('center_axis',(0.,0.,1.));
#17676=DIRECTION('ref_axis',(-1.,0.,0.));
#17677=DIRECTION('',(-1.,0.,0.));
#17678=DIRECTION('',(0.,-1.,0.));
#17679=DIRECTION('',(-1.,0.,0.));
#17680=DIRECTION('center_axis',(1.,0.,0.));
#17681=DIRECTION('ref_axis',(0.,0.,1.));
#17682=DIRECTION('',(0.,0.,1.));
#17683=DIRECTION('',(0.,-1.,0.));
#17684=DIRECTION('',(0.,0.,1.));
#17685=DIRECTION('center_axis',(0.,1.,0.));
#17686=DIRECTION('ref_axis',(1.,0.,0.));
#17687=DIRECTION('center_axis',(0.,1.,0.));
#17688=DIRECTION('ref_axis',(1.,0.,0.));
#17689=DIRECTION('center_axis',(0.,1.,0.));
#17690=DIRECTION('ref_axis',(1.,0.,0.));
#17691=DIRECTION('center_axis',(0.,1.,0.));
#17692=DIRECTION('ref_axis',(1.,0.,0.));
#17693=DIRECTION('center_axis',(0.,1.,0.));
#17694=DIRECTION('ref_axis',(0.,0.,1.));
#17695=DIRECTION('center_axis',(0.,-1.,0.));
#17696=DIRECTION('ref_axis',(1.,0.,0.));
#17697=DIRECTION('center_axis',(0.,-1.,0.));
#17698=DIRECTION('ref_axis',(1.,0.,0.));
#17699=DIRECTION('center_axis',(0.,-1.,0.));
#17700=DIRECTION('ref_axis',(1.,0.,0.));
#17701=DIRECTION('',(0.,0.,1.));
#17702=DIRECTION('center_axis',(0.,-1.,0.));
#17703=DIRECTION('ref_axis',(-0.707106781186548,0.,0.707106781186548));
#17704=DIRECTION('',(1.,0.,0.));
#17705=DIRECTION('center_axis',(0.,-1.,0.));
#17706=DIRECTION('ref_axis',(0.707106781186548,0.,0.707106781186548));
#17707=DIRECTION('',(-1.,0.,0.));
#17708=DIRECTION('',(0.,0.,-1.));
#17709=DIRECTION('center_axis',(0.,-1.,0.));
#17710=DIRECTION('ref_axis',(1.,0.,0.));
#17711=DIRECTION('center_axis',(0.,-1.,0.));
#17712=DIRECTION('ref_axis',(1.,0.,0.));
#17713=DIRECTION('center_axis',(0.,-1.,0.));
#17714=DIRECTION('ref_axis',(1.,0.,0.));
#17715=DIRECTION('center_axis',(0.,-1.,0.));
#17716=DIRECTION('ref_axis',(-1.,0.,0.));
#17717=DIRECTION('center_axis',(0.,-1.,0.));
#17718=DIRECTION('ref_axis',(-1.,0.,0.));
#17719=DIRECTION('center_axis',(0.,1.,0.));
#17720=DIRECTION('ref_axis',(-1.,0.,0.));
#17721=DIRECTION('center_axis',(0.,-1.,0.));
#17722=DIRECTION('ref_axis',(-1.,0.,0.));
#17723=DIRECTION('center_axis',(0.,-1.,0.));
#17724=DIRECTION('ref_axis',(-1.,0.,0.));
#17725=DIRECTION('center_axis',(0.707106781186548,-0.707106781186548,0.));
#17726=DIRECTION('ref_axis',(0.707104368765779,0.707104368765779,-0.00261215326844819));
#17727=DIRECTION('center_axis',(0.,1.,0.));
#17728=DIRECTION('ref_axis',(-1.,0.,0.));
#17729=DIRECTION('center_axis',(-0.707106781186548,0.707106781186548,0.));
#17730=DIRECTION('ref_axis',(0.,0.,1.));
#17731=DIRECTION('',(0.,0.,-1.));
#17732=DIRECTION('center_axis',(-0.707106781186548,0.707106781186548,0.));
#17733=DIRECTION('ref_axis',(0.707104368771539,0.707104368771539,0.0026121501499));
#17734=DIRECTION('',(0.,0.,1.));
#17735=DIRECTION('center_axis',(0.,-1.,0.));
#17736=DIRECTION('ref_axis',(1.,0.,0.));
#17737=DIRECTION('center_axis',(0.,-1.,0.));
#17738=DIRECTION('ref_axis',(1.,0.,0.));
#17739=DIRECTION('center_axis',(0.,1.,0.));
#17740=DIRECTION('ref_axis',(1.,0.,0.));
#17741=DIRECTION('center_axis',(0.,-1.,0.));
#17742=DIRECTION('ref_axis',(1.,0.,0.));
#17743=DIRECTION('center_axis',(0.,-1.,0.));
#17744=DIRECTION('ref_axis',(1.,0.,0.));
#17745=DIRECTION('center_axis',(0.,1.,0.));
#17746=DIRECTION('ref_axis',(1.,0.,0.));
#17747=DIRECTION('center_axis',(0.,-1.,0.));
#17748=DIRECTION('ref_axis',(-1.,0.,0.));
#17749=DIRECTION('center_axis',(0.,-1.,0.));
#17750=DIRECTION('ref_axis',(-1.,0.,0.));
#17751=DIRECTION('center_axis',(-0.707106781186948,-0.707106781186147,-3.20702973920932E-12));
#17752=DIRECTION('ref_axis',(0.707104368780728,-0.707104368781518,-0.00261214496127044));
#17753=DIRECTION('center_axis',(0.,1.,0.));
#17754=DIRECTION('ref_axis',(-1.,0.,0.));
#17755=DIRECTION('center_axis',(0.707106781186548,0.707106781186548,0.));
#17756=DIRECTION('ref_axis',(0.,0.,-1.));
#17757=DIRECTION('',(0.,0.,1.));
#17758=DIRECTION('center_axis',(0.707106781186948,0.707106781186147,-3.20702973916201E-12));
#17759=DIRECTION('ref_axis',(0.707104368789339,-0.707104368790129,0.00261214029942537));
#17760=DIRECTION('',(0.,0.,-1.));
#17761=DIRECTION('center_axis',(0.,-1.,0.));
#17762=DIRECTION('ref_axis',(1.,0.,0.));
#17763=DIRECTION('center_axis',(0.,1.,0.));
#17764=DIRECTION('ref_axis',(1.,0.,0.));
#17765=DIRECTION('center_axis',(0.,-1.,0.));
#17766=DIRECTION('ref_axis',(1.,0.,0.));
#17767=DIRECTION('center_axis',(0.,-1.,0.));
#17768=DIRECTION('ref_axis',(1.,0.,0.));
#17769=DIRECTION('center_axis',(0.,1.,0.));
#17770=DIRECTION('ref_axis',(1.,0.,0.));
#17771=DIRECTION('center_axis',(0.,-1.,0.));
#17772=DIRECTION('ref_axis',(1.,0.,0.));
#17773=DIRECTION('center_axis',(0.,-1.,0.));
#17774=DIRECTION('ref_axis',(1.,0.,0.));
#17775=DIRECTION('center_axis',(0.,1.,0.));
#17776=DIRECTION('ref_axis',(1.,0.,0.));
#17777=DIRECTION('center_axis',(0.,-1.,0.));
#17778=DIRECTION('ref_axis',(1.,0.,0.));
#17779=DIRECTION('center_axis',(0.,-1.,0.));
#17780=DIRECTION('ref_axis',(1.,0.,0.));
#17781=DIRECTION('center_axis',(0.,1.,0.));
#17782=DIRECTION('ref_axis',(1.,0.,0.));
#17783=DIRECTION('center_axis',(0.,-1.,0.));
#17784=DIRECTION('ref_axis',(1.,0.,0.));
#17785=DIRECTION('center_axis',(0.,-1.,0.));
#17786=DIRECTION('ref_axis',(-1.,0.,0.));
#17787=DIRECTION('center_axis',(0.,1.,0.));
#17788=DIRECTION('ref_axis',(-1.,0.,0.));
#17789=DIRECTION('center_axis',(0.,-1.,0.));
#17790=DIRECTION('ref_axis',(-1.,0.,0.));
#17791=DIRECTION('center_axis',(0.,1.,0.));
#17792=DIRECTION('ref_axis',(1.,0.,0.));
#17793=DIRECTION('',(0.,1.,0.));
#17794=DIRECTION('',(0.,1.,0.));
#17795=DIRECTION('center_axis',(0.,1.,0.));
#17796=DIRECTION('ref_axis',(1.,0.,0.));
#17797=DIRECTION('',(0.,1.,0.));
#17798=DIRECTION('center_axis',(0.,1.,0.));
#17799=DIRECTION('ref_axis',(1.,0.,0.));
#17800=DIRECTION('',(0.,-1.,0.));
#17801=DIRECTION('center_axis',(0.,1.,0.));
#17802=DIRECTION('ref_axis',(1.,0.,0.));
#17803=DIRECTION('',(0.,-1.,0.));
#17804=DIRECTION('center_axis',(0.,1.,0.));
#17805=DIRECTION('ref_axis',(-0.991227900682635,0.,0.132163720091018));
#17806=DIRECTION('',(0.,1.,0.));
#17807=DIRECTION('center_axis',(0.,1.,0.));
#17808=DIRECTION('ref_axis',(1.,0.,0.));
#17809=DIRECTION('',(0.,1.,0.));
#17810=DIRECTION('center_axis',(0.,1.,0.));
#17811=DIRECTION('ref_axis',(1.,0.,0.));
#17812=DIRECTION('center_axis',(0.,-1.,0.));
#17813=DIRECTION('ref_axis',(0.,0.,1.));
#17814=DIRECTION('center_axis',(0.,-1.,0.));
#17815=DIRECTION('ref_axis',(-1.,0.,0.));
#17816=DIRECTION('center_axis',(0.,-1.,0.));
#17817=DIRECTION('ref_axis',(-1.,0.,0.));
#17818=DIRECTION('center_axis',(0.,-1.,0.));
#17819=DIRECTION('ref_axis',(-1.,0.,0.));
#17820=DIRECTION('center_axis',(0.,-1.,0.));
#17821=DIRECTION('ref_axis',(-1.,0.,0.));
#17822=DIRECTION('center_axis',(0.,0.,1.));
#17823=DIRECTION('ref_axis',(1.,0.,0.));
#17824=DIRECTION('',(0.,0.,1.));
#17825=DIRECTION('center_axis',(0.,0.,1.));
#17826=DIRECTION('ref_axis',(1.,0.,0.));
#17827=DIRECTION('center_axis',(0.,0.,1.));
#17828=DIRECTION('ref_axis',(1.,0.,0.));
#17829=DIRECTION('',(-0.707106781186545,-8.6595605623549E-17,0.70710678118655));
#17830=DIRECTION('center_axis',(0.,0.,-1.));
#17831=DIRECTION('ref_axis',(1.,0.,0.));
#17832=DIRECTION('center_axis',(0.,0.,1.));
#17833=DIRECTION('ref_axis',(0.,-1.,0.));
#17834=DIRECTION('',(-1.04972719113862E-16,0.857167300702115,0.515038074910049));
#17835=DIRECTION('center_axis',(0.,0.,1.));
#17836=DIRECTION('ref_axis',(1.,0.,0.));
#17837=DIRECTION('center_axis',(0.,0.,1.));
#17838=DIRECTION('ref_axis',(0.,-1.,0.));
#17839=DIRECTION('',(0.,0.,1.));
#17840=DIRECTION('',(0.,0.,1.));
#17841=DIRECTION('center_axis',(0.,0.,1.));
#17842=DIRECTION('ref_axis',(1.,0.,0.));
#17843=DIRECTION('center_axis',(0.,0.,1.));
#17844=DIRECTION('ref_axis',(0.,-1.,0.));
#17845=DIRECTION('',(-8.65956056235501E-17,0.707106781186554,0.707106781186541));
#17846=DIRECTION('center_axis',(0.,0.,-1.));
#17847=DIRECTION('ref_axis',(0.,-1.,0.));
#17848=DIRECTION('center_axis',(0.,0.,-1.));
#17849=DIRECTION('ref_axis',(0.,-1.,0.));
#17850=DIRECTION('center_axis',(0.,0.,1.));
#17851=DIRECTION('ref_axis',(1.,0.,0.));
#17852=DIRECTION('',(0.,1.,0.));
#17853=DIRECTION('',(-1.,0.,0.));
#17854=DIRECTION('',(0.,-1.,0.));
#17855=DIRECTION('center_axis',(0.,0.,-1.));
#17856=DIRECTION('ref_axis',(0.,-1.,0.));
#17857=DIRECTION('center_axis',(0.,0.,-1.));
#17858=DIRECTION('ref_axis',(0.,-1.,0.));
#17859=DIRECTION('',(0.,-1.,0.));
#17860=DIRECTION('center_axis',(0.,0.,-1.));
#17861=DIRECTION('ref_axis',(0.,-1.,0.));
#17862=DIRECTION('center_axis',(0.,0.,-1.));
#17863=DIRECTION('ref_axis',(0.,-1.,0.));
#17864=DIRECTION('',(0.,-1.,0.));
#17865=DIRECTION('',(0.,1.,0.));
#17866=DIRECTION('center_axis',(0.,0.,-1.));
#17867=DIRECTION('ref_axis',(0.,-1.,0.));
#17868=DIRECTION('center_axis',(0.,0.,-1.));
#17869=DIRECTION('ref_axis',(0.,-1.,0.));
#17870=DIRECTION('',(0.,1.,0.));
#17871=DIRECTION('',(-1.,0.,0.));
#17872=DIRECTION('',(0.,1.,0.));
#17873=DIRECTION('',(1.,0.,0.));
#17874=DIRECTION('',(0.,-1.,0.));
#17875=DIRECTION('',(-1.,0.,0.));
#17876=DIRECTION('',(0.,1.,0.));
#17877=DIRECTION('',(1.,0.,0.));
#17878=DIRECTION('',(0.,-1.,0.));
#17879=DIRECTION('',(-1.,0.,0.));
#17880=DIRECTION('',(0.,1.,0.));
#17881=DIRECTION('',(1.,0.,0.));
#17882=DIRECTION('',(0.,-1.,0.));
#17883=DIRECTION('',(-1.,0.,0.));
#17884=DIRECTION('',(0.,1.,0.));
#17885=DIRECTION('',(1.,0.,0.));
#17886=DIRECTION('',(0.,-1.,0.));
#17887=DIRECTION('',(-1.,0.,0.));
#17888=DIRECTION('',(0.,1.,0.));
#17889=DIRECTION('',(1.,0.,0.));
#17890=DIRECTION('',(0.,-1.,0.));
#17891=DIRECTION('',(-1.,0.,0.));
#17892=DIRECTION('',(0.,1.,0.));
#17893=DIRECTION('',(1.,0.,0.));
#17894=DIRECTION('',(0.,-1.,0.));
#17895=DIRECTION('center_axis',(0.,0.,1.));
#17896=DIRECTION('ref_axis',(0.,-1.,0.));
#17897=DIRECTION('',(-1.04972719113862E-16,0.857167300702115,0.515038074910049));
#17898=DIRECTION('center_axis',(0.,0.,1.));
#17899=DIRECTION('ref_axis',(1.,0.,0.));
#17900=DIRECTION('center_axis',(0.,0.,1.));
#17901=DIRECTION('ref_axis',(0.,-1.,0.));
#17902=DIRECTION('',(0.,0.,1.));
#17903=DIRECTION('center_axis',(0.,0.,1.));
#17904=DIRECTION('ref_axis',(1.,0.,0.));
#17905=DIRECTION('center_axis',(0.,0.,1.));
#17906=DIRECTION('ref_axis',(0.,-1.,0.));
#17907=DIRECTION('',(-8.65956056235503E-17,0.707106781186555,0.70710678118654));
#17908=DIRECTION('center_axis',(0.,-1.,0.));
#17909=DIRECTION('ref_axis',(-0.707106781186548,0.,0.707106781186548));
#17910=DIRECTION('center_axis',(0.,1.,0.));
#17911=DIRECTION('ref_axis',(-0.707106781186548,0.,0.707106781186548));
#17912=DIRECTION('center_axis',(0.,0.,1.));
#17913=DIRECTION('ref_axis',(0.,-1.,0.));
#17914=DIRECTION('',(-1.04972719113862E-16,0.857167300702115,0.515038074910049));
#17915=DIRECTION('center_axis',(0.,0.,1.));
#17916=DIRECTION('ref_axis',(1.,0.,0.));
#17917=DIRECTION('center_axis',(0.,0.,1.));
#17918=DIRECTION('ref_axis',(0.,-1.,0.));
#17919=DIRECTION('',(0.,0.,1.));
#17920=DIRECTION('center_axis',(0.,0.,1.));
#17921=DIRECTION('ref_axis',(1.,0.,0.));
#17922=DIRECTION('center_axis',(0.,0.,1.));
#17923=DIRECTION('ref_axis',(0.,-1.,0.));
#17924=DIRECTION('',(-8.65956056235501E-17,0.707106781186554,0.707106781186541));
#17925=DIRECTION('center_axis',(0.,1.,0.));
#17926=DIRECTION('ref_axis',(0.707106781186548,0.,0.707106781186548));
#17927=DIRECTION('center_axis',(0.,1.,0.));
#17928=DIRECTION('ref_axis',(0.707106781186548,0.,0.707106781186548));
#17929=DIRECTION('center_axis',(0.,0.,1.));
#17930=DIRECTION('ref_axis',(0.,-1.,0.));
#17931=DIRECTION('',(-1.04972719113862E-16,0.857167300702115,0.515038074910049));
#17932=DIRECTION('center_axis',(0.,0.,1.));
#17933=DIRECTION('ref_axis',(1.,0.,0.));
#17934=DIRECTION('center_axis',(0.,0.,1.));
#17935=DIRECTION('ref_axis',(0.,-1.,0.));
#17936=DIRECTION('',(0.,0.,1.));
#17937=DIRECTION('center_axis',(0.,0.,1.));
#17938=DIRECTION('ref_axis',(1.,0.,0.));
#17939=DIRECTION('center_axis',(0.,0.,1.));
#17940=DIRECTION('ref_axis',(0.,-1.,0.));
#17941=DIRECTION('',(-8.65956056235503E-17,0.707106781186555,0.70710678118654));
#17942=DIRECTION('center_axis',(0.,1.,0.));
#17943=DIRECTION('ref_axis',(-1.,0.,0.));
#17944=DIRECTION('',(0.85716730070211,0.515038074910058,-1.04972719113862E-16));
#17945=DIRECTION('center_axis',(0.,1.,0.));
#17946=DIRECTION('ref_axis',(1.,0.,0.));
#17947=DIRECTION('center_axis',(0.,1.,0.));
#17948=DIRECTION('ref_axis',(-1.,0.,0.));
#17949=DIRECTION('',(0.,1.,0.));
#17950=DIRECTION('center_axis',(0.,1.,0.));
#17951=DIRECTION('ref_axis',(1.,0.,0.));
#17952=DIRECTION('center_axis',(0.,1.,0.));
#17953=DIRECTION('ref_axis',(-1.,0.,0.));
#17954=DIRECTION('',(0.707106781186544,0.707106781186551,-8.6595605623549E-17));
#17955=DIRECTION('center_axis',(0.,-1.,0.));
#17956=DIRECTION('ref_axis',(1.,0.,0.));
#17957=DIRECTION('',(-0.85716730070211,-0.515038074910058,-1.04972719113862E-16));
#17958=DIRECTION('center_axis',(0.,-1.,0.));
#17959=DIRECTION('ref_axis',(1.,0.,0.));
#17960=DIRECTION('center_axis',(0.,-1.,0.));
#17961=DIRECTION('ref_axis',(1.,0.,0.));
#17962=DIRECTION('',(0.,-1.,0.));
#17963=DIRECTION('center_axis',(0.,-1.,0.));
#17964=DIRECTION('ref_axis',(1.,0.,0.));
#17965=DIRECTION('center_axis',(0.,-1.,0.));
#17966=DIRECTION('ref_axis',(1.,0.,0.));
#17967=DIRECTION('',(-0.707106781186546,-0.707106781186549,-8.65956056235491E-17));
#17968=DIRECTION('center_axis',(0.,1.,0.));
#17969=DIRECTION('ref_axis',(1.,0.,0.));
#17970=DIRECTION('center_axis',(0.,1.,0.));
#17971=DIRECTION('ref_axis',(-1.,0.,0.));
#17972=DIRECTION('',(0.85716730070211,0.515038074910058,-1.04972719113862E-16));
#17973=DIRECTION('center_axis',(0.,1.,0.));
#17974=DIRECTION('ref_axis',(1.,0.,0.));
#17975=DIRECTION('center_axis',(0.,1.,0.));
#17976=DIRECTION('ref_axis',(-1.,0.,0.));
#17977=DIRECTION('',(0.,1.,0.));
#17978=DIRECTION('center_axis',(0.,1.,0.));
#17979=DIRECTION('ref_axis',(1.,0.,0.));
#17980=DIRECTION('center_axis',(0.,1.,0.));
#17981=DIRECTION('ref_axis',(-1.,0.,0.));
#17982=DIRECTION('',(0.707106781186546,0.707106781186549,-8.65956056235491E-17));
#17983=DIRECTION('center_axis',(0.,-1.,0.));
#17984=DIRECTION('ref_axis',(1.,0.,0.));
#17985=DIRECTION('',(-0.85716730070211,-0.515038074910058,-1.04972719113862E-16));
#17986=DIRECTION('center_axis',(0.,-1.,0.));
#17987=DIRECTION('ref_axis',(1.,0.,0.));
#17988=DIRECTION('center_axis',(0.,-1.,0.));
#17989=DIRECTION('ref_axis',(1.,0.,0.));
#17990=DIRECTION('',(0.,-1.,0.));
#17991=DIRECTION('center_axis',(0.,-1.,0.));
#17992=DIRECTION('ref_axis',(1.,0.,0.));
#17993=DIRECTION('center_axis',(0.,-1.,0.));
#17994=DIRECTION('ref_axis',(1.,0.,0.));
#17995=DIRECTION('',(-0.707106781186544,-0.707106781186551,-8.65956056235489E-17));
#17996=DIRECTION('center_axis',(0.,1.,0.));
#17997=DIRECTION('ref_axis',(1.,0.,0.));
#17998=DIRECTION('center_axis',(0.,1.,0.));
#17999=DIRECTION('ref_axis',(-1.,0.,0.));
#18000=DIRECTION('',(0.85716730070211,0.515038074910058,-1.04972719113862E-16));
#18001=DIRECTION('center_axis',(0.,1.,0.));
#18002=DIRECTION('ref_axis',(1.,0.,0.));
#18003=DIRECTION('center_axis',(0.,1.,0.));
#18004=DIRECTION('ref_axis',(-1.,0.,0.));
#18005=DIRECTION('',(0.,1.,0.));
#18006=DIRECTION('center_axis',(0.,1.,0.));
#18007=DIRECTION('ref_axis',(1.,0.,0.));
#18008=DIRECTION('center_axis',(0.,1.,0.));
#18009=DIRECTION('ref_axis',(-1.,0.,0.));
#18010=DIRECTION('',(0.707106781186544,0.707106781186551,-8.65956056235489E-17));
#18011=DIRECTION('center_axis',(0.,-1.,0.));
#18012=DIRECTION('ref_axis',(1.,0.,0.));
#18013=DIRECTION('',(-0.85716730070211,-0.515038074910058,-1.04972719113862E-16));
#18014=DIRECTION('center_axis',(0.,-1.,0.));
#18015=DIRECTION('ref_axis',(1.,0.,0.));
#18016=DIRECTION('center_axis',(0.,-1.,0.));
#18017=DIRECTION('ref_axis',(1.,0.,0.));
#18018=DIRECTION('',(0.,-1.,0.));
#18019=DIRECTION('center_axis',(0.,-1.,0.));
#18020=DIRECTION('ref_axis',(1.,0.,0.));
#18021=DIRECTION('center_axis',(0.,-1.,0.));
#18022=DIRECTION('ref_axis',(1.,0.,0.));
#18023=DIRECTION('',(-0.707106781186544,-0.707106781186551,-8.6595605623549E-17));
#18024=DIRECTION('center_axis',(0.,1.,0.));
#18025=DIRECTION('ref_axis',(1.,0.,0.));
#18026=DIRECTION('center_axis',(0.,1.,0.));
#18027=DIRECTION('ref_axis',(-1.,0.,0.));
#18028=DIRECTION('',(0.85716730070211,0.515038074910058,-1.04972719113862E-16));
#18029=DIRECTION('center_axis',(0.,1.,0.));
#18030=DIRECTION('ref_axis',(1.,0.,0.));
#18031=DIRECTION('center_axis',(0.,1.,0.));
#18032=DIRECTION('ref_axis',(-1.,0.,0.));
#18033=DIRECTION('',(0.,1.,0.));
#18034=DIRECTION('center_axis',(0.,1.,0.));
#18035=DIRECTION('ref_axis',(1.,0.,0.));
#18036=DIRECTION('center_axis',(0.,1.,0.));
#18037=DIRECTION('ref_axis',(-1.,0.,0.));
#18038=DIRECTION('',(0.707106781186544,0.707106781186551,-8.65956056235489E-17));
#18039=DIRECTION('center_axis',(0.,-1.,0.));
#18040=DIRECTION('ref_axis',(1.,0.,0.));
#18041=DIRECTION('',(-0.85716730070211,-0.515038074910058,-1.04972719113862E-16));
#18042=DIRECTION('center_axis',(0.,-1.,0.));
#18043=DIRECTION('ref_axis',(1.,0.,0.));
#18044=DIRECTION('center_axis',(0.,-1.,0.));
#18045=DIRECTION('ref_axis',(1.,0.,0.));
#18046=DIRECTION('',(0.,-1.,0.));
#18047=DIRECTION('center_axis',(0.,-1.,0.));
#18048=DIRECTION('ref_axis',(1.,0.,0.));
#18049=DIRECTION('center_axis',(0.,-1.,0.));
#18050=DIRECTION('ref_axis',(1.,0.,0.));
#18051=DIRECTION('',(-0.707106781186544,-0.707106781186551,-8.6595605623549E-17));
#18052=DIRECTION('center_axis',(0.,1.,0.));
#18053=DIRECTION('ref_axis',(1.,0.,0.));
#18054=DIRECTION('center_axis',(-1.,0.,0.));
#18055=DIRECTION('ref_axis',(0.,-1.,0.));
#18056=DIRECTION('',(-0.515038074910058,0.85716730070211,-1.04972719113862E-16));
#18057=DIRECTION('center_axis',(-1.,0.,0.));
#18058=DIRECTION('ref_axis',(0.,0.,1.));
#18059=DIRECTION('center_axis',(-1.,0.,0.));
#18060=DIRECTION('ref_axis',(0.,-1.,0.));
#18061=DIRECTION('',(-1.,0.,0.));
#18062=DIRECTION('center_axis',(-1.,0.,0.));
#18063=DIRECTION('ref_axis',(0.,0.,1.));
#18064=DIRECTION('center_axis',(-1.,0.,0.));
#18065=DIRECTION('ref_axis',(0.,-1.,0.));
#18066=DIRECTION('',(-0.707106781186546,0.707106781186549,-8.65956056235496E-17));
#18067=DIRECTION('center_axis',(-1.,0.,0.));
#18068=DIRECTION('ref_axis',(0.,-1.,0.));
#18069=DIRECTION('',(-0.515038074910058,0.85716730070211,-1.04972719113862E-16));
#18070=DIRECTION('center_axis',(-1.,0.,0.));
#18071=DIRECTION('ref_axis',(0.,0.,1.));
#18072=DIRECTION('center_axis',(-1.,0.,0.));
#18073=DIRECTION('ref_axis',(0.,-1.,0.));
#18074=DIRECTION('',(-1.,0.,0.));
#18075=DIRECTION('center_axis',(-1.,0.,0.));
#18076=DIRECTION('ref_axis',(0.,0.,1.));
#18077=DIRECTION('center_axis',(-1.,0.,0.));
#18078=DIRECTION('ref_axis',(0.,-1.,0.));
#18079=DIRECTION('',(-0.707106781186548,0.707106781186547,-8.65956056235493E-17));
#18080=DIRECTION('center_axis',(-1.,0.,0.));
#18081=DIRECTION('ref_axis',(0.,-1.,0.));
#18082=DIRECTION('',(-0.515038074910058,0.85716730070211,-1.04972719113862E-16));
#18083=DIRECTION('center_axis',(-1.,0.,0.));
#18084=DIRECTION('ref_axis',(0.,0.,1.));
#18085=DIRECTION('center_axis',(-1.,0.,0.));
#18086=DIRECTION('ref_axis',(0.,-1.,0.));
#18087=DIRECTION('',(-1.,0.,0.));
#18088=DIRECTION('center_axis',(-1.,0.,0.));
#18089=DIRECTION('ref_axis',(0.,0.,1.));
#18090=DIRECTION('center_axis',(-1.,0.,0.));
#18091=DIRECTION('ref_axis',(0.,-1.,0.));
#18092=DIRECTION('',(-0.707106781186546,0.707106781186549,-8.65956056235496E-17));
#18093=DIRECTION('center_axis',(-1.,0.,0.));
#18094=DIRECTION('ref_axis',(0.,-1.,0.));
#18095=DIRECTION('',(-0.515038074910058,0.85716730070211,-1.04972719113862E-16));
#18096=DIRECTION('center_axis',(-1.,0.,0.));
#18097=DIRECTION('ref_axis',(0.,0.,1.));
#18098=DIRECTION('center_axis',(-1.,0.,0.));
#18099=DIRECTION('ref_axis',(0.,-1.,0.));
#18100=DIRECTION('',(-1.,0.,0.));
#18101=DIRECTION('',(-1.,0.,0.));
#18102=DIRECTION('center_axis',(-1.,0.,0.));
#18103=DIRECTION('ref_axis',(0.,0.,1.));
#18104=DIRECTION('center_axis',(-1.,0.,0.));
#18105=DIRECTION('ref_axis',(0.,-1.,0.));
#18106=DIRECTION('',(-0.707106781186548,0.707106781186547,-8.65956056235493E-17));
#18107=DIRECTION('center_axis',(0.,0.,-1.));
#18108=DIRECTION('ref_axis',(0.,1.,0.));
#18109=DIRECTION('center_axis',(0.,0.,-1.));
#18110=DIRECTION('ref_axis',(0.,1.,0.));
#18111=DIRECTION('',(0.,0.,-1.));
#18112=DIRECTION('center_axis',(0.,0.,-1.));
#18113=DIRECTION('ref_axis',(1.,0.,0.));
#18114=DIRECTION('center_axis',(0.,0.,-1.));
#18115=DIRECTION('ref_axis',(0.,1.,0.));
#18116=DIRECTION('',(-8.65956056235492E-17,-0.707106781186547,-0.707106781186548));
#18117=DIRECTION('center_axis',(0.,0.,1.));
#18118=DIRECTION('ref_axis',(0.,1.,0.));
#18119=DIRECTION('center_axis',(0.,0.,-1.));
#18120=DIRECTION('ref_axis',(0.,1.,0.));
#18121=DIRECTION('center_axis',(0.,0.,-1.));
#18122=DIRECTION('ref_axis',(0.,1.,0.));
#18123=DIRECTION('',(0.,0.,-1.));
#18124=DIRECTION('center_axis',(0.,0.,-1.));
#18125=DIRECTION('ref_axis',(1.,0.,0.));
#18126=DIRECTION('center_axis',(0.,0.,-1.));
#18127=DIRECTION('ref_axis',(0.,1.,0.));
#18128=DIRECTION('',(-8.6595605623549E-17,-0.707106781186544,-0.707106781186551));
#18129=DIRECTION('center_axis',(0.,0.,1.));
#18130=DIRECTION('ref_axis',(0.,1.,0.));
#18131=DIRECTION('center_axis',(0.,0.,-1.));
#18132=DIRECTION('ref_axis',(0.,1.,0.));
#18133=DIRECTION('center_axis',(0.,0.,-1.));
#18134=DIRECTION('ref_axis',(0.,1.,0.));
#18135=DIRECTION('',(0.,0.,-1.));
#18136=DIRECTION('center_axis',(0.,0.,-1.));
#18137=DIRECTION('ref_axis',(1.,0.,0.));
#18138=DIRECTION('center_axis',(0.,0.,-1.));
#18139=DIRECTION('ref_axis',(0.,1.,0.));
#18140=DIRECTION('',(-8.65956056235492E-17,-0.707106781186547,-0.707106781186548));
#18141=DIRECTION('center_axis',(0.,0.,1.));
#18142=DIRECTION('ref_axis',(0.,1.,0.));
#18143=DIRECTION('center_axis',(0.,0.,-1.));
#18144=DIRECTION('ref_axis',(0.,1.,0.));
#18145=DIRECTION('center_axis',(0.,0.,-1.));
#18146=DIRECTION('ref_axis',(0.,1.,0.));
#18147=DIRECTION('',(0.,0.,-1.));
#18148=DIRECTION('center_axis',(0.,0.,-1.));
#18149=DIRECTION('ref_axis',(1.,0.,0.));
#18150=DIRECTION('center_axis',(0.,0.,-1.));
#18151=DIRECTION('ref_axis',(0.,1.,0.));
#18152=DIRECTION('',(-8.6595605623549E-17,-0.707106781186544,-0.707106781186551));
#18153=DIRECTION('center_axis',(0.,0.,1.));
#18154=DIRECTION('ref_axis',(0.,1.,0.));
#18155=DIRECTION('center_axis',(-1.,0.,0.));
#18156=DIRECTION('ref_axis',(0.,0.,-1.));
#18157=DIRECTION('',(0.,0.,1.));
#18158=DIRECTION('',(0.,-1.,0.));
#18159=DIRECTION('center_axis',(0.,0.,-1.));
#18160=DIRECTION('ref_axis',(1.,0.,0.));
#18161=DIRECTION('',(-1.,0.,0.));
#18162=DIRECTION('center_axis',(0.,0.,1.));
#18163=DIRECTION('ref_axis',(-1.,0.,0.));
#18164=DIRECTION('',(0.,-1.,0.));
#18165=DIRECTION('',(1.,0.,0.));
#18166=DIRECTION('center_axis',(1.,0.,0.));
#18167=DIRECTION('ref_axis',(0.,0.,1.));
#18168=DIRECTION('',(0.,0.,-1.));
#18169=DIRECTION('',(0.,-1.,0.));
#18170=DIRECTION('center_axis',(0.,0.,-1.));
#18171=DIRECTION('ref_axis',(1.,0.,0.));
#18172=DIRECTION('',(-1.,0.,0.));
#18173=DIRECTION('center_axis',(0.,-1.,0.));
#18174=DIRECTION('ref_axis',(0.,0.,-1.));
#18175=DIRECTION('center_axis',(0.,1.,0.));
#18176=DIRECTION('ref_axis',(-0.707106781186548,0.,-0.707106781186547));
#18177=DIRECTION('',(1.,0.,0.));
#18178=DIRECTION('',(0.,0.,1.));
#18179=DIRECTION('',(1.,0.,0.));
#18180=DIRECTION('',(0.,0.,-1.));
#18181=DIRECTION('',(1.,0.,0.));
#18182=DIRECTION('center_axis',(0.,1.,0.));
#18183=DIRECTION('ref_axis',(0.707106781186549,0.,-0.707106781186546));
#18184=DIRECTION('center_axis',(0.,1.,0.));
#18185=DIRECTION('ref_axis',(0.,0.,1.));
#18186=DIRECTION('center_axis',(0.,0.,-1.));
#18187=DIRECTION('ref_axis',(-1.,0.,0.));
#18188=DIRECTION('',(1.,0.,0.));
#18189=DIRECTION('',(0.,1.,0.));
#18190=DIRECTION('',(1.,0.,0.));
#18191=DIRECTION('center_axis',(0.,1.,0.));
#18192=DIRECTION('ref_axis',(1.,0.,0.));
#18193=DIRECTION('',(0.,0.,-1.));
#18194=DIRECTION('',(-1.,0.,0.));
#18195=DIRECTION('center_axis',(-1.,0.,0.));
#18196=DIRECTION('ref_axis',(0.,0.,1.));
#18197=DIRECTION('',(0.,1.,0.));
#18198=DIRECTION('',(0.,0.,-1.));
#18199=DIRECTION('',(0.,-1.,0.));
#18200=DIRECTION('center_axis',(0.,0.,1.));
#18201=DIRECTION('ref_axis',(1.,0.,0.));
#18202=DIRECTION('center_axis',(1.,0.,0.));
#18203=DIRECTION('ref_axis',(0.,0.,-1.));
#18204=DIRECTION('',(0.,1.,0.));
#18205=DIRECTION('',(0.,0.,1.));
#18206=DIRECTION('',(0.,1.,0.));
#18207=DIRECTION('',(0.,0.,1.));
#18208=DIRECTION('',(0.,-1.,0.));
#18209=DIRECTION('center_axis',(0.,0.,-1.));
#18210=DIRECTION('ref_axis',(-1.,0.,0.));
#18211=DIRECTION('',(1.,0.,0.));
#18212=DIRECTION('',(1.,0.,0.));
#18213=DIRECTION('center_axis',(0.,1.,0.));
#18214=DIRECTION('ref_axis',(1.,0.,0.));
#18215=DIRECTION('center_axis',(0.,1.,0.));
#18216=DIRECTION('ref_axis',(1.,0.,0.));
#18217=DIRECTION('center_axis',(0.,-1.,0.));
#18218=DIRECTION('ref_axis',(1.,0.,0.));
#18219=DIRECTION('',(0.,1.,0.));
#18220=DIRECTION('center_axis',(0.,1.,0.));
#18221=DIRECTION('ref_axis',(1.,0.,0.));
#18222=DIRECTION('center_axis',(0.,1.,0.));
#18223=DIRECTION('ref_axis',(1.,0.,0.));
#18224=DIRECTION('',(0.,1.,0.));
#18225=DIRECTION('center_axis',(0.,-1.,0.));
#18226=DIRECTION('ref_axis',(1.,0.,0.));
#18227=DIRECTION('center_axis',(0.,1.,0.));
#18228=DIRECTION('ref_axis',(0.,0.,1.));
#18229=DIRECTION('center_axis',(0.,-1.,0.));
#18230=DIRECTION('ref_axis',(0.707106781186549,0.,-0.707106781186546));
#18231=DIRECTION('',(-1.,0.,0.));
#18232=DIRECTION('',(0.,0.,1.));
#18233=DIRECTION('',(-1.,0.,0.));
#18234=DIRECTION('',(0.,0.,-1.));
#18235=DIRECTION('',(-1.,0.,0.));
#18236=DIRECTION('center_axis',(0.,-1.,0.));
#18237=DIRECTION('ref_axis',(-0.707106781186548,0.,-0.707106781186547));
#18238=DIRECTION('center_axis',(0.,-1.,0.));
#18239=DIRECTION('ref_axis',(1.,0.,0.));
#18240=DIRECTION('center_axis',(-1.,0.,0.));
#18241=DIRECTION('ref_axis',(0.,0.,1.));
#18242=DIRECTION('',(0.,-1.,0.));
#18243=DIRECTION('',(0.,-1.,0.));
#18244=DIRECTION('center_axis',(1.,0.,0.));
#18245=DIRECTION('ref_axis',(0.,0.,-1.));
#18246=DIRECTION('',(0.,1.,0.));
#18247=DIRECTION('',(0.,1.,0.));
#18248=DIRECTION('center_axis',(0.,0.,1.));
#18249=DIRECTION('ref_axis',(1.,0.,0.));
#18250=DIRECTION('center_axis',(0.,0.,-1.));
#18251=DIRECTION('ref_axis',(-1.,0.,0.));
#18252=DIRECTION('',(0.,1.,0.));
#18253=DIRECTION('center_axis',(0.,0.,-1.));
#18254=DIRECTION('ref_axis',(-1.,0.,0.));
#18255=DIRECTION('',(0.,-1.,0.));
#18256=DIRECTION('center_axis',(0.,-1.,0.));
#18257=DIRECTION('ref_axis',(-1.,0.,0.));
#18258=DIRECTION('',(0.,0.,-1.));
#18259=DIRECTION('',(-1.,0.,0.));
#18260=DIRECTION('',(0.,0.,-1.));
#18261=DIRECTION('center_axis',(1.,0.,0.));
#18262=DIRECTION('ref_axis',(0.,-1.,0.));
#18263=DIRECTION('',(0.,0.,-1.));
#18264=DIRECTION('',(0.,-1.,0.));
#18265=DIRECTION('center_axis',(0.,1.,0.));
#18266=DIRECTION('ref_axis',(1.,0.,0.));
#18267=DIRECTION('',(0.,0.,-1.));
#18268=DIRECTION('',(1.,0.,0.));
#18269=DIRECTION('center_axis',(-1.,0.,0.));
#18270=DIRECTION('ref_axis',(0.,1.,0.));
#18271=DIRECTION('',(0.,1.,0.));
#18272=DIRECTION('center_axis',(0.,0.,-1.));
#18273=DIRECTION('ref_axis',(-1.,0.,0.));
#18274=DIRECTION('center_axis',(0.,-1.,0.));
#18275=DIRECTION('ref_axis',(-1.,0.,0.));
#18276=DIRECTION('',(0.,0.,-1.));
#18277=DIRECTION('',(-1.,0.,0.));
#18278=DIRECTION('',(0.,0.,-1.));
#18279=DIRECTION('center_axis',(1.,0.,0.));
#18280=DIRECTION('ref_axis',(0.,-1.,0.));
#18281=DIRECTION('',(0.,0.,-1.));
#18282=DIRECTION('',(0.,-1.,0.));
#18283=DIRECTION('center_axis',(0.,1.,0.));
#18284=DIRECTION('ref_axis',(1.,0.,0.));
#18285=DIRECTION('',(0.,0.,-1.));
#18286=DIRECTION('',(1.,0.,0.));
#18287=DIRECTION('center_axis',(-1.,0.,0.));
#18288=DIRECTION('ref_axis',(0.,1.,0.));
#18289=DIRECTION('',(0.,1.,0.));
#18290=DIRECTION('center_axis',(0.,0.,-1.));
#18291=DIRECTION('ref_axis',(-1.,0.,0.));
#18292=DIRECTION('center_axis',(0.,-1.,0.));
#18293=DIRECTION('ref_axis',(-1.,0.,0.));
#18294=DIRECTION('',(0.,0.,-1.));
#18295=DIRECTION('',(-1.,0.,0.));
#18296=DIRECTION('',(0.,0.,-1.));
#18297=DIRECTION('center_axis',(1.,0.,0.));
#18298=DIRECTION('ref_axis',(0.,-1.,0.));
#18299=DIRECTION('',(0.,0.,-1.));
#18300=DIRECTION('',(0.,-1.,0.));
#18301=DIRECTION('center_axis',(0.,1.,0.));
#18302=DIRECTION('ref_axis',(1.,0.,0.));
#18303=DIRECTION('',(0.,0.,-1.));
#18304=DIRECTION('',(1.,0.,0.));
#18305=DIRECTION('center_axis',(-1.,0.,0.));
#18306=DIRECTION('ref_axis',(0.,1.,0.));
#18307=DIRECTION('',(0.,1.,0.));
#18308=DIRECTION('center_axis',(0.,0.,-1.));
#18309=DIRECTION('ref_axis',(-1.,0.,0.));
#18310=DIRECTION('center_axis',(0.,-1.,0.));
#18311=DIRECTION('ref_axis',(-1.,0.,0.));
#18312=DIRECTION('',(0.,0.,-1.));
#18313=DIRECTION('',(-1.,0.,0.));
#18314=DIRECTION('',(0.,0.,-1.));
#18315=DIRECTION('center_axis',(1.,0.,0.));
#18316=DIRECTION('ref_axis',(0.,-1.,0.));
#18317=DIRECTION('',(0.,0.,-1.));
#18318=DIRECTION('',(0.,-1.,0.));
#18319=DIRECTION('center_axis',(0.,1.,0.));
#18320=DIRECTION('ref_axis',(1.,0.,0.));
#18321=DIRECTION('',(0.,0.,-1.));
#18322=DIRECTION('',(1.,0.,0.));
#18323=DIRECTION('center_axis',(-1.,0.,0.));
#18324=DIRECTION('ref_axis',(0.,1.,0.));
#18325=DIRECTION('',(0.,1.,0.));
#18326=DIRECTION('center_axis',(0.,0.,-1.));
#18327=DIRECTION('ref_axis',(-1.,0.,0.));
#18328=DIRECTION('center_axis',(0.,-1.,0.));
#18329=DIRECTION('ref_axis',(-1.,0.,0.));
#18330=DIRECTION('',(0.,0.,-1.));
#18331=DIRECTION('',(-1.,0.,0.));
#18332=DIRECTION('',(0.,0.,-1.));
#18333=DIRECTION('center_axis',(1.,0.,0.));
#18334=DIRECTION('ref_axis',(0.,-1.,0.));
#18335=DIRECTION('',(0.,0.,-1.));
#18336=DIRECTION('',(0.,-1.,0.));
#18337=DIRECTION('center_axis',(0.,1.,0.));
#18338=DIRECTION('ref_axis',(1.,0.,0.));
#18339=DIRECTION('',(0.,0.,-1.));
#18340=DIRECTION('',(1.,0.,0.));
#18341=DIRECTION('center_axis',(-1.,0.,0.));
#18342=DIRECTION('ref_axis',(0.,1.,0.));
#18343=DIRECTION('',(0.,1.,0.));
#18344=DIRECTION('center_axis',(0.,0.,-1.));
#18345=DIRECTION('ref_axis',(-1.,0.,0.));
#18346=DIRECTION('center_axis',(0.,-1.,0.));
#18347=DIRECTION('ref_axis',(-1.,0.,0.));
#18348=DIRECTION('',(0.,0.,-1.));
#18349=DIRECTION('',(-1.,0.,0.));
#18350=DIRECTION('',(0.,0.,-1.));
#18351=DIRECTION('center_axis',(1.,0.,0.));
#18352=DIRECTION('ref_axis',(0.,-1.,0.));
#18353=DIRECTION('',(0.,0.,-1.));
#18354=DIRECTION('',(0.,-1.,0.));
#18355=DIRECTION('center_axis',(0.,1.,0.));
#18356=DIRECTION('ref_axis',(1.,0.,0.));
#18357=DIRECTION('',(0.,0.,-1.));
#18358=DIRECTION('',(1.,0.,0.));
#18359=DIRECTION('center_axis',(-1.,0.,0.));
#18360=DIRECTION('ref_axis',(0.,1.,0.));
#18361=DIRECTION('',(0.,1.,0.));
#18362=DIRECTION('center_axis',(0.,0.,-1.));
#18363=DIRECTION('ref_axis',(-1.,0.,0.));
#18364=DIRECTION('center_axis',(-1.,0.,0.));
#18365=DIRECTION('ref_axis',(0.,0.,1.));
#18366=DIRECTION('',(-1.,0.,0.));
#18367=DIRECTION('center_axis',(-1.,0.,0.));
#18368=DIRECTION('ref_axis',(0.,0.,1.));
#18369=DIRECTION('center_axis',(1.,0.,0.));
#18370=DIRECTION('ref_axis',(0.,0.,-1.));
#18371=DIRECTION('center_axis',(-1.,0.,0.));
#18372=DIRECTION('ref_axis',(0.,0.,1.));
#18373=DIRECTION('center_axis',(-1.,0.,0.));
#18374=DIRECTION('ref_axis',(0.,0.,1.));
#18375=DIRECTION('',(-1.,0.,0.));
#18376=DIRECTION('center_axis',(-1.,0.,0.));
#18377=DIRECTION('ref_axis',(0.,0.,1.));
#18378=DIRECTION('center_axis',(-1.,0.,0.));
#18379=DIRECTION('ref_axis',(0.,0.,1.));
#18380=DIRECTION('center_axis',(-1.,0.,0.));
#18381=DIRECTION('ref_axis',(0.,0.,1.));
#18382=DIRECTION('center_axis',(-1.,0.,0.));
#18383=DIRECTION('ref_axis',(0.,0.,1.));
#18384=DIRECTION('',(-1.,0.,0.));
#18385=DIRECTION('center_axis',(-1.,0.,0.));
#18386=DIRECTION('ref_axis',(0.,0.,1.));
#18387=DIRECTION('center_axis',(-1.,0.,0.));
#18388=DIRECTION('ref_axis',(0.,0.,1.));
#18389=DIRECTION('center_axis',(-1.,0.,0.));
#18390=DIRECTION('ref_axis',(0.,0.,1.));
#18391=DIRECTION('center_axis',(-1.,0.,0.));
#18392=DIRECTION('ref_axis',(0.,0.,1.));
#18393=DIRECTION('',(-1.,0.,0.));
#18394=DIRECTION('',(-1.,0.,0.));
#18395=DIRECTION('center_axis',(-1.,0.,0.));
#18396=DIRECTION('ref_axis',(0.,0.,1.));
#18397=DIRECTION('center_axis',(1.,0.,0.));
#18398=DIRECTION('ref_axis',(0.,0.,-1.));
#18399=DIRECTION('center_axis',(-1.,0.,0.));
#18400=DIRECTION('ref_axis',(0.,0.,1.));
#18401=DIRECTION('center_axis',(-1.,0.,0.));
#18402=DIRECTION('ref_axis',(0.,0.,1.));
#18403=DIRECTION('',(-1.,0.,0.));
#18404=DIRECTION('center_axis',(-1.,0.,0.));
#18405=DIRECTION('ref_axis',(0.,0.,1.));
#18406=DIRECTION('center_axis',(1.,0.,0.));
#18407=DIRECTION('ref_axis',(0.,0.,-1.));
#18408=DIRECTION('center_axis',(-1.,0.,0.));
#18409=DIRECTION('ref_axis',(0.,0.,1.));
#18410=DIRECTION('center_axis',(-1.,0.,0.));
#18411=DIRECTION('ref_axis',(0.,0.,1.));
#18412=DIRECTION('',(-1.,0.,0.));
#18413=DIRECTION('center_axis',(-1.,0.,0.));
#18414=DIRECTION('ref_axis',(0.,0.,1.));
#18415=DIRECTION('center_axis',(-1.,0.,0.));
#18416=DIRECTION('ref_axis',(0.,0.,1.));
#18417=DIRECTION('center_axis',(-1.,0.,0.));
#18418=DIRECTION('ref_axis',(0.,0.,1.));
#18419=DIRECTION('center_axis',(-1.,0.,0.));
#18420=DIRECTION('ref_axis',(0.,0.,1.));
#18421=DIRECTION('',(-1.,0.,0.));
#18422=DIRECTION('center_axis',(0.,1.,0.));
#18423=DIRECTION('ref_axis',(0.,0.,1.));
#18424=DIRECTION('',(0.,1.,0.));
#18425=DIRECTION('center_axis',(0.,1.,0.));
#18426=DIRECTION('ref_axis',(1.,0.,0.));
#18427=DIRECTION('center_axis',(0.,1.,0.));
#18428=DIRECTION('ref_axis',(0.,0.,1.));
#18429=DIRECTION('center_axis',(0.,1.,0.));
#18430=DIRECTION('ref_axis',(1.,0.,0.));
#18431=DIRECTION('center_axis',(0.,1.,0.));
#18432=DIRECTION('ref_axis',(0.,0.,1.));
#18433=DIRECTION('',(0.,1.,0.));
#18434=DIRECTION('center_axis',(0.,1.,0.));
#18435=DIRECTION('ref_axis',(1.,0.,0.));
#18436=DIRECTION('center_axis',(0.,1.,0.));
#18437=DIRECTION('ref_axis',(0.,0.,1.));
#18438=DIRECTION('center_axis',(0.,1.,0.));
#18439=DIRECTION('ref_axis',(1.,0.,0.));
#18440=DIRECTION('center_axis',(0.,1.,0.));
#18441=DIRECTION('ref_axis',(0.,0.,1.));
#18442=DIRECTION('',(0.,1.,0.));
#18443=DIRECTION('center_axis',(0.,1.,0.));
#18444=DIRECTION('ref_axis',(1.,0.,0.));
#18445=DIRECTION('center_axis',(0.,1.,0.));
#18446=DIRECTION('ref_axis',(0.,0.,1.));
#18447=DIRECTION('',(-8.65956056235489E-17,0.70710678118655,-0.707106781186544));
#18448=DIRECTION('center_axis',(0.,1.,0.));
#18449=DIRECTION('ref_axis',(1.,0.,0.));
#18450=DIRECTION('center_axis',(0.,1.,0.));
#18451=DIRECTION('ref_axis',(0.707106781186549,0.,-0.707106781186546));
#18452=DIRECTION('center_axis',(0.,1.,0.));
#18453=DIRECTION('ref_axis',(-0.707106781186548,0.,-0.707106781186547));
#18454=DIRECTION('axis',(0.,0.,1.));
#18455=DIRECTION('refdir',(1.,0.,0.));
#18456=DIRECTION('center_axis',(0.,-1.,0.));
#18457=DIRECTION('ref_axis',(1.,0.,0.));
#18458=DIRECTION('center_axis',(0.,1.,0.));
#18459=DIRECTION('ref_axis',(1.,0.,0.));
#18460=DIRECTION('',(0.707106781186546,0.707106781186549,8.65956056235491E-17));
#18461=DIRECTION('center_axis',(0.,-1.,0.));
#18462=DIRECTION('ref_axis',(1.,0.,0.));
#18463=DIRECTION('center_axis',(0.,1.,0.));
#18464=DIRECTION('ref_axis',(1.,0.,0.));
#18465=DIRECTION('',(0.,-1.,0.));
#18466=DIRECTION('center_axis',(0.,-1.,0.));
#18467=DIRECTION('ref_axis',(1.,0.,0.));
#18468=DIRECTION('center_axis',(0.,1.,0.));
#18469=DIRECTION('ref_axis',(1.,0.,0.));
#18470=DIRECTION('center_axis',(0.,-1.,0.));
#18471=DIRECTION('ref_axis',(0.,0.,1.));
#18472=DIRECTION('center_axis',(0.,1.,0.));
#18473=DIRECTION('ref_axis',(1.,0.,0.));
#18474=DIRECTION('center_axis',(0.,1.,0.));
#18475=DIRECTION('ref_axis',(1.,0.,0.));
#18476=DIRECTION('center_axis',(0.,-1.,0.));
#18477=DIRECTION('ref_axis',(1.,0.,0.));
#18478=DIRECTION('center_axis',(0.,1.,0.));
#18479=DIRECTION('ref_axis',(1.,0.,0.));
#18480=DIRECTION('center_axis',(0.,1.,0.));
#18481=DIRECTION('ref_axis',(1.,0.,0.));
#18482=DIRECTION('center_axis',(0.,-1.,0.));
#18483=DIRECTION('ref_axis',(1.,0.,0.));
#18484=DIRECTION('center_axis',(0.,1.,0.));
#18485=DIRECTION('ref_axis',(1.,0.,0.));
#18486=DIRECTION('center_axis',(0.,1.,0.));
#18487=DIRECTION('ref_axis',(1.,0.,0.));
#18488=DIRECTION('center_axis',(0.,-1.,0.));
#18489=DIRECTION('ref_axis',(1.,0.,0.));
#18490=DIRECTION('center_axis',(0.,1.,0.));
#18491=DIRECTION('ref_axis',(1.,0.,0.));
#18492=DIRECTION('center_axis',(0.,1.,0.));
#18493=DIRECTION('ref_axis',(1.,0.,0.));
#18494=DIRECTION('center_axis',(0.,-1.,0.));
#18495=DIRECTION('ref_axis',(1.,0.,0.));
#18496=DIRECTION('center_axis',(0.,1.,0.));
#18497=DIRECTION('ref_axis',(1.,0.,0.));
#18498=DIRECTION('center_axis',(0.,1.,0.));
#18499=DIRECTION('ref_axis',(1.,0.,0.));
#18500=DIRECTION('center_axis',(0.,-1.,0.));
#18501=DIRECTION('ref_axis',(1.,0.,0.));
#18502=DIRECTION('center_axis',(0.,1.,0.));
#18503=DIRECTION('ref_axis',(-1.,0.,0.));
#18504=DIRECTION('center_axis',(0.,-1.,0.));
#18505=DIRECTION('ref_axis',(-1.,0.,0.));
#18506=DIRECTION('center_axis',(0.,1.,0.));
#18507=DIRECTION('ref_axis',(-1.,0.,0.));
#18508=DIRECTION('center_axis',(0.,1.,0.));
#18509=DIRECTION('ref_axis',(-1.,0.,0.));
#18510=DIRECTION('center_axis',(0.,-1.,0.));
#18511=DIRECTION('ref_axis',(-1.,0.,0.));
#18512=DIRECTION('center_axis',(0.,1.,0.));
#18513=DIRECTION('ref_axis',(-1.,0.,0.));
#18514=DIRECTION('center_axis',(0.,1.,0.));
#18515=DIRECTION('ref_axis',(-1.,0.,0.));
#18516=DIRECTION('center_axis',(0.,-1.,0.));
#18517=DIRECTION('ref_axis',(-1.,0.,0.));
#18518=DIRECTION('center_axis',(0.,1.,0.));
#18519=DIRECTION('ref_axis',(-1.,0.,0.));
#18520=DIRECTION('center_axis',(0.,-1.,0.));
#18521=DIRECTION('ref_axis',(-0.656178714924787,0.,-0.754605522163505));
#18522=DIRECTION('',(0.,-1.,0.));
#18523=DIRECTION('center_axis',(0.,1.,0.));
#18524=DIRECTION('ref_axis',(1.,0.,0.));
#18525=DIRECTION('',(0.,-1.,0.));
#18526=DIRECTION('center_axis',(0.,-1.,0.));
#18527=DIRECTION('ref_axis',(1.,0.,0.));
#18528=DIRECTION('',(0.,-1.,0.));
#18529=DIRECTION('center_axis',(0.,1.,0.));
#18530=DIRECTION('ref_axis',(1.,0.,0.));
#18531=DIRECTION('center_axis',(0.,-1.,0.));
#18532=DIRECTION('ref_axis',(-0.991227900682635,0.,0.132163720091017));
#18533=DIRECTION('',(0.,-1.,0.));
#18534=DIRECTION('center_axis',(0.,1.,0.));
#18535=DIRECTION('ref_axis',(1.,0.,0.));
#18536=DIRECTION('center_axis',(0.,-1.,0.));
#18537=DIRECTION('ref_axis',(1.,0.,0.));
#18538=DIRECTION('',(0.,-1.,0.));
#18539=DIRECTION('center_axis',(0.,1.,0.));
#18540=DIRECTION('ref_axis',(1.,0.,0.));
#18541=DIRECTION('center_axis',(0.,1.,0.));
#18542=DIRECTION('ref_axis',(1.,0.,0.));
#18543=DIRECTION('center_axis',(0.,1.,0.));
#18544=DIRECTION('ref_axis',(0.,0.,1.));
#18545=DIRECTION('center_axis',(0.,1.,0.));
#18546=DIRECTION('ref_axis',(1.,0.,0.));
#18547=DIRECTION('center_axis',(0.,1.,0.));
#18548=DIRECTION('ref_axis',(1.,0.,0.));
#18549=DIRECTION('center_axis',(0.,1.,0.));
#18550=DIRECTION('ref_axis',(1.,0.,0.));
#18551=DIRECTION('center_axis',(0.,1.,0.));
#18552=DIRECTION('ref_axis',(1.,0.,0.));
#18553=DIRECTION('center_axis',(0.,1.,0.));
#18554=DIRECTION('ref_axis',(1.,0.,0.));
#18555=DIRECTION('center_axis',(0.,-1.,0.));
#18556=DIRECTION('ref_axis',(1.,0.,0.));
#18557=DIRECTION('',(-0.316227766016836,0.948683298050514,3.87267321454036E-17));
#18558=DIRECTION('center_axis',(0.,-1.,0.));
#18559=DIRECTION('ref_axis',(1.,0.,0.));
#18560=DIRECTION('center_axis',(0.,-1.,0.));
#18561=DIRECTION('ref_axis',(1.,0.,0.));
#18562=DIRECTION('',(0.,-1.,0.));
#18563=DIRECTION('center_axis',(0.,-1.,0.));
#18564=DIRECTION('ref_axis',(1.,0.,0.));
#18565=DIRECTION('center_axis',(0.,-1.,0.));
#18566=DIRECTION('ref_axis',(1.,0.,0.));
#18567=DIRECTION('',(-0.707106781186541,-0.707106781186554,-8.65956056235485E-17));
#18568=DIRECTION('center_axis',(0.,-1.,0.));
#18569=DIRECTION('ref_axis',(1.,0.,0.));
#18570=DIRECTION('center_axis',(0.,1.,0.));
#18571=DIRECTION('ref_axis',(0.,0.,1.));
#18572=DIRECTION('center_axis',(0.,-1.,0.));
#18573=DIRECTION('ref_axis',(1.,0.,0.));
#18574=DIRECTION('center_axis',(0.,-1.,0.));
#18575=DIRECTION('ref_axis',(1.,0.,0.));
#18576=DIRECTION('',(0.,-1.,0.));
#18577=DIRECTION('center_axis',(0.,1.,0.));
#18578=DIRECTION('ref_axis',(1.,0.,0.));
#18579=DIRECTION('center_axis',(0.,-1.,0.));
#18580=DIRECTION('ref_axis',(1.,0.,0.));
#18581=DIRECTION('',(-0.316227766016831,0.948683298050516,3.8726732145403E-17));
#18582=DIRECTION('center_axis',(0.,-1.,0.));
#18583=DIRECTION('ref_axis',(1.,0.,0.));
#18584=DIRECTION('center_axis',(0.,-1.,0.));
#18585=DIRECTION('ref_axis',(1.,0.,0.));
#18586=DIRECTION('',(0.,-1.,0.));
#18587=DIRECTION('center_axis',(0.,-1.,0.));
#18588=DIRECTION('ref_axis',(1.,0.,0.));
#18589=DIRECTION('center_axis',(0.,-1.,0.));
#18590=DIRECTION('ref_axis',(1.,0.,0.));
#18591=DIRECTION('',(-0.707106781186535,-0.70710678118656,-8.65956056235478E-17));
#18592=DIRECTION('center_axis',(0.,-1.,0.));
#18593=DIRECTION('ref_axis',(1.,0.,0.));
#18594=DIRECTION('center_axis',(0.,1.,0.));
#18595=DIRECTION('ref_axis',(0.,0.,1.));
#18596=DIRECTION('center_axis',(0.,-1.,0.));
#18597=DIRECTION('ref_axis',(1.,0.,0.));
#18598=DIRECTION('center_axis',(0.,-1.,0.));
#18599=DIRECTION('ref_axis',(1.,0.,0.));
#18600=DIRECTION('',(0.,-1.,0.));
#18601=DIRECTION('center_axis',(0.,1.,0.));
#18602=DIRECTION('ref_axis',(1.,0.,0.));
#18603=DIRECTION('center_axis',(0.,-1.,0.));
#18604=DIRECTION('ref_axis',(1.,0.,0.));
#18605=DIRECTION('',(-0.316227766016831,0.948683298050516,3.8726732145403E-17));
#18606=DIRECTION('center_axis',(0.,-1.,0.));
#18607=DIRECTION('ref_axis',(1.,0.,0.));
#18608=DIRECTION('center_axis',(0.,-1.,0.));
#18609=DIRECTION('ref_axis',(1.,0.,0.));
#18610=DIRECTION('',(0.,-1.,0.));
#18611=DIRECTION('center_axis',(0.,-1.,0.));
#18612=DIRECTION('ref_axis',(1.,0.,0.));
#18613=DIRECTION('center_axis',(0.,-1.,0.));
#18614=DIRECTION('ref_axis',(1.,0.,0.));
#18615=DIRECTION('',(-0.707106781186535,-0.70710678118656,-8.65956056235478E-17));
#18616=DIRECTION('center_axis',(0.,-1.,0.));
#18617=DIRECTION('ref_axis',(1.,0.,0.));
#18618=DIRECTION('center_axis',(0.,1.,0.));
#18619=DIRECTION('ref_axis',(0.,0.,1.));
#18620=DIRECTION('center_axis',(0.,-1.,0.));
#18621=DIRECTION('ref_axis',(1.,0.,0.));
#18622=DIRECTION('center_axis',(0.,-1.,0.));
#18623=DIRECTION('ref_axis',(1.,0.,0.));
#18624=DIRECTION('',(0.,-1.,0.));
#18625=DIRECTION('center_axis',(0.,1.,0.));
#18626=DIRECTION('ref_axis',(1.,0.,0.));
#18627=DIRECTION('center_axis',(0.,-1.,0.));
#18628=DIRECTION('ref_axis',(1.,0.,0.));
#18629=DIRECTION('',(-0.316227766016831,0.948683298050516,3.8726732145403E-17));
#18630=DIRECTION('center_axis',(0.,-1.,0.));
#18631=DIRECTION('ref_axis',(1.,0.,0.));
#18632=DIRECTION('center_axis',(0.,-1.,0.));
#18633=DIRECTION('ref_axis',(1.,0.,0.));
#18634=DIRECTION('',(0.,-1.,0.));
#18635=DIRECTION('center_axis',(0.,-1.,0.));
#18636=DIRECTION('ref_axis',(1.,0.,0.));
#18637=DIRECTION('center_axis',(0.,-1.,0.));
#18638=DIRECTION('ref_axis',(1.,0.,0.));
#18639=DIRECTION('',(-0.707106781186535,-0.70710678118656,-8.65956056235478E-17));
#18640=DIRECTION('center_axis',(0.,-1.,0.));
#18641=DIRECTION('ref_axis',(1.,0.,0.));
#18642=DIRECTION('center_axis',(0.,1.,0.));
#18643=DIRECTION('ref_axis',(0.,0.,1.));
#18644=DIRECTION('center_axis',(0.,-1.,0.));
#18645=DIRECTION('ref_axis',(1.,0.,0.));
#18646=DIRECTION('center_axis',(0.,-1.,0.));
#18647=DIRECTION('ref_axis',(1.,0.,0.));
#18648=DIRECTION('',(0.,-1.,0.));
#18649=DIRECTION('center_axis',(0.,-1.,0.));
#18650=DIRECTION('ref_axis',(0.,0.,1.));
#18651=DIRECTION('center_axis',(0.,1.,0.));
#18652=DIRECTION('ref_axis',(1.,0.,0.));
#18653=DIRECTION('',(8.65956056235489E-17,-0.70710678118655,-0.707106781186544));
#18654=DIRECTION('center_axis',(0.,1.,0.));
#18655=DIRECTION('ref_axis',(0.,0.,1.));
#18656=DIRECTION('',(0.,1.,0.));
#18657=DIRECTION('center_axis',(0.,1.,0.));
#18658=DIRECTION('ref_axis',(1.,0.,0.));
#18659=DIRECTION('center_axis',(0.,-1.,0.));
#18660=DIRECTION('ref_axis',(0.,0.,-1.));
#18661=DIRECTION('center_axis',(0.,1.,0.));
#18662=DIRECTION('ref_axis',(1.,0.,0.));
#18663=DIRECTION('center_axis',(0.,1.,0.));
#18664=DIRECTION('ref_axis',(0.,0.,1.));
#18665=DIRECTION('',(0.,1.,0.));
#18666=DIRECTION('center_axis',(0.,-1.,0.));
#18667=DIRECTION('ref_axis',(1.,0.,0.));
#18668=DIRECTION('',(0.,-1.,0.));
#18669=DIRECTION('center_axis',(0.,1.,0.));
#18670=DIRECTION('ref_axis',(1.,0.,0.));
#18671=DIRECTION('center_axis',(0.,-1.,0.));
#18672=DIRECTION('ref_axis',(1.,0.,0.));
#18673=DIRECTION('',(0.,-1.,0.));
#18674=DIRECTION('center_axis',(0.,1.,0.));
#18675=DIRECTION('ref_axis',(1.,0.,0.));
#18676=DIRECTION('center_axis',(0.,-1.,0.));
#18677=DIRECTION('ref_axis',(1.,0.,0.));
#18678=DIRECTION('',(0.,-1.,0.));
#18679=DIRECTION('center_axis',(0.,1.,0.));
#18680=DIRECTION('ref_axis',(1.,0.,0.));
#18681=DIRECTION('center_axis',(0.,-1.,0.));
#18682=DIRECTION('ref_axis',(1.,0.,0.));
#18683=DIRECTION('center_axis',(0.,1.,0.));
#18684=DIRECTION('ref_axis',(1.,0.,0.));
#18685=DIRECTION('center_axis',(0.,1.,0.));
#18686=DIRECTION('ref_axis',(1.,0.,0.));
#18687=DIRECTION('axis',(0.,0.,1.));
#18688=DIRECTION('refdir',(1.,0.,0.));
#18689=DIRECTION('center_axis',(-0.707106781186548,0.5,0.5));
#18690=DIRECTION('ref_axis',(0.577350269189625,-1.05152891894174E-16,0.816496580927726));
#18691=DIRECTION('',(0.,-0.707106781186548,0.707106781186547));
#18692=DIRECTION('',(0.678598344545845,0.281084637714803,0.678598344545857));
#18693=DIRECTION('',(0.,0.707106781186548,-0.707106781186547));
#18694=DIRECTION('',(0.678598344545846,0.678598344545852,0.281084637714809));
#18695=DIRECTION('center_axis',(-0.707106781186554,0.,0.707106781186541));
#18696=DIRECTION('ref_axis',(0.707106781186541,0.,0.707106781186554));
#18697=DIRECTION('',(0.,-1.,0.));
#18698=DIRECTION('',(0.678598344545847,-0.281084637714792,0.678598344545859));
#18699=DIRECTION('',(0.,1.,0.));
#18700=DIRECTION('center_axis',(-0.707106781186544,-0.500000000000003,0.500000000000003));
#18701=DIRECTION('ref_axis',(0.57735026918963,1.66848612271393E-17,0.816496580927723));
#18702=DIRECTION('',(0.,-0.707106781186548,-0.707106781186547));
#18703=DIRECTION('',(0.678598344545849,-0.678598344545849,0.281084637714811));
#18704=DIRECTION('',(0.,0.707106781186548,0.707106781186547));
#18705=DIRECTION('center_axis',(-0.707106781186548,-0.707106781186548,0.));
#18706=DIRECTION('ref_axis',(0.,0.,1.));
#18707=DIRECTION('',(0.,0.,-1.));
#18708=DIRECTION('',(0.678598344545844,-0.678598344545844,-0.281084637714833));
#18709=DIRECTION('',(0.,0.,1.));
#18710=DIRECTION('center_axis',(-0.707106781186553,-0.499999999999996,-0.499999999999996));
#18711=DIRECTION('ref_axis',(-0.57735026918962,1.74145151191031E-16,0.81649658092773));
#18712=DIRECTION('',(0.,0.707106781186548,-0.707106781186548));
#18713=DIRECTION('',(0.678598344545843,-0.281084637714838,-0.678598344545843));
#18714=DIRECTION('',(0.,-0.707106781186548,0.707106781186548));
#18715=DIRECTION('center_axis',(-0.707106781186548,0.,-0.707106781186548));
#18716=DIRECTION('ref_axis',(-0.707106781186548,0.,0.707106781186548));
#18717=DIRECTION('',(0.,-1.,0.));
#18718=DIRECTION('',(0.,1.,0.));
#18719=DIRECTION('',(0.678598344545846,0.281084637714827,-0.678598344545846));
#18720=DIRECTION('center_axis',(-0.707106781186548,0.5,-0.5));
#18721=DIRECTION('ref_axis',(-0.577350269189625,1.05152891894174E-16,0.816496580927726));
#18722=DIRECTION('',(0.,-0.707106781186548,-0.707106781186548));
#18723=DIRECTION('',(0.,0.707106781186548,0.707106781186548));
#18724=DIRECTION('',(0.678598344545846,0.678598344545846,-0.281084637714827));
#18725=DIRECTION('center_axis',(-0.707106781186548,0.707106781186548,0.));
#18726=DIRECTION('ref_axis',(0.,0.,1.));
#18727=DIRECTION('',(0.,0.,-1.));
#18728=DIRECTION('',(0.,0.,1.));
#18729=DIRECTION('center_axis',(0.,0.,-1.));
#18730=DIRECTION('ref_axis',(0.,-1.,0.));
#18731=DIRECTION('',(-1.,0.,0.));
#18732=DIRECTION('',(0.,1.,0.));
#18733=DIRECTION('',(-1.,0.,0.));
#18734=DIRECTION('center_axis',(0.,0.707106781186548,-0.707106781186548));
#18735=DIRECTION('ref_axis',(0.,-0.707106781186548,-0.707106781186548));
#18736=DIRECTION('',(-1.,0.,0.));
#18737=DIRECTION('',(0.,0.707106781186548,0.707106781186548));
#18738=DIRECTION('center_axis',(0.,1.,0.));
#18739=DIRECTION('ref_axis',(0.,0.,-1.));
#18740=DIRECTION('',(-1.,0.,0.));
#18741=DIRECTION('',(0.,0.,1.));
#18742=DIRECTION('center_axis',(0.,0.707106781186547,0.707106781186548));
#18743=DIRECTION('ref_axis',(0.,0.707106781186548,-0.707106781186547));
#18744=DIRECTION('',(-1.,0.,0.));
#18745=DIRECTION('',(0.,-0.707106781186548,0.707106781186547));
#18746=DIRECTION('center_axis',(-1.,0.,0.));
#18747=DIRECTION('ref_axis',(0.,0.,1.));
#18748=DIRECTION('center_axis',(1.,0.,0.));
#18749=DIRECTION('ref_axis',(0.,-1.,0.));
#18750=DIRECTION('',(0.,1.,0.));
#18751=DIRECTION('',(0.,0.,1.));
#18752=DIRECTION('',(0.,-1.,0.));
#18753=DIRECTION('',(0.,0.,-1.));
#18754=DIRECTION('',(0.,1.,0.));
#18755=DIRECTION('',(0.,0.,1.));
#18756=DIRECTION('',(0.,-1.,0.));
#18757=DIRECTION('',(0.,0.,-1.));
#18758=DIRECTION('',(0.,1.,0.));
#18759=DIRECTION('',(0.,0.,1.));
#18760=DIRECTION('',(0.,-1.,0.));
#18761=DIRECTION('',(0.,0.,-1.));
#18762=DIRECTION('',(0.,1.,0.));
#18763=DIRECTION('',(0.,0.,1.));
#18764=DIRECTION('',(0.,-1.,0.));
#18765=DIRECTION('',(0.,0.,-1.));
#18766=DIRECTION('center_axis',(1.,0.,0.));
#18767=DIRECTION('ref_axis',(0.,0.,-1.));
#18768=DIRECTION('center_axis',(1.,0.,0.));
#18769=DIRECTION('ref_axis',(0.,-1.,0.));
#18770=DIRECTION('center_axis',(1.,0.,0.));
#18771=DIRECTION('ref_axis',(0.,-1.,0.));
#18772=DIRECTION('center_axis',(1.,0.,0.));
#18773=DIRECTION('ref_axis',(0.,-1.,0.));
#18774=DIRECTION('center_axis',(1.,0.,0.));
#18775=DIRECTION('ref_axis',(0.,-1.,0.));
#18776=DIRECTION('center_axis',(-1.,0.,0.));
#18777=DIRECTION('ref_axis',(0.,0.,1.));
#18778=DIRECTION('',(0.948683298050512,0.316227766016844,3.87267321454047E-17));
#18779=DIRECTION('center_axis',(-1.,0.,0.));
#18780=DIRECTION('ref_axis',(0.,-1.,0.));
#18781=DIRECTION('center_axis',(-1.,0.,0.));
#18782=DIRECTION('ref_axis',(0.,-1.,0.));
#18783=DIRECTION('',(-1.,0.,0.));
#18784=DIRECTION('center_axis',(-1.,0.,0.));
#18785=DIRECTION('ref_axis',(0.,0.,1.));
#18786=DIRECTION('center_axis',(-1.,0.,0.));
#18787=DIRECTION('ref_axis',(0.,-1.,0.));
#18788=DIRECTION('',(-0.707106781186535,0.70710678118656,-8.65956056235509E-17));
#18789=DIRECTION('center_axis',(-1.,0.,0.));
#18790=DIRECTION('ref_axis',(0.,0.,1.));
#18791=DIRECTION('center_axis',(1.,0.,0.));
#18792=DIRECTION('ref_axis',(0.,0.,-1.));
#18793=DIRECTION('center_axis',(-1.,0.,0.));
#18794=DIRECTION('ref_axis',(0.,0.,1.));
#18795=DIRECTION('center_axis',(-1.,0.,0.));
#18796=DIRECTION('ref_axis',(0.,-1.,0.));
#18797=DIRECTION('',(-1.,0.,0.));
#18798=DIRECTION('center_axis',(1.,0.,0.));
#18799=DIRECTION('ref_axis',(0.,-1.,0.));
#18800=DIRECTION('center_axis',(1.,0.,0.));
#18801=DIRECTION('ref_axis',(0.,-1.,0.));
#18802=DIRECTION('center_axis',(-1.,0.,0.));
#18803=DIRECTION('ref_axis',(0.,0.,1.));
#18804=DIRECTION('',(0.948683298050513,0.31622776601684,3.87267321454041E-17));
#18805=DIRECTION('center_axis',(-1.,0.,0.));
#18806=DIRECTION('ref_axis',(0.,-1.,0.));
#18807=DIRECTION('center_axis',(-1.,0.,0.));
#18808=DIRECTION('ref_axis',(0.,-1.,0.));
#18809=DIRECTION('',(-1.,0.,0.));
#18810=DIRECTION('center_axis',(-1.,0.,0.));
#18811=DIRECTION('ref_axis',(0.,0.,1.));
#18812=DIRECTION('center_axis',(-1.,0.,0.));
#18813=DIRECTION('ref_axis',(0.,-1.,0.));
#18814=DIRECTION('',(-0.707106781186541,0.707106781186554,-8.65956056235501E-17));
#18815=DIRECTION('center_axis',(-1.,0.,0.));
#18816=DIRECTION('ref_axis',(0.,0.,1.));
#18817=DIRECTION('center_axis',(1.,0.,0.));
#18818=DIRECTION('ref_axis',(0.,0.,-1.));
#18819=DIRECTION('center_axis',(-1.,0.,0.));
#18820=DIRECTION('ref_axis',(0.,0.,1.));
#18821=DIRECTION('center_axis',(-1.,0.,0.));
#18822=DIRECTION('ref_axis',(0.,-1.,0.));
#18823=DIRECTION('',(-1.,0.,0.));
#18824=DIRECTION('center_axis',(1.,0.,0.));
#18825=DIRECTION('ref_axis',(0.,-1.,0.));
#18826=DIRECTION('center_axis',(1.,0.,0.));
#18827=DIRECTION('ref_axis',(0.,-1.,0.));
#18828=DIRECTION('center_axis',(-1.,0.,0.));
#18829=DIRECTION('ref_axis',(0.,0.,1.));
#18830=DIRECTION('',(0.948683298050512,0.316227766016844,3.87267321454047E-17));
#18831=DIRECTION('center_axis',(-1.,0.,0.));
#18832=DIRECTION('ref_axis',(0.,-1.,0.));
#18833=DIRECTION('center_axis',(-1.,0.,0.));
#18834=DIRECTION('ref_axis',(0.,-1.,0.));
#18835=DIRECTION('',(-1.,0.,0.));
#18836=DIRECTION('center_axis',(-1.,0.,0.));
#18837=DIRECTION('ref_axis',(0.,0.,1.));
#18838=DIRECTION('center_axis',(-1.,0.,0.));
#18839=DIRECTION('ref_axis',(0.,-1.,0.));
#18840=DIRECTION('',(-0.707106781186535,0.70710678118656,-8.65956056235509E-17));
#18841=DIRECTION('center_axis',(-1.,0.,0.));
#18842=DIRECTION('ref_axis',(0.,0.,1.));
#18843=DIRECTION('center_axis',(1.,0.,0.));
#18844=DIRECTION('ref_axis',(0.,0.,-1.));
#18845=DIRECTION('center_axis',(-1.,0.,0.));
#18846=DIRECTION('ref_axis',(0.,0.,1.));
#18847=DIRECTION('center_axis',(-1.,0.,0.));
#18848=DIRECTION('ref_axis',(0.,-1.,0.));
#18849=DIRECTION('',(-1.,0.,0.));
#18850=DIRECTION('center_axis',(1.,0.,0.));
#18851=DIRECTION('ref_axis',(0.,-1.,0.));
#18852=DIRECTION('center_axis',(1.,0.,0.));
#18853=DIRECTION('ref_axis',(0.,-1.,0.));
#18854=DIRECTION('center_axis',(-1.,0.,0.));
#18855=DIRECTION('ref_axis',(0.,0.,1.));
#18856=DIRECTION('',(0.948683298050513,0.31622776601684,3.87267321454041E-17));
#18857=DIRECTION('center_axis',(-1.,0.,0.));
#18858=DIRECTION('ref_axis',(0.,-1.,0.));
#18859=DIRECTION('center_axis',(-1.,0.,0.));
#18860=DIRECTION('ref_axis',(0.,-1.,0.));
#18861=DIRECTION('',(-1.,0.,0.));
#18862=DIRECTION('center_axis',(-1.,0.,0.));
#18863=DIRECTION('ref_axis',(0.,0.,1.));
#18864=DIRECTION('center_axis',(-1.,0.,0.));
#18865=DIRECTION('ref_axis',(0.,-1.,0.));
#18866=DIRECTION('',(-0.707106781186541,0.707106781186554,-8.65956056235501E-17));
#18867=DIRECTION('center_axis',(-1.,0.,0.));
#18868=DIRECTION('ref_axis',(0.,0.,1.));
#18869=DIRECTION('center_axis',(1.,0.,0.));
#18870=DIRECTION('ref_axis',(0.,0.,-1.));
#18871=DIRECTION('center_axis',(-1.,0.,0.));
#18872=DIRECTION('ref_axis',(0.,0.,1.));
#18873=DIRECTION('center_axis',(-1.,0.,0.));
#18874=DIRECTION('ref_axis',(0.,-1.,0.));
#18875=DIRECTION('',(-1.,0.,0.));
#18876=DIRECTION('center_axis',(1.,0.,0.));
#18877=DIRECTION('ref_axis',(0.,-1.,0.));
#18878=DIRECTION('center_axis',(1.,0.,0.));
#18879=DIRECTION('ref_axis',(0.,-1.,0.));
#18880=DIRECTION('center_axis',(-1.,0.,0.));
#18881=DIRECTION('ref_axis',(0.,0.,1.));
#18882=DIRECTION('',(0.707106781186548,0.707106781186547,8.65956056235493E-17));
#18883=DIRECTION('center_axis',(-1.,0.,0.));
#18884=DIRECTION('ref_axis',(0.,-1.,0.));
#18885=DIRECTION('center_axis',(-1.,0.,0.));
#18886=DIRECTION('ref_axis',(0.,-1.,0.));
#18887=DIRECTION('',(-1.,0.,0.));
#18888=DIRECTION('center_axis',(-1.,0.,0.));
#18889=DIRECTION('ref_axis',(0.,0.,1.));
#18890=DIRECTION('center_axis',(-1.,0.,0.));
#18891=DIRECTION('ref_axis',(0.,-1.,0.));
#18892=DIRECTION('',(-0.707106781186551,0.707106781186544,-8.65956056235489E-17));
#18893=DIRECTION('center_axis',(1.,0.,0.));
#18894=DIRECTION('ref_axis',(0.,-1.,0.));
#18895=DIRECTION('center_axis',(-1.,0.,0.));
#18896=DIRECTION('ref_axis',(0.,0.,1.));
#18897=DIRECTION('',(0.707106781186548,0.707106781186547,8.65956056235493E-17));
#18898=DIRECTION('center_axis',(-1.,0.,0.));
#18899=DIRECTION('ref_axis',(0.,-1.,0.));
#18900=DIRECTION('center_axis',(-1.,0.,0.));
#18901=DIRECTION('ref_axis',(0.,-1.,0.));
#18902=DIRECTION('',(-1.,0.,0.));
#18903=DIRECTION('center_axis',(-1.,0.,0.));
#18904=DIRECTION('ref_axis',(0.,0.,1.));
#18905=DIRECTION('center_axis',(-1.,0.,0.));
#18906=DIRECTION('ref_axis',(0.,-1.,0.));
#18907=DIRECTION('',(-0.707106781186551,0.707106781186544,-8.65956056235489E-17));
#18908=DIRECTION('center_axis',(1.,0.,0.));
#18909=DIRECTION('ref_axis',(0.,-1.,0.));
#18910=DIRECTION('center_axis',(-1.,0.,0.));
#18911=DIRECTION('ref_axis',(0.,0.,1.));
#18912=DIRECTION('',(0.707106781186548,0.707106781186547,8.65956056235493E-17));
#18913=DIRECTION('center_axis',(-1.,0.,0.));
#18914=DIRECTION('ref_axis',(0.,-1.,0.));
#18915=DIRECTION('center_axis',(-1.,0.,0.));
#18916=DIRECTION('ref_axis',(0.,-1.,0.));
#18917=DIRECTION('',(-1.,0.,0.));
#18918=DIRECTION('center_axis',(-1.,0.,0.));
#18919=DIRECTION('ref_axis',(0.,0.,1.));
#18920=DIRECTION('center_axis',(-1.,0.,0.));
#18921=DIRECTION('ref_axis',(0.,-1.,0.));
#18922=DIRECTION('',(-0.707106781186551,0.707106781186544,-8.65956056235489E-17));
#18923=DIRECTION('center_axis',(1.,0.,0.));
#18924=DIRECTION('ref_axis',(0.,-1.,0.));
#18925=DIRECTION('center_axis',(-1.,0.,0.));
#18926=DIRECTION('ref_axis',(0.,0.,1.));
#18927=DIRECTION('',(0.707106781186548,0.707106781186547,8.65956056235493E-17));
#18928=DIRECTION('center_axis',(-1.,0.,0.));
#18929=DIRECTION('ref_axis',(0.,-1.,0.));
#18930=DIRECTION('center_axis',(-1.,0.,0.));
#18931=DIRECTION('ref_axis',(0.,-1.,0.));
#18932=DIRECTION('',(-1.,0.,0.));
#18933=DIRECTION('center_axis',(-1.,0.,0.));
#18934=DIRECTION('ref_axis',(0.,0.,1.));
#18935=DIRECTION('center_axis',(-1.,0.,0.));
#18936=DIRECTION('ref_axis',(0.,-1.,0.));
#18937=DIRECTION('',(-0.707106781186551,0.707106781186544,-8.65956056235489E-17));
#18938=DIRECTION('center_axis',(0.,0.,-1.));
#18939=DIRECTION('ref_axis',(0.,-1.,0.));
#18940=DIRECTION('',(0.,-1.,0.));
#18941=DIRECTION('',(-1.,0.,0.));
#18942=DIRECTION('',(-1.,0.,0.));
#18943=DIRECTION('center_axis',(0.,1.,0.));
#18944=DIRECTION('ref_axis',(0.,0.,-1.));
#18945=DIRECTION('',(0.,0.,-1.));
#18946=DIRECTION('',(-1.,0.,0.));
#18947=DIRECTION('center_axis',(0.,0.,1.));
#18948=DIRECTION('ref_axis',(0.,1.,0.));
#18949=DIRECTION('',(0.,1.,0.));
#18950=DIRECTION('',(-1.,0.,0.));
#18951=DIRECTION('center_axis',(0.,-1.,0.));
#18952=DIRECTION('ref_axis',(0.,0.,1.));
#18953=DIRECTION('',(0.,0.,1.));
#18954=DIRECTION('center_axis',(0.,0.,-1.));
#18955=DIRECTION('ref_axis',(0.,-1.,0.));
#18956=DIRECTION('',(0.,-1.,0.));
#18957=DIRECTION('',(-1.,0.,0.));
#18958=DIRECTION('',(-1.,0.,0.));
#18959=DIRECTION('center_axis',(0.,1.,0.));
#18960=DIRECTION('ref_axis',(0.,0.,-1.));
#18961=DIRECTION('',(0.,0.,-1.));
#18962=DIRECTION('',(-1.,0.,0.));
#18963=DIRECTION('center_axis',(0.,0.,1.));
#18964=DIRECTION('ref_axis',(0.,1.,0.));
#18965=DIRECTION('',(0.,1.,0.));
#18966=DIRECTION('',(-1.,0.,0.));
#18967=DIRECTION('center_axis',(0.,-1.,0.));
#18968=DIRECTION('ref_axis',(0.,0.,1.));
#18969=DIRECTION('',(0.,0.,1.));
#18970=DIRECTION('center_axis',(0.,0.,-1.));
#18971=DIRECTION('ref_axis',(0.,-1.,0.));
#18972=DIRECTION('',(0.,-1.,0.));
#18973=DIRECTION('',(-1.,0.,0.));
#18974=DIRECTION('',(-1.,0.,0.));
#18975=DIRECTION('center_axis',(0.,1.,0.));
#18976=DIRECTION('ref_axis',(0.,0.,-1.));
#18977=DIRECTION('',(0.,0.,-1.));
#18978=DIRECTION('',(-1.,0.,0.));
#18979=DIRECTION('center_axis',(0.,0.,1.));
#18980=DIRECTION('ref_axis',(0.,1.,0.));
#18981=DIRECTION('',(0.,1.,0.));
#18982=DIRECTION('',(-1.,0.,0.));
#18983=DIRECTION('center_axis',(0.,-1.,0.));
#18984=DIRECTION('ref_axis',(0.,0.,1.));
#18985=DIRECTION('',(0.,0.,1.));
#18986=DIRECTION('center_axis',(0.,0.,-1.));
#18987=DIRECTION('ref_axis',(0.,-1.,0.));
#18988=DIRECTION('',(0.,-1.,0.));
#18989=DIRECTION('',(-1.,0.,0.));
#18990=DIRECTION('',(-1.,0.,0.));
#18991=DIRECTION('center_axis',(0.,1.,0.));
#18992=DIRECTION('ref_axis',(0.,0.,-1.));
#18993=DIRECTION('',(0.,0.,-1.));
#18994=DIRECTION('',(-1.,0.,0.));
#18995=DIRECTION('center_axis',(0.,0.,1.));
#18996=DIRECTION('ref_axis',(0.,1.,0.));
#18997=DIRECTION('',(0.,1.,0.));
#18998=DIRECTION('',(-1.,0.,0.));
#18999=DIRECTION('center_axis',(0.,-1.,0.));
#19000=DIRECTION('ref_axis',(0.,0.,1.));
#19001=DIRECTION('',(0.,0.,1.));
#19002=DIRECTION('center_axis',(-1.,0.,0.));
#19003=DIRECTION('ref_axis',(0.,0.,-1.));
#19004=DIRECTION('center_axis',(-1.,0.,0.));
#19005=DIRECTION('ref_axis',(0.,0.,-1.));
#19006=DIRECTION('',(-1.,0.,0.));
#19007=DIRECTION('center_axis',(1.,0.,0.));
#19008=DIRECTION('ref_axis',(0.,0.,-1.));
#19009=DIRECTION('center_axis',(1.,0.,0.));
#19010=DIRECTION('ref_axis',(0.,0.,-1.));
#19011=DIRECTION('',(1.,0.,0.));
#19012=DIRECTION('center_axis',(1.,0.,0.));
#19013=DIRECTION('ref_axis',(0.,0.,-1.));
#19014=DIRECTION('center_axis',(1.,0.,0.));
#19015=DIRECTION('ref_axis',(0.,0.,-1.));
#19016=DIRECTION('center_axis',(0.,0.,1.));
#19017=DIRECTION('ref_axis',(0.,1.,0.));
#19018=DIRECTION('',(-1.,0.,0.));
#19019=DIRECTION('',(0.,-1.,0.));
#19020=DIRECTION('center_axis',(0.,-0.707106781186547,0.707106781186548));
#19021=DIRECTION('ref_axis',(0.,0.707106781186548,0.707106781186547));
#19022=DIRECTION('',(-1.,0.,0.));
#19023=DIRECTION('',(0.,-0.707106781186548,-0.707106781186547));
#19024=DIRECTION('center_axis',(0.,-1.,0.));
#19025=DIRECTION('ref_axis',(0.,0.,1.));
#19026=DIRECTION('',(-1.,0.,0.));
#19027=DIRECTION('',(0.,0.,-1.));
#19028=DIRECTION('center_axis',(0.,-0.707106781186548,-0.707106781186548));
#19029=DIRECTION('ref_axis',(0.,-0.707106781186548,0.707106781186548));
#19030=DIRECTION('',(0.,0.707106781186548,-0.707106781186548));
#19031=DIRECTION('center_axis',(1.,0.,0.));
#19032=DIRECTION('ref_axis',(0.,0.,-1.));
#19033=DIRECTION('axis',(0.,0.,1.));
#19034=DIRECTION('refdir',(1.,0.,0.));
#19035=DIRECTION('center_axis',(-1.,0.,0.));
#19036=DIRECTION('ref_axis',(0.,0.437755261071371,0.899094172711811));
#19037=DIRECTION('',(1.,0.,0.));
#19038=DIRECTION('center_axis',(-1.,0.,0.));
#19039=DIRECTION('ref_axis',(0.,0.,1.));
#19040=DIRECTION('',(-1.,2.62207686119176E-10,0.));
#19041=DIRECTION('center_axis',(-1.,0.,0.));
#19042=DIRECTION('ref_axis',(0.,0.297498178236103,0.954722385799244));
#19043=DIRECTION('',(1.,0.,0.));
#19044=DIRECTION('center_axis',(-1.,0.,0.));
#19045=DIRECTION('ref_axis',(0.,0.297498178236103,0.954722385799244));
#19046=DIRECTION('',(1.,0.,0.));
#19047=DIRECTION('center_axis',(-1.,0.,0.));
#19048=DIRECTION('ref_axis',(0.,0.297498178236103,0.954722385799244));
#19049=DIRECTION('',(1.,0.,0.));
#19050=DIRECTION('center_axis',(-1.,0.,0.));
#19051=DIRECTION('ref_axis',(0.,0.297498178236103,0.954722385799244));
#19052=DIRECTION('',(1.,0.,0.));
#19053=DIRECTION('center_axis',(-1.,0.,0.));
#19054=DIRECTION('ref_axis',(0.,0.297498178236103,0.954722385799244));
#19055=DIRECTION('',(1.,0.,0.));
#19056=DIRECTION('center_axis',(-1.,0.,0.));
#19057=DIRECTION('ref_axis',(0.,-0.150453659663836,0.988617062513974));
#19058=DIRECTION('center_axis',(1.,0.,0.));
#19059=DIRECTION('ref_axis',(0.,0.,1.));
#19060=DIRECTION('',(1.,0.,0.));
#19061=DIRECTION('center_axis',(0.,-1.,0.));
#19062=DIRECTION('ref_axis',(1.,0.,0.));
#19063=DIRECTION('',(0.,0.,-1.));
#19064=DIRECTION('',(1.,0.,0.));
#19065=DIRECTION('',(0.,0.,1.));
#19066=DIRECTION('',(1.,0.,0.));
#19067=DIRECTION('center_axis',(1.,0.,0.));
#19068=DIRECTION('ref_axis',(0.,1.,0.));
#19069=DIRECTION('center_axis',(-1.,0.,0.));
#19070=DIRECTION('ref_axis',(0.,0.,1.));
#19071=DIRECTION('',(0.,1.,0.));
#19072=DIRECTION('',(0.,0.,1.));
#19073=DIRECTION('center_axis',(0.,1.,0.));
#19074=DIRECTION('ref_axis',(-1.,0.,0.));
#19075=DIRECTION('',(0.,0.,1.));
#19076=DIRECTION('',(-1.,0.,0.));
#19077=DIRECTION('',(-1.,0.,0.));
#19078=DIRECTION('center_axis',(0.,0.,1.));
#19079=DIRECTION('ref_axis',(1.,0.,0.));
#19080=DIRECTION('',(0.,-1.,0.));
#19081=DIRECTION('center_axis',(-1.,0.,0.));
#19082=DIRECTION('ref_axis',(0.,0.,1.));
#19083=DIRECTION('center_axis',(-1.,0.,0.));
#19084=DIRECTION('ref_axis',(0.,0.,1.));
#19085=DIRECTION('',(-1.,0.,0.));
#19086=DIRECTION('center_axis',(-1.,0.,0.));
#19087=DIRECTION('ref_axis',(0.,0.,1.));
#19088=DIRECTION('center_axis',(-1.,0.,0.));
#19089=DIRECTION('ref_axis',(0.,0.,1.));
#19090=DIRECTION('center_axis',(-1.,0.,0.));
#19091=DIRECTION('ref_axis',(0.,-1.22464679914735E-16,-1.));
#19092=DIRECTION('center_axis',(1.,0.,0.));
#19093=DIRECTION('ref_axis',(0.,0.,1.));
#19094=DIRECTION('center_axis',(-1.,0.,0.));
#19095=DIRECTION('ref_axis',(0.,0.,1.));
#19096=DIRECTION('',(-0.515038074910058,-1.04972719113862E-16,-0.85716730070211));
#19097=DIRECTION('center_axis',(-1.,0.,0.));
#19098=DIRECTION('ref_axis',(0.,0.,1.));
#19099=DIRECTION('center_axis',(-1.,0.,0.));
#19100=DIRECTION('ref_axis',(0.,0.,1.));
#19101=DIRECTION('',(1.,0.,0.));
#19102=DIRECTION('center_axis',(-1.,0.,0.));
#19103=DIRECTION('ref_axis',(0.,0.,1.));
#19104=DIRECTION('center_axis',(1.,0.,0.));
#19105=DIRECTION('ref_axis',(0.,0.,1.));
#19106=DIRECTION('',(0.701238976116887,0.,0.712926292385503));
#19107=DIRECTION('',(-0.701238976116887,-8.73082901997896E-17,0.712926292385503));
#19108=DIRECTION('center_axis',(-1.,0.,0.));
#19109=DIRECTION('ref_axis',(0.,0.,1.));
#19110=DIRECTION('',(-0.701238976116887,1.83871647159407E-10,-0.712926292385503));
#19111=DIRECTION('',(0.701238976116887,8.73082901997896E-17,0.712926292385503));
#19112=DIRECTION('center_axis',(-1.,0.,0.));
#19113=DIRECTION('ref_axis',(0.,0.,1.));
#19114=DIRECTION('center_axis',(-1.,0.,0.));
#19115=DIRECTION('ref_axis',(0.,0.,1.));
#19116=DIRECTION('',(1.,0.,0.));
#19117=DIRECTION('center_axis',(-1.,0.,0.));
#19118=DIRECTION('ref_axis',(0.,0.,1.));
#19119=DIRECTION('',(-0.342020143325669,0.,0.939692620785908));
#19120=DIRECTION('center_axis',(0.,1.,0.));
#19121=DIRECTION('ref_axis',(1.,0.,0.));
#19122=DIRECTION('',(-0.34202014332565,8.96784698282884E-11,0.939692620785916));
#19123=DIRECTION('center_axis',(2.62207686119176E-10,1.,1.96067283990894E-15));
#19124=DIRECTION('ref_axis',(2.49435711265653E-42,-1.96067283990894E-15,
1.));
#19125=DIRECTION('center_axis',(1.,0.,0.));
#19126=DIRECTION('ref_axis',(0.,0.,-1.));
#19127=DIRECTION('center_axis',(-1.,0.,0.));
#19128=DIRECTION('ref_axis',(0.,0.,1.));
#19129=DIRECTION('center_axis',(-1.,0.,0.));
#19130=DIRECTION('ref_axis',(0.,0.,1.));
#19131=DIRECTION('center_axis',(-1.,0.,0.));
#19132=DIRECTION('ref_axis',(0.,0.,1.));
#19133=DIRECTION('',(0.70710678118654,8.65956056235503E-17,0.707106781186555));
#19134=DIRECTION('center_axis',(-1.,0.,0.));
#19135=DIRECTION('ref_axis',(0.,0.,1.));
#19136=DIRECTION('center_axis',(-1.,0.,0.));
#19137=DIRECTION('ref_axis',(0.,0.,1.));
#19138=DIRECTION('',(1.,0.,0.));
#19139=DIRECTION('center_axis',(1.,0.,0.));
#19140=DIRECTION('ref_axis',(0.,0.,-1.));
#19141=DIRECTION('center_axis',(-1.,0.,0.));
#19142=DIRECTION('ref_axis',(0.,0.,1.));
#19143=DIRECTION('center_axis',(-1.,0.,0.));
#19144=DIRECTION('ref_axis',(0.,0.,1.));
#19145=DIRECTION('center_axis',(-1.,0.,0.));
#19146=DIRECTION('ref_axis',(0.,0.,1.));
#19147=DIRECTION('',(0.707106781186548,8.65956056235493E-17,0.707106781186547));
#19148=DIRECTION('center_axis',(-1.,0.,0.));
#19149=DIRECTION('ref_axis',(0.,0.,1.));
#19150=DIRECTION('center_axis',(-1.,0.,0.));
#19151=DIRECTION('ref_axis',(0.,0.,1.));
#19152=DIRECTION('',(1.,0.,0.));
#19153=DIRECTION('center_axis',(-1.,0.,0.));
#19154=DIRECTION('ref_axis',(0.,0.,1.));
#19155=DIRECTION('center_axis',(1.,0.,0.));
#19156=DIRECTION('ref_axis',(0.,0.,-1.));
#19157=DIRECTION('center_axis',(-1.,0.,0.));
#19158=DIRECTION('ref_axis',(0.,0.,1.));
#19159=DIRECTION('center_axis',(-1.,0.,0.));
#19160=DIRECTION('ref_axis',(0.,0.,1.));
#19161=DIRECTION('center_axis',(-1.,0.,0.));
#19162=DIRECTION('ref_axis',(0.,0.,1.));
#19163=DIRECTION('',(1.,0.,0.));
#19164=DIRECTION('center_axis',(1.,0.,0.));
#19165=DIRECTION('ref_axis',(0.,0.,1.));
#19166=DIRECTION('',(-0.707106781186548,-8.65956056235493E-17,0.707106781186547));
#19167=DIRECTION('center_axis',(-1.,0.,0.));
#19168=DIRECTION('ref_axis',(0.,0.,1.));
#19169=DIRECTION('center_axis',(-1.,0.,0.));
#19170=DIRECTION('ref_axis',(0.,0.,1.));
#19171=DIRECTION('center_axis',(-1.,0.,0.));
#19172=DIRECTION('ref_axis',(0.,0.,1.));
#19173=DIRECTION('center_axis',(-1.,0.,0.));
#19174=DIRECTION('ref_axis',(0.,0.,1.));
#19175=DIRECTION('center_axis',(-1.,0.,0.));
#19176=DIRECTION('ref_axis',(0.,0.,1.));
#19177=DIRECTION('',(1.,0.,0.));
#19178=DIRECTION('center_axis',(1.,0.,0.));
#19179=DIRECTION('ref_axis',(0.,0.,1.));
#19180=DIRECTION('',(-0.70710678118654,-8.65956056235503E-17,0.707106781186555));
#19181=DIRECTION('center_axis',(-1.,0.,0.));
#19182=DIRECTION('ref_axis',(0.,0.,1.));
#19183=DIRECTION('center_axis',(-1.,0.,0.));
#19184=DIRECTION('ref_axis',(0.,0.,1.));
#19185=DIRECTION('axis',(0.,0.,1.));
#19186=DIRECTION('refdir',(1.,0.,0.));
#19187=DIRECTION('center_axis',(0.,-1.,0.));
#19188=DIRECTION('ref_axis',(0.,0.,-1.));
#19189=DIRECTION('center_axis',(0.,1.,0.));
#19190=DIRECTION('ref_axis',(0.,0.,-1.));
#19191=DIRECTION('',(-8.65956056235491E-17,-0.707106781186549,0.707106781186546));
#19192=DIRECTION('center_axis',(0.,-1.,0.));
#19193=DIRECTION('ref_axis',(0.,0.,-1.));
#19194=DIRECTION('center_axis',(0.,1.,0.));
#19195=DIRECTION('ref_axis',(0.,0.,-1.));
#19196=DIRECTION('center_axis',(0.,1.,0.));
#19197=DIRECTION('ref_axis',(0.,0.,1.));
#19198=DIRECTION('',(0.,1.,0.));
#19199=DIRECTION('center_axis',(0.,-1.,0.));
#19200=DIRECTION('ref_axis',(0.,0.,-1.));
#19201=DIRECTION('center_axis',(0.,-1.,0.));
#19202=DIRECTION('ref_axis',(0.,0.,-1.));
#19203=DIRECTION('center_axis',(0.,-1.,0.));
#19204=DIRECTION('ref_axis',(0.,0.,-1.));
#19205=DIRECTION('center_axis',(0.,1.,0.));
#19206=DIRECTION('ref_axis',(1.,0.,0.));
#19207=DIRECTION('',(-0.904527495480339,0.,-0.426415302164528));
#19208=DIRECTION('center_axis',(0.,1.,0.));
#19209=DIRECTION('ref_axis',(1.,0.,0.));
#19210=DIRECTION('',(-0.79610467303825,0.,-0.605158945704896));
#19211=DIRECTION('center_axis',(0.,1.,0.));
#19212=DIRECTION('ref_axis',(1.,0.,0.));
#19213=DIRECTION('',(-0.652888256250524,0.,-0.757454239442984));
#19214=DIRECTION('center_axis',(0.,1.,0.));
#19215=DIRECTION('ref_axis',(1.,0.,0.));
#19216=DIRECTION('',(-0.481137489758913,0.,-0.876645148248989));
#19217=DIRECTION('center_axis',(0.,1.,0.));
#19218=DIRECTION('ref_axis',(1.,0.,0.));
#19219=DIRECTION('',(-0.288358706211123,0.,-0.957522457466271));
#19220=DIRECTION('center_axis',(0.,1.,0.));
#19221=DIRECTION('ref_axis',(1.,0.,0.));
#19222=DIRECTION('',(-0.0829772635033118,0.,-0.996551440589748));
#19223=DIRECTION('center_axis',(0.,1.,0.));
#19224=DIRECTION('ref_axis',(1.,0.,0.));
#19225=DIRECTION('',(0.126030683788683,0.,-0.992026343775082));
#19226=DIRECTION('center_axis',(0.,1.,0.));
#19227=DIRECTION('ref_axis',(1.,0.,0.));
#19228=DIRECTION('',(0.329530485436752,0.,-0.944144935466912));
#19229=DIRECTION('center_axis',(0.,1.,0.));
#19230=DIRECTION('ref_axis',(1.,0.,0.));
#19231=DIRECTION('',(0.518628223608573,0.,-0.854999862968771));
#19232=DIRECTION('center_axis',(0.,1.,0.));
#19233=DIRECTION('ref_axis',(1.,0.,0.));
#19234=DIRECTION('',(0.685059419754336,0.,-0.728487193714379));
#19235=DIRECTION('center_axis',(0.,1.,0.));
#19236=DIRECTION('ref_axis',(1.,0.,0.));
#19237=DIRECTION('',(0.821550231977042,0.,-0.570136138425262));
#19238=DIRECTION('center_axis',(0.,1.,0.));
#19239=DIRECTION('ref_axis',(1.,0.,0.));
#19240=DIRECTION('',(0.922135356826958,0.,-0.386867398070217));
#19241=DIRECTION('center_axis',(0.,1.,0.));
#19242=DIRECTION('ref_axis',(1.,0.,0.));
#19243=DIRECTION('',(0.98241874168714,0.,-0.186690696023813));
#19244=DIRECTION('center_axis',(0.,1.,0.));
#19245=DIRECTION('ref_axis',(1.,0.,0.));
#19246=DIRECTION('',(0.999765713367456,0.,0.0216452852802363));
#19247=DIRECTION('center_axis',(0.,1.,0.));
#19248=DIRECTION('ref_axis',(1.,0.,0.));
#19249=DIRECTION('',(0.973418125965458,0.,0.229035263751885));
#19250=DIRECTION('center_axis',(0.,1.,0.));
#19251=DIRECTION('ref_axis',(1.,0.,0.));
#19252=DIRECTION('',(0.904527495480356,0.,0.426415302164492));
#19253=DIRECTION('center_axis',(0.,1.,0.));
#19254=DIRECTION('ref_axis',(1.,0.,0.));
#19255=DIRECTION('',(0.79610467303827,0.,0.605158945704869));
#19256=DIRECTION('center_axis',(0.,1.,0.));
#19257=DIRECTION('ref_axis',(1.,0.,0.));
#19258=DIRECTION('',(0.652888256250397,0.,0.757454239443094));
#19259=DIRECTION('center_axis',(0.,1.,0.));
#19260=DIRECTION('ref_axis',(1.,0.,0.));
#19261=DIRECTION('',(0.481137489758878,0.,0.876645148249008));
#19262=DIRECTION('center_axis',(0.,1.,0.));
#19263=DIRECTION('ref_axis',(1.,0.,0.));
#19264=DIRECTION('',(0.288358706211123,0.,0.957522457466271));
#19265=DIRECTION('center_axis',(0.,1.,0.));
#19266=DIRECTION('ref_axis',(1.,0.,0.));
#19267=DIRECTION('',(0.0829772635033118,0.,0.996551440589748));
#19268=DIRECTION('center_axis',(0.,1.,0.));
#19269=DIRECTION('ref_axis',(1.,0.,0.));
#19270=DIRECTION('',(-0.126030683788684,0.,0.992026343775082));
#19271=DIRECTION('center_axis',(0.,1.,0.));
#19272=DIRECTION('ref_axis',(1.,0.,0.));
#19273=DIRECTION('',(-0.329530485436752,0.,0.944144935466912));
#19274=DIRECTION('center_axis',(0.,1.,0.));
#19275=DIRECTION('ref_axis',(1.,0.,0.));
#19276=DIRECTION('',(-0.518628223608573,0.,0.854999862968771));
#19277=DIRECTION('center_axis',(0.,1.,0.));
#19278=DIRECTION('ref_axis',(1.,0.,0.));
#19279=DIRECTION('',(-0.685059419754315,0.,0.728487193714399));
#19280=DIRECTION('center_axis',(0.,1.,0.));
#19281=DIRECTION('ref_axis',(1.,0.,0.));
#19282=DIRECTION('',(-0.821550231977102,0.,0.570136138425175));
#19283=DIRECTION('center_axis',(0.,1.,0.));
#19284=DIRECTION('ref_axis',(1.,0.,0.));
#19285=DIRECTION('',(-0.922135356827004,0.,0.386867398070107));
#19286=DIRECTION('center_axis',(0.,1.,0.));
#19287=DIRECTION('ref_axis',(1.,0.,0.));
#19288=DIRECTION('',(-0.98241874168718,0.,0.186690696023607));
#19289=DIRECTION('center_axis',(0.,1.,0.));
#19290=DIRECTION('ref_axis',(1.,0.,0.));
#19291=DIRECTION('',(-0.99976571336746,0.,-0.021645285280017));
#19292=DIRECTION('center_axis',(0.,1.,0.));
#19293=DIRECTION('ref_axis',(1.,0.,0.));
#19294=DIRECTION('',(-0.973418125965487,0.,-0.229035263751761));
#19295=DIRECTION('center_axis',(0.,1.,0.));
#19296=DIRECTION('ref_axis',(0.,0.,-1.));
#19297=DIRECTION('',(8.65956056235493E-17,0.707106781186548,0.707106781186547));
#19298=DIRECTION('center_axis',(0.,1.,0.));
#19299=DIRECTION('ref_axis',(0.,0.,-1.));
#19300=DIRECTION('center_axis',(0.,1.,0.));
#19301=DIRECTION('ref_axis',(0.,0.,1.));
#19302=DIRECTION('',(0.98241874168718,0.,0.186690696023607));
#19303=DIRECTION('center_axis',(0.,1.,0.));
#19304=DIRECTION('ref_axis',(1.,0.,0.));
#19305=DIRECTION('',(0.99976571336746,0.,-0.021645285280017));
#19306=DIRECTION('center_axis',(0.,1.,0.));
#19307=DIRECTION('ref_axis',(1.,0.,0.));
#19308=DIRECTION('',(0.973418125965488,0.,-0.22903526375176));
#19309=DIRECTION('center_axis',(0.,1.,0.));
#19310=DIRECTION('ref_axis',(1.,0.,0.));
#19311=DIRECTION('',(0.904527495480339,0.,-0.426415302164528));
#19312=DIRECTION('center_axis',(0.,1.,0.));
#19313=DIRECTION('ref_axis',(1.,0.,0.));
#19314=DIRECTION('',(0.79610467303825,0.,-0.605158945704896));
#19315=DIRECTION('center_axis',(0.,1.,0.));
#19316=DIRECTION('ref_axis',(1.,0.,0.));
#19317=DIRECTION('',(0.652888256250524,0.,-0.757454239442984));
#19318=DIRECTION('center_axis',(0.,1.,0.));
#19319=DIRECTION('ref_axis',(1.,0.,0.));
#19320=DIRECTION('',(0.481137489758913,0.,-0.876645148248989));
#19321=DIRECTION('center_axis',(0.,1.,0.));
#19322=DIRECTION('ref_axis',(1.,0.,0.));
#19323=DIRECTION('',(0.288358706211123,0.,-0.957522457466271));
#19324=DIRECTION('center_axis',(0.,1.,0.));
#19325=DIRECTION('ref_axis',(1.,0.,0.));
#19326=DIRECTION('',(0.0829772635033118,0.,-0.996551440589748));
#19327=DIRECTION('center_axis',(0.,1.,0.));
#19328=DIRECTION('ref_axis',(1.,0.,0.));
#19329=DIRECTION('',(-0.126030683788638,0.,-0.992026343775088));
#19330=DIRECTION('center_axis',(0.,1.,0.));
#19331=DIRECTION('ref_axis',(1.,0.,0.));
#19332=DIRECTION('',(-0.32953048543679,0.,-0.944144935466898));
#19333=DIRECTION('center_axis',(0.,1.,0.));
#19334=DIRECTION('ref_axis',(1.,0.,0.));
#19335=DIRECTION('',(-0.518628223608571,0.,-0.854999862968772));
#19336=DIRECTION('center_axis',(0.,1.,0.));
#19337=DIRECTION('ref_axis',(1.,0.,0.));
#19338=DIRECTION('',(-0.685059419754336,0.,-0.728487193714379));
#19339=DIRECTION('center_axis',(0.,1.,0.));
#19340=DIRECTION('ref_axis',(1.,0.,0.));
#19341=DIRECTION('',(-0.821550231977042,0.,-0.570136138425262));
#19342=DIRECTION('center_axis',(0.,1.,0.));
#19343=DIRECTION('ref_axis',(1.,0.,0.));
#19344=DIRECTION('',(-0.922135356826964,0.,-0.386867398070201));
#19345=DIRECTION('center_axis',(0.,1.,0.));
#19346=DIRECTION('ref_axis',(1.,0.,0.));
#19347=DIRECTION('',(-0.98241874168714,0.,-0.186690696023813));
#19348=DIRECTION('center_axis',(0.,1.,0.));
#19349=DIRECTION('ref_axis',(1.,0.,0.));
#19350=DIRECTION('',(-0.999765713367456,0.,0.0216452852801921));
#19351=DIRECTION('center_axis',(0.,1.,0.));
#19352=DIRECTION('ref_axis',(1.,0.,0.));
#19353=DIRECTION('',(-0.973418125965457,0.,0.229035263751892));
#19354=DIRECTION('center_axis',(0.,1.,0.));
#19355=DIRECTION('ref_axis',(1.,0.,0.));
#19356=DIRECTION('',(-0.904527495480356,0.,0.426415302164492));
#19357=DIRECTION('center_axis',(0.,1.,0.));
#19358=DIRECTION('ref_axis',(1.,0.,0.));
#19359=DIRECTION('',(-0.796104673038291,0.,0.605158945704842));
#19360=DIRECTION('center_axis',(0.,1.,0.));
#19361=DIRECTION('ref_axis',(1.,0.,0.));
#19362=DIRECTION('',(-0.652888256250376,0.,0.757454239443112));
#19363=DIRECTION('center_axis',(0.,1.,0.));
#19364=DIRECTION('ref_axis',(1.,0.,0.));
#19365=DIRECTION('',(-0.481137489758911,0.,0.87664514824899));
#19366=DIRECTION('center_axis',(0.,1.,0.));
#19367=DIRECTION('ref_axis',(1.,0.,0.));
#19368=DIRECTION('',(-0.288358706211123,0.,0.957522457466271));
#19369=DIRECTION('center_axis',(0.,1.,0.));
#19370=DIRECTION('ref_axis',(1.,0.,0.));
#19371=DIRECTION('',(-0.0829772635033118,0.,0.996551440589748));
#19372=DIRECTION('center_axis',(0.,1.,0.));
#19373=DIRECTION('ref_axis',(1.,0.,0.));
#19374=DIRECTION('',(0.126030683788633,0.,0.992026343775088));
#19375=DIRECTION('center_axis',(0.,1.,0.));
#19376=DIRECTION('ref_axis',(1.,0.,0.));
#19377=DIRECTION('',(0.32953048543679,0.,0.944144935466898));
#19378=DIRECTION('center_axis',(0.,1.,0.));
#19379=DIRECTION('ref_axis',(1.,0.,0.));
#19380=DIRECTION('',(0.518628223608571,0.,0.854999862968772));
#19381=DIRECTION('center_axis',(0.,1.,0.));
#19382=DIRECTION('ref_axis',(1.,0.,0.));
#19383=DIRECTION('',(0.685059419754315,0.,0.728487193714399));
#19384=DIRECTION('center_axis',(0.,1.,0.));
#19385=DIRECTION('ref_axis',(1.,0.,0.));
#19386=DIRECTION('',(0.821550231977102,0.,0.570136138425175));
#19387=DIRECTION('center_axis',(0.,1.,0.));
#19388=DIRECTION('ref_axis',(1.,0.,0.));
#19389=DIRECTION('',(0.922135356827004,0.,0.386867398070107));
#19390=DIRECTION('center_axis',(0.,1.,0.));
#19391=DIRECTION('ref_axis',(1.,0.,0.));
#19392=DIRECTION('center_axis',(0.,-1.,0.));
#19393=DIRECTION('ref_axis',(0.,0.,1.));
#19394=DIRECTION('center_axis',(0.,1.,0.));
#19395=DIRECTION('ref_axis',(1.,0.,0.));
#19396=DIRECTION('center_axis',(0.,1.,0.));
#19397=DIRECTION('ref_axis',(0.,0.,1.));
#19398=DIRECTION('center_axis',(0.,1.,0.));
#19399=DIRECTION('ref_axis',(1.,0.,0.));
#19400=DIRECTION('center_axis',(0.,1.,0.));
#19401=DIRECTION('ref_axis',(0.,0.,1.));
#19402=DIRECTION('center_axis',(0.,1.,0.));
#19403=DIRECTION('ref_axis',(1.,0.,0.));
#19404=DIRECTION('center_axis',(0.,1.,0.));
#19405=DIRECTION('ref_axis',(0.,0.,1.));
#19406=DIRECTION('center_axis',(0.,1.,0.));
#19407=DIRECTION('ref_axis',(1.,0.,0.));
#19408=DIRECTION('center_axis',(0.,1.,0.));
#19409=DIRECTION('ref_axis',(0.,0.,1.));
#19410=DIRECTION('center_axis',(0.,-1.,0.));
#19411=DIRECTION('ref_axis',(0.,0.,1.));
#19412=DIRECTION('center_axis',(0.,1.,0.));
#19413=DIRECTION('ref_axis',(1.,0.,0.));
#19414=DIRECTION('center_axis',(0.,1.,0.));
#19415=DIRECTION('ref_axis',(0.,0.,1.));
#19416=DIRECTION('center_axis',(0.,1.,0.));
#19417=DIRECTION('ref_axis',(1.,0.,0.));
#19418=DIRECTION('center_axis',(0.,1.,0.));
#19419=DIRECTION('ref_axis',(0.,0.,1.));
#19420=DIRECTION('center_axis',(0.,1.,0.));
#19421=DIRECTION('ref_axis',(1.,0.,0.));
#19422=DIRECTION('center_axis',(0.,1.,0.));
#19423=DIRECTION('ref_axis',(0.,0.,1.));
#19424=DIRECTION('center_axis',(0.,1.,0.));
#19425=DIRECTION('ref_axis',(1.,0.,0.));
#19426=DIRECTION('center_axis',(0.,1.,0.));
#19427=DIRECTION('ref_axis',(0.,0.,1.));
#19428=DIRECTION('center_axis',(0.,-1.,0.));
#19429=DIRECTION('ref_axis',(0.,0.,1.));
#19430=DIRECTION('center_axis',(0.,1.,0.));
#19431=DIRECTION('ref_axis',(1.,0.,0.));
#19432=DIRECTION('center_axis',(0.,1.,0.));
#19433=DIRECTION('ref_axis',(0.,0.,1.));
#19434=DIRECTION('center_axis',(0.,1.,0.));
#19435=DIRECTION('ref_axis',(1.,0.,0.));
#19436=DIRECTION('center_axis',(0.,1.,0.));
#19437=DIRECTION('ref_axis',(0.,0.,1.));
#19438=DIRECTION('center_axis',(0.,1.,0.));
#19439=DIRECTION('ref_axis',(1.,0.,0.));
#19440=DIRECTION('center_axis',(0.,1.,0.));
#19441=DIRECTION('ref_axis',(0.,0.,1.));
#19442=DIRECTION('center_axis',(0.,1.,0.));
#19443=DIRECTION('ref_axis',(1.,0.,0.));
#19444=DIRECTION('center_axis',(0.,1.,0.));
#19445=DIRECTION('ref_axis',(0.,0.,1.));
#19446=DIRECTION('center_axis',(0.,-1.,0.));
#19447=DIRECTION('ref_axis',(0.,0.,1.));
#19448=DIRECTION('center_axis',(0.,1.,0.));
#19449=DIRECTION('ref_axis',(1.,0.,0.));
#19450=DIRECTION('center_axis',(0.,1.,0.));
#19451=DIRECTION('ref_axis',(0.,0.,1.));
#19452=DIRECTION('center_axis',(0.,1.,0.));
#19453=DIRECTION('ref_axis',(1.,0.,0.));
#19454=DIRECTION('center_axis',(0.,1.,0.));
#19455=DIRECTION('ref_axis',(0.,0.,1.));
#19456=DIRECTION('center_axis',(0.,1.,0.));
#19457=DIRECTION('ref_axis',(1.,0.,0.));
#19458=DIRECTION('center_axis',(0.,1.,0.));
#19459=DIRECTION('ref_axis',(0.,0.,1.));
#19460=DIRECTION('center_axis',(0.,1.,0.));
#19461=DIRECTION('ref_axis',(1.,0.,0.));
#19462=DIRECTION('center_axis',(0.,1.,0.));
#19463=DIRECTION('ref_axis',(0.,0.,1.));
#19464=DIRECTION('center_axis',(0.,-1.,0.));
#19465=DIRECTION('ref_axis',(0.,0.,1.));
#19466=DIRECTION('center_axis',(0.,1.,0.));
#19467=DIRECTION('ref_axis',(1.,0.,0.));
#19468=DIRECTION('center_axis',(0.,1.,0.));
#19469=DIRECTION('ref_axis',(0.,0.,1.));
#19470=DIRECTION('center_axis',(0.,1.,0.));
#19471=DIRECTION('ref_axis',(1.,0.,0.));
#19472=DIRECTION('center_axis',(0.,1.,0.));
#19473=DIRECTION('ref_axis',(0.,0.,1.));
#19474=DIRECTION('center_axis',(0.,1.,0.));
#19475=DIRECTION('ref_axis',(1.,0.,0.));
#19476=DIRECTION('center_axis',(0.,1.,0.));
#19477=DIRECTION('ref_axis',(0.,0.,1.));
#19478=DIRECTION('center_axis',(0.,1.,0.));
#19479=DIRECTION('ref_axis',(1.,0.,0.));
#19480=DIRECTION('center_axis',(0.,1.,0.));
#19481=DIRECTION('ref_axis',(0.,0.,1.));
#19482=DIRECTION('center_axis',(0.,-1.,0.));
#19483=DIRECTION('ref_axis',(0.,0.,1.));
#19484=DIRECTION('center_axis',(0.,1.,0.));
#19485=DIRECTION('ref_axis',(1.,0.,0.));
#19486=DIRECTION('center_axis',(0.,1.,0.));
#19487=DIRECTION('ref_axis',(0.,0.,1.));
#19488=DIRECTION('center_axis',(0.,1.,0.));
#19489=DIRECTION('ref_axis',(1.,0.,0.));
#19490=DIRECTION('center_axis',(0.,1.,0.));
#19491=DIRECTION('ref_axis',(0.,0.,1.));
#19492=DIRECTION('center_axis',(0.,1.,0.));
#19493=DIRECTION('ref_axis',(1.,0.,0.));
#19494=DIRECTION('center_axis',(0.,1.,0.));
#19495=DIRECTION('ref_axis',(0.,0.,1.));
#19496=DIRECTION('center_axis',(0.,1.,0.));
#19497=DIRECTION('ref_axis',(1.,0.,0.));
#19498=DIRECTION('center_axis',(0.,1.,0.));
#19499=DIRECTION('ref_axis',(0.,0.,1.));
#19500=DIRECTION('center_axis',(0.,-1.,0.));
#19501=DIRECTION('ref_axis',(0.,0.,1.));
#19502=DIRECTION('center_axis',(0.,1.,0.));
#19503=DIRECTION('ref_axis',(1.,0.,0.));
#19504=DIRECTION('center_axis',(0.,1.,0.));
#19505=DIRECTION('ref_axis',(0.,0.,1.));
#19506=DIRECTION('center_axis',(0.,1.,0.));
#19507=DIRECTION('ref_axis',(1.,0.,0.));
#19508=DIRECTION('center_axis',(0.,1.,0.));
#19509=DIRECTION('ref_axis',(0.,0.,1.));
#19510=DIRECTION('center_axis',(0.,1.,0.));
#19511=DIRECTION('ref_axis',(1.,0.,0.));
#19512=DIRECTION('center_axis',(0.,1.,0.));
#19513=DIRECTION('ref_axis',(0.,0.,1.));
#19514=DIRECTION('center_axis',(0.,1.,0.));
#19515=DIRECTION('ref_axis',(1.,0.,0.));
#19516=DIRECTION('center_axis',(0.,1.,0.));
#19517=DIRECTION('ref_axis',(0.,0.,1.));
#19518=DIRECTION('center_axis',(0.,-1.,0.));
#19519=DIRECTION('ref_axis',(0.,0.,1.));
#19520=DIRECTION('center_axis',(0.,1.,0.));
#19521=DIRECTION('ref_axis',(1.,0.,0.));
#19522=DIRECTION('center_axis',(0.,1.,0.));
#19523=DIRECTION('ref_axis',(0.,0.,1.));
#19524=DIRECTION('center_axis',(0.,1.,0.));
#19525=DIRECTION('ref_axis',(1.,0.,0.));
#19526=DIRECTION('center_axis',(0.,1.,0.));
#19527=DIRECTION('ref_axis',(0.,0.,1.));
#19528=DIRECTION('center_axis',(0.,1.,0.));
#19529=DIRECTION('ref_axis',(1.,0.,0.));
#19530=DIRECTION('center_axis',(0.,1.,0.));
#19531=DIRECTION('ref_axis',(0.,0.,1.));
#19532=DIRECTION('center_axis',(0.,1.,0.));
#19533=DIRECTION('ref_axis',(1.,0.,0.));
#19534=DIRECTION('center_axis',(0.,1.,0.));
#19535=DIRECTION('ref_axis',(0.,0.,1.));
#19536=DIRECTION('center_axis',(0.,-1.,0.));
#19537=DIRECTION('ref_axis',(0.,0.,1.));
#19538=DIRECTION('center_axis',(0.,1.,0.));
#19539=DIRECTION('ref_axis',(1.,0.,0.));
#19540=DIRECTION('center_axis',(0.,1.,0.));
#19541=DIRECTION('ref_axis',(0.,0.,1.));
#19542=DIRECTION('center_axis',(0.,1.,0.));
#19543=DIRECTION('ref_axis',(1.,0.,0.));
#19544=DIRECTION('center_axis',(0.,1.,0.));
#19545=DIRECTION('ref_axis',(0.,0.,1.));
#19546=DIRECTION('center_axis',(0.,1.,0.));
#19547=DIRECTION('ref_axis',(1.,0.,0.));
#19548=DIRECTION('center_axis',(0.,1.,0.));
#19549=DIRECTION('ref_axis',(0.,0.,1.));
#19550=DIRECTION('center_axis',(0.,1.,0.));
#19551=DIRECTION('ref_axis',(1.,0.,0.));
#19552=DIRECTION('center_axis',(0.,1.,0.));
#19553=DIRECTION('ref_axis',(0.,0.,1.));
#19554=DIRECTION('center_axis',(0.,-1.,0.));
#19555=DIRECTION('ref_axis',(0.,0.,1.));
#19556=DIRECTION('center_axis',(0.,1.,0.));
#19557=DIRECTION('ref_axis',(1.,0.,0.));
#19558=DIRECTION('center_axis',(0.,1.,0.));
#19559=DIRECTION('ref_axis',(0.,0.,1.));
#19560=DIRECTION('center_axis',(0.,1.,0.));
#19561=DIRECTION('ref_axis',(1.,0.,0.));
#19562=DIRECTION('center_axis',(0.,1.,0.));
#19563=DIRECTION('ref_axis',(0.,0.,1.));
#19564=DIRECTION('center_axis',(0.,1.,0.));
#19565=DIRECTION('ref_axis',(1.,0.,0.));
#19566=DIRECTION('center_axis',(0.,1.,0.));
#19567=DIRECTION('ref_axis',(0.,0.,1.));
#19568=DIRECTION('center_axis',(0.,1.,0.));
#19569=DIRECTION('ref_axis',(1.,0.,0.));
#19570=DIRECTION('center_axis',(0.,1.,0.));
#19571=DIRECTION('ref_axis',(0.,0.,1.));
#19572=DIRECTION('center_axis',(0.,-1.,0.));
#19573=DIRECTION('ref_axis',(0.,0.,1.));
#19574=DIRECTION('center_axis',(0.,1.,0.));
#19575=DIRECTION('ref_axis',(1.,0.,0.));
#19576=DIRECTION('center_axis',(0.,1.,0.));
#19577=DIRECTION('ref_axis',(0.,0.,1.));
#19578=DIRECTION('center_axis',(0.,1.,0.));
#19579=DIRECTION('ref_axis',(1.,0.,0.));
#19580=DIRECTION('center_axis',(0.,1.,0.));
#19581=DIRECTION('ref_axis',(0.,0.,1.));
#19582=DIRECTION('center_axis',(0.,1.,0.));
#19583=DIRECTION('ref_axis',(1.,0.,0.));
#19584=DIRECTION('center_axis',(0.,1.,0.));
#19585=DIRECTION('ref_axis',(0.,0.,1.));
#19586=DIRECTION('center_axis',(0.,1.,0.));
#19587=DIRECTION('ref_axis',(1.,0.,0.));
#19588=DIRECTION('center_axis',(0.,1.,0.));
#19589=DIRECTION('ref_axis',(0.,0.,1.));
#19590=DIRECTION('center_axis',(0.,-1.,0.));
#19591=DIRECTION('ref_axis',(0.,0.,1.));
#19592=DIRECTION('center_axis',(0.,1.,0.));
#19593=DIRECTION('ref_axis',(1.,0.,0.));
#19594=DIRECTION('center_axis',(0.,1.,0.));
#19595=DIRECTION('ref_axis',(0.,0.,1.));
#19596=DIRECTION('center_axis',(0.,1.,0.));
#19597=DIRECTION('ref_axis',(1.,0.,0.));
#19598=DIRECTION('center_axis',(0.,1.,0.));
#19599=DIRECTION('ref_axis',(0.,0.,1.));
#19600=DIRECTION('center_axis',(0.,1.,0.));
#19601=DIRECTION('ref_axis',(1.,0.,0.));
#19602=DIRECTION('center_axis',(0.,1.,0.));
#19603=DIRECTION('ref_axis',(0.,0.,1.));
#19604=DIRECTION('center_axis',(0.,1.,0.));
#19605=DIRECTION('ref_axis',(1.,0.,0.));
#19606=DIRECTION('center_axis',(0.,1.,0.));
#19607=DIRECTION('ref_axis',(0.,0.,1.));
#19608=DIRECTION('center_axis',(0.,-1.,0.));
#19609=DIRECTION('ref_axis',(0.,0.,1.));
#19610=DIRECTION('center_axis',(0.,1.,0.));
#19611=DIRECTION('ref_axis',(1.,0.,0.));
#19612=DIRECTION('center_axis',(0.,1.,0.));
#19613=DIRECTION('ref_axis',(0.,0.,1.));
#19614=DIRECTION('center_axis',(0.,1.,0.));
#19615=DIRECTION('ref_axis',(1.,0.,0.));
#19616=DIRECTION('center_axis',(0.,1.,0.));
#19617=DIRECTION('ref_axis',(0.,0.,1.));
#19618=DIRECTION('center_axis',(0.,1.,0.));
#19619=DIRECTION('ref_axis',(1.,0.,0.));
#19620=DIRECTION('center_axis',(0.,1.,0.));
#19621=DIRECTION('ref_axis',(0.,0.,1.));
#19622=DIRECTION('center_axis',(0.,1.,0.));
#19623=DIRECTION('ref_axis',(1.,0.,0.));
#19624=DIRECTION('center_axis',(0.,1.,0.));
#19625=DIRECTION('ref_axis',(0.,0.,1.));
#19626=DIRECTION('center_axis',(0.,-1.,0.));
#19627=DIRECTION('ref_axis',(0.,0.,1.));
#19628=DIRECTION('center_axis',(0.,1.,0.));
#19629=DIRECTION('ref_axis',(1.,0.,0.));
#19630=DIRECTION('center_axis',(0.,1.,0.));
#19631=DIRECTION('ref_axis',(0.,0.,1.));
#19632=DIRECTION('center_axis',(0.,1.,0.));
#19633=DIRECTION('ref_axis',(1.,0.,0.));
#19634=DIRECTION('center_axis',(0.,1.,0.));
#19635=DIRECTION('ref_axis',(0.,0.,1.));
#19636=DIRECTION('center_axis',(0.,1.,0.));
#19637=DIRECTION('ref_axis',(1.,0.,0.));
#19638=DIRECTION('center_axis',(0.,1.,0.));
#19639=DIRECTION('ref_axis',(0.,0.,1.));
#19640=DIRECTION('center_axis',(0.,1.,0.));
#19641=DIRECTION('ref_axis',(1.,0.,0.));
#19642=DIRECTION('center_axis',(0.,1.,0.));
#19643=DIRECTION('ref_axis',(0.,0.,1.));
#19644=DIRECTION('center_axis',(0.,-1.,0.));
#19645=DIRECTION('ref_axis',(0.,0.,1.));
#19646=DIRECTION('center_axis',(0.,1.,0.));
#19647=DIRECTION('ref_axis',(1.,0.,0.));
#19648=DIRECTION('center_axis',(0.,1.,0.));
#19649=DIRECTION('ref_axis',(0.,0.,1.));
#19650=DIRECTION('center_axis',(0.,1.,0.));
#19651=DIRECTION('ref_axis',(1.,0.,0.));
#19652=DIRECTION('center_axis',(0.,1.,0.));
#19653=DIRECTION('ref_axis',(0.,0.,1.));
#19654=DIRECTION('center_axis',(0.,1.,0.));
#19655=DIRECTION('ref_axis',(1.,0.,0.));
#19656=DIRECTION('center_axis',(0.,1.,0.));
#19657=DIRECTION('ref_axis',(0.,0.,1.));
#19658=DIRECTION('center_axis',(0.,1.,0.));
#19659=DIRECTION('ref_axis',(1.,0.,0.));
#19660=DIRECTION('center_axis',(0.,1.,0.));
#19661=DIRECTION('ref_axis',(0.,0.,1.));
#19662=DIRECTION('center_axis',(0.,-1.,0.));
#19663=DIRECTION('ref_axis',(0.,0.,1.));
#19664=DIRECTION('center_axis',(0.,1.,0.));
#19665=DIRECTION('ref_axis',(1.,0.,0.));
#19666=DIRECTION('center_axis',(0.,1.,0.));
#19667=DIRECTION('ref_axis',(0.,0.,1.));
#19668=DIRECTION('center_axis',(0.,1.,0.));
#19669=DIRECTION('ref_axis',(1.,0.,0.));
#19670=DIRECTION('center_axis',(0.,1.,0.));
#19671=DIRECTION('ref_axis',(0.,0.,1.));
#19672=DIRECTION('center_axis',(0.,1.,0.));
#19673=DIRECTION('ref_axis',(1.,0.,0.));
#19674=DIRECTION('center_axis',(0.,1.,0.));
#19675=DIRECTION('ref_axis',(0.,0.,1.));
#19676=DIRECTION('center_axis',(0.,1.,0.));
#19677=DIRECTION('ref_axis',(1.,0.,0.));
#19678=DIRECTION('center_axis',(0.,1.,0.));
#19679=DIRECTION('ref_axis',(0.,0.,1.));
#19680=DIRECTION('center_axis',(0.,-1.,0.));
#19681=DIRECTION('ref_axis',(0.,0.,1.));
#19682=DIRECTION('center_axis',(0.,1.,0.));
#19683=DIRECTION('ref_axis',(1.,0.,0.));
#19684=DIRECTION('center_axis',(0.,1.,0.));
#19685=DIRECTION('ref_axis',(0.,0.,1.));
#19686=DIRECTION('center_axis',(0.,1.,0.));
#19687=DIRECTION('ref_axis',(1.,0.,0.));
#19688=DIRECTION('center_axis',(0.,1.,0.));
#19689=DIRECTION('ref_axis',(0.,0.,1.));
#19690=DIRECTION('center_axis',(0.,1.,0.));
#19691=DIRECTION('ref_axis',(1.,0.,0.));
#19692=DIRECTION('center_axis',(0.,1.,0.));
#19693=DIRECTION('ref_axis',(0.,0.,1.));
#19694=DIRECTION('center_axis',(0.,1.,0.));
#19695=DIRECTION('ref_axis',(1.,0.,0.));
#19696=DIRECTION('center_axis',(0.,1.,0.));
#19697=DIRECTION('ref_axis',(0.,0.,1.));
#19698=DIRECTION('center_axis',(0.,-1.,0.));
#19699=DIRECTION('ref_axis',(0.,0.,1.));
#19700=DIRECTION('center_axis',(0.,1.,0.));
#19701=DIRECTION('ref_axis',(1.,0.,0.));
#19702=DIRECTION('center_axis',(0.,1.,0.));
#19703=DIRECTION('ref_axis',(0.,0.,1.));
#19704=DIRECTION('center_axis',(0.,1.,0.));
#19705=DIRECTION('ref_axis',(1.,0.,0.));
#19706=DIRECTION('center_axis',(0.,1.,0.));
#19707=DIRECTION('ref_axis',(0.,0.,1.));
#19708=DIRECTION('center_axis',(0.,1.,0.));
#19709=DIRECTION('ref_axis',(1.,0.,0.));
#19710=DIRECTION('center_axis',(0.,1.,0.));
#19711=DIRECTION('ref_axis',(0.,0.,1.));
#19712=DIRECTION('center_axis',(0.,1.,0.));
#19713=DIRECTION('ref_axis',(1.,0.,0.));
#19714=DIRECTION('center_axis',(0.,1.,0.));
#19715=DIRECTION('ref_axis',(0.,0.,1.));
#19716=DIRECTION('center_axis',(0.,-1.,0.));
#19717=DIRECTION('ref_axis',(0.,0.,1.));
#19718=DIRECTION('center_axis',(0.,1.,0.));
#19719=DIRECTION('ref_axis',(1.,0.,0.));
#19720=DIRECTION('center_axis',(0.,1.,0.));
#19721=DIRECTION('ref_axis',(0.,0.,1.));
#19722=DIRECTION('center_axis',(0.,1.,0.));
#19723=DIRECTION('ref_axis',(1.,0.,0.));
#19724=DIRECTION('center_axis',(0.,1.,0.));
#19725=DIRECTION('ref_axis',(0.,0.,1.));
#19726=DIRECTION('center_axis',(0.,1.,0.));
#19727=DIRECTION('ref_axis',(1.,0.,0.));
#19728=DIRECTION('center_axis',(0.,1.,0.));
#19729=DIRECTION('ref_axis',(0.,0.,1.));
#19730=DIRECTION('center_axis',(0.,1.,0.));
#19731=DIRECTION('ref_axis',(1.,0.,0.));
#19732=DIRECTION('center_axis',(0.,1.,0.));
#19733=DIRECTION('ref_axis',(0.,0.,1.));
#19734=DIRECTION('center_axis',(0.,-1.,0.));
#19735=DIRECTION('ref_axis',(0.,0.,1.));
#19736=DIRECTION('center_axis',(0.,1.,0.));
#19737=DIRECTION('ref_axis',(1.,0.,0.));
#19738=DIRECTION('center_axis',(0.,1.,0.));
#19739=DIRECTION('ref_axis',(0.,0.,1.));
#19740=DIRECTION('center_axis',(0.,1.,0.));
#19741=DIRECTION('ref_axis',(1.,0.,0.));
#19742=DIRECTION('center_axis',(0.,1.,0.));
#19743=DIRECTION('ref_axis',(0.,0.,1.));
#19744=DIRECTION('center_axis',(0.,1.,0.));
#19745=DIRECTION('ref_axis',(1.,0.,0.));
#19746=DIRECTION('center_axis',(0.,1.,0.));
#19747=DIRECTION('ref_axis',(0.,0.,1.));
#19748=DIRECTION('center_axis',(0.,1.,0.));
#19749=DIRECTION('ref_axis',(1.,0.,0.));
#19750=DIRECTION('center_axis',(0.,1.,0.));
#19751=DIRECTION('ref_axis',(0.,0.,1.));
#19752=DIRECTION('center_axis',(0.,-1.,0.));
#19753=DIRECTION('ref_axis',(0.,0.,1.));
#19754=DIRECTION('center_axis',(0.,1.,0.));
#19755=DIRECTION('ref_axis',(1.,0.,0.));
#19756=DIRECTION('center_axis',(0.,1.,0.));
#19757=DIRECTION('ref_axis',(0.,0.,1.));
#19758=DIRECTION('center_axis',(0.,1.,0.));
#19759=DIRECTION('ref_axis',(1.,0.,0.));
#19760=DIRECTION('center_axis',(0.,1.,0.));
#19761=DIRECTION('ref_axis',(0.,0.,1.));
#19762=DIRECTION('center_axis',(0.,1.,0.));
#19763=DIRECTION('ref_axis',(1.,0.,0.));
#19764=DIRECTION('center_axis',(0.,1.,0.));
#19765=DIRECTION('ref_axis',(0.,0.,1.));
#19766=DIRECTION('center_axis',(0.,1.,0.));
#19767=DIRECTION('ref_axis',(1.,0.,0.));
#19768=DIRECTION('center_axis',(0.,1.,0.));
#19769=DIRECTION('ref_axis',(0.,0.,1.));
#19770=DIRECTION('center_axis',(0.,-1.,0.));
#19771=DIRECTION('ref_axis',(0.,0.,1.));
#19772=DIRECTION('center_axis',(0.,1.,0.));
#19773=DIRECTION('ref_axis',(1.,0.,0.));
#19774=DIRECTION('center_axis',(0.,1.,0.));
#19775=DIRECTION('ref_axis',(0.,0.,1.));
#19776=DIRECTION('center_axis',(0.,1.,0.));
#19777=DIRECTION('ref_axis',(1.,0.,0.));
#19778=DIRECTION('center_axis',(0.,1.,0.));
#19779=DIRECTION('ref_axis',(0.,0.,1.));
#19780=DIRECTION('center_axis',(0.,1.,0.));
#19781=DIRECTION('ref_axis',(1.,0.,0.));
#19782=DIRECTION('center_axis',(0.,1.,0.));
#19783=DIRECTION('ref_axis',(0.,0.,1.));
#19784=DIRECTION('center_axis',(0.,1.,0.));
#19785=DIRECTION('ref_axis',(1.,0.,0.));
#19786=DIRECTION('center_axis',(0.,1.,0.));
#19787=DIRECTION('ref_axis',(0.,0.,1.));
#19788=DIRECTION('center_axis',(0.,-1.,0.));
#19789=DIRECTION('ref_axis',(0.,0.,1.));
#19790=DIRECTION('center_axis',(0.,1.,0.));
#19791=DIRECTION('ref_axis',(1.,0.,0.));
#19792=DIRECTION('center_axis',(0.,1.,0.));
#19793=DIRECTION('ref_axis',(0.,0.,1.));
#19794=DIRECTION('center_axis',(0.,1.,0.));
#19795=DIRECTION('ref_axis',(1.,0.,0.));
#19796=DIRECTION('center_axis',(0.,1.,0.));
#19797=DIRECTION('ref_axis',(0.,0.,1.));
#19798=DIRECTION('center_axis',(0.,1.,0.));
#19799=DIRECTION('ref_axis',(1.,0.,0.));
#19800=DIRECTION('center_axis',(0.,1.,0.));
#19801=DIRECTION('ref_axis',(0.,0.,1.));
#19802=DIRECTION('center_axis',(0.,1.,0.));
#19803=DIRECTION('ref_axis',(1.,0.,0.));
#19804=DIRECTION('center_axis',(0.,1.,0.));
#19805=DIRECTION('ref_axis',(0.,0.,1.));
#19806=DIRECTION('center_axis',(0.,-1.,0.));
#19807=DIRECTION('ref_axis',(0.,0.,1.));
#19808=DIRECTION('center_axis',(0.,1.,0.));
#19809=DIRECTION('ref_axis',(1.,0.,0.));
#19810=DIRECTION('center_axis',(0.,1.,0.));
#19811=DIRECTION('ref_axis',(0.,0.,1.));
#19812=DIRECTION('center_axis',(0.,1.,0.));
#19813=DIRECTION('ref_axis',(1.,0.,0.));
#19814=DIRECTION('center_axis',(0.,1.,0.));
#19815=DIRECTION('ref_axis',(0.,0.,1.));
#19816=DIRECTION('center_axis',(0.,1.,0.));
#19817=DIRECTION('ref_axis',(1.,0.,0.));
#19818=DIRECTION('center_axis',(0.,1.,0.));
#19819=DIRECTION('ref_axis',(0.,0.,1.));
#19820=DIRECTION('center_axis',(0.,1.,0.));
#19821=DIRECTION('ref_axis',(1.,0.,0.));
#19822=DIRECTION('center_axis',(0.,1.,0.));
#19823=DIRECTION('ref_axis',(0.,0.,1.));
#19824=DIRECTION('center_axis',(0.,-1.,0.));
#19825=DIRECTION('ref_axis',(0.,0.,1.));
#19826=DIRECTION('center_axis',(0.,1.,0.));
#19827=DIRECTION('ref_axis',(1.,0.,0.));
#19828=DIRECTION('center_axis',(0.,1.,0.));
#19829=DIRECTION('ref_axis',(0.,0.,1.));
#19830=DIRECTION('center_axis',(0.,1.,0.));
#19831=DIRECTION('ref_axis',(1.,0.,0.));
#19832=DIRECTION('center_axis',(0.,1.,0.));
#19833=DIRECTION('ref_axis',(0.,0.,1.));
#19834=DIRECTION('center_axis',(0.,1.,0.));
#19835=DIRECTION('ref_axis',(1.,0.,0.));
#19836=DIRECTION('center_axis',(0.,1.,0.));
#19837=DIRECTION('ref_axis',(0.,0.,1.));
#19838=DIRECTION('center_axis',(0.,1.,0.));
#19839=DIRECTION('ref_axis',(1.,0.,0.));
#19840=DIRECTION('center_axis',(0.,1.,0.));
#19841=DIRECTION('ref_axis',(0.,0.,1.));
#19842=DIRECTION('center_axis',(0.,-1.,0.));
#19843=DIRECTION('ref_axis',(0.,0.,1.));
#19844=DIRECTION('center_axis',(0.,1.,0.));
#19845=DIRECTION('ref_axis',(1.,0.,0.));
#19846=DIRECTION('center_axis',(0.,1.,0.));
#19847=DIRECTION('ref_axis',(0.,0.,1.));
#19848=DIRECTION('center_axis',(0.,1.,0.));
#19849=DIRECTION('ref_axis',(1.,0.,0.));
#19850=DIRECTION('center_axis',(0.,1.,0.));
#19851=DIRECTION('ref_axis',(0.,0.,1.));
#19852=DIRECTION('center_axis',(0.,1.,0.));
#19853=DIRECTION('ref_axis',(1.,0.,0.));
#19854=DIRECTION('center_axis',(0.,1.,0.));
#19855=DIRECTION('ref_axis',(0.,0.,1.));
#19856=DIRECTION('center_axis',(0.,1.,0.));
#19857=DIRECTION('ref_axis',(1.,0.,0.));
#19858=DIRECTION('center_axis',(0.,1.,0.));
#19859=DIRECTION('ref_axis',(0.,0.,1.));
#19860=DIRECTION('center_axis',(0.,-1.,0.));
#19861=DIRECTION('ref_axis',(0.,0.,1.));
#19862=DIRECTION('center_axis',(0.,1.,0.));
#19863=DIRECTION('ref_axis',(1.,0.,0.));
#19864=DIRECTION('center_axis',(0.,1.,0.));
#19865=DIRECTION('ref_axis',(0.,0.,1.));
#19866=DIRECTION('center_axis',(0.,1.,0.));
#19867=DIRECTION('ref_axis',(1.,0.,0.));
#19868=DIRECTION('center_axis',(0.,1.,0.));
#19869=DIRECTION('ref_axis',(0.,0.,1.));
#19870=DIRECTION('center_axis',(0.,1.,0.));
#19871=DIRECTION('ref_axis',(1.,0.,0.));
#19872=DIRECTION('center_axis',(0.,1.,0.));
#19873=DIRECTION('ref_axis',(0.,0.,1.));
#19874=DIRECTION('center_axis',(0.,1.,0.));
#19875=DIRECTION('ref_axis',(1.,0.,0.));
#19876=DIRECTION('center_axis',(0.,1.,0.));
#19877=DIRECTION('ref_axis',(0.,0.,1.));
#19878=DIRECTION('center_axis',(0.,-1.,0.));
#19879=DIRECTION('ref_axis',(0.,0.,1.));
#19880=DIRECTION('center_axis',(0.,1.,0.));
#19881=DIRECTION('ref_axis',(1.,0.,0.));
#19882=DIRECTION('center_axis',(0.,-1.,0.));
#19883=DIRECTION('ref_axis',(0.,0.,1.));
#19884=DIRECTION('center_axis',(0.,1.,0.));
#19885=DIRECTION('ref_axis',(1.,0.,0.));
#19886=DIRECTION('center_axis',(0.,1.,0.));
#19887=DIRECTION('ref_axis',(0.,0.,1.));
#19888=DIRECTION('center_axis',(0.,1.,0.));
#19889=DIRECTION('ref_axis',(1.,0.,0.));
#19890=DIRECTION('center_axis',(0.,1.,0.));
#19891=DIRECTION('ref_axis',(0.,0.,1.));
#19892=DIRECTION('center_axis',(0.,1.,0.));
#19893=DIRECTION('ref_axis',(1.,0.,0.));
#19894=DIRECTION('center_axis',(0.,1.,0.));
#19895=DIRECTION('ref_axis',(0.,0.,1.));
#19896=DIRECTION('center_axis',(0.,1.,0.));
#19897=DIRECTION('ref_axis',(1.,0.,0.));
#19898=DIRECTION('center_axis',(0.,1.,0.));
#19899=DIRECTION('ref_axis',(0.,0.,1.));
#19900=DIRECTION('center_axis',(0.,-1.,0.));
#19901=DIRECTION('ref_axis',(0.,0.,1.));
#19902=DIRECTION('center_axis',(0.,1.,0.));
#19903=DIRECTION('ref_axis',(1.,0.,0.));
#19904=DIRECTION('center_axis',(0.,1.,0.));
#19905=DIRECTION('ref_axis',(0.,0.,1.));
#19906=DIRECTION('center_axis',(0.,1.,0.));
#19907=DIRECTION('ref_axis',(1.,0.,0.));
#19908=DIRECTION('center_axis',(0.,1.,0.));
#19909=DIRECTION('ref_axis',(0.,0.,1.));
#19910=DIRECTION('center_axis',(0.,1.,0.));
#19911=DIRECTION('ref_axis',(1.,0.,0.));
#19912=DIRECTION('center_axis',(0.,1.,0.));
#19913=DIRECTION('ref_axis',(0.,0.,1.));
#19914=DIRECTION('center_axis',(0.,1.,0.));
#19915=DIRECTION('ref_axis',(1.,0.,0.));
#19916=DIRECTION('center_axis',(0.,1.,0.));
#19917=DIRECTION('ref_axis',(0.,0.,1.));
#19918=DIRECTION('center_axis',(0.,1.,0.));
#19919=DIRECTION('ref_axis',(1.,0.,0.));
#19920=DIRECTION('center_axis',(0.,1.,0.));
#19921=DIRECTION('ref_axis',(0.,0.,1.));
#19922=DIRECTION('center_axis',(0.,1.,0.));
#19923=DIRECTION('ref_axis',(0.,0.,1.));
#19924=DIRECTION('center_axis',(0.,1.,0.));
#19925=DIRECTION('ref_axis',(1.,0.,0.));
#19926=DIRECTION('center_axis',(0.,1.,0.));
#19927=DIRECTION('ref_axis',(1.,0.,0.));
#19928=DIRECTION('center_axis',(0.,1.,0.));
#19929=DIRECTION('ref_axis',(0.,0.,1.));
#19930=DIRECTION('center_axis',(0.,1.,0.));
#19931=DIRECTION('ref_axis',(0.,0.,1.));
#19932=DIRECTION('axis',(0.,0.,1.));
#19933=DIRECTION('refdir',(1.,0.,0.));
#19934=DIRECTION('center_axis',(1.,0.,0.));
#19935=DIRECTION('ref_axis',(0.,0.,-1.));
#19936=DIRECTION('',(0.,0.,-1.));
#19937=DIRECTION('',(0.,1.,0.));
#19938=DIRECTION('',(0.,0.,1.));
#19939=DIRECTION('',(0.,1.,0.));
#19940=DIRECTION('center_axis',(0.,0.,1.));
#19941=DIRECTION('ref_axis',(1.,0.,0.));
#19942=DIRECTION('',(1.,0.,0.));
#19943=DIRECTION('',(0.,-1.,0.));
#19944=DIRECTION('',(-1.,0.,0.));
#19945=DIRECTION('center_axis',(-1.,0.,0.));
#19946=DIRECTION('ref_axis',(0.,0.,1.));
#19947=DIRECTION('',(0.,0.,1.));
#19948=DIRECTION('',(0.,-1.,0.));
#19949=DIRECTION('',(0.,0.,-1.));
#19950=DIRECTION('center_axis',(0.,-1.,0.));
#19951=DIRECTION('ref_axis',(0.,0.,-1.));
#19952=DIRECTION('center_axis',(0.,1.,0.));
#19953=DIRECTION('ref_axis',(1.,0.,0.));
#19954=DIRECTION('center_axis',(0.,1.,0.));
#19955=DIRECTION('ref_axis',(1.,0.,0.));
#19956=DIRECTION('center_axis',(0.,-1.,0.));
#19957=DIRECTION('ref_axis',(-1.22464679914735E-16,0.,-1.));
#19958=DIRECTION('center_axis',(0.,1.,0.));
#19959=DIRECTION('ref_axis',(1.,0.,0.));
#19960=DIRECTION('center_axis',(0.,1.,0.));
#19961=DIRECTION('ref_axis',(0.,0.,1.));
#19962=DIRECTION('center_axis',(0.,1.,0.));
#19963=DIRECTION('ref_axis',(1.,0.,0.));
#19964=DIRECTION('',(8.65956056235489E-17,-0.707106781186551,0.707106781186544));
#19965=DIRECTION('center_axis',(0.,1.,0.));
#19966=DIRECTION('ref_axis',(0.,0.,1.));
#19967=DIRECTION('center_axis',(0.,1.,0.));
#19968=DIRECTION('ref_axis',(1.,0.,0.));
#19969=DIRECTION('',(0.,-1.,0.));
#19970=DIRECTION('center_axis',(0.,-1.,0.));
#19971=DIRECTION('ref_axis',(0.,0.,-1.));
#19972=DIRECTION('center_axis',(0.,1.,0.));
#19973=DIRECTION('ref_axis',(1.,0.,0.));
#19974=DIRECTION('center_axis',(0.,1.,0.));
#19975=DIRECTION('ref_axis',(0.,0.,1.));
#19976=DIRECTION('center_axis',(0.,1.,0.));
#19977=DIRECTION('ref_axis',(1.,0.,0.));
#19978=DIRECTION('',(8.65956056235497E-17,-0.707106781186544,0.707106781186551));
#19979=DIRECTION('center_axis',(0.,1.,0.));
#19980=DIRECTION('ref_axis',(0.,0.,1.));
#19981=DIRECTION('center_axis',(0.,1.,0.));
#19982=DIRECTION('ref_axis',(1.,0.,0.));
#19983=DIRECTION('',(0.,-1.,0.));
#19984=DIRECTION('center_axis',(0.,-1.,0.));
#19985=DIRECTION('ref_axis',(0.,0.,-1.));
#19986=DIRECTION('center_axis',(0.,1.,0.));
#19987=DIRECTION('ref_axis',(1.,0.,0.));
#19988=DIRECTION('center_axis',(0.,1.,0.));
#19989=DIRECTION('ref_axis',(0.,0.,1.));
#19990=DIRECTION('center_axis',(0.,1.,0.));
#19991=DIRECTION('ref_axis',(1.,0.,0.));
#19992=DIRECTION('',(0.,-1.,0.));
#19993=DIRECTION('center_axis',(0.,1.,0.));
#19994=DIRECTION('ref_axis',(0.,0.,1.));
#19995=DIRECTION('center_axis',(0.,1.,0.));
#19996=DIRECTION('ref_axis',(1.,0.,0.));
#19997=DIRECTION('center_axis',(0.,1.,0.));
#19998=DIRECTION('ref_axis',(0.,0.,1.));
#19999=DIRECTION('center_axis',(0.,1.,0.));
#20000=DIRECTION('ref_axis',(1.,0.,0.));
#20001=DIRECTION('',(0.,-1.,0.));
#20002=DIRECTION('center_axis',(0.,-1.,0.));
#20003=DIRECTION('ref_axis',(0.,0.,1.));
#20004=DIRECTION('',(-8.65956056235497E-17,0.707106781186544,0.707106781186551));
#20005=DIRECTION('center_axis',(0.,1.,0.));
#20006=DIRECTION('ref_axis',(1.,0.,0.));
#20007=DIRECTION('center_axis',(0.,1.,0.));
#20008=DIRECTION('ref_axis',(0.,0.,1.));
#20009=DIRECTION('center_axis',(0.,1.,0.));
#20010=DIRECTION('ref_axis',(1.,0.,0.));
#20011=DIRECTION('center_axis',(0.,1.,0.));
#20012=DIRECTION('ref_axis',(0.,0.,1.));
#20013=DIRECTION('center_axis',(0.,1.,0.));
#20014=DIRECTION('ref_axis',(1.,0.,0.));
#20015=DIRECTION('',(0.,-1.,0.));
#20016=DIRECTION('center_axis',(0.,-1.,0.));
#20017=DIRECTION('ref_axis',(0.,0.,1.));
#20018=DIRECTION('',(-8.65956056235489E-17,0.707106781186551,0.707106781186544));
#20019=DIRECTION('center_axis',(0.,1.,0.));
#20020=DIRECTION('ref_axis',(1.,0.,0.));
#20021=DIRECTION('center_axis',(0.,1.,0.));
#20022=DIRECTION('ref_axis',(0.,0.,1.));
#20023=DIRECTION('center_axis',(0.,1.,0.));
#20024=DIRECTION('ref_axis',(1.,0.,0.));
#20025=DIRECTION('center_axis',(0.,1.,0.));
#20026=DIRECTION('ref_axis',(-1.22464679914735E-16,0.,-1.));
#20027=DIRECTION('center_axis',(0.,1.,0.));
#20028=DIRECTION('ref_axis',(1.,0.,0.));
#20029=DIRECTION('center_axis',(0.,1.,0.));
#20030=DIRECTION('ref_axis',(-1.22464679914735E-16,0.,-1.));
#20031=DIRECTION('axis',(0.,0.,1.));
#20032=DIRECTION('refdir',(1.,0.,0.));
#20033=DIRECTION('center_axis',(0.,0.,-1.));
#20034=DIRECTION('ref_axis',(-1.,0.,0.));
#20035=DIRECTION('center_axis',(0.,0.,1.));
#20036=DIRECTION('ref_axis',(1.,0.,0.));
#20037=DIRECTION('center_axis',(0.,0.,1.));
#20038=DIRECTION('ref_axis',(1.,0.,0.));
#20039=DIRECTION('center_axis',(0.,0.,1.));
#20040=DIRECTION('ref_axis',(1.,0.,0.));
#20041=DIRECTION('center_axis',(0.,0.,1.));
#20042=DIRECTION('ref_axis',(1.,0.,0.));
#20043=DIRECTION('',(0.707106781186549,8.65956056235496E-17,-0.707106781186546));
#20044=DIRECTION('center_axis',(0.,0.,1.));
#20045=DIRECTION('ref_axis',(1.,0.,0.));
#20046=DIRECTION('center_axis',(0.,0.,1.));
#20047=DIRECTION('ref_axis',(1.,0.,0.));
#20048=DIRECTION('',(0.,0.,-1.));
#20049=DIRECTION('center_axis',(0.,0.,-1.));
#20050=DIRECTION('ref_axis',(1.,0.,0.));
#20051=DIRECTION('',(0.707106781186547,-8.65956056235493E-17,0.707106781186548));
#20052=DIRECTION('center_axis',(0.,0.,1.));
#20053=DIRECTION('ref_axis',(1.,0.,0.));
#20054=DIRECTION('center_axis',(0.,0.,1.));
#20055=DIRECTION('ref_axis',(1.,0.,0.));
#20056=DIRECTION('center_axis',(0.,0.,1.));
#20057=DIRECTION('ref_axis',(1.,0.,0.));
#20058=DIRECTION('center_axis',(0.,0.,1.));
#20059=DIRECTION('ref_axis',(1.,0.,0.));
#20060=DIRECTION('center_axis',(0.,0.,1.));
#20061=DIRECTION('ref_axis',(1.,0.,0.));
#20062=DIRECTION('',(0.,0.,1.));
#20063=DIRECTION('center_axis',(0.,0.,1.));
#20064=DIRECTION('ref_axis',(1.,0.,0.));
#20065=DIRECTION('center_axis',(0.,0.,1.));
#20066=DIRECTION('ref_axis',(1.,0.,0.));
#20067=DIRECTION('center_axis',(0.,0.,1.));
#20068=DIRECTION('ref_axis',(1.,0.,0.));
#20069=DIRECTION('center_axis',(0.,0.,1.));
#20070=DIRECTION('ref_axis',(1.,0.,0.));
#20071=DIRECTION('',(-0.707106781186547,-8.65956056235493E-17,0.707106781186548));
#20072=DIRECTION('center_axis',(0.,0.,1.));
#20073=DIRECTION('ref_axis',(1.,0.,0.));
#20074=DIRECTION('center_axis',(0.,0.,1.));
#20075=DIRECTION('ref_axis',(1.,0.,0.));
#20076=DIRECTION('',(0.,0.,1.));
#20077=DIRECTION('center_axis',(0.,0.,-1.));
#20078=DIRECTION('ref_axis',(1.,0.,0.));
#20079=DIRECTION('',(-0.894427190999916,1.09535739652841E-16,-0.447213595499958));
#20080=DIRECTION('center_axis',(0.,0.,1.));
#20081=DIRECTION('ref_axis',(1.,0.,0.));
#20082=DIRECTION('center_axis',(0.,0.,-1.));
#20083=DIRECTION('ref_axis',(1.,0.,0.));
#20084=DIRECTION('',(-0.600000000000001,7.34788079488413E-17,-0.8));
#20085=DIRECTION('axis',(0.,0.,1.));
#20086=DIRECTION('refdir',(1.,0.,0.));
#20087=DIRECTION('center_axis',(0.,0.,1.));
#20088=DIRECTION('ref_axis',(1.,0.,0.));
#20089=DIRECTION('center_axis',(0.,0.,1.));
#20090=DIRECTION('ref_axis',(1.,0.,0.));
#20091=DIRECTION('',(0.,0.,-1.));
#20092=DIRECTION('center_axis',(0.,0.,1.));
#20093=DIRECTION('ref_axis',(1.,0.,0.));
#20094=DIRECTION('center_axis',(0.,0.,-1.));
#20095=DIRECTION('ref_axis',(-1.,0.,0.));
#20096=DIRECTION('center_axis',(0.,0.,1.));
#20097=DIRECTION('ref_axis',(1.,0.,0.));
#20098=DIRECTION('center_axis',(0.,0.,1.));
#20099=DIRECTION('ref_axis',(1.,0.,0.));
#20100=DIRECTION('',(0.,0.,1.));
#20101=DIRECTION('center_axis',(0.,0.,-1.));
#20102=DIRECTION('ref_axis',(1.,0.,0.));
#20103=DIRECTION('center_axis',(0.,0.,1.));
#20104=DIRECTION('ref_axis',(1.,0.,0.));
#20105=DIRECTION('center_axis',(0.,0.,1.));
#20106=DIRECTION('ref_axis',(1.,0.,0.));
#20107=DIRECTION('center_axis',(0.,0.,1.));
#20108=DIRECTION('ref_axis',(1.,0.,0.));
#20109=DIRECTION('center_axis',(0.,0.,1.));
#20110=DIRECTION('ref_axis',(1.,0.,0.));
#20111=DIRECTION('',(0.,0.,1.));
#20112=DIRECTION('center_axis',(0.,0.,1.));
#20113=DIRECTION('ref_axis',(1.,0.,0.));
#20114=DIRECTION('center_axis',(0.,0.,-1.));
#20115=DIRECTION('ref_axis',(-1.,0.,0.));
#20116=DIRECTION('center_axis',(0.,0.,1.));
#20117=DIRECTION('ref_axis',(1.,0.,0.));
#20118=DIRECTION('center_axis',(0.,0.,1.));
#20119=DIRECTION('ref_axis',(1.,0.,0.));
#20120=DIRECTION('center_axis',(0.,0.,1.));
#20121=DIRECTION('ref_axis',(1.,0.,0.));
#20122=DIRECTION('',(0.,0.,-1.));
#20123=DIRECTION('center_axis',(0.,0.,-1.));
#20124=DIRECTION('ref_axis',(1.,0.,0.));
#20125=DIRECTION('',(0.707106781186547,-8.65956056235493E-17,0.707106781186548));
#20126=DIRECTION('center_axis',(0.,0.,1.));
#20127=DIRECTION('ref_axis',(1.,0.,0.));
#20128=DIRECTION('center_axis',(0.,0.,-1.));
#20129=DIRECTION('ref_axis',(-1.,0.,0.));
#20130=DIRECTION('axis',(0.,0.,1.));
#20131=DIRECTION('refdir',(1.,0.,0.));
#20132=DIRECTION('center_axis',(0.,0.,1.));
#20133=DIRECTION('ref_axis',(0.0211112976229345,-0.999777131721203,0.));
#20134=DIRECTION('',(0.,0.,-1.));
#20135=DIRECTION('center_axis',(0.,0.,-1.));
#20136=DIRECTION('ref_axis',(1.,8.30866031508266E-15,0.));
#20137=DIRECTION('center_axis',(0.,0.,1.));
#20138=DIRECTION('ref_axis',(0.0211112976229345,-0.999777131721203,0.));
#20139=DIRECTION('',(0.,0.,-1.));
#20140=DIRECTION('center_axis',(0.,0.,1.));
#20141=DIRECTION('ref_axis',(0.0211112976229345,-0.999777131721203,0.));
#20142=DIRECTION('',(0.,0.,-1.));
#20143=DIRECTION('center_axis',(0.,0.,1.));
#20144=DIRECTION('ref_axis',(0.0211112976229345,-0.999777131721203,0.));
#20145=DIRECTION('',(0.,0.,-1.));
#20146=DIRECTION('center_axis',(0.,0.,1.));
#20147=DIRECTION('ref_axis',(0.0211112976229345,-0.999777131721203,0.));
#20148=DIRECTION('',(0.,0.,-1.));
#20149=DIRECTION('center_axis',(0.,0.,1.));
#20150=DIRECTION('ref_axis',(0.0211112976229345,-0.999777131721203,0.));
#20151=DIRECTION('',(0.,0.,-1.));
#20152=DIRECTION('center_axis',(0.,0.,1.));
#20153=DIRECTION('ref_axis',(1.,0.,0.));
#20154=DIRECTION('center_axis',(0.,0.,1.));
#20155=DIRECTION('ref_axis',(1.,0.,0.));
#20156=DIRECTION('center_axis',(0.,0.,-1.));
#20157=DIRECTION('ref_axis',(1.,0.,0.));
#20158=DIRECTION('center_axis',(0.,0.,1.));
#20159=DIRECTION('ref_axis',(0.0211112976229345,-0.999777131721203,0.));
#20160=DIRECTION('center_axis',(0.,0.,1.));
#20161=DIRECTION('ref_axis',(1.,8.30866031508266E-15,0.));
#20162=DIRECTION('center_axis',(0.,0.,1.));
#20163=DIRECTION('ref_axis',(1.,0.,0.));
#20164=DIRECTION('center_axis',(0.,0.,1.));
#20165=DIRECTION('ref_axis',(1.,0.,0.));
#20166=DIRECTION('center_axis',(0.,0.,1.));
#20167=DIRECTION('ref_axis',(1.,0.,0.));
#20168=DIRECTION('center_axis',(0.,0.,1.));
#20169=DIRECTION('ref_axis',(1.,0.,0.));
#20170=DIRECTION('center_axis',(0.,0.,1.));
#20171=DIRECTION('ref_axis',(1.,0.,0.));
#20172=DIRECTION('center_axis',(0.,0.,1.));
#20173=DIRECTION('ref_axis',(1.,0.,0.));
#20174=DIRECTION('',(-0.86602540378444,-1.06057523872491E-16,0.499999999999998));
#20175=DIRECTION('center_axis',(0.,0.,-1.));
#20176=DIRECTION('ref_axis',(1.,0.,0.));
#20177=DIRECTION('center_axis',(-0.5,-0.866025403784439,0.));
#20178=DIRECTION('ref_axis',(-0.866025403784439,0.5,0.));
#20179=DIRECTION('',(0.,0.,-1.));
#20180=DIRECTION('',(-0.866025403784439,0.5,0.));
#20181=DIRECTION('',(0.,0.,-1.));
#20182=DIRECTION('center_axis',(0.5,-0.866025403784439,0.));
#20183=DIRECTION('ref_axis',(-0.866025403784439,-0.5,0.));
#20184=DIRECTION('',(0.,0.,-1.));
#20185=DIRECTION('',(-0.866025403784439,-0.5,0.));
#20186=DIRECTION('center_axis',(1.,-3.84592537276713E-16,0.));
#20187=DIRECTION('ref_axis',(-3.84592537276713E-16,-1.,0.));
#20188=DIRECTION('',(0.,0.,-1.));
#20189=DIRECTION('',(-3.84592537276713E-16,-1.,0.));
#20190=DIRECTION('center_axis',(0.,0.,1.));
#20191=DIRECTION('ref_axis',(1.,0.,0.));
#20192=DIRECTION('',(-0.855621686410732,-1.04783435954396E-16,0.517601709564076));
#20193=DIRECTION('center_axis',(0.,0.,-1.));
#20194=DIRECTION('ref_axis',(1.,0.,0.));
#20195=DIRECTION('center_axis',(0.5,0.866025403784439,0.));
#20196=DIRECTION('ref_axis',(0.866025403784439,-0.5,0.));
#20197=DIRECTION('',(0.,0.,-1.));
#20198=DIRECTION('',(0.866025403784439,-0.5,0.));
#20199=DIRECTION('center_axis',(-0.5,0.866025403784439,0.));
#20200=DIRECTION('ref_axis',(0.866025403784439,0.5,0.));
#20201=DIRECTION('',(0.,0.,-1.));
#20202=DIRECTION('',(0.866025403784439,0.5,0.));
#20203=DIRECTION('center_axis',(-1.,-1.92296268638356E-16,0.));
#20204=DIRECTION('ref_axis',(-1.92296268638356E-16,1.,0.));
#20205=DIRECTION('',(-1.92296268638356E-16,1.,0.));
#20206=DIRECTION('center_axis',(0.,0.,-1.));
#20207=DIRECTION('ref_axis',(-1.,0.,0.));
#20208=DIRECTION('center_axis',(0.,0.,-1.));
#20209=DIRECTION('ref_axis',(-1.,0.,0.));
#20210=DIRECTION('center_axis',(0.,0.,1.));
#20211=DIRECTION('ref_axis',(1.,0.,0.));
#20212=DIRECTION('center_axis',(0.,0.,1.));
#20213=DIRECTION('ref_axis',(1.,0.,0.));
#20214=DIRECTION('',(0.707106781186547,8.65956056235493E-17,-0.707106781186548));
#20215=DIRECTION('center_axis',(0.,0.,1.));
#20216=DIRECTION('ref_axis',(1.,0.,0.));
#20217=DIRECTION('center_axis',(0.,0.,1.));
#20218=DIRECTION('ref_axis',(1.,0.,0.));
#20219=DIRECTION('center_axis',(0.,0.,1.));
#20220=DIRECTION('ref_axis',(1.,0.,0.));
#20221=DIRECTION('center_axis',(0.,0.,1.));
#20222=DIRECTION('ref_axis',(1.,0.,0.));
#20223=DIRECTION('center_axis',(0.,0.,1.));
#20224=DIRECTION('ref_axis',(1.,0.,0.));
#20225=DIRECTION('',(0.,0.,-1.));
#20226=DIRECTION('center_axis',(0.,0.,-1.));
#20227=DIRECTION('ref_axis',(-1.,0.,0.));
#20228=DIRECTION('center_axis',(0.,0.,1.));
#20229=DIRECTION('ref_axis',(1.,0.,0.));
#20230=DIRECTION('center_axis',(0.,0.,1.));
#20231=DIRECTION('ref_axis',(1.,0.,0.));
#20232=DIRECTION('center_axis',(0.,0.,1.));
#20233=DIRECTION('ref_axis',(1.,0.,0.));
#20234=DIRECTION('',(0.707106781186548,8.65956056235494E-17,-0.707106781186547));
#20235=DIRECTION('center_axis',(0.,0.,1.));
#20236=DIRECTION('ref_axis',(1.,0.,0.));
#20237=DIRECTION('center_axis',(0.,0.,1.));
#20238=DIRECTION('ref_axis',(1.,0.,0.));
#20239=DIRECTION('',(0.,0.,-1.));
#20240=DIRECTION('center_axis',(0.,0.,-1.));
#20241=DIRECTION('ref_axis',(1.,0.,0.));
#20242=DIRECTION('',(0.707106781186548,-8.65956056235494E-17,0.707106781186547));
#20243=DIRECTION('center_axis',(0.,0.,1.));
#20244=DIRECTION('ref_axis',(1.,0.,0.));
#20245=DIRECTION('center_axis',(0.,0.,1.));
#20246=DIRECTION('ref_axis',(1.,0.,0.));
#20247=DIRECTION('axis',(0.,0.,1.));
#20248=DIRECTION('refdir',(1.,0.,0.));
#20249=DIRECTION('center_axis',(0.,0.,-1.));
#20250=DIRECTION('ref_axis',(1.,0.,0.));
#20251=DIRECTION('center_axis',(0.,0.,1.));
#20252=DIRECTION('ref_axis',(1.,0.,0.));
#20253=DIRECTION('',(-0.707106781186548,8.65956056235494E-17,-0.707106781186547));
#20254=DIRECTION('center_axis',(0.,0.,1.));
#20255=DIRECTION('ref_axis',(1.,0.,0.));
#20256=DIRECTION('center_axis',(0.,0.,-1.));
#20257=DIRECTION('ref_axis',(-1.,0.,0.));
#20258=DIRECTION('center_axis',(0.,0.,1.));
#20259=DIRECTION('ref_axis',(1.,0.,0.));
#20260=DIRECTION('center_axis',(0.,0.,1.));
#20261=DIRECTION('ref_axis',(1.,0.,0.));
#20262=DIRECTION('center_axis',(0.,0.,1.));
#20263=DIRECTION('ref_axis',(1.,0.,0.));
#20264=DIRECTION('',(0.707106781186544,8.65956056235489E-17,-0.707106781186551));
#20265=DIRECTION('center_axis',(0.,0.,1.));
#20266=DIRECTION('ref_axis',(1.,0.,0.));
#20267=DIRECTION('center_axis',(0.,0.,1.));
#20268=DIRECTION('ref_axis',(1.,0.,0.));
#20269=DIRECTION('',(0.,0.,-1.));
#20270=DIRECTION('center_axis',(0.,0.,-1.));
#20271=DIRECTION('ref_axis',(1.,0.,0.));
#20272=DIRECTION('',(0.707106781186544,-8.65956056235489E-17,0.707106781186551));
#20273=DIRECTION('center_axis',(0.,0.,1.));
#20274=DIRECTION('ref_axis',(1.,0.,0.));
#20275=DIRECTION('center_axis',(0.,0.,1.));
#20276=DIRECTION('ref_axis',(1.,0.,0.));
#20277=DIRECTION('center_axis',(0.,0.,1.));
#20278=DIRECTION('ref_axis',(1.,0.,0.));
#20279=DIRECTION('center_axis',(0.,0.,1.));
#20280=DIRECTION('ref_axis',(1.,0.,0.));
#20281=DIRECTION('center_axis',(0.,0.,1.));
#20282=DIRECTION('ref_axis',(1.,0.,0.));
#20283=DIRECTION('',(-0.707106781186547,-8.65956056235493E-17,0.707106781186548));
#20284=DIRECTION('center_axis',(0.,0.,1.));
#20285=DIRECTION('ref_axis',(1.,0.,0.));
#20286=DIRECTION('',(0.,0.,1.));
#20287=DIRECTION('axis',(0.,0.,1.));
#20288=DIRECTION('refdir',(1.,0.,0.));
#20289=DIRECTION('center_axis',(0.,0.,1.));
#20290=DIRECTION('ref_axis',(1.,0.,0.));
#20291=DIRECTION('center_axis',(0.,0.,1.));
#20292=DIRECTION('ref_axis',(1.,0.,0.));
#20293=DIRECTION('',(0.,0.,1.));
#20294=DIRECTION('center_axis',(0.,0.,1.));
#20295=DIRECTION('ref_axis',(1.,0.,0.));
#20296=DIRECTION('center_axis',(0.,0.,-1.));
#20297=DIRECTION('ref_axis',(-1.,0.,0.));
#20298=DIRECTION('center_axis',(0.,0.,1.));
#20299=DIRECTION('ref_axis',(1.,0.,0.));
#20300=DIRECTION('center_axis',(0.,0.,1.));
#20301=DIRECTION('ref_axis',(1.,0.,0.));
#20302=DIRECTION('center_axis',(0.,0.,1.));
#20303=DIRECTION('ref_axis',(1.,0.,0.));
#20304=DIRECTION('',(0.707106781186547,8.65956056235493E-17,-0.707106781186548));
#20305=DIRECTION('center_axis',(0.,0.,1.));
#20306=DIRECTION('ref_axis',(1.,0.,0.));
#20307=DIRECTION('center_axis',(0.,0.,1.));
#20308=DIRECTION('ref_axis',(1.,0.,0.));
#20309=DIRECTION('',(0.,0.,-1.));
#20310=DIRECTION('center_axis',(0.,0.,-1.));
#20311=DIRECTION('ref_axis',(-1.,0.,0.));
#20312=DIRECTION('center_axis',(0.,0.,1.));
#20313=DIRECTION('ref_axis',(1.,0.,0.));
#20314=DIRECTION('center_axis',(0.,0.,1.));
#20315=DIRECTION('ref_axis',(1.,0.,0.));
#20316=DIRECTION('center_axis',(0.,0.,1.));
#20317=DIRECTION('ref_axis',(1.,0.,0.));
#20318=DIRECTION('',(0.707106781186547,8.65956056235492E-17,-0.707106781186548));
#20319=DIRECTION('center_axis',(0.,0.,1.));
#20320=DIRECTION('ref_axis',(1.,0.,0.));
#20321=DIRECTION('center_axis',(0.,0.,1.));
#20322=DIRECTION('ref_axis',(1.,0.,0.));
#20323=DIRECTION('',(0.,0.,-1.));
#20324=DIRECTION('center_axis',(0.,0.,-1.));
#20325=DIRECTION('ref_axis',(1.,0.,0.));
#20326=DIRECTION('',(0.707106781186546,-8.65956056235491E-17,0.707106781186549));
#20327=DIRECTION('center_axis',(0.,0.,1.));
#20328=DIRECTION('ref_axis',(1.,0.,0.));
#20329=DIRECTION('center_axis',(0.,0.,1.));
#20330=DIRECTION('ref_axis',(1.,0.,0.));
#20331=DIRECTION('center_axis',(0.,0.,-1.));
#20332=DIRECTION('ref_axis',(-1.,0.,0.));
#20333=DIRECTION('axis',(0.,0.,1.));
#20334=DIRECTION('refdir',(1.,0.,0.));
#20335=DIRECTION('center_axis',(0.,0.,1.));
#20336=DIRECTION('ref_axis',(1.,0.,0.));
#20337=DIRECTION('center_axis',(0.,0.,1.));
#20338=DIRECTION('ref_axis',(1.,0.,0.));
#20339=DIRECTION('',(0.,0.,-1.));
#20340=DIRECTION('center_axis',(0.,0.,-1.));
#20341=DIRECTION('ref_axis',(1.,0.,0.));
#20342=DIRECTION('center_axis',(0.,0.,1.));
#20343=DIRECTION('ref_axis',(1.,0.,0.));
#20344=DIRECTION('center_axis',(0.,0.,1.));
#20345=DIRECTION('ref_axis',(1.,0.,0.));
#20346=DIRECTION('',(0.,0.,1.));
#20347=DIRECTION('center_axis',(0.,0.,1.));
#20348=DIRECTION('ref_axis',(1.,0.,0.));
#20349=DIRECTION('center_axis',(0.,0.,1.));
#20350=DIRECTION('ref_axis',(1.,0.,0.));
#20351=DIRECTION('center_axis',(0.,0.,1.));
#20352=DIRECTION('ref_axis',(1.,0.,0.));
#20353=DIRECTION('center_axis',(0.,0.,1.));
#20354=DIRECTION('ref_axis',(1.,0.,0.));
#20355=DIRECTION('',(0.,0.,-1.));
#20356=DIRECTION('center_axis',(0.,0.,1.));
#20357=DIRECTION('ref_axis',(1.,0.,0.));
#20358=DIRECTION('center_axis',(0.,0.,-1.));
#20359=DIRECTION('ref_axis',(-1.,0.,0.));
#20360=DIRECTION('center_axis',(0.,0.,1.));
#20361=DIRECTION('ref_axis',(1.,0.,0.));
#20362=DIRECTION('center_axis',(0.,0.,1.));
#20363=DIRECTION('ref_axis',(1.,0.,0.));
#20364=DIRECTION('',(0.,0.,1.));
#20365=DIRECTION('center_axis',(0.,0.,-1.));
#20366=DIRECTION('ref_axis',(1.,0.,0.));
#20367=DIRECTION('center_axis',(0.,0.,-1.));
#20368=DIRECTION('ref_axis',(-1.,0.,0.));
#20369=DIRECTION('center_axis',(0.,0.,1.));
#20370=DIRECTION('ref_axis',(1.,0.,0.));
#20371=DIRECTION('center_axis',(0.,0.,1.));
#20372=DIRECTION('ref_axis',(1.,0.,0.));
#20373=DIRECTION('center_axis',(0.,0.,1.));
#20374=DIRECTION('ref_axis',(1.,0.,0.));
#20375=DIRECTION('center_axis',(0.,0.,1.));
#20376=DIRECTION('ref_axis',(1.,0.,0.));
#20377=DIRECTION('center_axis',(0.,0.,1.));
#20378=DIRECTION('ref_axis',(1.,0.,0.));
#20379=DIRECTION('',(0.,0.,1.));
#20380=DIRECTION('center_axis',(0.,0.,1.));
#20381=DIRECTION('ref_axis',(1.,0.,0.));
#20382=DIRECTION('center_axis',(0.,0.,-1.));
#20383=DIRECTION('ref_axis',(1.,0.,0.));
#20384=DIRECTION('',(-0.707106781186548,8.65956056235494E-17,-0.707106781186547));
#20385=DIRECTION('center_axis',(0.,0.,1.));
#20386=DIRECTION('ref_axis',(1.,0.,0.));
#20387=DIRECTION('center_axis',(0.,0.,-1.));
#20388=DIRECTION('ref_axis',(-1.,0.,0.));
#20389=DIRECTION('center_axis',(0.,0.,1.));
#20390=DIRECTION('ref_axis',(1.,0.,0.));
#20391=DIRECTION('center_axis',(0.,0.,-1.));
#20392=DIRECTION('ref_axis',(1.,0.,0.));
#20393=DIRECTION('',(-0.98568389974183,1.20711463278991E-16,-0.168603824955838));
#20394=DIRECTION('center_axis',(0.,0.,1.));
#20395=DIRECTION('ref_axis',(1.,0.,0.));
#20396=DIRECTION('center_axis',(0.,0.,-1.));
#20397=DIRECTION('ref_axis',(1.,0.,0.));
#20398=DIRECTION('',(-0.707106781186545,8.6595605623549E-17,-0.70710678118655));
#20399=DIRECTION('center_axis',(0.,0.,1.));
#20400=DIRECTION('ref_axis',(1.,0.,0.));
#20401=DIRECTION('center_axis',(0.,0.,-1.));
#20402=DIRECTION('ref_axis',(-1.,0.,0.));
#20403=DIRECTION('center_axis',(0.,0.,1.));
#20404=DIRECTION('ref_axis',(1.,0.,0.));
#20405=DIRECTION('center_axis',(0.,0.,1.));
#20406=DIRECTION('ref_axis',(1.,0.,0.));
#20407=DIRECTION('',(0.707106781186548,8.65956056235494E-17,-0.707106781186547));
#20408=DIRECTION('center_axis',(0.,0.,1.));
#20409=DIRECTION('ref_axis',(1.,0.,0.));
#20410=DIRECTION('center_axis',(0.,0.,1.));
#20411=DIRECTION('ref_axis',(1.,0.,0.));
#20412=DIRECTION('',(0.,0.,-1.));
#20413=DIRECTION('center_axis',(0.,0.,-1.));
#20414=DIRECTION('ref_axis',(1.,0.,0.));
#20415=DIRECTION('',(0.707106781186547,-8.65956056235493E-17,0.707106781186548));
#20416=DIRECTION('center_axis',(0.,0.,1.));
#20417=DIRECTION('ref_axis',(1.,0.,0.));
#20418=DIRECTION('center_axis',(0.,0.,1.));
#20419=DIRECTION('ref_axis',(1.,0.,0.));
#20420=DIRECTION('center_axis',(0.,0.,1.));
#20421=DIRECTION('ref_axis',(1.,0.,0.));
#20422=DIRECTION('center_axis',(0.,0.,1.));
#20423=DIRECTION('ref_axis',(1.,0.,0.));
#20424=DIRECTION('',(0.,0.,-1.));
#20425=DIRECTION('center_axis',(0.,0.,1.));
#20426=DIRECTION('ref_axis',(1.,0.,0.));
#20427=DIRECTION('center_axis',(0.,0.,1.));
#20428=DIRECTION('ref_axis',(1.,0.,0.));
#20429=DIRECTION('center_axis',(0.,0.,1.));
#20430=DIRECTION('ref_axis',(1.,0.,0.));
#20431=DIRECTION('',(-0.707106781186547,-8.65956056235493E-17,0.707106781186548));
#20432=DIRECTION('axis',(0.,0.,1.));
#20433=DIRECTION('refdir',(1.,0.,0.));
#20434=DIRECTION('center_axis',(0.,0.,1.));
#20435=DIRECTION('ref_axis',(1.,0.,0.));
#20436=DIRECTION('center_axis',(0.,0.,1.));
#20437=DIRECTION('ref_axis',(1.,0.,0.));
#20438=DIRECTION('',(0.,0.,1.));
#20439=DIRECTION('center_axis',(0.,0.,1.));
#20440=DIRECTION('ref_axis',(1.,0.,0.));
#20441=DIRECTION('center_axis',(0.,0.,-1.));
#20442=DIRECTION('ref_axis',(1.,0.,0.));
#20443=DIRECTION('',(-0.707106781186548,8.65956056235494E-17,-0.707106781186547));
#20444=DIRECTION('center_axis',(0.,0.,1.));
#20445=DIRECTION('ref_axis',(1.,0.,0.));
#20446=DIRECTION('center_axis',(0.,0.,-1.));
#20447=DIRECTION('ref_axis',(-1.,0.,0.));
#20448=DIRECTION('center_axis',(0.,0.,1.));
#20449=DIRECTION('ref_axis',(1.,0.,0.));
#20450=DIRECTION('center_axis',(0.,0.,1.));
#20451=DIRECTION('ref_axis',(1.,0.,0.));
#20452=DIRECTION('center_axis',(0.,0.,1.));
#20453=DIRECTION('ref_axis',(1.,0.,0.));
#20454=DIRECTION('',(0.,0.,-1.));
#20455=DIRECTION('center_axis',(0.,0.,-1.));
#20456=DIRECTION('ref_axis',(-1.,0.,0.));
#20457=DIRECTION('center_axis',(0.,0.,1.));
#20458=DIRECTION('ref_axis',(1.,0.,0.));
#20459=DIRECTION('center_axis',(0.,0.,1.));
#20460=DIRECTION('ref_axis',(1.,0.,0.));
#20461=DIRECTION('center_axis',(0.,0.,1.));
#20462=DIRECTION('ref_axis',(1.,0.,0.));
#20463=DIRECTION('',(0.,0.,1.));
#20464=DIRECTION('center_axis',(0.,0.,-1.));
#20465=DIRECTION('ref_axis',(-1.,0.,0.));
#20466=DIRECTION('center_axis',(0.,0.,1.));
#20467=DIRECTION('ref_axis',(1.,0.,0.));
#20468=DIRECTION('center_axis',(0.,0.,1.));
#20469=DIRECTION('ref_axis',(1.,0.,0.));
#20470=DIRECTION('center_axis',(0.,0.,1.));
#20471=DIRECTION('ref_axis',(1.,0.,0.));
#20472=DIRECTION('',(0.707106781186548,8.65956056235494E-17,-0.707106781186547));
#20473=DIRECTION('center_axis',(0.,0.,1.));
#20474=DIRECTION('ref_axis',(1.,0.,0.));
#20475=DIRECTION('center_axis',(0.,0.,1.));
#20476=DIRECTION('ref_axis',(1.,0.,0.));
#20477=DIRECTION('',(0.,0.,-1.));
#20478=DIRECTION('center_axis',(0.,0.,-1.));
#20479=DIRECTION('ref_axis',(1.,0.,0.));
#20480=DIRECTION('',(0.707106781186547,-8.65956056235493E-17,0.707106781186548));
#20481=DIRECTION('center_axis',(0.,0.,1.));
#20482=DIRECTION('ref_axis',(1.,0.,0.));
#20483=DIRECTION('center_axis',(0.,0.,1.));
#20484=DIRECTION('ref_axis',(1.,0.,0.));
#20485=DIRECTION('center_axis',(0.,0.,1.));
#20486=DIRECTION('ref_axis',(1.,0.,0.));
#20487=DIRECTION('center_axis',(0.,0.,1.));
#20488=DIRECTION('ref_axis',(1.,0.,0.));
#20489=DIRECTION('center_axis',(0.,0.,1.));
#20490=DIRECTION('ref_axis',(1.,0.,0.));
#20491=DIRECTION('',(0.,0.,1.));
#20492=DIRECTION('center_axis',(0.,0.,1.));
#20493=DIRECTION('ref_axis',(1.,0.,0.));
#20494=DIRECTION('center_axis',(0.,0.,1.));
#20495=DIRECTION('ref_axis',(1.,0.,0.));
#20496=DIRECTION('center_axis',(0.,0.,1.));
#20497=DIRECTION('ref_axis',(1.,0.,0.));
#20498=DIRECTION('center_axis',(0.,0.,1.));
#20499=DIRECTION('ref_axis',(1.,0.,0.));
#20500=DIRECTION('',(0.,0.,-1.));
#20501=DIRECTION('center_axis',(0.,0.,1.));
#20502=DIRECTION('ref_axis',(1.,0.,0.));
#20503=DIRECTION('center_axis',(0.,0.,1.));
#20504=DIRECTION('ref_axis',(1.,0.,0.));
#20505=DIRECTION('center_axis',(0.,0.,1.));
#20506=DIRECTION('ref_axis',(1.,0.,0.));
#20507=DIRECTION('',(-0.707106781186547,-8.65956056235493E-17,0.707106781186548));
#20508=DIRECTION('axis',(0.,0.,1.));
#20509=DIRECTION('refdir',(1.,0.,0.));
#20510=DIRECTION('center_axis',(0.,0.,-1.));
#20511=DIRECTION('ref_axis',(-1.,0.,0.));
#20512=DIRECTION('center_axis',(0.,0.,1.));
#20513=DIRECTION('ref_axis',(1.,0.,0.));
#20514=DIRECTION('center_axis',(0.,0.,1.));
#20515=DIRECTION('ref_axis',(1.,0.,0.));
#20516=DIRECTION('center_axis',(0.,0.,1.));
#20517=DIRECTION('ref_axis',(1.,0.,0.));
#20518=DIRECTION('center_axis',(0.,0.,1.));
#20519=DIRECTION('ref_axis',(1.,0.,0.));
#20520=DIRECTION('',(0.707106781186549,8.65956056235496E-17,-0.707106781186546));
#20521=DIRECTION('center_axis',(0.,0.,1.));
#20522=DIRECTION('ref_axis',(1.,0.,0.));
#20523=DIRECTION('center_axis',(0.,0.,1.));
#20524=DIRECTION('ref_axis',(1.,0.,0.));
#20525=DIRECTION('',(0.,0.,-1.));
#20526=DIRECTION('center_axis',(0.,0.,-1.));
#20527=DIRECTION('ref_axis',(1.,0.,0.));
#20528=DIRECTION('',(0.707106781186547,-8.65956056235493E-17,0.707106781186548));
#20529=DIRECTION('center_axis',(0.,0.,1.));
#20530=DIRECTION('ref_axis',(1.,0.,0.));
#20531=DIRECTION('center_axis',(0.,0.,1.));
#20532=DIRECTION('ref_axis',(1.,0.,0.));
#20533=DIRECTION('center_axis',(0.,0.,1.));
#20534=DIRECTION('ref_axis',(1.,0.,0.));
#20535=DIRECTION('center_axis',(0.,0.,1.));
#20536=DIRECTION('ref_axis',(1.,0.,0.));
#20537=DIRECTION('center_axis',(0.,0.,1.));
#20538=DIRECTION('ref_axis',(1.,0.,0.));
#20539=DIRECTION('',(0.,0.,1.));
#20540=DIRECTION('center_axis',(0.,0.,1.));
#20541=DIRECTION('ref_axis',(1.,0.,0.));
#20542=DIRECTION('center_axis',(0.,0.,1.));
#20543=DIRECTION('ref_axis',(1.,0.,0.));
#20544=DIRECTION('center_axis',(0.,0.,1.));
#20545=DIRECTION('ref_axis',(1.,0.,0.));
#20546=DIRECTION('center_axis',(0.,0.,1.));
#20547=DIRECTION('ref_axis',(1.,0.,0.));
#20548=DIRECTION('',(-0.661621637086846,-8.10252820105038E-17,0.749837855365093));
#20549=DIRECTION('center_axis',(0.,0.,1.));
#20550=DIRECTION('ref_axis',(1.,0.,0.));
#20551=DIRECTION('center_axis',(0.,0.,1.));
#20552=DIRECTION('ref_axis',(1.,0.,0.));
#20553=DIRECTION('',(0.,0.,1.));
#20554=DIRECTION('center_axis',(0.,0.,-1.));
#20555=DIRECTION('ref_axis',(1.,0.,0.));
#20556=DIRECTION('',(-0.857492925712543,1.05012596676536E-16,-0.514495755427529));
#20557=DIRECTION('center_axis',(0.,0.,1.));
#20558=DIRECTION('ref_axis',(1.,0.,0.));
#20559=DIRECTION('center_axis',(0.,0.,-1.));
#20560=DIRECTION('ref_axis',(1.,0.,0.));
#20561=DIRECTION('',(-0.52999894000318,6.49061505426384E-17,-0.847998304005088));
#20562=DIRECTION('axis',(0.,0.,1.));
#20563=DIRECTION('refdir',(1.,0.,0.));
#20564=DIRECTION('center_axis',(0.,0.,-1.));
#20565=DIRECTION('ref_axis',(1.,0.,0.));
#20566=DIRECTION('center_axis',(0.,0.,1.));
#20567=DIRECTION('ref_axis',(1.,0.,0.));
#20568=DIRECTION('',(-0.707106781186548,8.65956056235494E-17,-0.707106781186547));
#20569=DIRECTION('center_axis',(0.,0.,-1.));
#20570=DIRECTION('ref_axis',(1.,0.,0.));
#20571=DIRECTION('center_axis',(0.,0.,1.));
#20572=DIRECTION('ref_axis',(1.,0.,0.));
#20573=DIRECTION('',(0.,0.,1.));
#20574=DIRECTION('center_axis',(0.,0.,-1.));
#20575=DIRECTION('ref_axis',(1.,0.,0.));
#20576=DIRECTION('center_axis',(0.,0.,1.));
#20577=DIRECTION('ref_axis',(1.,0.,0.));
#20578=DIRECTION('',(0.,1.,0.));
#20579=DIRECTION('center_axis',(0.,0.,1.));
#20580=DIRECTION('ref_axis',(1.,0.,0.));
#20581=DIRECTION('',(0.,-1.,0.));
#20582=DIRECTION('center_axis',(0.,0.,-1.));
#20583=DIRECTION('ref_axis',(1.,0.,0.));
#20584=DIRECTION('center_axis',(0.,0.,1.));
#20585=DIRECTION('ref_axis',(1.,0.,0.));
#20586=DIRECTION('center_axis',(0.,0.,-1.));
#20587=DIRECTION('ref_axis',(1.,0.,0.));
#20588=DIRECTION('center_axis',(0.,0.,1.));
#20589=DIRECTION('ref_axis',(1.,0.,0.));
#20590=DIRECTION('center_axis',(0.,0.,-1.));
#20591=DIRECTION('ref_axis',(1.,0.,0.));
#20592=DIRECTION('center_axis',(0.,0.,-1.));
#20593=DIRECTION('ref_axis',(1.,0.,0.));
#20594=DIRECTION('center_axis',(0.,0.,1.));
#20595=DIRECTION('ref_axis',(1.,0.,0.));
#20596=DIRECTION('',(-0.707106781186547,-8.65956056235493E-17,0.707106781186548));
#20597=DIRECTION('center_axis',(0.,0.,1.));
#20598=DIRECTION('ref_axis',(1.,0.,0.));
#20599=DIRECTION('center_axis',(0.,0.,1.));
#20600=DIRECTION('ref_axis',(1.,0.,0.));
#20601=DIRECTION('',(0.,-1.,0.));
#20602=DIRECTION('center_axis',(0.,0.,-1.));
#20603=DIRECTION('ref_axis',(1.,0.,0.));
#20604=DIRECTION('center_axis',(0.,0.,1.));
#20605=DIRECTION('ref_axis',(1.,0.,0.));
#20606=DIRECTION('center_axis',(0.,0.,-1.));
#20607=DIRECTION('ref_axis',(1.,0.,0.));
#20608=DIRECTION('center_axis',(0.,0.,1.));
#20609=DIRECTION('ref_axis',(1.,0.,0.));
#20610=DIRECTION('center_axis',(0.,0.,-1.));
#20611=DIRECTION('ref_axis',(1.,0.,0.));
#20612=DIRECTION('',(0.,1.,0.));
#20613=DIRECTION('center_axis',(0.,0.,1.));
#20614=DIRECTION('ref_axis',(1.,0.,0.));
#20615=DIRECTION('center_axis',(0.,0.,1.));
#20616=DIRECTION('ref_axis',(1.,0.,0.));
#20617=DIRECTION('center_axis',(0.,0.,-1.));
#20618=DIRECTION('ref_axis',(1.,0.,0.));
#20619=DIRECTION('center_axis',(0.,0.,1.));
#20620=DIRECTION('ref_axis',(1.,0.,0.));
#20621=DIRECTION('',(-0.707106781186548,8.65956056235494E-17,-0.707106781186547));
#20622=DIRECTION('center_axis',(0.,0.,1.));
#20623=DIRECTION('ref_axis',(1.,0.,0.));
#20624=DIRECTION('',(0.,0.,1.));
#20625=DIRECTION('center_axis',(0.,0.,-1.));
#20626=DIRECTION('ref_axis',(1.,0.,0.));
#20627=DIRECTION('center_axis',(0.,0.,1.));
#20628=DIRECTION('ref_axis',(1.,0.,0.));
#20629=DIRECTION('',(-0.707106781186547,-8.65956056235493E-17,0.707106781186548));
#20630=DIRECTION('center_axis',(-1.,0.,0.));
#20631=DIRECTION('ref_axis',(0.,-1.,0.));
#20632=DIRECTION('',(0.,0.,1.));
#20633=DIRECTION('',(0.,0.,-1.));
#20634=DIRECTION('center_axis',(1.,0.,0.));
#20635=DIRECTION('ref_axis',(0.,1.,0.));
#20636=DIRECTION('',(0.,0.,-1.));
#20637=DIRECTION('',(0.,0.,1.));
#20638=DIRECTION('center_axis',(0.,0.,1.));
#20639=DIRECTION('ref_axis',(1.,0.,0.));
#20640=DIRECTION('',(0.,0.,1.));
#20641=DIRECTION('center_axis',(0.,0.,1.));
#20642=DIRECTION('ref_axis',(1.,0.,0.));
#20643=DIRECTION('',(0.,0.,1.));
#20644=DIRECTION('center_axis',(0.,0.,1.));
#20645=DIRECTION('ref_axis',(-1.83697019872103E-16,-1.,0.));
#20646=DIRECTION('',(0.,0.,1.));
#20647=DIRECTION('center_axis',(0.,0.,1.));
#20648=DIRECTION('ref_axis',(-0.247524504876091,-0.96888163337213,0.));
#20649=DIRECTION('',(0.,0.,1.));
#20650=DIRECTION('center_axis',(0.,0.,1.));
#20651=DIRECTION('ref_axis',(1.,0.,0.));
#20652=DIRECTION('center_axis',(0.,0.,1.));
#20653=DIRECTION('ref_axis',(6.12323399573677E-17,-1.,0.));
#20654=DIRECTION('axis',(0.,0.,1.));
#20655=DIRECTION('refdir',(1.,0.,0.));
#20656=DIRECTION('center_axis',(0.,0.,1.));
#20657=DIRECTION('ref_axis',(0.176828393097112,-0.984241697650883,0.));
#20658=DIRECTION('',(0.,0.,-1.));
#20659=DIRECTION('center_axis',(0.,0.,-1.));
#20660=DIRECTION('ref_axis',(1.,9.72557910080329E-14,0.));
#20661=DIRECTION('center_axis',(0.,0.,1.));
#20662=DIRECTION('ref_axis',(0.176828393097112,-0.984241697650883,0.));
#20663=DIRECTION('',(0.,0.,-1.));
#20664=DIRECTION('center_axis',(0.,0.,1.));
#20665=DIRECTION('ref_axis',(0.176828393097112,-0.984241697650883,0.));
#20666=DIRECTION('',(0.,0.,-1.));
#20667=DIRECTION('center_axis',(0.,0.,1.));
#20668=DIRECTION('ref_axis',(0.176828393097112,-0.984241697650883,0.));
#20669=DIRECTION('',(0.,0.,-1.));
#20670=DIRECTION('center_axis',(0.,0.,1.));
#20671=DIRECTION('ref_axis',(0.176828393097112,-0.984241697650883,0.));
#20672=DIRECTION('',(0.,0.,-1.));
#20673=DIRECTION('center_axis',(0.,0.,1.));
#20674=DIRECTION('ref_axis',(0.176828393097112,-0.984241697650883,0.));
#20675=DIRECTION('',(0.,0.,-1.));
#20676=DIRECTION('center_axis',(0.,0.,1.));
#20677=DIRECTION('ref_axis',(0.176828393097112,-0.984241697650883,0.));
#20678=DIRECTION('',(0.,0.,-1.));
#20679=DIRECTION('center_axis',(0.,0.,1.));
#20680=DIRECTION('ref_axis',(0.176828393097112,-0.984241697650883,0.));
#20681=DIRECTION('',(0.,0.,-1.));
#20682=DIRECTION('center_axis',(0.,0.,1.));
#20683=DIRECTION('ref_axis',(0.176828393097112,-0.984241697650883,0.));
#20684=DIRECTION('',(0.,0.,-1.));
#20685=DIRECTION('center_axis',(0.,0.,1.));
#20686=DIRECTION('ref_axis',(0.176828393097112,-0.984241697650883,0.));
#20687=DIRECTION('',(0.,0.,-1.));
#20688=DIRECTION('center_axis',(0.,0.,1.));
#20689=DIRECTION('ref_axis',(0.176828393097112,-0.984241697650883,0.));
#20690=DIRECTION('',(0.,0.,-1.));
#20691=DIRECTION('center_axis',(0.,0.,1.));
#20692=DIRECTION('ref_axis',(0.176828393097112,-0.984241697650883,0.));
#20693=DIRECTION('',(0.,0.,-1.));
#20694=DIRECTION('center_axis',(0.,0.,1.));
#20695=DIRECTION('ref_axis',(0.176828393097112,-0.984241697650883,0.));
#20696=DIRECTION('',(0.,0.,-1.));
#20697=DIRECTION('center_axis',(0.,0.,1.));
#20698=DIRECTION('ref_axis',(0.176828393097112,-0.984241697650883,0.));
#20699=DIRECTION('',(0.,0.,-1.));
#20700=DIRECTION('center_axis',(0.,0.,1.));
#20701=DIRECTION('ref_axis',(0.176828393097112,-0.984241697650883,0.));
#20702=DIRECTION('',(0.,0.,-1.));
#20703=DIRECTION('center_axis',(0.,0.,1.));
#20704=DIRECTION('ref_axis',(0.176828393097112,-0.984241697650883,0.));
#20705=DIRECTION('',(0.,0.,-1.));
#20706=DIRECTION('center_axis',(0.,0.,1.));
#20707=DIRECTION('ref_axis',(0.176828393097112,-0.984241697650883,0.));
#20708=DIRECTION('',(0.,0.,-1.));
#20709=DIRECTION('center_axis',(0.,0.,1.));
#20710=DIRECTION('ref_axis',(0.176828393097112,-0.984241697650883,0.));
#20711=DIRECTION('',(0.,0.,-1.));
#20712=DIRECTION('center_axis',(0.,0.,1.));
#20713=DIRECTION('ref_axis',(0.176828393097112,-0.984241697650883,0.));
#20714=DIRECTION('',(0.,0.,-1.));
#20715=DIRECTION('center_axis',(0.,0.,1.));
#20716=DIRECTION('ref_axis',(1.,0.,0.));
#20717=DIRECTION('center_axis',(0.,0.,1.));
#20718=DIRECTION('ref_axis',(1.,0.,0.));
#20719=DIRECTION('center_axis',(-0.0068787995302466,0.0538364315100811,
0.998526074150937));
#20720=DIRECTION('ref_axis',(-0.982073479159668,-0.188467899125696,0.00339595794621756));
#20721=DIRECTION('center_axis',(0.,0.,1.));
#20722=DIRECTION('ref_axis',(1.,0.,0.));
#20723=DIRECTION('center_axis',(0.,0.,1.));
#20724=DIRECTION('ref_axis',(1.,0.,0.));
#20725=DIRECTION('center_axis',(0.,0.,1.));
#20726=DIRECTION('ref_axis',(-0.501423668270377,-0.86520188678613,0.));
#20727=DIRECTION('center_axis',(0.,0.,1.));
#20728=DIRECTION('ref_axis',(1.,9.72557910080329E-14,0.));
#20729=DIRECTION('center_axis',(0.,0.,1.));
#20730=DIRECTION('ref_axis',(1.,0.,0.));
#20731=DIRECTION('center_axis',(0.,0.,1.));
#20732=DIRECTION('ref_axis',(1.,0.,0.));
#20733=DIRECTION('center_axis',(0.,0.,1.));
#20734=DIRECTION('ref_axis',(1.,0.,0.));
#20735=DIRECTION('center_axis',(0.,0.,1.));
#20736=DIRECTION('ref_axis',(1.,0.,0.));
#20737=DIRECTION('center_axis',(0.,0.,1.));
#20738=DIRECTION('ref_axis',(1.,0.,0.));
#20739=DIRECTION('center_axis',(0.,0.,1.));
#20740=DIRECTION('ref_axis',(1.,0.,0.));
#20741=DIRECTION('center_axis',(0.,0.,-1.));
#20742=DIRECTION('ref_axis',(1.,0.,0.));
#20743=DIRECTION('center_axis',(-1.22464679914735E-16,1.,0.));
#20744=DIRECTION('ref_axis',(-1.,-1.22464679914735E-16,0.));
#20745=DIRECTION('center_axis',(0.,0.,-1.));
#20746=DIRECTION('ref_axis',(-1.,0.,0.));
#20747=DIRECTION('center_axis',(0.,0.,1.));
#20748=DIRECTION('ref_axis',(1.,0.,0.));
#20749=DIRECTION('center_axis',(0.,0.,1.));
#20750=DIRECTION('ref_axis',(1.,0.,0.));
#20751=DIRECTION('',(-0.86602540378444,-1.06057523872491E-16,0.499999999999998));
#20752=DIRECTION('center_axis',(0.,0.,-1.));
#20753=DIRECTION('ref_axis',(1.,0.,0.));
#20754=DIRECTION('center_axis',(-0.5,-0.866025403784439,0.));
#20755=DIRECTION('ref_axis',(-0.866025403784439,0.5,0.));
#20756=DIRECTION('',(0.,0.,-1.));
#20757=DIRECTION('',(-0.866025403784439,0.5,0.));
#20758=DIRECTION('',(0.,0.,-1.));
#20759=DIRECTION('center_axis',(0.5,-0.866025403784439,0.));
#20760=DIRECTION('ref_axis',(-0.866025403784439,-0.5,0.));
#20761=DIRECTION('',(0.,0.,-1.));
#20762=DIRECTION('',(-0.866025403784439,-0.5,0.));
#20763=DIRECTION('center_axis',(1.,-3.84592537276713E-16,0.));
#20764=DIRECTION('ref_axis',(-3.84592537276713E-16,-1.,0.));
#20765=DIRECTION('',(0.,0.,-1.));
#20766=DIRECTION('',(-3.84592537276713E-16,-1.,0.));
#20767=DIRECTION('center_axis',(0.,0.,1.));
#20768=DIRECTION('ref_axis',(1.,0.,0.));
#20769=DIRECTION('',(-0.855621686410732,-1.04783435954396E-16,0.517601709564076));
#20770=DIRECTION('center_axis',(0.,0.,-1.));
#20771=DIRECTION('ref_axis',(1.,0.,0.));
#20772=DIRECTION('center_axis',(0.5,0.866025403784439,0.));
#20773=DIRECTION('ref_axis',(0.866025403784439,-0.5,0.));
#20774=DIRECTION('',(0.,0.,-1.));
#20775=DIRECTION('',(0.866025403784439,-0.5,0.));
#20776=DIRECTION('center_axis',(-0.5,0.866025403784439,0.));
#20777=DIRECTION('ref_axis',(0.866025403784439,0.5,0.));
#20778=DIRECTION('',(0.,0.,-1.));
#20779=DIRECTION('',(0.866025403784439,0.5,0.));
#20780=DIRECTION('center_axis',(-1.,-1.92296268638356E-16,0.));
#20781=DIRECTION('ref_axis',(-1.92296268638356E-16,1.,0.));
#20782=DIRECTION('',(-1.92296268638356E-16,1.,0.));
#20783=DIRECTION('center_axis',(0.,0.,-1.));
#20784=DIRECTION('ref_axis',(-1.,0.,0.));
#20785=DIRECTION('center_axis',(0.,0.,1.));
#20786=DIRECTION('ref_axis',(1.,0.,0.));
#20787=DIRECTION('center_axis',(0.,0.,-1.));
#20788=DIRECTION('ref_axis',(-1.,1.22464679914735E-16,0.));
#20789=DIRECTION('center_axis',(1.22464679914735E-16,-1.,0.));
#20790=DIRECTION('ref_axis',(-1.,-1.22464679914735E-16,0.));
#20791=DIRECTION('center_axis',(0.,0.,1.));
#20792=DIRECTION('ref_axis',(-1.,1.22464679914735E-16,0.));
#20793=DIRECTION('center_axis',(0.,0.,1.));
#20794=DIRECTION('ref_axis',(1.,0.,0.));
#20795=DIRECTION('',(0.,0.,-1.));
#20796=DIRECTION('center_axis',(0.,0.,1.));
#20797=DIRECTION('ref_axis',(1.,0.,0.));
#20798=DIRECTION('center_axis',(0.,0.,1.));
#20799=DIRECTION('ref_axis',(1.,0.,0.));
#20800=DIRECTION('center_axis',(0.,0.,-1.));
#20801=DIRECTION('ref_axis',(-1.,0.,0.));
#20802=DIRECTION('center_axis',(0.,0.,1.));
#20803=DIRECTION('ref_axis',(1.,0.,0.));
#20804=DIRECTION('center_axis',(0.,0.,1.));
#20805=DIRECTION('ref_axis',(1.,0.,0.));
#20806=DIRECTION('',(0.707106781186548,8.65956056235494E-17,-0.707106781186547));
#20807=DIRECTION('center_axis',(0.,0.,1.));
#20808=DIRECTION('ref_axis',(1.,0.,0.));
#20809=DIRECTION('',(0.707106781186548,8.65956056235494E-17,-0.707106781186547));
#20810=DIRECTION('axis',(0.,0.,1.));
#20811=DIRECTION('refdir',(1.,0.,0.));
#20812=DIRECTION('center_axis',(0.,0.,1.));
#20813=DIRECTION('ref_axis',(0.17681385355385,-0.984244309707421,0.));
#20814=DIRECTION('',(0.,0.,-1.));
#20815=DIRECTION('center_axis',(0.,0.,-1.));
#20816=DIRECTION('ref_axis',(1.,9.72557910080329E-14,0.));
#20817=DIRECTION('center_axis',(0.,0.,1.));
#20818=DIRECTION('ref_axis',(0.17681385355385,-0.984244309707421,0.));
#20819=DIRECTION('',(0.,0.,-1.));
#20820=DIRECTION('center_axis',(0.,0.,1.));
#20821=DIRECTION('ref_axis',(0.17681385355385,-0.984244309707421,0.));
#20822=DIRECTION('',(0.,0.,-1.));
#20823=DIRECTION('center_axis',(0.,0.,1.));
#20824=DIRECTION('ref_axis',(0.17681385355385,-0.984244309707421,0.));
#20825=DIRECTION('',(0.,0.,-1.));
#20826=DIRECTION('center_axis',(0.,0.,1.));
#20827=DIRECTION('ref_axis',(0.17681385355385,-0.984244309707421,0.));
#20828=DIRECTION('',(0.,0.,-1.));
#20829=DIRECTION('center_axis',(0.,0.,1.));
#20830=DIRECTION('ref_axis',(0.17681385355385,-0.984244309707421,0.));
#20831=DIRECTION('',(0.,0.,-1.));
#20832=DIRECTION('center_axis',(0.,0.,1.));
#20833=DIRECTION('ref_axis',(0.17681385355385,-0.984244309707421,0.));
#20834=DIRECTION('',(0.,0.,-1.));
#20835=DIRECTION('center_axis',(0.,0.,1.));
#20836=DIRECTION('ref_axis',(0.17681385355385,-0.984244309707421,0.));
#20837=DIRECTION('',(0.,0.,-1.));
#20838=DIRECTION('center_axis',(0.,0.,1.));
#20839=DIRECTION('ref_axis',(0.17681385355385,-0.984244309707421,0.));
#20840=DIRECTION('',(0.,0.,-1.));
#20841=DIRECTION('center_axis',(0.,0.,1.));
#20842=DIRECTION('ref_axis',(0.17681385355385,-0.984244309707421,0.));
#20843=DIRECTION('',(0.,0.,-1.));
#20844=DIRECTION('center_axis',(0.,0.,1.));
#20845=DIRECTION('ref_axis',(0.17681385355385,-0.984244309707421,0.));
#20846=DIRECTION('',(0.,0.,-1.));
#20847=DIRECTION('center_axis',(0.,0.,1.));
#20848=DIRECTION('ref_axis',(0.17681385355385,-0.984244309707421,0.));
#20849=DIRECTION('',(0.,0.,-1.));
#20850=DIRECTION('center_axis',(0.,0.,1.));
#20851=DIRECTION('ref_axis',(0.17681385355385,-0.984244309707421,0.));
#20852=DIRECTION('',(0.,0.,-1.));
#20853=DIRECTION('center_axis',(0.,0.,1.));
#20854=DIRECTION('ref_axis',(0.17681385355385,-0.984244309707421,0.));
#20855=DIRECTION('',(0.,0.,-1.));
#20856=DIRECTION('center_axis',(0.,0.,1.));
#20857=DIRECTION('ref_axis',(0.17681385355385,-0.984244309707421,0.));
#20858=DIRECTION('',(0.,0.,-1.));
#20859=DIRECTION('center_axis',(0.,0.,1.));
#20860=DIRECTION('ref_axis',(1.,0.,0.));
#20861=DIRECTION('center_axis',(0.,0.,1.));
#20862=DIRECTION('ref_axis',(1.,0.,0.));
#20863=DIRECTION('center_axis',(-0.00688311457455106,0.0538278304439539,
0.998526508112554));
#20864=DIRECTION('ref_axis',(-0.982071861916797,-0.188476423288724,0.00339055977177));
#20865=DIRECTION('center_axis',(0.,0.,1.));
#20866=DIRECTION('ref_axis',(1.,0.,0.));
#20867=DIRECTION('center_axis',(0.,0.,1.));
#20868=DIRECTION('ref_axis',(1.,0.,0.));
#20869=DIRECTION('center_axis',(0.,0.,1.));
#20870=DIRECTION('ref_axis',(-0.501290049117399,-0.865279311353205,0.));
#20871=DIRECTION('center_axis',(0.,0.,1.));
#20872=DIRECTION('ref_axis',(1.,9.72557910080329E-14,0.));
#20873=DIRECTION('center_axis',(0.,0.,1.));
#20874=DIRECTION('ref_axis',(1.,0.,0.));
#20875=DIRECTION('center_axis',(0.,0.,1.));
#20876=DIRECTION('ref_axis',(1.,0.,0.));
#20877=DIRECTION('center_axis',(0.,0.,1.));
#20878=DIRECTION('ref_axis',(1.,0.,0.));
#20879=DIRECTION('center_axis',(0.,0.,1.));
#20880=DIRECTION('ref_axis',(1.,0.,0.));
#20881=DIRECTION('center_axis',(0.,0.,1.));
#20882=DIRECTION('ref_axis',(1.,0.,0.));
#20883=DIRECTION('center_axis',(0.,0.,1.));
#20884=DIRECTION('ref_axis',(1.,0.,0.));
#20885=DIRECTION('center_axis',(0.,0.,-1.));
#20886=DIRECTION('ref_axis',(1.,0.,0.));
#20887=DIRECTION('center_axis',(-1.22464679914735E-16,1.,0.));
#20888=DIRECTION('ref_axis',(-1.,-1.22464679914735E-16,0.));
#20889=DIRECTION('center_axis',(0.,0.,-1.));
#20890=DIRECTION('ref_axis',(-1.,0.,0.));
#20891=DIRECTION('center_axis',(0.,0.,1.));
#20892=DIRECTION('ref_axis',(1.,0.,0.));
#20893=DIRECTION('center_axis',(0.,0.,1.));
#20894=DIRECTION('ref_axis',(1.,0.,0.));
#20895=DIRECTION('',(-0.86602540378444,-1.06057523872491E-16,0.499999999999998));
#20896=DIRECTION('center_axis',(0.,0.,-1.));
#20897=DIRECTION('ref_axis',(1.,0.,0.));
#20898=DIRECTION('center_axis',(-0.5,-0.866025403784439,0.));
#20899=DIRECTION('ref_axis',(-0.866025403784439,0.5,0.));
#20900=DIRECTION('',(0.,0.,-1.));
#20901=DIRECTION('',(-0.866025403784439,0.5,0.));
#20902=DIRECTION('',(0.,0.,-1.));
#20903=DIRECTION('center_axis',(0.5,-0.866025403784439,0.));
#20904=DIRECTION('ref_axis',(-0.866025403784439,-0.5,0.));
#20905=DIRECTION('',(0.,0.,-1.));
#20906=DIRECTION('',(-0.866025403784439,-0.5,0.));
#20907=DIRECTION('center_axis',(1.,-3.84592537276713E-16,0.));
#20908=DIRECTION('ref_axis',(-3.84592537276713E-16,-1.,0.));
#20909=DIRECTION('',(0.,0.,-1.));
#20910=DIRECTION('',(-3.84592537276713E-16,-1.,0.));
#20911=DIRECTION('center_axis',(0.,0.,1.));
#20912=DIRECTION('ref_axis',(1.,0.,0.));
#20913=DIRECTION('',(-0.855621686410732,-1.04783435954396E-16,0.517601709564076));
#20914=DIRECTION('center_axis',(0.,0.,-1.));
#20915=DIRECTION('ref_axis',(1.,0.,0.));
#20916=DIRECTION('center_axis',(0.5,0.866025403784439,0.));
#20917=DIRECTION('ref_axis',(0.866025403784439,-0.5,0.));
#20918=DIRECTION('',(0.,0.,-1.));
#20919=DIRECTION('',(0.866025403784439,-0.5,0.));
#20920=DIRECTION('center_axis',(-0.5,0.866025403784439,0.));
#20921=DIRECTION('ref_axis',(0.866025403784439,0.5,0.));
#20922=DIRECTION('',(0.,0.,-1.));
#20923=DIRECTION('',(0.866025403784439,0.5,0.));
#20924=DIRECTION('center_axis',(-1.,-1.92296268638356E-16,0.));
#20925=DIRECTION('ref_axis',(-1.92296268638356E-16,1.,0.));
#20926=DIRECTION('',(-1.92296268638356E-16,1.,0.));
#20927=DIRECTION('center_axis',(0.,0.,-1.));
#20928=DIRECTION('ref_axis',(-1.,0.,0.));
#20929=DIRECTION('center_axis',(0.,0.,1.));
#20930=DIRECTION('ref_axis',(1.,0.,0.));
#20931=DIRECTION('center_axis',(0.,0.,-1.));
#20932=DIRECTION('ref_axis',(-1.,1.22464679914735E-16,0.));
#20933=DIRECTION('center_axis',(1.22464679914735E-16,-1.,0.));
#20934=DIRECTION('ref_axis',(-1.,-1.22464679914735E-16,0.));
#20935=DIRECTION('center_axis',(0.,0.,1.));
#20936=DIRECTION('ref_axis',(-1.,1.22464679914735E-16,0.));
#20937=DIRECTION('center_axis',(0.,0.,1.));
#20938=DIRECTION('ref_axis',(1.,0.,0.));
#20939=DIRECTION('',(0.,0.,-1.));
#20940=DIRECTION('center_axis',(0.,0.,1.));
#20941=DIRECTION('ref_axis',(1.,0.,0.));
#20942=DIRECTION('center_axis',(0.,0.,1.));
#20943=DIRECTION('ref_axis',(1.,0.,0.));
#20944=DIRECTION('center_axis',(0.,0.,-1.));
#20945=DIRECTION('ref_axis',(-1.,0.,0.));
#20946=DIRECTION('center_axis',(0.,0.,1.));
#20947=DIRECTION('ref_axis',(1.,0.,0.));
#20948=DIRECTION('center_axis',(0.,0.,1.));
#20949=DIRECTION('ref_axis',(1.,0.,0.));
#20950=DIRECTION('',(0.707106781186548,8.65956056235494E-17,-0.707106781186547));
#20951=DIRECTION('center_axis',(0.,0.,1.));
#20952=DIRECTION('ref_axis',(1.,0.,0.));
#20953=DIRECTION('',(0.707106781186548,8.65956056235494E-17,-0.707106781186547));
#20954=DIRECTION('axis',(0.,0.,1.));
#20955=DIRECTION('refdir',(1.,0.,0.));
#20956=DIRECTION('center_axis',(0.,0.,1.));
#20957=DIRECTION('ref_axis',(1.,0.,0.));
#20958=DIRECTION('center_axis',(0.,0.,1.));
#20959=DIRECTION('ref_axis',(1.,0.,0.));
#20960=DIRECTION('',(0.,0.,1.));
#20961=DIRECTION('center_axis',(0.,0.,1.));
#20962=DIRECTION('ref_axis',(1.,0.,0.));
#20963=DIRECTION('center_axis',(0.,0.,-1.));
#20964=DIRECTION('ref_axis',(-1.,0.,0.));
#20965=DIRECTION('center_axis',(0.,0.,1.));
#20966=DIRECTION('ref_axis',(1.,0.,0.));
#20967=DIRECTION('center_axis',(0.,0.,1.));
#20968=DIRECTION('ref_axis',(1.,0.,0.));
#20969=DIRECTION('center_axis',(0.,0.,1.));
#20970=DIRECTION('ref_axis',(1.,0.,0.));
#20971=DIRECTION('',(0.707106781186547,8.65956056235493E-17,-0.707106781186548));
#20972=DIRECTION('center_axis',(0.,0.,1.));
#20973=DIRECTION('ref_axis',(1.,0.,0.));
#20974=DIRECTION('center_axis',(0.,0.,1.));
#20975=DIRECTION('ref_axis',(1.,0.,0.));
#20976=DIRECTION('',(0.,0.,-1.));
#20977=DIRECTION('center_axis',(0.,0.,-1.));
#20978=DIRECTION('ref_axis',(-1.,0.,0.));
#20979=DIRECTION('center_axis',(0.,0.,1.));
#20980=DIRECTION('ref_axis',(1.,0.,0.));
#20981=DIRECTION('center_axis',(0.,0.,1.));
#20982=DIRECTION('ref_axis',(1.,0.,0.));
#20983=DIRECTION('center_axis',(0.,0.,1.));
#20984=DIRECTION('ref_axis',(1.,0.,0.));
#20985=DIRECTION('',(0.707106781186548,8.65956056235494E-17,-0.707106781186547));
#20986=DIRECTION('center_axis',(0.,0.,1.));
#20987=DIRECTION('ref_axis',(1.,0.,0.));
#20988=DIRECTION('center_axis',(0.,0.,1.));
#20989=DIRECTION('ref_axis',(1.,0.,0.));
#20990=DIRECTION('',(0.,0.,-1.));
#20991=DIRECTION('center_axis',(0.,0.,-1.));
#20992=DIRECTION('ref_axis',(1.,0.,0.));
#20993=DIRECTION('',(0.707106781186548,-8.65956056235494E-17,0.707106781186547));
#20994=DIRECTION('center_axis',(0.,0.,1.));
#20995=DIRECTION('ref_axis',(1.,0.,0.));
#20996=DIRECTION('center_axis',(0.,0.,1.));
#20997=DIRECTION('ref_axis',(1.,0.,0.));
#20998=DIRECTION('center_axis',(0.,0.,-1.));
#20999=DIRECTION('ref_axis',(-1.,0.,0.));
#21000=DIRECTION('',(0.,0.,1.));
#21001=DIRECTION('',(1.,0.,0.));
#21002=DIRECTION('',(0.,0.,1.));
#21003=DIRECTION('',(1.,0.,0.));
#21004=DIRECTION('',(0.,0.,1.));
#21005=DIRECTION('',(1.,0.,0.));
#21006=DIRECTION('',(0.,0.,1.));
#21007=DIRECTION('',(1.,0.,0.));
#21008=DIRECTION('',(0.,0.,1.));
#21009=DIRECTION('',(1.,0.,0.));
#21010=DIRECTION('',(0.,0.,1.));
#21011=DIRECTION('',(1.,0.,0.));
#21012=DIRECTION('',(1.,0.,0.));
#21013=DIRECTION('',(0.,1.,0.));
#21014=DIRECTION('',(0.,1.,0.));
#21015=DIRECTION('',(1.,0.,0.));
#21016=DIRECTION('',(0.,1.,0.));
#21017=DIRECTION('',(1.,0.,0.));
#21018=DIRECTION('',(-1.,0.,0.));
#21019=DIRECTION('',(0.,1.,0.));
#21020=DIRECTION('',(1.,0.,0.));
#21021=DIRECTION('',(0.,1.,0.));
#21022=DIRECTION('',(1.,0.,0.));
#21023=DIRECTION('',(0.,-1.,0.));
#21024=DIRECTION('',(0.,0.,1.));
#21025=DIRECTION('',(1.,0.,0.));
#21026=DIRECTION('',(0.,0.,1.));
#21027=DIRECTION('',(1.,0.,0.));
#21028=DIRECTION('',(-1.,0.,0.));
#21029=DIRECTION('',(0.,1.,0.));
#21030=DIRECTION('',(0.,-1.,0.));
#21031=DIRECTION('',(1.,0.,0.));
#21032=DIRECTION('',(0.,1.,0.));
#21033=DIRECTION('',(1.,0.,0.));
#21034=DIRECTION('',(-1.,0.,0.));
#21035=DIRECTION('',(0.,1.,0.));
#21036=DIRECTION('',(-1.,0.,0.));
#21037=DIRECTION('',(0.,1.,0.));
#21038=DIRECTION('',(0.,-1.,0.));
#21039=DIRECTION('',(1.,0.,0.));
#21040=DIRECTION('',(0.,-1.,0.));
#21041=DIRECTION('',(1.,0.,0.));
#21042=DIRECTION('',(-1.,0.,0.));
#21043=DIRECTION('',(0.,1.,0.));
#21044=DIRECTION('',(-1.,0.,0.));
#21045=DIRECTION('',(0.,1.,0.));
#21046=DIRECTION('',(-1.,0.,0.));
#21047=DIRECTION('',(0.,1.,0.));
#21048=DIRECTION('',(-1.,0.,0.));
#21049=DIRECTION('',(0.,1.,0.));
#21050=DIRECTION('',(0.,-1.,0.));
#21051=DIRECTION('',(1.,0.,0.));
#21052=DIRECTION('',(0.,-1.,0.));
#21053=DIRECTION('',(1.,0.,0.));
#21054=DIRECTION('',(0.,-1.,0.));
#21055=DIRECTION('',(1.,0.,0.));
#21056=DIRECTION('',(0.,-1.,0.));
#21057=DIRECTION('',(1.,0.,0.));
#21058=CARTESIAN_POINT('',(0.,0.,0.));
#21059=CARTESIAN_POINT('',(0.,0.,0.));
#21060=CARTESIAN_POINT('Origin',(7.2,2.3,1.4));
#21061=CARTESIAN_POINT('',(7.2,2.3,1.4));
#21062=CARTESIAN_POINT('',(7.2,1.9,1.4));
#21063=CARTESIAN_POINT('',(7.2,1.15,1.4));
#21064=CARTESIAN_POINT('',(6.6,2.3,1.4));
#21065=CARTESIAN_POINT('',(7.2,2.3,1.4));
#21066=CARTESIAN_POINT('',(6.6,1.9,1.4));
#21067=CARTESIAN_POINT('',(6.6,1.9,1.4));
#21068=CARTESIAN_POINT('',(7.2,1.9,1.4));
#21069=CARTESIAN_POINT('Origin',(7.2,2.3,10.));
#21070=CARTESIAN_POINT('',(7.2,2.3,10.));
#21071=CARTESIAN_POINT('',(7.2,2.3,13.7));
#21072=CARTESIAN_POINT('',(6.6,2.3,10.));
#21073=CARTESIAN_POINT('',(7.2,2.3,10.));
#21074=CARTESIAN_POINT('',(6.6,2.3,1.4));
#21075=CARTESIAN_POINT('Origin',(7.2,1.9,10.));
#21076=CARTESIAN_POINT('',(7.2,1.9,10.));
#21077=CARTESIAN_POINT('',(7.2,0.95,10.));
#21078=CARTESIAN_POINT('',(6.6,1.9,10.));
#21079=CARTESIAN_POINT('',(7.2,1.9,10.));
#21080=CARTESIAN_POINT('',(6.6,2.3,10.));
#21081=CARTESIAN_POINT('Origin',(7.2,1.9,1.4));
#21082=CARTESIAN_POINT('',(7.2,1.9,9.4));
#21083=CARTESIAN_POINT('',(6.6,1.9,10.));
#21084=CARTESIAN_POINT('Origin',(6.6,2.1,5.7));
#21085=CARTESIAN_POINT('Origin',(7.2,-3.3,1.4));
#21086=CARTESIAN_POINT('',(7.2,-3.6,1.4));
#21087=CARTESIAN_POINT('',(6.6,-3.6,1.4));
#21088=CARTESIAN_POINT('',(6.625,-3.6,1.4));
#21089=CARTESIAN_POINT('',(7.2,-3.3,1.4));
#21090=CARTESIAN_POINT('',(7.2,-1.65,1.4));
#21091=CARTESIAN_POINT('',(6.6,-3.3,1.4));
#21092=CARTESIAN_POINT('',(7.2,-3.3,1.4));
#21093=CARTESIAN_POINT('',(6.6,-3.7,1.4));
#21094=CARTESIAN_POINT('Origin',(6.6,-3.5,5.7));
#21095=CARTESIAN_POINT('',(6.6,-3.6,3.4));
#21096=CARTESIAN_POINT('',(6.6,-3.6,4.));
#21097=CARTESIAN_POINT('',(6.6,-3.3,10.));
#21098=CARTESIAN_POINT('',(6.6,-3.3,1.4));
#21099=CARTESIAN_POINT('',(6.6,-3.7,10.));
#21100=CARTESIAN_POINT('',(6.6,-3.3,10.));
#21101=CARTESIAN_POINT('',(6.6,-3.7,3.4));
#21102=CARTESIAN_POINT('',(6.6,-3.7,10.));
#21103=CARTESIAN_POINT('',(6.6,-3.55,3.4));
#21104=CARTESIAN_POINT('Origin',(7.2,-3.3,10.));
#21105=CARTESIAN_POINT('',(7.2,-3.3,10.));
#21106=CARTESIAN_POINT('',(7.2,-3.3,13.7));
#21107=CARTESIAN_POINT('',(7.2,-3.3,10.));
#21108=CARTESIAN_POINT('Origin',(7.2,-3.7,10.));
#21109=CARTESIAN_POINT('',(7.2,-3.7,10.));
#21110=CARTESIAN_POINT('',(7.2,-1.85,10.));
#21111=CARTESIAN_POINT('',(7.2,-3.7,10.));
#21112=CARTESIAN_POINT('Origin',(7.2,-3.7,1.4));
#21113=CARTESIAN_POINT('',(7.2,-3.7,3.4));
#21114=CARTESIAN_POINT('',(7.25,-3.7,3.4));
#21115=CARTESIAN_POINT('',(7.2,-3.7,9.4));
#21116=CARTESIAN_POINT('Origin',(7.2,-1.9,1.4));
#21117=CARTESIAN_POINT('',(7.2,-1.9,1.4));
#21118=CARTESIAN_POINT('',(7.2,-2.3,1.4));
#21119=CARTESIAN_POINT('',(7.2,-0.95,1.4));
#21120=CARTESIAN_POINT('',(6.6,-1.9,1.4));
#21121=CARTESIAN_POINT('',(7.2,-1.9,1.4));
#21122=CARTESIAN_POINT('',(6.6,-2.3,1.4));
#21123=CARTESIAN_POINT('',(6.6,-2.3,1.4));
#21124=CARTESIAN_POINT('',(7.2,-2.3,1.4));
#21125=CARTESIAN_POINT('Origin',(7.2,-1.9,10.));
#21126=CARTESIAN_POINT('',(7.2,-1.9,10.));
#21127=CARTESIAN_POINT('',(7.2,-1.9,13.7));
#21128=CARTESIAN_POINT('',(6.6,-1.9,10.));
#21129=CARTESIAN_POINT('',(7.2,-1.9,10.));
#21130=CARTESIAN_POINT('',(6.6,-1.9,1.4));
#21131=CARTESIAN_POINT('Origin',(7.2,-2.3,10.));
#21132=CARTESIAN_POINT('',(7.2,-2.3,10.));
#21133=CARTESIAN_POINT('',(7.2,-1.15,10.));
#21134=CARTESIAN_POINT('',(6.6,-2.3,10.));
#21135=CARTESIAN_POINT('',(7.2,-2.3,10.));
#21136=CARTESIAN_POINT('',(6.6,-1.9,10.));
#21137=CARTESIAN_POINT('Origin',(7.2,-2.3,1.4));
#21138=CARTESIAN_POINT('',(7.2,-2.3,9.4));
#21139=CARTESIAN_POINT('',(6.6,-2.3,10.));
#21140=CARTESIAN_POINT('Origin',(6.6,-2.1,5.7));
#21141=CARTESIAN_POINT('Origin',(7.2,-0.5,1.4));
#21142=CARTESIAN_POINT('',(7.2,-0.5,1.4));
#21143=CARTESIAN_POINT('',(7.2,-0.9,1.4));
#21144=CARTESIAN_POINT('',(7.2,-0.25,1.4));
#21145=CARTESIAN_POINT('',(6.6,-0.5,1.4));
#21146=CARTESIAN_POINT('',(7.2,-0.5,1.4));
#21147=CARTESIAN_POINT('',(6.6,-0.9,1.4));
#21148=CARTESIAN_POINT('',(6.6,-0.9,1.4));
#21149=CARTESIAN_POINT('',(7.2,-0.9,1.4));
#21150=CARTESIAN_POINT('Origin',(7.2,-0.5,10.));
#21151=CARTESIAN_POINT('',(7.2,-0.5,10.));
#21152=CARTESIAN_POINT('',(7.2,-0.5,13.7));
#21153=CARTESIAN_POINT('',(6.6,-0.5,10.));
#21154=CARTESIAN_POINT('',(7.2,-0.5,10.));
#21155=CARTESIAN_POINT('',(6.6,-0.5,1.4));
#21156=CARTESIAN_POINT('Origin',(7.2,-0.9,10.));
#21157=CARTESIAN_POINT('',(7.2,-0.9,10.));
#21158=CARTESIAN_POINT('',(7.2,-0.45,10.));
#21159=CARTESIAN_POINT('',(6.6,-0.9,10.));
#21160=CARTESIAN_POINT('',(7.2,-0.9,10.));
#21161=CARTESIAN_POINT('',(6.6,-0.5,10.));
#21162=CARTESIAN_POINT('Origin',(7.2,-0.9,1.4));
#21163=CARTESIAN_POINT('',(7.2,-0.9,9.4));
#21164=CARTESIAN_POINT('',(6.6,-0.9,10.));
#21165=CARTESIAN_POINT('Origin',(6.6,-0.7,5.7));
#21166=CARTESIAN_POINT('Origin',(7.2,0.9,1.4));
#21167=CARTESIAN_POINT('',(7.2,0.9,1.4));
#21168=CARTESIAN_POINT('',(7.2,0.5,1.4));
#21169=CARTESIAN_POINT('',(7.2,0.45,1.4));
#21170=CARTESIAN_POINT('',(6.6,0.9,1.4));
#21171=CARTESIAN_POINT('',(7.2,0.9,1.4));
#21172=CARTESIAN_POINT('',(6.6,0.5,1.4));
#21173=CARTESIAN_POINT('',(6.6,0.5,1.4));
#21174=CARTESIAN_POINT('',(7.2,0.5,1.4));
#21175=CARTESIAN_POINT('Origin',(7.2,0.9,10.));
#21176=CARTESIAN_POINT('',(7.2,0.9,10.));
#21177=CARTESIAN_POINT('',(7.2,0.9,13.7));
#21178=CARTESIAN_POINT('',(6.6,0.9,10.));
#21179=CARTESIAN_POINT('',(7.2,0.9,10.));
#21180=CARTESIAN_POINT('',(6.6,0.9,1.4));
#21181=CARTESIAN_POINT('Origin',(7.2,0.5,10.));
#21182=CARTESIAN_POINT('',(7.2,0.5,10.));
#21183=CARTESIAN_POINT('',(7.2,0.25,10.));
#21184=CARTESIAN_POINT('',(6.6,0.5,10.));
#21185=CARTESIAN_POINT('',(7.2,0.5,10.));
#21186=CARTESIAN_POINT('',(6.6,0.9,10.));
#21187=CARTESIAN_POINT('Origin',(7.2,0.5,1.4));
#21188=CARTESIAN_POINT('',(7.2,0.5,9.4));
#21189=CARTESIAN_POINT('',(6.6,0.5,10.));
#21190=CARTESIAN_POINT('Origin',(6.6,0.7,5.7));
#21191=CARTESIAN_POINT('Origin',(7.2,3.7,1.4));
#21192=CARTESIAN_POINT('',(6.6,3.6,1.4));
#21193=CARTESIAN_POINT('',(7.2,3.6,1.4));
#21194=CARTESIAN_POINT('',(6.625,3.6,1.4));
#21195=CARTESIAN_POINT('',(6.6,3.3,1.4));
#21196=CARTESIAN_POINT('',(6.6,3.3,1.4));
#21197=CARTESIAN_POINT('',(7.2,3.3,1.4));
#21198=CARTESIAN_POINT('',(7.2,3.3,1.4));
#21199=CARTESIAN_POINT('',(7.2,1.85,1.4));
#21200=CARTESIAN_POINT('Origin',(7.2,3.7,10.));
#21201=CARTESIAN_POINT('',(7.2,3.7,3.4));
#21202=CARTESIAN_POINT('',(6.6,3.7,3.4));
#21203=CARTESIAN_POINT('',(6.,3.7,3.4));
#21204=CARTESIAN_POINT('',(7.2,3.7,10.));
#21205=CARTESIAN_POINT('',(7.2,3.7,13.7));
#21206=CARTESIAN_POINT('',(6.6,3.7,10.));
#21207=CARTESIAN_POINT('',(7.2,3.7,10.));
#21208=CARTESIAN_POINT('',(6.6,3.7,1.4));
#21209=CARTESIAN_POINT('Origin',(7.2,3.3,10.));
#21210=CARTESIAN_POINT('',(7.2,3.3,10.));
#21211=CARTESIAN_POINT('',(7.2,1.65,10.));
#21212=CARTESIAN_POINT('',(6.6,3.3,10.));
#21213=CARTESIAN_POINT('',(7.2,3.3,10.));
#21214=CARTESIAN_POINT('',(6.6,3.7,10.));
#21215=CARTESIAN_POINT('Origin',(7.2,3.3,1.4));
#21216=CARTESIAN_POINT('',(7.2,3.3,9.4));
#21217=CARTESIAN_POINT('',(6.6,3.3,10.));
#21218=CARTESIAN_POINT('Origin',(6.6,3.5,5.7));
#21219=CARTESIAN_POINT('',(6.6,3.6,3.4));
#21220=CARTESIAN_POINT('',(6.6,3.6,4.));
#21221=CARTESIAN_POINT('',(6.6,3.55,3.4));
#21222=CARTESIAN_POINT('Origin',(6.05,-3.6,2.3));
#21223=CARTESIAN_POINT('',(4.8,-3.6,3.4));
#21224=CARTESIAN_POINT('',(7.3,-3.6,3.4));
#21225=CARTESIAN_POINT('',(4.8,-3.6,1.2));
#21226=CARTESIAN_POINT('',(4.8,-3.6,3.4));
#21227=CARTESIAN_POINT('',(7.2,-3.6,1.2));
#21228=CARTESIAN_POINT('',(4.8,-3.6,1.2));
#21229=CARTESIAN_POINT('',(7.2,-3.6,9.85));
#21230=CARTESIAN_POINT('Origin',(7.3,-3.6,3.4));
#21231=CARTESIAN_POINT('',(7.2,-4.6,3.4));
#21232=CARTESIAN_POINT('',(7.2,-1.8,3.4));
#21233=CARTESIAN_POINT('',(4.8,-4.6,3.4));
#21234=CARTESIAN_POINT('',(3.65,-4.6,3.4));
#21235=CARTESIAN_POINT('',(4.8,-3.6,3.4));
#21236=CARTESIAN_POINT('Origin',(7.2,0.,17.4));
#21237=CARTESIAN_POINT('',(7.2,-4.6,1.2));
#21238=CARTESIAN_POINT('',(7.2,-1.8,1.2));
#21239=CARTESIAN_POINT('',(7.2,-4.6,0.6));
#21240=CARTESIAN_POINT('',(7.2,-4.6,0.));
#21241=CARTESIAN_POINT('',(7.2,4.6,0.6));
#21242=CARTESIAN_POINT('',(7.2,0.,0.6));
#21243=CARTESIAN_POINT('',(7.2,4.6,1.2));
#21244=CARTESIAN_POINT('',(7.2,4.6,0.));
#21245=CARTESIAN_POINT('',(7.2,3.6,1.2));
#21246=CARTESIAN_POINT('',(7.2,1.8,1.2));
#21247=CARTESIAN_POINT('',(7.2,3.6,9.85));
#21248=CARTESIAN_POINT('',(7.2,4.6,3.4));
#21249=CARTESIAN_POINT('',(7.2,1.8,3.4));
#21250=CARTESIAN_POINT('',(7.2,4.6,16.8));
#21251=CARTESIAN_POINT('',(7.2,4.6,0.));
#21252=CARTESIAN_POINT('',(7.2,-4.6,16.8));
#21253=CARTESIAN_POINT('',(7.2,0.,16.8));
#21254=CARTESIAN_POINT('',(7.2,-4.6,0.));
#21255=CARTESIAN_POINT('',(7.2,-3.18408167778312E-16,10.9));
#21256=CARTESIAN_POINT('Origin',(7.2,0.,13.5));
#21257=CARTESIAN_POINT('Origin',(-7.2,2.3,6.));
#21258=CARTESIAN_POINT('',(-7.2,2.3,6.));
#21259=CARTESIAN_POINT('',(-7.2,1.9,6.));
#21260=CARTESIAN_POINT('',(-7.2,1.15,6.));
#21261=CARTESIAN_POINT('',(-6.6,2.3,6.));
#21262=CARTESIAN_POINT('',(-7.2,2.3,6.));
#21263=CARTESIAN_POINT('',(-6.6,1.9,6.));
#21264=CARTESIAN_POINT('',(-6.6,2.3,6.));
#21265=CARTESIAN_POINT('',(-7.2,1.9,6.));
#21266=CARTESIAN_POINT('Origin',(-7.2,2.3,1.4));
#21267=CARTESIAN_POINT('',(-7.2,2.3,1.4));
#21268=CARTESIAN_POINT('',(-7.2,2.3,0.7));
#21269=CARTESIAN_POINT('',(-6.6,2.3,1.4));
#21270=CARTESIAN_POINT('',(-7.2,2.3,1.4));
#21271=CARTESIAN_POINT('',(-6.6,2.3,1.4));
#21272=CARTESIAN_POINT('Origin',(-7.2,1.9,1.4));
#21273=CARTESIAN_POINT('',(-7.2,1.9,1.4));
#21274=CARTESIAN_POINT('',(-7.2,0.95,1.4));
#21275=CARTESIAN_POINT('',(-6.6,1.9,1.4));
#21276=CARTESIAN_POINT('',(-7.2,1.9,1.4));
#21277=CARTESIAN_POINT('',(-6.6,1.9,1.4));
#21278=CARTESIAN_POINT('Origin',(-7.2,1.9,6.));
#21279=CARTESIAN_POINT('',(-7.2,1.9,3.));
#21280=CARTESIAN_POINT('',(-6.6,1.9,6.));
#21281=CARTESIAN_POINT('Origin',(-6.6,2.1,3.7));
#21282=CARTESIAN_POINT('Origin',(-7.2,-3.7,1.4));
#21283=CARTESIAN_POINT('',(-6.6,-3.6,1.4));
#21284=CARTESIAN_POINT('',(-7.2,-3.6,1.4));
#21285=CARTESIAN_POINT('',(-6.625,-3.6,1.4));
#21286=CARTESIAN_POINT('',(-6.6,-3.3,1.4));
#21287=CARTESIAN_POINT('',(-6.6,-3.7,1.4));
#21288=CARTESIAN_POINT('',(-7.2,-3.3,1.4));
#21289=CARTESIAN_POINT('',(-7.2,-3.3,1.4));
#21290=CARTESIAN_POINT('',(-7.2,-1.85,1.4));
#21291=CARTESIAN_POINT('Origin',(-7.2,-3.3,6.));
#21292=CARTESIAN_POINT('',(-7.2,-3.3,6.));
#21293=CARTESIAN_POINT('',(-7.2,-3.7,6.));
#21294=CARTESIAN_POINT('',(-7.2,-1.65,6.));
#21295=CARTESIAN_POINT('',(-6.6,-3.3,6.));
#21296=CARTESIAN_POINT('',(-7.2,-3.3,6.));
#21297=CARTESIAN_POINT('',(-6.6,-3.7,6.));
#21298=CARTESIAN_POINT('',(-6.6,-3.3,6.));
#21299=CARTESIAN_POINT('',(-7.2,-3.7,6.));
#21300=CARTESIAN_POINT('Origin',(-7.2,-3.3,1.4));
#21301=CARTESIAN_POINT('',(-7.2,-3.3,0.7));
#21302=CARTESIAN_POINT('',(-6.6,-3.3,1.4));
#21303=CARTESIAN_POINT('Origin',(-7.2,-3.7,6.));
#21304=CARTESIAN_POINT('',(-7.2,-3.7,3.4));
#21305=CARTESIAN_POINT('',(-6.6,-3.7,3.4));
#21306=CARTESIAN_POINT('',(-6.,-3.7,3.4));
#21307=CARTESIAN_POINT('',(-7.2,-3.7,3.));
#21308=CARTESIAN_POINT('',(-6.6,-3.7,6.));
#21309=CARTESIAN_POINT('Origin',(-6.6,-3.5,3.7));
#21310=CARTESIAN_POINT('',(-6.6,-3.6,3.4));
#21311=CARTESIAN_POINT('',(-6.6,-3.6,3.));
#21312=CARTESIAN_POINT('',(-6.6,-3.55,3.4));
#21313=CARTESIAN_POINT('Origin',(-7.2,-1.9,6.));
#21314=CARTESIAN_POINT('',(-7.2,-1.9,6.));
#21315=CARTESIAN_POINT('',(-7.2,-2.3,6.));
#21316=CARTESIAN_POINT('',(-7.2,-0.95,6.));
#21317=CARTESIAN_POINT('',(-6.6,-1.9,6.));
#21318=CARTESIAN_POINT('',(-7.2,-1.9,6.));
#21319=CARTESIAN_POINT('',(-6.6,-2.3,6.));
#21320=CARTESIAN_POINT('',(-6.6,-1.9,6.));
#21321=CARTESIAN_POINT('',(-7.2,-2.3,6.));
#21322=CARTESIAN_POINT('Origin',(-7.2,-1.9,1.4));
#21323=CARTESIAN_POINT('',(-7.2,-1.9,1.4));
#21324=CARTESIAN_POINT('',(-7.2,-1.9,0.7));
#21325=CARTESIAN_POINT('',(-6.6,-1.9,1.4));
#21326=CARTESIAN_POINT('',(-7.2,-1.9,1.4));
#21327=CARTESIAN_POINT('',(-6.6,-1.9,1.4));
#21328=CARTESIAN_POINT('Origin',(-7.2,-2.3,1.4));
#21329=CARTESIAN_POINT('',(-7.2,-2.3,1.4));
#21330=CARTESIAN_POINT('',(-7.2,-1.15,1.4));
#21331=CARTESIAN_POINT('',(-6.6,-2.3,1.4));
#21332=CARTESIAN_POINT('',(-7.2,-2.3,1.4));
#21333=CARTESIAN_POINT('',(-6.6,-2.3,1.4));
#21334=CARTESIAN_POINT('Origin',(-7.2,-2.3,6.));
#21335=CARTESIAN_POINT('',(-7.2,-2.3,3.));
#21336=CARTESIAN_POINT('',(-6.6,-2.3,6.));
#21337=CARTESIAN_POINT('Origin',(-6.6,-2.1,3.7));
#21338=CARTESIAN_POINT('Origin',(-7.2,-0.5,6.));
#21339=CARTESIAN_POINT('',(-7.2,-0.5,6.));
#21340=CARTESIAN_POINT('',(-7.2,-0.9,6.));
#21341=CARTESIAN_POINT('',(-7.2,-0.25,6.));
#21342=CARTESIAN_POINT('',(-6.6,-0.5,6.));
#21343=CARTESIAN_POINT('',(-7.2,-0.5,6.));
#21344=CARTESIAN_POINT('',(-6.6,-0.9,6.));
#21345=CARTESIAN_POINT('',(-6.6,-0.5,6.));
#21346=CARTESIAN_POINT('',(-7.2,-0.9,6.));
#21347=CARTESIAN_POINT('Origin',(-7.2,-0.5,1.4));
#21348=CARTESIAN_POINT('',(-7.2,-0.5,1.4));
#21349=CARTESIAN_POINT('',(-7.2,-0.5,0.7));
#21350=CARTESIAN_POINT('',(-6.6,-0.5,1.4));
#21351=CARTESIAN_POINT('',(-7.2,-0.5,1.4));
#21352=CARTESIAN_POINT('',(-6.6,-0.5,1.4));
#21353=CARTESIAN_POINT('Origin',(-7.2,-0.9,1.4));
#21354=CARTESIAN_POINT('',(-7.2,-0.9,1.4));
#21355=CARTESIAN_POINT('',(-7.2,-0.45,1.4));
#21356=CARTESIAN_POINT('',(-6.6,-0.9,1.4));
#21357=CARTESIAN_POINT('',(-7.2,-0.9,1.4));
#21358=CARTESIAN_POINT('',(-6.6,-0.9,1.4));
#21359=CARTESIAN_POINT('Origin',(-7.2,-0.9,6.));
#21360=CARTESIAN_POINT('',(-7.2,-0.9,3.));
#21361=CARTESIAN_POINT('',(-6.6,-0.9,6.));
#21362=CARTESIAN_POINT('Origin',(-6.6,-0.7,3.7));
#21363=CARTESIAN_POINT('Origin',(-7.2,0.9,6.));
#21364=CARTESIAN_POINT('',(-7.2,0.9,6.));
#21365=CARTESIAN_POINT('',(-7.2,0.5,6.));
#21366=CARTESIAN_POINT('',(-7.2,0.45,6.));
#21367=CARTESIAN_POINT('',(-6.6,0.9,6.));
#21368=CARTESIAN_POINT('',(-7.2,0.9,6.));
#21369=CARTESIAN_POINT('',(-6.6,0.5,6.));
#21370=CARTESIAN_POINT('',(-6.6,0.9,6.));
#21371=CARTESIAN_POINT('',(-7.2,0.5,6.));
#21372=CARTESIAN_POINT('Origin',(-7.2,0.9,1.4));
#21373=CARTESIAN_POINT('',(-7.2,0.9,1.4));
#21374=CARTESIAN_POINT('',(-7.2,0.9,0.7));
#21375=CARTESIAN_POINT('',(-6.6,0.9,1.4));
#21376=CARTESIAN_POINT('',(-7.2,0.9,1.4));
#21377=CARTESIAN_POINT('',(-6.6,0.9,1.4));
#21378=CARTESIAN_POINT('Origin',(-7.2,0.5,1.4));
#21379=CARTESIAN_POINT('',(-7.2,0.5,1.4));
#21380=CARTESIAN_POINT('',(-7.2,0.25,1.4));
#21381=CARTESIAN_POINT('',(-6.6,0.5,1.4));
#21382=CARTESIAN_POINT('',(-7.2,0.5,1.4));
#21383=CARTESIAN_POINT('',(-6.6,0.5,1.4));
#21384=CARTESIAN_POINT('Origin',(-7.2,0.5,6.));
#21385=CARTESIAN_POINT('',(-7.2,0.5,3.));
#21386=CARTESIAN_POINT('',(-6.6,0.5,6.));
#21387=CARTESIAN_POINT('Origin',(-6.6,0.7,3.7));
#21388=CARTESIAN_POINT('Origin',(-7.2,3.7,1.4));
#21389=CARTESIAN_POINT('',(-6.6,3.7,3.4));
#21390=CARTESIAN_POINT('',(-7.2,3.7,3.4));
#21391=CARTESIAN_POINT('',(-7.25,3.7,3.4));
#21392=CARTESIAN_POINT('',(-6.6,3.7,6.));
#21393=CARTESIAN_POINT('',(-6.6,3.7,1.4));
#21394=CARTESIAN_POINT('',(-7.2,3.7,6.));
#21395=CARTESIAN_POINT('',(-7.2,3.7,6.));
#21396=CARTESIAN_POINT('',(-7.2,3.7,0.7));
#21397=CARTESIAN_POINT('Origin',(-7.2,3.7,6.));
#21398=CARTESIAN_POINT('',(-7.2,3.3,6.));
#21399=CARTESIAN_POINT('',(-7.2,1.85,6.));
#21400=CARTESIAN_POINT('',(-6.6,3.3,6.));
#21401=CARTESIAN_POINT('',(-6.6,3.7,6.));
#21402=CARTESIAN_POINT('',(-7.2,3.3,6.));
#21403=CARTESIAN_POINT('Origin',(-7.2,3.3,1.4));
#21404=CARTESIAN_POINT('',(-7.2,3.6,1.4));
#21405=CARTESIAN_POINT('',(-6.6,3.6,1.4));
#21406=CARTESIAN_POINT('',(-6.625,3.6,1.4));
#21407=CARTESIAN_POINT('',(-7.2,3.3,1.4));
#21408=CARTESIAN_POINT('',(-7.2,1.65,1.4));
#21409=CARTESIAN_POINT('',(-6.6,3.3,1.4));
#21410=CARTESIAN_POINT('',(-7.2,3.3,1.4));
#21411=CARTESIAN_POINT('',(-6.6,3.3,1.4));
#21412=CARTESIAN_POINT('Origin',(-7.2,3.3,6.));
#21413=CARTESIAN_POINT('',(-7.2,3.3,3.));
#21414=CARTESIAN_POINT('',(-6.6,3.3,6.));
#21415=CARTESIAN_POINT('Origin',(-6.6,3.5,3.7));
#21416=CARTESIAN_POINT('',(-6.6,3.6,3.4));
#21417=CARTESIAN_POINT('',(-6.6,3.55,3.4));
#21418=CARTESIAN_POINT('',(-6.6,3.6,3.));
#21419=CARTESIAN_POINT('Origin',(-6.05,-3.6,2.3));
#21420=CARTESIAN_POINT('',(-7.2,-3.6,1.2));
#21421=CARTESIAN_POINT('',(-7.2,-3.6,1.15));
#21422=CARTESIAN_POINT('',(-4.8,-3.6,1.2));
#21423=CARTESIAN_POINT('',(-7.3,-3.6,1.2));
#21424=CARTESIAN_POINT('',(-4.8,-3.6,3.4));
#21425=CARTESIAN_POINT('',(-4.8,-3.6,1.2));
#21426=CARTESIAN_POINT('',(-4.8,-3.6,3.4));
#21427=CARTESIAN_POINT('Origin',(-7.3,3.6,3.4));
#21428=CARTESIAN_POINT('',(-7.2,4.6,3.4));
#21429=CARTESIAN_POINT('',(-7.2,1.8,3.4));
#21430=CARTESIAN_POINT('',(-4.8,4.6,3.4));
#21431=CARTESIAN_POINT('',(-3.65,4.6,3.4));
#21432=CARTESIAN_POINT('',(-4.8,3.6,3.4));
#21433=CARTESIAN_POINT('',(-4.8,3.6,3.4));
#21434=CARTESIAN_POINT('',(-4.8,3.6,3.4));
#21435=CARTESIAN_POINT('Origin',(-7.2,0.,0.));
#21436=CARTESIAN_POINT('',(-7.2,-4.6,3.4));
#21437=CARTESIAN_POINT('',(-7.2,-1.8,3.4));
#21438=CARTESIAN_POINT('',(-7.2,-4.6,16.8));
#21439=CARTESIAN_POINT('',(-7.2,-4.6,17.4));
#21440=CARTESIAN_POINT('',(-7.2,-3.51681487422156,16.8));
#21441=CARTESIAN_POINT('',(-7.2,0.,16.8));
#21442=CARTESIAN_POINT('',(-7.2,-2.827,16.682));
#21443=CARTESIAN_POINT('Origin',(-7.2,-3.182,16.682));
#21444=CARTESIAN_POINT('',(-7.2,-2.84718512577844,16.8));
#21445=CARTESIAN_POINT('Origin',(-7.2,-3.182,16.682));
#21446=CARTESIAN_POINT('',(-7.2,2.84718512577844,16.8));
#21447=CARTESIAN_POINT('',(-7.2,0.,16.8));
#21448=CARTESIAN_POINT('',(-7.2,3.537,16.682));
#21449=CARTESIAN_POINT('Origin',(-7.2,3.182,16.682));
#21450=CARTESIAN_POINT('',(-7.2,3.51681487422156,16.8));
#21451=CARTESIAN_POINT('Origin',(-7.2,3.182,16.682));
#21452=CARTESIAN_POINT('',(-7.2,4.6,16.8));
#21453=CARTESIAN_POINT('',(-7.2,0.,16.8));
#21454=CARTESIAN_POINT('',(-7.2,4.6,17.4));
#21455=CARTESIAN_POINT('',(-7.2,3.6,1.2));
#21456=CARTESIAN_POINT('',(-7.2,3.6,1.15));
#21457=CARTESIAN_POINT('',(-7.2,4.6,1.2));
#21458=CARTESIAN_POINT('',(-7.2,1.8,1.2));
#21459=CARTESIAN_POINT('',(-7.2,4.6,0.600000000000001));
#21460=CARTESIAN_POINT('',(-7.2,4.6,17.4));
#21461=CARTESIAN_POINT('',(-7.2,-4.6,0.600000000000001));
#21462=CARTESIAN_POINT('',(-7.2,0.,0.6));
#21463=CARTESIAN_POINT('',(-7.2,-4.6,1.2));
#21464=CARTESIAN_POINT('',(-7.2,-4.6,17.4));
#21465=CARTESIAN_POINT('',(-7.2,-1.8,1.2));
#21466=CARTESIAN_POINT('',(-7.2,-3.18408167778312E-16,10.9));
#21467=CARTESIAN_POINT('Origin',(-7.2,0.,13.5));
#21468=CARTESIAN_POINT('',(-7.2,3.537,10.318));
#21469=CARTESIAN_POINT('Origin',(-7.2,3.182,10.318));
#21470=CARTESIAN_POINT('',(-7.2,-2.827,10.318));
#21471=CARTESIAN_POINT('Origin',(-7.2,-3.182,10.318));
#21472=CARTESIAN_POINT('Origin',(0.,-4.6,7.2));
#21473=CARTESIAN_POINT('',(5.57660788571496,-4.6,8.79419085713778));
#21474=CARTESIAN_POINT('',(-5.57660788571496,-4.6,8.79419085713778));
#21475=CARTESIAN_POINT('Origin',(0.,-4.6,7.2));
#21476=CARTESIAN_POINT('',(5.57660788571496,-4.1,8.79419085713778));
#21477=CARTESIAN_POINT('',(5.57660788571496,-4.6,8.79419085713778));
#21478=CARTESIAN_POINT('',(-5.57660788571496,-4.1,8.79419085713778));
#21479=CARTESIAN_POINT('Origin',(0.,-4.1,7.2));
#21480=CARTESIAN_POINT('',(-5.57660788571496,-4.6,8.79419085713778));
#21481=CARTESIAN_POINT('Origin',(6.,-4.6,8.));
#21482=CARTESIAN_POINT('',(6.4,-4.6,8.80622577482985));
#21483=CARTESIAN_POINT('Origin',(6.,-4.6,8.));
#21484=CARTESIAN_POINT('',(6.4,-4.1,8.80622577482985));
#21485=CARTESIAN_POINT('',(6.4,-4.6,8.80622577482985));
#21486=CARTESIAN_POINT('Origin',(6.,-4.1,8.));
#21487=CARTESIAN_POINT('Origin',(6.4,-4.6,16.));
#21488=CARTESIAN_POINT('',(6.4,-4.6,16.));
#21489=CARTESIAN_POINT('',(6.4,-4.6,12.35));
#21490=CARTESIAN_POINT('',(6.4,-4.1,16.));
#21491=CARTESIAN_POINT('',(6.4,-4.6,16.));
#21492=CARTESIAN_POINT('',(6.4,-4.1,1.4));
#21493=CARTESIAN_POINT('Origin',(-6.4,-4.6,16.));
#21494=CARTESIAN_POINT('',(-6.4,-4.6,16.));
#21495=CARTESIAN_POINT('',(-3.2,-4.6,16.));
#21496=CARTESIAN_POINT('',(-6.4,-4.1,16.));
#21497=CARTESIAN_POINT('',(-6.4,-4.6,16.));
#21498=CARTESIAN_POINT('',(6.4,-4.1,16.));
#21499=CARTESIAN_POINT('Origin',(-6.4,-4.6,8.80622577482985));
#21500=CARTESIAN_POINT('',(-6.4,-4.6,8.80622577482985));
#21501=CARTESIAN_POINT('',(-6.4,-4.6,8.75311288741493));
#21502=CARTESIAN_POINT('',(-6.4,-4.1,8.80622577482985));
#21503=CARTESIAN_POINT('',(-6.4,-4.6,8.80622577482985));
#21504=CARTESIAN_POINT('',(-6.4,-4.1,16.));
#21505=CARTESIAN_POINT('Origin',(-6.,-4.6,8.));
#21506=CARTESIAN_POINT('Origin',(-6.,-4.6,8.));
#21507=CARTESIAN_POINT('Origin',(-6.,-4.1,8.));
#21508=CARTESIAN_POINT('Origin',(0.,-4.1,12.3970954285689));
#21509=CARTESIAN_POINT('Origin',(-6.4,4.6,16.));
#21510=CARTESIAN_POINT('',(-6.4,4.6,16.));
#21511=CARTESIAN_POINT('',(-6.4,4.6,8.80622577482985));
#21512=CARTESIAN_POINT('',(-6.4,4.6,12.35));
#21513=CARTESIAN_POINT('',(-6.4,4.1,16.));
#21514=CARTESIAN_POINT('',(-6.4,4.6,16.));
#21515=CARTESIAN_POINT('',(-6.4,4.1,8.80622577482985));
#21516=CARTESIAN_POINT('',(-6.4,4.1,16.));
#21517=CARTESIAN_POINT('',(-6.4,4.6,8.80622577482985));
#21518=CARTESIAN_POINT('Origin',(6.4,4.6,16.));
#21519=CARTESIAN_POINT('',(6.4,4.6,16.));
#21520=CARTESIAN_POINT('',(3.2,4.6,16.));
#21521=CARTESIAN_POINT('',(6.4,4.1,16.));
#21522=CARTESIAN_POINT('',(6.4,4.6,16.));
#21523=CARTESIAN_POINT('',(6.4,4.1,16.));
#21524=CARTESIAN_POINT('Origin',(6.4,4.6,8.80622577482985));
#21525=CARTESIAN_POINT('',(6.4,4.6,8.80622577482985));
#21526=CARTESIAN_POINT('',(6.4,4.6,8.75311288741493));
#21527=CARTESIAN_POINT('',(6.4,4.1,8.80622577482985));
#21528=CARTESIAN_POINT('',(6.4,4.6,8.80622577482985));
#21529=CARTESIAN_POINT('',(6.4,4.1,1.4));
#21530=CARTESIAN_POINT('Origin',(0.,4.1,12.3970954285689));
#21531=CARTESIAN_POINT('',(-5.57660788571496,4.1,8.79419085713778));
#21532=CARTESIAN_POINT('Origin',(-6.,4.1,8.));
#21533=CARTESIAN_POINT('',(5.57660788571496,4.1,8.79419085713778));
#21534=CARTESIAN_POINT('Origin',(6.,4.1,8.));
#21535=CARTESIAN_POINT('Origin',(0.,4.1,7.2));
#21536=CARTESIAN_POINT('Origin',(0.,4.6,8.7));
#21537=CARTESIAN_POINT('',(-5.79948381734181,4.6,7.12262136993645));
#21538=CARTESIAN_POINT('Origin',(-6.,4.6,8.));
#21539=CARTESIAN_POINT('',(-4.39098268679659,4.6,3.41063711895356));
#21540=CARTESIAN_POINT('Origin',(0.,4.6,7.2));
#21541=CARTESIAN_POINT('',(-4.8,4.6,3.01231056256177));
#21542=CARTESIAN_POINT('Origin',(-4.,4.6,2.6));
#21543=CARTESIAN_POINT('',(-4.8,4.6,6.05));
#21544=CARTESIAN_POINT('',(-6.6,4.6,17.4));
#21545=CARTESIAN_POINT('Origin',(-6.6,4.6,16.8));
#21546=CARTESIAN_POINT('',(6.6,4.6,17.4));
#21547=CARTESIAN_POINT('',(7.2,4.6,17.4));
#21548=CARTESIAN_POINT('Origin',(6.6,4.6,16.8));
#21549=CARTESIAN_POINT('',(4.8,4.6,3.4));
#21550=CARTESIAN_POINT('',(2.4,4.6,3.4));
#21551=CARTESIAN_POINT('',(4.8,4.6,3.01231056256177));
#21552=CARTESIAN_POINT('',(4.8,4.6,4.95));
#21553=CARTESIAN_POINT('',(4.39098268679659,4.6,3.41063711895356));
#21554=CARTESIAN_POINT('Origin',(4.,4.6,2.6));
#21555=CARTESIAN_POINT('',(5.79948381734181,4.6,7.12262136993645));
#21556=CARTESIAN_POINT('Origin',(0.,4.6,7.2));
#21557=CARTESIAN_POINT('Origin',(6.,4.6,8.));
#21558=CARTESIAN_POINT('Origin',(0.,5.55,7.2));
#21559=CARTESIAN_POINT('',(-5.69969977760644,5.6,7.25850166795172));
#21560=CARTESIAN_POINT('',(-4.22058574132406,5.6,3.36898760115136));
#21561=CARTESIAN_POINT('Origin',(0.,5.6,7.2));
#21562=CARTESIAN_POINT('',(-4.39098268679659,5.5,3.41063711895356));
#21563=CARTESIAN_POINT('Ctrl Pts',(-4.22058574132406,5.6,3.36898760115136));
#21564=CARTESIAN_POINT('Ctrl Pts',(-4.27772143963443,5.56861968092285,3.38524395544776));
#21565=CARTESIAN_POINT('Ctrl Pts',(-4.33480274427802,5.53491157572285,3.39897341264218));
#21566=CARTESIAN_POINT('Ctrl Pts',(-4.39098268679659,5.5,3.41063711895356));
#21567=CARTESIAN_POINT('',(-5.79948381734181,5.5,7.12262136993645));
#21568=CARTESIAN_POINT('Origin',(0.,5.5,7.2));
#21569=CARTESIAN_POINT('Ctrl Pts',(-5.69969977760644,5.6,7.25850166795172));
#21570=CARTESIAN_POINT('Ctrl Pts',(-5.73181372922814,5.56837145414589,7.21137187414533));
#21571=CARTESIAN_POINT('Ctrl Pts',(-5.76536271654192,5.53469693041621,7.16601092713632));
#21572=CARTESIAN_POINT('Ctrl Pts',(-5.79948381734181,5.5,7.12262136993645));
#21573=CARTESIAN_POINT('Origin',(-4.,5.55,2.6));
#21574=CARTESIAN_POINT('',(-4.7,5.6,2.98729833462074));
#21575=CARTESIAN_POINT('Origin',(-4.,5.6,2.6));
#21576=CARTESIAN_POINT('',(-4.8,5.5,3.01231056256177));
#21577=CARTESIAN_POINT('Origin',(-110.862782237101,-100.562782237101,2.99768857927433));
#21578=CARTESIAN_POINT('Origin',(-4.,5.5,2.6));
#21579=CARTESIAN_POINT('Origin',(-4.75,5.55,5.3));
#21580=CARTESIAN_POINT('',(-4.7,5.6,2.21270166537926));
#21581=CARTESIAN_POINT('',(-4.7,5.6,5.3));
#21582=CARTESIAN_POINT('',(-4.8,5.5,2.18768943743823));
#21583=CARTESIAN_POINT('Origin',(-110.862909719179,-100.562909719179,2.20231142463878));
#21584=CARTESIAN_POINT('',(-4.8,5.5,5.3));
#21585=CARTESIAN_POINT('Origin',(-4.,5.55,2.6));
#21586=CARTESIAN_POINT('',(-3.20783191206668,5.6,2.48833209744929));
#21587=CARTESIAN_POINT('Origin',(-4.,5.6,2.6));
#21588=CARTESIAN_POINT('',(-3.14292474054464,5.5,2.32536933960403));
#21589=CARTESIAN_POINT('Ctrl Pts',(-3.20783191206668,5.6,2.48833209744929));
#21590=CARTESIAN_POINT('Ctrl Pts',(-3.18379924141574,5.56861968092285,2.43400726134455));
#21591=CARTESIAN_POINT('Ctrl Pts',(-3.16227654075062,5.53491157572284,2.37938540957487));
#21592=CARTESIAN_POINT('Ctrl Pts',(-3.14292474054464,5.5,2.32536933960403));
#21593=CARTESIAN_POINT('Origin',(-4.,5.5,2.6));
#21594=CARTESIAN_POINT('Origin',(0.,5.55,7.2));
#21595=CARTESIAN_POINT('',(3.20783191206668,5.6,2.48833209744929));
#21596=CARTESIAN_POINT('Origin',(0.,5.6,7.2));
#21597=CARTESIAN_POINT('',(3.14292474054464,5.5,2.32536933960403));
#21598=CARTESIAN_POINT('Ctrl Pts',(3.20783191206668,5.6,2.48833209744929));
#21599=CARTESIAN_POINT('Ctrl Pts',(3.18379924141574,5.56861968092285,2.43400726134454));
#21600=CARTESIAN_POINT('Ctrl Pts',(3.16227654075062,5.53491157572284,2.37938540957487));
#21601=CARTESIAN_POINT('Ctrl Pts',(3.14292474054464,5.5,2.32536933960403));
#21602=CARTESIAN_POINT('Origin',(0.,5.5,7.2));
#21603=CARTESIAN_POINT('Origin',(4.,5.55,2.6));
#21604=CARTESIAN_POINT('',(4.7,5.6,2.21270166537926));
#21605=CARTESIAN_POINT('Origin',(4.,5.6,2.6));
#21606=CARTESIAN_POINT('',(4.8,5.5,2.18768943743823));
#21607=CARTESIAN_POINT('Origin',(110.863125461215,-100.563125461335,2.20231141751144));
#21608=CARTESIAN_POINT('Origin',(4.,5.5,2.6));
#21609=CARTESIAN_POINT('Origin',(4.75,5.55,4.2));
#21610=CARTESIAN_POINT('',(4.7,5.6,2.98729833462074));
#21611=CARTESIAN_POINT('',(4.7,5.6,4.2));
#21612=CARTESIAN_POINT('',(4.8,5.5,3.01231056256177));
#21613=CARTESIAN_POINT('Origin',(110.863314523851,-100.563314523971,2.99768857098632));
#21614=CARTESIAN_POINT('',(4.8,5.5,4.2));
#21615=CARTESIAN_POINT('Origin',(4.,5.55,2.6));
#21616=CARTESIAN_POINT('',(4.39098268679659,5.5,3.41063711895356));
#21617=CARTESIAN_POINT('Origin',(4.,5.5,2.6));
#21618=CARTESIAN_POINT('',(4.22058574132406,5.6,3.36898760115135));
#21619=CARTESIAN_POINT('Origin',(4.,5.6,2.6));
#21620=CARTESIAN_POINT('Ctrl Pts',(4.22058574132406,5.6,3.36898760115136));
#21621=CARTESIAN_POINT('Ctrl Pts',(4.27772143963443,5.56861968092285,3.38524395544776));
#21622=CARTESIAN_POINT('Ctrl Pts',(4.33480274427803,5.53491157572284,3.39897341264218));
#21623=CARTESIAN_POINT('Ctrl Pts',(4.39098268679659,5.5,3.41063711895356));
#21624=CARTESIAN_POINT('Origin',(0.,5.55,7.2));
#21625=CARTESIAN_POINT('',(5.79948381734181,5.5,7.12262136993645));
#21626=CARTESIAN_POINT('Origin',(0.,5.5,7.2));
#21627=CARTESIAN_POINT('',(5.69969977760644,5.6,7.25850166795172));
#21628=CARTESIAN_POINT('Origin',(0.,5.6,7.2));
#21629=CARTESIAN_POINT('Ctrl Pts',(5.69969977760644,5.6,7.25850166795172));
#21630=CARTESIAN_POINT('Ctrl Pts',(5.73181372922814,5.56837145414589,7.21137187414533));
#21631=CARTESIAN_POINT('Ctrl Pts',(5.76536271654191,5.53469693041622,7.16601092713632));
#21632=CARTESIAN_POINT('Ctrl Pts',(5.79948381734181,5.5,7.12262136993645));
#21633=CARTESIAN_POINT('Origin',(6.,5.55,8.));
#21634=CARTESIAN_POINT('',(5.57660788571496,5.5,8.79419085713778));
#21635=CARTESIAN_POINT('Origin',(6.,5.5,8.));
#21636=CARTESIAN_POINT('',(5.51591157610535,5.6,8.63691317920985));
#21637=CARTESIAN_POINT('Origin',(6.,5.6,8.));
#21638=CARTESIAN_POINT('Ctrl Pts',(5.51591157610535,5.6,8.63691317920985));
#21639=CARTESIAN_POINT('Ctrl Pts',(5.53455522536305,5.56837145414589,8.6908106531335));
#21640=CARTESIAN_POINT('Ctrl Pts',(5.55504723137093,5.53469693041621,8.74337706591873));
#21641=CARTESIAN_POINT('Ctrl Pts',(5.57660788571496,5.5,8.79419085713778));
#21642=CARTESIAN_POINT('Origin',(0.,5.55,7.2));
#21643=CARTESIAN_POINT('',(-5.57660788571496,5.5,8.79419085713778));
#21644=CARTESIAN_POINT('Origin',(0.,5.5,7.2));
#21645=CARTESIAN_POINT('',(-5.51591157610535,5.6,8.63691317920985));
#21646=CARTESIAN_POINT('Origin',(0.,5.6,7.2));
#21647=CARTESIAN_POINT('Ctrl Pts',(-5.51591157610535,5.6,8.63691317920985));
#21648=CARTESIAN_POINT('Ctrl Pts',(-5.53455522536306,5.56837145414589,8.6908106531335));
#21649=CARTESIAN_POINT('Ctrl Pts',(-5.55504723137093,5.53469693041621,8.74337706591873));
#21650=CARTESIAN_POINT('Ctrl Pts',(-5.57660788571496,5.5,8.79419085713779));
#21651=CARTESIAN_POINT('Origin',(-6.,5.55,8.));
#21652=CARTESIAN_POINT('Origin',(-6.,5.5,8.));
#21653=CARTESIAN_POINT('Origin',(-6.,5.6,8.));
#21654=CARTESIAN_POINT('Origin',(4.,4.6,2.6));
#21655=CARTESIAN_POINT('',(4.39098268679659,4.6,3.41063711895356));
#21656=CARTESIAN_POINT('',(4.8,4.6,3.01231056256177));
#21657=CARTESIAN_POINT('Origin',(0.,4.6,7.2));
#21658=CARTESIAN_POINT('',(5.79948381734181,4.6,7.12262136993645));
#21659=CARTESIAN_POINT('Origin',(6.,4.6,8.));
#21660=CARTESIAN_POINT('',(5.57660788571496,4.6,8.79419085713778));
#21661=CARTESIAN_POINT('Origin',(0.,4.6,7.2));
#21662=CARTESIAN_POINT('',(-5.57660788571496,4.6,8.79419085713778));
#21663=CARTESIAN_POINT('Origin',(-6.,4.6,8.));
#21664=CARTESIAN_POINT('',(-5.79948381734181,4.6,7.12262136993645));
#21665=CARTESIAN_POINT('Origin',(0.,4.6,7.2));
#21666=CARTESIAN_POINT('',(-4.39098268679659,4.6,3.41063711895356));
#21667=CARTESIAN_POINT('Origin',(0.,5.6,7.2));
#21668=CARTESIAN_POINT('',(3.85763741731416E-16,5.6,4.05));
#21669=CARTESIAN_POINT('Origin',(0.,5.6,7.2));
#21670=CARTESIAN_POINT('',(6.355,5.6,8.));
#21671=CARTESIAN_POINT('Origin',(6.,5.6,8.));
#21672=CARTESIAN_POINT('',(-5.645,5.6,8.));
#21673=CARTESIAN_POINT('Origin',(-6.,5.6,8.));
#21674=CARTESIAN_POINT('',(4.355,5.6,2.6));
#21675=CARTESIAN_POINT('Origin',(4.,5.6,2.6));
#21676=CARTESIAN_POINT('',(-3.645,5.6,2.6));
#21677=CARTESIAN_POINT('Origin',(-4.,5.6,2.6));
#21678=CARTESIAN_POINT('Origin',(-2.,0.,16.4725));
#21679=CARTESIAN_POINT('',(-2.,0.505,15.7438749965183));
#21680=CARTESIAN_POINT('',(-2.505,-2.39834377745635E-17,15.8));
#21681=CARTESIAN_POINT('Ctrl Pts',(-2.,0.505,15.7438749965183));
#21682=CARTESIAN_POINT('Ctrl Pts',(-2.06363520780063,0.505,15.7438749965183));
#21683=CARTESIAN_POINT('Ctrl Pts',(-2.13136458034946,0.492239912224197,
15.7468631623588));
#21684=CARTESIAN_POINT('Ctrl Pts',(-2.25572131394491,0.440639774787125,
15.7575497283031));
#21685=CARTESIAN_POINT('Ctrl Pts',(-2.31236734386936,0.401810505129054,
15.7650822805951));
#21686=CARTESIAN_POINT('Ctrl Pts',(-2.40180683616854,0.312371012829873,
15.7791387482964));
#21687=CARTESIAN_POINT('Ctrl Pts',(-2.44063897524859,0.255723435800378,
15.7865912587439));
#21688=CARTESIAN_POINT('Ctrl Pts',(-2.49224119847989,0.131361285500179,
15.7970934401131));
#21689=CARTESIAN_POINT('Ctrl Pts',(-2.505,0.0636299871652783,15.8));
#21690=CARTESIAN_POINT('Ctrl Pts',(-2.505,6.93889390390723E-17,15.8));
#21691=CARTESIAN_POINT('Ctrl Pts',(-2.505,6.93889390390723E-17,15.8));
#21692=CARTESIAN_POINT('Ctrl Pts',(-2.505,-0.0636299871652782,15.8));
#21693=CARTESIAN_POINT('Ctrl Pts',(-2.49224119847989,-0.131361285500179,
15.7970934401131));
#21694=CARTESIAN_POINT('Ctrl Pts',(-2.44063897524859,-0.255723435800378,
15.7865912587439));
#21695=CARTESIAN_POINT('Ctrl Pts',(-2.40180683616854,-0.312371012829873,
15.7791387482964));
#21696=CARTESIAN_POINT('Ctrl Pts',(-2.31236734386936,-0.401810505129054,
15.7650822805951));
#21697=CARTESIAN_POINT('Ctrl Pts',(-2.25572131394491,-0.440639774787125,
15.7575497283031));
#21698=CARTESIAN_POINT('Ctrl Pts',(-2.13136458034946,-0.492239912224197,
15.7468631623588));
#21699=CARTESIAN_POINT('Ctrl Pts',(-2.06363520780063,-0.505,15.7438749965183));
#21700=CARTESIAN_POINT('Ctrl Pts',(-1.93636479219937,-0.505,15.7438749965183));
#21701=CARTESIAN_POINT('Ctrl Pts',(-1.86863541965054,-0.492239912224197,
15.7468631623588));
#21702=CARTESIAN_POINT('Ctrl Pts',(-1.74427868605509,-0.440639774787125,
15.7575497283031));
#21703=CARTESIAN_POINT('Ctrl Pts',(-1.68763265613064,-0.401810505129054,
15.7650822805951));
#21704=CARTESIAN_POINT('Ctrl Pts',(-1.59819316383146,-0.312371012829873,
15.7791387482964));
#21705=CARTESIAN_POINT('Ctrl Pts',(-1.55936102475141,-0.255723435800378,
15.7865912587439));
#21706=CARTESIAN_POINT('Ctrl Pts',(-1.50775880152011,-0.131361285500179,
15.7970934401131));
#21707=CARTESIAN_POINT('Ctrl Pts',(-1.495,-0.0636299871652784,15.8));
#21708=CARTESIAN_POINT('Ctrl Pts',(-1.495,0.0636299871652782,15.8));
#21709=CARTESIAN_POINT('Ctrl Pts',(-1.50775880152011,0.131361285500179,
15.7970934401131));
#21710=CARTESIAN_POINT('Ctrl Pts',(-1.55936102475141,0.255723435800378,
15.7865912587439));
#21711=CARTESIAN_POINT('Ctrl Pts',(-1.59819316383146,0.312371012829873,
15.7791387482964));
#21712=CARTESIAN_POINT('Ctrl Pts',(-1.68763265613064,0.401810505129053,
15.7650822805951));
#21713=CARTESIAN_POINT('Ctrl Pts',(-1.74427868605509,0.440639774787125,
15.7575497283031));
#21714=CARTESIAN_POINT('Ctrl Pts',(-1.86863541965054,0.492239912224197,
15.7468631623588));
#21715=CARTESIAN_POINT('Ctrl Pts',(-1.93636479219937,0.505,15.7438749965183));
#21716=CARTESIAN_POINT('Ctrl Pts',(-2.,0.505,15.7438749965183));
#21717=CARTESIAN_POINT('',(-2.505,-6.18446633569413E-17,17.345));
#21718=CARTESIAN_POINT('',(-2.505,-6.18446633569413E-17,16.4725));
#21719=CARTESIAN_POINT('Origin',(-2.,0.,17.345));
#21720=CARTESIAN_POINT('Origin',(-2.,0.,17.3975));
#21721=CARTESIAN_POINT('',(-2.56,6.85802207522515E-17,17.4));
#21722=CARTESIAN_POINT('',(-2.5575,-6.82740590524649E-17,17.3975));
#21723=CARTESIAN_POINT('Origin',(-2.,0.,17.4));
#21724=CARTESIAN_POINT('Origin',(-6.2,-3.6,16.0783257246469));
#21725=CARTESIAN_POINT('',(-6.2,-3.6,15.9566514492938));
#21726=CARTESIAN_POINT('',(-6.2,-3.195,16.2));
#21727=CARTESIAN_POINT('',(-6.2,-3.3975,16.0783257246469));
#21728=CARTESIAN_POINT('Origin',(-6.2,-3.6,16.2));
#21729=CARTESIAN_POINT('Origin',(-6.2,-3.6,16.775));
#21730=CARTESIAN_POINT('',(-6.2,-3.195,16.3772771751247));
#21731=CARTESIAN_POINT('',(-6.2,-3.195,16.775));
#21732=CARTESIAN_POINT('',(-6.58891644346826,-3.487,16.682));
#21733=CARTESIAN_POINT('Ctrl Pts',(-6.58891644346826,-3.487,16.682));
#21734=CARTESIAN_POINT('Ctrl Pts',(-6.58891644346826,-3.487,16.6370619871072));
#21735=CARTESIAN_POINT('Ctrl Pts',(-6.58627670754491,-3.47639022136029,
16.5899241279869));
#21736=CARTESIAN_POINT('Ctrl Pts',(-6.57098354914856,-3.43610864188054,
16.5071507944627));
#21737=CARTESIAN_POINT('Ctrl Pts',(-6.55767741152601,-3.40643270490172,
16.471639261428));
#21738=CARTESIAN_POINT('Ctrl Pts',(-6.52737350118872,-3.36091702023246,
16.4342657910843));
#21739=CARTESIAN_POINT('Ctrl Pts',(-6.51499170641379,-3.34453211479069,
16.4232781228103));
#21740=CARTESIAN_POINT('Ctrl Pts',(-6.48629352194951,-3.31273768137677,
16.4058454179434));
#21741=CARTESIAN_POINT('Ctrl Pts',(-6.46996141031638,-3.29738179217064,
16.3993285535958));
#21742=CARTESIAN_POINT('Ctrl Pts',(-6.42036530129365,-3.25750827485252,
16.3851229200232));
#21743=CARTESIAN_POINT('Ctrl Pts',(-6.37932965869714,-3.23386275495577,
16.3810300297351));
#21744=CARTESIAN_POINT('Ctrl Pts',(-6.29109237758623,-3.20261126494113,
16.3772905860687));
#21745=CARTESIAN_POINT('Ctrl Pts',(-6.24390854386675,-3.195,16.3772771751247));
#21746=CARTESIAN_POINT('Ctrl Pts',(-6.2,-3.195,16.3772771751247));
#21747=CARTESIAN_POINT('',(-6.2,-3.195,16.9867228248753));
#21748=CARTESIAN_POINT('Ctrl Pts',(-6.2,-3.195,16.9867228248753));
#21749=CARTESIAN_POINT('Ctrl Pts',(-6.24390854386675,-3.195,16.9867228248753));
#21750=CARTESIAN_POINT('Ctrl Pts',(-6.29109237758623,-3.20261126494113,
16.9867094139313));
#21751=CARTESIAN_POINT('Ctrl Pts',(-6.37932965869714,-3.23386275495577,
16.9829699702649));
#21752=CARTESIAN_POINT('Ctrl Pts',(-6.42036530129365,-3.25750827485252,
16.9788770799768));
#21753=CARTESIAN_POINT('Ctrl Pts',(-6.46996141031638,-3.29738179217064,
16.9646714464042));
#21754=CARTESIAN_POINT('Ctrl Pts',(-6.48629352194951,-3.31273768137677,
16.9581545820566));
#21755=CARTESIAN_POINT('Ctrl Pts',(-6.51499170641379,-3.34453211479069,
16.9407218771897));
#21756=CARTESIAN_POINT('Ctrl Pts',(-6.52737350118872,-3.36091702023246,
16.9297342089157));
#21757=CARTESIAN_POINT('Ctrl Pts',(-6.55767741152601,-3.40643270490172,
16.892360738572));
#21758=CARTESIAN_POINT('Ctrl Pts',(-6.57098354914856,-3.43610864188054,
16.8568492055373));
#21759=CARTESIAN_POINT('Ctrl Pts',(-6.58627670754491,-3.47639022136029,
16.7740758720131));
#21760=CARTESIAN_POINT('Ctrl Pts',(-6.58891644346826,-3.487,16.7269380128928));
#21761=CARTESIAN_POINT('Ctrl Pts',(-6.58891644346826,-3.487,16.682));
#21762=CARTESIAN_POINT('',(-6.2,-3.195,17.35));
#21763=CARTESIAN_POINT('',(-6.2,-3.195,16.775));
#21764=CARTESIAN_POINT('Origin',(-6.2,-3.6,17.35));
#21765=CARTESIAN_POINT('Ctrl Pts',(-6.2,-3.195,16.3772771751247));
#21766=CARTESIAN_POINT('Ctrl Pts',(-6.15609145613325,-3.195,16.3772771751247));
#21767=CARTESIAN_POINT('Ctrl Pts',(-6.10890762241377,-3.20261126494113,
16.3772905860687));
#21768=CARTESIAN_POINT('Ctrl Pts',(-6.02067034130286,-3.23386275495577,
16.3810300297351));
#21769=CARTESIAN_POINT('Ctrl Pts',(-5.97963469870635,-3.25750827485252,
16.3851229200232));
#21770=CARTESIAN_POINT('Ctrl Pts',(-5.93003858968362,-3.29738179217064,
16.3993285535958));
#21771=CARTESIAN_POINT('Ctrl Pts',(-5.91370647805049,-3.31273768137677,
16.4058454179434));
#21772=CARTESIAN_POINT('Ctrl Pts',(-5.88500829358621,-3.34453211479069,
16.4232781228103));
#21773=CARTESIAN_POINT('Ctrl Pts',(-5.87262649881128,-3.36091702023246,
16.4342657910843));
#21774=CARTESIAN_POINT('Ctrl Pts',(-5.84232258847399,-3.40643270490172,
16.471639261428));
#21775=CARTESIAN_POINT('Ctrl Pts',(-5.82901645085144,-3.43610864188054,
16.5071507944627));
#21776=CARTESIAN_POINT('Ctrl Pts',(-5.81372329245509,-3.47639022136029,
16.5899241279869));
#21777=CARTESIAN_POINT('Ctrl Pts',(-5.81108355653174,-3.487,16.6370619871072));
#21778=CARTESIAN_POINT('Ctrl Pts',(-5.81108355653174,-3.487,16.682));
#21779=CARTESIAN_POINT('Ctrl Pts',(-5.81108355653174,-3.487,16.7269380128928));
#21780=CARTESIAN_POINT('Ctrl Pts',(-5.81372329245509,-3.47639022136029,
16.7740758720131));
#21781=CARTESIAN_POINT('Ctrl Pts',(-5.82901645085144,-3.43610864188054,
16.8568492055373));
#21782=CARTESIAN_POINT('Ctrl Pts',(-5.84232258847399,-3.40643270490172,
16.892360738572));
#21783=CARTESIAN_POINT('Ctrl Pts',(-5.87262649881128,-3.36091702023246,
16.9297342089157));
#21784=CARTESIAN_POINT('Ctrl Pts',(-5.88500829358621,-3.34453211479069,
16.9407218771897));
#21785=CARTESIAN_POINT('Ctrl Pts',(-5.91370647805049,-3.31273768137677,
16.9581545820566));
#21786=CARTESIAN_POINT('Ctrl Pts',(-5.93003858968362,-3.29738179217064,
16.9646714464042));
#21787=CARTESIAN_POINT('Ctrl Pts',(-5.97963469870635,-3.25750827485252,
16.9788770799768));
#21788=CARTESIAN_POINT('Ctrl Pts',(-6.02067034130286,-3.23386275495577,
16.9829699702649));
#21789=CARTESIAN_POINT('Ctrl Pts',(-6.10890762241377,-3.20261126494113,
16.9867094139313));
#21790=CARTESIAN_POINT('Ctrl Pts',(-6.15609145613325,-3.195,16.9867228248753));
#21791=CARTESIAN_POINT('Ctrl Pts',(-6.2,-3.195,16.9867228248753));
#21792=CARTESIAN_POINT('Origin',(-6.2,-3.6,17.4));
#21793=CARTESIAN_POINT('',(-6.2,-3.145,17.4));
#21794=CARTESIAN_POINT('',(-6.2,-3.145,17.4));
#21795=CARTESIAN_POINT('',(-6.6,-3.38314751557799,17.4));
#21796=CARTESIAN_POINT('Origin',(-6.2,-3.6,17.4));
#21797=CARTESIAN_POINT('',(-6.6,-3.81685248442201,17.4));
#21798=CARTESIAN_POINT('Ctrl Pts',(-6.60000000000001,-3.81685248442201,
17.4));
#21799=CARTESIAN_POINT('Ctrl Pts',(-6.60722705774228,-3.8035216567646,17.4));
#21800=CARTESIAN_POINT('Ctrl Pts',(-6.61371814969366,-3.78968189727386,
17.3998706495795));
#21801=CARTESIAN_POINT('Ctrl Pts',(-6.64208716999993,-3.71948476448862,
17.3989501445254));
#21802=CARTESIAN_POINT('Ctrl Pts',(-6.65268264098811,-3.6576935008072,17.3976826409881));
#21803=CARTESIAN_POINT('Ctrl Pts',(-6.65268264098811,-3.54039232396793,
17.3976826409881));
#21804=CARTESIAN_POINT('Ctrl Pts',(-6.64137663777292,-3.47668030239153,
17.3990538411799));
#21805=CARTESIAN_POINT('Ctrl Pts',(-6.61214628380182,-3.40699633192777,
17.3998996744314));
#21806=CARTESIAN_POINT('Ctrl Pts',(-6.60635819878554,-3.39487567041556,
17.4));
#21807=CARTESIAN_POINT('Ctrl Pts',(-6.6,-3.38314751557799,17.4));
#21808=CARTESIAN_POINT('Origin',(-6.2,-3.6,17.4));
#21809=CARTESIAN_POINT('Origin',(-7.2,0.,17.4));
#21810=CARTESIAN_POINT('',(-6.6,-4.6,17.4));
#21811=CARTESIAN_POINT('',(-6.6,0.,17.4));
#21812=CARTESIAN_POINT('',(6.6,-4.6,17.4));
#21813=CARTESIAN_POINT('',(7.2,-4.6,17.4));
#21814=CARTESIAN_POINT('',(6.6,-3.81685248442201,17.4));
#21815=CARTESIAN_POINT('',(6.6,0.,17.4));
#21816=CARTESIAN_POINT('',(6.2,-3.145,17.4));
#21817=CARTESIAN_POINT('Origin',(6.2,-3.6,17.4));
#21818=CARTESIAN_POINT('',(6.6,-3.38314751557799,17.4));
#21819=CARTESIAN_POINT('Origin',(6.2,-3.6,17.4));
#21820=CARTESIAN_POINT('',(6.6,3.38314751557798,17.4));
#21821=CARTESIAN_POINT('',(6.6,0.,17.4));
#21822=CARTESIAN_POINT('',(6.2,4.055,17.4));
#21823=CARTESIAN_POINT('Origin',(6.2,3.6,17.4));
#21824=CARTESIAN_POINT('',(6.6,3.81685248442202,17.4));
#21825=CARTESIAN_POINT('Origin',(6.2,3.6,17.4));
#21826=CARTESIAN_POINT('',(6.6,0.,17.4));
#21827=CARTESIAN_POINT('',(-6.6,3.81685248442202,17.4));
#21828=CARTESIAN_POINT('',(-6.6,0.,17.4));
#21829=CARTESIAN_POINT('',(-6.2,4.05500000000001,17.4));
#21830=CARTESIAN_POINT('Origin',(-6.2,3.6,17.4));
#21831=CARTESIAN_POINT('',(-6.6,3.38314751557798,17.4));
#21832=CARTESIAN_POINT('Origin',(-6.2,3.6,17.4));
#21833=CARTESIAN_POINT('',(-6.6,0.,17.4));
#21834=CARTESIAN_POINT('',(5.,-2.8,17.4));
#21835=CARTESIAN_POINT('',(-5.,-2.8,17.4));
#21836=CARTESIAN_POINT('',(-1.1,-2.8,17.4));
#21837=CARTESIAN_POINT('',(-5.,-2.4,17.4));
#21838=CARTESIAN_POINT('',(-5.,-1.4,17.4));
#21839=CARTESIAN_POINT('',(5.,-2.4,17.4));
#21840=CARTESIAN_POINT('',(-6.1,-2.4,17.4));
#21841=CARTESIAN_POINT('',(5.,-1.2,17.4));
#21842=CARTESIAN_POINT('',(5.,-1.2,17.4));
#21843=CARTESIAN_POINT('',(-5.,-1.2,17.4));
#21844=CARTESIAN_POINT('',(-1.1,-1.2,17.4));
#21845=CARTESIAN_POINT('',(-5.,-0.8,17.4));
#21846=CARTESIAN_POINT('',(-5.,-0.6,17.4));
#21847=CARTESIAN_POINT('',(5.,-0.8,17.4));
#21848=CARTESIAN_POINT('',(-6.1,-0.8,17.4));
#21849=CARTESIAN_POINT('',(5.,-0.4,17.4));
#21850=CARTESIAN_POINT('',(5.,2.4,17.4));
#21851=CARTESIAN_POINT('',(-5.,2.4,17.4));
#21852=CARTESIAN_POINT('',(-1.1,2.4,17.4));
#21853=CARTESIAN_POINT('',(-5.,2.8,17.4));
#21854=CARTESIAN_POINT('',(-5.,1.2,17.4));
#21855=CARTESIAN_POINT('',(5.,2.8,17.4));
#21856=CARTESIAN_POINT('',(-6.1,2.8,17.4));
#21857=CARTESIAN_POINT('',(5.,1.4,17.4));
#21858=CARTESIAN_POINT('',(5.,1.6,17.4));
#21859=CARTESIAN_POINT('',(-5.,1.6,17.4));
#21860=CARTESIAN_POINT('',(-1.1,1.6,17.4));
#21861=CARTESIAN_POINT('',(-5.,2.,17.4));
#21862=CARTESIAN_POINT('',(-5.,0.8,17.4));
#21863=CARTESIAN_POINT('',(5.,2.,17.4));
#21864=CARTESIAN_POINT('',(-6.1,2.,17.4));
#21865=CARTESIAN_POINT('',(5.,1.,17.4));
#21866=CARTESIAN_POINT('',(5.,0.8,17.4));
#21867=CARTESIAN_POINT('',(-5.,0.8,17.4));
#21868=CARTESIAN_POINT('',(-1.1,0.8,17.4));
#21869=CARTESIAN_POINT('',(-5.,1.2,17.4));
#21870=CARTESIAN_POINT('',(-5.,0.4,17.4));
#21871=CARTESIAN_POINT('',(5.,1.2,17.4));
#21872=CARTESIAN_POINT('',(-6.1,1.2,17.4));
#21873=CARTESIAN_POINT('',(5.,0.6,17.4));
#21874=CARTESIAN_POINT('',(5.,-2.,17.4));
#21875=CARTESIAN_POINT('',(-5.,-2.,17.4));
#21876=CARTESIAN_POINT('',(-1.1,-2.,17.4));
#21877=CARTESIAN_POINT('',(-5.,-1.6,17.4));
#21878=CARTESIAN_POINT('',(-5.,-1.,17.4));
#21879=CARTESIAN_POINT('',(5.,-1.6,17.4));
#21880=CARTESIAN_POINT('',(-6.1,-1.6,17.4));
#21881=CARTESIAN_POINT('',(5.,-0.8,17.4));
#21882=CARTESIAN_POINT('Origin',(-6.2,3.6,16.0783257246469));
#21883=CARTESIAN_POINT('',(-6.2,3.6,15.9566514492938));
#21884=CARTESIAN_POINT('',(-6.2,4.005,16.2));
#21885=CARTESIAN_POINT('',(-6.2,3.8025,16.0783257246469));
#21886=CARTESIAN_POINT('Origin',(-6.2,3.6,16.2));
#21887=CARTESIAN_POINT('Origin',(-6.2,3.6,16.775));
#21888=CARTESIAN_POINT('',(-6.2,4.005,17.35));
#21889=CARTESIAN_POINT('',(-6.2,4.005,16.775));
#21890=CARTESIAN_POINT('Origin',(-6.2,3.6,17.35));
#21891=CARTESIAN_POINT('',(-5.81108355653174,3.487,16.682));
#21892=CARTESIAN_POINT('',(-6.58891644346826,3.487,16.682));
#21893=CARTESIAN_POINT('Ctrl Pts',(-5.81108355653174,3.487,16.682));
#21894=CARTESIAN_POINT('Ctrl Pts',(-5.81108355653174,3.487,16.6370619871072));
#21895=CARTESIAN_POINT('Ctrl Pts',(-5.81372329245509,3.47639022136029,16.5899241279869));
#21896=CARTESIAN_POINT('Ctrl Pts',(-5.82901645085144,3.43610864188054,16.5071507944627));
#21897=CARTESIAN_POINT('Ctrl Pts',(-5.84232258847399,3.40643270490172,16.471639261428));
#21898=CARTESIAN_POINT('Ctrl Pts',(-5.87262649881128,3.36091702023246,16.4342657910843));
#21899=CARTESIAN_POINT('Ctrl Pts',(-5.88500829358621,3.34453211479069,16.4232781228103));
#21900=CARTESIAN_POINT('Ctrl Pts',(-5.91370647805049,3.31273768137677,16.4058454179434));
#21901=CARTESIAN_POINT('Ctrl Pts',(-5.93003858968362,3.29738179217064,16.3993285535958));
#21902=CARTESIAN_POINT('Ctrl Pts',(-5.97963469870635,3.25750827485252,16.3851229200232));
#21903=CARTESIAN_POINT('Ctrl Pts',(-6.02067034130286,3.23386275495577,16.3810300297351));
#21904=CARTESIAN_POINT('Ctrl Pts',(-6.10890762241377,3.20261126494113,16.3772905860687));
#21905=CARTESIAN_POINT('Ctrl Pts',(-6.15609145613325,3.195,16.3772771751247));
#21906=CARTESIAN_POINT('Ctrl Pts',(-6.24390854386675,3.195,16.3772771751247));
#21907=CARTESIAN_POINT('Ctrl Pts',(-6.29109237758623,3.20261126494113,16.3772905860687));
#21908=CARTESIAN_POINT('Ctrl Pts',(-6.37932965869714,3.23386275495577,16.3810300297351));
#21909=CARTESIAN_POINT('Ctrl Pts',(-6.42036530129365,3.25750827485252,16.3851229200232));
#21910=CARTESIAN_POINT('Ctrl Pts',(-6.46996141031638,3.29738179217064,16.3993285535958));
#21911=CARTESIAN_POINT('Ctrl Pts',(-6.48629352194951,3.31273768137677,16.4058454179434));
#21912=CARTESIAN_POINT('Ctrl Pts',(-6.51499170641379,3.34453211479069,16.4232781228103));
#21913=CARTESIAN_POINT('Ctrl Pts',(-6.52737350118872,3.36091702023246,16.4342657910843));
#21914=CARTESIAN_POINT('Ctrl Pts',(-6.55767741152601,3.40643270490172,16.471639261428));
#21915=CARTESIAN_POINT('Ctrl Pts',(-6.57098354914856,3.43610864188054,16.5071507944627));
#21916=CARTESIAN_POINT('Ctrl Pts',(-6.58627670754491,3.47639022136029,16.5899241279869));
#21917=CARTESIAN_POINT('Ctrl Pts',(-6.58891644346826,3.487,16.6370619871072));
#21918=CARTESIAN_POINT('Ctrl Pts',(-6.58891644346826,3.487,16.682));
#21919=CARTESIAN_POINT('Ctrl Pts',(-6.58891644346826,3.487,16.682));
#21920=CARTESIAN_POINT('Ctrl Pts',(-6.58891644346826,3.487,16.7269380128928));
#21921=CARTESIAN_POINT('Ctrl Pts',(-6.58627670754491,3.47639022136029,16.7740758720131));
#21922=CARTESIAN_POINT('Ctrl Pts',(-6.57098354914856,3.43610864188054,16.8568492055373));
#21923=CARTESIAN_POINT('Ctrl Pts',(-6.55767741152601,3.40643270490172,16.892360738572));
#21924=CARTESIAN_POINT('Ctrl Pts',(-6.52737350118872,3.36091702023246,16.9297342089157));
#21925=CARTESIAN_POINT('Ctrl Pts',(-6.51499170641379,3.34453211479069,16.9407218771897));
#21926=CARTESIAN_POINT('Ctrl Pts',(-6.48629352194951,3.31273768137677,16.9581545820566));
#21927=CARTESIAN_POINT('Ctrl Pts',(-6.46996141031638,3.29738179217064,16.9646714464042));
#21928=CARTESIAN_POINT('Ctrl Pts',(-6.42036530129365,3.25750827485252,16.9788770799768));
#21929=CARTESIAN_POINT('Ctrl Pts',(-6.37932965869714,3.23386275495577,16.9829699702649));
#21930=CARTESIAN_POINT('Ctrl Pts',(-6.29109237758623,3.20261126494113,16.9867094139313));
#21931=CARTESIAN_POINT('Ctrl Pts',(-6.24390854386675,3.195,16.9867228248753));
#21932=CARTESIAN_POINT('Ctrl Pts',(-6.15609145613325,3.195,16.9867228248753));
#21933=CARTESIAN_POINT('Ctrl Pts',(-6.10890762241377,3.20261126494113,16.9867094139313));
#21934=CARTESIAN_POINT('Ctrl Pts',(-6.02067034130286,3.23386275495577,16.9829699702649));
#21935=CARTESIAN_POINT('Ctrl Pts',(-5.97963469870635,3.25750827485252,16.9788770799768));
#21936=CARTESIAN_POINT('Ctrl Pts',(-5.93003858968362,3.29738179217064,16.9646714464042));
#21937=CARTESIAN_POINT('Ctrl Pts',(-5.91370647805049,3.31273768137677,16.9581545820566));
#21938=CARTESIAN_POINT('Ctrl Pts',(-5.88500829358621,3.34453211479069,16.9407218771897));
#21939=CARTESIAN_POINT('Ctrl Pts',(-5.87262649881128,3.36091702023246,16.9297342089157));
#21940=CARTESIAN_POINT('Ctrl Pts',(-5.84232258847399,3.40643270490172,16.892360738572));
#21941=CARTESIAN_POINT('Ctrl Pts',(-5.82901645085144,3.43610864188054,16.8568492055373));
#21942=CARTESIAN_POINT('Ctrl Pts',(-5.81372329245509,3.47639022136029,16.7740758720131));
#21943=CARTESIAN_POINT('Ctrl Pts',(-5.81108355653174,3.487,16.7269380128928));
#21944=CARTESIAN_POINT('Ctrl Pts',(-5.81108355653174,3.487,16.682));
#21945=CARTESIAN_POINT('Origin',(-6.2,3.6,17.4));
#21946=CARTESIAN_POINT('',(-6.2,4.055,17.4));
#21947=CARTESIAN_POINT('Ctrl Pts',(-6.6,3.38314751557798,17.4));
#21948=CARTESIAN_POINT('Ctrl Pts',(-6.60635819878554,3.39487567041556,17.4));
#21949=CARTESIAN_POINT('Ctrl Pts',(-6.61214628380182,3.40699633192776,17.3998996744314));
#21950=CARTESIAN_POINT('Ctrl Pts',(-6.64137663777293,3.47668030239153,17.3990538411799));
#21951=CARTESIAN_POINT('Ctrl Pts',(-6.65268264098811,3.54039232396793,17.3976826409881));
#21952=CARTESIAN_POINT('Ctrl Pts',(-6.65268264098811,3.6576935008072,17.3976826409881));
#21953=CARTESIAN_POINT('Ctrl Pts',(-6.64208716999993,3.71948476448862,17.3989501445254));
#21954=CARTESIAN_POINT('Ctrl Pts',(-6.61371814969366,3.78968189727386,17.3998706495795));
#21955=CARTESIAN_POINT('Ctrl Pts',(-6.60722705774228,3.80352165676461,17.4));
#21956=CARTESIAN_POINT('Ctrl Pts',(-6.6,3.81685248442202,17.4));
#21957=CARTESIAN_POINT('Origin',(-6.6,0.,16.8));
#21958=CARTESIAN_POINT('Ctrl Pts',(-7.2,3.51681487422156,16.8));
#21959=CARTESIAN_POINT('Ctrl Pts',(-7.2,3.51609674163657,16.8020376395857));
#21960=CARTESIAN_POINT('Ctrl Pts',(-7.19998961387021,3.5153556448834,16.8040498114376));
#21961=CARTESIAN_POINT('Ctrl Pts',(-7.19977035141354,3.50699129405166,16.8258511124764));
#21962=CARTESIAN_POINT('Ctrl Pts',(-7.19851062225153,3.49591868053171,16.8461520439008));
#21963=CARTESIAN_POINT('Ctrl Pts',(-7.19451004267811,3.46878210020379,16.8830829863768));
#21964=CARTESIAN_POINT('Ctrl Pts',(-7.19181581041583,3.45275112599972,16.8997422622249));
#21965=CARTESIAN_POINT('Ctrl Pts',(-7.1837030970831,3.40350950448746,16.9418791378472));
#21966=CARTESIAN_POINT('Ctrl Pts',(-7.17712501665467,3.36220580742002,16.9648485824245));
#21967=CARTESIAN_POINT('Ctrl Pts',(-7.16767615167579,3.27351018239752,16.9949156250641));
#21968=CARTESIAN_POINT('Ctrl Pts',(-7.16498109471003,3.22608873509771,17.00198109471));
#21969=CARTESIAN_POINT('Ctrl Pts',(-7.16498109471003,3.182,17.00198109471));
#21970=CARTESIAN_POINT('Ctrl Pts',(-7.16498109471003,3.13791126490229,17.00198109471));
#21971=CARTESIAN_POINT('Ctrl Pts',(-7.16767615167579,3.09048981760248,16.9949156250641));
#21972=CARTESIAN_POINT('Ctrl Pts',(-7.17712501665467,3.00179419257998,16.9648485824245));
#21973=CARTESIAN_POINT('Ctrl Pts',(-7.1837030970831,2.96049049551254,16.9418791378472));
#21974=CARTESIAN_POINT('Ctrl Pts',(-7.19181581041583,2.91124887400028,16.8997422622249));
#21975=CARTESIAN_POINT('Ctrl Pts',(-7.19451004267811,2.89521789979621,16.8830829863768));
#21976=CARTESIAN_POINT('Ctrl Pts',(-7.19851062225153,2.86808131946829,16.8461520439008));
#21977=CARTESIAN_POINT('Ctrl Pts',(-7.19977035141354,2.85700870594834,16.8258511124764));
#21978=CARTESIAN_POINT('Ctrl Pts',(-7.19998961387021,2.8486443551166,16.8040498114376));
#21979=CARTESIAN_POINT('Ctrl Pts',(-7.2,2.84790325836343,16.8020376395857));
#21980=CARTESIAN_POINT('Ctrl Pts',(-7.2,2.84718512577844,16.8));
#21981=CARTESIAN_POINT('Ctrl Pts',(-7.2,-2.84718512577844,16.8));
#21982=CARTESIAN_POINT('Ctrl Pts',(-7.2,-2.84790325836343,16.8020376395857));
#21983=CARTESIAN_POINT('Ctrl Pts',(-7.19998961387021,-2.8486443551166,16.8040498114376));
#21984=CARTESIAN_POINT('Ctrl Pts',(-7.19977035141354,-2.85700870594834,
16.8258511124764));
#21985=CARTESIAN_POINT('Ctrl Pts',(-7.19851062225153,-2.86808131946829,
16.8461520439008));
#21986=CARTESIAN_POINT('Ctrl Pts',(-7.19451004267811,-2.89521789979621,
16.8830829863768));
#21987=CARTESIAN_POINT('Ctrl Pts',(-7.19181581041583,-2.91124887400028,
16.8997422622249));
#21988=CARTESIAN_POINT('Ctrl Pts',(-7.1837030970831,-2.96049049551254,16.9418791378472));
#21989=CARTESIAN_POINT('Ctrl Pts',(-7.17712501665467,-3.00179419257999,
16.9648485824245));
#21990=CARTESIAN_POINT('Ctrl Pts',(-7.16767615167579,-3.09048981760248,
16.9949156250641));
#21991=CARTESIAN_POINT('Ctrl Pts',(-7.16498109471003,-3.13791126490229,
17.00198109471));
#21992=CARTESIAN_POINT('Ctrl Pts',(-7.16498109471003,-3.182,17.00198109471));
#21993=CARTESIAN_POINT('Ctrl Pts',(-7.16498109471003,-3.22608873509771,
17.00198109471));
#21994=CARTESIAN_POINT('Ctrl Pts',(-7.16767615167579,-3.27351018239752,
16.9949156250641));
#21995=CARTESIAN_POINT('Ctrl Pts',(-7.17712501665467,-3.36220580742002,
16.9648485824245));
#21996=CARTESIAN_POINT('Ctrl Pts',(-7.1837030970831,-3.40350950448746,16.9418791378472));
#21997=CARTESIAN_POINT('Ctrl Pts',(-7.19181581041583,-3.45275112599972,
16.8997422622249));
#21998=CARTESIAN_POINT('Ctrl Pts',(-7.19451004267811,-3.46878210020379,
16.8830829863768));
#21999=CARTESIAN_POINT('Ctrl Pts',(-7.19851062225153,-3.49591868053171,
16.8461520439008));
#22000=CARTESIAN_POINT('Ctrl Pts',(-7.19977035141354,-3.50699129405166,
16.8258511124764));
#22001=CARTESIAN_POINT('Ctrl Pts',(-7.19998961387021,-3.5153556448834,16.8040498114376));
#22002=CARTESIAN_POINT('Ctrl Pts',(-7.2,-3.51609674163657,16.8020376395857));
#22003=CARTESIAN_POINT('Ctrl Pts',(-7.2,-3.51681487422156,16.8));
#22004=CARTESIAN_POINT('Origin',(-6.6,-4.6,16.8));
#22005=CARTESIAN_POINT('Origin',(6.2,-3.6,16.0783257246469));
#22006=CARTESIAN_POINT('',(6.2,-3.6,15.9566514492938));
#22007=CARTESIAN_POINT('',(6.2,-3.195,16.2));
#22008=CARTESIAN_POINT('',(6.2,-3.3975,16.0783257246469));
#22009=CARTESIAN_POINT('Origin',(6.2,-3.6,16.2));
#22010=CARTESIAN_POINT('Origin',(6.2,-3.6,16.775));
#22011=CARTESIAN_POINT('',(6.2,-3.195,17.35));
#22012=CARTESIAN_POINT('',(6.2,-3.195,16.775));
#22013=CARTESIAN_POINT('Origin',(6.2,-3.6,17.35));
#22014=CARTESIAN_POINT('Origin',(6.2,-3.6,17.4));
#22015=CARTESIAN_POINT('',(6.2,-3.145,17.4));
#22016=CARTESIAN_POINT('Ctrl Pts',(6.6,-3.38314751557799,17.4));
#22017=CARTESIAN_POINT('Ctrl Pts',(6.60635819878554,-3.39487567041556,17.4));
#22018=CARTESIAN_POINT('Ctrl Pts',(6.61214628380182,-3.40699633192777,17.3998996744314));
#22019=CARTESIAN_POINT('Ctrl Pts',(6.64137663777292,-3.47668030239153,17.3990538411799));
#22020=CARTESIAN_POINT('Ctrl Pts',(6.65268264098811,-3.54039232396793,17.3976826409881));
#22021=CARTESIAN_POINT('Ctrl Pts',(6.65268264098811,-3.6576935008072,17.3976826409881));
#22022=CARTESIAN_POINT('Ctrl Pts',(6.64208716999993,-3.71948476448862,17.3989501445254));
#22023=CARTESIAN_POINT('Ctrl Pts',(6.61371814969366,-3.78968189727386,17.3998706495795));
#22024=CARTESIAN_POINT('Ctrl Pts',(6.60722705774228,-3.8035216567646,17.4));
#22025=CARTESIAN_POINT('Ctrl Pts',(6.6,-3.81685248442201,17.4));
#22026=CARTESIAN_POINT('Origin',(6.6,0.,16.8));
#22027=CARTESIAN_POINT('Origin',(6.6,-4.6,16.8));
#22028=CARTESIAN_POINT('Ctrl Pts',(6.6,3.81685248442202,17.4));
#22029=CARTESIAN_POINT('Ctrl Pts',(6.60722705774228,3.80352165676461,17.4));
#22030=CARTESIAN_POINT('Ctrl Pts',(6.61371814969366,3.78968189727386,17.3998706495795));
#22031=CARTESIAN_POINT('Ctrl Pts',(6.64208716999993,3.71948476448862,17.3989501445254));
#22032=CARTESIAN_POINT('Ctrl Pts',(6.65268264098811,3.6576935008072,17.3976826409881));
#22033=CARTESIAN_POINT('Ctrl Pts',(6.65268264098811,3.54039232396793,17.3976826409881));
#22034=CARTESIAN_POINT('Ctrl Pts',(6.64137663777293,3.47668030239153,17.3990538411799));
#22035=CARTESIAN_POINT('Ctrl Pts',(6.61214628380182,3.40699633192776,17.3998996744314));
#22036=CARTESIAN_POINT('Ctrl Pts',(6.60635819878554,3.39487567041556,17.4));
#22037=CARTESIAN_POINT('Ctrl Pts',(6.6,3.38314751557798,17.4));
#22038=CARTESIAN_POINT('Origin',(6.2,3.6,16.0783257246469));
#22039=CARTESIAN_POINT('',(6.2,3.6,15.9566514492938));
#22040=CARTESIAN_POINT('',(6.2,4.005,16.2));
#22041=CARTESIAN_POINT('',(6.2,3.8025,16.0783257246469));
#22042=CARTESIAN_POINT('Origin',(6.2,3.6,16.2));
#22043=CARTESIAN_POINT('Origin',(6.2,3.6,16.775));
#22044=CARTESIAN_POINT('',(6.2,4.005,17.35));
#22045=CARTESIAN_POINT('',(6.2,4.005,16.775));
#22046=CARTESIAN_POINT('Origin',(6.2,3.6,17.35));
#22047=CARTESIAN_POINT('Origin',(6.2,3.6,17.4));
#22048=CARTESIAN_POINT('',(6.2,4.055,17.4));
#22049=CARTESIAN_POINT('Origin',(-4.,4.3083687555983,2.6));
#22050=CARTESIAN_POINT('',(-4.,4.21673751119659,2.6));
#22051=CARTESIAN_POINT('',(-3.695,4.4,2.6));
#22052=CARTESIAN_POINT('',(-3.8475,4.3083687555983,2.6));
#22053=CARTESIAN_POINT('Origin',(-4.,4.4,2.6));
#22054=CARTESIAN_POINT('Origin',(-4.,4.975,2.6));
#22055=CARTESIAN_POINT('',(-3.695,5.55,2.6));
#22056=CARTESIAN_POINT('',(-3.695,4.975,2.6));
#22057=CARTESIAN_POINT('Origin',(-4.,5.55,2.6));
#22058=CARTESIAN_POINT('Origin',(-4.,5.6,2.6));
#22059=CARTESIAN_POINT('',(-3.645,5.6,2.6));
#22060=CARTESIAN_POINT('Origin',(-4.,-2.7083687555983,2.6));
#22061=CARTESIAN_POINT('',(-4.,-2.61673751119659,2.6));
#22062=CARTESIAN_POINT('',(-4.305,-2.8,2.6));
#22063=CARTESIAN_POINT('',(-4.1525,-2.7083687555983,2.6));
#22064=CARTESIAN_POINT('Origin',(-4.,-2.8,2.6));
#22065=CARTESIAN_POINT('Origin',(-4.,-3.675,2.6));
#22066=CARTESIAN_POINT('',(-4.305,-4.55,2.6));
#22067=CARTESIAN_POINT('',(-4.305,-3.675,2.6));
#22068=CARTESIAN_POINT('Origin',(-4.,-4.55,2.6));
#22069=CARTESIAN_POINT('Origin',(-4.,-4.6,2.6));
#22070=CARTESIAN_POINT('',(-4.355,-4.6,2.6));
#22071=CARTESIAN_POINT('',(-4.355,-4.6,2.6));
#22072=CARTESIAN_POINT('Origin',(-4.,-4.6,2.6));
#22073=CARTESIAN_POINT('Origin',(4.,4.3083687555983,2.6));
#22074=CARTESIAN_POINT('',(4.,4.21673751119659,2.6));
#22075=CARTESIAN_POINT('',(4.305,4.4,2.6));
#22076=CARTESIAN_POINT('',(4.1525,4.3083687555983,2.6));
#22077=CARTESIAN_POINT('Origin',(4.,4.4,2.6));
#22078=CARTESIAN_POINT('Origin',(4.,4.975,2.6));
#22079=CARTESIAN_POINT('',(4.305,5.55,2.6));
#22080=CARTESIAN_POINT('',(4.305,4.975,2.6));
#22081=CARTESIAN_POINT('Origin',(4.,5.55,2.6));
#22082=CARTESIAN_POINT('Origin',(4.,5.6,2.6));
#22083=CARTESIAN_POINT('',(4.355,5.6,2.6));
#22084=CARTESIAN_POINT('Origin',(4.,-2.7083687555983,2.6));
#22085=CARTESIAN_POINT('',(4.,-2.61673751119659,2.6));
#22086=CARTESIAN_POINT('',(3.695,-2.8,2.6));
#22087=CARTESIAN_POINT('',(3.8475,-2.7083687555983,2.6));
#22088=CARTESIAN_POINT('Origin',(4.,-2.8,2.6));
#22089=CARTESIAN_POINT('Origin',(4.,-3.675,2.6));
#22090=CARTESIAN_POINT('',(3.695,-4.55,2.6));
#22091=CARTESIAN_POINT('',(3.695,-3.675,2.6));
#22092=CARTESIAN_POINT('Origin',(4.,-4.55,2.6));
#22093=CARTESIAN_POINT('Origin',(4.,-4.6,2.6));
#22094=CARTESIAN_POINT('',(3.645,-4.6,2.6));
#22095=CARTESIAN_POINT('',(3.645,-4.6,2.6));
#22096=CARTESIAN_POINT('Origin',(4.,-4.6,2.6));
#22097=CARTESIAN_POINT('Origin',(-6.,4.3083687555983,8.));
#22098=CARTESIAN_POINT('',(-6.,4.21673751119659,8.));
#22099=CARTESIAN_POINT('',(-5.695,4.4,8.));
#22100=CARTESIAN_POINT('',(-5.8475,4.3083687555983,8.));
#22101=CARTESIAN_POINT('Origin',(-6.,4.4,8.));
#22102=CARTESIAN_POINT('Origin',(-6.,4.975,8.));
#22103=CARTESIAN_POINT('',(-5.695,5.55,8.));
#22104=CARTESIAN_POINT('',(-5.695,4.975,8.));
#22105=CARTESIAN_POINT('Origin',(-6.,5.55,8.));
#22106=CARTESIAN_POINT('Origin',(-6.,5.6,8.));
#22107=CARTESIAN_POINT('',(-5.645,5.6,8.));
#22108=CARTESIAN_POINT('Origin',(-6.,-2.7083687555983,8.));
#22109=CARTESIAN_POINT('',(-6.,-2.61673751119659,8.));
#22110=CARTESIAN_POINT('',(-6.305,-2.8,8.));
#22111=CARTESIAN_POINT('',(-6.1525,-2.7083687555983,8.));
#22112=CARTESIAN_POINT('Origin',(-6.,-2.8,8.));
#22113=CARTESIAN_POINT('Origin',(-6.,-3.675,8.));
#22114=CARTESIAN_POINT('',(-6.305,-4.55,8.));
#22115=CARTESIAN_POINT('',(-6.305,-3.675,8.));
#22116=CARTESIAN_POINT('Origin',(-6.,-4.55,8.));
#22117=CARTESIAN_POINT('Origin',(-6.,-4.6,8.));
#22118=CARTESIAN_POINT('',(-6.355,-4.6,8.));
#22119=CARTESIAN_POINT('',(-6.355,-4.6,8.));
#22120=CARTESIAN_POINT('Origin',(-6.,-4.6,8.));
#22121=CARTESIAN_POINT('Origin',(6.,4.3083687555983,8.));
#22122=CARTESIAN_POINT('',(6.,4.21673751119659,8.));
#22123=CARTESIAN_POINT('',(6.305,4.4,8.));
#22124=CARTESIAN_POINT('',(6.1525,4.3083687555983,8.));
#22125=CARTESIAN_POINT('Origin',(6.,4.4,8.));
#22126=CARTESIAN_POINT('Origin',(6.,4.975,8.));
#22127=CARTESIAN_POINT('',(6.305,5.55,8.));
#22128=CARTESIAN_POINT('',(6.305,4.975,8.));
#22129=CARTESIAN_POINT('Origin',(6.,5.55,8.));
#22130=CARTESIAN_POINT('Origin',(6.,5.6,8.));
#22131=CARTESIAN_POINT('',(6.355,5.6,8.));
#22132=CARTESIAN_POINT('Origin',(6.,-2.7083687555983,8.));
#22133=CARTESIAN_POINT('',(6.,-2.61673751119659,8.));
#22134=CARTESIAN_POINT('',(5.695,-2.8,8.));
#22135=CARTESIAN_POINT('',(5.8475,-2.7083687555983,8.));
#22136=CARTESIAN_POINT('Origin',(6.,-2.8,8.));
#22137=CARTESIAN_POINT('Origin',(6.,-3.675,8.));
#22138=CARTESIAN_POINT('',(5.695,-4.55,8.));
#22139=CARTESIAN_POINT('',(5.695,-3.675,8.));
#22140=CARTESIAN_POINT('Origin',(6.,-4.55,8.));
#22141=CARTESIAN_POINT('Origin',(6.,-4.6,8.));
#22142=CARTESIAN_POINT('',(5.645,-4.6,8.));
#22143=CARTESIAN_POINT('',(5.645,-4.6,8.));
#22144=CARTESIAN_POINT('Origin',(6.,-4.6,8.));
#22145=CARTESIAN_POINT('Origin',(-5.3083687555983,-3.182,10.318));
#22146=CARTESIAN_POINT('',(-5.21673751119659,-3.182,10.318));
#22147=CARTESIAN_POINT('',(-5.4,-2.877,10.318));
#22148=CARTESIAN_POINT('',(-5.3083687555983,-3.0295,10.318));
#22149=CARTESIAN_POINT('Origin',(-5.4,-3.182,10.318));
#22150=CARTESIAN_POINT('Origin',(-6.275,-3.182,10.318));
#22151=CARTESIAN_POINT('',(-7.15,-2.877,10.318));
#22152=CARTESIAN_POINT('',(-6.275,-2.877,10.318));
#22153=CARTESIAN_POINT('Origin',(-7.15,-3.182,10.318));
#22154=CARTESIAN_POINT('Origin',(-7.2,-3.182,10.318));
#22155=CARTESIAN_POINT('',(-7.2,-2.827,10.318));
#22156=CARTESIAN_POINT('Origin',(-5.3083687555983,3.182,10.318));
#22157=CARTESIAN_POINT('',(-5.21673751119659,3.182,10.318));
#22158=CARTESIAN_POINT('',(-5.4,3.487,10.318));
#22159=CARTESIAN_POINT('',(-5.3083687555983,3.3345,10.318));
#22160=CARTESIAN_POINT('Origin',(-5.4,3.182,10.318));
#22161=CARTESIAN_POINT('Origin',(-6.275,3.182,10.318));
#22162=CARTESIAN_POINT('',(-7.15,3.487,10.318));
#22163=CARTESIAN_POINT('',(-6.275,3.487,10.318));
#22164=CARTESIAN_POINT('Origin',(-7.15,3.182,10.318));
#22165=CARTESIAN_POINT('Origin',(-7.2,3.182,10.318));
#22166=CARTESIAN_POINT('',(-7.2,3.537,10.318));
#22167=CARTESIAN_POINT('Origin',(-5.3083687555983,-3.182,16.682));
#22168=CARTESIAN_POINT('',(-5.21673751119659,-3.182,16.682));
#22169=CARTESIAN_POINT('',(-5.4,-2.877,16.682));
#22170=CARTESIAN_POINT('',(-5.3083687555983,-3.0295,16.682));
#22171=CARTESIAN_POINT('Origin',(-5.4,-3.182,16.682));
#22172=CARTESIAN_POINT('Origin',(-6.275,-3.182,16.682));
#22173=CARTESIAN_POINT('',(-7.15,-2.877,16.682));
#22174=CARTESIAN_POINT('',(-6.275,-2.877,16.682));
#22175=CARTESIAN_POINT('Origin',(-7.15,-3.182,16.682));
#22176=CARTESIAN_POINT('Origin',(-7.2,-3.182,16.682));
#22177=CARTESIAN_POINT('',(-7.2,-2.827,16.682));
#22178=CARTESIAN_POINT('Origin',(-5.3083687555983,3.182,16.682));
#22179=CARTESIAN_POINT('',(-5.21673751119659,3.182,16.682));
#22180=CARTESIAN_POINT('',(-5.4,3.487,16.682));
#22181=CARTESIAN_POINT('',(-5.3083687555983,3.3345,16.682));
#22182=CARTESIAN_POINT('Origin',(-5.4,3.182,16.682));
#22183=CARTESIAN_POINT('Origin',(-6.275,3.182,16.682));
#22184=CARTESIAN_POINT('',(-6.275,3.487,16.682));
#22185=CARTESIAN_POINT('',(-7.15,3.487,16.682));
#22186=CARTESIAN_POINT('',(-6.275,3.487,16.682));
#22187=CARTESIAN_POINT('Origin',(-7.15,3.182,16.682));
#22188=CARTESIAN_POINT('Origin',(-7.2,3.182,16.682));
#22189=CARTESIAN_POINT('',(-7.2,3.537,16.682));
#22190=CARTESIAN_POINT('Origin',(-6.,-4.1,0.6375));
#22191=CARTESIAN_POINT('',(-6.,-4.525,1.2));
#22192=CARTESIAN_POINT('Origin',(-6.,-4.1,1.2));
#22193=CARTESIAN_POINT('',(-6.,-4.525,0.025));
#22194=CARTESIAN_POINT('',(-6.,-4.525,0.6375));
#22195=CARTESIAN_POINT('Origin',(-6.,-4.1,0.025));
#22196=CARTESIAN_POINT('Origin',(-6.,-4.1,-0.0125));
#22197=CARTESIAN_POINT('',(-6.,-4.55,0.));
#22198=CARTESIAN_POINT('',(-6.,-4.5625,-0.0125));
#22199=CARTESIAN_POINT('Origin',(-6.,-4.1,0.));
#22200=CARTESIAN_POINT('Origin',(-6.,4.1,0.6375));
#22201=CARTESIAN_POINT('',(-6.,3.675,1.2));
#22202=CARTESIAN_POINT('Origin',(-6.,4.1,1.2));
#22203=CARTESIAN_POINT('',(-6.,3.675,0.025));
#22204=CARTESIAN_POINT('',(-6.,3.675,0.6375));
#22205=CARTESIAN_POINT('Origin',(-6.,4.1,0.025));
#22206=CARTESIAN_POINT('Origin',(-6.,4.1,-0.0125));
#22207=CARTESIAN_POINT('',(-6.,3.65,0.));
#22208=CARTESIAN_POINT('',(-6.,3.6375,-0.0125));
#22209=CARTESIAN_POINT('Origin',(-6.,4.1,0.));
#22210=CARTESIAN_POINT('Origin',(6.,-4.1,0.6375));
#22211=CARTESIAN_POINT('',(6.,-4.525,1.2));
#22212=CARTESIAN_POINT('Origin',(6.,-4.1,1.2));
#22213=CARTESIAN_POINT('',(6.,-4.525,0.025));
#22214=CARTESIAN_POINT('',(6.,-4.525,0.6375));
#22215=CARTESIAN_POINT('Origin',(6.,-4.1,0.025));
#22216=CARTESIAN_POINT('Origin',(6.,-4.1,-0.0125));
#22217=CARTESIAN_POINT('',(6.,-4.55,0.));
#22218=CARTESIAN_POINT('',(6.,-4.5625,-0.0125));
#22219=CARTESIAN_POINT('Origin',(6.,-4.1,0.));
#22220=CARTESIAN_POINT('Origin',(6.,4.1,0.6375));
#22221=CARTESIAN_POINT('',(6.,3.675,1.2));
#22222=CARTESIAN_POINT('Origin',(6.,4.1,1.2));
#22223=CARTESIAN_POINT('',(6.,3.675,0.025));
#22224=CARTESIAN_POINT('',(6.,3.675,0.6375));
#22225=CARTESIAN_POINT('Origin',(6.,4.1,0.025));
#22226=CARTESIAN_POINT('Origin',(6.,4.1,-0.0125));
#22227=CARTESIAN_POINT('',(6.,3.65,0.));
#22228=CARTESIAN_POINT('',(6.,3.6375,-0.0125));
#22229=CARTESIAN_POINT('Origin',(6.,4.1,0.));
#22230=CARTESIAN_POINT('Origin',(4.8,-3.6,3.4));
#22231=CARTESIAN_POINT('',(4.8,-4.6,1.2));
#22232=CARTESIAN_POINT('',(4.8,-4.6,6.05));
#22233=CARTESIAN_POINT('',(4.8,-3.6,1.2));
#22234=CARTESIAN_POINT('Origin',(4.8,-3.6,1.2));
#22235=CARTESIAN_POINT('',(2.4,-4.6,1.2));
#22236=CARTESIAN_POINT('Origin',(-4.8,-3.6,3.4));
#22237=CARTESIAN_POINT('',(-4.8,-4.6,3.4));
#22238=CARTESIAN_POINT('',(-4.8,-3.6,3.4));
#22239=CARTESIAN_POINT('',(-2.4,-4.6,3.4));
#22240=CARTESIAN_POINT('Origin',(-4.8,-3.6,1.2));
#22241=CARTESIAN_POINT('',(-4.8,-4.6,1.2));
#22242=CARTESIAN_POINT('',(-4.8,-4.6,4.95));
#22243=CARTESIAN_POINT('',(-4.8,-3.6,1.2));
#22244=CARTESIAN_POINT('Origin',(-7.3,-3.6,1.2));
#22245=CARTESIAN_POINT('',(-3.65,-4.6,1.2));
#22246=CARTESIAN_POINT('Origin',(0.,-4.6,8.7));
#22247=CARTESIAN_POINT('',(-6.6,-4.6,0.));
#22248=CARTESIAN_POINT('Origin',(-6.6,-4.6,0.6));
#22249=CARTESIAN_POINT('',(-4.,-4.6,0.));
#22250=CARTESIAN_POINT('',(-7.2,-4.6,0.));
#22251=CARTESIAN_POINT('',(-4.,-4.6,0.8));
#22252=CARTESIAN_POINT('',(-4.,-4.6,4.3));
#22253=CARTESIAN_POINT('',(4.,-4.6,0.8));
#22254=CARTESIAN_POINT('',(-2.,-4.6,0.8));
#22255=CARTESIAN_POINT('',(4.,-4.6,0.));
#22256=CARTESIAN_POINT('',(4.,-4.6,4.75));
#22257=CARTESIAN_POINT('',(6.6,-4.6,0.));
#22258=CARTESIAN_POINT('',(-7.2,-4.6,0.));
#22259=CARTESIAN_POINT('Origin',(6.6,-4.6,0.6));
#22260=CARTESIAN_POINT('',(-6.49062803548097E-16,-4.6,1.9));
#22261=CARTESIAN_POINT('Origin',(0.,-4.6,7.2));
#22262=CARTESIAN_POINT('Origin',(7.3,3.6,1.2));
#22263=CARTESIAN_POINT('',(4.8,4.6,1.2));
#22264=CARTESIAN_POINT('',(3.65,4.6,1.2));
#22265=CARTESIAN_POINT('',(4.8,3.6,1.2));
#22266=CARTESIAN_POINT('',(4.8,3.6,1.2));
#22267=CARTESIAN_POINT('',(4.8,3.6,1.2));
#22268=CARTESIAN_POINT('Origin',(6.05,3.6,2.3));
#22269=CARTESIAN_POINT('',(4.8,3.6,3.4));
#22270=CARTESIAN_POINT('',(4.8,3.6,3.4));
#22271=CARTESIAN_POINT('',(7.3,3.6,3.4));
#22272=CARTESIAN_POINT('Origin',(4.8,3.6,1.2));
#22273=CARTESIAN_POINT('',(4.8,3.6,3.4));
#22274=CARTESIAN_POINT('',(4.8,4.6,2.18768943743823));
#22275=CARTESIAN_POINT('',(4.8,4.6,4.95));
#22276=CARTESIAN_POINT('',(4.8,4.6,2.18768943743823));
#22277=CARTESIAN_POINT('Origin',(4.8,3.6,3.4));
#22278=CARTESIAN_POINT('Origin',(-4.8,3.6,3.4));
#22279=CARTESIAN_POINT('',(-4.8,4.6,2.18768943743823));
#22280=CARTESIAN_POINT('',(-4.8,4.6,2.18768943743823));
#22281=CARTESIAN_POINT('',(-4.8,4.6,1.2));
#22282=CARTESIAN_POINT('',(-4.8,4.6,6.05));
#22283=CARTESIAN_POINT('',(-4.8,3.6,1.2));
#22284=CARTESIAN_POINT('',(-4.8,3.6,1.2));
#22285=CARTESIAN_POINT('',(-4.8,3.6,1.2));
#22286=CARTESIAN_POINT('',(-4.8,4.6,3.01231056256177));
#22287=CARTESIAN_POINT('Origin',(-4.8,3.6,1.2));
#22288=CARTESIAN_POINT('',(-2.4,4.6,1.2));
#22289=CARTESIAN_POINT('',(-7.3,3.6,1.2));
#22290=CARTESIAN_POINT('Origin',(-6.05,3.6,2.3));
#22291=CARTESIAN_POINT('Origin',(4.,4.6,2.6));
#22292=CARTESIAN_POINT('',(3.14292474054464,4.6,2.32536933960403));
#22293=CARTESIAN_POINT('Origin',(4.,4.6,2.6));
#22294=CARTESIAN_POINT('',(3.14292474054464,4.6,2.32536933960403));
#22295=CARTESIAN_POINT('Origin',(-4.,4.6,2.6));
#22296=CARTESIAN_POINT('Origin',(-4.,4.6,2.6));
#22297=CARTESIAN_POINT('',(-3.14292474054464,4.6,2.32536933960403));
#22298=CARTESIAN_POINT('',(-3.14292474054464,4.6,2.32536933960403));
#22299=CARTESIAN_POINT('Origin',(-4.,4.6,2.6));
#22300=CARTESIAN_POINT('Origin',(0.,4.6,8.7));
#22301=CARTESIAN_POINT('',(6.6,4.6,0.));
#22302=CARTESIAN_POINT('Origin',(6.6,4.6,0.6));
#22303=CARTESIAN_POINT('',(4.,4.6,0.));
#22304=CARTESIAN_POINT('',(-7.2,4.6,0.));
#22305=CARTESIAN_POINT('',(4.,4.6,0.8));
#22306=CARTESIAN_POINT('',(4.,4.6,4.75));
#22307=CARTESIAN_POINT('',(-4.,4.6,0.8));
#22308=CARTESIAN_POINT('',(-2.,4.6,0.8));
#22309=CARTESIAN_POINT('',(-4.,4.6,0.));
#22310=CARTESIAN_POINT('',(-4.,4.6,4.3));
#22311=CARTESIAN_POINT('',(-6.6,4.6,0.));
#22312=CARTESIAN_POINT('',(-7.2,4.6,0.));
#22313=CARTESIAN_POINT('Origin',(-6.6,4.6,0.6));
#22314=CARTESIAN_POINT('Origin',(0.,4.6,7.2));
#22315=CARTESIAN_POINT('Origin',(-4.,0.,-0.1));
#22316=CARTESIAN_POINT('',(-4.,0.,0.8));
#22317=CARTESIAN_POINT('',(-4.,0.,0.));
#22318=CARTESIAN_POINT('Origin',(4.,0.,0.8));
#22319=CARTESIAN_POINT('',(4.,0.,0.));
#22320=CARTESIAN_POINT('',(4.,0.,0.8));
#22321=CARTESIAN_POINT('Origin',(-4.,0.,0.8));
#22322=CARTESIAN_POINT('Origin',(7.2,0.,0.));
#22323=CARTESIAN_POINT('',(6.6,0.,0.));
#22324=CARTESIAN_POINT('Origin',(7.2,0.,0.));
#22325=CARTESIAN_POINT('',(-6.6,0.,0.));
#22326=CARTESIAN_POINT('Origin',(5.,-2.,17.4));
#22327=CARTESIAN_POINT('',(5.,-2.,16.6));
#22328=CARTESIAN_POINT('',(5.,-2.,17.4));
#22329=CARTESIAN_POINT('',(-5.,-2.,16.6));
#22330=CARTESIAN_POINT('',(-5.,-2.,16.6));
#22331=CARTESIAN_POINT('',(-5.,-2.,17.4));
#22332=CARTESIAN_POINT('Origin',(5.,-1.6,17.4));
#22333=CARTESIAN_POINT('',(5.,-1.6,16.6));
#22334=CARTESIAN_POINT('',(5.,-1.6,17.4));
#22335=CARTESIAN_POINT('',(5.,-2.,16.6));
#22336=CARTESIAN_POINT('Origin',(-5.,-1.6,17.4));
#22337=CARTESIAN_POINT('',(-5.,-1.6,16.6));
#22338=CARTESIAN_POINT('',(-5.,-1.6,17.4));
#22339=CARTESIAN_POINT('',(5.,-1.6,16.6));
#22340=CARTESIAN_POINT('Origin',(-5.,-2.,17.4));
#22341=CARTESIAN_POINT('',(-5.,-1.6,16.6));
#22342=CARTESIAN_POINT('Origin',(0.,-1.8,16.6));
#22343=CARTESIAN_POINT('Origin',(5.,0.8,17.4));
#22344=CARTESIAN_POINT('',(5.,0.8,16.6));
#22345=CARTESIAN_POINT('',(5.,0.8,17.4));
#22346=CARTESIAN_POINT('',(-5.,0.8,16.6));
#22347=CARTESIAN_POINT('',(-5.,0.8,16.6));
#22348=CARTESIAN_POINT('',(-5.,0.8,17.4));
#22349=CARTESIAN_POINT('Origin',(5.,1.2,17.4));
#22350=CARTESIAN_POINT('',(5.,1.2,16.6));
#22351=CARTESIAN_POINT('',(5.,1.2,17.4));
#22352=CARTESIAN_POINT('',(5.,0.8,16.6));
#22353=CARTESIAN_POINT('Origin',(-5.,1.2,17.4));
#22354=CARTESIAN_POINT('',(-5.,1.2,16.6));
#22355=CARTESIAN_POINT('',(-5.,1.2,17.4));
#22356=CARTESIAN_POINT('',(5.,1.2,16.6));
#22357=CARTESIAN_POINT('Origin',(-5.,0.8,17.4));
#22358=CARTESIAN_POINT('',(-5.,1.2,16.6));
#22359=CARTESIAN_POINT('Origin',(0.,1.,16.6));
#22360=CARTESIAN_POINT('Origin',(5.,1.6,17.4));
#22361=CARTESIAN_POINT('',(5.,1.6,16.6));
#22362=CARTESIAN_POINT('',(5.,1.6,17.4));
#22363=CARTESIAN_POINT('',(-5.,1.6,16.6));
#22364=CARTESIAN_POINT('',(-5.,1.6,16.6));
#22365=CARTESIAN_POINT('',(-5.,1.6,17.4));
#22366=CARTESIAN_POINT('Origin',(5.,2.,17.4));
#22367=CARTESIAN_POINT('',(5.,2.,16.6));
#22368=CARTESIAN_POINT('',(5.,2.,17.4));
#22369=CARTESIAN_POINT('',(5.,1.6,16.6));
#22370=CARTESIAN_POINT('Origin',(-5.,2.,17.4));
#22371=CARTESIAN_POINT('',(-5.,2.,16.6));
#22372=CARTESIAN_POINT('',(-5.,2.,17.4));
#22373=CARTESIAN_POINT('',(5.,2.,16.6));
#22374=CARTESIAN_POINT('Origin',(-5.,1.6,17.4));
#22375=CARTESIAN_POINT('',(-5.,2.,16.6));
#22376=CARTESIAN_POINT('Origin',(0.,1.8,16.6));
#22377=CARTESIAN_POINT('Origin',(5.,2.4,17.4));
#22378=CARTESIAN_POINT('',(5.,2.4,16.6));
#22379=CARTESIAN_POINT('',(5.,2.4,17.4));
#22380=CARTESIAN_POINT('',(-5.,2.4,16.6));
#22381=CARTESIAN_POINT('',(-5.,2.4,16.6));
#22382=CARTESIAN_POINT('',(-5.,2.4,17.4));
#22383=CARTESIAN_POINT('Origin',(5.,2.8,17.4));
#22384=CARTESIAN_POINT('',(5.,2.8,16.6));
#22385=CARTESIAN_POINT('',(5.,2.8,17.4));
#22386=CARTESIAN_POINT('',(5.,2.4,16.6));
#22387=CARTESIAN_POINT('Origin',(-5.,2.8,17.4));
#22388=CARTESIAN_POINT('',(-5.,2.8,16.6));
#22389=CARTESIAN_POINT('',(-5.,2.8,17.4));
#22390=CARTESIAN_POINT('',(5.,2.8,16.6));
#22391=CARTESIAN_POINT('Origin',(-5.,2.4,17.4));
#22392=CARTESIAN_POINT('',(-5.,2.8,16.6));
#22393=CARTESIAN_POINT('Origin',(0.,2.6,16.6));
#22394=CARTESIAN_POINT('Origin',(5.,-1.2,17.4));
#22395=CARTESIAN_POINT('',(5.,-1.2,16.6));
#22396=CARTESIAN_POINT('',(5.,-1.2,17.4));
#22397=CARTESIAN_POINT('',(-5.,-1.2,16.6));
#22398=CARTESIAN_POINT('',(-5.,-1.2,16.6));
#22399=CARTESIAN_POINT('',(-5.,-1.2,17.4));
#22400=CARTESIAN_POINT('Origin',(5.,-0.8,17.4));
#22401=CARTESIAN_POINT('',(5.,-0.8,16.6));
#22402=CARTESIAN_POINT('',(5.,-0.8,17.4));
#22403=CARTESIAN_POINT('',(5.,-1.2,16.6));
#22404=CARTESIAN_POINT('Origin',(-5.,-0.8,17.4));
#22405=CARTESIAN_POINT('',(-5.,-0.8,16.6));
#22406=CARTESIAN_POINT('',(-5.,-0.8,17.4));
#22407=CARTESIAN_POINT('',(5.,-0.8,16.6));
#22408=CARTESIAN_POINT('Origin',(-5.,-1.2,17.4));
#22409=CARTESIAN_POINT('',(-5.,-0.8,16.6));
#22410=CARTESIAN_POINT('Origin',(0.,-1.,16.6));
#22411=CARTESIAN_POINT('Origin',(5.,-2.8,17.4));
#22412=CARTESIAN_POINT('',(5.,-2.8,16.6));
#22413=CARTESIAN_POINT('',(5.,-2.8,17.4));
#22414=CARTESIAN_POINT('',(-5.,-2.8,16.6));
#22415=CARTESIAN_POINT('',(-5.,-2.8,16.6));
#22416=CARTESIAN_POINT('',(-5.,-2.8,17.4));
#22417=CARTESIAN_POINT('Origin',(5.,-2.4,17.4));
#22418=CARTESIAN_POINT('',(5.,-2.4,16.6));
#22419=CARTESIAN_POINT('',(5.,-2.4,17.4));
#22420=CARTESIAN_POINT('',(5.,-2.8,16.6));
#22421=CARTESIAN_POINT('Origin',(-5.,-2.4,17.4));
#22422=CARTESIAN_POINT('',(-5.,-2.4,16.6));
#22423=CARTESIAN_POINT('',(-5.,-2.4,17.4));
#22424=CARTESIAN_POINT('',(5.,-2.4,16.6));
#22425=CARTESIAN_POINT('Origin',(-5.,-2.8,17.4));
#22426=CARTESIAN_POINT('',(-5.,-2.4,16.6));
#22427=CARTESIAN_POINT('Origin',(0.,-2.6,16.6));
#22428=CARTESIAN_POINT('Origin',(6.5575,0.,13.5));
#22429=CARTESIAN_POINT('',(5.915,-3.18408167778312E-16,10.9));
#22430=CARTESIAN_POINT('',(6.5575,-3.18408167778312E-16,10.9));
#22431=CARTESIAN_POINT('Origin',(5.915,0.,13.5));
#22432=CARTESIAN_POINT('Origin',(5.915,0.,16.25));
#22433=CARTESIAN_POINT('',(5.915,-3.36777869765522E-16,10.75));
#22434=CARTESIAN_POINT('Origin',(5.915,0.,13.5));
#22435=CARTESIAN_POINT('Origin',(5.8075,0.,13.5));
#22436=CARTESIAN_POINT('',(5.7,-3.36777869765522E-16,10.75));
#22437=CARTESIAN_POINT('',(5.8075,-3.36777869765522E-16,10.75));
#22438=CARTESIAN_POINT('Origin',(5.7,0.,13.5));
#22439=CARTESIAN_POINT('Origin',(5.7,0.,16.1));
#22440=CARTESIAN_POINT('',(5.7,-3.18408167778312E-16,10.9));
#22441=CARTESIAN_POINT('Origin',(5.7,0.,13.5));
#22442=CARTESIAN_POINT('Origin',(5.05,0.,13.5));
#22443=CARTESIAN_POINT('',(4.4,-3.18408167778312E-16,10.9));
#22444=CARTESIAN_POINT('',(5.05,-3.18408167778312E-16,10.9));
#22445=CARTESIAN_POINT('Origin',(4.4,0.,13.5));
#22446=CARTESIAN_POINT('Origin',(4.4,0.,15.8));
#22447=CARTESIAN_POINT('',(4.4,-2.81668763803891E-16,11.2));
#22448=CARTESIAN_POINT('Origin',(4.4,0.,13.5));
#22449=CARTESIAN_POINT('Origin',(0.,0.,13.5));
#22450=CARTESIAN_POINT('',(3.47706773014274,-1.40834381901946E-16,11.2));
#22451=CARTESIAN_POINT('',(0.,-2.81668763803891E-16,11.2));
#22452=CARTESIAN_POINT('',(1.66533453693773E-16,-2.0712315177208,12.5));
#22453=CARTESIAN_POINT('Ctrl Pts',(0.,-2.0712315177208,12.5));
#22454=CARTESIAN_POINT('Ctrl Pts',(0.29627842792801,-2.0712315177208,12.5));
#22455=CARTESIAN_POINT('Ctrl Pts',(0.601922961286425,-2.05958767676481,
12.4745443794946));
#22456=CARTESIAN_POINT('Ctrl Pts',(1.20334931546476,-2.00447274662769,12.3705976495442));
#22457=CARTESIAN_POINT('Ctrl Pts',(1.49912274563406,-1.96094879925114,12.292086027079));
#22458=CARTESIAN_POINT('Ctrl Pts',(2.05395568676163,-1.82468777995446,12.0946869078541));
#22459=CARTESIAN_POINT('Ctrl Pts',(2.31304412039431,-1.73185180887424,11.9758067799491));
#22460=CARTESIAN_POINT('Ctrl Pts',(2.77233292995656,-1.47332713087679,11.7246738665425));
#22461=CARTESIAN_POINT('Ctrl Pts',(2.97292007577089,-1.30853389661232,11.5922075947285));
#22462=CARTESIAN_POINT('Ctrl Pts',(3.18569785359246,-1.01845799849145,11.4362114294288));
#22463=CARTESIAN_POINT('Ctrl Pts',(3.23470613609049,-0.939780894043197,
11.398772551631));
#22464=CARTESIAN_POINT('Ctrl Pts',(3.32099876549632,-0.770171936350533,
11.3308572866818));
#22465=CARTESIAN_POINT('Ctrl Pts',(3.35829264222579,-0.679232393641301,
11.300412215585));
#22466=CARTESIAN_POINT('Ctrl Pts',(3.41804439766507,-0.490271405037467,
11.2507383977881));
#22467=CARTESIAN_POINT('Ctrl Pts',(3.44056498067965,-0.392091297884813,
11.2314874762236));
#22468=CARTESIAN_POINT('Ctrl Pts',(3.47007525605945,-0.19487349905874,11.2061148726341));
#22469=CARTESIAN_POINT('Ctrl Pts',(3.47706773014274,-0.0958353476442229,
11.2));
#22470=CARTESIAN_POINT('Ctrl Pts',(3.47706773014274,-2.77555756156289E-17,
11.2));
#22471=CARTESIAN_POINT('',(-3.47706773014274,-1.40834381901946E-16,11.2));
#22472=CARTESIAN_POINT('Ctrl Pts',(-3.47706773014274,0.,11.2));
#22473=CARTESIAN_POINT('Ctrl Pts',(-3.47706773014274,-0.0958353476442226,
11.2));
#22474=CARTESIAN_POINT('Ctrl Pts',(-3.47007525605945,-0.194873499058739,
11.2061148726341));
#22475=CARTESIAN_POINT('Ctrl Pts',(-3.44056498067966,-0.392091297884812,
11.2314874762236));
#22476=CARTESIAN_POINT('Ctrl Pts',(-3.41804439766507,-0.490271405037466,
11.2507383977881));
#22477=CARTESIAN_POINT('Ctrl Pts',(-3.35829264222578,-0.679232393641301,
11.300412215585));
#22478=CARTESIAN_POINT('Ctrl Pts',(-3.32099876549632,-0.770171936350533,
11.3308572866818));
#22479=CARTESIAN_POINT('Ctrl Pts',(-3.23470613609049,-0.939780894043197,
11.398772551631));
#22480=CARTESIAN_POINT('Ctrl Pts',(-3.18569785359246,-1.01845799849145,
11.4362114294288));
#22481=CARTESIAN_POINT('Ctrl Pts',(-2.97292007577089,-1.30853389661232,
11.5922075947285));
#22482=CARTESIAN_POINT('Ctrl Pts',(-2.77233292995656,-1.47332713087679,
11.7246738665425));
#22483=CARTESIAN_POINT('Ctrl Pts',(-2.31304412039431,-1.73185180887424,
11.9758067799491));
#22484=CARTESIAN_POINT('Ctrl Pts',(-2.05395568676163,-1.82468777995446,
12.0946869078541));
#22485=CARTESIAN_POINT('Ctrl Pts',(-1.49912274563406,-1.96094879925114,
12.292086027079));
#22486=CARTESIAN_POINT('Ctrl Pts',(-1.20334931546476,-2.00447274662769,
12.3705976495442));
#22487=CARTESIAN_POINT('Ctrl Pts',(-0.601922961286425,-2.05958767676481,
12.4745443794946));
#22488=CARTESIAN_POINT('Ctrl Pts',(-0.29627842792801,-2.0712315177208,12.5));
#22489=CARTESIAN_POINT('Ctrl Pts',(0.,-2.0712315177208,12.5));
#22490=CARTESIAN_POINT('',(-4.4,-2.81668763803891E-16,11.2));
#22491=CARTESIAN_POINT('',(0.,-2.81668763803891E-16,11.2));
#22492=CARTESIAN_POINT('Origin',(-4.4,0.,13.5));
#22493=CARTESIAN_POINT('Ctrl Pts',(3.47706773014274,-5.55111512312578E-17,
11.2));
#22494=CARTESIAN_POINT('Ctrl Pts',(3.47706773014274,0.0958353476442228,
11.2));
#22495=CARTESIAN_POINT('Ctrl Pts',(3.47007525605945,0.194873499058739,11.2061148726341));
#22496=CARTESIAN_POINT('Ctrl Pts',(3.44056498067965,0.392091297884812,11.2314874762236));
#22497=CARTESIAN_POINT('Ctrl Pts',(3.41804439766507,0.490271405037467,11.2507383977881));
#22498=CARTESIAN_POINT('Ctrl Pts',(3.35829264222579,0.679232393641301,11.300412215585));
#22499=CARTESIAN_POINT('Ctrl Pts',(3.32099876549632,0.770171936350533,11.3308572866818));
#22500=CARTESIAN_POINT('Ctrl Pts',(3.23470613609049,0.939780894043197,11.398772551631));
#22501=CARTESIAN_POINT('Ctrl Pts',(3.18569785359246,1.01845799849145,11.4362114294288));
#22502=CARTESIAN_POINT('Ctrl Pts',(2.97292007577089,1.30853389661232,11.5922075947285));
#22503=CARTESIAN_POINT('Ctrl Pts',(2.77233292995656,1.47332713087679,11.7246738665425));
#22504=CARTESIAN_POINT('Ctrl Pts',(2.31304412039431,1.73185180887424,11.9758067799491));
#22505=CARTESIAN_POINT('Ctrl Pts',(2.05395568676163,1.82468777995446,12.0946869078541));
#22506=CARTESIAN_POINT('Ctrl Pts',(1.49912274563406,1.96094879925114,12.292086027079));
#22507=CARTESIAN_POINT('Ctrl Pts',(1.20334931546476,2.00447274662769,12.3705976495442));
#22508=CARTESIAN_POINT('Ctrl Pts',(0.601922961286424,2.05958767676481,12.4745443794946));
#22509=CARTESIAN_POINT('Ctrl Pts',(0.29627842792801,2.0712315177208,12.5));
#22510=CARTESIAN_POINT('Ctrl Pts',(0.,2.0712315177208,12.5));
#22511=CARTESIAN_POINT('Ctrl Pts',(-0.29627842792801,2.0712315177208,12.5));
#22512=CARTESIAN_POINT('Ctrl Pts',(-0.601922961286424,2.05958767676481,
12.4745443794946));
#22513=CARTESIAN_POINT('Ctrl Pts',(-1.20334931546475,2.00447274662769,12.3705976495442));
#22514=CARTESIAN_POINT('Ctrl Pts',(-1.49912274563406,1.96094879925114,12.292086027079));
#22515=CARTESIAN_POINT('Ctrl Pts',(-2.05395568676163,1.82468777995446,12.0946869078541));
#22516=CARTESIAN_POINT('Ctrl Pts',(-2.31304412039431,1.73185180887424,11.9758067799491));
#22517=CARTESIAN_POINT('Ctrl Pts',(-2.77233292995656,1.47332713087679,11.7246738665425));
#22518=CARTESIAN_POINT('Ctrl Pts',(-2.97292007577089,1.30853389661232,11.5922075947285));
#22519=CARTESIAN_POINT('Ctrl Pts',(-3.18569785359246,1.01845799849145,11.4362114294288));
#22520=CARTESIAN_POINT('Ctrl Pts',(-3.23470613609049,0.939780894043197,
11.398772551631));
#22521=CARTESIAN_POINT('Ctrl Pts',(-3.32099876549632,0.770171936350533,
11.3308572866818));
#22522=CARTESIAN_POINT('Ctrl Pts',(-3.35829264222578,0.679232393641301,
11.300412215585));
#22523=CARTESIAN_POINT('Ctrl Pts',(-3.41804439766507,0.490271405037466,
11.2507383977881));
#22524=CARTESIAN_POINT('Ctrl Pts',(-3.44056498067966,0.392091297884812,
11.2314874762236));
#22525=CARTESIAN_POINT('Ctrl Pts',(-3.47007525605945,0.194873499058739,
11.2061148726341));
#22526=CARTESIAN_POINT('Ctrl Pts',(-3.47706773014274,0.0958353476442226,
11.2));
#22527=CARTESIAN_POINT('Ctrl Pts',(-3.47706773014274,2.77555756156289E-17,
11.2));
#22528=CARTESIAN_POINT('Origin',(-4.4,0.,16.1));
#22529=CARTESIAN_POINT('',(-4.4,-3.18408167778312E-16,10.9));
#22530=CARTESIAN_POINT('Origin',(-4.4,0.,13.5));
#22531=CARTESIAN_POINT('Origin',(-5.05,0.,13.5));
#22532=CARTESIAN_POINT('',(-5.7,-3.18408167778312E-16,10.9));
#22533=CARTESIAN_POINT('',(-5.05,-3.18408167778312E-16,10.9));
#22534=CARTESIAN_POINT('Origin',(-5.7,0.,13.5));
#22535=CARTESIAN_POINT('Origin',(-5.7,0.,16.25));
#22536=CARTESIAN_POINT('',(-5.7,-3.36777869765522E-16,10.75));
#22537=CARTESIAN_POINT('Origin',(-5.7,0.,13.5));
#22538=CARTESIAN_POINT('Origin',(-5.8075,0.,13.5));
#22539=CARTESIAN_POINT('',(-5.915,-3.36777869765522E-16,10.75));
#22540=CARTESIAN_POINT('',(-5.8075,-3.36777869765522E-16,10.75));
#22541=CARTESIAN_POINT('Origin',(-5.915,0.,13.5));
#22542=CARTESIAN_POINT('Origin',(-5.915,0.,16.1));
#22543=CARTESIAN_POINT('',(-5.915,-3.18408167778312E-16,10.9));
#22544=CARTESIAN_POINT('Origin',(-5.915,0.,13.5));
#22545=CARTESIAN_POINT('Origin',(-6.5575,0.,13.5));
#22546=CARTESIAN_POINT('',(-6.5575,-3.18408167778312E-16,10.9));
#22547=CARTESIAN_POINT('Origin',(0.,-1.25,7.2));
#22548=CARTESIAN_POINT('',(-6.49062803548097E-16,2.2,1.9));
#22549=CARTESIAN_POINT('',(-6.49062803548097E-16,-1.25,1.9));
#22550=CARTESIAN_POINT('Origin',(0.,2.2,7.2));
#22551=CARTESIAN_POINT('Origin',(0.,2.2,10.95));
#22552=CARTESIAN_POINT('',(-4.59242549680257E-16,2.2,3.45));
#22553=CARTESIAN_POINT('Origin',(0.,2.2,7.2));
#22554=CARTESIAN_POINT('Origin',(0.,3.5,7.2));
#22555=CARTESIAN_POINT('',(-4.59242549680257E-16,4.8,3.45));
#22556=CARTESIAN_POINT('',(-4.59242549680257E-16,3.5,3.45));
#22557=CARTESIAN_POINT('Origin',(0.,4.8,7.2));
#22558=CARTESIAN_POINT('Origin',(0.,4.8,10.3));
#22559=CARTESIAN_POINT('',(-3.7964050773568E-16,4.8,4.1));
#22560=CARTESIAN_POINT('Origin',(0.,4.8,7.2));
#22561=CARTESIAN_POINT('Origin',(0.,5.175,7.2));
#22562=CARTESIAN_POINT('',(-3.7964050773568E-16,5.55,4.1));
#22563=CARTESIAN_POINT('',(-3.79640507735679E-16,5.175,4.1));
#22564=CARTESIAN_POINT('Origin',(0.,5.55,7.2));
#22565=CARTESIAN_POINT('Origin',(0.,5.605,7.2));
#22566=CARTESIAN_POINT('',(-3.8637606513099E-16,5.605,4.045));
#22567=CARTESIAN_POINT('Origin',(0.,4.6,7.2));
#22568=CARTESIAN_POINT('Origin',(6.6,0.,0.6));
#22569=CARTESIAN_POINT('Origin',(-6.6,0.,0.6));
#22570=CARTESIAN_POINT('',(0.,0.,0.));
#22571=CARTESIAN_POINT('Origin',(0.,-2.45,7.2));
#22572=CARTESIAN_POINT('',(-5.295,-2.5,7.2));
#22573=CARTESIAN_POINT('Origin',(0.,-2.5,7.2));
#22574=CARTESIAN_POINT('',(-5.195,-2.4,7.2));
#22575=CARTESIAN_POINT('',(-5.245,-2.45,7.2));
#22576=CARTESIAN_POINT('Origin',(0.,-2.4,7.2));
#22577=CARTESIAN_POINT('Origin',(0.,-4.6,7.2));
#22578=CARTESIAN_POINT('',(-5.295,-4.6,7.2));
#22579=CARTESIAN_POINT('',(-5.295,-4.6,7.2));
#22580=CARTESIAN_POINT('Origin',(0.,-4.6,7.2));
#22581=CARTESIAN_POINT('Origin',(0.,-2.4,7.2));
#22582=CARTESIAN_POINT('',(4.59242549680257E-16,-2.4,3.45));
#22583=CARTESIAN_POINT('Origin',(0.,-2.4,7.2));
#22584=CARTESIAN_POINT('Origin',(0.,-5.55,7.2));
#22585=CARTESIAN_POINT('',(-5.51591157610535,-5.6,8.63691317920985));
#22586=CARTESIAN_POINT('',(5.51591157610535,-5.6,8.63691317920985));
#22587=CARTESIAN_POINT('Origin',(0.,-5.6,7.2));
#22588=CARTESIAN_POINT('',(5.57660788571496,-5.5,8.79419085713778));
#22589=CARTESIAN_POINT('Ctrl Pts',(5.51591157610535,-5.6,8.63691317920985));
#22590=CARTESIAN_POINT('Ctrl Pts',(5.53455522536305,-5.56837145414589,8.69081065313349));
#22591=CARTESIAN_POINT('Ctrl Pts',(5.55504723137092,-5.53469693041622,8.74337706591871));
#22592=CARTESIAN_POINT('Ctrl Pts',(5.57660788571496,-5.5,8.79419085713778));
#22593=CARTESIAN_POINT('',(-5.57660788571496,-5.5,8.79419085713778));
#22594=CARTESIAN_POINT('Origin',(0.,-5.5,7.2));
#22595=CARTESIAN_POINT('Ctrl Pts',(-5.51591157610535,-5.6,8.63691317920985));
#22596=CARTESIAN_POINT('Ctrl Pts',(-5.53455522536305,-5.56837145414589,
8.6908106531335));
#22597=CARTESIAN_POINT('Ctrl Pts',(-5.55504723137093,-5.53469693041621,
8.74337706591873));
#22598=CARTESIAN_POINT('Ctrl Pts',(-5.57660788571496,-5.5,8.79419085713778));
#22599=CARTESIAN_POINT('Origin',(6.,-5.55,8.));
#22600=CARTESIAN_POINT('',(5.69969977760644,-5.6,7.25850166795172));
#22601=CARTESIAN_POINT('Origin',(6.,-5.6,8.));
#22602=CARTESIAN_POINT('',(5.79948381734181,-5.5,7.12262136993645));
#22603=CARTESIAN_POINT('Ctrl Pts',(5.69969977760644,-5.6,7.25850166795172));
#22604=CARTESIAN_POINT('Ctrl Pts',(5.73181372922814,-5.56837145414589,7.21137187414533));
#22605=CARTESIAN_POINT('Ctrl Pts',(5.76536271654192,-5.53469693041621,7.16601092713632));
#22606=CARTESIAN_POINT('Ctrl Pts',(5.79948381734181,-5.5,7.12262136993645));
#22607=CARTESIAN_POINT('Origin',(6.,-5.5,8.));
#22608=CARTESIAN_POINT('Origin',(0.,-5.55,7.2));
#22609=CARTESIAN_POINT('',(4.22058574132406,-5.6,3.36898760115136));
#22610=CARTESIAN_POINT('Origin',(0.,-5.6,7.2));
#22611=CARTESIAN_POINT('',(4.39098268679659,-5.5,3.41063711895356));
#22612=CARTESIAN_POINT('Ctrl Pts',(4.22058574132406,-5.6,3.36898760115136));
#22613=CARTESIAN_POINT('Ctrl Pts',(4.27772143963444,-5.56861968092285,3.38524395544776));
#22614=CARTESIAN_POINT('Ctrl Pts',(4.33480274427804,-5.53491157572283,3.39897341264218));
#22615=CARTESIAN_POINT('Ctrl Pts',(4.39098268679659,-5.5,3.41063711895356));
#22616=CARTESIAN_POINT('Origin',(0.,-5.5,7.2));
#22617=CARTESIAN_POINT('Origin',(4.,-5.55,2.6));
#22618=CARTESIAN_POINT('',(3.20783191206668,-5.6,2.48833209744929));
#22619=CARTESIAN_POINT('Origin',(4.,-5.6,2.6));
#22620=CARTESIAN_POINT('',(3.14292474054464,-5.5,2.32536933960403));
#22621=CARTESIAN_POINT('Ctrl Pts',(3.20783191206668,-5.6,2.48833209744929));
#22622=CARTESIAN_POINT('Ctrl Pts',(3.18379924141574,-5.56861968092285,2.43400726134454));
#22623=CARTESIAN_POINT('Ctrl Pts',(3.16227654075062,-5.53491157572284,2.37938540957487));
#22624=CARTESIAN_POINT('Ctrl Pts',(3.14292474054464,-5.5,2.32536933960403));
#22625=CARTESIAN_POINT('Origin',(4.,-5.5,2.6));
#22626=CARTESIAN_POINT('Origin',(0.,-5.55,7.2));
#22627=CARTESIAN_POINT('',(-3.20783191206668,-5.6,2.48833209744929));
#22628=CARTESIAN_POINT('Origin',(0.,-5.6,7.2));
#22629=CARTESIAN_POINT('',(-3.14292474054464,-5.5,2.32536933960403));
#22630=CARTESIAN_POINT('Ctrl Pts',(-3.20783191206668,-5.6,2.48833209744929));
#22631=CARTESIAN_POINT('Ctrl Pts',(-3.18379924141574,-5.56861968092285,
2.43400726134455));
#22632=CARTESIAN_POINT('Ctrl Pts',(-3.16227654075063,-5.53491157572285,
2.37938540957488));
#22633=CARTESIAN_POINT('Ctrl Pts',(-3.14292474054464,-5.5,2.32536933960403));
#22634=CARTESIAN_POINT('Origin',(0.,-5.5,7.2));
#22635=CARTESIAN_POINT('Origin',(-4.,-5.55,2.6));
#22636=CARTESIAN_POINT('',(-4.39098268679659,-5.5,3.41063711895356));
#22637=CARTESIAN_POINT('Origin',(-4.,-5.5,2.6));
#22638=CARTESIAN_POINT('',(-4.22058574132406,-5.6,3.36898760115135));
#22639=CARTESIAN_POINT('Origin',(-4.,-5.6,2.6));
#22640=CARTESIAN_POINT('Ctrl Pts',(-4.22058574132406,-5.6,3.36898760115136));
#22641=CARTESIAN_POINT('Ctrl Pts',(-4.27772143963443,-5.56861968092285,
3.38524395544776));
#22642=CARTESIAN_POINT('Ctrl Pts',(-4.33480274427803,-5.53491157572284,
3.39897341264218));
#22643=CARTESIAN_POINT('Ctrl Pts',(-4.39098268679659,-5.5,3.41063711895356));
#22644=CARTESIAN_POINT('Origin',(0.,-5.55,7.2));
#22645=CARTESIAN_POINT('',(-5.79948381734181,-5.5,7.12262136993645));
#22646=CARTESIAN_POINT('Origin',(0.,-5.5,7.2));
#22647=CARTESIAN_POINT('',(-5.69969977760644,-5.6,7.25850166795172));
#22648=CARTESIAN_POINT('Origin',(0.,-5.6,7.2));
#22649=CARTESIAN_POINT('Ctrl Pts',(-5.69969977760644,-5.6,7.25850166795172));
#22650=CARTESIAN_POINT('Ctrl Pts',(-5.73181372922814,-5.56837145414589,
7.21137187414533));
#22651=CARTESIAN_POINT('Ctrl Pts',(-5.76536271654191,-5.53469693041622,
7.16601092713633));
#22652=CARTESIAN_POINT('Ctrl Pts',(-5.79948381734181,-5.5,7.12262136993645));
#22653=CARTESIAN_POINT('Origin',(-6.,-5.55,8.));
#22654=CARTESIAN_POINT('Origin',(-6.,-5.5,8.));
#22655=CARTESIAN_POINT('Origin',(-6.,-5.6,8.));
#22656=CARTESIAN_POINT('Origin',(-4.,-4.6,2.6));
#22657=CARTESIAN_POINT('',(-4.39098268679659,-4.6,3.41063711895356));
#22658=CARTESIAN_POINT('',(-4.39098268679659,-4.6,3.41063711895356));
#22659=CARTESIAN_POINT('',(-3.14292474054464,-4.6,2.32536933960403));
#22660=CARTESIAN_POINT('Origin',(-4.,-4.6,2.6));
#22661=CARTESIAN_POINT('',(-3.14292474054464,-4.6,2.32536933960403));
#22662=CARTESIAN_POINT('Origin',(0.,-4.6,7.2));
#22663=CARTESIAN_POINT('',(-5.79948381734181,-4.6,7.12262136993645));
#22664=CARTESIAN_POINT('',(-5.79948381734181,-4.6,7.12262136993645));
#22665=CARTESIAN_POINT('Origin',(0.,-4.6,7.2));
#22666=CARTESIAN_POINT('Origin',(-6.,-4.6,8.));
#22667=CARTESIAN_POINT('',(-5.57660788571496,-4.6,8.79419085713778));
#22668=CARTESIAN_POINT('',(-5.57660788571496,-4.6,8.79419085713778));
#22669=CARTESIAN_POINT('Origin',(-6.,-4.6,8.));
#22670=CARTESIAN_POINT('Origin',(0.,-4.6,7.2));
#22671=CARTESIAN_POINT('',(5.57660788571496,-4.6,8.79419085713778));
#22672=CARTESIAN_POINT('',(5.57660788571496,-4.6,8.79419085713778));
#22673=CARTESIAN_POINT('Origin',(0.,-4.6,7.2));
#22674=CARTESIAN_POINT('Origin',(0.,-5.6,7.2));
#22675=CARTESIAN_POINT('',(-3.85763741731416E-16,-5.6,4.05));
#22676=CARTESIAN_POINT('Origin',(0.,-5.6,7.2));
#22677=CARTESIAN_POINT('',(5.45,-5.6,8.));
#22678=CARTESIAN_POINT('Origin',(6.,-5.6,8.));
#22679=CARTESIAN_POINT('',(-6.55,-5.6,8.));
#22680=CARTESIAN_POINT('Origin',(-6.,-5.6,8.));
#22681=CARTESIAN_POINT('',(3.45,-5.6,2.6));
#22682=CARTESIAN_POINT('Origin',(4.,-5.6,2.6));
#22683=CARTESIAN_POINT('',(-4.55,-5.6,2.6));
#22684=CARTESIAN_POINT('Origin',(-4.,-5.6,2.6));
#22685=CARTESIAN_POINT('Origin',(-4.,-4.5875,2.6));
#22686=CARTESIAN_POINT('',(-4.33,-4.625,2.6));
#22687=CARTESIAN_POINT('Origin',(-4.,-4.625,2.6));
#22688=CARTESIAN_POINT('',(-4.33833333333333,-4.6,2.6));
#22689=CARTESIAN_POINT('',(-4.3425,-4.5875,2.6));
#22690=CARTESIAN_POINT('Origin',(-4.,-4.6,2.6));
#22691=CARTESIAN_POINT('Origin',(-4.,-4.775,2.6));
#22692=CARTESIAN_POINT('',(-4.33,-4.925,2.6));
#22693=CARTESIAN_POINT('',(-4.33,-4.775,2.6));
#22694=CARTESIAN_POINT('Origin',(-4.,-4.925,2.6));
#22695=CARTESIAN_POINT('Origin',(-4.,-4.9375,2.6));
#22696=CARTESIAN_POINT('',(-4.355,-4.95,2.6));
#22697=CARTESIAN_POINT('',(-4.3425,-4.9375,2.6));
#22698=CARTESIAN_POINT('Origin',(-4.,-4.95,2.6));
#22699=CARTESIAN_POINT('Origin',(-3.45,-4.95,2.6));
#22700=CARTESIAN_POINT('',(-4.55,-4.95,2.6));
#22701=CARTESIAN_POINT('Origin',(-4.,-4.95,2.6));
#22702=CARTESIAN_POINT('Origin',(-4.,-5.275,2.6));
#22703=CARTESIAN_POINT('',(-4.55,-5.275,2.6));
#22704=CARTESIAN_POINT('Origin',(4.,-4.5875,2.6));
#22705=CARTESIAN_POINT('',(3.67,-4.625,2.6));
#22706=CARTESIAN_POINT('Origin',(4.,-4.625,2.6));
#22707=CARTESIAN_POINT('',(3.66166666666667,-4.6,2.6));
#22708=CARTESIAN_POINT('',(3.6575,-4.5875,2.6));
#22709=CARTESIAN_POINT('Origin',(4.,-4.6,2.6));
#22710=CARTESIAN_POINT('Origin',(4.,-4.775,2.6));
#22711=CARTESIAN_POINT('',(3.67,-4.925,2.6));
#22712=CARTESIAN_POINT('',(3.67,-4.775,2.6));
#22713=CARTESIAN_POINT('Origin',(4.,-4.925,2.6));
#22714=CARTESIAN_POINT('Origin',(4.,-4.9375,2.6));
#22715=CARTESIAN_POINT('',(3.645,-4.95,2.6));
#22716=CARTESIAN_POINT('',(3.6575,-4.9375,2.6));
#22717=CARTESIAN_POINT('Origin',(4.,-4.95,2.6));
#22718=CARTESIAN_POINT('Origin',(4.55,-4.95,2.6));
#22719=CARTESIAN_POINT('',(3.45,-4.95,2.6));
#22720=CARTESIAN_POINT('Origin',(4.,-4.95,2.6));
#22721=CARTESIAN_POINT('Origin',(4.,-5.275,2.6));
#22722=CARTESIAN_POINT('',(3.45,-5.275,2.6));
#22723=CARTESIAN_POINT('Origin',(-6.,-4.5875,8.));
#22724=CARTESIAN_POINT('',(-6.33,-4.625,8.));
#22725=CARTESIAN_POINT('Origin',(-6.,-4.625,8.));
#22726=CARTESIAN_POINT('',(-6.33833333333333,-4.6,8.));
#22727=CARTESIAN_POINT('',(-6.3425,-4.5875,8.));
#22728=CARTESIAN_POINT('Origin',(-6.,-4.6,8.));
#22729=CARTESIAN_POINT('Origin',(-6.,-4.775,8.));
#22730=CARTESIAN_POINT('',(-6.33,-4.925,8.));
#22731=CARTESIAN_POINT('',(-6.33,-4.775,8.));
#22732=CARTESIAN_POINT('Origin',(-6.,-4.925,8.));
#22733=CARTESIAN_POINT('Origin',(-6.,-4.9375,8.));
#22734=CARTESIAN_POINT('',(-6.355,-4.95,8.));
#22735=CARTESIAN_POINT('',(-6.3425,-4.9375,8.));
#22736=CARTESIAN_POINT('Origin',(-6.,-4.95,8.));
#22737=CARTESIAN_POINT('Origin',(-5.45,-4.95,8.));
#22738=CARTESIAN_POINT('',(-6.55,-4.95,8.));
#22739=CARTESIAN_POINT('Origin',(-6.,-4.95,8.));
#22740=CARTESIAN_POINT('Origin',(-6.,-5.275,8.));
#22741=CARTESIAN_POINT('',(-6.55,-5.275,8.));
#22742=CARTESIAN_POINT('Origin',(6.,-4.5875,8.));
#22743=CARTESIAN_POINT('',(5.67,-4.625,8.));
#22744=CARTESIAN_POINT('Origin',(6.,-4.625,8.));
#22745=CARTESIAN_POINT('',(5.66166666666667,-4.6,8.));
#22746=CARTESIAN_POINT('',(5.6575,-4.5875,8.));
#22747=CARTESIAN_POINT('Origin',(6.,-4.6,8.));
#22748=CARTESIAN_POINT('Origin',(6.,-4.775,8.));
#22749=CARTESIAN_POINT('',(5.67,-4.925,8.));
#22750=CARTESIAN_POINT('',(5.67,-4.775,8.));
#22751=CARTESIAN_POINT('Origin',(6.,-4.925,8.));
#22752=CARTESIAN_POINT('Origin',(6.,-4.9375,8.));
#22753=CARTESIAN_POINT('',(5.645,-4.95,8.));
#22754=CARTESIAN_POINT('',(5.6575,-4.9375,8.));
#22755=CARTESIAN_POINT('Origin',(6.,-4.95,8.));
#22756=CARTESIAN_POINT('Origin',(6.55,-4.95,8.));
#22757=CARTESIAN_POINT('',(5.45,-4.95,8.));
#22758=CARTESIAN_POINT('Origin',(6.,-4.95,8.));
#22759=CARTESIAN_POINT('Origin',(6.,-5.275,8.));
#22760=CARTESIAN_POINT('',(5.45,-5.275,8.));
#22761=CARTESIAN_POINT('Origin',(0.,-5.605,7.2));
#22762=CARTESIAN_POINT('',(-3.79640507735679E-16,-5.55,4.1));
#22763=CARTESIAN_POINT('Origin',(0.,-5.55,7.2));
#22764=CARTESIAN_POINT('',(3.8637606513099E-16,-5.605,4.045));
#22765=CARTESIAN_POINT('Origin',(0.,-5.175,7.2));
#22766=CARTESIAN_POINT('',(-3.7964050773568E-16,-4.8,4.1));
#22767=CARTESIAN_POINT('',(-3.79640507735679E-16,-5.175,4.1));
#22768=CARTESIAN_POINT('Origin',(0.,-4.8,7.2));
#22769=CARTESIAN_POINT('Origin',(0.,-4.8,10.95));
#22770=CARTESIAN_POINT('',(-4.59242549680257E-16,-4.8,3.45));
#22771=CARTESIAN_POINT('Origin',(0.,-4.8,7.2));
#22772=CARTESIAN_POINT('Origin',(0.,-3.55,7.2));
#22773=CARTESIAN_POINT('',(-4.59242549680257E-16,-3.55,3.45));
#22774=CARTESIAN_POINT('Origin',(6.,-4.6,8.));
#22775=CARTESIAN_POINT('',(5.79948381734181,-4.6,7.12262136993645));
#22776=CARTESIAN_POINT('',(5.79948381734181,-4.6,7.12262136993645));
#22777=CARTESIAN_POINT('Origin',(6.,-4.6,8.));
#22778=CARTESIAN_POINT('Origin',(0.,-4.6,7.2));
#22779=CARTESIAN_POINT('',(4.39098268679659,-4.6,3.41063711895356));
#22780=CARTESIAN_POINT('',(4.39098268679659,-4.6,3.41063711895356));
#22781=CARTESIAN_POINT('Origin',(0.,-4.6,7.2));
#22782=CARTESIAN_POINT('Origin',(4.,-4.6,2.6));
#22783=CARTESIAN_POINT('',(3.14292474054464,-4.6,2.32536933960403));
#22784=CARTESIAN_POINT('',(3.14292474054464,-4.6,2.32536933960403));
#22785=CARTESIAN_POINT('Origin',(4.,-4.6,2.6));
#22786=CARTESIAN_POINT('Origin',(0.,-4.6,7.2));
#22787=CARTESIAN_POINT('Origin',(0.,-4.6,7.2));
#22788=CARTESIAN_POINT('Origin',(0.,-4.6,7.2));
#22789=CARTESIAN_POINT('',(0.,0.,0.));
#22790=CARTESIAN_POINT('Origin',(-8.55,6.01214466094067,20.1471446609407));
#22791=CARTESIAN_POINT('',(-8.6,6.9,19.1885786437627));
#22792=CARTESIAN_POINT('',(-8.6,5.68857864376269,20.4));
#22793=CARTESIAN_POINT('',(-8.6,5.97678932188134,20.1117893218813));
#22794=CARTESIAN_POINT('',(-8.5,5.73,20.5));
#22795=CARTESIAN_POINT('',(-8.6,5.68857864376269,20.4));
#22796=CARTESIAN_POINT('',(-8.5,7.,19.23));
#22797=CARTESIAN_POINT('',(-8.5,6.0475,20.1825));
#22798=CARTESIAN_POINT('',(-8.6,6.9,19.1885786437627));
#22799=CARTESIAN_POINT('Origin',(-8.55,-2.865,20.45));
#22800=CARTESIAN_POINT('',(-8.6,-5.68857864376269,20.4));
#22801=CARTESIAN_POINT('',(-8.6,-2.865,20.4));
#22802=CARTESIAN_POINT('',(-8.5,-5.73,20.5));
#22803=CARTESIAN_POINT('',(-8.6,-5.68857864376269,20.4));
#22804=CARTESIAN_POINT('',(-8.5,-2.865,20.5));
#22805=CARTESIAN_POINT('Origin',(-8.55,-6.64714466094067,19.5121446609407));
#22806=CARTESIAN_POINT('',(-8.6,-6.9,19.1885786437627));
#22807=CARTESIAN_POINT('',(-8.6,-6.61178932188135,19.4767893218813));
#22808=CARTESIAN_POINT('',(-8.5,-7.,19.23));
#22809=CARTESIAN_POINT('',(-8.6,-6.9,19.1885786437627));
#22810=CARTESIAN_POINT('',(-8.5,-6.6825,19.5475));
#22811=CARTESIAN_POINT('Origin',(-8.55,-6.95,10.635));
#22812=CARTESIAN_POINT('',(-8.6,-6.9,7.81142135623731));
#22813=CARTESIAN_POINT('',(-8.6,-6.9,10.635));
#22814=CARTESIAN_POINT('',(-8.5,-7.,7.77));
#22815=CARTESIAN_POINT('',(-8.6,-6.9,7.81142135623731));
#22816=CARTESIAN_POINT('',(-8.5,-7.,10.635));
#22817=CARTESIAN_POINT('Origin',(-8.55,-6.01214466094067,6.85285533905933));
#22818=CARTESIAN_POINT('',(-8.6,-5.68857864376269,6.6));
#22819=CARTESIAN_POINT('',(-8.6,-5.97678932188134,6.88821067811866));
#22820=CARTESIAN_POINT('',(-8.5,-5.73,6.5));
#22821=CARTESIAN_POINT('',(-8.6,-5.68857864376269,6.6));
#22822=CARTESIAN_POINT('',(-8.5,-6.0475,6.8175));
#22823=CARTESIAN_POINT('Origin',(-8.55,2.865,6.55));
#22824=CARTESIAN_POINT('',(-8.5,5.73,6.5));
#22825=CARTESIAN_POINT('',(-8.5,2.865,6.5));
#22826=CARTESIAN_POINT('',(-8.6,5.68857864376269,6.6));
#22827=CARTESIAN_POINT('',(-8.6,2.865,6.6));
#22828=CARTESIAN_POINT('',(-8.6,5.68857864376269,6.6));
#22829=CARTESIAN_POINT('Origin',(-8.55,6.64714466094067,7.48785533905933));
#22830=CARTESIAN_POINT('',(-8.5,7.,7.77));
#22831=CARTESIAN_POINT('',(-8.5,6.6825,7.4525));
#22832=CARTESIAN_POINT('',(-8.6,6.9,7.81142135623731));
#22833=CARTESIAN_POINT('',(-8.6,6.61178932188134,7.52321067811866));
#22834=CARTESIAN_POINT('',(-8.6,6.9,7.81142135623731));
#22835=CARTESIAN_POINT('Origin',(-8.55,6.95,16.365));
#22836=CARTESIAN_POINT('',(-8.5,7.,16.365));
#22837=CARTESIAN_POINT('',(-8.6,6.9,16.365));
#22838=CARTESIAN_POINT('Origin',(-7.2,5.73,6.5));
#22839=CARTESIAN_POINT('',(-7.2,5.73,6.5));
#22840=CARTESIAN_POINT('',(-7.2,5.73,6.5));
#22841=CARTESIAN_POINT('',(-7.2,-5.73,6.5));
#22842=CARTESIAN_POINT('',(-7.2,-5.73,6.5));
#22843=CARTESIAN_POINT('',(-7.2,-5.73,6.5));
#22844=CARTESIAN_POINT('Origin',(-7.2,7.,7.77));
#22845=CARTESIAN_POINT('',(-7.2,7.,7.77));
#22846=CARTESIAN_POINT('',(-7.2,7.,7.77));
#22847=CARTESIAN_POINT('',(-7.2,5.73,6.5));
#22848=CARTESIAN_POINT('Origin',(-7.2,7.,19.23));
#22849=CARTESIAN_POINT('',(-7.2,7.,19.23));
#22850=CARTESIAN_POINT('',(-7.2,7.,19.23));
#22851=CARTESIAN_POINT('',(-7.2,7.,7.77));
#22852=CARTESIAN_POINT('Origin',(-7.2,5.73,20.5));
#22853=CARTESIAN_POINT('',(-7.2,5.73,20.5));
#22854=CARTESIAN_POINT('',(-7.2,5.73,20.5));
#22855=CARTESIAN_POINT('',(-7.2,7.,19.23));
#22856=CARTESIAN_POINT('Origin',(-8.6,0.,13.5));
#22857=CARTESIAN_POINT('',(-8.6,-4.116,8.904));
#22858=CARTESIAN_POINT('Origin',(-8.6,-4.596,8.904));
#22859=CARTESIAN_POINT('',(-8.6,5.9,12.));
#22860=CARTESIAN_POINT('',(-8.6,6.6,12.));
#22861=CARTESIAN_POINT('',(-8.6,3.3,12.));
#22862=CARTESIAN_POINT('',(-8.6,6.6,15.));
#22863=CARTESIAN_POINT('',(-8.6,6.6,14.25));
#22864=CARTESIAN_POINT('',(-8.6,5.9,15.));
#22865=CARTESIAN_POINT('',(-8.6,2.95,15.));
#22866=CARTESIAN_POINT('',(-8.6,5.9,12.75));
#22867=CARTESIAN_POINT('',(-8.6,-1.5,6.9));
#22868=CARTESIAN_POINT('',(-8.6,1.5,6.9));
#22869=CARTESIAN_POINT('',(-8.6,0.75,6.9));
#22870=CARTESIAN_POINT('',(-8.6,1.5,7.6));
#22871=CARTESIAN_POINT('',(-8.6,1.5,10.55));
#22872=CARTESIAN_POINT('',(-8.6,-1.5,7.6));
#22873=CARTESIAN_POINT('',(-8.6,-0.75,7.6));
#22874=CARTESIAN_POINT('',(-8.6,-1.5,10.2));
#22875=CARTESIAN_POINT('',(-8.6,-1.5,19.4));
#22876=CARTESIAN_POINT('',(-8.6,1.5,19.4));
#22877=CARTESIAN_POINT('',(-8.6,0.75,19.4));
#22878=CARTESIAN_POINT('',(-8.6,1.5,20.1));
#22879=CARTESIAN_POINT('',(-8.6,1.5,16.8));
#22880=CARTESIAN_POINT('',(-8.6,-1.5,20.1));
#22881=CARTESIAN_POINT('',(-8.6,-0.75,20.1));
#22882=CARTESIAN_POINT('',(-8.6,-1.5,16.45));
#22883=CARTESIAN_POINT('',(-8.6,-6.6,12.));
#22884=CARTESIAN_POINT('',(-8.6,-5.9,12.));
#22885=CARTESIAN_POINT('',(-8.6,-2.95,12.));
#22886=CARTESIAN_POINT('',(-8.6,-5.9,15.));
#22887=CARTESIAN_POINT('',(-8.6,-5.9,14.25));
#22888=CARTESIAN_POINT('',(-8.6,-6.6,15.));
#22889=CARTESIAN_POINT('',(-8.6,-3.3,15.));
#22890=CARTESIAN_POINT('',(-8.6,-6.6,12.75));
#22891=CARTESIAN_POINT('',(-8.6,-6.73678204210959E-16,19.001));
#22892=CARTESIAN_POINT('Origin',(-8.6,0.,13.5));
#22893=CARTESIAN_POINT('',(-8.6,5.076,18.096));
#22894=CARTESIAN_POINT('Origin',(-8.6,4.596,18.096));
#22895=CARTESIAN_POINT('',(-8.6,-4.116,18.096));
#22896=CARTESIAN_POINT('Origin',(-8.6,-4.596,18.096));
#22897=CARTESIAN_POINT('',(-8.6,5.076,8.904));
#22898=CARTESIAN_POINT('Origin',(-8.6,4.596,8.904));
#22899=CARTESIAN_POINT('Origin',(-7.1875,-3.182,10.318));
#22900=CARTESIAN_POINT('',(-7.225,-2.852,10.318));
#22901=CARTESIAN_POINT('Origin',(-7.225,-3.182,10.318));
#22902=CARTESIAN_POINT('',(-7.2,-2.84366666666667,10.318));
#22903=CARTESIAN_POINT('',(-7.1875,-2.8395,10.318));
#22904=CARTESIAN_POINT('Origin',(-7.2,-3.182,10.318));
#22905=CARTESIAN_POINT('Origin',(-7.375,-3.182,10.318));
#22906=CARTESIAN_POINT('',(-7.525,-2.852,10.318));
#22907=CARTESIAN_POINT('',(-7.375,-2.852,10.318));
#22908=CARTESIAN_POINT('Origin',(-7.525,-3.182,10.318));
#22909=CARTESIAN_POINT('Origin',(-7.5375,-3.182,10.318));
#22910=CARTESIAN_POINT('',(-7.55,-2.827,10.318));
#22911=CARTESIAN_POINT('',(-7.5375,-2.8395,10.318));
#22912=CARTESIAN_POINT('Origin',(-7.55,-3.182,10.318));
#22913=CARTESIAN_POINT('Origin',(-7.55,-3.732,10.318));
#22914=CARTESIAN_POINT('',(-7.55,-2.632,10.318));
#22915=CARTESIAN_POINT('Origin',(-7.55,-3.182,10.318));
#22916=CARTESIAN_POINT('Origin',(-7.875,-3.182,10.318));
#22917=CARTESIAN_POINT('',(-8.2,-2.632,10.318));
#22918=CARTESIAN_POINT('',(-7.875,-2.632,10.318));
#22919=CARTESIAN_POINT('Origin',(-8.2,-3.182,10.318));
#22920=CARTESIAN_POINT('Origin',(-7.1875,3.182,10.318));
#22921=CARTESIAN_POINT('',(-7.225,3.512,10.318));
#22922=CARTESIAN_POINT('Origin',(-7.225,3.182,10.318));
#22923=CARTESIAN_POINT('',(-7.2,3.52033333333333,10.318));
#22924=CARTESIAN_POINT('',(-7.1875,3.5245,10.318));
#22925=CARTESIAN_POINT('Origin',(-7.2,3.182,10.318));
#22926=CARTESIAN_POINT('Origin',(-7.375,3.182,10.318));
#22927=CARTESIAN_POINT('',(-7.525,3.512,10.318));
#22928=CARTESIAN_POINT('',(-7.375,3.512,10.318));
#22929=CARTESIAN_POINT('Origin',(-7.525,3.182,10.318));
#22930=CARTESIAN_POINT('Origin',(-7.5375,3.182,10.318));
#22931=CARTESIAN_POINT('',(-7.55,3.537,10.318));
#22932=CARTESIAN_POINT('',(-7.5375,3.5245,10.318));
#22933=CARTESIAN_POINT('Origin',(-7.55,3.182,10.318));
#22934=CARTESIAN_POINT('Origin',(-7.55,2.632,10.318));
#22935=CARTESIAN_POINT('',(-7.55,3.732,10.318));
#22936=CARTESIAN_POINT('Origin',(-7.55,3.182,10.318));
#22937=CARTESIAN_POINT('Origin',(-7.875,3.182,10.318));
#22938=CARTESIAN_POINT('',(-8.2,3.732,10.318));
#22939=CARTESIAN_POINT('',(-7.875,3.732,10.318));
#22940=CARTESIAN_POINT('Origin',(-8.2,3.182,10.318));
#22941=CARTESIAN_POINT('Origin',(-7.1875,-3.182,16.682));
#22942=CARTESIAN_POINT('',(-7.225,-2.852,16.682));
#22943=CARTESIAN_POINT('Origin',(-7.225,-3.182,16.682));
#22944=CARTESIAN_POINT('',(-7.2,-2.84366666666667,16.682));
#22945=CARTESIAN_POINT('',(-7.1875,-2.8395,16.682));
#22946=CARTESIAN_POINT('Origin',(-7.2,-3.182,16.682));
#22947=CARTESIAN_POINT('Origin',(-7.375,-3.182,16.682));
#22948=CARTESIAN_POINT('',(-7.525,-2.852,16.682));
#22949=CARTESIAN_POINT('',(-7.375,-2.852,16.682));
#22950=CARTESIAN_POINT('Origin',(-7.525,-3.182,16.682));
#22951=CARTESIAN_POINT('Origin',(-7.5375,-3.182,16.682));
#22952=CARTESIAN_POINT('',(-7.55,-2.827,16.682));
#22953=CARTESIAN_POINT('',(-7.5375,-2.8395,16.682));
#22954=CARTESIAN_POINT('Origin',(-7.55,-3.182,16.682));
#22955=CARTESIAN_POINT('Origin',(-7.55,-3.732,16.682));
#22956=CARTESIAN_POINT('',(-7.55,-2.632,16.682));
#22957=CARTESIAN_POINT('Origin',(-7.55,-3.182,16.682));
#22958=CARTESIAN_POINT('Origin',(-7.875,-3.182,16.682));
#22959=CARTESIAN_POINT('',(-8.2,-2.632,16.682));
#22960=CARTESIAN_POINT('',(-7.875,-2.632,16.682));
#22961=CARTESIAN_POINT('Origin',(-8.2,-3.182,16.682));
#22962=CARTESIAN_POINT('Origin',(-7.1875,3.182,16.682));
#22963=CARTESIAN_POINT('',(-7.225,3.512,16.682));
#22964=CARTESIAN_POINT('Origin',(-7.225,3.182,16.682));
#22965=CARTESIAN_POINT('',(-7.2,3.52033333333333,16.682));
#22966=CARTESIAN_POINT('',(-7.1875,3.5245,16.682));
#22967=CARTESIAN_POINT('Origin',(-7.2,3.182,16.682));
#22968=CARTESIAN_POINT('Origin',(-7.375,3.182,16.682));
#22969=CARTESIAN_POINT('',(-7.525,3.512,16.682));
#22970=CARTESIAN_POINT('',(-7.375,3.512,16.682));
#22971=CARTESIAN_POINT('Origin',(-7.525,3.182,16.682));
#22972=CARTESIAN_POINT('Origin',(-7.5375,3.182,16.682));
#22973=CARTESIAN_POINT('',(-7.55,3.537,16.682));
#22974=CARTESIAN_POINT('',(-7.5375,3.5245,16.682));
#22975=CARTESIAN_POINT('Origin',(-7.55,3.182,16.682));
#22976=CARTESIAN_POINT('Origin',(-7.55,2.632,16.682));
#22977=CARTESIAN_POINT('',(-7.55,3.732,16.682));
#22978=CARTESIAN_POINT('Origin',(-7.55,3.182,16.682));
#22979=CARTESIAN_POINT('Origin',(-7.875,3.182,16.682));
#22980=CARTESIAN_POINT('',(-8.2,3.732,16.682));
#22981=CARTESIAN_POINT('',(-7.875,3.732,16.682));
#22982=CARTESIAN_POINT('Origin',(-8.2,3.182,16.682));
#22983=CARTESIAN_POINT('Origin',(-7.19,-4.596,8.904));
#22984=CARTESIAN_POINT('',(-7.23,-4.146,8.904));
#22985=CARTESIAN_POINT('Origin',(-7.23,-4.596,8.904));
#22986=CARTESIAN_POINT('',(-7.2,-4.116,8.904));
#22987=CARTESIAN_POINT('',(-7.19,-4.106,8.904));
#22988=CARTESIAN_POINT('Origin',(-7.2,-4.596,8.904));
#22989=CARTESIAN_POINT('Origin',(-7.9,-4.596,8.904));
#22990=CARTESIAN_POINT('',(-8.57,-4.146,8.904));
#22991=CARTESIAN_POINT('',(-7.9,-4.146,8.904));
#22992=CARTESIAN_POINT('Origin',(-8.57,-4.596,8.904));
#22993=CARTESIAN_POINT('Origin',(-8.61,-4.596,8.904));
#22994=CARTESIAN_POINT('',(-8.61,-4.106,8.904));
#22995=CARTESIAN_POINT('Origin',(-7.19,4.596,8.904));
#22996=CARTESIAN_POINT('',(-7.23,5.046,8.904));
#22997=CARTESIAN_POINT('Origin',(-7.23,4.596,8.904));
#22998=CARTESIAN_POINT('',(-7.2,5.076,8.904));
#22999=CARTESIAN_POINT('',(-7.19,5.086,8.904));
#23000=CARTESIAN_POINT('Origin',(-7.2,4.596,8.904));
#23001=CARTESIAN_POINT('Origin',(-7.9,4.596,8.904));
#23002=CARTESIAN_POINT('',(-8.57,5.046,8.904));
#23003=CARTESIAN_POINT('',(-7.9,5.046,8.904));
#23004=CARTESIAN_POINT('Origin',(-8.57,4.596,8.904));
#23005=CARTESIAN_POINT('Origin',(-8.61,4.596,8.904));
#23006=CARTESIAN_POINT('',(-8.61,5.086,8.904));
#23007=CARTESIAN_POINT('Origin',(-7.19,-4.596,18.096));
#23008=CARTESIAN_POINT('',(-7.23,-4.146,18.096));
#23009=CARTESIAN_POINT('Origin',(-7.23,-4.596,18.096));
#23010=CARTESIAN_POINT('',(-7.2,-4.116,18.096));
#23011=CARTESIAN_POINT('',(-7.19,-4.106,18.096));
#23012=CARTESIAN_POINT('Origin',(-7.2,-4.596,18.096));
#23013=CARTESIAN_POINT('Origin',(-7.9,-4.596,18.096));
#23014=CARTESIAN_POINT('',(-8.57,-4.146,18.096));
#23015=CARTESIAN_POINT('',(-7.9,-4.146,18.096));
#23016=CARTESIAN_POINT('Origin',(-8.57,-4.596,18.096));
#23017=CARTESIAN_POINT('Origin',(-8.61,-4.596,18.096));
#23018=CARTESIAN_POINT('',(-8.61,-4.106,18.096));
#23019=CARTESIAN_POINT('Origin',(-7.19,4.596,18.096));
#23020=CARTESIAN_POINT('',(-7.23,5.046,18.096));
#23021=CARTESIAN_POINT('Origin',(-7.23,4.596,18.096));
#23022=CARTESIAN_POINT('',(-7.2,5.076,18.096));
#23023=CARTESIAN_POINT('',(-7.19,5.086,18.096));
#23024=CARTESIAN_POINT('Origin',(-7.2,4.596,18.096));
#23025=CARTESIAN_POINT('Origin',(-7.9,4.596,18.096));
#23026=CARTESIAN_POINT('',(-8.57,5.046,18.096));
#23027=CARTESIAN_POINT('',(-7.9,5.046,18.096));
#23028=CARTESIAN_POINT('Origin',(-8.57,4.596,18.096));
#23029=CARTESIAN_POINT('Origin',(-8.61,4.596,18.096));
#23030=CARTESIAN_POINT('',(-8.61,5.086,18.096));
#23031=CARTESIAN_POINT('Origin',(-7.2,6.6,12.));
#23032=CARTESIAN_POINT('',(-7.2,6.6,12.));
#23033=CARTESIAN_POINT('',(-7.2,5.9,12.));
#23034=CARTESIAN_POINT('',(-7.2,3.3,12.));
#23035=CARTESIAN_POINT('',(-7.2,6.6,12.));
#23036=CARTESIAN_POINT('',(-7.2,5.9,12.));
#23037=CARTESIAN_POINT('Origin',(-7.2,6.6,15.));
#23038=CARTESIAN_POINT('',(-7.2,6.6,15.));
#23039=CARTESIAN_POINT('',(-7.2,6.6,14.25));
#23040=CARTESIAN_POINT('',(-7.2,6.6,15.));
#23041=CARTESIAN_POINT('Origin',(-7.2,5.9,15.));
#23042=CARTESIAN_POINT('',(-7.2,5.9,15.));
#23043=CARTESIAN_POINT('',(-7.2,2.95,15.));
#23044=CARTESIAN_POINT('',(-7.2,5.9,15.));
#23045=CARTESIAN_POINT('Origin',(-7.2,5.9,12.));
#23046=CARTESIAN_POINT('',(-7.2,5.9,12.75));
#23047=CARTESIAN_POINT('Origin',(-7.2,1.5,6.9));
#23048=CARTESIAN_POINT('',(-7.2,1.5,6.9));
#23049=CARTESIAN_POINT('',(-7.2,-1.5,6.9));
#23050=CARTESIAN_POINT('',(-7.2,0.75,6.9));
#23051=CARTESIAN_POINT('',(-7.2,1.5,6.9));
#23052=CARTESIAN_POINT('',(-7.2,-1.5,6.9));
#23053=CARTESIAN_POINT('Origin',(-7.2,1.5,7.6));
#23054=CARTESIAN_POINT('',(-7.2,1.5,7.6));
#23055=CARTESIAN_POINT('',(-7.2,1.5,10.55));
#23056=CARTESIAN_POINT('',(-7.2,1.5,7.6));
#23057=CARTESIAN_POINT('Origin',(-7.2,-1.5,7.6));
#23058=CARTESIAN_POINT('',(-7.2,-1.5,7.6));
#23059=CARTESIAN_POINT('',(-7.2,-0.75,7.6));
#23060=CARTESIAN_POINT('',(-7.2,-1.5,7.6));
#23061=CARTESIAN_POINT('Origin',(-7.2,-1.5,6.9));
#23062=CARTESIAN_POINT('',(-7.2,-1.5,10.2));
#23063=CARTESIAN_POINT('Origin',(-7.2,1.5,19.4));
#23064=CARTESIAN_POINT('',(-7.2,1.5,19.4));
#23065=CARTESIAN_POINT('',(-7.2,-1.5,19.4));
#23066=CARTESIAN_POINT('',(-7.2,0.75,19.4));
#23067=CARTESIAN_POINT('',(-7.2,1.5,19.4));
#23068=CARTESIAN_POINT('',(-7.2,-1.5,19.4));
#23069=CARTESIAN_POINT('Origin',(-7.2,1.5,20.1));
#23070=CARTESIAN_POINT('',(-7.2,1.5,20.1));
#23071=CARTESIAN_POINT('',(-7.2,1.5,16.8));
#23072=CARTESIAN_POINT('',(-7.2,1.5,20.1));
#23073=CARTESIAN_POINT('Origin',(-7.2,-1.5,20.1));
#23074=CARTESIAN_POINT('',(-7.2,-1.5,20.1));
#23075=CARTESIAN_POINT('',(-7.2,-0.75,20.1));
#23076=CARTESIAN_POINT('',(-7.2,-1.5,20.1));
#23077=CARTESIAN_POINT('Origin',(-7.2,-1.5,19.4));
#23078=CARTESIAN_POINT('',(-7.2,-1.5,16.45));
#23079=CARTESIAN_POINT('Origin',(-7.2,-5.9,12.));
#23080=CARTESIAN_POINT('',(-7.2,-5.9,12.));
#23081=CARTESIAN_POINT('',(-7.2,-6.6,12.));
#23082=CARTESIAN_POINT('',(-7.2,-2.95,12.));
#23083=CARTESIAN_POINT('',(-7.2,-5.9,12.));
#23084=CARTESIAN_POINT('',(-7.2,-6.6,12.));
#23085=CARTESIAN_POINT('Origin',(-7.2,-5.9,15.));
#23086=CARTESIAN_POINT('',(-7.2,-5.9,15.));
#23087=CARTESIAN_POINT('',(-7.2,-5.9,14.25));
#23088=CARTESIAN_POINT('',(-7.2,-5.9,15.));
#23089=CARTESIAN_POINT('Origin',(-7.2,-6.6,15.));
#23090=CARTESIAN_POINT('',(-7.2,-6.6,15.));
#23091=CARTESIAN_POINT('',(-7.2,-3.3,15.));
#23092=CARTESIAN_POINT('',(-7.2,-6.6,15.));
#23093=CARTESIAN_POINT('Origin',(-7.2,-6.6,12.));
#23094=CARTESIAN_POINT('',(-7.2,-6.6,12.75));
#23095=CARTESIAN_POINT('Origin',(-7.2,0.,13.5));
#23096=CARTESIAN_POINT('',(-7.2,-2.44929359829471E-16,15.5));
#23097=CARTESIAN_POINT('Origin',(-7.2,0.,13.5));
#23098=CARTESIAN_POINT('',(-8.2,-2.44929359829471E-16,15.5));
#23099=CARTESIAN_POINT('',(-7.2,2.44929359829471E-16,15.5));
#23100=CARTESIAN_POINT('Origin',(-8.2,0.,13.5));
#23101=CARTESIAN_POINT('Origin',(-8.6,0.,13.5));
#23102=CARTESIAN_POINT('',(-8.2,-6.73678204210959E-16,19.001));
#23103=CARTESIAN_POINT('',(-8.6,-6.73678204210959E-16,19.001));
#23104=CARTESIAN_POINT('Origin',(-8.2,0.,13.5));
#23105=CARTESIAN_POINT('Origin',(-8.2,0.,13.5));
#23106=CARTESIAN_POINT('Origin',(-7.2,-5.73,20.5));
#23107=CARTESIAN_POINT('',(-7.2,-5.73,20.5));
#23108=CARTESIAN_POINT('',(-7.2,-5.73,20.5));
#23109=CARTESIAN_POINT('',(-7.2,5.73,20.5));
#23110=CARTESIAN_POINT('Origin',(-7.2,-7.,19.23));
#23111=CARTESIAN_POINT('',(-7.2,-7.,19.23));
#23112=CARTESIAN_POINT('',(-7.2,-7.,19.23));
#23113=CARTESIAN_POINT('',(-7.2,-5.73,20.5));
#23114=CARTESIAN_POINT('Origin',(-7.2,-7.,7.77));
#23115=CARTESIAN_POINT('',(-7.2,-7.,7.77));
#23116=CARTESIAN_POINT('',(-7.2,-7.,7.77));
#23117=CARTESIAN_POINT('',(-7.2,-7.,19.23));
#23118=CARTESIAN_POINT('Origin',(-7.2,-5.73,6.5));
#23119=CARTESIAN_POINT('',(-7.2,-7.,7.77));
#23120=CARTESIAN_POINT('Origin',(-7.2,0.,13.5));
#23121=CARTESIAN_POINT('',(0.,0.,0.));
#23122=CARTESIAN_POINT('Origin',(0.,0.,13.5));
#23123=CARTESIAN_POINT('',(2.22083974265588,-0.416497439768541,12.1633886568391));
#23124=CARTESIAN_POINT('',(2.40093257836374,-0.416497469208933,12.163388666013));
#23125=CARTESIAN_POINT('',(0.,-0.416497449530544,12.1633886598811));
#23126=CARTESIAN_POINT('',(3.11803278688524,-0.795264618259144,12.3478046229284));
#23127=CARTESIAN_POINT('Ctrl Pts',(2.22083974265588,-0.41649743976857,12.1633886568392));
#23128=CARTESIAN_POINT('Ctrl Pts',(2.2220583526003,-0.405658322369837,12.1600111120734));
#23129=CARTESIAN_POINT('Ctrl Pts',(2.22327782186277,-0.394773680664366,
12.1567640315656));
#23130=CARTESIAN_POINT('Ctrl Pts',(2.22938824338899,-0.34005543600158,12.141163821239));
#23131=CARTESIAN_POINT('Ctrl Pts',(2.23428033926222,-0.295682000890378,
12.1308230099316));
#23132=CARTESIAN_POINT('Ctrl Pts',(2.24895685570008,-0.161170286254102,
12.10632153116));
#23133=CARTESIAN_POINT('Ctrl Pts',(2.25866610420412,-0.070073656053006,
12.0987841785454));
#23134=CARTESIAN_POINT('Ctrl Pts',(2.27331012373895,0.0668268643511414,
12.1008485412387));
#23135=CARTESIAN_POINT('Ctrl Pts',(2.27820301388258,0.112483216940743,12.1037772244606));
#23136=CARTESIAN_POINT('Ctrl Pts',(2.29279615275694,0.24770334958519,12.1191273943385));
#23137=CARTESIAN_POINT('Ctrl Pts',(2.30249930101493,0.336296155354615,12.1379899977253));
#23138=CARTESIAN_POINT('Ctrl Pts',(2.3206444637074,0.497852571538328,12.1891233324526));
#23139=CARTESIAN_POINT('Ctrl Pts',(2.3290677605188,0.571096236923704,12.2193345192887));
#23140=CARTESIAN_POINT('Ctrl Pts',(2.34241546071034,0.681984453214291,12.2764877494031));
#23141=CARTESIAN_POINT('Ctrl Pts',(2.34730489916618,0.721524101820936,12.2993802178688));
#23142=CARTESIAN_POINT('Ctrl Pts',(2.36188217783804,0.83563462320767,12.3731230947425));
#23143=CARTESIAN_POINT('Ctrl Pts',(2.3715671462109,0.906487948408386,12.4292913789087));
#23144=CARTESIAN_POINT('Ctrl Pts',(2.39082504161259,1.036075619433,12.5541652941715));
#23145=CARTESIAN_POINT('Ctrl Pts',(2.40038146080491,1.09456759418981,12.6225162833593));
#23146=CARTESIAN_POINT('Ctrl Pts',(2.41973055679119,1.19830818950665,12.7703988020955));
#23147=CARTESIAN_POINT('Ctrl Pts',(2.42948098070764,1.24313391978949,12.8497092131317));
#23148=CARTESIAN_POINT('Ctrl Pts',(2.45867561213097,1.35340306175113,13.098545263797));
#23149=CARTESIAN_POINT('Ctrl Pts',(2.47789933184414,1.39396340856472,13.2769907630923));
#23150=CARTESIAN_POINT('Ctrl Pts',(2.50712132114416,1.40210544760839,13.5495874517168));
#23151=CARTESIAN_POINT('Ctrl Pts',(2.51687140626553,1.39587676776904,13.6410204447446));
#23152=CARTESIAN_POINT('Ctrl Pts',(2.53643597386339,1.36570547636464,13.8212170813072));
#23153=CARTESIAN_POINT('Ctrl Pts',(2.54621714872809,1.34186370907104,13.9095525151614));
#23154=CARTESIAN_POINT('Ctrl Pts',(2.57551273484634,1.24530587458394,14.1650438428224));
#23155=CARTESIAN_POINT('Ctrl Pts',(2.59470675330616,1.14848483177222,14.3210067294209));
#23156=CARTESIAN_POINT('Ctrl Pts',(2.62394307084879,0.962900170700194,14.5202981151465));
#23157=CARTESIAN_POINT('Ctrl Pts',(2.63364712817475,0.894970769260525,14.5803762919486));
#23158=CARTESIAN_POINT('Ctrl Pts',(2.6482121350503,0.78480653483361,14.6602402565328));
#23159=CARTESIAN_POINT('Ctrl Pts',(2.65308657104942,0.746607731332198,14.6851816883857));
#23160=CARTESIAN_POINT('Ctrl Pts',(2.66774732143052,0.628442913409038,14.7543525783653));
#23161=CARTESIAN_POINT('Ctrl Pts',(2.67752998692593,0.54530029314993,14.7926670500713));
#23162=CARTESIAN_POINT('Ctrl Pts',(2.70677127875774,0.287719996404971,14.8820622920458));
#23163=CARTESIAN_POINT('Ctrl Pts',(2.72591975017619,0.106490054773707,14.9076709254911));
#23164=CARTESIAN_POINT('Ctrl Pts',(2.75031354364582,-0.120195919936996,
14.8955788049496));
#23165=CARTESIAN_POINT('Ctrl Pts',(2.75522162089908,-0.165671790034989,
14.8909134542766));
#23166=CARTESIAN_POINT('Ctrl Pts',(2.77009054777941,-0.302795607010329,
14.8700245083829));
#23167=CARTESIAN_POINT('Ctrl Pts',(2.77999346651961,-0.393128585453869,
14.846886229962));
#23168=CARTESIAN_POINT('Ctrl Pts',(2.79970562545924,-0.565980620889559,
14.7837246427035));
#23169=CARTESIAN_POINT('Ctrl Pts',(2.80946709376518,-0.648213481481454,
14.7442274274943));
#23170=CARTESIAN_POINT('Ctrl Pts',(2.83857898677403,-0.880210390133891,
14.6035157318107));
#23171=CARTESIAN_POINT('Ctrl Pts',(2.85755216608694,-1.01488049741367,14.4810880890802));
#23172=CARTESIAN_POINT('Ctrl Pts',(2.88658123226053,-1.17626758116645,14.2644970249803));
#23173=CARTESIAN_POINT('Ctrl Pts',(2.89623374033106,-1.22286448705829,14.1875059788387));
#23174=CARTESIAN_POINT('Ctrl Pts',(2.91546261859488,-1.30070133902556,14.0255956353864));
#23175=CARTESIAN_POINT('Ctrl Pts',(2.92503074564317,-1.33174756560988,13.9410478719655));
#23176=CARTESIAN_POINT('Ctrl Pts',(2.9542902699067,-1.40088297110484,13.6766037982742));
#23177=CARTESIAN_POINT('Ctrl Pts',(2.97375228394956,-1.41194580410859,13.4916972316156));
#23178=CARTESIAN_POINT('Ctrl Pts',(3.0031538638659,-1.37477554337072,13.2204474743347));
#23179=CARTESIAN_POINT('Ctrl Pts',(3.01284518917861,-1.35388256235668,13.1323577884262));
#23180=CARTESIAN_POINT('Ctrl Pts',(3.03801192591717,-1.27754760755037,12.9091939938116));
#23181=CARTESIAN_POINT('Ctrl Pts',(3.05337881302878,-1.20926446619212,12.7796830412083));
#23182=CARTESIAN_POINT('Ctrl Pts',(3.07715259870693,-1.07705433667825,12.602407122906));
#23183=CARTESIAN_POINT('Ctrl Pts',(3.08530606893138,-1.0270062147963,12.5455488825751));
#23184=CARTESIAN_POINT('Ctrl Pts',(3.09756951055421,-0.94510461144696,12.4664430758878));
#23185=CARTESIAN_POINT('Ctrl Pts',(3.10168008047209,-0.916517926702076,
12.4410109684072));
#23186=CARTESIAN_POINT('Ctrl Pts',(3.10986378955223,-0.857326209600113,
12.392545637421));
#23187=CARTESIAN_POINT('Ctrl Pts',(3.11393406542358,-0.826747140816238,
12.3695343892349));
#23188=CARTESIAN_POINT('Ctrl Pts',(3.11803278688524,-0.79526461825914,12.3478046229284));
#23189=CARTESIAN_POINT('',(3.11803278688524,-7.6193401827091E-11,12.1));
#23190=CARTESIAN_POINT('Origin',(3.11803278688524,0.,13.5));
#23191=CARTESIAN_POINT('',(2.4462258455051,9.9958277766099E-11,12.1));
#23192=CARTESIAN_POINT('',(2.82743338823077,3.99408172289043E-15,12.1));
#23193=CARTESIAN_POINT('Ctrl Pts',(2.44622584550511,9.99578197991013E-11,
12.1));
#23194=CARTESIAN_POINT('Ctrl Pts',(2.43535738742254,-0.101588171354874,
12.0999999999927));
#23195=CARTESIAN_POINT('Ctrl Pts',(2.4245285855633,-0.202874837380493,12.1110572920391));
#23196=CARTESIAN_POINT('Ctrl Pts',(2.40940149924196,-0.340651325123096,
12.1415015994721));
#23197=CARTESIAN_POINT('Ctrl Pts',(2.40516687749463,-0.378827339870843,
12.1516503894212));
#23198=CARTESIAN_POINT('Ctrl Pts',(2.40093257836374,-0.416497469208933,
12.163388666013));
#23199=CARTESIAN_POINT('Origin',(0.,0.,13.5));
#23200=CARTESIAN_POINT('',(1.2784105384869,-0.416497393834651,12.1633886425258));
#23201=CARTESIAN_POINT('',(1.45844776950583,-0.416497492092897,12.1633886731438));
#23202=CARTESIAN_POINT('',(0.,-0.416497449530544,12.1633886598811));
#23203=CARTESIAN_POINT('Ctrl Pts',(1.27841053848688,-0.416497393834759,
12.1633886425259));
#23204=CARTESIAN_POINT('Ctrl Pts',(1.28527178782894,-0.35549476439837,12.1443797989789));
#23205=CARTESIAN_POINT('Ctrl Pts',(1.2921365525235,-0.293132247098585,12.1295287146373));
#23206=CARTESIAN_POINT('Ctrl Pts',(1.31508503284192,-0.0811815868699625,
12.0942553113078));
#23207=CARTESIAN_POINT('Ctrl Pts',(1.33101467229848,0.0704855897874028,
12.0936793574202));
#23208=CARTESIAN_POINT('Ctrl Pts',(1.35683082249829,0.307564317060159,12.131282019496));
#23209=CARTESIAN_POINT('Ctrl Pts',(1.36646427484744,0.394276150658717,12.153697192415));
#23210=CARTESIAN_POINT('Ctrl Pts',(1.38646947732948,0.569484258485247,12.217381876624));
#23211=CARTESIAN_POINT('Ctrl Pts',(1.39676539950078,0.657015788254973,12.2599384696789));
#23212=CARTESIAN_POINT('Ctrl Pts',(1.41693666553056,0.817140830789634,12.3595378026002));
#23213=CARTESIAN_POINT('Ctrl Pts',(1.42673342773507,0.889914770527173,12.4153690187576));
#23214=CARTESIAN_POINT('Ctrl Pts',(1.4561871961819,1.09044099002743,12.6030677246971));
#23215=CARTESIAN_POINT('Ctrl Pts',(1.47577090895044,1.19831474728728,12.7532764172855));
#23216=CARTESIAN_POINT('Ctrl Pts',(1.5047821378587,1.31110480527774,13.001063248523));
#23217=CARTESIAN_POINT('Ctrl Pts',(1.51422500293577,1.34018478089476,13.0854665168065));
#23218=CARTESIAN_POINT('Ctrl Pts',(1.53890976520056,1.39428227099436,13.3099853245802));
#23219=CARTESIAN_POINT('Ctrl Pts',(1.55417473125633,1.40635549640416,13.4521616967641));
#23220=CARTESIAN_POINT('Ctrl Pts',(1.58277681906667,1.38857272398384,13.7172532563586));
#23221=CARTESIAN_POINT('Ctrl Pts',(1.59588733586668,1.3639299051115,13.8391616710263));
#23222=CARTESIAN_POINT('Ctrl Pts',(1.61888907739522,1.29376233059279,14.0427221212447));
#23223=CARTESIAN_POINT('Ctrl Pts',(1.6286552621968,1.25554658577749,14.126075444644));
#23224=CARTESIAN_POINT('Ctrl Pts',(1.64824339761474,1.16347297778776,14.284011208513));
#23225=CARTESIAN_POINT('Ctrl Pts',(1.65803625950705,1.10985864349576,14.3582285694769));
#23226=CARTESIAN_POINT('Ctrl Pts',(1.68755347029578,0.927901482507346,14.5642796080963));
#23227=CARTESIAN_POINT('Ctrl Pts',(1.70686773435893,0.780522374477723,14.6766380391314));
#23228=CARTESIAN_POINT('Ctrl Pts',(1.73623813954844,0.534872879558241,14.7969210847266));
#23229=CARTESIAN_POINT('Ctrl Pts',(1.74590859244064,0.450449288583891,14.8286042597794));
#23230=CARTESIAN_POINT('Ctrl Pts',(1.76519305260318,0.27659512533074,14.8753569881007));
#23231=CARTESIAN_POINT('Ctrl Pts',(1.77479216187826,0.187565754538626,14.8902988283207));
#23232=CARTESIAN_POINT('Ctrl Pts',(1.79417060446524,0.0071422485920177,
14.9029232059173));
#23233=CARTESIAN_POINT('Ctrl Pts',(1.80390303357478,-0.0838383583836259,
14.9004341828375));
#23234=CARTESIAN_POINT('Ctrl Pts',(1.82328449409847,-0.263534104947346,
14.8779345155732));
#23235=CARTESIAN_POINT('Ctrl Pts',(1.83290954613354,-0.351836618136786,
14.8580738231442));
#23236=CARTESIAN_POINT('Ctrl Pts',(1.85231855018614,-0.523817649789653,
14.8014806159072));
#23237=CARTESIAN_POINT('Ctrl Pts',(1.86205654006245,-0.607064073991918,
14.7647964320767));
#23238=CARTESIAN_POINT('Ctrl Pts',(1.88150900832868,-0.76529633500339,14.6758237571641));
#23239=CARTESIAN_POINT('Ctrl Pts',(1.89119673559068,-0.839905901416373,
14.6237429072962));
#23240=CARTESIAN_POINT('Ctrl Pts',(1.91071720391687,-0.978460482517055,
14.505469172187));
#23241=CARTESIAN_POINT('Ctrl Pts',(1.92048812916967,-1.04199674537574,14.4394658315659));
#23242=CARTESIAN_POINT('Ctrl Pts',(1.94994329715363,-1.21245600572361,14.2236480957466));
#23243=CARTESIAN_POINT('Ctrl Pts',(1.96951967562116,-1.29681486411763,14.058558569738));
#23244=CARTESIAN_POINT('Ctrl Pts',(2.00441118245624,-1.38579273892104,13.7447485931775));
#23245=CARTESIAN_POINT('Ctrl Pts',(2.01950536501099,-1.40350427074367,13.6024594297712));
#23246=CARTESIAN_POINT('Ctrl Pts',(2.0444644722023,-1.39685941518724,13.3702059476167));
#23247=CARTESIAN_POINT('Ctrl Pts',(2.05412297400445,-1.38566229137934,13.2809033073099));
#23248=CARTESIAN_POINT('Ctrl Pts',(2.07236012816617,-1.34835985142555,13.114770747565));
#23249=CARTESIAN_POINT('Ctrl Pts',(2.08093204423063,-1.32399268173303,13.0379183062463));
#23250=CARTESIAN_POINT('Ctrl Pts',(2.09930330238021,-1.25818800648483,12.8792800237421));
#23251=CARTESIAN_POINT('Ctrl Pts',(2.10907328381213,-1.21505694275106,12.7985966563273));
#23252=CARTESIAN_POINT('Ctrl Pts',(2.12849960866751,-1.11435028434478,12.6477420840303));
#23253=CARTESIAN_POINT('Ctrl Pts',(2.13810698755743,-1.0571992888945,12.5778017232459));
#23254=CARTESIAN_POINT('Ctrl Pts',(2.15750276471468,-0.929763103826513,
12.4493878627635));
#23255=CARTESIAN_POINT('Ctrl Pts',(2.16724806963363,-0.859682219986245,
12.3913108074149));
#23256=CARTESIAN_POINT('Ctrl Pts',(2.19165096222075,-0.67107647846954,12.2637150953956));
#23257=CARTESIAN_POINT('Ctrl Pts',(2.20615776602033,-0.54708858513539,12.2040817707949));
#23258=CARTESIAN_POINT('Ctrl Pts',(2.22083974265588,-0.416497439768571,
12.1633886568392));
#23259=CARTESIAN_POINT('Ctrl Pts',(2.40093257836374,-0.416497469208933,
12.163388666013));
#23260=CARTESIAN_POINT('Ctrl Pts',(2.3942679260537,-0.475789056022099,12.1818643404481));
#23261=CARTESIAN_POINT('Ctrl Pts',(2.3876098108882,-0.533827934293694,12.2042780440777));
#23262=CARTESIAN_POINT('Ctrl Pts',(2.36685390738263,-0.709184394622676,
12.285805323635));
#23263=CARTESIAN_POINT('Ctrl Pts',(2.3527720126406,-0.819788955100745,12.3575640409707));
#23264=CARTESIAN_POINT('Ctrl Pts',(2.32196013711664,-1.03777754350177,12.5471676522693));
#23265=CARTESIAN_POINT('Ctrl Pts',(2.30536793090488,-1.13842662625283,12.6700281321853));
#23266=CARTESIAN_POINT('Ctrl Pts',(2.27942573841901,-1.25778282043891,12.8795602954755));
#23267=CARTESIAN_POINT('Ctrl Pts',(2.27041266920003,-1.29251910490724,12.9556133187173));
#23268=CARTESIAN_POINT('Ctrl Pts',(2.25165158192398,-1.35037421679487,13.1196356318881));
#23269=CARTESIAN_POINT('Ctrl Pts',(2.24199800499422,-1.3721307398421,13.2076879561223));
#23270=CARTESIAN_POINT('Ctrl Pts',(2.21274112166428,-1.41179852640499,13.4786777448907));
#23271=CARTESIAN_POINT('Ctrl Pts',(2.19331161153257,-1.40245000186556,13.6635882072515));
#23272=CARTESIAN_POINT('Ctrl Pts',(2.16398044318386,-1.33570747042758,13.9289974853134));
#23273=CARTESIAN_POINT('Ctrl Pts',(2.15429101166608,-1.30526626220759,14.014230366182));
#23274=CARTESIAN_POINT('Ctrl Pts',(2.13492457891323,-1.22848069206958,14.1774602022811));
#23275=CARTESIAN_POINT('Ctrl Pts',(2.12533659082138,-1.18234924039453,14.2550948763787));
#23276=CARTESIAN_POINT('Ctrl Pts',(2.09659716247621,-1.02317339201938,14.4722133868433));
#23277=CARTESIAN_POINT('Ctrl Pts',(2.07743672410967,-0.890526978712175,
14.5950077189689));
#23278=CARTESIAN_POINT('Ctrl Pts',(2.05337558622913,-0.699595503347848,
14.7135266609751));
#23279=CARTESIAN_POINT('Ctrl Pts',(2.04850445727977,-0.659686081635776,
14.73567600164));
#23280=CARTESIAN_POINT('Ctrl Pts',(2.02397082167762,-0.453799667660683,
14.8371187382518));
#23281=CARTESIAN_POINT('Ctrl Pts',(2.00437023026017,-0.274422283731444,
14.8851040943022));
#23282=CARTESIAN_POINT('Ctrl Pts',(1.97493918266089,0.000437004015423861,
14.9029891737956));
#23283=CARTESIAN_POINT('Ctrl Pts',(1.96517813060858,0.0921405430985885,
14.8999600698876));
#23284=CARTESIAN_POINT('Ctrl Pts',(1.94558496699582,0.273177956461229,14.8761059608175));
#23285=CARTESIAN_POINT('Ctrl Pts',(1.93580459714485,0.362093112473848,14.8554271781499));
#23286=CARTESIAN_POINT('Ctrl Pts',(1.91627695806057,0.534844137746019,14.7970251990701));
#23287=CARTESIAN_POINT('Ctrl Pts',(1.90654738375972,0.618252854745831,14.7594030249013));
#23288=CARTESIAN_POINT('Ctrl Pts',(1.88698003020699,0.776588871269993,14.6684389306091));
#23289=CARTESIAN_POINT('Ctrl Pts',(1.87719230806854,0.851134107596775,14.615307554439));
#23290=CARTESIAN_POINT('Ctrl Pts',(1.86255386709511,0.95430049655303,14.5253704040316));
#23291=CARTESIAN_POINT('Ctrl Pts',(1.85769220445115,0.987147379380306,14.4937876919291));
#23292=CARTESIAN_POINT('Ctrl Pts',(1.83342093916487,1.14292514580336,14.3286476146511));
#23293=CARTESIAN_POINT('Ctrl Pts',(1.81405632478123,1.24060384114422,14.1736732899444));
#23294=CARTESIAN_POINT('Ctrl Pts',(1.78485771682689,1.33886019962667,13.9192612648863));
#23295=CARTESIAN_POINT('Ctrl Pts',(1.77513100297321,1.36333430114081,13.8311285134366));
#23296=CARTESIAN_POINT('Ctrl Pts',(1.75555071726262,1.39481470298217,13.6511723335134));
#23297=CARTESIAN_POINT('Ctrl Pts',(1.74575167681533,1.40170907790057,13.5597733543252));
#23298=CARTESIAN_POINT('Ctrl Pts',(1.72615648732792,1.39757523499232,13.3769231235782));
#23299=CARTESIAN_POINT('Ctrl Pts',(1.71638039675177,1.38655345072885,13.2859112806918));
#23300=CARTESIAN_POINT('Ctrl Pts',(1.69690518488617,1.34716398179204,13.1084565694359));
#23301=CARTESIAN_POINT('Ctrl Pts',(1.68724354472194,1.31910639494897,13.0223857576645));
#23302=CARTESIAN_POINT('Ctrl Pts',(1.67269223440346,1.26470051115681,12.8978268208691));
#23303=CARTESIAN_POINT('Ctrl Pts',(1.66782223879557,1.24441422456665,12.8569500556959));
#23304=CARTESIAN_POINT('Ctrl Pts',(1.64637722897859,1.1465645019785,12.6818215784041));
#23305=CARTESIAN_POINT('Ctrl Pts',(1.62980792907299,1.04901018847223,12.5599989844274));
#23306=CARTESIAN_POINT('Ctrl Pts',(1.60831216041011,0.899479242881735,12.4262119475076));
#23307=CARTESIAN_POINT('Ctrl Pts',(1.6034369151753,0.86399168139286,12.3974564960722));
#23308=CARTESIAN_POINT('Ctrl Pts',(1.58124002742741,0.696442070404857,12.2747570532381));
#23309=CARTESIAN_POINT('Ctrl Pts',(1.56393722882228,0.550091032214942,12.2024446972363));
#23310=CARTESIAN_POINT('Ctrl Pts',(1.54168997577148,0.350850647229146,12.1439073992733));
#23311=CARTESIAN_POINT('Ctrl Pts',(1.53681457014148,0.306454612382846,12.1331902129952));
#23312=CARTESIAN_POINT('Ctrl Pts',(1.51462781442213,0.10256795488322,12.0944073277006));
#23313=CARTESIAN_POINT('Ctrl Pts',(1.49733357660129,-0.0605264833183406,
12.0919708883101));
#23314=CARTESIAN_POINT('Ctrl Pts',(1.47511125510869,-0.265463597988811,
12.1246413840912));
#23315=CARTESIAN_POINT('Ctrl Pts',(1.47023957074921,-0.31014865132287,12.1340240986041));
#23316=CARTESIAN_POINT('Ctrl Pts',(1.46305678534565,-0.375181790474972,
12.1510356975939));
#23317=CARTESIAN_POINT('Ctrl Pts',(1.46075201473401,-0.395920905392733,
12.1569768639781));
#23318=CARTESIAN_POINT('Ctrl Pts',(1.45844776950582,-0.416497492092995,
12.1633886731438));
#23319=CARTESIAN_POINT('Origin',(0.,0.,13.5));
#23320=CARTESIAN_POINT('',(0.335948685957609,-0.416497449525761,12.1633886598796));
#23321=CARTESIAN_POINT('',(0.51591329100944,-0.416497503173569,12.1633886765966));
#23322=CARTESIAN_POINT('',(0.,-0.416497449530544,12.1633886598811));
#23323=CARTESIAN_POINT('Ctrl Pts',(0.33594868595761,-0.41649744952576,12.1633886598796));
#23324=CARTESIAN_POINT('Ctrl Pts',(0.338092137022063,-0.397430723115034,
12.1574473344676));
#23325=CARTESIAN_POINT('Ctrl Pts',(0.340232102393261,-0.378231240764015,
12.1519122386787));
#23326=CARTESIAN_POINT('Ctrl Pts',(0.355812558107325,-0.237457708666163,
12.1145748990151));
#23327=CARTESIAN_POINT('Ctrl Pts',(0.369115667260259,-0.112219229772241,
12.0988592976413));
#23328=CARTESIAN_POINT('Ctrl Pts',(0.392254665094067,0.103470382396172,
12.1009280078));
#23329=CARTESIAN_POINT('Ctrl Pts',(0.401944321812012,0.19321951081267,12.1104769948009));
#23330=CARTESIAN_POINT('Ctrl Pts',(0.429305497035372,0.442459199927157,
12.1616227618598));
#23331=CARTESIAN_POINT('Ctrl Pts',(0.446618745266285,0.596421336295759,
12.222773843572));
#23332=CARTESIAN_POINT('Ctrl Pts',(0.473903955602125,0.812774735809414,
12.3565435122433));
#23333=CARTESIAN_POINT('Ctrl Pts',(0.483577366325789,0.884563388325348,
12.4111276384374));
#23334=CARTESIAN_POINT('Ctrl Pts',(0.499640090606945,0.994534335407759,
12.5128422998071));
#23335=CARTESIAN_POINT('Ctrl Pts',(0.506017782138323,1.03580385112511,12.5562365973114));
#23336=CARTESIAN_POINT('Ctrl Pts',(0.53199673668229,1.19139469283705,12.7423800946747));
#23337=CARTESIAN_POINT('Ctrl Pts',(0.551404636661235,1.28002686676363,12.9042313657085));
#23338=CARTESIAN_POINT('Ctrl Pts',(0.575879097201786,1.34880308277725,13.1220893768416));
#23339=CARTESIAN_POINT('Ctrl Pts',(0.580766698942489,1.36041365575882,13.1662922129466));
#23340=CARTESIAN_POINT('Ctrl Pts',(0.590553404302888,1.37927566207682,13.2556918339382));
#23341=CARTESIAN_POINT('Ctrl Pts',(0.595446882381403,1.38651405868556,13.3008352938842));
#23342=CARTESIAN_POINT('Ctrl Pts',(0.60523878008134,1.39655005696943,13.3916681562918));
#23343=CARTESIAN_POINT('Ctrl Pts',(0.610129967868918,1.39934162048136,13.4373032431323));
#23344=CARTESIAN_POINT('Ctrl Pts',(0.619920599759535,1.40045172493147,13.5286787763786));
#23345=CARTESIAN_POINT('Ctrl Pts',(0.624814422836377,1.39876997354232,13.5743644686515));
#23346=CARTESIAN_POINT('Ctrl Pts',(0.639475059197237,1.38705003220774,13.7107244634538));
#23347=CARTESIAN_POINT('Ctrl Pts',(0.649206048549967,1.37038764506943,13.8005830608694));
#23348=CARTESIAN_POINT('Ctrl Pts',(0.663871512140508,1.33245393080345,13.9320292970078));
#23349=CARTESIAN_POINT('Ctrl Pts',(0.668763870510218,1.31766337636763,13.9752326059005));
#23350=CARTESIAN_POINT('Ctrl Pts',(0.683389203926127,1.26720104388982,14.1020414657331));
#23351=CARTESIAN_POINT('Ctrl Pts',(0.693084241148559,1.22547720712379,14.182977295026));
#23352=CARTESIAN_POINT('Ctrl Pts',(0.707714908290906,1.15145876403461,14.2976371985038));
#23353=CARTESIAN_POINT('Ctrl Pts',(0.712607191073157,1.12484960903662,14.3347429304424));
#23354=CARTESIAN_POINT('Ctrl Pts',(0.727225623704985,1.04002533502238,14.4415891269759));
#23355=CARTESIAN_POINT('Ctrl Pts',(0.736899857886182,0.97679134081702,14.5070360362464));
#23356=CARTESIAN_POINT('Ctrl Pts',(0.756396983623417,0.838164987882815,
14.6250835129975));
#23357=CARTESIAN_POINT('Ctrl Pts',(0.766173387598592,0.763040411002447,
14.6773285986624));
#23358=CARTESIAN_POINT('Ctrl Pts',(0.795621374482452,0.523215582157543,
14.8114558805551));
#23359=CARTESIAN_POINT('Ctrl Pts',(0.815191282547029,0.347000479778492,
14.8686730293357));
#23360=CARTESIAN_POINT('Ctrl Pts',(0.844409565680878,0.0748791223030258,
14.9009234741048));
#23361=CARTESIAN_POINT('Ctrl Pts',(0.854031190077165,-0.0158285778211942,
14.9028335972271));
#23362=CARTESIAN_POINT('Ctrl Pts',(0.872199699440062,-0.184895990780581,
14.8899859897267));
#23363=CARTESIAN_POINT('Ctrl Pts',(0.880694956781953,-0.263059204620027,
14.8773331552573));
#23364=CARTESIAN_POINT('Ctrl Pts',(0.908999943449859,-0.517933496143129,
14.8135780149835));
#23365=CARTESIAN_POINT('Ctrl Pts',(0.92842488150862,-0.685636395733855,
14.7343618976148));
#23366=CARTESIAN_POINT('Ctrl Pts',(0.957892544291619,-0.906734517687264,
14.5706040444889));
#23367=CARTESIAN_POINT('Ctrl Pts',(0.967663928233954,-0.97470328053528,
14.5091154198522));
#23368=CARTESIAN_POINT('Ctrl Pts',(0.987261220477669,-1.09768780537988,
14.3737534516641));
#23369=CARTESIAN_POINT('Ctrl Pts',(0.997027096616553,-1.15240592287781,
14.3002026136494));
#23370=CARTESIAN_POINT('Ctrl Pts',(1.01662000331737,-1.2466914968752,14.1435188180007));
#23371=CARTESIAN_POINT('Ctrl Pts',(1.02639719284007,-1.28603939852387,14.0607662365323));
#23372=CARTESIAN_POINT('Ctrl Pts',(1.04598492052491,-1.34802389003489,13.888818195646));
#23373=CARTESIAN_POINT('Ctrl Pts',(1.0557199396963,-1.37052024212579,13.8000374920693));
#23374=CARTESIAN_POINT('Ctrl Pts',(1.07038622751275,-1.39104982008156,13.6645238239822));
#23375=CARTESIAN_POINT('Ctrl Pts',(1.07527834582645,-1.39567792843094,13.619040724484));
#23376=CARTESIAN_POINT('Ctrl Pts',(1.08989561361535,-1.40282341212471,13.4829635874722));
#23377=CARTESIAN_POINT('Ctrl Pts',(1.09961197157324,-1.39878420382174,13.3922647135418));
#23378=CARTESIAN_POINT('Ctrl Pts',(1.11418923719126,-1.37958955273921,13.2574973538008));
#23379=CARTESIAN_POINT('Ctrl Pts',(1.11906060732706,-1.37096964926112,13.2127421404134));
#23380=CARTESIAN_POINT('Ctrl Pts',(1.13369038436817,-1.33862874088626,13.0800487859611));
#23381=CARTESIAN_POINT('Ctrl Pts',(1.14343021921865,-1.30849982164006,12.9939225852327));
#23382=CARTESIAN_POINT('Ctrl Pts',(1.16287424891295,-1.23209947466277,12.8290662240178));
#23383=CARTESIAN_POINT('Ctrl Pts',(1.17254497351587,-1.18607288397003,12.7506989625543));
#23384=CARTESIAN_POINT('Ctrl Pts',(1.1919948476445,-1.07948530677624,12.6039299282727));
#23385=CARTESIAN_POINT('Ctrl Pts',(1.201720950175,-1.01916717323023,12.5358793063566));
#23386=CARTESIAN_POINT('Ctrl Pts',(1.22114976917045,-0.886187310618468,
12.4123837972148));
#23387=CARTESIAN_POINT('Ctrl Pts',(1.23083383566112,-0.813836349809595,
12.3572370346479));
#23388=CARTESIAN_POINT('Ctrl Pts',(1.25320840746357,-0.636295706514283,
12.2473798016744));
#23389=CARTESIAN_POINT('Ctrl Pts',(1.26579107429575,-0.528695691748085,
12.1983504123869));
#23390=CARTESIAN_POINT('Ctrl Pts',(1.27841053848688,-0.41649739383476,12.1633886425259));
#23391=CARTESIAN_POINT('Ctrl Pts',(1.45844776950582,-0.416497492092994,
12.1633886731438));
#23392=CARTESIAN_POINT('Ctrl Pts',(1.44390140370835,-0.546394498428389,
12.2038654941029));
#23393=CARTESIAN_POINT('Ctrl Pts',(1.42932090092249,-0.66980860421863,12.2630972886968));
#23394=CARTESIAN_POINT('Ctrl Pts',(1.40497113230301,-0.858142498666153,
12.3901120941702));
#23395=CARTESIAN_POINT('Ctrl Pts',(1.39529191720086,-0.928364884453008,
12.4481451379525));
#23396=CARTESIAN_POINT('Ctrl Pts',(1.37589278928849,-1.0561522778362,12.5765847592017));
#23397=CARTESIAN_POINT('Ctrl Pts',(1.36621708162912,-1.11349612870909,12.6466070920168));
#23398=CARTESIAN_POINT('Ctrl Pts',(1.35165264523808,-1.18905132560126,12.7595697679454));
#23399=CARTESIAN_POINT('Ctrl Pts',(1.34677567923691,-1.21253937447488,12.7986952875696));
#23400=CARTESIAN_POINT('Ctrl Pts',(1.3266664764074,-1.30123595698637,12.9642646260475));
#23401=CARTESIAN_POINT('Ctrl Pts',(1.31143822683817,-1.34890190962999,13.099137562112));
#23402=CARTESIAN_POINT('Ctrl Pts',(1.29132750458486,-1.38394639101076,13.2837200195658));
#23403=CARTESIAN_POINT('Ctrl Pts',(1.28645640659027,-1.39026346900012,13.3289670970169));
#23404=CARTESIAN_POINT('Ctrl Pts',(1.26164462562856,-1.41110536175855,13.5604230724584));
#23405=CARTESIAN_POINT('Ctrl Pts',(1.24171274821886,-1.39047412541093,13.7478856871491));
#23406=CARTESIAN_POINT('Ctrl Pts',(1.21196375405839,-1.30604124250456,14.0123677418593));
#23407=CARTESIAN_POINT('Ctrl Pts',(1.20229122750465,-1.27002421989132,14.0960732585933));
#23408=CARTESIAN_POINT('Ctrl Pts',(1.18279514596295,-1.18206371535408,14.2556903818919));
#23409=CARTESIAN_POINT('Ctrl Pts',(1.17302428235503,-1.13025820137227,14.3311790212574));
#23410=CARTESIAN_POINT('Ctrl Pts',(1.15343684225622,-1.01265757072314,14.4710174152128));
#23411=CARTESIAN_POINT('Ctrl Pts',(1.14367565859755,-0.947136867220968,
14.5350275439779));
#23412=CARTESIAN_POINT('Ctrl Pts',(1.12414012684928,-0.804903306426751,
14.6490867902023));
#23413=CARTESIAN_POINT('Ctrl Pts',(1.11440175457461,-0.72858366905622,14.6989311100021));
#23414=CARTESIAN_POINT('Ctrl Pts',(1.09491224012219,-0.567171507992726,
14.7832088066028));
#23415=CARTESIAN_POINT('Ctrl Pts',(1.08520084686711,-0.48244522490888,14.8174045751253));
#23416=CARTESIAN_POINT('Ctrl Pts',(1.06576506079662,-0.308447106548023,
14.8685757280464));
#23417=CARTESIAN_POINT('Ctrl Pts',(1.05608578405447,-0.219637104216404,
14.88560406286));
#23418=CARTESIAN_POINT('Ctrl Pts',(1.04152804715565,-0.084374639456373,
14.8981999478329));
#23419=CARTESIAN_POINT('Ctrl Pts',(1.03665029630423,-0.0387602206887427,
14.9002070899748));
#23420=CARTESIAN_POINT('Ctrl Pts',(1.02199519541023,0.0982033775170876,
14.8995348936809));
#23421=CARTESIAN_POINT('Ctrl Pts',(1.01222986789598,0.189271681394011,14.8901501746134));
#23422=CARTESIAN_POINT('Ctrl Pts',(0.982826771131795,0.457798104227207,
14.8355875198765));
#23423=CARTESIAN_POINT('Ctrl Pts',(0.963568332078361,0.627983659964473,
14.7645194167979));
#23424=CARTESIAN_POINT('Ctrl Pts',(0.939048234817051,0.817635902210224,
14.637346262212));
#23425=CARTESIAN_POINT('Ctrl Pts',(0.934139659251513,0.854293238047118,
14.610075661621));
#23426=CARTESIAN_POINT('Ctrl Pts',(0.909573582717069,1.0306746403647,14.4649403458635));
#23427=CARTESIAN_POINT('Ctrl Pts',(0.890268741296078,1.14770538454531,14.3222983994732));
#23428=CARTESIAN_POINT('Ctrl Pts',(0.860853984559888,1.27727792581275,14.0804734489303));
#23429=CARTESIAN_POINT('Ctrl Pts',(0.851063086401508,1.31250714136801,13.9956944862125));
#23430=CARTESIAN_POINT('Ctrl Pts',(0.831247961053441,1.36628502388815,13.8192130425103));
#23431=CARTESIAN_POINT('Ctrl Pts',(0.821260870522121,1.38445311748892,13.7278637351812));
#23432=CARTESIAN_POINT('Ctrl Pts',(0.791622230502018,1.41124680096498,13.4521001652212));
#23433=CARTESIAN_POINT('Ctrl Pts',(0.772309782213003,1.3927180268365,13.2670917214919));
#23434=CARTESIAN_POINT('Ctrl Pts',(0.747567348924004,1.32559012452433,13.0473499858023));
#23435=CARTESIAN_POINT('Ctrl Pts',(0.742646789672397,1.31013735305008,13.0043981120919));
#23436=CARTESIAN_POINT('Ctrl Pts',(0.718228233628566,1.22321168507718,12.7954398106915));
#23437=CARTESIAN_POINT('Ctrl Pts',(0.699178436344836,1.12215614097056,12.643598446638));
#23438=CARTESIAN_POINT('Ctrl Pts',(0.670085606053116,0.930779510263475,
12.4502420779579));
#23439=CARTESIAN_POINT('Ctrl Pts',(0.660337607383824,0.860331074096645,
12.3917707444403));
#23440=CARTESIAN_POINT('Ctrl Pts',(0.637622694486556,0.684965571709589,
12.2730837732651));
#23441=CARTESIAN_POINT('Ctrl Pts',(0.624671890713921,0.576943551247466,
12.2187355726817));
#23442=CARTESIAN_POINT('Ctrl Pts',(0.602204515054362,0.378628769124433,
12.1491884842473));
#23443=CARTESIAN_POINT('Ctrl Pts',(0.592687701417284,0.291294760816019,
12.1277029502485));
#23444=CARTESIAN_POINT('Ctrl Pts',(0.563970789415144,0.025163055150938,
12.0887985245306));
#23445=CARTESIAN_POINT('Ctrl Pts',(0.544733641290613,-0.155515562515679,
12.0971688025917));
#23446=CARTESIAN_POINT('Ctrl Pts',(0.52232947888016,-0.358895607883152,
12.1464503794261));
#23447=CARTESIAN_POINT('Ctrl Pts',(0.519120376922039,-0.387843916658138,
12.1544600172087));
#23448=CARTESIAN_POINT('Ctrl Pts',(0.515913291009439,-0.416497503173569,
12.1633886765966));
#23449=CARTESIAN_POINT('Origin',(0.,0.,13.5));
#23450=CARTESIAN_POINT('',(-0.606544106580495,-0.416497449298501,12.1633886598088));
#23451=CARTESIAN_POINT('',(-0.426566464895915,-0.416497451671886,12.1633886605483));
#23452=CARTESIAN_POINT('',(0.,-0.416497449530544,12.1633886598811));
#23453=CARTESIAN_POINT('Ctrl Pts',(-0.606544106580495,-0.416497449298501,
12.1633886598088));
#23454=CARTESIAN_POINT('Ctrl Pts',(-0.601905488457186,-0.375006509663048,
12.1504597925999));
#23455=CARTESIAN_POINT('Ctrl Pts',(-0.597278269205687,-0.33293461748609,
12.1394694228009));
#23456=CARTESIAN_POINT('Ctrl Pts',(-0.582914697219095,-0.201117435002572,
12.1115170003321));
#23457=CARTESIAN_POINT('Ctrl Pts',(-0.57318643731515,-0.110182143195263,
12.1013607375965));
#23458=CARTESIAN_POINT('Ctrl Pts',(-0.553446929682907,0.0735757584082064,
12.0988782990464));
#23459=CARTESIAN_POINT('Ctrl Pts',(-0.54348018098935,0.165959238117452,
12.106797694933));
#23460=CARTESIAN_POINT('Ctrl Pts',(-0.523806474452879,0.345932180485655,
12.140390867513));
#23461=CARTESIAN_POINT('Ctrl Pts',(-0.514163696021878,0.433160474790576,
12.1656166336715));
#23462=CARTESIAN_POINT('Ctrl Pts',(-0.494700198953667,0.602343600699843,
12.2328968501379));
#23463=CARTESIAN_POINT('Ctrl Pts',(-0.484926277070032,0.68382862997349,
12.274950451567));
#23464=CARTESIAN_POINT('Ctrl Pts',(-0.470256490022007,0.798912786317021,
12.3494270619555));
#23465=CARTESIAN_POINT('Ctrl Pts',(-0.465378379653816,0.835965197363722,
12.3760596745377));
#23466=CARTESIAN_POINT('Ctrl Pts',(-0.450806540735884,0.94238070263997,
12.4607271465437));
#23467=CARTESIAN_POINT('Ctrl Pts',(-0.441114127584034,1.00749393308657,
12.523718727768));
#23468=CARTESIAN_POINT('Ctrl Pts',(-0.421637519360729,1.12516184376022,
12.6619549708284));
#23469=CARTESIAN_POINT('Ctrl Pts',(-0.411917585888672,1.17732541969383,
12.7369706621761));
#23470=CARTESIAN_POINT('Ctrl Pts',(-0.397263403204919,1.24410900676983,
12.8563571984881));
#23471=CARTESIAN_POINT('Ctrl Pts',(-0.392372898074839,1.26443035750525,
12.8972570085663));
#23472=CARTESIAN_POINT('Ctrl Pts',(-0.377693102703635,1.31929797812323,
13.0227279275616));
#23473=CARTESIAN_POINT('Ctrl Pts',(-0.367948862541147,1.34760789891663,
13.1097580647508));
#23474=CARTESIAN_POINT('Ctrl Pts',(-0.353273452437169,1.37705457699646,
13.2434802862271));
#23475=CARTESIAN_POINT('Ctrl Pts',(-0.348382685477986,1.38468248994158,
13.2884910085762));
#23476=CARTESIAN_POINT('Ctrl Pts',(-0.338592869039751,1.39552242749479,
13.3791528265224));
#23477=CARTESIAN_POINT('Ctrl Pts',(-0.333702520235257,1.3987224381974,13.4247506469136));
#23478=CARTESIAN_POINT('Ctrl Pts',(-0.31901389140055,1.4016192986816,13.5618417327739));
#23479=CARTESIAN_POINT('Ctrl Pts',(-0.309236318680863,1.39459013493301,
13.6532297388385));
#23480=CARTESIAN_POINT('Ctrl Pts',(-0.294543086364255,1.37076269807332,
13.7882646719869));
#23481=CARTESIAN_POINT('Ctrl Pts',(-0.289652656692205,1.36062728265345,
13.8328367382274));
#23482=CARTESIAN_POINT('Ctrl Pts',(-0.274958173542438,1.32371463845123,
13.9649122781796));
#23483=CARTESIAN_POINT('Ctrl Pts',(-0.265177775503078,1.29052677984863,
14.0503676019019));
#23484=CARTESIAN_POINT('Ctrl Pts',(-0.250484024407631,1.22862612997252,
14.172728679251));
#23485=CARTESIAN_POINT('Ctrl Pts',(-0.245591449054255,1.20602678094004,
14.2124503065406));
#23486=CARTESIAN_POINT('Ctrl Pts',(-0.235809207093606,1.15706239937249,
14.2894849551875));
#23487=CARTESIAN_POINT('Ctrl Pts',(-0.230928306990082,1.13073216643731,
14.326755504826));
#23488=CARTESIAN_POINT('Ctrl Pts',(-0.216285894299332,1.04652533933224,
14.4343847291161));
#23489=CARTESIAN_POINT('Ctrl Pts',(-0.206512619347025,0.983557927149029,
14.5004521250684));
#23490=CARTESIAN_POINT('Ctrl Pts',(-0.187095300662516,0.846029882079955,
14.6191253457583));
#23491=CARTESIAN_POINT('Ctrl Pts',(-0.177461575585183,0.771854941797795,
14.6715151752137));
#23492=CARTESIAN_POINT('Ctrl Pts',(-0.1523894013015,0.568451047806307,14.7874236212691));
#23493=CARTESIAN_POINT('Ctrl Pts',(-0.136960075163453,0.433573633496984,
14.8388842178022));
#23494=CARTESIAN_POINT('Ctrl Pts',(-0.112009582165764,0.205348834270106,
14.8877720473929));
#23495=CARTESIAN_POINT('Ctrl Pts',(-0.10246771960711,0.115847909542865,
14.8980911195459));
#23496=CARTESIAN_POINT('Ctrl Pts',(-0.0790818126658175,-0.102882316765015,
14.9021503972281));
#23497=CARTESIAN_POINT('Ctrl Pts',(-0.0652493200739028,-0.231453906580911,
14.8867361917234));
#23498=CARTESIAN_POINT('Ctrl Pts',(-0.0418508851995083,-0.442188056310697,
14.8313135019221));
#23499=CARTESIAN_POINT('Ctrl Pts',(-0.0323988608236905,-0.525933210372259,
14.8005080645975));
#23500=CARTESIAN_POINT('Ctrl Pts',(-0.0037040324834651,-0.768649969783498,
14.6839177890224));
#23501=CARTESIAN_POINT('Ctrl Pts',(0.0155776225967351,-0.914514945141154,
14.5752380582826));
#23502=CARTESIAN_POINT('Ctrl Pts',(0.0446595079971736,-1.0962344430835,
14.3754142026245));
#23503=CARTESIAN_POINT('Ctrl Pts',(0.0542063633042762,-1.15016838717273,
14.303240073177));
#23504=CARTESIAN_POINT('Ctrl Pts',(0.0758893164280386,-1.2560581069539,
14.1287738615946));
#23505=CARTESIAN_POINT('Ctrl Pts',(0.0879925333356952,-1.30313504295692,
14.0242845872087));
#23506=CARTESIAN_POINT('Ctrl Pts',(0.112234309053797,-1.36998634282861,
13.8090405622336));
#23507=CARTESIAN_POINT('Ctrl Pts',(0.124280390147709,-1.39019951632661,
13.699279640849));
#23508=CARTESIAN_POINT('Ctrl Pts',(0.145772293821565,-1.40275690694015,
13.5005638594427));
#23509=CARTESIAN_POINT('Ctrl Pts',(0.15512101706407,-1.40002642418665,13.4125026890467));
#23510=CARTESIAN_POINT('Ctrl Pts',(0.172561160499419,-1.37950805013817,
13.2493865276265));
#23511=CARTESIAN_POINT('Ctrl Pts',(0.180645864754135,-1.3637604292113,13.174413425371));
#23512=CARTESIAN_POINT('Ctrl Pts',(0.201537058586901,-1.30786707793749,
12.9863765421109));
#23513=CARTESIAN_POINT('Ctrl Pts',(0.214368119941527,-1.25919610294344,
12.8765055454839));
#23514=CARTESIAN_POINT('Ctrl Pts',(0.237031423027273,-1.15055531918141,
12.6973159661113));
#23515=CARTESIAN_POINT('Ctrl Pts',(0.246734793056764,-1.09665714528703,
12.6251142358414));
#23516=CARTESIAN_POINT('Ctrl Pts',(0.275519091084943,-0.915499506244006,
12.42571825934));
#23517=CARTESIAN_POINT('Ctrl Pts',(0.294374707439548,-0.770366427214801,
12.3173108041002));
#23518=CARTESIAN_POINT('Ctrl Pts',(0.32111414060799,-0.546585086849063,
12.2092611808737));
#23519=CARTESIAN_POINT('Ctrl Pts',(0.328547651546869,-0.482332168407897,
12.18390321911));
#23520=CARTESIAN_POINT('Ctrl Pts',(0.335948685957608,-0.416497449525761,
12.1633886598796));
#23521=CARTESIAN_POINT('Ctrl Pts',(0.515913291009439,-0.41649750317357,
12.1633886765966));
#23522=CARTESIAN_POINT('Ctrl Pts',(0.509385662631614,-0.474818349437701,
12.1815618630919));
#23523=CARTESIAN_POINT('Ctrl Pts',(0.502864638142664,-0.531918062096211,
12.203542253374));
#23524=CARTESIAN_POINT('Ctrl Pts',(0.476756448285556,-0.753481412729099,
12.3059597836098));
#23525=CARTESIAN_POINT('Ctrl Pts',(0.457267808032133,-0.902892290928627,
12.4145270387944));
#23526=CARTESIAN_POINT('Ctrl Pts',(0.427915708355189,-1.08929367372358,
12.6158094276354));
#23527=CARTESIAN_POINT('Ctrl Pts',(0.418168647906485,-1.14467899180946,
12.688788970831));
#23528=CARTESIAN_POINT('Ctrl Pts',(0.403475540394033,-1.21646022311045,
12.8055166231118));
#23529=CARTESIAN_POINT('Ctrl Pts',(0.398579668370075,-1.23845035331473,
12.8455358563514));
#23530=CARTESIAN_POINT('Ctrl Pts',(0.373982865261525,-1.33888291910941,
13.051568108984));
#23531=CARTESIAN_POINT('Ctrl Pts',(0.354487604621236,-1.38608585555331,
13.2308029737511));
#23532=CARTESIAN_POINT('Ctrl Pts',(0.325084129822677,-1.40296674794631,
13.5052012864122));
#23533=CARTESIAN_POINT('Ctrl Pts',(0.315348432130469,-1.39963998647743,
13.5966967078372));
#23534=CARTESIAN_POINT('Ctrl Pts',(0.295775690609116,-1.37522960445915,
13.7776009944865));
#23535=CARTESIAN_POINT('Ctrl Pts',(0.285989779203554,-1.35422922945079,
13.8665816749947));
#23536=CARTESIAN_POINT('Ctrl Pts',(0.266421317507451,-1.29515206523774,
14.0393867564002));
#23537=CARTESIAN_POINT('Ctrl Pts',(0.256660776143199,-1.25717829009425,
14.1227838801369));
#23538=CARTESIAN_POINT('Ctrl Pts',(0.237071198525041,-1.16550271994426,
14.2810026863609));
#23539=CARTESIAN_POINT('Ctrl Pts',(0.227285202486673,-1.11201669976392,
14.3554417807662));
#23540=CARTESIAN_POINT('Ctrl Pts',(0.207690579985672,-0.991283909256496,
14.492834862049));
#23541=CARTESIAN_POINT('Ctrl Pts',(0.197914985592649,-0.924324804420834,
14.555456496884));
#23542=CARTESIAN_POINT('Ctrl Pts',(0.178363730211615,-0.77956034377627,
14.6664291133161));
#23543=CARTESIAN_POINT('Ctrl Pts',(0.168653455761846,-0.702161868325127,
14.714594487812));
#23544=CARTESIAN_POINT('Ctrl Pts',(0.154931884130335,-0.587493405545037,
14.7713060468275));
#23545=CARTESIAN_POINT('Ctrl Pts',(0.150957159681852,-0.553710047719918,
14.7863796373724));
#23546=CARTESIAN_POINT('Ctrl Pts',(0.127324858889503,-0.349250469145506,
14.8680583278928));
#23547=CARTESIAN_POINT('Ctrl Pts',(0.108116044219979,-0.167433982443867,
14.9019724727693));
#23548=CARTESIAN_POINT('Ctrl Pts',(0.0835087904628999,0.0614075991326112,
14.8993976932663));
#23549=CARTESIAN_POINT('Ctrl Pts',(0.0785922418302401,0.107011311437968,
14.8966507365185));
#23550=CARTESIAN_POINT('Ctrl Pts',(0.0539490465634395,0.334401323629049,
14.8717499795437));
#23551=CARTESIAN_POINT('Ctrl Pts',(0.0346178541707623,0.510744903939716,
14.8163078569111));
#23552=CARTESIAN_POINT('Ctrl Pts',(0.00524394571155688,0.751512883388005,
14.6847193706286));
#23553=CARTESIAN_POINT('Ctrl Pts',(-0.00449437637938378,0.827135223948516,
14.633216073014));
#23554=CARTESIAN_POINT('Ctrl Pts',(-0.0239809671530538,0.966665453230061,
14.5167327070529));
#23555=CARTESIAN_POINT('Ctrl Pts',(-0.0336895932364449,1.03034167195237,
14.4521467881692));
#23556=CARTESIAN_POINT('Ctrl Pts',(-0.0482825683721452,1.11609336739054,
14.3464156472311));
#23557=CARTESIAN_POINT('Ctrl Pts',(-0.053164629659224,1.14309714236796,
14.309575719996));
#23558=CARTESIAN_POINT('Ctrl Pts',(-0.0677481618582202,1.21817300793428,
14.1958885992343));
#23559=CARTESIAN_POINT('Ctrl Pts',(-0.0774376677821613,1.26063801176348,
14.1156280639987));
#23560=CARTESIAN_POINT('Ctrl Pts',(-0.092038069202919,1.31239243389686,
13.989602038624));
#23561=CARTESIAN_POINT('Ctrl Pts',(-0.0969214262161361,1.32765868048064,
13.9465495779731));
#23562=CARTESIAN_POINT('Ctrl Pts',(-0.111558553938572,1.36698955369234,
13.8156386792069));
#23563=CARTESIAN_POINT('Ctrl Pts',(-0.121301079176293,1.38461760607521,
13.726101915061));
#23564=CARTESIAN_POINT('Ctrl Pts',(-0.135956737723329,1.39784990153599,
13.5900170563907));
#23565=CARTESIAN_POINT('Ctrl Pts',(-0.140847394293321,1.40004291833416,
13.5443539040244));
#23566=CARTESIAN_POINT('Ctrl Pts',(-0.150635935487247,1.39995582251888,
13.4529906466906));
#23567=CARTESIAN_POINT('Ctrl Pts',(-0.155528014375707,1.3976771103293,13.4073453936515));
#23568=CARTESIAN_POINT('Ctrl Pts',(-0.165317128395896,1.38866429108346,
13.3164271729165));
#23569=CARTESIAN_POINT('Ctrl Pts',(-0.170208300733083,1.38193418373819,
13.2712088297759));
#23570=CARTESIAN_POINT('Ctrl Pts',(-0.179996367698184,1.36408470341974,
13.1816346357667));
#23571=CARTESIAN_POINT('Ctrl Pts',(-0.184887463766744,1.35298011079629,
13.1373315573546));
#23572=CARTESIAN_POINT('Ctrl Pts',(-0.194676525210845,1.32646843542118,
13.0499227933076));
#23573=CARTESIAN_POINT('Ctrl Pts',(-0.199568583723516,1.31107267433573,
13.0068707570027));
#23574=CARTESIAN_POINT('Ctrl Pts',(-0.224133279370017,1.22341634625858,
12.7950618050139));
#23575=CARTESIAN_POINT('Ctrl Pts',(-0.243582772426096,1.12056594042943,
12.6409215730407));
#23576=CARTESIAN_POINT('Ctrl Pts',(-0.268223405498791,0.958500833830214,
12.4785393669544));
#23577=CARTESIAN_POINT('Ctrl Pts',(-0.273127971641192,0.924505941863352,
12.4476717361654));
#23578=CARTESIAN_POINT('Ctrl Pts',(-0.287763435569983,0.818663282345703,
12.360660590545));
#23579=CARTESIAN_POINT('Ctrl Pts',(-0.297460822492334,0.742790149119399,
12.3098041868957));
#23580=CARTESIAN_POINT('Ctrl Pts',(-0.316837758362703,0.583558266532999,
12.2242675683729));
#23581=CARTESIAN_POINT('Ctrl Pts',(-0.326471785116992,0.500710003383573,
12.1895335380189));
#23582=CARTESIAN_POINT('Ctrl Pts',(-0.355703250292568,0.241025341260821,
12.1089086515452));
#23583=CARTESIAN_POINT('Ctrl Pts',(-0.374841164489171,0.0580452120556191,
12.0893760843612));
#23584=CARTESIAN_POINT('Ctrl Pts',(-0.404054607129763,-0.21295706204091,
12.1133822289271));
#23585=CARTESIAN_POINT('Ctrl Pts',(-0.413718349790429,-0.301412881187743,
12.129886898215));
#23586=CARTESIAN_POINT('Ctrl Pts',(-0.424419123574571,-0.39731761879081,
12.1575249144134));
#23587=CARTESIAN_POINT('Ctrl Pts',(-0.425493451182981,-0.406924727303341,
12.1604057326115));
#23588=CARTESIAN_POINT('Ctrl Pts',(-0.426566464895915,-0.416497451671893,
12.1633886605483));
#23589=CARTESIAN_POINT('Origin',(0.,0.,13.5));
#23590=CARTESIAN_POINT('',(-1.54907858904864,-0.416497429633284,12.1633886536809));
#23591=CARTESIAN_POINT('',(-1.36903602092574,-0.416497450391696,12.1633886601494));
#23592=CARTESIAN_POINT('',(0.,-0.416497449530544,12.1633886598811));
#23593=CARTESIAN_POINT('Ctrl Pts',(-1.54907858904864,-0.416497429633283,
12.1633886536809));
#23594=CARTESIAN_POINT('Ctrl Pts',(-1.5406601768603,-0.341467258642645,
12.1400087284329));
#23595=CARTESIAN_POINT('Ctrl Pts',(-1.53223076875421,-0.264582379274244,
12.1229820008525));
#23596=CARTESIAN_POINT('Ctrl Pts',(-1.51405475451702,-0.0967165221040692,
12.1003995460753));
#23597=CARTESIAN_POINT('Ctrl Pts',(-1.50438038760605,-0.00581264136751285,
12.0970737445648));
#23598=CARTESIAN_POINT('Ctrl Pts',(-1.48499579176796,0.174894239452828,
12.1080359841145));
#23599=CARTESIAN_POINT('Ctrl Pts',(-1.47532269477495,0.264275420538007,
12.1222082992012));
#23600=CARTESIAN_POINT('Ctrl Pts',(-1.4559898682012,0.438783328667831,12.1674949504344));
#23601=CARTESIAN_POINT('Ctrl Pts',(-1.44641307495146,0.523518550496798,
12.1984511731486));
#23602=CARTESIAN_POINT('Ctrl Pts',(-1.41723115468807,0.769798342132802,
12.3163948316969));
#23603=CARTESIAN_POINT('Ctrl Pts',(-1.39765278865023,0.917799738045793,
12.4270818124817));
#23604=CARTESIAN_POINT('Ctrl Pts',(-1.36830303425761,1.10138944928039,12.630935239729));
#23605=CARTESIAN_POINT('Ctrl Pts',(-1.35856878431637,1.15569532346242,12.7045753741589));
#23606=CARTESIAN_POINT('Ctrl Pts',(-1.33898672035889,1.24928999982123,12.8615328485505));
#23607=CARTESIAN_POINT('Ctrl Pts',(-1.32920497571206,1.28832329599532,12.944492458197));
#23608=CARTESIAN_POINT('Ctrl Pts',(-1.31012567309657,1.34793079918636,13.1120084287429));
#23609=CARTESIAN_POINT('Ctrl Pts',(-1.30085354674442,1.36928881084673,13.195857172909));
#23610=CARTESIAN_POINT('Ctrl Pts',(-1.27636586378979,1.4049429148567,13.421120658934));
#23611=CARTESIAN_POINT('Ctrl Pts',(-1.26143470085253,1.40571524860204,13.563662147314));
#23612=CARTESIAN_POINT('Ctrl Pts',(-1.23123469457865,1.36454425423093,13.8433548834731));
#23613=CARTESIAN_POINT('Ctrl Pts',(-1.21608201599808,1.32306591394079,13.9789211786688));
#23614=CARTESIAN_POINT('Ctrl Pts',(-1.19116793334073,1.22295966287602,14.1874056751138));
#23615=CARTESIAN_POINT('Ctrl Pts',(-1.18154744554627,1.1760789529253,14.2648507244898));
#23616=CARTESIAN_POINT('Ctrl Pts',(-1.15228241326668,1.0120831148425,14.4846360297138));
#23617=CARTESIAN_POINT('Ctrl Pts',(-1.13281234829334,0.874135765416674,
14.6089193614054));
#23618=CARTESIAN_POINT('Ctrl Pts',(-1.1046516246046,0.648893779113152,14.7430038285068));
#23619=CARTESIAN_POINT('Ctrl Pts',(-1.09623154730318,0.578426543600241,
14.7773192602803));
#23620=CARTESIAN_POINT('Ctrl Pts',(-1.07827921096874,0.422219105135024,
14.8377963745812));
#23621=CARTESIAN_POINT('Ctrl Pts',(-1.06881041043044,0.336081057265623,
14.8619906736324));
#23622=CARTESIAN_POINT('Ctrl Pts',(-1.03931196184981,0.0638887425558035,
14.9110284431873));
#23623=CARTESIAN_POINT('Ctrl Pts',(-1.01924554289577,-0.125246622046433,
14.9069085771062));
#23624=CARTESIAN_POINT('Ctrl Pts',(-0.989427198333877,-0.396709589278914,
14.8456968435733));
#23625=CARTESIAN_POINT('Ctrl Pts',(-0.979747013658032,-0.483306516047289,
14.8170777504331));
#23626=CARTESIAN_POINT('Ctrl Pts',(-0.950619670555937,-0.732398469067639,
14.7068548157767));
#23627=CARTESIAN_POINT('Ctrl Pts',(-0.93129645471337,-0.882445703779912,
14.6019050418648));
#23628=CARTESIAN_POINT('Ctrl Pts',(-0.906998790584779,-1.03992217926085,
14.4384245136461));
#23629=CARTESIAN_POINT('Ctrl Pts',(-0.902127602436768,-1.06992979208714,
14.4040624864748));
#23630=CARTESIAN_POINT('Ctrl Pts',(-0.887481419388395,-1.15484462150804,
14.2966637353185));
#23631=CARTESIAN_POINT('Ctrl Pts',(-0.877714846127587,-1.20433645683066,
14.2196612259094));
#23632=CARTESIAN_POINT('Ctrl Pts',(-0.858105037739448,-1.28765509093986,
14.0570447439249));
#23633=CARTESIAN_POINT('Ctrl Pts',(-0.848336101586714,-1.32126823889005,
13.9718104088243));
#23634=CARTESIAN_POINT('Ctrl Pts',(-0.828815227017753,-1.37123717891394,
13.7965742090084));
#23635=CARTESIAN_POINT('Ctrl Pts',(-0.819088224933466,-1.38758415073027,
13.70702194967));
#23636=CARTESIAN_POINT('Ctrl Pts',(-0.799625119408226,-1.40272113880701,
13.5257793559006));
#23637=CARTESIAN_POINT('Ctrl Pts',(-0.789925667583875,-1.40142889436572,
13.4345167996021));
#23638=CARTESIAN_POINT('Ctrl Pts',(-0.770481057338387,-1.38121325807439,
13.2541906062254));
#23639=CARTESIAN_POINT('Ctrl Pts',(-0.760781272839151,-1.36246400098675,
13.1655392050373));
#23640=CARTESIAN_POINT('Ctrl Pts',(-0.741285534984833,-1.30782631815192,
12.9921124871005));
#23641=CARTESIAN_POINT('Ctrl Pts',(-0.73152636222953,-1.27187594788111,
12.9078081282214));
#23642=CARTESIAN_POINT('Ctrl Pts',(-0.711956793810037,-1.18413070434302,
12.7475613086016));
#23643=CARTESIAN_POINT('Ctrl Pts',(-0.702191074851079,-1.13257481192257,
12.6719880898317));
#23644=CARTESIAN_POINT('Ctrl Pts',(-0.687515128589093,-1.04472172005135,
12.5669166485645));
#23645=CARTESIAN_POINT('Ctrl Pts',(-0.682623587019187,-1.01371214468988,
12.533317165612));
#23646=CARTESIAN_POINT('Ctrl Pts',(-0.667943407696058,-0.915978980449471,
12.4373053893992));
#23647=CARTESIAN_POINT('Ctrl Pts',(-0.658177088437864,-0.844738418762731,
12.3798418084721));
#23648=CARTESIAN_POINT('Ctrl Pts',(-0.643521699190297,-0.730382585888922,
12.3047548168733));
#23649=CARTESIAN_POINT('Ctrl Pts',(-0.638653607585438,-0.691158639037145,
12.2816529733307));
#23650=CARTESIAN_POINT('Ctrl Pts',(-0.624913176954061,-0.577673895825769,
12.2220603506758));
#23651=CARTESIAN_POINT('Ctrl Pts',(-0.616028611275531,-0.501204185921513,
12.1901786140452));
#23652=CARTESIAN_POINT('Ctrl Pts',(-0.606981870383497,-0.42041157768316,
12.1646130483831));
#23653=CARTESIAN_POINT('Ctrl Pts',(-0.606762975409993,-0.41845516022692,
12.1639986962372));
#23654=CARTESIAN_POINT('Ctrl Pts',(-0.606544106580495,-0.416497449298501,
12.1633886598088));
#23655=CARTESIAN_POINT('Ctrl Pts',(-0.426566464895916,-0.416497451671892,
12.1633886605483));
#23656=CARTESIAN_POINT('Ctrl Pts',(-0.436856069340607,-0.508294551767764,
12.1919932796566));
#23657=CARTESIAN_POINT('Ctrl Pts',(-0.447040629083815,-0.59692816148061,
12.2299871481661));
#23658=CARTESIAN_POINT('Ctrl Pts',(-0.476149466322508,-0.83511538098895,
12.3625904307335));
#23659=CARTESIAN_POINT('Ctrl Pts',(-0.495150053700609,-0.971644105280062,
12.4767602650293));
#23660=CARTESIAN_POINT('Ctrl Pts',(-0.521283783031458,-1.12612952048971,
12.6654996575978));
#23661=CARTESIAN_POINT('Ctrl Pts',(-0.528447086558006,-1.16506077741258,
12.7207742336957));
#23662=CARTESIAN_POINT('Ctrl Pts',(-0.550935070772576,-1.27412220508858,
12.9021793696774));
#23663=CARTESIAN_POINT('Ctrl Pts',(-0.566218063130956,-1.32886280026531,
13.0364339089676));
#23664=CARTESIAN_POINT('Ctrl Pts',(-0.591343705020871,-1.38258883934397,
13.2627643601562));
#23665=CARTESIAN_POINT('Ctrl Pts',(-0.600938265013163,-1.39481826377124,
13.3506184312601));
#23666=CARTESIAN_POINT('Ctrl Pts',(-0.619721830656807,-1.40240900477448,
13.5247749214712));
#23667=CARTESIAN_POINT('Ctrl Pts',(-0.628824778906351,-1.39825516663194,
13.61067680339));
#23668=CARTESIAN_POINT('Ctrl Pts',(-0.646212924619432,-1.37533891727802,
13.7730353808866));
#23669=CARTESIAN_POINT('Ctrl Pts',(-0.654477069604567,-1.35796056198493,
13.8493535325463));
#23670=CARTESIAN_POINT('Ctrl Pts',(-0.669299655442823,-1.31587716252923,
13.9818440834017));
#23671=CARTESIAN_POINT('Ctrl Pts',(-0.675815032393579,-1.29368274942276,
14.0386005730431));
#23672=CARTESIAN_POINT('Ctrl Pts',(-0.692220433519471,-1.22904882393156,
14.1766217490664));
#23673=CARTESIAN_POINT('Ctrl Pts',(-0.702125852709566,-1.18219577255753,
14.2555067173899));
#23674=CARTESIAN_POINT('Ctrl Pts',(-0.725294061861772,-1.0550557000675,
14.4284481301938));
#23675=CARTESIAN_POINT('Ctrl Pts',(-0.738308575104036,-0.96936000748964,
14.5175967454973));
#23676=CARTESIAN_POINT('Ctrl Pts',(-0.771095147590407,-0.728704749111746,
14.7095919635518));
#23677=CARTESIAN_POINT('Ctrl Pts',(-0.790886881321988,-0.562925190647617,
14.7950800433673));
#23678=CARTESIAN_POINT('Ctrl Pts',(-0.822223990982272,-0.28168981208092,
14.8756008001747));
#23679=CARTESIAN_POINT('Ctrl Pts',(-0.833650660513492,-0.174944210460729,
14.8932055858379));
#23680=CARTESIAN_POINT('Ctrl Pts',(-0.864350735910949,0.111628812394898,
14.9069849291186));
#23681=CARTESIAN_POINT('Ctrl Pts',(-0.883559305371559,0.290497728729643,
14.8811880074753));
#23682=CARTESIAN_POINT('Ctrl Pts',(-0.912360850008062,0.545294985669325,
14.7926231989879));
#23683=CARTESIAN_POINT('Ctrl Pts',(-0.922009061556224,0.627844285719284,
14.7546044436973));
#23684=CARTESIAN_POINT('Ctrl Pts',(-0.941429641103666,0.784320502320354,
14.6632025432421));
#23685=CARTESIAN_POINT('Ctrl Pts',(-0.951157831762751,0.857890680035994,
14.6100549109342));
#23686=CARTESIAN_POINT('Ctrl Pts',(-0.970603595769792,0.99374928117037,
14.4902854078429));
#23687=CARTESIAN_POINT('Ctrl Pts',(-0.980243707293165,1.05571606782114,
14.4239408539999));
#23688=CARTESIAN_POINT('Ctrl Pts',(-0.994838580468196,1.13861676189503,
14.3158644134718));
#23689=CARTESIAN_POINT('Ctrl Pts',(-0.999727647061573,1.16460628651257,
14.2783155451848));
#23690=CARTESIAN_POINT('Ctrl Pts',(-1.01441146505272,1.23702331607857,14.1619183483613));
#23691=CARTESIAN_POINT('Ctrl Pts',(-1.02418705320635,1.27760755818296,14.0797253990493));
#23692=CARTESIAN_POINT('Ctrl Pts',(-1.03887470254296,1.32601335702106,13.9514156711329));
#23693=CARTESIAN_POINT('Ctrl Pts',(-1.04376480430155,1.34003821962249,13.9079032807479));
#23694=CARTESIAN_POINT('Ctrl Pts',(-1.05355449742676,1.36378158168263,13.81966697846));
#23695=CARTESIAN_POINT('Ctrl Pts',(-1.05844747059606,1.37348622838814,13.77499593399));
#23696=CARTESIAN_POINT('Ctrl Pts',(-1.07313867235388,1.39600857517004,13.6397241422986));
#23697=CARTESIAN_POINT('Ctrl Pts',(-1.08290931164055,1.40215313332635,13.5482629108958));
#23698=CARTESIAN_POINT('Ctrl Pts',(-1.10250933181918,1.39651712469916,13.3654539108859));
#23699=CARTESIAN_POINT('Ctrl Pts',(-1.11227241806947,1.3847500654353,13.2745447561302));
#23700=CARTESIAN_POINT('Ctrl Pts',(-1.13184640717828,1.34369127902684,13.0964815911587));
#23701=CARTESIAN_POINT('Ctrl Pts',(-1.14161942173393,1.31452875233355,13.0097474187859));
#23702=CARTESIAN_POINT('Ctrl Pts',(-1.15628531409457,1.25841897095193,12.8848023314274));
#23703=CARTESIAN_POINT('Ctrl Pts',(-1.16117209841051,1.23767832878196,12.8440740817254));
#23704=CARTESIAN_POINT('Ctrl Pts',(-1.17582898554725,1.16970591158298,12.7253430500136));
#23705=CARTESIAN_POINT('Ctrl Pts',(-1.18559009693822,1.1168129127689,12.6508625288843));
#23706=CARTESIAN_POINT('Ctrl Pts',(-1.2050522836408,0.997571959916159,12.5135512491387));
#23707=CARTESIAN_POINT('Ctrl Pts',(-1.21472655783085,0.9315683882803,12.4509951955105));
#23708=CARTESIAN_POINT('Ctrl Pts',(-1.229337525625,0.82398700372118,12.3672485533638));
#23709=CARTESIAN_POINT('Ctrl Pts',(-1.23422763508291,0.786647482698989,
12.3410064175952));
#23710=CARTESIAN_POINT('Ctrl Pts',(-1.24892256039466,0.670828831577373,
12.2677888014863));
#23711=CARTESIAN_POINT('Ctrl Pts',(-1.25868707861522,0.588965527511864,
12.22662839331));
#23712=CARTESIAN_POINT('Ctrl Pts',(-1.27822616168259,0.41908910589679,12.1611261320018));
#23713=CARTESIAN_POINT('Ctrl Pts',(-1.28795438003646,0.331530453908728,
12.1368025075342));
#23714=CARTESIAN_POINT('Ctrl Pts',(-1.31333296220026,0.0975617312448524,
12.0957002236768));
#23715=CARTESIAN_POINT('Ctrl Pts',(-1.3288531321092,-0.0502088032899908,
12.0932117268099));
#23716=CARTESIAN_POINT('Ctrl Pts',(-1.35276419127933,-0.270507663066689,
12.1243034285597));
#23717=CARTESIAN_POINT('Ctrl Pts',(-1.36090638824632,-0.344364594037876,
12.1409115571464));
#23718=CARTESIAN_POINT('Ctrl Pts',(-1.36903602092574,-0.416497450391695,
12.1633886601494));
#23719=CARTESIAN_POINT('Origin',(0.,0.,13.5));
#23720=CARTESIAN_POINT('',(-2.49153227027379,-0.416497403609636,12.1633886455718));
#23721=CARTESIAN_POINT('',(-2.31145225782316,-0.416497494886935,12.1633886740144));
#23722=CARTESIAN_POINT('',(0.,-0.416497449530544,12.1633886598811));
#23723=CARTESIAN_POINT('Ctrl Pts',(-2.49153227027379,-0.416497403609637,
12.1633886455718));
#23724=CARTESIAN_POINT('Ctrl Pts',(-2.48377759386758,-0.347468400922449,
12.1418787277503));
#23725=CARTESIAN_POINT('Ctrl Pts',(-2.47601354514147,-0.276847582414752,
12.1257394777351));
#23726=CARTESIAN_POINT('Ctrl Pts',(-2.46337215890503,-0.160100728167568,
12.1084352599308));
#23727=CARTESIAN_POINT('Ctrl Pts',(-2.45849711705798,-0.114634837042245,
12.1039542840005));
#23728=CARTESIAN_POINT('Ctrl Pts',(-2.43419614037067,0.112519097027662,
12.0927401847591));
#23729=CARTESIAN_POINT('Ctrl Pts',(-2.41480592826936,0.294086936803198,
12.1192203848806));
#23730=CARTESIAN_POINT('Ctrl Pts',(-2.38556824782432,0.551677657416333,
12.2100390762164));
#23731=CARTESIAN_POINT('Ctrl Pts',(-2.37582669014715,0.634662303048093,
12.2487801906221));
#23732=CARTESIAN_POINT('Ctrl Pts',(-2.36115008617931,0.752488449996106,
12.3185443183758));
#23733=CARTESIAN_POINT('Ctrl Pts',(-2.35626398826519,0.790541390226631,
12.3436606570512));
#23734=CARTESIAN_POINT('Ctrl Pts',(-2.34168031498338,0.900246641204636,
12.4240204249908));
#23735=CARTESIAN_POINT('Ctrl Pts',(-2.33204530358468,0.967844787647961,
12.4843952604642));
#23736=CARTESIAN_POINT('Ctrl Pts',(-2.30287250743473,1.15279927099767,12.684941919434));
#23737=CARTESIAN_POINT('Ctrl Pts',(-2.28340827706671,1.24906570563351,12.8418966503144));
#23738=CARTESIAN_POINT('Ctrl Pts',(-2.25411301591339,1.34430474565109,13.098518628679));
#23739=CARTESIAN_POINT('Ctrl Pts',(-2.24437372807563,1.36762809005532,13.1870532149905));
#23740=CARTESIAN_POINT('Ctrl Pts',(-2.22478159000079,1.39670824504616,13.3674755372028));
#23741=CARTESIAN_POINT('Ctrl Pts',(-2.21498909654132,1.40238025146898,13.4589340742773));
#23742=CARTESIAN_POINT('Ctrl Pts',(-2.18568716103912,1.39255584062942,13.7322520605856));
#23743=CARTESIAN_POINT('Ctrl Pts',(-2.16633857511812,1.35057933199256,13.9112040608549));
#23744=CARTESIAN_POINT('Ctrl Pts',(-2.14198168246296,1.25674829820127,14.1185938447382));
#23745=CARTESIAN_POINT('Ctrl Pts',(-2.13711836627855,1.23595875252239,14.1591514505222));
#23746=CARTESIAN_POINT('Ctrl Pts',(-2.11614875473995,1.13808286942347,14.32912266523));
#23747=CARTESIAN_POINT('Ctrl Pts',(-2.10003915852141,1.04237141114805,14.4466453455716));
#23748=CARTESIAN_POINT('Ctrl Pts',(-2.07902261227106,0.895684084578088,
14.5769547781812));
#23749=CARTESIAN_POINT('Ctrl Pts',(-2.07415016887986,0.860113650291088,
14.6055705253448));
#23750=CARTESIAN_POINT('Ctrl Pts',(-2.04970556948249,0.675127730358556,
14.7400480198235));
#23751=CARTESIAN_POINT('Ctrl Pts',(-2.03017148796127,0.507359241860883,
14.817612551329));
#23752=CARTESIAN_POINT('Ctrl Pts',(-2.00082455849128,0.240662255076382,
14.8821802881563));
#23753=CARTESIAN_POINT('Ctrl Pts',(-1.99109139201528,0.150010486708826,
14.8949326508275));
#23754=CARTESIAN_POINT('Ctrl Pts',(-1.97133043004739,-0.0341083947857306,
14.9026679937534));
#23755=CARTESIAN_POINT('Ctrl Pts',(-1.96134793998215,-0.127141301000997,
14.8973103419758));
#23756=CARTESIAN_POINT('Ctrl Pts',(-1.94650726074608,-0.264019383396102,
14.8756363941141));
#23757=CARTESIAN_POINT('Ctrl Pts',(-1.94163609258797,-0.308708703192616,
14.8663018582216));
#23758=CARTESIAN_POINT('Ctrl Pts',(-1.91945790680511,-0.509566913570251,
14.8139876521769));
#23759=CARTESIAN_POINT('Ctrl Pts',(-1.90216586855344,-0.658006283194157,
14.7462935509965));
#23760=CARTESIAN_POINT('Ctrl Pts',(-1.87507752023587,-0.866521505981471,
14.6033581069912));
#23761=CARTESIAN_POINT('Ctrl Pts',(-1.86539795153523,-0.936297771913995,
14.5447991730715));
#23762=CARTESIAN_POINT('Ctrl Pts',(-1.84597259989742,-1.06326139298109,
14.4152424783883));
#23763=CARTESIAN_POINT('Ctrl Pts',(-1.8362713986498,-1.12019802305971,14.3446004003708));
#23764=CARTESIAN_POINT('Ctrl Pts',(-1.81678516152418,-1.22009380401549,
14.1926161974074));
#23765=CARTESIAN_POINT('Ctrl Pts',(-1.80703971528604,-1.26267897580898,
14.1115453629672));
#23766=CARTESIAN_POINT('Ctrl Pts',(-1.78887058392302,-1.32642166587171,
13.9546328582154));
#23767=CARTESIAN_POINT('Ctrl Pts',(-1.78049468158165,-1.34968935628625,
13.8800317236812));
#23768=CARTESIAN_POINT('Ctrl Pts',(-1.76250218670362,-1.38611096094181,
13.7162361092004));
#23769=CARTESIAN_POINT('Ctrl Pts',(-1.75295731014169,-1.39712351726591,
13.6269174236735));
#23770=CARTESIAN_POINT('Ctrl Pts',(-1.72377142004812,-1.40437243116028,
13.353908122551));
#23771=CARTESIAN_POINT('Ctrl Pts',(-1.70415058337538,-1.3731989144026,13.1714742819655));
#23772=CARTESIAN_POINT('Ctrl Pts',(-1.67478380946666,-1.27514573804416,
12.9148925399848));
#23773=CARTESIAN_POINT('Ctrl Pts',(-1.66505071523327,-1.23425531818042,
12.8329460698071));
#23774=CARTESIAN_POINT('Ctrl Pts',(-1.64547168751001,-1.13704679109676,
12.6781193062635));
#23775=CARTESIAN_POINT('Ctrl Pts',(-1.63568267335985,-1.08094703361817,
12.6056193489201));
#23776=CARTESIAN_POINT('Ctrl Pts',(-1.62099125749229,-0.986817086254176,
12.5058772385525));
#23777=CARTESIAN_POINT('Ctrl Pts',(-1.61609821231226,-0.953846142866909,
12.4742000397494));
#23778=CARTESIAN_POINT('Ctrl Pts',(-1.60146146019077,-0.850811108408571,
12.3844783193595));
#23779=CARTESIAN_POINT('Ctrl Pts',(-1.59173204114866,-0.776582088982317,
12.3315872605324));
#23780=CARTESIAN_POINT('Ctrl Pts',(-1.57226834088642,-0.619119849626152,
12.2410651847151));
#23781=CARTESIAN_POINT('Ctrl Pts',(-1.56260707085518,-0.536281388983477,
12.2036093642709));
#23782=CARTESIAN_POINT('Ctrl Pts',(-1.55162440893478,-0.439145982974093,
12.1706045824513));
#23783=CARTESIAN_POINT('Ctrl Pts',(-1.55035155684989,-0.427842917316238,
12.1669239868733));
#23784=CARTESIAN_POINT('Ctrl Pts',(-1.54907858904864,-0.416497429633283,
12.1633886536809));
#23785=CARTESIAN_POINT('Ctrl Pts',(-1.36903602092574,-0.416497450391695,
12.1633886601494));
#23786=CARTESIAN_POINT('Ctrl Pts',(-1.37055630404986,-0.429986665530214,
12.1675919940173));
#23787=CARTESIAN_POINT('Ctrl Pts',(-1.37207596709313,-0.443415607308437,
12.1720005753452));
#23788=CARTESIAN_POINT('Ctrl Pts',(-1.38016695316969,-0.514617638283364,
12.1965766368901));
#23789=CARTESIAN_POINT('Ctrl Pts',(-1.38668001305955,-0.57108368251163,
12.2203096644137));
#23790=CARTESIAN_POINT('Ctrl Pts',(-1.40296155657829,-0.707169183262192,
12.2883142054731));
#23791=CARTESIAN_POINT('Ctrl Pts',(-1.4126955046026,-0.784366074695015,
12.3367973222343));
#23792=CARTESIAN_POINT('Ctrl Pts',(-1.42733008015005,-0.892470436642723,
12.42037724037));
#23793=CARTESIAN_POINT('Ctrl Pts',(-1.43222273412454,-0.927236836738582,
12.4500854254159));
#23794=CARTESIAN_POINT('Ctrl Pts',(-1.44201572448199,-0.993737226622791,
12.5127943896425));
#23795=CARTESIAN_POINT('Ctrl Pts',(-1.44690951607711,-1.02543152920955,
12.5457574910582));
#23796=CARTESIAN_POINT('Ctrl Pts',(-1.46160331503236,-1.11552634929339,
12.6491412336523));
#23797=CARTESIAN_POINT('Ctrl Pts',(-1.47136592281737,-1.16869919717314,
12.7237900733827));
#23798=CARTESIAN_POINT('Ctrl Pts',(-1.4909596634891,-1.25972038856916,12.882374098493));
#23799=CARTESIAN_POINT('Ctrl Pts',(-1.50073942681233,-1.29735262604247,
12.9659275401047));
#23800=CARTESIAN_POINT('Ctrl Pts',(-1.52029606830947,-1.35569686312962,
13.1389029286828));
#23801=CARTESIAN_POINT('Ctrl Pts',(-1.53000129719526,-1.37632231821543,
13.2278933038496));
#23802=CARTESIAN_POINT('Ctrl Pts',(-1.54953196511918,-1.40000539138166,
13.4087824924846));
#23803=CARTESIAN_POINT('Ctrl Pts',(-1.55931752269324,-1.40297366362121,
13.5002514645915));
#23804=CARTESIAN_POINT('Ctrl Pts',(-1.58881724745846,-1.38503995608772,
13.7744997609866));
#23805=CARTESIAN_POINT('Ctrl Pts',(-1.60827700302614,-1.33716438228231,
13.9535192941375));
#23806=CARTESIAN_POINT('Ctrl Pts',(-1.63279556542512,-1.23595895928569,
14.1591580854752));
#23807=CARTESIAN_POINT('Ctrl Pts',(-1.63767465958672,-1.21381003363761,
14.1991059284103));
#23808=CARTESIAN_POINT('Ctrl Pts',(-1.65234396474022,-1.14159072792032,
14.3155483615572));
#23809=CARTESIAN_POINT('Ctrl Pts',(-1.66213210403576,-1.08594656988133,
14.3882950615527));
#23810=CARTESIAN_POINT('Ctrl Pts',(-1.69154038888768,-0.898932281795321,
14.5887250831049));
#23811=CARTESIAN_POINT('Ctrl Pts',(-1.7108834370603,-0.749282123885,14.6966528911975));
#23812=CARTESIAN_POINT('Ctrl Pts',(-1.74026139106864,-0.500243991061622,
14.8107508678375));
#23813=CARTESIAN_POINT('Ctrl Pts',(-1.75004056336101,-0.413847590560855,
14.8405379461715));
#23814=CARTESIAN_POINT('Ctrl Pts',(-1.7798787288382,-0.143192886693771,
14.9051692043203));
#23815=CARTESIAN_POINT('Ctrl Pts',(-1.79951934952144,0.0456593073224952,
14.911707423503));
#23816=CARTESIAN_POINT('Ctrl Pts',(-1.82928632628386,0.318590552131681,
14.8662099324968));
#23817=CARTESIAN_POINT('Ctrl Pts',(-1.83894752496594,0.405360836840588,
14.8430236418812));
#23818=CARTESIAN_POINT('Ctrl Pts',(-1.85883289055153,0.579108170720027,
14.7782087981025));
#23819=CARTESIAN_POINT('Ctrl Pts',(-1.86900114187339,0.665222765504545,
14.7355822452673));
#23820=CARTESIAN_POINT('Ctrl Pts',(-1.88903956520451,0.823694474386146,
14.6357348058695));
#23821=CARTESIAN_POINT('Ctrl Pts',(-1.89883311377528,0.896115948541066,
14.5795100191461));
#23822=CARTESIAN_POINT('Ctrl Pts',(-1.92824791000986,1.09530820757515,14.3909163792467));
#23823=CARTESIAN_POINT('Ctrl Pts',(-1.94779722878606,1.20218403566685,14.240399190362));
#23824=CARTESIAN_POINT('Ctrl Pts',(-1.97682766485052,1.31382113728833,13.9918391985901));
#23825=CARTESIAN_POINT('Ctrl Pts',(-1.98633002286068,1.34260384155628,13.9067507459095));
#23826=CARTESIAN_POINT('Ctrl Pts',(-2.0120400414814,1.39747926223019,13.6726392534436));
#23827=CARTESIAN_POINT('Ctrl Pts',(-2.02828849510217,1.40794165964757,13.5211808202616));
#23828=CARTESIAN_POINT('Ctrl Pts',(-2.05497486306235,1.38505568715582,13.2738684574458));
#23829=CARTESIAN_POINT('Ctrl Pts',(-2.06533068198525,1.36594077564537,13.177941121327));
#23830=CARTESIAN_POINT('Ctrl Pts',(-2.08552170664394,1.30985235566511,12.997336518746));
#23831=CARTESIAN_POINT('Ctrl Pts',(-2.09529461618589,1.27418345627835,12.9127694663235));
#23832=CARTESIAN_POINT('Ctrl Pts',(-2.12465204047475,1.14343094971824,12.6718056249336));
#23833=CARTESIAN_POINT('Ctrl Pts',(-2.14414013309284,1.0257830350729,12.5298908410156));
#23834=CARTESIAN_POINT('Ctrl Pts',(-2.17335866262273,0.813545005322425,
12.3569986300674));
#23835=CARTESIAN_POINT('Ctrl Pts',(-2.18306730770509,0.737427447863767,
12.3064726590416));
#23836=CARTESIAN_POINT('Ctrl Pts',(-2.20253472026112,0.577156163115864,
12.2213075788084));
#23837=CARTESIAN_POINT('Ctrl Pts',(-2.21224818242629,0.493451613008539,
12.1867335142098));
#23838=CARTESIAN_POINT('Ctrl Pts',(-2.23754581469018,0.267832394698486,
12.1181815529036));
#23839=CARTESIAN_POINT('Ctrl Pts',(-2.2529785965965,0.12291760233651,12.0978415590498));
#23840=CARTESIAN_POINT('Ctrl Pts',(-2.28294885814402,-0.156439897817064,
12.1023354354469));
#23841=CARTESIAN_POINT('Ctrl Pts',(-2.29715378790174,-0.289106120400033,
12.1236926252734));
#23842=CARTESIAN_POINT('Ctrl Pts',(-2.31145225782327,-0.416497494887886,
12.1633886740147));
#23843=CARTESIAN_POINT('Origin',(0.,0.,13.5));
#23844=CARTESIAN_POINT('',(-3.1180327855299,0.795259447899244,12.3478010527258));
#23845=CARTESIAN_POINT('Ctrl Pts',(-2.31145225782327,-0.416497494887886,
12.1633886740147));
#23846=CARTESIAN_POINT('Ctrl Pts',(-2.3167521873648,-0.463716904565301,
12.1781025743524));
#23847=CARTESIAN_POINT('Ctrl Pts',(-2.32206620895333,-0.510211567222956,
12.1953357212503));
#23848=CARTESIAN_POINT('Ctrl Pts',(-2.33229991020307,-0.597693045802501,
12.233173817206));
#23849=CARTESIAN_POINT('Ctrl Pts',(-2.33720164067599,-0.638696499194981,
12.253343498657));
#23850=CARTESIAN_POINT('Ctrl Pts',(-2.35182609492161,-0.758044075161683,
12.3194871727543));
#23851=CARTESIAN_POINT('Ctrl Pts',(-2.36151340155549,-0.83297903747351,
12.371112325251));
#23852=CARTESIAN_POINT('Ctrl Pts',(-2.38103415191372,-0.97226540446231,
12.4885388985911));
#23853=CARTESIAN_POINT('Ctrl Pts',(-2.3908061863421,-1.03620742481829,12.5541523183872));
#23854=CARTESIAN_POINT('Ctrl Pts',(-2.42025680254283,-1.20796240853674,
12.7688866301326));
#23855=CARTESIAN_POINT('Ctrl Pts',(-2.43982312600438,-1.29331998098181,
12.9334109226447));
#23856=CARTESIAN_POINT('Ctrl Pts',(-2.47466620114974,-1.38409577536895,
13.2461198462985));
#23857=CARTESIAN_POINT('Ctrl Pts',(-2.48970038938532,-1.402704004665,13.3877645272084));
#23858=CARTESIAN_POINT('Ctrl Pts',(-2.51462424398795,-1.39776875624929,
13.6197852242924));
#23859=CARTESIAN_POINT('Ctrl Pts',(-2.52430994314769,-1.38717554817382,
13.7094050293777));
#23860=CARTESIAN_POINT('Ctrl Pts',(-2.54245933154651,-1.35119409578135,
13.8749286173372));
#23861=CARTESIAN_POINT('Ctrl Pts',(-2.55091248218538,-1.32777537595692,
13.9508989001517));
#23862=CARTESIAN_POINT('Ctrl Pts',(-2.56917308308684,-1.2638119902416,14.1092046896047));
#23863=CARTESIAN_POINT('Ctrl Pts',(-2.57895229850129,-1.22136348749128,
14.190378113102));
#23864=CARTESIAN_POINT('Ctrl Pts',(-2.59846139720312,-1.12161698798404,
14.3427373178754));
#23865=CARTESIAN_POINT('Ctrl Pts',(-2.6081322712015,-1.06466344008099,14.4136315100372));
#23866=CARTESIAN_POINT('Ctrl Pts',(-2.62760843372855,-0.937668490314083,
14.543577447306));
#23867=CARTESIAN_POINT('Ctrl Pts',(-2.63737030289336,-0.867893247000527,
14.6022872855144));
#23868=CARTESIAN_POINT('Ctrl Pts',(-2.65679337332192,-0.718574559597896,
14.7049015851361));
#23869=CARTESIAN_POINT('Ctrl Pts',(-2.66639112991186,-0.639466084224944,
14.7486875801947));
#23870=CARTESIAN_POINT('Ctrl Pts',(-2.68092952061222,-0.514803287617618,
14.8027134017972));
#23871=CARTESIAN_POINT('Ctrl Pts',(-2.68581920989598,-0.472048025464354,
14.8188082341359));
#23872=CARTESIAN_POINT('Ctrl Pts',(-2.70041223268387,-0.342590669370393,
14.8604378397063));
#23873=CARTESIAN_POINT('Ctrl Pts',(-2.71011363466229,-0.254121430526818,
14.8797037187546));
#23874=CARTESIAN_POINT('Ctrl Pts',(-2.7294086780924,-0.0750932251353697,
14.9008749733284));
#23875=CARTESIAN_POINT('Ctrl Pts',(-2.73898533044384,0.0150370781420963,
14.9028055849289));
#23876=CARTESIAN_POINT('Ctrl Pts',(-2.75836409190454,0.195440539002722,
14.8892725344481));
#23877=CARTESIAN_POINT('Ctrl Pts',(-2.76812368298385,0.285274149539204,
14.8736424048526));
#23878=CARTESIAN_POINT('Ctrl Pts',(-2.78762987367098,0.460540422606209,
14.8252019094676));
#23879=CARTESIAN_POINT('Ctrl Pts',(-2.79730018784044,0.545563984803865,
14.792523874345));
#23880=CARTESIAN_POINT('Ctrl Pts',(-2.81190854088784,0.667683178766226,
14.7313762949139));
#23881=CARTESIAN_POINT('Ctrl Pts',(-2.81679996050081,0.7075189164068,14.7089273179091));
#23882=CARTESIAN_POINT('Ctrl Pts',(-2.83139954255971,0.822688831613105,
14.6363795055697));
#23883=CARTESIAN_POINT('Ctrl Pts',(-2.84110944631101,0.894345491985826,
14.5808893635849));
#23884=CARTESIAN_POINT('Ctrl Pts',(-2.86039366562439,1.02543771398911,14.457353248677));
#23885=CARTESIAN_POINT('Ctrl Pts',(-2.86994280580073,1.08466095268082,14.3896956913934));
#23886=CARTESIAN_POINT('Ctrl Pts',(-2.88930432824196,1.19016061908563,14.2428448976629));
#23887=CARTESIAN_POINT('Ctrl Pts',(-2.89907467613071,1.23596830086219,14.1638393708666));
#23888=CARTESIAN_POINT('Ctrl Pts',(-2.92843101455799,1.34949690146608,13.9149187599842));
#23889=CARTESIAN_POINT('Ctrl Pts',(-2.94777333733644,1.39203401948613,13.7356737401434));
#23890=CARTESIAN_POINT('Ctrl Pts',(-2.97712004430575,1.40246577308113,13.4619756526989));
#23891=CARTESIAN_POINT('Ctrl Pts',(-2.98687033518447,1.39699251432984,13.3705080545567));
#23892=CARTESIAN_POINT('Ctrl Pts',(-3.00643901032036,1.36829687580028,13.1899756322952));
#23893=CARTESIAN_POINT('Ctrl Pts',(-3.01622731821428,1.34514862602942,13.101344544025));
#23894=CARTESIAN_POINT('Ctrl Pts',(-3.04141266551141,1.26391422487236,12.8810618542207));
#23895=CARTESIAN_POINT('Ctrl Pts',(-3.05661944091923,1.19391980854937,12.7549364988526));
#23896=CARTESIAN_POINT('Ctrl Pts',(-3.07966134533297,1.0620265877888,12.5849899766776));
#23897=CARTESIAN_POINT('Ctrl Pts',(-3.08735366480303,1.01376606064143,12.5317945273643));
#23898=CARTESIAN_POINT('Ctrl Pts',(-3.09890496797339,0.935610634270255,
12.4579271143655));
#23899=CARTESIAN_POINT('Ctrl Pts',(-3.10275037665096,0.908641978613474,
12.4343297929454));
#23900=CARTESIAN_POINT('Ctrl Pts',(-3.11040658761295,0.853109352415768,
12.3893815571006));
#23901=CARTESIAN_POINT('Ctrl Pts',(-3.11421620510946,0.824575859088257,
12.3680355398651));
#23902=CARTESIAN_POINT('Ctrl Pts',(-3.11803278657939,0.7952594475796,12.3478010540556));
#23903=CARTESIAN_POINT('',(-3.11803278688524,0.,14.9));
#23904=CARTESIAN_POINT('Origin',(-3.11803278688524,0.,13.5));
#23905=CARTESIAN_POINT('',(-2.91746474354357,0.,14.9));
#23906=CARTESIAN_POINT('',(0.,0.,14.9));
#23907=CARTESIAN_POINT('Ctrl Pts',(-2.91746474354356,8.32667268468867E-16,
14.9));
#23908=CARTESIAN_POINT('Ctrl Pts',(-2.90757293093835,-0.0924594044157247,
14.9));
#23909=CARTESIAN_POINT('Ctrl Pts',(-2.89771271548873,-0.184691566429423,
14.8908406471496));
#23910=CARTESIAN_POINT('Ctrl Pts',(-2.87788082299124,-0.366121167923027,
14.8544471970385));
#23911=CARTESIAN_POINT('Ctrl Pts',(-2.86796372368023,-0.454867233609991,
14.8272782269122));
#23912=CARTESIAN_POINT('Ctrl Pts',(-2.84124661433094,-0.684587979546175,
14.7311818185962));
#23913=CARTESIAN_POINT('Ctrl Pts',(-2.82448139317192,-0.817770227731554,
14.6470506633447));
#23914=CARTESIAN_POINT('Ctrl Pts',(-2.79449519173347,-1.02730970995846,
14.4592906694374));
#23915=CARTESIAN_POINT('Ctrl Pts',(-2.78130510865068,-1.10876333275197,
14.3638553696772));
#23916=CARTESIAN_POINT('Ctrl Pts',(-2.75555577135647,-1.23891302852057,
14.1620902827348));
#23917=CARTESIAN_POINT('Ctrl Pts',(-2.74312347368462,-1.2891672738364,14.0579558991923));
#23918=CARTESIAN_POINT('Ctrl Pts',(-2.72099075705634,-1.35502115159312,
13.8633967680281));
#23919=CARTESIAN_POINT('Ctrl Pts',(-2.71138423761646,-1.37561913391642,
13.7753415654217));
#23920=CARTESIAN_POINT('Ctrl Pts',(-2.68215668485679,-1.41198572154935,
13.5039122886093));
#23921=CARTESIAN_POINT('Ctrl Pts',(-2.66271368248315,-1.40032578005776,
13.3188842013009));
#23922=CARTESIAN_POINT('Ctrl Pts',(-2.63340568277471,-1.33032649598374,
13.0547244643092));
#23923=CARTESIAN_POINT('Ctrl Pts',(-2.6237756819577,-1.29908768118497,12.9704626653747));
#23924=CARTESIAN_POINT('Ctrl Pts',(-2.60451951442829,-1.22090765216068,
12.8090359941975));
#23925=CARTESIAN_POINT('Ctrl Pts',(-2.59497820215046,-1.17413824150344,
12.7322455266302));
#23926=CARTESIAN_POINT('Ctrl Pts',(-2.56608332448149,-1.01186755014022,
12.5157005711754));
#23927=CARTESIAN_POINT('Ctrl Pts',(-2.54672775468785,-0.876360220239523,
12.393332780747));
#23928=CARTESIAN_POINT('Ctrl Pts',(-2.51762480991736,-0.643287763981639,
12.2532148297775));
#23929=CARTESIAN_POINT('Ctrl Pts',(-2.50792686736518,-0.560851342787942,
12.2140225281083));
#23930=CARTESIAN_POINT('Ctrl Pts',(-2.49595816639203,-0.455768936955594,
12.1761037787382));
#23931=CARTESIAN_POINT('Ctrl Pts',(-2.49374542515372,-0.43619801600797,
12.169527493552));
#23932=CARTESIAN_POINT('Ctrl Pts',(-2.49153227027379,-0.416497403609637,
12.1633886455718));
#23933=CARTESIAN_POINT('Origin',(-7.25,-0.25,13.5));
#23934=CARTESIAN_POINT('',(-7.2,-0.25,14.43));
#23935=CARTESIAN_POINT('',(-7.2,-0.25,14.1858571279793));
#23936=CARTESIAN_POINT('',(-7.2,-0.25,13.5));
#23937=CARTESIAN_POINT('',(-4.4,-0.25,14.43));
#23938=CARTESIAN_POINT('',(-7.25,-0.25,14.43));
#23939=CARTESIAN_POINT('',(-4.4,-0.25,14.1538348415311));
#23940=CARTESIAN_POINT('',(-4.4,-0.25,13.5));
#23941=CARTESIAN_POINT('',(-7.17,-0.25,14.1538348415311));
#23942=CARTESIAN_POINT('',(-5.585,-0.25,14.1538348415311));
#23943=CARTESIAN_POINT('Ctrl Pts',(-7.2,-0.25,14.1858571279793));
#23944=CARTESIAN_POINT('Ctrl Pts',(-7.18464145915026,-0.25,14.1695100866453));
#23945=CARTESIAN_POINT('Ctrl Pts',(-7.17,-0.25,14.1538348415311));
#23946=CARTESIAN_POINT('Origin',(-4.4,-0.25,13.5));
#23947=CARTESIAN_POINT('',(-4.4,0.25,14.1538348415311));
#23948=CARTESIAN_POINT('Origin',(-4.4,0.,13.5));
#23949=CARTESIAN_POINT('',(-4.4,0.25,14.43));
#23950=CARTESIAN_POINT('',(-4.4,-0.25,14.43));
#23951=CARTESIAN_POINT('',(-4.4,0.25,13.5));
#23952=CARTESIAN_POINT('Origin',(-4.4,0.25,13.5));
#23953=CARTESIAN_POINT('',(-7.2,0.25,14.1858571279793));
#23954=CARTESIAN_POINT('',(-7.2,0.25,14.43));
#23955=CARTESIAN_POINT('',(-7.2,0.25,13.5));
#23956=CARTESIAN_POINT('',(-7.17,0.25,14.1538348415311));
#23957=CARTESIAN_POINT('Ctrl Pts',(-7.17,0.25,14.1538348415311));
#23958=CARTESIAN_POINT('Ctrl Pts',(-7.18464145915026,0.25,14.1695100866453));
#23959=CARTESIAN_POINT('Ctrl Pts',(-7.2,0.25,14.1858571279793));
#23960=CARTESIAN_POINT('',(-5.585,0.25,14.1538348415311));
#23961=CARTESIAN_POINT('',(-4.4,0.25,14.43));
#23962=CARTESIAN_POINT('Origin',(-5.825,0.,14.43));
#23963=CARTESIAN_POINT('',(-7.2,0.,14.43));
#23964=CARTESIAN_POINT('Origin',(-5.585,0.,13.5));
#23965=CARTESIAN_POINT('',(-4.,-8.57252759403146E-17,12.8));
#23966=CARTESIAN_POINT('Origin',(-4.,0.,13.5));
#23967=CARTESIAN_POINT('',(-7.17,-8.57252759403146E-17,12.8));
#23968=CARTESIAN_POINT('',(-5.585,-8.57252759403146E-17,12.8));
#23969=CARTESIAN_POINT('Origin',(-7.17,0.,13.5));
#23970=CARTESIAN_POINT('Origin',(-7.17,0.,13.5));
#23971=CARTESIAN_POINT('Origin',(-7.21,0.,13.5));
#23972=CARTESIAN_POINT('Origin',(-7.2,0.,13.5));
#23973=CARTESIAN_POINT('Origin',(-3.78969878334035,0.,13.5));
#23974=CARTESIAN_POINT('',(-3.57939756668071,0.,13.5));
#23975=CARTESIAN_POINT('',(-3.78969878334035,-4.28626379701574E-17,13.15));
#23976=CARTESIAN_POINT('Origin',(-3.61,0.,13.5));
#23977=CARTESIAN_POINT('',(-4.1,-1.712056225208E-16,12.102));
#23978=CARTESIAN_POINT('Origin',(-4.1,0.,13.5));
#23979=CARTESIAN_POINT('',(-3.12,-1.712056225208E-16,12.102));
#23980=CARTESIAN_POINT('',(-3.61,-1.712056225208E-16,12.102));
#23981=CARTESIAN_POINT('Origin',(-3.12,0.,13.5));
#23982=CARTESIAN_POINT('Origin',(-2.76,0.,13.5));
#23983=CARTESIAN_POINT('',(-2.9716366454152,0.,15.0488360771612));
#23984=CARTESIAN_POINT('',(-2.6276958156896,4.102857932342E-16,11.6014907459511));
#23985=CARTESIAN_POINT('Ctrl Pts',(-2.9716366454152,7.60502771868232E-15,
15.0488360771612));
#23986=CARTESIAN_POINT('Ctrl Pts',(-2.96513918497401,-0.0920375220506268,
15.0554418286098));
#23987=CARTESIAN_POINT('Ctrl Pts',(-2.95870046090467,-0.184510271773937,
15.0537810097104));
#23988=CARTESIAN_POINT('Ctrl Pts',(-2.94574540539509,-0.369537679687644,
15.0340535994561));
#23989=CARTESIAN_POINT('Ctrl Pts',(-2.93925228407338,-0.461737874031516,
15.0157596972663));
#23990=CARTESIAN_POINT('Ctrl Pts',(-2.91958652769516,-0.735865978954469,
14.9355197227161));
#23991=CARTESIAN_POINT('Ctrl Pts',(-2.90654874341827,-0.908932390668185,
14.8486604536394));
#23992=CARTESIAN_POINT('Ctrl Pts',(-2.88661663694525,-1.1476938338663,14.6696722402344));
#23993=CARTESIAN_POINT('Ctrl Pts',(-2.87963270291874,-1.22619265279611,
14.5977533374101));
#23994=CARTESIAN_POINT('Ctrl Pts',(-2.85827410403415,-1.44301835851629,
14.3568412674897));
#23995=CARTESIAN_POINT('Ctrl Pts',(-2.843906091307,-1.5556936748727,14.1673389814163));
#23996=CARTESIAN_POINT('Ctrl Pts',(-2.82263789490064,-1.66604286105911,
13.8572055037074));
#23997=CARTESIAN_POINT('Ctrl Pts',(-2.81559948523675,-1.69277726945658,
13.749379202055));
#23998=CARTESIAN_POINT('Ctrl Pts',(-2.79429900209064,-1.74166074208239,
13.417417949714));
#23999=CARTESIAN_POINT('Ctrl Pts',(-2.78031251610869,-1.73033660024184,
13.1908637168291));
#24000=CARTESIAN_POINT('Ctrl Pts',(-2.75909846476153,-1.64895833456621,
12.8603458898717));
#24001=CARTESIAN_POINT('Ctrl Pts',(-2.75193057197317,-1.61035130266583,
12.7511403637933));
#24002=CARTESIAN_POINT('Ctrl Pts',(-2.73773225640633,-1.51216303880933,
12.5414445443358));
#24003=CARTESIAN_POINT('Ctrl Pts',(-2.73072541788755,-1.45276422182245,
12.4414862625126));
#24004=CARTESIAN_POINT('Ctrl Pts',(-2.70917560177417,-1.24230101342177,
12.1543537334464));
#24005=CARTESIAN_POINT('Ctrl Pts',(-2.69478862312514,-1.06343354425305,
11.9910281778624));
#24006=CARTESIAN_POINT('Ctrl Pts',(-2.66611563845589,-0.64786062771374,
11.7400700233335));
#24007=CARTESIAN_POINT('Ctrl Pts',(-2.65185433641513,-0.415477599079208,
11.6563602555503));
#24008=CARTESIAN_POINT('Ctrl Pts',(-2.63435622392806,-0.115608928180287,
11.610909632013));
#24009=CARTESIAN_POINT('Ctrl Pts',(-2.63102379259863,-0.057881494981571,
11.6048741891419));
#24010=CARTESIAN_POINT('Ctrl Pts',(-2.6276958156896,-4.16333634234434E-17,
11.6014907459511));
#24011=CARTESIAN_POINT('',(-2.76,0.,15.264));
#24012=CARTESIAN_POINT('',(-2.42954235284503,-0.728141132413258,15.4696174511348));
#24013=CARTESIAN_POINT('Ctrl Pts',(-2.42950897630267,-0.72814559274872,
15.4695817140195));
#24014=CARTESIAN_POINT('Ctrl Pts',(-2.43828133387365,-0.652393922688123,
15.4881130997835));
#24015=CARTESIAN_POINT('Ctrl Pts',(-2.44710731128846,-0.575762085981697,
15.5023539166817));
#24016=CARTESIAN_POINT('Ctrl Pts',(-2.45598857155625,-0.498622745157995,
15.5122142918554));
#24017=CARTESIAN_POINT('Ctrl Pts',(-2.46354562505042,-0.432984974443784,
15.5206044730249));
#24018=CARTESIAN_POINT('Ctrl Pts',(-2.47114270491829,-0.36697910323544,
15.5258224467513));
#24019=CARTESIAN_POINT('Ctrl Pts',(-2.47878083569838,-0.300830869104269,
15.5277833167051));
#24020=CARTESIAN_POINT('Ctrl Pts',(-2.48542346325084,-0.243303956403079,
15.5294886198948));
#24021=CARTESIAN_POINT('Ctrl Pts',(-2.49209713843209,-0.185669120678873,
15.5287299263396));
#24022=CARTESIAN_POINT('Ctrl Pts',(-2.49880253512854,-0.128089393860388,
15.5255228966375));
#24023=CARTESIAN_POINT('Ctrl Pts',(-2.5072738296511,-0.0553457745803134,
15.521471280547));
#24024=CARTESIAN_POINT('Ctrl Pts',(-2.51578575259894,0.0170141412883056,
15.5134623775051));
#24025=CARTESIAN_POINT('Ctrl Pts',(-2.52435299120783,0.0886762807947775,
15.5015542669419));
#24026=CARTESIAN_POINT('Ctrl Pts',(-2.53280268327874,0.159355182085626,
15.4898095412493));
#24027=CARTESIAN_POINT('Ctrl Pts',(-2.54130618351024,0.229356191559046,
15.4742714490102));
#24028=CARTESIAN_POINT('Ctrl Pts',(-2.54987758284735,0.298357125319829,
15.454950376115));
#24029=CARTESIAN_POINT('Ctrl Pts',(-2.55591084252828,0.346925688658546,
15.44135060722));
#24030=CARTESIAN_POINT('Ctrl Pts',(-2.56197774287886,0.394998346664019,
15.4258756141398));
#24031=CARTESIAN_POINT('Ctrl Pts',(-2.56808319796508,0.442452970992676,
15.4085168966114));
#24032=CARTESIAN_POINT('Ctrl Pts',(-2.57337296203872,0.483567640310015,
15.3934773100368));
#24033=CARTESIAN_POINT('Ctrl Pts',(-2.57866827746268,0.52409371908305,15.3770890380495));
#24034=CARTESIAN_POINT('Ctrl Pts',(-2.58397493596881,0.563963099394563,
15.3593573159425));
#24035=CARTESIAN_POINT('Ctrl Pts',(-2.5923929959919,0.627208706052391,15.3312291255121));
#24036=CARTESIAN_POINT('Ctrl Pts',(-2.60083959988352,0.688803992220178,
15.2997217492959));
#24037=CARTESIAN_POINT('Ctrl Pts',(-2.60933786728269,0.748496053253066,
15.2649883767521));
#24038=CARTESIAN_POINT('Ctrl Pts',(-2.61771331374979,0.807325416723062,
15.2307569871407));
#24039=CARTESIAN_POINT('Ctrl Pts',(-2.62613894118528,0.864306631227038,
15.193391324339));
#24040=CARTESIAN_POINT('Ctrl Pts',(-2.63463688123865,0.91915493949617,15.1530124968274));
#24041=CARTESIAN_POINT('Ctrl Pts',(-2.6430080517745,0.973185038466007,15.1132360275873));
#24042=CARTESIAN_POINT('Ctrl Pts',(-2.65144939354802,1.0251457497766,15.0705348700075));
#24043=CARTESIAN_POINT('Ctrl Pts',(-2.65998206245267,1.07471716779012,15.0250116008781));
#24044=CARTESIAN_POINT('Ctrl Pts',(-2.66856889690476,1.12460326612508,14.9791993491548));
#24045=CARTESIAN_POINT('Ctrl Pts',(-2.67717652916123,1.17184634124863,14.930832044474));
#24046=CARTESIAN_POINT('Ctrl Pts',(-2.68582721608512,1.21619181790131,14.880055106104));
#24047=CARTESIAN_POINT('Ctrl Pts',(-2.68693017405182,1.22184584251129,14.873581073557));
#24048=CARTESIAN_POINT('Ctrl Pts',(-2.68803383192009,1.22745270054738,14.8670678400251));
#24049=CARTESIAN_POINT('Ctrl Pts',(-2.68913823582054,1.23301180794913,14.8605156828892));
#24050=CARTESIAN_POINT('Ctrl Pts',(-2.69780686600573,1.27664606730464,14.8090868287324));
#24051=CARTESIAN_POINT('Ctrl Pts',(-2.7065214585854,1.317342655988,14.7552605774778));
#24052=CARTESIAN_POINT('Ctrl Pts',(-2.71530432135743,1.35491020711387,14.6992948620781));
#24053=CARTESIAN_POINT('Ctrl Pts',(-2.723931202225,1.39181056596746,14.6443230867067));
#24054=CARTESIAN_POINT('Ctrl Pts',(-2.73262394988786,1.42569206891259,14.587286214873));
#24055=CARTESIAN_POINT('Ctrl Pts',(-2.74140370458174,1.45632354330652,14.5284296470777));
#24056=CARTESIAN_POINT('Ctrl Pts',(-2.74485822024362,1.46837591968032,14.5052717181443));
#24057=CARTESIAN_POINT('Ctrl Pts',(-2.74832620579143,1.47992459466916,14.4818321617964));
#24058=CARTESIAN_POINT('Ctrl Pts',(-2.75180894895332,1.49095330984029,14.4581264477211));
#24059=CARTESIAN_POINT('Ctrl Pts',(-2.76059084527361,1.51876272003126,14.3983514044491));
#24060=CARTESIAN_POINT('Ctrl Pts',(-2.76941014808247,1.5431441216538,14.3372177086219));
#24061=CARTESIAN_POINT('Ctrl Pts',(-2.77828383165334,1.56394559838933,14.2749870597415));
#24062=CARTESIAN_POINT('Ctrl Pts',(-2.78361136491003,1.57643427439537,14.2376253655986));
#24063=CARTESIAN_POINT('Ctrl Pts',(-2.78895849968681,1.58763161386914,14.199868008425));
#24064=CARTESIAN_POINT('Ctrl Pts',(-2.79432890929644,1.5974957180488,14.1617708044219));
#24065=CARTESIAN_POINT('Ctrl Pts',(-2.7995038989002,1.60700088437512,14.1250598924099));
#24066=CARTESIAN_POINT('Ctrl Pts',(-2.80470050031048,1.6152878476834,14.0880410272743));
#24067=CARTESIAN_POINT('Ctrl Pts',(-2.8099220002496,1.62232851562243,14.0507753415377));
#24068=CARTESIAN_POINT('Ctrl Pts',(-2.81057126118396,1.62320397874565,14.0461415860608));
#24069=CARTESIAN_POINT('Ctrl Pts',(-2.81122090708287,1.6240601616151,14.0415040152221));
#24070=CARTESIAN_POINT('Ctrl Pts',(-2.81187094425713,1.62489704744289,14.0368627492777));
#24071=CARTESIAN_POINT('Ctrl Pts',(-2.81381623018475,1.62740149224743,14.0229734061976));
#24072=CARTESIAN_POINT('Ctrl Pts',(-2.81576502021133,1.62973313669868,14.009050970835));
#24073=CARTESIAN_POINT('Ctrl Pts',(-2.81771748379929,1.6318903765127,13.9950985850967));
#24074=CARTESIAN_POINT('Ctrl Pts',(-2.82545005793353,1.64043395032895,13.9398412897819));
#24075=CARTESIAN_POINT('Ctrl Pts',(-2.833240250158,1.64624395051514,13.8841130893233));
#24076=CARTESIAN_POINT('Ctrl Pts',(-2.84109858067896,1.64923640968078,13.8281266562807));
#24077=CARTESIAN_POINT('Ctrl Pts',(-2.84193367124711,1.64955441290273,13.8221770793249));
#24078=CARTESIAN_POINT('Ctrl Pts',(-2.84276953130881,1.64984057390514,13.8162246004353));
#24079=CARTESIAN_POINT('Ctrl Pts',(-2.84360617348995,1.65009480603853,13.8102694912202));
#24080=CARTESIAN_POINT('Ctrl Pts',(-2.85053440500889,1.65220010161102,13.7609552487722));
#24081=CARTESIAN_POINT('Ctrl Pts',(-2.85748562231733,1.65210954291448,13.711675457902));
#24082=CARTESIAN_POINT('Ctrl Pts',(-2.86446969399717,1.64981830164746,13.6625695815424));
#24083=CARTESIAN_POINT('Ctrl Pts',(-2.87221299374171,1.64727798294357,13.6081254782596));
#24084=CARTESIAN_POINT('Ctrl Pts',(-2.87999667721129,1.6420328224924,13.553894471909));
#24085=CARTESIAN_POINT('Ctrl Pts',(-2.88783420560974,1.63407416166227,13.5000808184616));
#24086=CARTESIAN_POINT('Ctrl Pts',(-2.89669160433426,1.6250798679638,13.4392645813553));
#24087=CARTESIAN_POINT('Ctrl Pts',(-2.90561777488003,1.61258123845351,13.3789842494571));
#24088=CARTESIAN_POINT('Ctrl Pts',(-2.91463213809415,1.59662058112076,13.3195527785932));
#24089=CARTESIAN_POINT('Ctrl Pts',(-2.92143823922656,1.58456982996219,13.2746803243179));
#24090=CARTESIAN_POINT('Ctrl Pts',(-2.92829461609412,1.57054460426979,13.2302923047606));
#24091=CARTESIAN_POINT('Ctrl Pts',(-2.93520962564436,1.5545508931325,13.1865389682066));
#24092=CARTESIAN_POINT('Ctrl Pts',(-2.94421617859849,1.5337196556274,13.1295518100935));
#24093=CARTESIAN_POINT('Ctrl Pts',(-2.95327041031035,1.50967160688709,13.0739612407976));
#24094=CARTESIAN_POINT('Ctrl Pts',(-2.96239011792779,1.48249585547248,13.0200487040156));
#24095=CARTESIAN_POINT('Ctrl Pts',(-2.96867214801171,1.46377607901678,12.9829115289907));
#24096=CARTESIAN_POINT('Ctrl Pts',(-2.97498524643709,1.44357121811679,12.9465710635193));
#24097=CARTESIAN_POINT('Ctrl Pts',(-2.98133522842137,1.42189964112574,12.9111289027924));
#24098=CARTESIAN_POINT('Ctrl Pts',(-2.98521698496443,1.40865176325903,12.8894630398588));
#24099=CARTESIAN_POINT('Ctrl Pts',(-2.98911252429411,1.39487333007331,12.8681244140488));
#24100=CARTESIAN_POINT('Ctrl Pts',(-2.99302318265689,1.38055563147682,12.8471482007924));
#24101=CARTESIAN_POINT('Ctrl Pts',(-3.00222557049681,1.34686385806242,12.7977879059544));
#24102=CARTESIAN_POINT('Ctrl Pts',(-3.01151167911897,1.31018675736906,12.7504310994907));
#24103=CARTESIAN_POINT('Ctrl Pts',(-3.02089883194599,1.2707144390074,12.7053595163719));
#24104=CARTESIAN_POINT('Ctrl Pts',(-3.02282748276932,1.26260459774779,12.696099270215));
#24105=CARTESIAN_POINT('Ctrl Pts',(-3.02476039888356,1.2543767198893,12.6869356583494));
#24106=CARTESIAN_POINT('Ctrl Pts',(-3.02669773049638,1.24603239893449,12.6778713956583));
#24107=CARTESIAN_POINT('Ctrl Pts',(-3.03587169974251,1.20651900674461,12.634948817708));
#24108=CARTESIAN_POINT('Ctrl Pts',(-3.04510691998591,1.16459151076389,12.5945250929969));
#24109=CARTESIAN_POINT('Ctrl Pts',(-3.05442054614937,1.1204751933185,12.5568057770798));
#24110=CARTESIAN_POINT('Ctrl Pts',(-3.06357860128224,1.07709577693082,12.5197165093038));
#24111=CARTESIAN_POINT('Ctrl Pts',(-3.07281246497777,1.03159910549671,12.485241612509));
#24112=CARTESIAN_POINT('Ctrl Pts',(-3.08213843971222,0.984178358509514,
12.45362145311));
#24113=CARTESIAN_POINT('Ctrl Pts',(-3.08746848512046,0.957076126096147,
12.4355496815032));
#24114=CARTESIAN_POINT('Ctrl Pts',(-3.09282861781865,0.929345098676938,
12.4184112541742));
#24115=CARTESIAN_POINT('Ctrl Pts',(-3.09822187997365,0.901019921332647,
12.4022586271553));
#24116=CARTESIAN_POINT('Ctrl Pts',(-3.10477478547288,0.866604347779572,
12.3826329098479));
#24117=CARTESIAN_POINT('Ctrl Pts',(-3.11137659861426,0.831311551242717,
12.3644620673644));
#24118=CARTESIAN_POINT('Ctrl Pts',(-3.11803278626624,0.795259448582878,
12.3478010539834));
#24119=CARTESIAN_POINT('',(-2.42950819541372,2.0402249837135,13.997475649067));
#24120=CARTESIAN_POINT('Ctrl Pts',(-2.42950819541372,2.0402249837135,13.997475649067));
#24121=CARTESIAN_POINT('Ctrl Pts',(-2.42950819680997,2.03104070784062,14.0351417863892));
#24122=CARTESIAN_POINT('Ctrl Pts',(-2.4295078943495,2.02082185143214,14.0725200484997));
#24123=CARTESIAN_POINT('Ctrl Pts',(-2.4295077739925,2.00958407097205,14.1095684266328));
#24124=CARTESIAN_POINT('Ctrl Pts',(-2.42950772057022,2.0045960122126,14.1260129093958));
#24125=CARTESIAN_POINT('Ctrl Pts',(-2.42950772487925,1.99940718549468,14.1423924033825));
#24126=CARTESIAN_POINT('Ctrl Pts',(-2.42950770490987,1.99401905946343,14.1587033403071));
#24127=CARTESIAN_POINT('Ctrl Pts',(-2.42950769825192,1.99222261438882,14.164141539438));
#24128=CARTESIAN_POINT('Ctrl Pts',(-2.42950768941003,1.99040401448508,14.1695721175525));
#24129=CARTESIAN_POINT('Ctrl Pts',(-2.42950768353223,1.98856330462253,14.1749949442969));
#24130=CARTESIAN_POINT('Ctrl Pts',(-2.42950763650018,1.97383462039571,14.2183864120994));
#24131=CARTESIAN_POINT('Ctrl Pts',(-2.42950748653377,1.95769054165353,14.2612816804408));
#24132=CARTESIAN_POINT('Ctrl Pts',(-2.42950667483392,1.94015919913297,14.3036098434447));
#24133=CARTESIAN_POINT('Ctrl Pts',(-2.42950537091809,1.91199682484255,14.3716058664614));
#24134=CARTESIAN_POINT('Ctrl Pts',(-2.42953396383665,1.88022422208483,14.4381290972791));
#24135=CARTESIAN_POINT('Ctrl Pts',(-2.42955788537467,1.84497965647924,14.5029147018465));
#24136=CARTESIAN_POINT('Ctrl Pts',(-2.42958299061506,1.80799109448428,14.5709060732749));
#24137=CARTESIAN_POINT('Ctrl Pts',(-2.42960241503354,1.76731073394805,14.6367401361202));
#24138=CARTESIAN_POINT('Ctrl Pts',(-2.42960150222464,1.72316139552393,14.7001318258739));
#24139=CARTESIAN_POINT('Ctrl Pts',(-2.42960058952012,1.67901710536999,14.7635162670846));
#24140=CARTESIAN_POINT('Ctrl Pts',(-2.42957934719993,1.63140464193822,14.8244588516644));
#24141=CARTESIAN_POINT('Ctrl Pts',(-2.42955053246563,1.58052679997558,14.8826620204458));
#24142=CARTESIAN_POINT('Ctrl Pts',(-2.42954063326503,1.56304789635725,14.9026575143223));
#24143=CARTESIAN_POINT('Ctrl Pts',(-2.42953007693327,1.54518342161295,14.9223295821176));
#24144=CARTESIAN_POINT('Ctrl Pts',(-2.42952011418379,1.52694101005491,14.9416657949728));
#24145=CARTESIAN_POINT('Ctrl Pts',(-2.42949966636738,1.48949979133883,14.9813519610452));
#24146=CARTESIAN_POINT('Ctrl Pts',(-2.42948144177566,1.45058462751578,15.0194988701834));
#24147=CARTESIAN_POINT('Ctrl Pts',(-2.42948064766016,1.41028422127532,15.0560257229549));
#24148=CARTESIAN_POINT('Ctrl Pts',(-2.42947952101429,1.35310829921469,15.1078479421833));
#24149=CARTESIAN_POINT('Ctrl Pts',(-2.42951234976274,1.293143106258,15.1564118688575));
#24150=CARTESIAN_POINT('Ctrl Pts',(-2.42953875010086,1.23069375916773,15.2015470634631));
#24151=CARTESIAN_POINT('Ctrl Pts',(-2.42956521275925,1.16809699500034,15.2467888035935));
#24152=CARTESIAN_POINT('Ctrl Pts',(-2.42958504927452,1.10300405208996,15.2885852272081));
#24153=CARTESIAN_POINT('Ctrl Pts',(-2.42958398637795,1.03571625753847,15.3267370412771));
#24154=CARTESIAN_POINT('Ctrl Pts',(-2.42958311156895,0.980335546350388,
15.3581376037467));
#24155=CARTESIAN_POINT('Ctrl Pts',(-2.42956855809535,0.923467978597577,
15.3870688303849));
#24156=CARTESIAN_POINT('Ctrl Pts',(-2.42954659138197,0.865279467155291,
15.4134073011364));
#24157=CARTESIAN_POINT('Ctrl Pts',(-2.42951986269709,0.794476777723754,
15.4454554583842));
#24158=CARTESIAN_POINT('Ctrl Pts',(-2.42948178901242,0.722099894650869,
15.4734932183326));
#24159=CARTESIAN_POINT('Ctrl Pts',(-2.42946854755221,0.648485392194134,
15.4974073194238));
#24160=CARTESIAN_POINT('Ctrl Pts',(-2.42946622137184,0.635553237597292,
15.5016084053788));
#24161=CARTESIAN_POINT('Ctrl Pts',(-2.42946472289851,0.62258280157832,15.5056821886663));
#24162=CARTESIAN_POINT('Ctrl Pts',(-2.42946432430103,0.609575796683492,
15.5096279967501));
#24163=CARTESIAN_POINT('Ctrl Pts',(-2.42946205900156,0.53565470480022,15.5320527166816));
#24164=CARTESIAN_POINT('Ctrl Pts',(-2.42949335707758,0.460551672769708,
15.5503467455696));
#24165=CARTESIAN_POINT('Ctrl Pts',(-2.42951843576671,0.38461200192984,15.5644684273091));
#24166=CARTESIAN_POINT('Ctrl Pts',(-2.42954349448136,0.308732814924717,
15.578578861522));
#24167=CARTESIAN_POINT('Ctrl Pts',(-2.42956216754896,0.232018215097528,
15.5885231154159));
#24168=CARTESIAN_POINT('Ctrl Pts',(-2.42956073494453,0.154822861515672,
15.5942314929807));
#24169=CARTESIAN_POINT('Ctrl Pts',(-2.42956023651616,0.127965235290666,
15.5962175383043));
#24170=CARTESIAN_POINT('Ctrl Pts',(-2.4295575461063,0.101049510913713,15.5976906247383));
#24171=CARTESIAN_POINT('Ctrl Pts',(-2.4295528717745,0.074090926958688,15.5986471294928));
#24172=CARTESIAN_POINT('Ctrl Pts',(-2.42953939803581,-0.00361706023941163,
15.6014042497977));
#24173=CARTESIAN_POINT('Ctrl Pts',(-2.42950755976971,-0.0812632159739146,
15.5998562556563));
#24174=CARTESIAN_POINT('Ctrl Pts',(-2.42948139432591,-0.158486510405496,
15.5940383169824));
#24175=CARTESIAN_POINT('Ctrl Pts',(-2.42946441726226,-0.208591710033162,
15.590263432981));
#24176=CARTESIAN_POINT('Ctrl Pts',(-2.42945039794091,-0.258519331802215,
15.5846905206051));
#24177=CARTESIAN_POINT('Ctrl Pts',(-2.42945157053088,-0.308175379396695,
15.5773227319512));
#24178=CARTESIAN_POINT('Ctrl Pts',(-2.42945337836478,-0.384732307896107,
15.5659634857667));
#24179=CARTESIAN_POINT('Ctrl Pts',(-2.42949008892026,-0.460646632046284,
15.5503387762186));
#24180=CARTESIAN_POINT('Ctrl Pts',(-2.42952017157432,-0.535581221553956,
15.5305421991785));
#24181=CARTESIAN_POINT('Ctrl Pts',(-2.42954627109418,-0.600593996101206,
15.513366814508));
#24182=CARTESIAN_POINT('Ctrl Pts',(-2.42956765411205,-0.664868833921869,
15.4930505486365));
#24183=CARTESIAN_POINT('Ctrl Pts',(-2.42957323886436,-0.728169658321024,
15.4696424099624));
#24184=CARTESIAN_POINT('Ctrl Pts',(-2.6276958156896,1.52655665885959E-16,
11.6014907459511));
#24185=CARTESIAN_POINT('Ctrl Pts',(-2.62394006512444,0.0653215041544882,
11.5976723995432));
#24186=CARTESIAN_POINT('Ctrl Pts',(-2.62018977471018,0.130839214337266,
11.5972317286682));
#24187=CARTESIAN_POINT('Ctrl Pts',(-2.60924600079219,0.321708528580622,
11.605764455657));
#24188=CARTESIAN_POINT('Ctrl Pts',(-2.60206759657853,0.446362335031581,
11.6237172245559));
#24189=CARTESIAN_POINT('Ctrl Pts',(-2.58787639794491,0.689733221082812,
11.6835386074477));
#24190=CARTESIAN_POINT('Ctrl Pts',(-2.58088693136192,0.807990259168507,
11.7251684660431));
#24191=CARTESIAN_POINT('Ctrl Pts',(-2.566729012865,1.0376094825962,11.8316904957494));
#24192=CARTESIAN_POINT('Ctrl Pts',(-2.55958384779881,1.14832818180093,11.8969492545597));
#24193=CARTESIAN_POINT('Ctrl Pts',(-2.5454256196204,1.35516943309115,12.0478477449589));
#24194=CARTESIAN_POINT('Ctrl Pts',(-2.53844069958128,1.45094868699436,12.1331852719129));
#24195=CARTESIAN_POINT('Ctrl Pts',(-2.51696790688888,1.71765987875923,12.4211611768747));
#24196=CARTESIAN_POINT('Ctrl Pts',(-2.50269556727083,1.85703571789682,12.6487824541898));
#24197=CARTESIAN_POINT('Ctrl Pts',(-2.48361000855449,1.98085492461562,12.983639184611));
#24198=CARTESIAN_POINT('Ctrl Pts',(-2.47872042512685,2.00684884077783,13.071830082245));
#24199=CARTESIAN_POINT('Ctrl Pts',(-2.46638211843693,2.05734586452424,13.2980002064133));
#24200=CARTESIAN_POINT('Ctrl Pts',(-2.45897955765079,2.07380945906283,13.4372088906499));
#24201=CARTESIAN_POINT('Ctrl Pts',(-2.44419130460703,2.07839281191841,13.7182033191773));
#24202=CARTESIAN_POINT('Ctrl Pts',(-2.43683437473473,2.06633102056939,13.8589688601983));
#24203=CARTESIAN_POINT('Ctrl Pts',(-2.42949658771307,2.0402367405008,13.9974772490428));
#24204=CARTESIAN_POINT('',(-2.76,2.16027695369593E-16,11.736));
#24205=CARTESIAN_POINT('Origin',(2.76,0.,13.5));
#24206=CARTESIAN_POINT('',(2.42946620026141,0.728215466689312,15.4697414959281));
#24207=CARTESIAN_POINT('Ctrl Pts',(2.4295428593244,0.728207872842018,15.4696612109339));
#24208=CARTESIAN_POINT('Ctrl Pts',(2.45091245476581,0.544260182117664,15.5145058956143));
#24209=CARTESIAN_POINT('Ctrl Pts',(2.47243403011723,0.353895986727487,15.5344506012717));
#24210=CARTESIAN_POINT('Ctrl Pts',(2.51574798427622,-0.0184887986635827,
15.5203893841951));
#24211=CARTESIAN_POINT('Ctrl Pts',(2.53729267461328,-0.198366817608611,
15.4886959758906));
#24212=CARTESIAN_POINT('Ctrl Pts',(2.57335815717529,-0.484693670484068,
15.396371826893));
#24213=CARTESIAN_POINT('Ctrl Pts',(2.58772300656413,-0.594462359872026,
15.3495656517267));
#24214=CARTESIAN_POINT('Ctrl Pts',(2.61758761270735,-0.808160240452916,
15.2336270291036));
#24215=CARTESIAN_POINT('Ctrl Pts',(2.63300531424843,-0.910881098739636,
15.1641102349212));
#24216=CARTESIAN_POINT('Ctrl Pts',(2.67898127911371,-1.19167129608836,14.9304922263634));
#24217=CARTESIAN_POINT('Ctrl Pts',(2.70945231761375,-1.34589255217788,14.7416369283767));
#24218=CARTESIAN_POINT('Ctrl Pts',(2.75688651831879,-1.51006470327172,14.4249429786798));
#24219=CARTESIAN_POINT('Ctrl Pts',(2.77232144014209,-1.55283890794701,14.3180479678811));
#24220=CARTESIAN_POINT('Ctrl Pts',(2.80297552759952,-1.61574634612789,14.1008746920454));
#24221=CARTESIAN_POINT('Ctrl Pts',(2.81822477516551,-1.636289288732,13.99103340657));
#24222=CARTESIAN_POINT('Ctrl Pts',(2.86341962914337,-1.66363957104621,13.6682439161839));
#24223=CARTESIAN_POINT('Ctrl Pts',(2.8936148904857,-1.64104738498822,13.4542373098146));
#24224=CARTESIAN_POINT('Ctrl Pts',(2.95523022888075,-1.5150429038044,13.0571671419898));
#24225=CARTESIAN_POINT('Ctrl Pts',(2.98583545551893,-1.41570656735004,12.8748297123451));
#24226=CARTESIAN_POINT('Ctrl Pts',(3.0341141182629,-1.21525684562294,12.6397726471057));
#24227=CARTESIAN_POINT('Ctrl Pts',(3.05076154939996,-1.13920589486915,12.5677922695722));
#24228=CARTESIAN_POINT('Ctrl Pts',(3.07606134278261,-1.01540336829484,12.4739551790739));
#24229=CARTESIAN_POINT('Ctrl Pts',(3.08439653127644,-0.973317553865625,
12.4454466927866));
#24230=CARTESIAN_POINT('Ctrl Pts',(3.10110102258154,-0.886501873825729,
12.3931612938824));
#24231=CARTESIAN_POINT('Ctrl Pts',(3.10951634275777,-0.841391123218596,
12.3691213536139));
#24232=CARTESIAN_POINT('Ctrl Pts',(3.11803278688524,-0.79526461825914,12.3478046229284));
#24233=CARTESIAN_POINT('',(2.42950897538817,-2.04022719656258,13.9974632264163));
#24234=CARTESIAN_POINT('Ctrl Pts',(2.42950897535609,-2.04022719645617,13.9974632268527));
#24235=CARTESIAN_POINT('Ctrl Pts',(2.42950872897253,-2.00274565249741,14.1511859288549));
#24236=CARTESIAN_POINT('Ctrl Pts',(2.42930928961135,-1.94798539314298,14.3007710907449));
#24237=CARTESIAN_POINT('Ctrl Pts',(2.42923224593775,-1.80707757751576,14.5816641247516));
#24238=CARTESIAN_POINT('Ctrl Pts',(2.42952850076456,-1.72154152557879,14.7125426586374));
#24239=CARTESIAN_POINT('Ctrl Pts',(2.42971570504825,-1.50237106737774,14.9792353537282));
#24240=CARTESIAN_POINT('Ctrl Pts',(2.42911821842147,-1.30001519781745,15.1877063217083));
#24241=CARTESIAN_POINT('Ctrl Pts',(2.42962442410881,-0.773863563946308,
15.4667317038028));
#24242=CARTESIAN_POINT('Ctrl Pts',(2.42929816410876,-0.508411158962302,
15.5612192539789));
#24243=CARTESIAN_POINT('Ctrl Pts',(2.42960691697754,-0.0439201933795526,
15.6052575674409));
#24244=CARTESIAN_POINT('Ctrl Pts',(2.42973955557419,0.113432076793043,15.6025240418254));
#24245=CARTESIAN_POINT('Ctrl Pts',(2.42959753284754,0.425077640835638,15.5624814344048));
#24246=CARTESIAN_POINT('Ctrl Pts',(2.42940744355207,0.579271575329576,15.5248698940994));
#24247=CARTESIAN_POINT('Ctrl Pts',(2.42946620026141,0.728215466689312,15.4697414959281));
#24248=CARTESIAN_POINT('',(2.62767578687551,5.23812981406848E-11,11.6014703833234));
#24249=CARTESIAN_POINT('Ctrl Pts',(2.62767578687551,5.23796561680001E-11,
11.6014703833234));
#24250=CARTESIAN_POINT('Ctrl Pts',(2.62098011477951,-0.116414384474613,
11.5946631166893));
#24251=CARTESIAN_POINT('Ctrl Pts',(2.61433244389839,-0.233246843799019,
11.5986165460831));
#24252=CARTESIAN_POINT('Ctrl Pts',(2.60094196653965,-0.466404619323598,
11.6278926160068));
#24253=CARTESIAN_POINT('Ctrl Pts',(2.59422809304221,-0.582218819371836,
11.6534619509933));
#24254=CARTESIAN_POINT('Ctrl Pts',(2.57394533253695,-0.924654145743048,
11.7628407986736));
#24255=CARTESIAN_POINT('Ctrl Pts',(2.56048209332691,-1.13879792156818,11.8782924728836));
#24256=CARTESIAN_POINT('Ctrl Pts',(2.54018166141812,-1.42710311554983,12.1107845923993));
#24257=CARTESIAN_POINT('Ctrl Pts',(2.53322887545074,-1.51904167092177,12.201074994458));
#24258=CARTESIAN_POINT('Ctrl Pts',(2.5116856423392,-1.77388914413096,12.5045620247723));
#24259=CARTESIAN_POINT('Ctrl Pts',(2.4970626279049,-1.90362480482177,12.7420350185755));
#24260=CARTESIAN_POINT('Ctrl Pts',(2.4737929908366,-2.0331806915867,13.1580907394865));
#24261=CARTESIAN_POINT('Ctrl Pts',(2.46501245235341,-2.06306535902456,13.3231803556173));
#24262=CARTESIAN_POINT('Ctrl Pts',(2.45173509424097,-2.07779160731285,13.5745989517968));
#24263=CARTESIAN_POINT('Ctrl Pts',(2.44727333901277,-2.07755004137547,13.6595228653821));
#24264=CARTESIAN_POINT('Ctrl Pts',(2.43837136332853,-2.06665570422367,13.8292367080807));
#24265=CARTESIAN_POINT('Ctrl Pts',(2.43393725252676,-2.0559925643255,13.9138000778369));
#24266=CARTESIAN_POINT('Ctrl Pts',(2.42950458733698,-2.04023164095418,13.9974638311817));
#24267=CARTESIAN_POINT('',(2.76,1.76862604618026E-11,11.736));
#24268=CARTESIAN_POINT('',(3.12,-1.712056225208E-16,12.102));
#24269=CARTESIAN_POINT('',(2.76,-2.16027695369593E-16,11.736));
#24270=CARTESIAN_POINT('Origin',(3.12,0.,13.5));
#24271=CARTESIAN_POINT('Origin',(3.61,0.,13.5));
#24272=CARTESIAN_POINT('',(4.1,-1.712056225208E-16,12.102));
#24273=CARTESIAN_POINT('',(3.61,-1.712056225208E-16,12.102));
#24274=CARTESIAN_POINT('Origin',(4.1,0.,13.5));
#24275=CARTESIAN_POINT('Ctrl Pts',(-2.4295462516368,2.04037572573852,13.9968570253301));
#24276=CARTESIAN_POINT('Ctrl Pts',(-2.42676399539611,2.03115983127861,14.0347026749067));
#24277=CARTESIAN_POINT('Ctrl Pts',(-2.42275455106802,2.0163620858964,14.0888717436244));
#24278=CARTESIAN_POINT('Ctrl Pts',(-2.41833606520329,1.99767985787329,14.1478468672687));
#24279=CARTESIAN_POINT('Ctrl Pts',(-2.41342732442686,1.97585722502828,14.2130128614707));
#24280=CARTESIAN_POINT('Ctrl Pts',(-2.40974577055595,1.95769272238393,14.261277921562));
#24281=CARTESIAN_POINT('Ctrl Pts',(-2.38438395519232,1.82183653240103,14.5893116957435));
#24282=CARTESIAN_POINT('Ctrl Pts',(-2.34020530861667,1.45696855344266,15.1074622666804));
#24283=CARTESIAN_POINT('Ctrl Pts',(-2.2739373382268,0.62977347580106,15.5760953406599));
#24284=CARTESIAN_POINT('Ctrl Pts',(-2.20766936827494,-0.31829920263192,
15.6461013495652));
#24285=CARTESIAN_POINT('Ctrl Pts',(-2.14385576769032,-1.17248093264124,
15.3164944266901));
#24286=CARTESIAN_POINT('Ctrl Pts',(-2.08249653614418,-1.79133169412791,
14.6971225551438));
#24287=CARTESIAN_POINT('Ctrl Pts',(-2.01868293537138,-2.14067149238402,
13.8556172017264));
#24288=CARTESIAN_POINT('Ctrl Pts',(-1.95977807328636,-2.0990703334386,13.0070783687417));
#24289=CARTESIAN_POINT('Ctrl Pts',(-1.9131450572471,-1.81590690250113,12.410569648822));
#24290=CARTESIAN_POINT('Ctrl Pts',(-1.88860136456768,-1.60407022565932,
12.138968949739));
#24291=CARTESIAN_POINT('Ctrl Pts',(-1.87878388758855,-1.50925008150214,
12.0393936930147));
#24292=CARTESIAN_POINT('Ctrl Pts',(-1.8714207797393,-1.43636217244859,11.9664998633223));
#24293=CARTESIAN_POINT('Ctrl Pts',(-1.8566945641682,-1.28341706100303,11.8279079030736));
#24294=CARTESIAN_POINT('Ctrl Pts',(-1.82233339458021,-0.881586233572867,
11.5590960177494));
#24295=CARTESIAN_POINT('Ctrl Pts',(-1.77324600952379,-0.211348166169894,
11.355717775956));
#24296=CARTESIAN_POINT('Ctrl Pts',(-1.70943240871259,0.695366325214471,
11.444765962131));
#24297=CARTESIAN_POINT('Ctrl Pts',(-1.66525376189339,1.24201258995575,11.7719946812417));
#24298=CARTESIAN_POINT('Ctrl Pts',(-1.62352948442918,1.65511419058129,12.1850871361999));
#24299=CARTESIAN_POINT('Ctrl Pts',(-1.58916831486898,1.93554864063555,12.5840848980242));
#24300=CARTESIAN_POINT('Ctrl Pts',(-1.52535471408587,2.17939055703516,13.4583963500157));
#24301=CARTESIAN_POINT('Ctrl Pts',(-1.46154111311181,1.99758949424158,14.3723763583426));
#24302=CARTESIAN_POINT('Ctrl Pts',(-1.3977275123059,1.43775329796456,15.0868868062281));
#24303=CARTESIAN_POINT('Ctrl Pts',(-1.36336634275071,1.02596017097957,15.3480904456428));
#24304=CARTESIAN_POINT('Ctrl Pts',(-1.31673332685749,0.422785352598646,
15.5985301254968));
#24305=CARTESIAN_POINT('Ctrl Pts',(-1.27255468010616,-0.219266399693367,
15.6608495079931));
#24306=CARTESIAN_POINT('Ctrl Pts',(-1.21364981772633,-1.00437124126938,
15.3786380262801));
#24307=CARTESIAN_POINT('Ctrl Pts',(-1.18419738671256,-1.33912457693599,
15.1307661354804));
#24308=CARTESIAN_POINT('Ctrl Pts',(-1.14983621711478,-1.6792932828141,14.7905634620183));
#24309=CARTESIAN_POINT('Ctrl Pts',(-1.13020126291748,-1.83495172588154,
14.557619759006));
#24310=CARTESIAN_POINT('Ctrl Pts',(-1.10565757040559,-1.96644792402424,
14.240164168935));
#24311=CARTESIAN_POINT('Ctrl Pts',(-1.09829446266241,-2.00122704859806,
14.1429882818207));
#24312=CARTESIAN_POINT('Ctrl Pts',(-1.0835682468725,-2.05621222310087,13.9442324744642));
#24313=CARTESIAN_POINT('Ctrl Pts',(-1.05411581628574,-2.12713274945685,
13.5368487102677));
#24314=CARTESIAN_POINT('Ctrl Pts',(-1.01730027703454,-2.07558331110669,
13.0140445022799));
#24315=CARTESIAN_POINT('Ctrl Pts',(-0.978030368980419,-1.86393795722917,
12.5036741054457));
#24316=CARTESIAN_POINT('Ctrl Pts',(-0.953486676180038,-1.67220003622907,
12.2165761921044));
#24317=CARTESIAN_POINT('Ctrl Pts',(-0.938760460748136,-1.53355113591613,
12.0636380569739));
#24318=CARTESIAN_POINT('Ctrl Pts',(-0.92403424516514,-1.38777482274071,
11.9178520451545));
#24319=CARTESIAN_POINT('Ctrl Pts',(-0.904399291043347,-1.1742634362821,
11.7425661865439));
#24320=CARTESIAN_POINT('Ctrl Pts',(-0.884764336947749,-0.930655306467975,
11.6124317243282));
#24321=CARTESIAN_POINT('Ctrl Pts',(-0.84549442877046,-0.422795803049391,
11.4014872112732));
#24322=CARTESIAN_POINT('Ctrl Pts',(-0.798861412839077,0.255001957070318,
11.335773527586));
#24323=CARTESIAN_POINT('Ctrl Pts',(-0.735047811954554,1.10113310782084,
11.6633392165017));
#24324=CARTESIAN_POINT('Ctrl Pts',(-0.685960426710027,1.62914331739752,
12.1183931288629));
#24325=CARTESIAN_POINT('Ctrl Pts',(-0.654053626379446,1.86126704948603,
12.5059440282019));
#24326=CARTESIAN_POINT('Ctrl Pts',(-0.624601195412295,2.01907157883037,
12.8868615420783));
#24327=CARTESIAN_POINT('Ctrl Pts',(-0.600057502795961,2.10343342036855,
13.2238084748929));
#24328=CARTESIAN_POINT('Ctrl Pts',(-0.570605071587877,2.10336458500336,
13.6381488881852));
#24329=CARTESIAN_POINT('Ctrl Pts',(-0.546061378980283,2.05290020198756,
13.9784521638003));
#24330=CARTESIAN_POINT('Ctrl Pts',(-0.53133516342537,1.99278329430259,14.1767068394653));
#24331=CARTESIAN_POINT('Ctrl Pts',(-0.519063317041293,1.92703808468239,
14.3354372284454));
#24332=CARTESIAN_POINT('Ctrl Pts',(-0.514154578439539,1.8991827786045,14.398284675188));
#24333=CARTESIAN_POINT('Ctrl Pts',(-0.504337101639833,1.83736662386643,
14.5210899579476));
#24334=CARTESIAN_POINT('Ctrl Pts',(-0.487156516667517,1.7135883000647,14.7276726331592));
#24335=CARTESIAN_POINT('Ctrl Pts',(-0.472430301157928,1.58214497145923,
14.8877980148624));
#24336=CARTESIAN_POINT('Ctrl Pts',(-0.435614762275021,1.2179310545379,15.2525189427683));
#24337=CARTESIAN_POINT('Ctrl Pts',(-0.381618638640641,0.535697183972207,
15.6386283611074));
#24338=CARTESIAN_POINT('Ctrl Pts',(-0.298170083766961,-0.675545338924911,
15.6090937700565));
#24339=CARTESIAN_POINT('Ctrl Pts',(-0.207358420958111,-1.78071661015833,
14.8720476608843));
#24340=CARTESIAN_POINT('Ctrl Pts',(-0.143544820167066,-2.10078048070695,
13.9811745633393));
#24341=CARTESIAN_POINT('Ctrl Pts',(-0.0748224810432098,-2.10079571528789,
13.018892234084));
#24342=CARTESIAN_POINT('Ctrl Pts',(-0.0110088802683666,-1.78076034062204,
12.1280093081936));
#24343=CARTESIAN_POINT('Ctrl Pts',(0.0798027825760428,-0.675612415650728,
11.3909286410548));
#24344=CARTESIAN_POINT('Ctrl Pts',(0.163251337403203,0.535627767915652,
11.3613573628603));
#24345=CARTESIAN_POINT('Ctrl Pts',(0.217247461051789,1.21787351269776,11.7474459840713));
#24346=CARTESIAN_POINT('Ctrl Pts',(0.254062999989602,1.58209728013173,12.1121568182762));
#24347=CARTESIAN_POINT('Ctrl Pts',(0.26633484629195,1.69164149438975,12.2455893496679));
#24348=CARTESIAN_POINT('Ctrl Pts',(0.281061061609305,1.80196383977949,12.4198331801394));
#24349=CARTESIAN_POINT('Ctrl Pts',(0.290878538947051,1.86973551168152,12.539455210692));
#24350=CARTESIAN_POINT('Ctrl Pts',(0.298241646680488,1.91386222842472,12.632757087791));
#24351=CARTESIAN_POINT('Ctrl Pts',(0.308059123789946,1.96646043482015,12.7597400679814));
#24352=CARTESIAN_POINT('Ctrl Pts',(0.322785339298095,2.03602087158878,12.9540884692955));
#24353=CARTESIAN_POINT('Ctrl Pts',(0.347329031870305,2.10336694998667,13.2927234020508));
#24354=CARTESIAN_POINT('Ctrl Pts',(0.381690201597044,2.10342891367037,13.7761229454928));
#24355=CARTESIAN_POINT('Ctrl Pts',(0.40623389420153,2.01909426618207,14.1130728120558));
#24356=CARTESIAN_POINT('Ctrl Pts',(0.435686325163057,1.8613003699308,14.4939896139498));
#24357=CARTESIAN_POINT('Ctrl Pts',(0.467593125498422,1.62918101096397,14.8816101604613));
#24358=CARTESIAN_POINT('Ctrl Pts',(0.516680510744503,1.10120661715989,15.3365095698264));
#24359=CARTESIAN_POINT('Ctrl Pts',(0.580494111628017,0.255029767888532,
15.6645333138311));
#24360=CARTESIAN_POINT('Ctrl Pts',(0.636944604582806,-0.565351704997995,
15.5841353192661));
#24361=CARTESIAN_POINT('Ctrl Pts',(0.686031989830427,-1.17415741609758,
15.257079999352));
#24362=CARTESIAN_POINT('Ctrl Pts',(0.705666943950803,-1.38772915100266,
15.0822244571842));
#24363=CARTESIAN_POINT('Ctrl Pts',(0.720393159536148,-1.53350604431233,
14.9364120026342));
#24364=CARTESIAN_POINT('Ctrl Pts',(0.735119374971491,-1.67216060831638,
14.7834847823105));
#24365=CARTESIAN_POINT('Ctrl Pts',(0.759663067736636,-1.86390687171186,
14.4963874011454));
#24366=CARTESIAN_POINT('Ctrl Pts',(0.798932975863961,-2.07556857418935,
13.9860258561317));
#24367=CARTESIAN_POINT('Ctrl Pts',(0.835748515047526,-2.12713404052499,
13.4632196613971));
#24368=CARTESIAN_POINT('Ctrl Pts',(0.865200945667048,-2.05622636621962,
13.0558339354759));
#24369=CARTESIAN_POINT('Ctrl Pts',(0.879927161444758,-2.00124743186629,
12.8570763057862));
#24370=CARTESIAN_POINT('Ctrl Pts',(0.887290269190745,-1.96647136320517,
12.75989931555));
#24371=CARTESIAN_POINT('Ctrl Pts',(0.911833961708695,-1.83498513568377,
12.4424394580257));
#24372=CARTESIAN_POINT('Ctrl Pts',(0.931468915902892,-1.67933397373734,
12.2094904271853));
#24373=CARTESIAN_POINT('Ctrl Pts',(0.965830085499491,-1.33917594806349,
11.8692768701963));
#24374=CARTESIAN_POINT('Ctrl Pts',(0.99528251651406,-1.00443038587671,11.6213942448987));
#24375=CARTESIAN_POINT('Ctrl Pts',(1.05418737889393,-0.219334396744861,
11.3391578691636));
#24376=CARTESIAN_POINT('Ctrl Pts',(1.09836602564571,0.422719333041569,11.4014569267992));
#24377=CARTESIAN_POINT('Ctrl Pts',(1.14499904153829,1.02590204107926,11.6518775623672));
#24378=CARTESIAN_POINT('Ctrl Pts',(1.17936021109236,1.43770339847263,11.9130681734602));
#24379=CARTESIAN_POINT('Ctrl Pts',(1.24317381189954,1.99756208939828,12.627560943781));
#24380=CARTESIAN_POINT('Ctrl Pts',(1.30698741287357,2.1793919241302,13.5415351936699));
#24381=CARTESIAN_POINT('Ctrl Pts',(1.37080101365562,1.93557754847214,14.4158542879512));
#24382=CARTESIAN_POINT('Ctrl Pts',(1.40516218321472,1.65515568903686,14.8148608582693));
#24383=CARTESIAN_POINT('Ctrl Pts',(1.44688646067973,1.24206712723018,15.2279662967193));
#24384=CARTESIAN_POINT('Ctrl Pts',(1.49106510750054,0.695431288255876,15.5552121917209));
#24385=CARTESIAN_POINT('Ctrl Pts',(1.55487870831301,-0.211280294656861,
15.6442888912545));
#24386=CARTESIAN_POINT('Ctrl Pts',(1.60396609336863,-0.881524522312744,
15.4409317243134));
#24387=CARTESIAN_POINT('Ctrl Pts',(1.63832726295486,-1.28336371294544,15.1721324773309));
#24388=CARTESIAN_POINT('Ctrl Pts',(1.65305347852583,-1.43631314893798,15.0335453274474));
#24389=CARTESIAN_POINT('Ctrl Pts',(1.66041658637534,-1.50920334155228,14.9606537902615));
#24390=CARTESIAN_POINT('Ctrl Pts',(1.67023406335438,-1.60402660101632,14.8610815159075));
#24391=CARTESIAN_POINT('Ctrl Pts',(1.69477775603514,-1.81587172112341,14.5894874803237));
#24392=CARTESIAN_POINT('Ctrl Pts',(1.74141077207343,-2.09905323873564,13.9929876745797));
#24393=CARTESIAN_POINT('Ctrl Pts',(1.80031563416003,-2.14068062617532,13.1444501566802));
#24394=CARTESIAN_POINT('Ctrl Pts',(1.86412923492969,-1.79136523454947,12.3029338445012));
#24395=CARTESIAN_POINT('Ctrl Pts',(1.92548846647922,-1.17253132238636,11.6835425466965));
#24396=CARTESIAN_POINT('Ctrl Pts',(1.98930206706247,-0.318356075436173,
11.3539088134527));
#24397=CARTESIAN_POINT('Ctrl Pts',(2.05557003701416,0.629726925134857,11.4238851191756));
#24398=CARTESIAN_POINT('Ctrl Pts',(2.1218380074072,1.45694422261059,11.8924922830572));
#24399=CARTESIAN_POINT('Ctrl Pts',(2.16601665398091,1.82184455239142,12.4106316046563));
#24400=CARTESIAN_POINT('Ctrl Pts',(2.19137846934136,1.95771445605756,12.7386611556245));
#24401=CARTESIAN_POINT('Ctrl Pts',(2.19506002321179,1.97588078470422,12.7869256444275));
#24402=CARTESIAN_POINT('Ctrl Pts',(2.19996876398827,1.99770550570674,12.8520909604627));
#24403=CARTESIAN_POINT('Ctrl Pts',(2.2065137316803,2.02538213011809,12.9394480697009));
#24404=CARTESIAN_POINT('Ctrl Pts',(2.21755844451523,2.06300081475712,13.0896209287977));
#24405=CARTESIAN_POINT('Ctrl Pts',(2.23228457099678,2.0932917010527,13.2938014535001));
#24406=CARTESIAN_POINT('Ctrl Pts',(2.24210211668464,2.10004670844963,13.4312473488259));
#24407=CARTESIAN_POINT('Ctrl Pts',(2.26664587493493,2.10005562155831,13.7748621762512));
#24408=CARTESIAN_POINT('Ctrl Pts',(2.28628054219918,2.04541956405879,14.0496593153248));
#24409=CARTESIAN_POINT('Ctrl Pts',(2.30837007995999,1.92707046676835,14.3353692677506));
#24410=CARTESIAN_POINT('Ctrl Pts',(2.33291408542307,1.78788494078656,14.6496709541517));
#24411=CARTESIAN_POINT('Ctrl Pts',(2.37709177928891,1.39799452919363,15.1490237584087));
#24412=CARTESIAN_POINT('Ctrl Pts',(2.44090672233169,0.5945258343695,15.578593294924));
#24413=CARTESIAN_POINT('Ctrl Pts',(2.50471913818021,-0.318078252393418,
15.6459868908612));
#24414=CARTESIAN_POINT('Ctrl Pts',(2.57344108274706,-1.23849201601544,15.2914055940067));
#24415=CARTESIAN_POINT('Ctrl Pts',(2.63266364818555,-1.81210740078466,14.6585754201023));
#24416=CARTESIAN_POINT('Ctrl Pts',(2.6697881072228,-1.99847008378947,14.1687025596367));
#24417=CARTESIAN_POINT('Ctrl Pts',(2.68237314822326,-2.04021308540786,13.9975277660334));
#24418=CARTESIAN_POINT('Ctrl Pts',(-2.51383678391223,2.04037051569869,13.9968784157014));
#24419=CARTESIAN_POINT('Ctrl Pts',(-2.51105452767153,2.03115422555428,14.0347239687683));
#24420=CARTESIAN_POINT('Ctrl Pts',(-2.50704508334344,2.01635591393393,14.0888928831956));
#24421=CARTESIAN_POINT('Ctrl Pts',(-2.50262659747871,1.99767306539875,14.1478678099595));
#24422=CARTESIAN_POINT('Ctrl Pts',(-2.49771785670229,1.97584974973882,14.2130335759246));
#24423=CARTESIAN_POINT('Ctrl Pts',(-2.49403630283137,1.95768474123331,14.261298444883));
#24424=CARTESIAN_POINT('Ctrl Pts',(-2.46867448746776,1.82182511115358,14.5893307981028));
#24425=CARTESIAN_POINT('Ctrl Pts',(-2.42449584089209,1.45695170113379,15.1074775399189));
#24426=CARTESIAN_POINT('Ctrl Pts',(-2.35822787050222,0.629751710402464,
15.5761019436571));
#24427=CARTESIAN_POINT('Ctrl Pts',(-2.29195990055035,-0.318321701676844,
15.6460980120573));
#24428=CARTESIAN_POINT('Ctrl Pts',(-2.22814629996575,-1.17249997604108,
15.3164821347062));
#24429=CARTESIAN_POINT('Ctrl Pts',(-2.1667870684196,-1.79134424397442,14.6971037747127));
#24430=CARTESIAN_POINT('Ctrl Pts',(-2.10297346764681,-2.14067522041323,
13.8555947608319));
#24431=CARTESIAN_POINT('Ctrl Pts',(-2.04406860556179,-2.09906516524119,
13.0070563621922));
#24432=CARTESIAN_POINT('Ctrl Pts',(-1.99743558952253,-1.81589548119543,
12.4105506139921));
#24433=CARTESIAN_POINT('Ctrl Pts',(-1.97289189684311,-1.60405595666689,
12.1389521317244));
#24434=CARTESIAN_POINT('Ctrl Pts',(-1.96307441986398,-1.50923476887834,
12.0393778713429));
#24435=CARTESIAN_POINT('Ctrl Pts',(-1.95571131201473,-1.43634609502682,
11.9664848049889));
#24436=CARTESIAN_POINT('Ctrl Pts',(-1.94098509644363,-1.28339953200227,
11.8278944487704));
#24437=CARTESIAN_POINT('Ctrl Pts',(-1.90662392685564,-0.881565884890355,
11.5590867757594));
#24438=CARTESIAN_POINT('Ctrl Pts',(-1.85753654179922,-0.211325685334219,
11.3557155604428));
#24439=CARTESIAN_POINT('Ctrl Pts',(-1.79372294098802,0.695387870237467,
11.4447732528524));
#24440=CARTESIAN_POINT('Ctrl Pts',(-1.74954429416882,1.24203070958418,11.7720077023501));
#24441=CARTESIAN_POINT('Ctrl Pts',(-1.70782001670461,1.65512797284224,12.1851044890556));
#24442=CARTESIAN_POINT('Ctrl Pts',(-1.6734588471444,1.93555824400004,12.584105187986));
#24443=CARTESIAN_POINT('Ctrl Pts',(-1.6096452463613,2.17939099147149,13.4584191984726));
#24444=CARTESIAN_POINT('Ctrl Pts',(-1.54583164538723,1.99758034946137,14.3723973010337));
#24445=CARTESIAN_POINT('Ctrl Pts',(-1.48201804458132,1.43773666005063,15.0869018769287));
#24446=CARTESIAN_POINT('Ctrl Pts',(-1.44765687502613,1.02594079907934,15.3481012030357));
#24447=CARTESIAN_POINT('Ctrl Pts',(-1.40102385913291,0.422763348534303,
15.5985345560026));
#24448=CARTESIAN_POINT('Ctrl Pts',(-1.35684521238158,-0.219289053323828,
15.6608472100048));
#24449=CARTESIAN_POINT('Ctrl Pts',(-1.29794035000175,-1.00439093500475,
15.3786274956859));
#24450=CARTESIAN_POINT('Ctrl Pts',(-1.26848791898798,-1.33914167588447,
15.1307520966607));
#24451=CARTESIAN_POINT('Ctrl Pts',(-1.2341267493902,-1.67930680851392,14.7905458562925));
#24452=CARTESIAN_POINT('Ctrl Pts',(-1.21449179519291,-1.8349628189688,14.5576005194465));
#24453=CARTESIAN_POINT('Ctrl Pts',(-1.18994810268102,-1.96645568244719,
14.2401435539693));
#24454=CARTESIAN_POINT('Ctrl Pts',(-1.18258499493783,-2.0012337895352,14.1429673007638));
#24455=CARTESIAN_POINT('Ctrl Pts',(-1.16785877914793,-2.05621688004258,
13.9442109190832));
#24456=CARTESIAN_POINT('Ctrl Pts',(-1.13840634856118,-2.12713313546642,
13.5368264082867));
#24457=CARTESIAN_POINT('Ctrl Pts',(-1.10159080930997,-2.07557821659641,
13.0140227425138));
#24458=CARTESIAN_POINT('Ctrl Pts',(-1.06232090125584,-1.86392751211601,
12.5036545650749));
#24459=CARTESIAN_POINT('Ctrl Pts',(-1.03777720845546,-1.6721865817914,12.2165586611969));
#24460=CARTESIAN_POINT('Ctrl Pts',(-1.02305099302356,-1.53353607750216,
12.0636219802384));
#24461=CARTESIAN_POINT('Ctrl Pts',(-1.00832477744056,-1.38775823789867,
11.9178374965157));
#24462=CARTESIAN_POINT('Ctrl Pts',(-0.988689823318778,-1.17424500879164,
11.7425538760864));
#24463=CARTESIAN_POINT('Ctrl Pts',(-0.969054869223174,-0.930635521833597,
11.6124219684523));
#24464=CARTESIAN_POINT('Ctrl Pts',(-0.929784961045884,-0.422773795796279,
11.4014827783018));
#24465=CARTESIAN_POINT('Ctrl Pts',(-0.883151945114507,0.255024643293703,
11.3357762016639));
#24466=CARTESIAN_POINT('Ctrl Pts',(-0.819338344229977,1.10115236427924,
11.6633507604566));
#24467=CARTESIAN_POINT('Ctrl Pts',(-0.770250958985457,1.62915780240659,
12.1184102084985));
#24468=CARTESIAN_POINT('Ctrl Pts',(-0.738344158654869,1.86127747045704,
12.5059635409483));
#24469=CARTESIAN_POINT('Ctrl Pts',(-0.708891727687721,2.01907800775109,
12.8868827095552));
#24470=CARTESIAN_POINT('Ctrl Pts',(-0.684348035071388,2.10343631582984,
13.223830526392));
#24471=CARTESIAN_POINT('Ctrl Pts',(-0.654895603863301,2.10336313724252,
13.6381709389644));
#24472=CARTESIAN_POINT('Ctrl Pts',(-0.630351911255712,2.05289518642211,
13.9784736853838));
#24473=CARTESIAN_POINT('Ctrl Pts',(-0.615625695700795,1.99277620041693,
14.1767277310439));
#24474=CARTESIAN_POINT('Ctrl Pts',(-0.603353849316717,1.92702932690731,
14.3354574303556));
#24475=CARTESIAN_POINT('Ctrl Pts',(-0.598445110714969,1.89917336159767,
14.3983045855388));
#24476=CARTESIAN_POINT('Ctrl Pts',(-0.588627633915256,1.83735592021535,
14.5211092192054));
#24477=CARTESIAN_POINT('Ctrl Pts',(-0.571447048942948,1.71357542899754,
14.7276905988158));
#24478=CARTESIAN_POINT('Ctrl Pts',(-0.556720833433352,1.5821304245265,14.8878145993562));
#24479=CARTESIAN_POINT('Ctrl Pts',(-0.519905294550446,1.21791267958507,
15.2525317138587));
#24480=CARTESIAN_POINT('Ctrl Pts',(-0.465909170916065,0.535674767624319,
15.6386339750025));
#24481=CARTESIAN_POINT('Ctrl Pts',(-0.382460616042388,-0.675567454408333,
15.6090866894905));
#24482=CARTESIAN_POINT('Ctrl Pts',(-0.291648953233538,-1.78073099288634,
14.8720289916999));
#24483=CARTESIAN_POINT('Ctrl Pts',(-0.227835352442492,-2.10078552644068,
13.9811525387388));
#24484=CARTESIAN_POINT('Ctrl Pts',(-0.159113013318636,-2.10079066955095,
13.0188702094965));
#24485=CARTESIAN_POINT('Ctrl Pts',(-0.0952994125437925,-1.78074595791222,
12.1279906389835));
#24486=CARTESIAN_POINT('Ctrl Pts',(-0.00448774969938476,-0.675590300139453,
11.3909215605209));
#24487=CARTESIAN_POINT('Ctrl Pts',(0.0789608051277796,0.535650184199022,
11.361362976682));
#24488=CARTESIAN_POINT('Ctrl Pts',(0.132956928776363,1.21789188774156,11.7474587552716));
#24489=CARTESIAN_POINT('Ctrl Pts',(0.169772467714179,1.58211182691082,12.1121734025769));
#24490=CARTESIAN_POINT('Ctrl Pts',(0.182044314016518,1.69165464540701,12.2456070858446));
#24491=CARTESIAN_POINT('Ctrl Pts',(0.196770529333881,1.80197516219225,12.4198520707251));
#24492=CARTESIAN_POINT('Ctrl Pts',(0.206588006671623,1.86974558093869,12.539474812745));
#24493=CARTESIAN_POINT('Ctrl Pts',(0.213951114405061,1.91387131899328,12.6327771518145));
#24494=CARTESIAN_POINT('Ctrl Pts',(0.223768591514521,1.96646819424218,12.7597606835474));
#24495=CARTESIAN_POINT('Ctrl Pts',(0.238494807022666,2.03602659373201,12.9541098141789));
#24496=CARTESIAN_POINT('Ctrl Pts',(0.26303849959488,2.10336912153095,13.2927454528611));
#24497=CARTESIAN_POINT('Ctrl Pts',(0.297399669321619,2.10342601846571,13.7761449969021));
#24498=CARTESIAN_POINT('Ctrl Pts',(0.321943361926104,2.01908783680841,14.1130939795258));
#24499=CARTESIAN_POINT('Ctrl Pts',(0.351395792887634,1.86128994972974,14.494009126764));
#24500=CARTESIAN_POINT('Ctrl Pts',(0.383302593222992,1.62916652410642,14.8816272398943));
#24501=CARTESIAN_POINT('Ctrl Pts',(0.43238997846908,1.10118736333318,15.3365211140863));
#24502=CARTESIAN_POINT('Ctrl Pts',(0.496203579352586,0.25500707638925,15.6645359872915));
#24503=CARTESIAN_POINT('Ctrl Pts',(0.552654072307385,-0.565373559877596,
15.5841293911837));
#24504=CARTESIAN_POINT('Ctrl Pts',(0.601741457554998,-1.17417583117015,
15.257067690362));
#24505=CARTESIAN_POINT('Ctrl Pts',(0.621376411675378,-1.38774574185824,
15.0822099078348));
#24506=CARTESIAN_POINT('Ctrl Pts',(0.636102627260723,-1.53352110099643,
14.9363959261039));
#24507=CARTESIAN_POINT('Ctrl Pts',(0.650828842696062,-1.67217406423484,
14.7834672512282));
#24508=CARTESIAN_POINT('Ctrl Pts',(0.675372535461211,-1.86391731608368,
14.4963678608596));
#24509=CARTESIAN_POINT('Ctrl Pts',(0.714642443588536,-2.07557366934684,
13.9860040962929));
#24510=CARTESIAN_POINT('Ctrl Pts',(0.751457982772098,-2.12713365409934,
13.4631973594635));
#24511=CARTESIAN_POINT('Ctrl Pts',(0.780910413391623,-2.05622170942674,
13.0558123800778));
#24512=CARTESIAN_POINT('Ctrl Pts',(0.795636629169332,-2.00124069083438,
12.8570553247401));
#24513=CARTESIAN_POINT('Ctrl Pts',(0.80299973691532,-1.96646360481137,12.759878700581));
#24514=CARTESIAN_POINT('Ctrl Pts',(0.827543429433267,-1.8349740425443,12.4424202184717));
#24515=CARTESIAN_POINT('Ctrl Pts',(0.847178383627465,-1.67932044807009,
12.2094728214553));
#24516=CARTESIAN_POINT('Ctrl Pts',(0.881539553224067,-1.33915884910206,
11.8692628313779));
#24517=CARTESIAN_POINT('Ctrl Pts',(0.910991984238634,-1.00441069214917,
11.6213837143031));
#24518=CARTESIAN_POINT('Ctrl Pts',(0.969896846618502,-0.219311743108901,
11.3391555711753));
#24519=CARTESIAN_POINT('Ctrl Pts',(1.0140754933703,0.422741337103771,11.401461357304));
#24520=CARTESIAN_POINT('Ctrl Pts',(1.06070850926287,1.02592141298073,11.6518883197597));
#24521=CARTESIAN_POINT('Ctrl Pts',(1.09506967881695,1.43772003638653,11.9130832441603));
#24522=CARTESIAN_POINT('Ctrl Pts',(1.15888327962412,1.99757123417929,12.627581886472));
#24523=CARTESIAN_POINT('Ctrl Pts',(1.22269688059815,2.17939148969465,13.5415580421266));
#24524=CARTESIAN_POINT('Ctrl Pts',(1.2865104813802,1.93556794510799,14.4158745779137));
#24525=CARTESIAN_POINT('Ctrl Pts',(1.3208716509393,1.6551419067762,14.8148782111249));
#24526=CARTESIAN_POINT('Ctrl Pts',(1.36259592840431,1.24204900760236,15.2279793178278));
#24527=CARTESIAN_POINT('Ctrl Pts',(1.40677457522512,0.69540974323271,15.555219482443));
#24528=CARTESIAN_POINT('Ctrl Pts',(1.47058817603759,-0.211302775492013,
15.6442866757422));
#24529=CARTESIAN_POINT('Ctrl Pts',(1.51967556109321,-0.881544870996376,
15.4409224823238));
#24530=CARTESIAN_POINT('Ctrl Pts',(1.55403673067944,-1.28338124194598,15.1721190230281));
#24531=CARTESIAN_POINT('Ctrl Pts',(1.56876294625041,-1.43632922636008,15.0335302691141));
#24532=CARTESIAN_POINT('Ctrl Pts',(1.57612605409992,-1.50921865417633,14.9606379685896));
#24533=CARTESIAN_POINT('Ctrl Pts',(1.58594353107896,-1.60404087000891,14.8610646978933));
#24534=CARTESIAN_POINT('Ctrl Pts',(1.61048722375972,-1.81588314242947,14.5894684454936));
#24535=CARTESIAN_POINT('Ctrl Pts',(1.65712023979801,-2.09905840693387,13.9929656680311));
#24536=CARTESIAN_POINT('Ctrl Pts',(1.71602510188461,-2.14067689814634,13.1444277157845));
#24537=CARTESIAN_POINT('Ctrl Pts',(1.77983870265428,-1.7913526847043,12.3029150640716));
#24538=CARTESIAN_POINT('Ctrl Pts',(1.8411979342038,-1.1725122789855,11.6835302547082));
#24539=CARTESIAN_POINT('Ctrl Pts',(1.90501153478705,-0.318333576394129,
11.3539054759517));
#24540=CARTESIAN_POINT('Ctrl Pts',(1.97127950473874,0.629748690539184,11.4238917221576));
#24541=CARTESIAN_POINT('Ctrl Pts',(2.03754747513178,1.45696107490744,11.8925075563253));
#24542=CARTESIAN_POINT('Ctrl Pts',(2.08172612170549,1.8218559736609,12.4106507069619));
#24543=CARTESIAN_POINT('Ctrl Pts',(2.10708793706594,1.95772243717073,12.7386816790409));
#24544=CARTESIAN_POINT('Ctrl Pts',(2.11076949093637,1.97588826019748,12.7869463583648));
#24545=CARTESIAN_POINT('Ctrl Pts',(2.11567823171285,1.99771229805176,12.8521119034831));
#24546=CARTESIAN_POINT('Ctrl Pts',(2.12222319940488,2.02538800399747,12.9394693025088));
#24547=CARTESIAN_POINT('Ctrl Pts',(2.13326791223981,2.06300512290958,13.0896425565393));
#24548=CARTESIAN_POINT('Ctrl Pts',(2.14799403872137,2.09329385346697,13.2938233974499));
#24549=CARTESIAN_POINT('Ctrl Pts',(2.15781158440922,2.10004742944095,13.4312693672659));
#24550=CARTESIAN_POINT('Ctrl Pts',(2.18235534265953,2.10005277188115,13.7748841760795));
#24551=CARTESIAN_POINT('Ctrl Pts',(2.20199000992373,2.04541374138347,14.0496807748905));
#24552=CARTESIAN_POINT('Ctrl Pts',(2.22407954768458,1.92706171431628,14.3353894648931));
#24553=CARTESIAN_POINT('Ctrl Pts',(2.24862355314762,1.78787291788821,14.6496897709558));
#24554=CARTESIAN_POINT('Ctrl Pts',(2.29280124701354,1.39797717703433,15.1490382788963));
#24555=CARTESIAN_POINT('Ctrl Pts',(2.35661619005622,0.594504104329255,15.5785996905196));
#24556=CARTESIAN_POINT('Ctrl Pts',(2.42042860590492,-0.318100812988892,
15.6459834169773));
#24557=CARTESIAN_POINT('Ctrl Pts',(2.48915055047148,-1.23851059813794,15.2913925342509));
#24558=CARTESIAN_POINT('Ctrl Pts',(2.54837311591077,-1.81212008137858,14.6585567792867));
#24559=CARTESIAN_POINT('Ctrl Pts',(2.58549757494722,-1.99847675263324,14.1686814022878));
#24560=CARTESIAN_POINT('Ctrl Pts',(2.5980826159495,-2.0402177892642,13.997506252196));
#24561=CARTESIAN_POINT('Ctrl Pts',(-2.59812731618765,2.04036530566024,13.9968998060665));
#24562=CARTESIAN_POINT('Ctrl Pts',(-2.59534505994695,2.03114861974595,14.0347452630157));
#24563=CARTESIAN_POINT('Ctrl Pts',(-2.59133561561887,2.01634974207102,14.088914022261));
#24564=CARTESIAN_POINT('Ctrl Pts',(-2.58691712975414,1.99766627284527,14.1478887530375));
#24565=CARTESIAN_POINT('Ctrl Pts',(-2.58200838897772,1.9758422746189,14.2130542894858));
#24566=CARTESIAN_POINT('Ctrl Pts',(-2.5783268351068,1.95767675979263,14.2613189694603));
#24567=CARTESIAN_POINT('Ctrl Pts',(-2.55296501974317,1.82181369270838,14.5893498915566));
#24568=CARTESIAN_POINT('Ctrl Pts',(-2.5087863731675,1.45693484860441,15.1074928158849));
#24569=CARTESIAN_POINT('Ctrl Pts',(-2.44251840277764,0.62972994555188,15.5761085436532));
#24570=CARTESIAN_POINT('Ctrl Pts',(-2.37625043282579,-0.318344200487585,
15.6460946753124));
#24571=CARTESIAN_POINT('Ctrl Pts',(-2.31243683224114,-1.17251901929372,
15.3164698418647));
#24572=CARTESIAN_POINT('Ctrl Pts',(-2.251077600695,-1.79135679412861,14.6970849956997));
#24573=CARTESIAN_POINT('Ctrl Pts',(-2.18726399992216,-2.14067894781455,
13.8555723158434));
#24574=CARTESIAN_POINT('Ctrl Pts',(-2.12835913783721,-2.09905999758198,
13.0070343576013));
#24575=CARTESIAN_POINT('Ctrl Pts',(-2.08172612179798,-1.81588405920725,
12.4105315721756));
#24576=CARTESIAN_POINT('Ctrl Pts',(-2.05718242911857,-1.60404168806122,
12.1389353188883));
#24577=CARTESIAN_POINT('Ctrl Pts',(-2.04736495213942,-1.50921945576282,
12.0393620480447));
#24578=CARTESIAN_POINT('Ctrl Pts',(-2.04000184429017,-1.43633001895298,
11.9664697474652));
#24579=CARTESIAN_POINT('Ctrl Pts',(-2.02527562871905,-1.2833820002978,11.8278809934843));
#24580=CARTESIAN_POINT('Ctrl Pts',(-1.99091445913108,-0.881545538385891,
11.5590775340104));
#24581=CARTESIAN_POINT('Ctrl Pts',(-1.94182707407465,-0.211303206956926,
11.3557133455025));
#24582=CARTESIAN_POINT('Ctrl Pts',(-1.8780134732634,0.69540941925258,11.4447805426057));
#24583=CARTESIAN_POINT('Ctrl Pts',(-1.83383482644428,1.24204881717818,11.7720207235788));
#24584=CARTESIAN_POINT('Ctrl Pts',(-1.79211054898006,1.65514176280649,12.1851218390422));
#24585=CARTESIAN_POINT('Ctrl Pts',(-1.75774937941984,1.9355678426377,12.584125483555));
#24586=CARTESIAN_POINT('Ctrl Pts',(-1.69393577863675,2.17939142999823,13.4584420456258));
#24587=CARTESIAN_POINT('Ctrl Pts',(-1.63012217766268,1.99757120080247,14.3724182414288));
#24588=CARTESIAN_POINT('Ctrl Pts',(-1.56630857685675,1.43772002594656,15.0869169536628));
#24589=CARTESIAN_POINT('Ctrl Pts',(-1.53194740730155,1.02592141791999,15.3481119548905));
#24590=CARTESIAN_POINT('Ctrl Pts',(-1.48531439140832,0.422741355371464,
15.598538991029));
#24591=CARTESIAN_POINT('Ctrl Pts',(-1.4411357446571,-0.21931170653463,15.6608449087876));
#24592=CARTESIAN_POINT('Ctrl Pts',(-1.3822308822772,-1.00441063212639,15.37861696754));
#24593=CARTESIAN_POINT('Ctrl Pts',(-1.3527784512634,-1.33915876666712,15.1307380565637));
#24594=CARTESIAN_POINT('Ctrl Pts',(-1.31841728166562,-1.67932034588269,
14.7905282515356));
#24595=CARTESIAN_POINT('Ctrl Pts',(-1.29878232746832,-1.83497389521851,
14.5575812868999));
#24596=CARTESIAN_POINT('Ctrl Pts',(-1.27423863495645,-1.96646344354817,
14.2401229366851));
#24597=CARTESIAN_POINT('Ctrl Pts',(-1.26687552721325,-2.00124052925931,
14.1429463218818));
#24598=CARTESIAN_POINT('Ctrl Pts',(-1.25214931142335,-2.05622153683595,
13.9441893596129));
#24599=CARTESIAN_POINT('Ctrl Pts',(-1.2226968808366,-2.12713352117015,13.5368041117153));
#24600=CARTESIAN_POINT('Ctrl Pts',(-1.18588134158537,-2.07557312081611,
13.0140009829725));
#24601=CARTESIAN_POINT('Ctrl Pts',(-1.14661143353127,-1.86391706588866,
12.5036350235708));
#24602=CARTESIAN_POINT('Ctrl Pts',(-1.12206774073086,-1.67217312482415,
12.2165411311398));
#24603=CARTESIAN_POINT('Ctrl Pts',(-1.10734152529897,-1.53352101847216,
12.0636059026328));
#24604=CARTESIAN_POINT('Ctrl Pts',(-1.09261530971597,-1.38774164664309,
11.9178229476107));
#24605=CARTESIAN_POINT('Ctrl Pts',(-1.07298035559411,-1.17422658984893,
11.7425415659256));
#24606=CARTESIAN_POINT('Ctrl Pts',(-1.05334540149858,-0.930615724615552,
11.6124122110264));
#24607=CARTESIAN_POINT('Ctrl Pts',(-1.01407549332128,-0.422751809620052,
11.401478347902));
#24608=CARTESIAN_POINT('Ctrl Pts',(-0.967442477390011,0.255047337510375,
11.3357788746702));
#24609=CARTESIAN_POINT('Ctrl Pts',(-0.903628876505371,1.10117161573409,
11.6633623053098));
#24610=CARTESIAN_POINT('Ctrl Pts',(-0.854541491260921,1.62917228431376,
12.1184272880757));
#24611=CARTESIAN_POINT('Ctrl Pts',(-0.822634690930238,1.86128789168044,
12.5059830549408));
#24612=CARTESIAN_POINT('Ctrl Pts',(-0.793182259963081,2.01908443269519,
12.8869038770426));
#24613=CARTESIAN_POINT('Ctrl Pts',(-0.768638567346796,2.10343921024085,
13.2238525787215));
#24614=CARTESIAN_POINT('Ctrl Pts',(-0.739186136138703,2.10336168670159,
13.6381929904004));
#24615=CARTESIAN_POINT('Ctrl Pts',(-0.714642443531089,2.05289016857552,
13.9784952079289));
#24616=CARTESIAN_POINT('Ctrl Pts',(-0.699916227976207,1.99276910397954,
14.1767486226491));
#24617=CARTESIAN_POINT('Ctrl Pts',(-0.68764438159213,1.92702056606835,14.3354776334837));
#24618=CARTESIAN_POINT('Ctrl Pts',(-0.682735642990384,1.89916394265223,
14.3983244956345));
#24619=CARTESIAN_POINT('Ctrl Pts',(-0.67291816619067,1.83734521207404,14.5211284832248));
#24620=CARTESIAN_POINT('Ctrl Pts',(-0.65573758121835,1.71356255861117,14.7277085610067));
#24621=CARTESIAN_POINT('Ctrl Pts',(-0.641011365708785,1.58211586986789,
14.8878311897117));
#24622=CARTESIAN_POINT('Ctrl Pts',(-0.604195826825868,1.2178943102614,15.2525444759611));
#24623=CARTESIAN_POINT('Ctrl Pts',(-0.550199703191467,0.535652337781153,
15.6386395941889));
#24624=CARTESIAN_POINT('Ctrl Pts',(-0.466751148317924,-0.675589555932738,
15.6090796029729));
#24625=CARTESIAN_POINT('Ctrl Pts',(-0.375939485509005,-1.78074537880574,
14.8720103239888));
#24626=CARTESIAN_POINT('Ctrl Pts',(-0.31212588471795,-2.10079056737381,
13.9811305159176));
#24627=CARTESIAN_POINT('Ctrl Pts',(-0.243403545594093,-2.10078562864891,
13.018848186645));
#24628=CARTESIAN_POINT('Ctrl Pts',(-0.179589944819259,-1.78073157198358,
12.127971971317));
#24629=CARTESIAN_POINT('Ctrl Pts',(-0.088778281974919,-0.67556819871279,
11.390914473911));
#24630=CARTESIAN_POINT('Ctrl Pts',(-0.00532972714761881,0.535672614096381,
11.3613685959817));
#24631=CARTESIAN_POINT('Ctrl Pts',(0.0486663965009476,1.21791025677753,
11.7474715171088));
#24632=CARTESIAN_POINT('Ctrl Pts',(0.0854819354387522,1.58212638175774,
12.1121899932069));
#24633=CARTESIAN_POINT('Ctrl Pts',(0.097753781741119,1.69166779517795,12.2456248179755));
#24634=CARTESIAN_POINT('Ctrl Pts',(0.112479997058482,1.80198648889417,12.4198709638171));
#24635=CARTESIAN_POINT('Ctrl Pts',(0.122297474396219,1.86975565182069,12.5394944142019));
#24636=CARTESIAN_POINT('Ctrl Pts',(0.129660582129661,1.91388041275862,12.6327972171707));
#24637=CARTESIAN_POINT('Ctrl Pts',(0.139478059239116,1.96647595649454,12.7597813000298));
#24638=CARTESIAN_POINT('Ctrl Pts',(0.154204274747277,2.0360323180508,12.9541311597142));
#24639=CARTESIAN_POINT('Ctrl Pts',(0.178747967319465,2.10337129653229,13.2927675044316));
#24640=CARTESIAN_POINT('Ctrl Pts',(0.213109137046184,2.1034231236121,13.7761670489127));
#24641=CARTESIAN_POINT('Ctrl Pts',(0.23765282965073,2.01908141283192,14.1131151470859));
#24642=CARTESIAN_POINT('Ctrl Pts',(0.267105260612252,1.86127952720513,14.4940286406423));
#24643=CARTESIAN_POINT('Ctrl Pts',(0.299012060947521,1.62915204416609,14.8816443196594));
#24644=CARTESIAN_POINT('Ctrl Pts',(0.34809944619367,1.10116811030529,15.3365326588097));
#24645=CARTESIAN_POINT('Ctrl Pts',(0.4119130470771,0.25498438275294,15.6645386602339));
#24646=CARTESIAN_POINT('Ctrl Pts',(0.468363540031971,-0.565395398106497,
15.5841234654303));
#24647=CARTESIAN_POINT('Ctrl Pts',(0.517450925279634,-1.17419426258121,
15.2570553788871));
#24648=CARTESIAN_POINT('Ctrl Pts',(0.537085879399974,-1.38776232212866,
15.0821953602152));
#24649=CARTESIAN_POINT('Ctrl Pts',(0.551812094985311,-1.53353616354587,
14.9363798480822));
#24650=CARTESIAN_POINT('Ctrl Pts',(0.56653831042067,-1.67218751851079,14.7834497214876));
#24651=CARTESIAN_POINT('Ctrl Pts',(0.591082003185787,-1.86392776386923,
14.4963483191671));
#24652=CARTESIAN_POINT('Ctrl Pts',(0.630351911313134,-2.07557876402105,
13.9859823368843));
#24653=CARTESIAN_POINT('Ctrl Pts',(0.667167450496672,-2.12713326926079,
13.4631750627901));
#24654=CARTESIAN_POINT('Ctrl Pts',(0.696619881116207,-2.05621705239711,
13.0557908206335));
#24655=CARTESIAN_POINT('Ctrl Pts',(0.711346096893909,-2.00123395135074,
12.8570343458293));
#24656=CARTESIAN_POINT('Ctrl Pts',(0.718709204639899,-1.96645584370435,
12.7598580832961));
#24657=CARTESIAN_POINT('Ctrl Pts',(0.743252897157858,-1.83496296645056,
12.4424009859059));
#24658=CARTESIAN_POINT('Ctrl Pts',(0.762887851352057,-1.67930691067268,
12.2094552167024));
#24659=CARTESIAN_POINT('Ctrl Pts',(0.797249020948654,-1.33914175837502,
11.8692487912752));
#24660=CARTESIAN_POINT('Ctrl Pts',(0.826701451963186,-1.00439099503339,
11.6213731861561));
#24661=CARTESIAN_POINT('Ctrl Pts',(0.885606314342979,-0.219289089925647,
11.3391532699561));
#24662=CARTESIAN_POINT('Ctrl Pts',(0.929784961094886,0.422763330259709,
11.4014657923317));
#24663=CARTESIAN_POINT('Ctrl Pts',(0.976417976987453,1.02594079413025,11.6518990716162));
#24664=CARTESIAN_POINT('Ctrl Pts',(1.01077914654152,1.43773667048348,11.9130983208989));
#24665=CARTESIAN_POINT('Ctrl Pts',(1.07459274734868,1.99758038283143,12.6276028268694));
#24666=CARTESIAN_POINT('Ctrl Pts',(1.13840634832269,2.17939105116197,13.5415808892922));
#24667=CARTESIAN_POINT('Ctrl Pts',(1.20221994910475,1.93555834646513,14.4158948734873));
#24668=CARTESIAN_POINT('Ctrl Pts',(1.23658111866385,1.65512811680158,14.8148955611299));
#24669=CARTESIAN_POINT('Ctrl Pts',(1.27830539612885,1.24203089999581,15.2279923390823));
#24670=CARTESIAN_POINT('Ctrl Pts',(1.32248404294974,0.695388194198749,15.5552267722387));
#24671=CARTESIAN_POINT('Ctrl Pts',(1.38629764376216,-0.211325253897595,
15.6442844608611));
#24672=CARTESIAN_POINT('Ctrl Pts',(1.43538502881776,-0.881565217530111,
15.4409132406642));
#24673=CARTESIAN_POINT('Ctrl Pts',(1.469746198404,-1.28339877368803,15.1721055678425));
#24674=CARTESIAN_POINT('Ctrl Pts',(1.48447241397496,-1.43634530247318,15.0335152116947));
#24675=CARTESIAN_POINT('Ctrl Pts',(1.49183552182448,-1.50923396733164,14.9606221453972));
#24676=CARTESIAN_POINT('Ctrl Pts',(1.5016529988035,-1.60405513865477,14.8610478851651));
#24677=CARTESIAN_POINT('Ctrl Pts',(1.52619669148426,-1.81589456446389,14.5894494037982));
#24678=CARTESIAN_POINT('Ctrl Pts',(1.57282970752259,-2.09906357467187,13.9929436636473));
#24679=CARTESIAN_POINT('Ctrl Pts',(1.63173456960926,-2.14067317084883,13.1444052710657));
#24680=CARTESIAN_POINT('Ctrl Pts',(1.69554817037887,-1.79134013475203,12.3028962855908));
#24681=CARTESIAN_POINT('Ctrl Pts',(1.75690740192841,-1.17249323607165,11.6835179627534));
#24682=CARTESIAN_POINT('Ctrl Pts',(1.82072100251162,-0.318311078103806,
11.3539021405768));
#24683=CARTESIAN_POINT('Ctrl Pts',(1.88698897246334,0.629770454452938,11.4238983246291));
#24684=CARTESIAN_POINT('Ctrl Pts',(1.95325694285639,1.45697792616486,11.8925228356508));
#24685=CARTESIAN_POINT('Ctrl Pts',(1.9974355894301,1.82186738996764,12.4106698060297));
#24686=CARTESIAN_POINT('Ctrl Pts',(2.02279740479054,1.95773041642441,12.738702209394));
#24687=CARTESIAN_POINT('Ctrl Pts',(2.02647895866097,1.97589573262478,12.7869670789265));
#24688=CARTESIAN_POINT('Ctrl Pts',(2.03138769943745,1.99771908858928,12.8521328519387));
#24689=CARTESIAN_POINT('Ctrl Pts',(2.03793266712948,2.02539387364681,12.9394905444958));
#24690=CARTESIAN_POINT('Ctrl Pts',(2.0489773799644,2.06300943248826,13.0896641864174));
#24691=CARTESIAN_POINT('Ctrl Pts',(2.06370350644596,2.09329599720291,13.2938453553922));
#24692=CARTESIAN_POINT('Ctrl Pts',(2.07352105213382,2.10004815600896,13.4312913837394));
#24693=CARTESIAN_POINT('Ctrl Pts',(2.09806481038409,2.10004987360911,13.7749062346504));
#24694=CARTESIAN_POINT('Ctrl Pts',(2.11769947764844,2.04540797017558,14.0497021502391));
#24695=CARTESIAN_POINT('Ctrl Pts',(2.13978901540921,1.92705294342672,14.3354096916135));
#24696=CARTESIAN_POINT('Ctrl Pts',(2.16433302087232,1.78786096674117,14.6497084864173));
#24697=CARTESIAN_POINT('Ctrl Pts',(2.20851071473805,1.39795979608125,15.1490528441138));
#24698=CARTESIAN_POINT('Ctrl Pts',(2.27232565778123,0.594482403270171,15.5786060645117));
#24699=CARTESIAN_POINT('Ctrl Pts',(2.33613807362933,-0.318123399654151,
15.6459799188749));
#24700=CARTESIAN_POINT('Ctrl Pts',(2.40486001819769,-1.23852912499723,15.2913795806851));
#24701=CARTESIAN_POINT('Ctrl Pts',(2.46408258363523,-1.81213280646108,14.6585380478362));
#24702=CARTESIAN_POINT('Ctrl Pts',(2.50120704267464,-1.99848332383328,14.1686604525656));
#24703=CARTESIAN_POINT('Ctrl Pts',(2.51379208367573,-2.04022249312054,13.9974847383588));
#24704=CARTESIAN_POINT('Ctrl Pts',(-2.68241784846308,2.04036009562041,13.9969211964378));
#24705=CARTESIAN_POINT('Ctrl Pts',(-2.67963559222238,2.03114301402161,14.0347665568773));
#24706=CARTESIAN_POINT('Ctrl Pts',(-2.6756261478943,2.01634357010855,14.0889351618321));
#24707=CARTESIAN_POINT('Ctrl Pts',(-2.67120766202956,1.99765948037072,14.1479096957282));
#24708=CARTESIAN_POINT('Ctrl Pts',(-2.66629892125314,1.97583479932944,14.2130750039397));
#24709=CARTESIAN_POINT('Ctrl Pts',(-2.66261736738221,1.95766877864201,14.2613394927813));
#24710=CARTESIAN_POINT('Ctrl Pts',(-2.63725555201859,1.82180227146093,14.5893689939159));
#24711=CARTESIAN_POINT('Ctrl Pts',(-2.59307690544293,1.45691799629554,15.1075080891233));
#24712=CARTESIAN_POINT('Ctrl Pts',(-2.52680893505306,0.629708180153284,
15.5761151466503));
#24713=CARTESIAN_POINT('Ctrl Pts',(-2.46054096510122,-0.31836669953251,
15.6460913378045));
#24714=CARTESIAN_POINT('Ctrl Pts',(-2.39672736451656,-1.17253806269356,
15.3164575498808));
#24715=CARTESIAN_POINT('Ctrl Pts',(-2.33536813297043,-1.79136934397512,
14.6970662152686));
#24716=CARTESIAN_POINT('Ctrl Pts',(-2.27155453219758,-2.14068267584376,
13.8555498749489));
#24717=CARTESIAN_POINT('Ctrl Pts',(-2.21264967011264,-2.09905482938455,
13.0070123510517));
#24718=CARTESIAN_POINT('Ctrl Pts',(-2.16601665407342,-1.81587263790155,
12.4105125373456));
#24719=CARTESIAN_POINT('Ctrl Pts',(-2.141472961394,-1.60402741906879,12.1389185008737));
#24720=CARTESIAN_POINT('Ctrl Pts',(-2.13165548441485,-1.50920414313901,
12.0393462263728));
#24721=CARTESIAN_POINT('Ctrl Pts',(-2.12429237656559,-1.43631394153121,
11.9664546891318));
#24722=CARTESIAN_POINT('Ctrl Pts',(-2.10956616099448,-1.28336447129704,
11.8278675391811));
#24723=CARTESIAN_POINT('Ctrl Pts',(-2.07520499140651,-0.881525189703381,
11.5590682920204));
#24724=CARTESIAN_POINT('Ctrl Pts',(-2.02611760635007,-0.21128072612125,
11.3557111299893));
#24725=CARTESIAN_POINT('Ctrl Pts',(-1.96230400553883,0.695430964275577,
11.4447878333271));
#24726=CARTESIAN_POINT('Ctrl Pts',(-1.9181253587197,1.2420669368066,11.7720337446871));
#24727=CARTESIAN_POINT('Ctrl Pts',(-1.87640108125549,1.65515554506745,12.1851391918979));
#24728=CARTESIAN_POINT('Ctrl Pts',(-1.84203991169527,1.93557744600219,12.5841457735168));
#24729=CARTESIAN_POINT('Ctrl Pts',(-1.77822631091218,2.17939186443456,13.4584648940827));
#24730=CARTESIAN_POINT('Ctrl Pts',(-1.71441270993811,1.99756205602226,14.3724391841198));
#24731=CARTESIAN_POINT('Ctrl Pts',(-1.65059910913218,1.43770338803263,15.0869320243634));
#24732=CARTESIAN_POINT('Ctrl Pts',(-1.61623793957698,1.02590204601976,15.3481227122834));
#24733=CARTESIAN_POINT('Ctrl Pts',(-1.56960492368374,0.422719351307122,
15.5985434215348));
#24734=CARTESIAN_POINT('Ctrl Pts',(-1.52542627693254,-0.21933436016509,
15.6608426107993));
#24735=CARTESIAN_POINT('Ctrl Pts',(-1.46652141455263,-1.00443032586176,
15.3786064369457));
#24736=CARTESIAN_POINT('Ctrl Pts',(-1.43706898353883,-1.3391758656156,15.130724017744));
#24737=CARTESIAN_POINT('Ctrl Pts',(-1.40270781394105,-1.67933387158251,
14.7905106458097));
#24738=CARTESIAN_POINT('Ctrl Pts',(-1.38307285974375,-1.83498498830578,
14.5575620473403));
#24739=CARTESIAN_POINT('Ctrl Pts',(-1.35852916723187,-1.96647120197112,
14.2401023217195));
#24740=CARTESIAN_POINT('Ctrl Pts',(-1.35116605948868,-2.00124727019645,
14.1429253408249));
#24741=CARTESIAN_POINT('Ctrl Pts',(-1.33643984369878,-2.05622619377765,
13.9441678042319));
#24742=CARTESIAN_POINT('Ctrl Pts',(-1.30698741311203,-2.12713390717972,
13.5367818097343));
#24743=CARTESIAN_POINT('Ctrl Pts',(-1.2701718738608,-2.07556802630583,13.0139792232064));
#24744=CARTESIAN_POINT('Ctrl Pts',(-1.2309019658067,-1.86390662077551,12.5036154832002));
#24745=CARTESIAN_POINT('Ctrl Pts',(-1.20635827300629,-1.67215967038646,
12.2165236002323));
#24746=CARTESIAN_POINT('Ctrl Pts',(-1.1916320575744,-1.53350596005819,12.0635898258973));
#24747=CARTESIAN_POINT('Ctrl Pts',(-1.1769058419914,-1.38772506180105,11.917808398972));
#24748=CARTESIAN_POINT('Ctrl Pts',(-1.15727088786955,-1.17420816235846,
11.7425292554681));
#24749=CARTESIAN_POINT('Ctrl Pts',(-1.13763593377401,-0.930595939981174,
11.6124024551505));
#24750=CARTESIAN_POINT('Ctrl Pts',(-1.09836602559671,-0.42272980236694,
11.4014739149307));
#24751=CARTESIAN_POINT('Ctrl Pts',(-1.05173300966544,0.25507002373376,11.3357815487481));
#24752=CARTESIAN_POINT('Ctrl Pts',(-0.987919408780793,1.10119087219249,
11.6633738492646));
#24753=CARTESIAN_POINT('Ctrl Pts',(-0.93883202353635,1.62918676932283,12.1184443677113));
#24754=CARTESIAN_POINT('Ctrl Pts',(-0.90692522320566,1.86129831265145,12.5060025676873));
#24755=CARTESIAN_POINT('Ctrl Pts',(-0.877472792238505,2.0190908616159,12.8869250445196));
#24756=CARTESIAN_POINT('Ctrl Pts',(-0.852929099622222,2.10344210570215,
13.2238746302206));
#24757=CARTESIAN_POINT('Ctrl Pts',(-0.823476668414125,2.10336023894075,
13.6382150411795));
#24758=CARTESIAN_POINT('Ctrl Pts',(-0.798932975806517,2.05288515301006,
13.9785167295123));
#24759=CARTESIAN_POINT('Ctrl Pts',(-0.784206760251632,1.99276201009388,
14.1767695142279));
#24760=CARTESIAN_POINT('Ctrl Pts',(-0.771934913867553,1.92701180829326,
14.335497835394));
#24761=CARTESIAN_POINT('Ctrl Pts',(-0.767026175265813,1.89915452564541,
14.3983444059853));
#24762=CARTESIAN_POINT('Ctrl Pts',(-0.757208698466093,1.83733450842296,
14.5211477444828));
#24763=CARTESIAN_POINT('Ctrl Pts',(-0.740028113493781,1.71354968754401,
14.7277265266632));
#24764=CARTESIAN_POINT('Ctrl Pts',(-0.725301897984208,1.58210132293516,
14.8878477742055));
#24765=CARTESIAN_POINT('Ctrl Pts',(-0.688486359101292,1.21787593530857,
15.2525572470515));
#24766=CARTESIAN_POINT('Ctrl Pts',(-0.634490235466891,0.535629921433265,
15.638645208084));
#24767=CARTESIAN_POINT('Ctrl Pts',(-0.551041680593352,-0.67561167141616,
15.6090725224069));
#24768=CARTESIAN_POINT('Ctrl Pts',(-0.460230017784431,-1.78075976153375,
14.8719916548044));
#24769=CARTESIAN_POINT('Ctrl Pts',(-0.396416416993376,-2.10079561310753,
13.9811084913171));
#24770=CARTESIAN_POINT('Ctrl Pts',(-0.327694077869519,-2.10078058291197,
13.0188261620575));
#24771=CARTESIAN_POINT('Ctrl Pts',(-0.263880477094685,-1.78071718927376,
12.1279533021069));
#24772=CARTESIAN_POINT('Ctrl Pts',(-0.173068814250347,-0.675546083201514,
11.3909073933772));
#24773=CARTESIAN_POINT('Ctrl Pts',(-0.0896202594230419,0.535695030379752,
11.3613742098035));
#24774=CARTESIAN_POINT('Ctrl Pts',(-0.0356241357744778,1.21792863182134,
11.7474842883091));
#24775=CARTESIAN_POINT('Ctrl Pts',(0.00119140316332885,1.58214092853682,
12.1122065775076));
#24776=CARTESIAN_POINT('Ctrl Pts',(0.0134632494656868,1.69168094619521,
12.2456425541522));
#24777=CARTESIAN_POINT('Ctrl Pts',(0.0281894647830582,1.80199781130694,
12.4198898544029));
#24778=CARTESIAN_POINT('Ctrl Pts',(0.0380069421207919,1.86976572107786,
12.539514016255));
#24779=CARTESIAN_POINT('Ctrl Pts',(0.0453700498542355,1.91388950332719,
12.6328172811942));
#24780=CARTESIAN_POINT('Ctrl Pts',(0.0551875269636911,1.96648371591656,
12.7598019155958));
#24781=CARTESIAN_POINT('Ctrl Pts',(0.0699137424718479,2.03603804019403,
12.9541525045977));
#24782=CARTESIAN_POINT('Ctrl Pts',(0.0944574350440407,2.10337346807658,
13.2927895552418));
#24783=CARTESIAN_POINT('Ctrl Pts',(0.128818604770759,2.10342022840744,13.7761891003219));
#24784=CARTESIAN_POINT('Ctrl Pts',(0.153362297375304,2.01907498345824,14.1131363145558));
#24785=CARTESIAN_POINT('Ctrl Pts',(0.182814728336829,1.86126910700408,14.4940481534565));
#24786=CARTESIAN_POINT('Ctrl Pts',(0.214721528672091,1.62913755730854,14.8816613990925));
#24787=CARTESIAN_POINT('Ctrl Pts',(0.263808913918248,1.10114885647858,15.3365442030697));
#24788=CARTESIAN_POINT('Ctrl Pts',(0.327622514801669,0.254961691253659,
15.6645413336943));
#24789=CARTESIAN_POINT('Ctrl Pts',(0.38407300775655,-0.565417252986099,
15.5841175373479));
#24790=CARTESIAN_POINT('Ctrl Pts',(0.433160393004205,-1.17421267765378,
15.2570430698972));
#24791=CARTESIAN_POINT('Ctrl Pts',(0.452795347124548,-1.38777891298425,
15.082180810866));
#24792=CARTESIAN_POINT('Ctrl Pts',(0.467521562709886,-1.53355122022996,
14.9363637715519));
#24793=CARTESIAN_POINT('Ctrl Pts',(0.482247778145241,-1.67220097442926,
14.7834321904053));
#24794=CARTESIAN_POINT('Ctrl Pts',(0.506791470910362,-1.86393820824105,
14.4963287788814));
#24795=CARTESIAN_POINT('Ctrl Pts',(0.546061379037708,-2.07558385917854,
13.9859605770456));
#24796=CARTESIAN_POINT('Ctrl Pts',(0.582876918221244,-2.12713288283513,
13.4631527608566));
#24797=CARTESIAN_POINT('Ctrl Pts',(0.612329348840782,-2.05621239560423,
13.0557692652354));
#24798=CARTESIAN_POINT('Ctrl Pts',(0.627055564618482,-2.00122721031883,
12.8570133647833));
#24799=CARTESIAN_POINT('Ctrl Pts',(0.634418672364474,-1.96644808531056,
12.7598374683271));
#24800=CARTESIAN_POINT('Ctrl Pts',(0.65896236488243,-1.83495187331109,12.4423817463518));
#24801=CARTESIAN_POINT('Ctrl Pts',(0.67859731907663,-1.67929338500544,12.2094376109722));
#24802=CARTESIAN_POINT('Ctrl Pts',(0.712958488673231,-1.33912465941359,
11.8692347524568));
#24803=CARTESIAN_POINT('Ctrl Pts',(0.74241091968776,-1.00437130130585,11.6213626555605));
#24804=CARTESIAN_POINT('Ctrl Pts',(0.801315782067549,-0.219266436289686,
11.3391509719678));
#24805=CARTESIAN_POINT('Ctrl Pts',(0.845494428819463,0.422785334321912,
11.4014702228365));
#24806=CARTESIAN_POINT('Ctrl Pts',(0.892127444712026,1.02596016603173,11.6519098290087));
#24807=CARTESIAN_POINT('Ctrl Pts',(0.926488614266094,1.43775330839738,11.913113391599));
#24808=CARTESIAN_POINT('Ctrl Pts',(0.990302215073251,1.99758952761244,12.6276237695603));
#24809=CARTESIAN_POINT('Ctrl Pts',(1.05411581604726,2.17939061672641,13.5416037377489));
#24810=CARTESIAN_POINT('Ctrl Pts',(1.11792941682932,1.93554874310097,14.4159151634498));
#24811=CARTESIAN_POINT('Ctrl Pts',(1.15229058638842,1.65511433454093,14.8149129139855));
#24812=CARTESIAN_POINT('Ctrl Pts',(1.19401486385342,1.24201278036798,15.2280053601908));
#24813=CARTESIAN_POINT('Ctrl Pts',(1.23819351067431,0.695366649175583,15.5552340629608));
#24814=CARTESIAN_POINT('Ctrl Pts',(1.30200711148673,-0.211347734732747,
15.6442822453488));
#24815=CARTESIAN_POINT('Ctrl Pts',(1.35109449654233,-0.881585566213743,
15.4409039986746));
#24816=CARTESIAN_POINT('Ctrl Pts',(1.38545566612857,-1.28341630268856,15.1720921135398));
#24817=CARTESIAN_POINT('Ctrl Pts',(1.40018188169953,-1.43636137989527,15.0335001533614));
#24818=CARTESIAN_POINT('Ctrl Pts',(1.40754498954905,-1.5092492799557,14.9606063237254));
#24819=CARTESIAN_POINT('Ctrl Pts',(1.41736246652807,-1.60406940764737,14.8610310671509));
#24820=CARTESIAN_POINT('Ctrl Pts',(1.44190615920883,-1.81590598576995,14.589430368968));
#24821=CARTESIAN_POINT('Ctrl Pts',(1.48853917524716,-2.0990687428701,13.9929216570987));
#24822=CARTESIAN_POINT('Ctrl Pts',(1.54744403733383,-2.14066944281984,13.1443828301699));
#24823=CARTESIAN_POINT('Ctrl Pts',(1.61125763810345,-1.79132758490686,12.3028775051611));
#24824=CARTESIAN_POINT('Ctrl Pts',(1.67261686965298,-1.17247419267079,11.6835056707651));
#24825=CARTESIAN_POINT('Ctrl Pts',(1.73643047023619,-0.318288579061762,
11.3538988030757));
#24826=CARTESIAN_POINT('Ctrl Pts',(1.80269844018791,0.629792219857265,11.4239049276112));
#24827=CARTESIAN_POINT('Ctrl Pts',(1.86896641058096,1.45699477846171,11.892538108919));
#24828=CARTESIAN_POINT('Ctrl Pts',(1.91314505715466,1.82187881123711,12.4106889083354));
#24829=CARTESIAN_POINT('Ctrl Pts',(1.93850687251511,1.95773839753758,12.7387227328106));
#24830=CARTESIAN_POINT('Ctrl Pts',(1.94218842638554,1.97590320811804,12.7869877928638));
#24831=CARTESIAN_POINT('Ctrl Pts',(1.94709716716202,1.99772588093429,12.8521537949592));
#24832=CARTESIAN_POINT('Ctrl Pts',(1.95364213485405,2.02539974752619,12.9395117773037));
#24833=CARTESIAN_POINT('Ctrl Pts',(1.96468684768897,2.06301374064072,13.089685814159));
#24834=CARTESIAN_POINT('Ctrl Pts',(1.97941297417053,2.09329814961718,13.293867299342));
#24835=CARTESIAN_POINT('Ctrl Pts',(1.98923051985839,2.10004887700028,13.4313134021794));
#24836=CARTESIAN_POINT('Ctrl Pts',(2.01377427810869,2.10004702393194,13.7749282344788));
#24837=CARTESIAN_POINT('Ctrl Pts',(2.03340894537298,2.04540214750026,14.0497236098048));
#24838=CARTESIAN_POINT('Ctrl Pts',(2.05549848313379,1.92704419097465,14.335429888756));
#24839=CARTESIAN_POINT('Ctrl Pts',(2.08004248859686,1.78784894384282,14.6497273032214));
#24840=CARTESIAN_POINT('Ctrl Pts',(2.12422018246268,1.39794244392195,15.1490673646013));
#24841=CARTESIAN_POINT('Ctrl Pts',(2.18803512550574,0.594460673229926,15.5786124601074));
#24842=CARTESIAN_POINT('Ctrl Pts',(2.25184754135404,-0.318145960249626,
15.645976444991));
#24843=CARTESIAN_POINT('Ctrl Pts',(2.3205694859221,-1.23854770711973,15.2913665209294));
#24844=CARTESIAN_POINT('Ctrl Pts',(2.37979205136044,-1.81214548705499,14.6585194070205));
#24845=CARTESIAN_POINT('Ctrl Pts',(2.41691651039905,-1.99848999267705,14.1686392952167));
#24846=CARTESIAN_POINT('Ctrl Pts',(2.42950155140196,-2.04022719697688,13.9974632245214));
#24847=CARTESIAN_POINT('Ctrl Pts',(-2.42950802845431,-0.728165094212968,
15.4695758861306));
#24848=CARTESIAN_POINT('Ctrl Pts',(-2.41776054273089,-0.882441814565159,
15.4125097574631));
#24849=CARTESIAN_POINT('Ctrl Pts',(-2.38637810294572,-1.27683944237258,
15.2120617751923));
#24850=CARTESIAN_POINT('Ctrl Pts',(-2.33536070898422,-1.79136934286978,
14.6970662169227));
#24851=CARTESIAN_POINT('Ctrl Pts',(-2.27154710821138,-2.14068267551541,
13.8555498769254));
#24852=CARTESIAN_POINT('Ctrl Pts',(-2.21264224612643,-2.09905482983975,
13.00701235299));
#24853=CARTESIAN_POINT('Ctrl Pts',(-2.16600923008721,-1.8158726389075,12.4105125390221));
#24854=CARTESIAN_POINT('Ctrl Pts',(-2.14146553740779,-1.60402742032555,
12.138918502355));
#24855=CARTESIAN_POINT('Ctrl Pts',(-2.13164806042864,-1.50920414448769,
12.0393462277663));
#24856=CARTESIAN_POINT('Ctrl Pts',(-2.12428495257939,-1.43631394294725,
11.9664546904581));
#24857=CARTESIAN_POINT('Ctrl Pts',(-2.10955873700828,-1.28336447284093,
11.8278675403661));
#24858=CARTESIAN_POINT('Ctrl Pts',(-2.0751975674203,-0.881525191495615,
11.5590682928344));
#24859=CARTESIAN_POINT('Ctrl Pts',(-2.02611018236387,-0.211280728101276,
11.3557111301844));
#24860=CARTESIAN_POINT('Ctrl Pts',(-1.96229658155262,0.695430962377974,
11.444787832685));
#24861=CARTESIAN_POINT('Ctrl Pts',(-1.91811793473349,1.24206693521069,11.7720337435403));
#24862=CARTESIAN_POINT('Ctrl Pts',(-1.87639365726928,1.65515554385356,12.1851391903695));
#24863=CARTESIAN_POINT('Ctrl Pts',(-1.84203248770906,1.93557744515636,12.5841457717297));
#24864=CARTESIAN_POINT('Ctrl Pts',(-1.77821888692597,2.1793918643963,13.4584648920703));
#24865=CARTESIAN_POINT('Ctrl Pts',(-1.7144052859519,1.9975620568277,14.3724391822753));
#24866=CARTESIAN_POINT('Ctrl Pts',(-1.65059168514597,1.43770338949803,15.086932023036));
#24867=CARTESIAN_POINT('Ctrl Pts',(-1.61623051559077,1.02590204772596,15.3481227113359));
#24868=CARTESIAN_POINT('Ctrl Pts',(-1.56959749969753,0.422719353245155,
15.5985434211446));
#24869=CARTESIAN_POINT('Ctrl Pts',(-1.52541885294633,-0.219334358169845,
15.6608426110017));
#24870=CARTESIAN_POINT('Ctrl Pts',(-1.46651399056642,-1.00443032412721,
15.3786064378732));
#24871=CARTESIAN_POINT('Ctrl Pts',(-1.43706155955262,-1.33917586410959,
15.1307240189805));
#24872=CARTESIAN_POINT('Ctrl Pts',(-1.40270038995484,-1.67933387039122,
14.7905106473604));
#24873=CARTESIAN_POINT('Ctrl Pts',(-1.38306543575754,-1.83498498732874,
14.5575620490349));
#24874=CARTESIAN_POINT('Ctrl Pts',(-1.35852174324566,-1.96647120128779,
14.2401023235352));
#24875=CARTESIAN_POINT('Ctrl Pts',(-1.35115863550247,-2.00124726960273,
14.1429253426728));
#24876=CARTESIAN_POINT('Ctrl Pts',(-1.33643241971257,-2.05622619336749,
13.9441678061304));
#24877=CARTESIAN_POINT('Ctrl Pts',(-1.30697998912582,-2.12713390714572,
13.5367818116986));
#24878=CARTESIAN_POINT('Ctrl Pts',(-1.27016444987459,-2.07556802675454,
13.0139792251229));
#24879=CARTESIAN_POINT('Ctrl Pts',(-1.23089454182049,-1.86390662169548,
12.5036154849212));
#24880=CARTESIAN_POINT('Ctrl Pts',(-1.20635084902008,-1.67215967157148,
12.2165236017764));
#24881=CARTESIAN_POINT('Ctrl Pts',(-1.19162463358819,-1.53350596138448,
12.0635898273133));
#24882=CARTESIAN_POINT('Ctrl Pts',(-1.17689841800519,-1.38772506326178,
11.9178084002534));
#24883=CARTESIAN_POINT('Ctrl Pts',(-1.15726346388334,-1.17420816398148,
11.7425292565524));
#24884=CARTESIAN_POINT('Ctrl Pts',(-1.1376285097878,-0.930595941723729,
11.6124024560098));
#24885=CARTESIAN_POINT('Ctrl Pts',(-1.0983586016105,-0.422729804305254,
11.4014739153211));
#24886=CARTESIAN_POINT('Ctrl Pts',(-1.05172558567923,0.255070021735645,
11.3357815485126));
#24887=CARTESIAN_POINT('Ctrl Pts',(-0.987911984794588,1.10119087049646,
11.6633738482479));
#24888=CARTESIAN_POINT('Ctrl Pts',(-0.938824599550145,1.62918676804705,
12.118444366207));
#24889=CARTESIAN_POINT('Ctrl Pts',(-0.906917799219455,1.86129831173361,
12.5060025659687));
#24890=CARTESIAN_POINT('Ctrl Pts',(-0.8774653682523,2.01909086104967,12.8869250426553));
#24891=CARTESIAN_POINT('Ctrl Pts',(-0.852921675636017,2.10344210544713,
13.2238746282784));
#24892=CARTESIAN_POINT('Ctrl Pts',(-0.82346924442792,2.10336023906826,13.6382150392374));
#24893=CARTESIAN_POINT('Ctrl Pts',(-0.798925551820312,2.05288515345181,
13.9785167276168));
#24894=CARTESIAN_POINT('Ctrl Pts',(-0.784199336265427,1.99276201071868,
14.1767695123879));
#24895=CARTESIAN_POINT('Ctrl Pts',(-0.771927489881348,1.92701180906461,
14.3354978336147));
#24896=CARTESIAN_POINT('Ctrl Pts',(-0.767018751279608,1.89915452647482,
14.3983444042317));
#24897=CARTESIAN_POINT('Ctrl Pts',(-0.757201274479887,1.8373345093657,14.5211477427863));
#24898=CARTESIAN_POINT('Ctrl Pts',(-0.740020689507575,1.71354968867764,
14.7277265250809));
#24899=CARTESIAN_POINT('Ctrl Pts',(-0.725294473998003,1.5821013242164,14.8878477727448));
#24900=CARTESIAN_POINT('Ctrl Pts',(-0.688478935115087,1.21787593692697,
15.2525572459267));
#24901=CARTESIAN_POINT('Ctrl Pts',(-0.634482811480685,0.535629923407611,
15.6386452075896));
#24902=CARTESIAN_POINT('Ctrl Pts',(-0.551034256607146,-0.675611669468313,
15.6090725230305));
#24903=CARTESIAN_POINT('Ctrl Pts',(-0.460222593798225,-1.78075976026697,
14.8719916564487));
#24904=CARTESIAN_POINT('Ctrl Pts',(-0.39640899300717,-2.10079561266312,
13.9811084932569));
#24905=CARTESIAN_POINT('Ctrl Pts',(-0.327686653883313,-2.10078058335638,
13.0188261639973));
#24906=CARTESIAN_POINT('Ctrl Pts',(-0.263873053108479,-1.78071719054053,
12.1279533037512));
#24907=CARTESIAN_POINT('Ctrl Pts',(-0.173061390264141,-0.675546085149363,
11.3909073940008));
#24908=CARTESIAN_POINT('Ctrl Pts',(-0.0896128354368363,0.535695028405412,
11.3613742093091));
#24909=CARTESIAN_POINT('Ctrl Pts',(-0.0356167117882722,1.21792863020294,
11.7474842871843));
#24910=CARTESIAN_POINT('Ctrl Pts',(0.00119882714953449,1.5821409272556,
12.1122065760469));
#24911=CARTESIAN_POINT('Ctrl Pts',(0.0134706734518924,1.69168094503692,
12.2456425525901));
#24912=CARTESIAN_POINT('Ctrl Pts',(0.0281968887692638,1.80199781030971,
12.4198898527391));
#24913=CARTESIAN_POINT('Ctrl Pts',(0.0380143661069976,1.869765720191,12.5395140145285));
#24914=CARTESIAN_POINT('Ctrl Pts',(0.0453774738404411,1.91388950252653,
12.632817279427));
#24915=CARTESIAN_POINT('Ctrl Pts',(0.0551949509498967,1.96648371523314,
12.7598019137801));
#24916=CARTESIAN_POINT('Ctrl Pts',(0.0699211664580535,2.03603803969005,
12.9541525027177));
#24917=CARTESIAN_POINT('Ctrl Pts',(0.0944648590302464,2.10337346788532,
13.2927895532997));
#24918=CARTESIAN_POINT('Ctrl Pts',(0.128826028756965,2.10342022866244,13.7761890983797));
#24919=CARTESIAN_POINT('Ctrl Pts',(0.15336972136151,2.01907498402452,14.1131363126915));
#24920=CARTESIAN_POINT('Ctrl Pts',(0.182822152323035,1.86126910792185,14.4940481517379));
#24921=CARTESIAN_POINT('Ctrl Pts',(0.214728952658297,1.62913755858449,14.8816613975882));
#24922=CARTESIAN_POINT('Ctrl Pts',(0.263816337904454,1.10114885817438,15.3365442020529));
#24923=CARTESIAN_POINT('Ctrl Pts',(0.327629938787875,0.254961693252239,
15.6645413334588));
#24924=CARTESIAN_POINT('Ctrl Pts',(0.384080431742756,-0.565417251061205,
15.58411753787));
#24925=CARTESIAN_POINT('Ctrl Pts',(0.433167816990411,-1.17421267603185,
15.2570430709813));
#24926=CARTESIAN_POINT('Ctrl Pts',(0.452802771110754,-1.38777891152299,
15.0821808121475));
#24927=CARTESIAN_POINT('Ctrl Pts',(0.467528986696092,-1.53355121890383,
14.9363637729679));
#24928=CARTESIAN_POINT('Ctrl Pts',(0.482255202131447,-1.67220097324411,
14.7834321919494));
#24929=CARTESIAN_POINT('Ctrl Pts',(0.506798894896568,-1.86393820732115,
14.4963287806024));
#24930=CARTESIAN_POINT('Ctrl Pts',(0.546068803023914,-2.07558385872978,
13.9859605789621));
#24931=CARTESIAN_POINT('Ctrl Pts',(0.58288434220745,-2.12713288286917,13.4631527628209));
#24932=CARTESIAN_POINT('Ctrl Pts',(0.612336772826988,-2.05621239601438,
13.0557692671339));
#24933=CARTESIAN_POINT('Ctrl Pts',(0.627062988604688,-2.00122721091256,
12.8570133666312));
#24934=CARTESIAN_POINT('Ctrl Pts',(0.63442609635068,-1.96644808599389,12.7598374701428));
#24935=CARTESIAN_POINT('Ctrl Pts',(0.658969788868636,-1.83495187428813,
12.4423817480464));
#24936=CARTESIAN_POINT('Ctrl Pts',(0.678604743062836,-1.67929338619673,
12.2094376125229));
#24937=CARTESIAN_POINT('Ctrl Pts',(0.712965912659437,-1.3391246609196,11.8692347536933));
#24938=CARTESIAN_POINT('Ctrl Pts',(0.742418343673966,-1.0043713030404,11.621362656488));
#24939=CARTESIAN_POINT('Ctrl Pts',(0.801323206053755,-0.219266438284931,
11.3391509721702));
#24940=CARTESIAN_POINT('Ctrl Pts',(0.845501852805669,0.422785332383879,
11.4014702224463));
#24941=CARTESIAN_POINT('Ctrl Pts',(0.892134868698232,1.02596016432553,11.6519098280612));
#24942=CARTESIAN_POINT('Ctrl Pts',(0.9264960382523,1.43775330693198,11.9131133902716));
#24943=CARTESIAN_POINT('Ctrl Pts',(0.990309639059457,1.997589526807,12.6276237677157));
#24944=CARTESIAN_POINT('Ctrl Pts',(1.05412324003347,2.17939061676467,13.5416037357365));
#24945=CARTESIAN_POINT('Ctrl Pts',(1.11793684081553,1.9355487439468,14.4159151616627));
#24946=CARTESIAN_POINT('Ctrl Pts',(1.15229801037463,1.65511433575482,14.8149129124571));
#24947=CARTESIAN_POINT('Ctrl Pts',(1.19402228783963,1.24201278196389,15.228005359044));
#24948=CARTESIAN_POINT('Ctrl Pts',(1.23820093466052,0.695366651073186,15.5552340623187));
#24949=CARTESIAN_POINT('Ctrl Pts',(1.30201453547294,-0.211347732752721,
15.6442822455439));
#24950=CARTESIAN_POINT('Ctrl Pts',(1.35110192052854,-0.881585564421509,
15.4409039994886));
#24951=CARTESIAN_POINT('Ctrl Pts',(1.38546309011478,-1.28341630114467,15.1720921147248));
#24952=CARTESIAN_POINT('Ctrl Pts',(1.40018930568574,-1.43636137847923,15.0335001546877));
#24953=CARTESIAN_POINT('Ctrl Pts',(1.40755241353526,-1.50924927860702,14.9606063251189));
#24954=CARTESIAN_POINT('Ctrl Pts',(1.41736989051428,-1.60406940639061,14.8610310686322));
#24955=CARTESIAN_POINT('Ctrl Pts',(1.44191358319504,-1.81590598476401,14.5894303706445));
#24956=CARTESIAN_POINT('Ctrl Pts',(1.48854659923337,-2.09906874241491,13.992921659037));
#24957=CARTESIAN_POINT('Ctrl Pts',(1.54745146132004,-2.14066944314819,13.1443828321464));
#24958=CARTESIAN_POINT('Ctrl Pts',(1.61126506208966,-1.7913275860122,12.3028775068152));
#24959=CARTESIAN_POINT('Ctrl Pts',(1.67262429363919,-1.17247419434806,11.6835056718477));
#24960=CARTESIAN_POINT('Ctrl Pts',(1.7364378942224,-0.318288581043391,11.3538988033697));
#24961=CARTESIAN_POINT('Ctrl Pts',(1.80270586417412,0.629792217940252,11.4239049270296));
#24962=CARTESIAN_POINT('Ctrl Pts',(1.86897383456717,1.45699477697742,11.8925381075738));
#24963=CARTESIAN_POINT('Ctrl Pts',(1.91315248114087,1.82187881023117,12.4106889066529));
#24964=CARTESIAN_POINT('Ctrl Pts',(1.93851429650132,1.95773839683463,12.738722731003));
#24965=CARTESIAN_POINT('Ctrl Pts',(1.94219585037175,1.97590320745963,12.7869877910394));
#24966=CARTESIAN_POINT('Ctrl Pts',(1.94710459114823,1.99772588033605,12.8521537931146));
#24967=CARTESIAN_POINT('Ctrl Pts',(1.95364955884026,2.02539974700884,12.9395117754336));
#24968=CARTESIAN_POINT('Ctrl Pts',(1.96469427167518,2.06301374026127,13.0896858122541));
#24969=CARTESIAN_POINT('Ctrl Pts',(1.97942039815674,2.0932981494276,13.2938672974093));
#24970=CARTESIAN_POINT('Ctrl Pts',(1.9892379438446,2.10004887693678,13.4313134002401));
#24971=CARTESIAN_POINT('Ctrl Pts',(2.0137817020949,2.10004702418293,13.7749282325411));
#24972=CARTESIAN_POINT('Ctrl Pts',(2.03341636935919,2.0454021480131,14.0497236079147));
#24973=CARTESIAN_POINT('Ctrl Pts',(2.05550590712,1.92704419174553,14.3354298869771));
#24974=CARTESIAN_POINT('Ctrl Pts',(2.08004991258307,1.78784894490175,14.6497273015641));
#24975=CARTESIAN_POINT('Ctrl Pts',(2.12422760644889,1.39794244545026,15.1490673633224));
#24976=CARTESIAN_POINT('Ctrl Pts',(2.18804254949195,0.594460675143825,15.5786124595441));
#24977=CARTESIAN_POINT('Ctrl Pts',(2.25185496534025,-0.318145958262575,
15.645976445297));
#24978=CARTESIAN_POINT('Ctrl Pts',(2.32057690990831,-1.23854770548309,15.2913665220797));
#24979=CARTESIAN_POINT('Ctrl Pts',(2.37979947534665,-1.81214548593813,14.6585194086623));
#24980=CARTESIAN_POINT('Ctrl Pts',(2.41692393438526,-1.99848999208968,14.1686392970802));
#24981=CARTESIAN_POINT('Ctrl Pts',(2.42950897538817,-2.04022719656258,13.9974632264163));
#24982=CARTESIAN_POINT('Ctrl Pts',(-2.42950819541373,2.04022498371351,13.9974756490669));
#24983=CARTESIAN_POINT('Ctrl Pts',(-2.42674114460071,2.03104804718875,14.0351116867474));
#24984=CARTESIAN_POINT('Ctrl Pts',(-2.42397402178904,2.02082976629947,14.0724948353366));
#24985=CARTESIAN_POINT('Ctrl Pts',(-2.42120691438128,2.00958510169509,14.1095664735261));
#24986=CARTESIAN_POINT('Ctrl Pts',(-2.41997973024847,2.00459820673664,14.126007369906));
#24987=CARTESIAN_POINT('Ctrl Pts',(-2.41875254898007,1.99940944248508,14.1423870005916));
#24988=CARTESIAN_POINT('Ctrl Pts',(-2.41752536541593,1.99402051067355,14.158700523574));
#24989=CARTESIAN_POINT('Ctrl Pts',(-2.41711630398564,1.99222419900596,14.1641383677883));
#24990=CARTESIAN_POINT('Ctrl Pts',(-2.41670724230984,1.99040564651285,14.1695688665664));
#24991=CARTESIAN_POINT('Ctrl Pts',(-2.41629818055378,1.98856490186073,14.1749918427932));
#24992=CARTESIAN_POINT('Ctrl Pts',(-2.41302569401814,1.97383897845102,14.2183755530088));
#24993=CARTESIAN_POINT('Ctrl Pts',(-2.40975320191403,1.95769276117011,14.2612778280205));
#24994=CARTESIAN_POINT('Ctrl Pts',(-2.40648070220672,1.94016289051323,14.3036048623514));
#24995=CARTESIAN_POINT('Ctrl Pts',(-2.38439162460657,1.82183784608482,14.5893085230205));
#24996=CARTESIAN_POINT('Ctrl Pts',(-2.3623022032065,1.63940406945196,14.8483855979339));
#24997=CARTESIAN_POINT('Ctrl Pts',(-2.34021273250533,1.41031970034931,15.0560301376478));
#24998=CARTESIAN_POINT('Ctrl Pts',(-2.31812341576338,1.18123692791921,15.2636732301204));
#24999=CARTESIAN_POINT('Ctrl Pts',(-2.29603411303243,0.905505533036176,
15.4198842057763));
#25000=CARTESIAN_POINT('Ctrl Pts',(-2.27394476221729,0.609627206226399,
15.5096574973231));
#25001=CARTESIAN_POINT('Ctrl Pts',(-2.25185547180329,0.313749688466697,
15.5994305433937));
#25002=CARTESIAN_POINT('Ctrl Pts',(-2.22976611622983,-0.00227496943738387,
15.6227660146606));
#25003=CARTESIAN_POINT('Ctrl Pts',(-2.20767679227486,-0.308126237136206,
15.5773863291275));
#25004=CARTESIAN_POINT('Ctrl Pts',(-2.18558744186399,-0.613977871146414,
15.5320065892441));
#25005=CARTESIAN_POINT('Ctrl Pts',(-2.16349812250749,-0.909656056643092,
15.4179117602001));
#25006=CARTESIAN_POINT('Ctrl Pts',(-2.14140882241474,-1.16674418597445,
15.2461753231618));
#25007=CARTESIAN_POINT('Ctrl Pts',(-2.12177391930598,-1.39526661487161,
15.0935209480874));
#25008=CARTESIAN_POINT('Ctrl Pts',(-2.10213903478246,-1.59329820329036,
14.8953227476681));
#25009=CARTESIAN_POINT('Ctrl Pts',(-2.0825041621263,-1.74605858618704,14.6667620421749));
#25010=CARTESIAN_POINT('Ctrl Pts',(-2.08250409479468,-1.74605911003076,
14.6667612583978));
#25011=CARTESIAN_POINT('Ctrl Pts',(-2.08250402746306,-1.74605963387394,
14.6667604746204));
#25012=CARTESIAN_POINT('Ctrl Pts',(-2.08250396013143,-1.7460601577166,14.6667596908426));
#25013=CARTESIAN_POINT('Ctrl Pts',(-2.06286901262028,-1.89882081250176,
14.4381979057571));
#25014=CARTESIAN_POINT('Ctrl Pts',(-2.04323407886215,-2.00630986779613,
14.1792734563894));
#25015=CARTESIAN_POINT('Ctrl Pts',(-2.02359915022586,-2.05986296659802,
13.9097172614467));
#25016=CARTESIAN_POINT('Ctrl Pts',(-1.99905543479842,-2.12680448910616,
13.5727712677571));
#25017=CARTESIAN_POINT('Ctrl Pts',(-1.97451177180188,-2.10947063979331,
13.2192131314304));
#25018=CARTESIAN_POINT('Ctrl Pts',(-1.94996810871334,-2.00982457650015,
12.8904089102543));
#25019=CARTESIAN_POINT('Ctrl Pts',(-1.94996807924008,-2.00982445684016,
12.8904085154097));
#25020=CARTESIAN_POINT('Ctrl Pts',(-1.94996804976682,-2.00982433718006,
12.8904081205652));
#25021=CARTESIAN_POINT('Ctrl Pts',(-1.94996802029356,-2.00982421751983,
12.8904077257206));
#25022=CARTESIAN_POINT('Ctrl Pts',(-1.93524184625727,-1.95003655762578,
12.6931255477529));
#25023=CARTESIAN_POINT('Ctrl Pts',(-1.92051567219421,-1.86061663401723,
12.5047548108404));
#25024=CARTESIAN_POINT('Ctrl Pts',(-1.90578949814881,-1.7460755686484,12.3333245625983));
#25025=CARTESIAN_POINT('Ctrl Pts',(-1.90578945655368,-1.746075245119,12.3333240783814));
#25026=CARTESIAN_POINT('Ctrl Pts',(-1.90578941495855,-1.74607492158938,
12.3333235941645));
#25027=CARTESIAN_POINT('Ctrl Pts',(-1.90578937336342,-1.74607459805957,
12.3333231099478));
#25028=CARTESIAN_POINT('Ctrl Pts',(-1.89842630966666,-1.68880417584947,
12.2476083052181));
#25029=CARTESIAN_POINT('Ctrl Pts',(-1.8910632459746,-1.62525351353008,12.1661286004572));
#25030=CARTESIAN_POINT('Ctrl Pts',(-1.88370018232131,-1.55602981070863,
12.0897478844421));
#25031=CARTESIAN_POINT('Ctrl Pts',(-1.88370013825672,-1.55602939643622,
12.0897474273382));
#25032=CARTESIAN_POINT('Ctrl Pts',(-1.88370009419213,-1.55602898216361,
12.0897469702345));
#25033=CARTESIAN_POINT('Ctrl Pts',(-1.88370005012754,-1.5560285678908,12.089746513131));
#25034=CARTESIAN_POINT('Ctrl Pts',(-1.88124572632274,-1.53295426671103,
12.0642866137492));
#25035=CARTESIAN_POINT('Ctrl Pts',(-1.87879140252236,-1.50924964356994,
12.0393932550014));
#25036=CARTESIAN_POINT('Ctrl Pts',(-1.87633707871304,-1.4849541104208,12.0150957483871));
#25037=CARTESIAN_POINT('Ctrl Pts',(-1.8763370332392,-1.48495366027189,12.0150952982016));
#25038=CARTESIAN_POINT('Ctrl Pts',(-1.87633698776536,-1.48495321012277,
12.0150948480164));
#25039=CARTESIAN_POINT('Ctrl Pts',(-1.87633694229152,-1.48495275997345,
12.0150943978313));
#25040=CARTESIAN_POINT('Ctrl Pts',(-1.87142825123432,-1.43636121939717,
11.9664989990058));
#25041=CARTESIAN_POINT('Ctrl Pts',(-1.86651956014098,-1.38537997155816,
11.9203021351265));
#25042=CARTESIAN_POINT('Ctrl Pts',(-1.86161086905512,-1.33225786159872,
11.8767037612623));
#25043=CARTESIAN_POINT('Ctrl Pts',(-1.86161082154616,-1.33225734745437,
11.8767033392938));
#25044=CARTESIAN_POINT('Ctrl Pts',(-1.86161077403721,-1.33225683330981,
11.8767029173255));
#25045=CARTESIAN_POINT('Ctrl Pts',(-1.86161072652826,-1.33225631916505,
11.8767024953575));
#25046=CARTESIAN_POINT('Ctrl Pts',(-1.85179329949156,-1.22601153083311,
11.7895054497431));
#25047=CARTESIAN_POINT('Ctrl Pts',(-1.84197587248468,-1.11120322439108,
11.7127024754497));
#25048=CARTESIAN_POINT('Ctrl Pts',(-1.83215844548016,-0.989982106116297,
11.6479419959326));
#25049=CARTESIAN_POINT('Ctrl Pts',(-1.83215839556304,-0.989981489762385,
11.6479416666551));
#25050=CARTESIAN_POINT('Ctrl Pts',(-1.83215834564591,-0.989980873408307,
11.6479413373781));
#25051=CARTESIAN_POINT('Ctrl Pts',(-1.83215829572879,-0.989980257054064,
11.6479410081013));
#25052=CARTESIAN_POINT('Ctrl Pts',(-1.81252337676606,-0.747537088060934,
11.5184198655243));
#25053=CARTESIAN_POINT('Ctrl Pts',(-1.79288845781252,-0.479442595783242,
11.4370689939149));
#25054=CARTESIAN_POINT('Ctrl Pts',(-1.77325353885603,-0.205901241008463,
11.4100931451571));
#25055=CARTESIAN_POINT('Ctrl Pts',(-1.77325350373935,-0.20590075178484,
11.4100930969113));
#25056=CARTESIAN_POINT('Ctrl Pts',(-1.77325346862266,-0.2059002625612,11.4100930486656));
#25057=CARTESIAN_POINT('Ctrl Pts',(-1.77325343350597,-0.205899773337542,
11.4100930004202));
#25058=CARTESIAN_POINT('Ctrl Pts',(-1.75361847943279,0.0676420901441113,
11.3831172979145));
#25059=CARTESIAN_POINT('Ctrl Pts',(-1.7339835253537,0.346630828755626,11.4105168521258));
#25060=CARTESIAN_POINT('Ctrl Pts',(-1.71434857242285,0.609603866520623,
11.4903764787249));
#25061=CARTESIAN_POINT('Ctrl Pts',(-1.68980486892179,0.938320328964335,
11.5902010621531));
#25062=CARTESIAN_POINT('Ctrl Pts',(-1.6652612051415,1.24201240084444,11.7719944916856));
#25063=CARTESIAN_POINT('Ctrl Pts',(-1.64071749321192,1.48501353328398,12.0149902447657));
#25064=CARTESIAN_POINT('Ctrl Pts',(-1.62353691580565,1.65511411862609,12.1850870645608));
#25065=CARTESIAN_POINT('Ctrl Pts',(-1.60635635576066,1.79533116747464,12.3845856394649));
#25066=CARTESIAN_POINT('Ctrl Pts',(-1.58917577804077,1.89826466745226,12.6020307354384));
#25067=CARTESIAN_POINT('Ctrl Pts',(-1.5719951880423,2.00119824099418,12.8194759868151));
#25068=CARTESIAN_POINT('Ctrl Pts',(-1.55481458653507,2.06684809797279,13.0548677492271));
#25069=CARTESIAN_POINT('Ctrl Pts',(-1.53763399538281,2.09027822246632,13.2941941600668));
#25070=CARTESIAN_POINT('Ctrl Pts',(-1.50818155323899,2.13044415039933,13.7044680095681));
#25071=CARTESIAN_POINT('Ctrl Pts',(-1.4787291219308,2.04653592497719,14.1263049840991));
#25072=CARTESIAN_POINT('Ctrl Pts',(-1.4492766906698,1.8524311106118,14.489997079784));
#25073=CARTESIAN_POINT('Ctrl Pts',(-1.43209610586582,1.73920330287967,14.7021508010533));
#25074=CARTESIAN_POINT('Ctrl Pts',(-1.41491552107903,1.5884779921667,14.8945191155991));
#25075=CARTESIAN_POINT('Ctrl Pts',(-1.39773493629675,1.41016704340693,15.0560041043591));
#25076=CARTESIAN_POINT('Ctrl Pts',(-1.38055437088535,1.23185629569033,15.2174889110469));
#25077=CARTESIAN_POINT('Ctrl Pts',(-1.3633738054772,1.02596005906369,15.3480904923515));
#25078=CARTESIAN_POINT('Ctrl Pts',(-1.34619324006513,0.803737867906403,
15.4403576967632));
#25079=CARTESIAN_POINT('Ctrl Pts',(-1.31674078958715,0.4227848594816,15.5985303298225));
#25080=CARTESIAN_POINT('Ctrl Pts',(-1.28728833908306,-0.00524924459700965,
15.6400763386564));
#25081=CARTESIAN_POINT('Ctrl Pts',(-1.25783590545734,-0.409628820444091,
15.5598546599255));
#25082=CARTESIAN_POINT('Ctrl Pts',(-1.24310969827096,-0.611818476196675,
15.5197438467804));
#25083=CARTESIAN_POINT('Ctrl Pts',(-1.22838349533185,-0.808094526764447,
15.4491910797825));
#25084=CARTESIAN_POINT('Ctrl Pts',(-1.21365729740076,-0.989920784653124,
15.3519468553259));
#25085=CARTESIAN_POINT('Ctrl Pts',(-1.19893106332822,-1.17174748878488,
15.2547023922097));
#25086=CARTESIAN_POINT('Ctrl Pts',(-1.18420483651807,-1.33912432283608,
15.1307663898753));
#25087=CARTESIAN_POINT('Ctrl Pts',(-1.16947859519051,-1.48491116620748,
14.984964988673));
#25088=CARTESIAN_POINT('Ctrl Pts',(-1.14984364421075,-1.6792932532193,14.7905634912569));
#25089=CARTESIAN_POINT('Ctrl Pts',(-1.13020869301272,-1.83495169412861,
14.5576198363276));
#25090=CARTESIAN_POINT('Ctrl Pts',(-1.11057373294137,-1.94014868488491,
14.3036552857682));
#25091=CARTESIAN_POINT('Ctrl Pts',(-1.10566499452238,-1.96644792400799,
14.2401641688082));
#25092=CARTESIAN_POINT('Ctrl Pts',(-1.10075625582403,-1.98963400801686,
14.175380241394));
#25093=CARTESIAN_POINT('Ctrl Pts',(-1.09584751722856,-2.00958163007088,
14.1096176421577));
#25094=CARTESIAN_POINT('Ctrl Pts',(-1.09339314802592,-2.01955544071146,
14.0767363438136));
#25095=CARTESIAN_POINT('Ctrl Pts',(-1.09093877881162,-2.02871963617376,
14.0436103770613));
#25096=CARTESIAN_POINT('Ctrl Pts',(-1.08848440943675,-2.03707029425241,
14.0102787380594));
#25097=CARTESIAN_POINT('Ctrl Pts',(-1.08112130266013,-2.06212226390212,
13.9102838393599));
#25098=CARTESIAN_POINT('Ctrl Pts',(-1.073758194709,-2.07985239778025,13.8084378943978));
#25099=CARTESIAN_POINT('Ctrl Pts',(-1.06639508644147,-2.08993525216245,
13.7058515180497));
#25100=CARTESIAN_POINT('Ctrl Pts',(-1.04676013622054,-2.11682285678353,
13.4322879196678));
#25101=CARTESIAN_POINT('Ctrl Pts',(-1.02712518272871,-2.08932984595779,
13.1534590171884));
#25102=CARTESIAN_POINT('Ctrl Pts',(-1.0074902241626,-2.00961703191972,12.8903925215421));
#25103=CARTESIAN_POINT('Ctrl Pts',(-0.9976727489314,-1.96976064135018,12.7588593280053));
#25104=CARTESIAN_POINT('Ctrl Pts',(-0.987855272123554,-1.91684930918749,
12.6312667292722));
#25105=CARTESIAN_POINT('Ctrl Pts',(-0.978037792689152,-1.85204603988445,
12.5100508178963));
#25106=CARTESIAN_POINT('Ctrl Pts',(-0.968220316533942,-1.78724279222673,
12.3888349470084));
#25107=CARTESIAN_POINT('Ctrl Pts',(-0.958402838465585,-1.71054761693102,
12.2739957704127));
#25108=CARTESIAN_POINT('Ctrl Pts',(-0.948585361863547,-1.62336083090999,
12.1677435485743));
#25109=CARTESIAN_POINT('Ctrl Pts',(-0.94367662333245,-1.5797674358562,12.1146174351651));
#25110=CARTESIAN_POINT('Ctrl Pts',(-0.938767885031536,-1.5335511375318,
12.0636380585001));
#25111=CARTESIAN_POINT('Ctrl Pts',(-0.933859146167239,-1.48495902976283,
12.0150427179392));
#25112=CARTESIAN_POINT('Ctrl Pts',(-0.924041681378216,-1.38777494231502,
11.9178521649162));
#25113=CARTESIAN_POINT('Ctrl Pts',(-0.914224210606306,-1.28101932887551,
11.8302092806163));
#25114=CARTESIAN_POINT('Ctrl Pts',(-0.904406743663767,-1.16673958206988,
11.753854257216));
#25115=CARTESIAN_POINT('Ctrl Pts',(-0.894589255603972,-1.05245958944984,
11.6774990695769));
#25116=CARTESIAN_POINT('Ctrl Pts',(-0.88477176938882,-0.930655414068331,
11.6124317688854));
#25117=CARTESIAN_POINT('Ctrl Pts',(-0.874954292095242,-0.803690428821663,
11.5596955953223));
#25118=CARTESIAN_POINT('Ctrl Pts',(-0.845501855242577,-0.422795408781944,
11.4014870479254));
#25119=CARTESIAN_POINT('Ctrl Pts',(-0.816049452022228,0.00528652468371188,
11.3599840213373));
#25120=CARTESIAN_POINT('Ctrl Pts',(-0.786597089225995,0.409645871011201,
11.4401775802091));
#25121=CARTESIAN_POINT('Ctrl Pts',(-0.786597056327444,0.409646322684179,
11.4401776697861));
#25122=CARTESIAN_POINT('Ctrl Pts',(-0.786597023428893,0.409646774357131,
11.4401777593631));
#25123=CARTESIAN_POINT('Ctrl Pts',(-0.786596990530342,0.409647226030055,
11.4401778489404));
#25124=CARTESIAN_POINT('Ctrl Pts',(-0.769416403546797,0.645524057364277,
11.4869576979523));
#25125=CARTESIAN_POINT('Ctrl Pts',(-0.752235817686795,0.87332860630921,
11.575148477315));
#25126=CARTESIAN_POINT('Ctrl Pts',(-0.735055235941776,1.07963262593515,
11.6988782710634));
#25127=CARTESIAN_POINT('Ctrl Pts',(-0.717874652738578,1.28593666307088,
11.8226080753131));
#25128=CARTESIAN_POINT('Ctrl Pts',(-0.700694074591393,1.47074018212349,
11.9818768663883));
#25129=CARTESIAN_POINT('Ctrl Pts',(-0.683513481359785,1.6233363607327,12.1677524954149));
#25130=CARTESIAN_POINT('Ctrl Pts',(-0.668787274631776,1.75413294277208,
12.3270742895953));
#25131=CARTESIAN_POINT('Ctrl Pts',(-0.654061054253819,1.86126702957128,
12.5059439796336));
#25132=CARTESIAN_POINT('Ctrl Pts',(-0.639334834882043,1.94016931490041,
12.696402786932));
#25133=CARTESIAN_POINT('Ctrl Pts',(-0.624608625535828,2.01907154651313,
12.8868614645667));
#25134=CARTESIAN_POINT('Ctrl Pts',(-0.609882413220272,2.06968867103886,
13.0890295728516));
#25135=CARTESIAN_POINT('Ctrl Pts',(-0.595156188405869,2.08991487504364,
13.294199089229));
#25136=CARTESIAN_POINT('Ctrl Pts',(-0.58533871587763,2.10339899637617,13.4309786179985));
#25137=CARTESIAN_POINT('Ctrl Pts',(-0.575521237900467,2.10337606278161,
13.5690921017574));
#25138=CARTESIAN_POINT('Ctrl Pts',(-0.565703756895726,2.08991123995878,
13.7058775206741));
#25139=CARTESIAN_POINT('Ctrl Pts',(-0.560795019318317,2.08317883255898,
13.7742701893794));
#25140=CARTESIAN_POINT('Ctrl Pts',(-0.555886280937762,2.07308595742924,
13.842330842726));
#25141=CARTESIAN_POINT('Ctrl Pts',(-0.550977541525792,2.05967771413265,
13.9097329223357));
#25142=CARTESIAN_POINT('Ctrl Pts',(-0.541160067288429,2.03286124006774,
14.0445370185767));
#25143=CARTESIAN_POINT('Ctrl Pts',(-0.531342589841728,1.9927833066971,14.1767068098724));
#25144=CARTESIAN_POINT('Ctrl Pts',(-0.5215251103279,1.94018712599076,14.3036911521357));
#25145=CARTESIAN_POINT('Ctrl Pts',(-0.519070741184284,1.92703808475101,
14.3354372281967));
#25146=CARTESIAN_POINT('Ctrl Pts',(-0.516616371956897,1.9131104322214,14.3668609506688));
#25147=CARTESIAN_POINT('Ctrl Pts',(-0.514162002461475,1.89841958485982,
14.3979234757846));
#25148=CARTESIAN_POINT('Ctrl Pts',(-0.51170763341165,1.88372874016539,14.428985995261));
#25149=CARTESIAN_POINT('Ctrl Pts',(-0.509253264130661,1.86827470105863,
14.4596873170088));
#25150=CARTESIAN_POINT('Ctrl Pts',(-0.506798894708835,1.8520778013819,14.4899921367648));
#25151=CARTESIAN_POINT('Ctrl Pts',(-0.501890157154438,1.81968401053648,
14.5506017603581));
#25152=CARTESIAN_POINT('Ctrl Pts',(-0.49698141893446,1.78431877874814,14.6096253783924));
#25153=CARTESIAN_POINT('Ctrl Pts',(-0.492072679301037,1.74613713236444,
14.6667661811286));
#25154=CARTESIAN_POINT('Ctrl Pts',(-0.482255202690933,1.66977386026196,
14.7810477556749));
#25155=CARTESIAN_POINT('Ctrl Pts',(-0.472437721954167,1.58214493861985,
14.8877980479252));
#25156=CARTESIAN_POINT('Ctrl Pts',(-0.462620248100799,1.48502125883098,
14.9850569304199));
#25157=CARTESIAN_POINT('Ctrl Pts',(-0.435622177181761,1.21793096309691,
15.2525190338407));
#25158=CARTESIAN_POINT('Ctrl Pts',(-0.408624102841353,0.876813824205406,
15.4455737261616));
#25159=CARTESIAN_POINT('Ctrl Pts',(-0.381626062624241,0.510319359615874,
15.5373233525677));
#25160=CARTESIAN_POINT('Ctrl Pts',(-0.354627945393328,0.143823849575187,
15.629073240696));
#25161=CARTESIAN_POINT('Ctrl Pts',(-0.327629911818704,-0.248048342260192,
15.6195176327191));
#25162=CARTESIAN_POINT('Ctrl Pts',(-0.300631877133074,-0.609642748411725,
15.509734974347));
#25163=CARTESIAN_POINT('Ctrl Pts',(-0.271179585708896,-1.00410789935089,
15.3899725218076));
#25164=CARTESIAN_POINT('Ctrl Pts',(-0.241727227064518,-1.36254128548648,
15.1509318358614));
#25165=CARTESIAN_POINT('Ctrl Pts',(-0.212274823799054,-1.62372373608068,
14.8324458723416));
#25166=CARTESIAN_POINT('Ctrl Pts',(-0.212274743641377,-1.62372444691498,
14.83244500555));
#25167=CARTESIAN_POINT('Ctrl Pts',(-0.212274663483701,-1.62372515774856,
14.8324441387578));
#25168=CARTESIAN_POINT('Ctrl Pts',(-0.212274583326024,-1.62372586858142,
14.8324432719651));
#25169=CARTESIAN_POINT('Ctrl Pts',(-0.177913437855339,-1.92843818387098,
14.4608757199683));
#25170=CARTESIAN_POINT('Ctrl Pts',(-0.143552266179561,-2.10078048114957,
13.9811748698202));
#25171=CARTESIAN_POINT('Ctrl Pts',(-0.109191126344327,-2.10078809799742,
13.5000333967581));
#25172=CARTESIAN_POINT('Ctrl Pts',(-0.0748299864062528,-2.10079571484529,
13.0188919222559));
#25173=CARTESIAN_POINT('Ctrl Pts',(-0.0404688972292225,-1.92846876156254,
12.5391857828251));
#25174=CARTESIAN_POINT('Ctrl Pts',(-0.00610780800733998,-1.6237682830356,
12.1676087467629));
#25175=CARTESIAN_POINT('Ctrl Pts',(-0.00610772729228924,-1.62376756728662,
12.1676078739192));
#25176=CARTESIAN_POINT('Ctrl Pts',(-0.00610764657723845,-1.62376685153691,
12.1676070010762));
#25177=CARTESIAN_POINT('Ctrl Pts',(-0.0061075658621877,-1.62376613578647,
12.1676061282337));
#25178=CARTESIAN_POINT('Ctrl Pts',(0.02334478860921,-1.36259383244188,11.8491120447897));
#25179=CARTESIAN_POINT('Ctrl Pts',(0.05279714312824,-1.00416802444854,11.61006015913));
#25180=CARTESIAN_POINT('Ctrl Pts',(0.0822494975908918,-0.609706932634201,
11.4902855935791));
#25181=CARTESIAN_POINT('Ctrl Pts',(0.0822495743794314,-0.609705904190406,
11.4902852813014));
#25182=CARTESIAN_POINT('Ctrl Pts',(0.0822496511679713,-0.609704875746364,
11.4902849690245));
#25183=CARTESIAN_POINT('Ctrl Pts',(0.0822497279565109,-0.60970384730208,
11.4902846567484));
#25184=CARTESIAN_POINT('Ctrl Pts',(0.109247743340253,-0.248114022230177,
11.3804917783663));
#25185=CARTESIAN_POINT('Ctrl Pts',(0.136245758689709,0.143756217175248,
11.3709246089638));
#25186=CARTESIAN_POINT('Ctrl Pts',(0.163243774048536,0.510253294332396,
11.4626631077541));
#25187=CARTESIAN_POINT('Ctrl Pts',(0.163243820507498,0.510253925011116,
11.4626632656204));
#25188=CARTESIAN_POINT('Ctrl Pts',(0.163243866966459,0.510254555689758,
11.4626634234869));
#25189=CARTESIAN_POINT('Ctrl Pts',(0.163243913425421,0.510255186368329,
11.4626635813538));
#25190=CARTESIAN_POINT('Ctrl Pts',(0.190241878204261,0.876751489577878,
11.5544022569341));
#25191=CARTESIAN_POINT('Ctrl Pts',(0.217239842989431,1.2178738606094,11.747446331933));
#25192=CARTESIAN_POINT('Ctrl Pts',(0.244237807829364,1.48497094349646,12.0149005971686));
#25193=CARTESIAN_POINT('Ctrl Pts',(0.244237904868314,1.48497190352514,12.0149015584811));
#25194=CARTESIAN_POINT('Ctrl Pts',(0.244238001907264,1.48497286355289,12.0149025197945));
#25195=CARTESIAN_POINT('Ctrl Pts',(0.244238098946214,1.48497382357971,12.0149034811088));
#25196=CARTESIAN_POINT('Ctrl Pts',(0.254055452352873,1.58209897381699,12.112158889888));
#25197=CARTESIAN_POINT('Ctrl Pts',(0.263872805766597,1.66973342405645,12.2189039991451));
#25198=CARTESIAN_POINT('Ctrl Pts',(0.273690159063131,1.74609831161928,12.3331820937207));
#25199=CARTESIAN_POINT('Ctrl Pts',(0.273690282714057,1.74609927344562,12.3331835330691));
#25200=CARTESIAN_POINT('Ctrl Pts',(0.273690406364982,1.74610023527018,12.3331849724187));
#25201=CARTESIAN_POINT('Ctrl Pts',(0.273690530015907,1.74610119709294,12.3331864117696));
#25202=CARTESIAN_POINT('Ctrl Pts',(0.276144769954554,1.76519158271812,12.3617548376027));
#25203=CARTESIAN_POINT('Ctrl Pts',(0.278599009885722,1.78357767573002,12.3907940324315));
#25204=CARTESIAN_POINT('Ctrl Pts',(0.281053249869367,1.80124177100558,12.4202656164393));
#25205=CARTESIAN_POINT('Ctrl Pts',(0.281053379138125,1.80124270140182,12.4202671687549));
#25206=CARTESIAN_POINT('Ctrl Pts',(0.281053508406883,1.80124363179606,12.4202687210717));
#25207=CARTESIAN_POINT('Ctrl Pts',(0.281053637675641,1.8012445621883,12.4202702733897));
#25208=CARTESIAN_POINT('Ctrl Pts',(0.283507872405506,1.8189085435929,12.4497418398569));
#25209=CARTESIAN_POINT('Ctrl Pts',(0.285962107187923,1.83585052932966,12.4796457923116));
#25210=CARTESIAN_POINT('Ctrl Pts',(0.288416341937125,1.85204792326276,12.5099480764146));
#25211=CARTESIAN_POINT('Ctrl Pts',(0.28841647645967,1.85204881108111,12.5099497373561));
#25212=CARTESIAN_POINT('Ctrl Pts',(0.288416610982214,1.85204969889722,12.5099513982988));
#25213=CARTESIAN_POINT('Ctrl Pts',(0.288416745504759,1.8520505867111,12.5099530592427));
#25214=CARTESIAN_POINT('Ctrl Pts',(0.293325339412051,1.88444603239207,12.5705592508536));
#25215=CARTESIAN_POINT('Ctrl Pts',(0.298233933186252,1.91386295584123,12.6327588437499));
#25216=CARTESIAN_POINT('Ctrl Pts',(0.303142526986869,1.94016133240765,12.6962485797819));
#25217=CARTESIAN_POINT('Ctrl Pts',(0.303142671740902,1.94016210794465,12.6962504520891));
#25218=CARTESIAN_POINT('Ctrl Pts',(0.303142816494935,1.94016288347893,12.6962523243973));
#25219=CARTESIAN_POINT('Ctrl Pts',(0.303142961248968,1.94016365901051,12.6962541967068));
#25220=CARTESIAN_POINT('Ctrl Pts',(0.308051545804713,1.96646180249381,12.7597438893171));
#25221=CARTESIAN_POINT('Ctrl Pts',(0.312960130387062,1.98964784013356,12.824524823218));
#25222=CARTESIAN_POINT('Ctrl Pts',(0.317868714962949,2.00959486168208,12.8902870681624));
#25223=CARTESIAN_POINT('Ctrl Pts',(0.317868868961942,2.00959548748799,12.8902891313476));
#25224=CARTESIAN_POINT('Ctrl Pts',(0.317869022960934,2.00959611329071,12.8902911945339));
#25225=CARTESIAN_POINT('Ctrl Pts',(0.317869176959927,2.00959673909024,12.8902932577211));
#25226=CARTESIAN_POINT('Ctrl Pts',(0.327686486540518,2.04949094636648,13.0218197521394));
#25227=CARTESIAN_POINT('Ctrl Pts',(0.337503796094336,2.07642872743024,13.1572715479576));
#25228=CARTESIAN_POINT('Ctrl Pts',(0.34732110568671,2.08990658617332,13.2940534921889));
#25229=CARTESIAN_POINT('Ctrl Pts',(0.347321273019919,2.08990681589953,13.2940558235977));
#25230=CARTESIAN_POINT('Ctrl Pts',(0.347321440353127,2.08990704562183,13.2940581550069));
#25231=CARTESIAN_POINT('Ctrl Pts',(0.347321607686336,2.08990727534022,13.2940604864164));
#25232=CARTESIAN_POINT('Ctrl Pts',(0.357138906642224,2.10338466063984,13.4308423277957));
#25233=CARTESIAN_POINT('Ctrl Pts',(0.366956205636128,2.10340210560045,13.5689542730069));
#25234=CARTESIAN_POINT('Ctrl Pts',(0.376773504604774,2.08991943609055,13.7057321885871));
#25235=CARTESIAN_POINT('Ctrl Pts',(0.37677368281039,2.08991919135038,13.7057346714078));
#25236=CARTESIAN_POINT('Ctrl Pts',(0.376773861016006,2.08991894660576,13.705737154228));
#25237=CARTESIAN_POINT('Ctrl Pts',(0.376774039221622,2.08991870185669,13.7057396370478));
#25238=CARTESIAN_POINT('Ctrl Pts',(0.391500037988321,2.06969389332211,13.9109071387579));
#25239=CARTESIAN_POINT('Ctrl Pts',(0.406226036698119,2.01909411423775,14.1130731793926));
#25240=CARTESIAN_POINT('Ctrl Pts',(0.420952035419789,1.94019731724951,14.303531214951));
#25241=CARTESIAN_POINT('Ctrl Pts',(0.420952252178541,1.94019615593125,14.3035340183905));
#25242=CARTESIAN_POINT('Ctrl Pts',(0.420952468937293,1.94019499460687,14.3035368218274));
#25243=CARTESIAN_POINT('Ctrl Pts',(0.420952685696044,1.94019383327638,14.3035396252619));
#25244=CARTESIAN_POINT('Ctrl Pts',(0.434481269190616,1.86771160838567,14.4785106329094));
#25245=CARTESIAN_POINT('Ctrl Pts',(0.448008986792176,1.77141272625529,14.6437074692471));
#25246=CARTESIAN_POINT('Ctrl Pts',(0.461537796611524,1.65482107705438,14.7929482633317));
#25247=CARTESIAN_POINT('Ctrl Pts',(0.462735448633046,1.64449967951663,14.8061599605257));
#25248=CARTESIAN_POINT('Ctrl Pts',(0.463933109214126,1.63401922235494,14.8192465934779));
#25249=CARTESIAN_POINT('Ctrl Pts',(0.465130779713237,1.62338213487436,14.8322038608054));
#25250=CARTESIAN_POINT('Ctrl Pts',(0.465130944545937,1.62338067091591,14.832205644085));
#25251=CARTESIAN_POINT('Ctrl Pts',(0.46513110937864,1.62337920695447,14.8322074273622));
#25252=CARTESIAN_POINT('Ctrl Pts',(0.465131274211341,1.62337774299007,14.8322092106369));
#25253=CARTESIAN_POINT('Ctrl Pts',(0.478955704393602,1.50059583489349,14.9817715028384));
#25254=CARTESIAN_POINT('Ctrl Pts',(0.492779776911533,1.35694827832357,15.1140870662735));
#25255=CARTESIAN_POINT('Ctrl Pts',(0.506603776941329,1.19804096667469,15.2245442356261));
#25256=CARTESIAN_POINT('Ctrl Pts',(0.509959725573088,1.15946423244761,15.251359092799));
#25257=CARTESIAN_POINT('Ctrl Pts',(0.513315669932859,1.11998833437995,15.2768859445942));
#25258=CARTESIAN_POINT('Ctrl Pts',(0.516671614100621,1.07969371213375,15.3010592167427));
#25259=CARTESIAN_POINT('Ctrl Pts',(0.516672103318057,1.07968783812906,15.3010627406351));
#25260=CARTESIAN_POINT('Ctrl Pts',(0.516672592535493,1.07968196410698,15.3010662644988));
#25261=CARTESIAN_POINT('Ctrl Pts',(0.516673081752929,1.07967609006749,15.3010697883337));
#25262=CARTESIAN_POINT('Ctrl Pts',(0.530551977098522,0.913032031030918,
15.4010395197798));
#25263=CARTESIAN_POINT('Ctrl Pts',(0.544428753882176,0.732367331110731,
15.4778744913662));
#25264=CARTESIAN_POINT('Ctrl Pts',(0.55830747106023,0.544729936753596,15.528371771255));
#25265=CARTESIAN_POINT('Ctrl Pts',(0.56160911318365,0.500092416067036,15.5403846932175));
#25266=CARTESIAN_POINT('Ctrl Pts',(0.564910865119463,0.455060225981205,
15.55090686959));
#25267=CARTESIAN_POINT('Ctrl Pts',(0.568212781513419,0.409728188158243,
15.559894738988));
#25268=CARTESIAN_POINT('Ctrl Pts',(0.568213447694807,0.409719042148382,
15.5598965523445));
#25269=CARTESIAN_POINT('Ctrl Pts',(0.56821411387619,0.409709896126496,15.5598983656384));
#25270=CARTESIAN_POINT('Ctrl Pts',(0.568214780057566,0.409700750092578,
15.5599001788699));
#25271=CARTESIAN_POINT('Ctrl Pts',(0.581928416503704,0.221425621908934,
15.5972263451643));
#25272=CARTESIAN_POINT('Ctrl Pts',(0.595639553657022,0.0280542714909028,
15.6080758169591));
#25273=CARTESIAN_POINT('Ctrl Pts',(0.609351027864107,-0.163321464899338,
15.5931068606506));
#25274=CARTESIAN_POINT('Ctrl Pts',(0.622795372555139,-0.3509687832454,15.5784295323608));
#25275=CARTESIAN_POINT('Ctrl Pts',(0.636240041294779,-0.53669963793286,
15.53892962429));
#25276=CARTESIAN_POINT('Ctrl Pts',(0.649687707863583,-0.713820511199585,
15.4751808339352));
#25277=CARTESIAN_POINT('Ctrl Pts',(0.651980844743659,-0.744023699584802,
15.4643101969012));
#25278=CARTESIAN_POINT('Ctrl Pts',(0.654274068794924,-0.773976462880374,
15.4527343431749));
#25279=CARTESIAN_POINT('Ctrl Pts',(0.656567393275285,-0.803645518258464,
15.4404559890673));
#25280=CARTESIAN_POINT('Ctrl Pts',(0.656568184580581,-0.80365575548431,
15.440451752455));
#25281=CARTESIAN_POINT('Ctrl Pts',(0.656568975885889,-0.803665992676384,
15.4404475157591));
#25282=CARTESIAN_POINT('Ctrl Pts',(0.656569767191209,-0.803676229834673,
15.4404432789796));
#25283=CARTESIAN_POINT('Ctrl Pts',(0.663812108772192,-0.897370781476111,
15.4016665844495));
#25284=CARTESIAN_POINT('Ctrl Pts',(0.671052677623533,-0.988141871459333,
15.3559275979264));
#25285=CARTESIAN_POINT('Ctrl Pts',(0.678292085188014,-1.07517040420396,
15.3039440676059));
#25286=CARTESIAN_POINT('Ctrl Pts',(0.680868544002631,-1.10614330196056,
15.285443461898));
#25287=CARTESIAN_POINT('Ctrl Pts',(0.683444855728359,-1.13664199148525,
15.2661514640664));
#25288=CARTESIAN_POINT('Ctrl Pts',(0.686021047927556,-1.16662883208436,
15.246099027821));
#25289=CARTESIAN_POINT('Ctrl Pts',(0.686022220568065,-1.16664248160322,
15.2460899002804));
#25290=CARTESIAN_POINT('Ctrl Pts',(0.6860233932087,-1.16665613101697,15.2460807725815));
#25291=CARTESIAN_POINT('Ctrl Pts',(0.686024565849459,-1.16666978032559,
15.2460716447245));
#25292=CARTESIAN_POINT('Ctrl Pts',(0.692997505214798,-1.24783342794592,
15.1917941575912));
#25293=CARTESIAN_POINT('Ctrl Pts',(0.699974870617991,-1.32527758889574,
15.1319195204613));
#25294=CARTESIAN_POINT('Ctrl Pts',(0.706951313639467,-1.39816345999789,
15.0669372185642));
#25295=CARTESIAN_POINT('Ctrl Pts',(0.709793278232913,-1.42785467433119,
15.0404656483637));
#25296=CARTESIAN_POINT('Ctrl Pts',(0.712635089759945,-1.45678979408922,
15.0131469672997));
#25297=CARTESIAN_POINT('Ctrl Pts',(0.715476386661461,-1.48491374763697,
14.9850161530564));
#25298=CARTESIAN_POINT('Ctrl Pts',(0.715476590101837,-1.48491576134687,
14.9850141388553));
#25299=CARTESIAN_POINT('Ctrl Pts',(0.71547679354221,-1.48491777505265,14.9850121246502));
#25300=CARTESIAN_POINT('Ctrl Pts',(0.715476996982581,-1.48491978875431,
14.985010110441));
#25301=CARTESIAN_POINT('Ctrl Pts',(0.720385621727778,-1.53350653583757,
14.9364111175307));
#25302=CARTESIAN_POINT('Ctrl Pts',(0.725294246463601,-1.57972464684981,
14.8854357575768));
#25303=CARTESIAN_POINT('Ctrl Pts',(0.730202871213679,-1.62331944447614,
14.832312607229));
#25304=CARTESIAN_POINT('Ctrl Pts',(0.730202985035305,-1.62332045535617,
14.8323113754047));
#25305=CARTESIAN_POINT('Ctrl Pts',(0.730203098856931,-1.62332146623479,
14.8323101435792));
#25306=CARTESIAN_POINT('Ctrl Pts',(0.730203212678557,-1.62332247711201,
14.8323089117526));
#25307=CARTESIAN_POINT('Ctrl Pts',(0.740020566846144,-1.71051275863889,
14.7260612791048));
#25308=CARTESIAN_POINT('Ctrl Pts',(0.749837921070188,-1.78720936133621,
14.6112244926074));
#25309=CARTESIAN_POINT('Ctrl Pts',(0.75965527526951,-1.8520153313365,14.490011685232));
#25310=CARTESIAN_POINT('Ctrl Pts',(0.759655398009369,-1.8520161415625,14.4900101697888));
#25311=CARTESIAN_POINT('Ctrl Pts',(0.759655520749229,-1.85201695178665,
14.4900086543445));
#25312=CARTESIAN_POINT('Ctrl Pts',(0.759655643489088,-1.85201776200893,
14.4900071388993));
#25313=CARTESIAN_POINT('Ctrl Pts',(0.769472986443132,-1.91682336045115,
14.3687943109336));
#25314=CARTESIAN_POINT('Ctrl Pts',(0.77929032937172,-1.96973820656263,14.2412050332778));
#25315=CARTESIAN_POINT('Ctrl Pts',(0.78910767232613,-2.00959827133535,14.1096747058508));
#25316=CARTESIAN_POINT('Ctrl Pts',(0.789107806547215,-2.00959881629554,
14.10967290759));
#25317=CARTESIAN_POINT('Ctrl Pts',(0.789107940768299,-2.0095993612533,14.1096711093284));
#25318=CARTESIAN_POINT('Ctrl Pts',(0.789108074989384,-2.00959990620861,
14.1096693110661));
#25319=CARTESIAN_POINT('Ctrl Pts',(0.808742936023748,-2.08932003286046,
13.846606094399));
#25320=CARTESIAN_POINT('Ctrl Pts',(0.82837779715767,-2.11682078260621,13.5677792192079));
#25321=CARTESIAN_POINT('Ctrl Pts',(0.84801265800844,-2.08994189988692,13.2942160069116));
#25322=CARTESIAN_POINT('Ctrl Pts',(0.848012751089102,-2.08994177246538,
13.2942147100629));
#25323=CARTESIAN_POINT('Ctrl Pts',(0.848012844169764,-2.08994164504261,
13.2942134132142));
#25324=CARTESIAN_POINT('Ctrl Pts',(0.848012937250426,-2.08994151761863,
13.2942121163657));
#25325=CARTESIAN_POINT('Ctrl Pts',(0.855375954735624,-2.07986181900396,
13.1916267014093));
#25326=CARTESIAN_POINT('Ctrl Pts',(0.862738972180859,-2.06213502104451,
13.089781475879));
#25327=CARTESIAN_POINT('Ctrl Pts',(0.870101989801644,-2.03708650871674,
12.989787025545));
#25328=CARTESIAN_POINT('Ctrl Pts',(0.870102079952299,-2.03708620203001,
12.9897858012419));
#25329=CARTESIAN_POINT('Ctrl Pts',(0.870102170102954,-2.03708589534218,
12.9897845769391));
#25330=CARTESIAN_POINT('Ctrl Pts',(0.870102260253609,-2.03708558865326,
12.9897833526366));
#25331=CARTESIAN_POINT('Ctrl Pts',(0.87255654094624,-2.02873622384413,12.9564526789597));
#25332=CARTESIAN_POINT('Ctrl Pts',(0.875010821658363,-2.01957337622892,
12.9233276386553));
#25333=CARTESIAN_POINT('Ctrl Pts',(0.877465102348043,-2.00960096503899,
12.890447224065));
#25334=CARTESIAN_POINT('Ctrl Pts',(0.87746519091255,-2.00960060517727,12.8904460375513));
#25335=CARTESIAN_POINT('Ctrl Pts',(0.877465279477059,-2.00960024531448,
12.8904448510379));
#25336=CARTESIAN_POINT('Ctrl Pts',(0.877465368041566,-2.00959988545065,
12.8904436645248));
#25337=CARTESIAN_POINT('Ctrl Pts',(0.882374021359468,-1.98965457264248,
12.8246816389388));
#25338=CARTESIAN_POINT('Ctrl Pts',(0.887282674587836,-1.96647088347394,
12.7598981571171));
#25339=CARTESIAN_POINT('Ctrl Pts',(0.892191327830066,-1.94017411668049,
12.6964073415817));
#25340=CARTESIAN_POINT('Ctrl Pts',(0.892191413138483,-1.94017365966399,
12.6964062381628));
#25341=CARTESIAN_POINT('Ctrl Pts',(0.892191498446901,-1.94017320264653,
12.6964051347442));
#25342=CARTESIAN_POINT('Ctrl Pts',(0.892191583755318,-1.94017274562812,
12.6964040313261));
#25343=CARTESIAN_POINT('Ctrl Pts',(0.911826482788449,-1.83498370745887,
12.4424372517412));
#25344=CARTESIAN_POINT('Ctrl Pts',(0.931461382050589,-1.67933317186298,
12.2094896248129));
#25345=CARTESIAN_POINT('Ctrl Pts',(0.951096281204927,-1.4849579573314,12.0150826785992));
#25346=CARTESIAN_POINT('Ctrl Pts',(0.951096336138496,-1.48495741351785,
12.0150821346969));
#25347=CARTESIAN_POINT('Ctrl Pts',(0.951096391072066,-1.48495686970399,
12.0150815907949));
#25348=CARTESIAN_POINT('Ctrl Pts',(0.951096446005635,-1.48495632588983,
12.0150810468931));
#25349=CARTESIAN_POINT('Ctrl Pts',(0.965822633066912,-1.33917462823082,
11.869275874655));
#25350=CARTESIAN_POINT('Ctrl Pts',(0.980548820070348,-1.17180250312542,
11.745335202403));
#25351=CARTESIAN_POINT('Ctrl Pts',(0.995275007116836,-0.989979777509019,
11.6480853541108));
#25352=CARTESIAN_POINT('Ctrl Pts',(0.995275035562517,-0.989979426293108,
11.6480851662591));
#25353=CARTESIAN_POINT('Ctrl Pts',(0.995275064008198,-0.989979075077144,
11.6480849784076));
#25354=CARTESIAN_POINT('Ctrl Pts',(0.995275092453878,-0.989978723861126,
11.6480847905562));
#25355=CARTESIAN_POINT('Ctrl Pts',(1.01000130806403,-0.808155589745198,
11.5508348567475));
#25356=CARTESIAN_POINT('Ctrl Pts',(1.02472752371917,-0.611881820252042,
11.4802759155044));
#25357=CARTESIAN_POINT('Ctrl Pts',(1.03945373105097,-0.409693485003987,
11.440158724781));
#25358=CARTESIAN_POINT('Ctrl Pts',(1.06890616740358,-0.00531651672141092,
11.3599242842489));
#25359=CARTESIAN_POINT('Ctrl Pts',(1.09835856480083,0.422718858224769,11.4014567292572));
#25360=CARTESIAN_POINT('Ctrl Pts',(1.12781103276819,0.803676834887431,11.5596173290528));
#25361=CARTESIAN_POINT('Ctrl Pts',(1.14499162521319,1.02590214187921,11.651877604455));
#25362=CARTESIAN_POINT('Ctrl Pts',(1.16217219918441,1.23180268872304,11.7824728394942));
#25363=CARTESIAN_POINT('Ctrl Pts',(1.17935278711131,1.41011865337131,11.9439522408167));
#25364=CARTESIAN_POINT('Ctrl Pts',(1.19653335546924,1.58843441491473,12.1054314582116));
#25365=CARTESIAN_POINT('Ctrl Pts',(1.2137139339289,1.73916557016386,12.2977947961871));
#25366=CARTESIAN_POINT('Ctrl Pts',(1.23089450663577,1.85239993741931,12.5099446821812));
#25367=CARTESIAN_POINT('Ctrl Pts',(1.26034695262402,2.04651623042694,12.8736306410409));
#25368=CARTESIAN_POINT('Ctrl Pts',(1.28979938757549,2.13043776648119,13.2954649769137));
#25369=CARTESIAN_POINT('Ctrl Pts',(1.31925182923742,2.09028477105871,13.7057401076938));
#25370=CARTESIAN_POINT('Ctrl Pts',(1.33643242010862,2.06686219052956,13.9450672659467));
#25371=CARTESIAN_POINT('Ctrl Pts',(1.35361300488886,2.001219748377,14.1804611088586));
#25372=CARTESIAN_POINT('Ctrl Pts',(1.37079358966893,1.89829301947601,14.3979096156095));
#25373=CARTESIAN_POINT('Ctrl Pts',(1.38797416029483,1.79536637537092,14.615357943216));
#25374=CARTESIAN_POINT('Ctrl Pts',(1.40515473092063,1.65515561944934,14.8148609281759));
#25375=CARTESIAN_POINT('Ctrl Pts',(1.42233530156288,1.4850603979144,14.9849630985979));
#25376=CARTESIAN_POINT('Ctrl Pts',(1.4468790083845,1.24206688296988,15.2279665405379));
#25377=CARTESIAN_POINT('Ctrl Pts',(1.4714227152453,0.938380485043318,15.4097695620104));
#25378=CARTESIAN_POINT('Ctrl Pts',(1.49596640169769,0.609667108510358,15.5096044609241));
#25379=CARTESIAN_POINT('Ctrl Pts',(1.51560133948904,0.346696559569775,15.5894723338038));
#25380=CARTESIAN_POINT('Ctrl Pts',(1.53523627501737,0.0677086654466856,
15.6168806170934));
#25381=CARTESIAN_POINT('Ctrl Pts',(1.55487121127339,-0.205834035211254,
15.5899134502986));
#25382=CARTESIAN_POINT('Ctrl Pts',(1.55487123562311,-0.205834374437557,
15.589913416856));
#25383=CARTESIAN_POINT('Ctrl Pts',(1.55487125997282,-0.205834713663856,
15.5899133834133));
#25384=CARTESIAN_POINT('Ctrl Pts',(1.55487128432254,-0.205835052890142,
15.5899133499706));
#25385=CARTESIAN_POINT('Ctrl Pts',(1.57450623185346,-0.479377897118042,
15.562946032826));
#25386=CARTESIAN_POINT('Ctrl Pts',(1.59414118117083,-0.747475540434009,
15.4816032311223));
#25387=CARTESIAN_POINT('Ctrl Pts',(1.61377614654412,-0.98992317360716,15.3520891539012));
#25388=CARTESIAN_POINT('Ctrl Pts',(1.62359362126025,-1.1111468917757,15.2873321678649));
#25389=CARTESIAN_POINT('Ctrl Pts',(1.63341109989897,-1.22595810977214,15.2105323735039));
#25390=CARTESIAN_POINT('Ctrl Pts',(1.64322857734255,-1.3322060403397,15.1233381527734));
#25391=CARTESIAN_POINT('Ctrl Pts',(1.64813731592424,-1.38533000410731,15.0797410436524));
#25392=CARTESIAN_POINT('Ctrl Pts',(1.65304605413425,-1.43631314634105,15.0335453301341));
#25393=CARTESIAN_POINT('Ctrl Pts',(1.65795479310598,-1.48490661205212,14.9849509679522));
#25394=CARTESIAN_POINT('Ctrl Pts',(1.66040916231399,-1.50920334215706,14.9606537896119));
#25395=CARTESIAN_POINT('Ctrl Pts',(1.66286353177777,-1.53290915910416,14.935760718772));
#25396=CARTESIAN_POINT('Ctrl Pts',(1.66531790094196,-1.55598464741419,14.91030106731));
#25397=CARTESIAN_POINT('Ctrl Pts',(1.67268100955675,-1.62521112289486,14.8339221012835));
#25398=CARTESIAN_POINT('Ctrl Pts',(1.68004411584012,-1.68876464552562,14.7524439070898));
#25399=CARTESIAN_POINT('Ctrl Pts',(1.68740722417849,-1.74603796406667,14.6667303670645));
#25400=CARTESIAN_POINT('Ctrl Pts',(1.70213341481545,-1.8605843986006,14.4953035901415));
#25401=CARTESIAN_POINT('Ctrl Pts',(1.71685961218156,-1.9500100817809,14.3069354949345));
#25402=CARTESIAN_POINT('Ctrl Pts',(1.73158581284833,-2.00980375572884,14.1096551008173));
#25403=CARTESIAN_POINT('Ctrl Pts',(1.75612952953808,-2.10946007757489,13.7808537887058));
#25404=CARTESIAN_POINT('Ctrl Pts',(1.78067325411209,-2.12680487991182,13.4272960132384));
#25405=CARTESIAN_POINT('Ctrl Pts',(1.80521694776939,-2.0598735121679,13.0903479751824));
#25406=CARTESIAN_POINT('Ctrl Pts',(1.82485190274241,-2.00632841784409,12.8207895440898));
#25407=CARTESIAN_POINT('Ctrl Pts',(1.84448685684207,-1.89884663042453,12.5618614060858));
#25408=CARTESIAN_POINT('Ctrl Pts',(1.86412181094562,-1.74609230897846,12.3332947925067));
#25409=CARTESIAN_POINT('Ctrl Pts',(1.8837567530877,-1.59333808058931,12.104728318169));
#25410=CARTESIAN_POINT('Ctrl Pts',(1.90339169523091,-1.3953113626414,11.9065233012212));
#25411=CARTESIAN_POINT('Ctrl Pts',(1.92302663734601,-1.16679229992759,11.7538614684367));
#25412=CARTESIAN_POINT('Ctrl Pts',(1.94511597261414,-0.909708058891522,
11.5821167091573));
#25413=CARTESIAN_POINT('Ctrl Pts',(1.967205307845,-0.614031857234684,11.4680127023866));
#25414=CARTESIAN_POINT('Ctrl Pts',(1.98929464309025,-0.308179898006852,
11.4226234687801));
#25415=CARTESIAN_POINT('Ctrl Pts',(2.01138396637403,-0.00232810439934122,
11.3772342597521));
#25416=CARTESIAN_POINT('Ctrl Pts',(2.0334732896713,0.313699460404102,11.4005597148878));
#25417=CARTESIAN_POINT('Ctrl Pts',(2.05556261303284,0.60958282695562,11.4903236518632));
#25418=CARTESIAN_POINT('Ctrl Pts',(2.07765193645337,0.905466194297148,11.5800875890782));
#25419=CARTESIAN_POINT('Ctrl Pts',(2.09974125993653,1.18120528463916,11.7362899754543));
#25420=CARTESIAN_POINT('Ctrl Pts',(2.12183058332263,1.410299996729,11.9439261381736));
#25421=CARTESIAN_POINT('Ctrl Pts',(2.14391987100573,1.63939433853275,12.1515619652902));
#25422=CARTESIAN_POINT('Ctrl Pts',(2.16600915858905,1.82184454727678,12.4106315915512));
#25423=CARTESIAN_POINT('Ctrl Pts',(2.18809844591148,1.9401828561742,12.6963347633748));
#25424=CARTESIAN_POINT('Ctrl Pts',(2.18809848161448,1.94018304744489,12.696335225158));
#25425=CARTESIAN_POINT('Ctrl Pts',(2.18809851731748,1.9401832387154,12.6963356869412));
#25426=CARTESIAN_POINT('Ctrl Pts',(2.18809855302049,1.94018342998576,12.6963361487246));
#25427=CARTESIAN_POINT('Ctrl Pts',(2.19137100463778,1.95771481149831,12.7386620993256));
#25428=CARTESIAN_POINT('Ctrl Pts',(2.19464345624932,1.97386246874068,12.7815634093583));
#25429=CARTESIAN_POINT('Ctrl Pts',(2.19791590921346,1.98858967767696,12.8249462719838));
#25430=CARTESIAN_POINT('Ctrl Pts',(2.1979159499312,1.98858986092135,12.8249468117783));
#25431=CARTESIAN_POINT('Ctrl Pts',(2.19791599064894,1.98859004416552,12.8249473515729));
#25432=CARTESIAN_POINT('Ctrl Pts',(2.19791603136667,1.98859022740948,12.8249478913675));
#25433=CARTESIAN_POINT('Ctrl Pts',(2.19832505183986,1.99043096143246,12.8303702714888));
#25434=CARTESIAN_POINT('Ctrl Pts',(2.19873407233418,1.99224950487864,12.8358001745293));
#25435=CARTESIAN_POINT('Ctrl Pts',(2.19914309251777,1.99404581840139,12.8412374204345));
#25436=CARTESIAN_POINT('Ctrl Pts',(2.1991431337548,1.99404599950401,12.8412379686124));
#25437=CARTESIAN_POINT('Ctrl Pts',(2.19914317499182,1.9940461806064,12.8412385167904));
#25438=CARTESIAN_POINT('Ctrl Pts',(2.19914321622885,1.99404636170857,12.8412390649686));
#25439=CARTESIAN_POINT('Ctrl Pts',(2.20037035749464,1.9994356433095,12.8575518801008));
#25440=CARTESIAN_POINT('Ctrl Pts',(2.20159749596331,2.00462482923011,12.8739307895866));
#25441=CARTESIAN_POINT('Ctrl Pts',(2.20282463620707,2.0096121270271,12.8903709813945));
#25442=CARTESIAN_POINT('Ctrl Pts',(2.20282467920292,2.00961230176922,12.8903715574166));
#25443=CARTESIAN_POINT('Ctrl Pts',(2.20282472219877,2.00961247651109,12.8903721334389));
#25444=CARTESIAN_POINT('Ctrl Pts',(2.20282476519461,2.00961265125272,12.8903727094612));
#25445=CARTESIAN_POINT('Ctrl Pts',(2.20773344473922,2.02956226773413,12.956135082359));
#25446=CARTESIAN_POINT('Ctrl Pts',(2.21264215268916,2.04628151524348,13.0228780180129));
#25447=CARTESIAN_POINT('Ctrl Pts',(2.21755083441069,2.05968958847734,13.0902792715416));
#25448=CARTESIAN_POINT('Ctrl Pts',(2.2175508877071,2.05968973405659,13.0902800033562));
#25449=CARTESIAN_POINT('Ctrl Pts',(2.21755094100351,2.05968987963544,13.0902807351709));
#25450=CARTESIAN_POINT('Ctrl Pts',(2.21755099429992,2.05969002521391,13.0902814669856));
#25451=CARTESIAN_POINT('Ctrl Pts',(2.22245966546082,2.07309799770043,13.1576825898092));
#25452=CARTESIAN_POINT('Ctrl Pts',(2.22736831039274,2.0831948122282,13.2257420223163));
#25453=CARTESIAN_POINT('Ctrl Pts',(2.23227698732179,2.08993197186516,13.294132840081));
#25454=CARTESIAN_POINT('Ctrl Pts',(2.23227705117833,2.08993205950827,13.294133729771));
#25455=CARTESIAN_POINT('Ctrl Pts',(2.23227711503487,2.0899321471508,13.2941346194611));
#25456=CARTESIAN_POINT('Ctrl Pts',(2.23227717889141,2.08993223479277,13.2941355091512));
#25457=CARTESIAN_POINT('Ctrl Pts',(2.23718584354925,2.09666929017565,13.3625261645558));
#25458=CARTESIAN_POINT('Ctrl Pts',(2.24209454020457,2.10004670853711,13.431248199927));
#25459=CARTESIAN_POINT('Ctrl Pts',(2.24700321565604,2.100048491072,13.4999703169702));
#25460=CARTESIAN_POINT('Ctrl Pts',(2.24700329190274,2.10004849109969,13.4999713844344));
#25461=CARTESIAN_POINT('Ctrl Pts',(2.24700336814945,2.10004849112656,13.4999724518985));
#25462=CARTESIAN_POINT('Ctrl Pts',(2.24700344439615,2.1000484911526,13.4999735193626));
#25463=CARTESIAN_POINT('Ctrl Pts',(2.26663826965199,2.10005519695717,13.7748637151604));
#25464=CARTESIAN_POINT('Ctrl Pts',(2.28627275562331,2.04541865167645,14.049661518633));
#25465=CARTESIAN_POINT('Ctrl Pts',(2.30590771896488,1.94022036581116,14.3036237190645));
#25466=CARTESIAN_POINT('Ctrl Pts',(2.30590790026447,1.94021939446198,14.3036260640264));
#25467=CARTESIAN_POINT('Ctrl Pts',(2.30590808156405,1.9402184231086,14.3036284089866));
#25468=CARTESIAN_POINT('Ctrl Pts',(2.30590826286364,1.94021745175103,14.3036307539451));
#25469=CARTESIAN_POINT('Ctrl Pts',(2.30836247613272,1.92706839443353,14.3353739497992));
#25470=CARTESIAN_POINT('Ctrl Pts',(2.31081669685968,1.91315083832213,14.3668017108966));
#25471=CARTESIAN_POINT('Ctrl Pts',(2.31327090916692,1.89845915781642,14.397860772894));
#25472=CARTESIAN_POINT('Ctrl Pts',(2.31327108900851,1.89845808122856,14.397863048863));
#25473=CARTESIAN_POINT('Ctrl Pts',(2.3132712688501,1.89845700463654,14.39786532483));
#25474=CARTESIAN_POINT('Ctrl Pts',(2.31327144869169,1.89845592804037,14.397867600795));
#25475=CARTESIAN_POINT('Ctrl Pts',(2.33536062905591,1.76622218206149,14.6774147398563));
#25476=CARTESIAN_POINT('Ctrl Pts',(2.3574491272971,1.5712727079731,14.9270944739197));
#25477=CARTESIAN_POINT('Ctrl Pts',(2.37953812370172,1.33229823339003,15.1233059771142));
#25478=CARTESIAN_POINT('Ctrl Pts',(2.37953847242699,1.33229446063208,15.1233090747609));
#25479=CARTESIAN_POINT('Ctrl Pts',(2.37953882115225,1.33229068786315,15.1233121723944));
#25480=CARTESIAN_POINT('Ctrl Pts',(2.37953916987752,1.33228691508325,15.1233152700145));
#25481=CARTESIAN_POINT('Ctrl Pts',(2.39619417790619,1.15210014392739,15.2712566242786));
#25482=CARTESIAN_POINT('Ctrl Pts',(2.41284942436104,0.946889344827322,15.3888028114828));
#25483=CARTESIAN_POINT('Ctrl Pts',(2.42950445771064,0.72822518719892,15.4697378980373));
#25484=CARTESIAN_POINT('Ctrl Pts',(-2.91746145426695,0.0017636091677427,
14.8994712573462));
#25485=CARTESIAN_POINT('Ctrl Pts',(-2.90019488125942,-0.159580608660099,
14.8996791954146));
#25486=CARTESIAN_POINT('Ctrl Pts',(-2.8657687140242,-0.480302096407746,
14.8438693373306));
#25487=CARTESIAN_POINT('Ctrl Pts',(-2.8019397152456,-1.00709100316185,14.5467293865288));
#25488=CARTESIAN_POINT('Ctrl Pts',(-2.73563696441919,-1.36578226769601,
14.010223019711));
#25489=CARTESIAN_POINT('Ctrl Pts',(-2.66693256929167,-1.42867373571422,
13.3592124992167));
#25490=CARTESIAN_POINT('Ctrl Pts',(-2.60311084828023,-1.25321990519817,
12.778393947455));
#25491=CARTESIAN_POINT('Ctrl Pts',(-2.53684614509442,-0.825318372599696,
12.3061946322186));
#25492=CARTESIAN_POINT('Ctrl Pts',(-2.4681235097376,-0.212191066831822,
12.069869359948));
#25493=CARTESIAN_POINT('Ctrl Pts',(-2.40430901915543,0.396119640741886,
12.114743545489));
#25494=CARTESIAN_POINT('Ctrl Pts',(-2.34049642694395,0.931518502467678,
12.4009672018237));
#25495=CARTESIAN_POINT('Ctrl Pts',(-2.29631706441142,1.19141144078301,12.7337364170638));
#25496=CARTESIAN_POINT('Ctrl Pts',(-2.27177360676358,1.2841798179601,12.9431797613183));
#25497=CARTESIAN_POINT('Ctrl Pts',(-2.24968444446761,1.36306447008945,13.1335712056504));
#25498=CARTESIAN_POINT('Ctrl Pts',(-2.23004927493927,1.3994922408639,13.3167047863868));
#25499=CARTESIAN_POINT('Ctrl Pts',(-2.20550563155682,1.39950586152936,13.5456943898369));
#25500=CARTESIAN_POINT('Ctrl Pts',(-2.1956882060897,1.39501224621372,13.6372896660342));
#25501=CARTESIAN_POINT('Ctrl Pts',(-2.1809619237048,1.37483761753456,13.7733623001193));
#25502=CARTESIAN_POINT('Ctrl Pts',(-2.16991730065325,1.34977676370599,13.8734411623136));
#25503=CARTESIAN_POINT('Ctrl Pts',(-2.16337230325175,1.33133763959568,13.9316592238358));
#25504=CARTESIAN_POINT('Ctrl Pts',(-2.15846356632158,1.31679708591878,13.9750876202867));
#25505=CARTESIAN_POINT('Ctrl Pts',(-2.15478201233856,1.30469358312819,14.0072528950141));
#25506=CARTESIAN_POINT('Ctrl Pts',(-2.12942019628186,1.21416701951389,14.2258649461565));
#25507=CARTESIAN_POINT('Ctrl Pts',(-2.08524154941588,0.971022892704046,
14.5711831154863));
#25508=CARTESIAN_POINT('Ctrl Pts',(-2.01897357959321,0.419779824527784,
14.8835182023753));
#25509=CARTESIAN_POINT('Ctrl Pts',(-1.95270560955346,-0.212032912475402,
14.930206696884));
#25510=CARTESIAN_POINT('Ctrl Pts',(-1.88889200873837,-0.781287448270816,
14.7105831133688));
#25511=CARTESIAN_POINT('Ctrl Pts',(-1.82753277730078,-1.19372337695382,
14.2978470446545));
#25512=CARTESIAN_POINT('Ctrl Pts',(-1.76371917662607,-1.42656061512116,
13.7370678108623));
#25513=CARTESIAN_POINT('Ctrl Pts',(-1.7048143142447,-1.39886856763557,13.1715868436166));
#25514=CARTESIAN_POINT('Ctrl Pts',(-1.65818129841028,-1.21018686470934,
12.7740536866313));
#25515=CARTESIAN_POINT('Ctrl Pts',(-1.63363760575663,-1.06902587007685,
12.5930469222915));
#25516=CARTESIAN_POINT('Ctrl Pts',(-1.62382012866622,-1.00584000033722,
12.5266849165902));
#25517=CARTESIAN_POINT('Ctrl Pts',(-1.61645702078024,-0.957269064068352,
12.4781046551932));
#25518=CARTESIAN_POINT('Ctrl Pts',(-1.60173080532553,-0.855349270287673,
12.3857391481269));
#25519=CARTESIAN_POINT('Ctrl Pts',(-1.56736963573534,-0.587573086682263,
12.2065836919316));
#25520=CARTESIAN_POINT('Ctrl Pts',(-1.51828225061532,-0.140924113539522,
12.0710241098653));
#25521=CARTESIAN_POINT('Ctrl Pts',(-1.45446864975801,0.463327639827352,
12.1303333085334));
#25522=CARTESIAN_POINT('Ctrl Pts',(-1.4102900030623,0.827632817053937,12.3483837391908));
#25523=CARTESIAN_POINT('Ctrl Pts',(-1.36856572560249,1.10294509845384,12.6236601489423));
#25524=CARTESIAN_POINT('Ctrl Pts',(-1.33420455599182,1.28984508344393,12.8895483365267));
#25525=CARTESIAN_POINT('Ctrl Pts',(-1.27039095511894,1.45237769519615,13.4721941418966));
#25526=CARTESIAN_POINT('Ctrl Pts',(-1.20657735438816,1.33125646100672,14.0812913187321));
#25527=CARTESIAN_POINT('Ctrl Pts',(-1.14276375353099,0.958199115373982,
14.5574728751379));
#25528=CARTESIAN_POINT('Ctrl Pts',(-1.10840258391648,0.683783826603428,
14.7315587417309));
#25529=CARTESIAN_POINT('Ctrl Pts',(-1.06176956797103,0.281828004010735,
14.8984788199422));
#25530=CARTESIAN_POINT('Ctrl Pts',(-1.01759092122265,-0.146042922087093,
14.9400333797164));
#25531=CARTESIAN_POINT('Ctrl Pts',(-0.958686059061629,-0.669259334769407,
14.7519920373476));
#25532=CARTESIAN_POINT('Ctrl Pts',(-0.929233627848142,-0.892353263312432,
14.5868188755852));
#25533=CARTESIAN_POINT('Ctrl Pts',(-0.894872458265258,-1.11905952818674,
14.3601151929184));
#25534=CARTESIAN_POINT('Ctrl Pts',(-0.875237504264326,-1.22280109179422,
14.2048833087194));
#25535=CARTESIAN_POINT('Ctrl Pts',(-0.850693811484429,-1.31044387511483,
13.9933309242246));
#25536=CARTESIAN_POINT('Ctrl Pts',(-0.843330703622131,-1.33362477081705,
13.9285726569875));
#25537=CARTESIAN_POINT('Ctrl Pts',(-0.828604488330937,-1.37027511219623,
13.796120759091));
#25538=CARTESIAN_POINT('Ctrl Pts',(-0.799152057004847,-1.41755272872254,
13.5246365146694));
#25539=CARTESIAN_POINT('Ctrl Pts',(-0.762336518301005,-1.38321876804832,
13.1762297382245));
#25540=CARTESIAN_POINT('Ctrl Pts',(-0.723066610044072,-1.24219377380554,
12.8361031544499));
#25541=CARTESIAN_POINT('Ctrl Pts',(-0.698522917480207,-1.11442727944758,
12.6447694003354));
#25542=CARTESIAN_POINT('Ctrl Pts',(-0.683796701920851,-1.022035166451,12.5428438921579));
#25543=CARTESIAN_POINT('Ctrl Pts',(-0.669070486267723,-0.924892975936484,
12.4456842991101));
#25544=CARTESIAN_POINT('Ctrl Pts',(-0.649435532212222,-0.782612198906497,
12.3288629646018));
#25545=CARTESIAN_POINT('Ctrl Pts',(-0.629800578134346,-0.620272858103612,
12.2421298000267));
#25546=CARTESIAN_POINT('Ctrl Pts',(-0.590530669970707,-0.281835429088842,
12.1015329289278));
#25547=CARTESIAN_POINT('Ctrl Pts',(-0.543897653950655,0.169856841999108,
12.057714018699));
#25548=CARTESIAN_POINT('Ctrl Pts',(-0.480084053153129,0.733743693002342,
12.2759770805796));
#25549=CARTESIAN_POINT('Ctrl Pts',(-0.430996667965097,1.08563450897863,
12.5792117928079));
#25550=CARTESIAN_POINT('Ctrl Pts',(-0.399089867586218,1.24033965540433,
12.8374730527932));
#25551=CARTESIAN_POINT('Ctrl Pts',(-0.369637436543767,1.34551709542376,
13.0913163915541));
#25552=CARTESIAN_POINT('Ctrl Pts',(-0.345093743843038,1.40174956442927,
13.3158597093218));
#25553=CARTESIAN_POINT('Ctrl Pts',(-0.315641312775735,1.4017190298085,13.5919825333234));
#25554=CARTESIAN_POINT('Ctrl Pts',(-0.291097620067433,1.36810137257278,
13.8187677293287));
#25555=CARTESIAN_POINT('Ctrl Pts',(-0.276371404600847,1.32804594187603,
13.9508899624769));
#25556=CARTESIAN_POINT('Ctrl Pts',(-0.264099558306616,1.28423821565556,
14.0566727881033));
#25557=CARTESIAN_POINT('Ctrl Pts',(-0.259190819742416,1.26567732595888,
14.0985563199077));
#25558=CARTESIAN_POINT('Ctrl Pts',(-0.249373342517745,1.2244866667904,14.1803979865844));
#25559=CARTESIAN_POINT('Ctrl Pts',(-0.232192757856559,1.14200653059235,
14.3180724570658));
#25560=CARTESIAN_POINT('Ctrl Pts',(-0.217466542354616,1.05441689387111,
14.4247877087319));
#25561=CARTESIAN_POINT('Ctrl Pts',(-0.180651003477795,0.811713222933898,
14.6678575357953));
#25562=CARTESIAN_POINT('Ctrl Pts',(-0.126654879772195,0.357076873077649,
14.9251932675087));
#25563=CARTESIAN_POINT('Ctrl Pts',(-0.0432063248173501,-0.45011407660554,
14.9055610385193));
#25564=CARTESIAN_POINT('Ctrl Pts',(0.0476053377514023,-1.1866456835083,
14.4144219839806));
#25565=CARTESIAN_POINT('Ctrl Pts',(0.111418938619706,-1.39997507961811,
13.8207407870374));
#25566=CARTESIAN_POINT('Ctrl Pts',(0.180141277840581,-1.40002079011879,
13.1794589876531));
#25567=CARTESIAN_POINT('Ctrl Pts',(0.243954878721026,-1.18677621847386,
12.5857475948577));
#25568=CARTESIAN_POINT('Ctrl Pts',(0.33476654126412,-0.450314644322968,
12.0945038436987));
#25569=CARTESIAN_POINT('Ctrl Pts',(0.418215096253102,0.356872553823869,
12.0747577299328));
#25570=CARTESIAN_POINT('Ctrl Pts',(0.472211219947981,0.81154531020039,12.3320292976198));
#25571=CARTESIAN_POINT('Ctrl Pts',(0.509026758783489,1.05428248464001,12.5750655439176));
#25572=CARTESIAN_POINT('Ctrl Pts',(0.521298605036259,1.12728903261987,12.6639834235209));
#25573=CARTESIAN_POINT('Ctrl Pts',(0.536024820681476,1.2008160076927,12.7800981181811));
#25574=CARTESIAN_POINT('Ctrl Pts',(0.545842297501875,1.24598447329656,12.8598136192458));
#25575=CARTESIAN_POINT('Ctrl Pts',(0.55320540537187,1.27539462490051,12.9219898354186));
#25576=CARTESIAN_POINT('Ctrl Pts',(0.563022882570486,1.31045155162959,13.0066113374631));
#25577=CARTESIAN_POINT('Ctrl Pts',(0.577749098072713,1.35681484657344,13.1361256281581));
#25578=CARTESIAN_POINT('Ctrl Pts',(0.602292790807561,1.40170777207648,13.3617946126849));
#25579=CARTESIAN_POINT('Ctrl Pts',(0.6366539602946,1.4017668435254,13.6839400854214));
#25580=CARTESIAN_POINT('Ctrl Pts',(0.661197653004655,1.3455774953339,13.9084907361462));
#25581=CARTESIAN_POINT('Ctrl Pts',(0.69065008405075,1.24043476680437,14.1623493334017));
#25582=CARTESIAN_POINT('Ctrl Pts',(0.722556884425975,1.08576652175257,14.420632835335));
#25583=CARTESIAN_POINT('Ctrl Pts',(0.771644269613912,0.733918423823554,
14.7239179023662));
#25584=CARTESIAN_POINT('Ctrl Pts',(0.835457870411991,0.170062504683883,
14.9422614843921));
#25585=CARTESIAN_POINT('Ctrl Pts',(0.882090886436469,-0.281636142740509,
14.8985069783426));
#25586=CARTESIAN_POINT('Ctrl Pts',(0.921360794598973,-0.620093629397158,
14.7579583436346));
#25587=CARTESIAN_POINT('Ctrl Pts',(0.940995748673728,-0.78244533749354,
14.6712483123915));
#25588=CARTESIAN_POINT('Ctrl Pts',(0.960630702731577,-0.924742763084939,
14.5544472535077));
#25589=CARTESIAN_POINT('Ctrl Pts',(0.975356918382398,-1.02189879158319,
14.4573014979626));
#25590=CARTESIAN_POINT('Ctrl Pts',(0.990083133939201,-1.11430541824352,
14.3553891484536));
#25591=CARTESIAN_POINT('Ctrl Pts',(1.01462682652934,-1.2420991675918,14.1640736023963));
#25592=CARTESIAN_POINT('Ctrl Pts',(1.05389673473115,-1.3831725908153,13.8239671087647));
#25593=CARTESIAN_POINT('Ctrl Pts',(1.09071227348601,-1.41755618749819,13.4755652595451));
#25594=CARTESIAN_POINT('Ctrl Pts',(1.12016470478803,-1.37031722480694,13.2040742906169));
#25595=CARTESIAN_POINT('Ctrl Pts',(1.13489092008799,-1.3336857405026,13.0716171771824));
#25596=CARTESIAN_POINT('Ctrl Pts',(1.14225402794831,-1.31051406497217,13.0068556110899));
#25597=CARTESIAN_POINT('Ctrl Pts',(1.16679772072381,-1.22290140273311,12.7952907540047));
#25598=CARTESIAN_POINT('Ctrl Pts',(1.1864326747268,-1.11918194748711,12.6400441106599));
#25599=CARTESIAN_POINT('Ctrl Pts',(1.2207938443113,-0.892507962849632,12.4133081589902));
#25600=CARTESIAN_POINT('Ctrl Pts',(1.25024627552374,-0.669437554782479,
12.2481032416591));
#25601=CARTESIAN_POINT('Ctrl Pts',(1.3091511376846,-0.146247920258923,12.0599874179223));
#25602=CARTESIAN_POINT('Ctrl Pts',(1.35332978443315,0.281628913559978,12.1014810662009));
#25603=CARTESIAN_POINT('Ctrl Pts',(1.39996280037785,0.683608494465903,12.268343919929));
#25604=CARTESIAN_POINT('Ctrl Pts',(1.43432396999435,0.958048563093325,12.442390719136));
#25605=CARTESIAN_POINT('Ctrl Pts',(1.4981375708502,1.33117369477561,12.9185191623767));
#25606=CARTESIAN_POINT('Ctrl Pts',(1.56195117158053,1.45238164110855,13.5275990903951));
#25607=CARTESIAN_POINT('Ctrl Pts',(1.62576477245543,1.28993197840348,14.1102680289494));
#25608=CARTESIAN_POINT('Ctrl Pts',(1.66012594206798,1.10306984876638,14.3761828219785));
#25609=CARTESIAN_POINT('Ctrl Pts',(1.70185021952445,0.827796759986248,14.6514984236658));
#25610=CARTESIAN_POINT('Ctrl Pts',(1.74602886622133,0.463522631126779,14.8696007159398));
#25611=CARTESIAN_POINT('Ctrl Pts',(1.80984246707339,-0.1407206716199,14.9289959381943));
#25612=CARTESIAN_POINT('Ctrl Pts',(1.85892985219695,-0.587388936191916,
14.7934999445719));
#25613=CARTESIAN_POINT('Ctrl Pts',(1.8932910217891,-0.855190621007161,14.6143826120952));
#25614=CARTESIAN_POINT('Ctrl Pts',(1.90801723724395,-0.95712356280611,14.5220316155655));
#25615=CARTESIAN_POINT('Ctrl Pts',(1.91538034513003,-1.00570141455371,14.4734582694652));
#25616=CARTESIAN_POINT('Ctrl Pts',(1.92519782222027,-1.06889673120442,14.4071052598134));
#25617=CARTESIAN_POINT('Ctrl Pts',(1.94974151487335,-1.21008349176762,14.2261185936406));
#25618=CARTESIAN_POINT('Ctrl Pts',(1.99637453070844,-1.39882177721573,13.8286123034665));
#25619=CARTESIAN_POINT('Ctrl Pts',(2.05527939308903,-1.42659432214954,13.2631352856935));
#25620=CARTESIAN_POINT('Ctrl Pts',(2.11909299376731,-1.19383689080884,12.7023229120511));
#25621=CARTESIAN_POINT('Ctrl Pts',(2.18045222520523,-0.781459684572717,
12.2895281354887));
#25622=CARTESIAN_POINT('Ctrl Pts',(2.24426582602376,-0.212236361467477,
12.0698235172568));
#25623=CARTESIAN_POINT('Ctrl Pts',(2.31053379607291,0.419583147593255,12.1164220761731));
#25624=CARTESIAN_POINT('Ctrl Pts',(2.37680176589273,0.970870796055125,12.4286786933557));
#25625=CARTESIAN_POINT('Ctrl Pts',(2.42098041277556,1.21406435463139,12.7739622687326));
#25626=CARTESIAN_POINT('Ctrl Pts',(2.44634222883891,1.30462209891747,12.9925614349691));
#25627=CARTESIAN_POINT('Ctrl Pts',(2.4500237828227,1.31673018620759,13.0247249870419));
#25628=CARTESIAN_POINT('Ctrl Pts',(2.45493251975282,1.33127691935092,13.0681513140835));
#25629=CARTESIAN_POINT('Ctrl Pts',(2.46147751715357,1.34972436758129,13.1263667423369));
#25630=CARTESIAN_POINT('Ctrl Pts',(2.47252214020686,1.37479942108684,13.2264420569245));
#25631=CARTESIAN_POINT('Ctrl Pts',(2.48724842259595,1.39499363824062,13.3625117988546));
#25632=CARTESIAN_POINT('Ctrl Pts',(2.49706584806392,1.39950021010734,13.4541064541347));
#25633=CARTESIAN_POINT('Ctrl Pts',(2.52160949145431,1.39951926866424,13.6830960638344));
#25634=CARTESIAN_POINT('Ctrl Pts',(2.54124466103345,1.3631190589702,13.8662350598753));
#25635=CARTESIAN_POINT('Ctrl Pts',(2.56333382333658,1.2842613255101,14.0566376252996));
#25636=CARTESIAN_POINT('Ctrl Pts',(2.58787728099126,1.19152225787391,14.2660936889693));
#25637=CARTESIAN_POINT('Ctrl Pts',(2.63205664366046,0.931682750775297,14.5989038479848));
#25638=CARTESIAN_POINT('Ctrl Pts',(2.69586923597156,0.396320608623301,14.8851965578387));
#25639=CARTESIAN_POINT('Ctrl Pts',(2.75968372689716,-0.211964411383521,
14.9301722674985));
#25640=CARTESIAN_POINT('Ctrl Pts',(2.82840636255072,-0.825146742340399,
14.6939085236109));
#25641=CARTESIAN_POINT('Ctrl Pts',(2.89467106680061,-1.25302913630202,14.221827888447));
#25642=CARTESIAN_POINT('Ctrl Pts',(2.95849278830799,-1.42868057472017,13.6409334123114));
#25643=CARTESIAN_POINT('Ctrl Pts',(3.02719718612572,-1.36551532321063,12.9901843349406));
#25644=CARTESIAN_POINT('Ctrl Pts',(3.0805160037115,-1.07762573723313,12.55826580189));
#25645=CARTESIAN_POINT('Ctrl Pts',(3.11415879661038,-0.826194988464377,
12.3697490786105));
#25646=CARTESIAN_POINT('Ctrl Pts',(3.11836033000717,-0.79392026024566,12.3475163248423));
#25647=CARTESIAN_POINT('Ctrl Pts',(-3.00252836970136,0.00205538494515771,
15.1331908023729));
#25648=CARTESIAN_POINT('Ctrl Pts',(-2.98527982013788,-0.185981147804069,
15.1334545181963));
#25649=CARTESIAN_POINT('Ctrl Pts',(-2.95085538393473,-0.560235514350509,
15.0684314612154));
#25650=CARTESIAN_POINT('Ctrl Pts',(-2.88698949839108,-1.17552199967255,
14.7213621162832));
#25651=CARTESIAN_POINT('Ctrl Pts',(-2.82071377950267,-1.59379469789951,
14.0955052168205));
#25652=CARTESIAN_POINT('Ctrl Pts',(-2.75199539264616,-1.66728946021813,
13.3356189189095));
#25653=CARTESIAN_POINT('Ctrl Pts',(-2.68817998979099,-1.46249020257107,
12.6578747738934));
#25654=CARTESIAN_POINT('Ctrl Pts',(-2.62191274641039,-0.963128682093589,
12.1067915533372));
#25655=CARTESIAN_POINT('Ctrl Pts',(-2.5531903417797,-0.247577521527219,
11.8310330526963));
#25656=CARTESIAN_POINT('Ctrl Pts',(-2.48937654342735,0.462308854742993,
11.8833961450926));
#25657=CARTESIAN_POINT('Ctrl Pts',(-2.42556316698634,1.08711300487288,12.2174675831258));
#25658=CARTESIAN_POINT('Ctrl Pts',(-2.38138436118434,1.39043544977562,12.6057667639547));
#25659=CARTESIAN_POINT('Ctrl Pts',(-2.3568407207863,1.49864818055694,12.8502306958011));
#25660=CARTESIAN_POINT('Ctrl Pts',(-2.33475143321486,1.59075305876895,13.072392949461));
#25661=CARTESIAN_POINT('Ctrl Pts',(-2.31511643129009,1.63320798368394,13.2861490673466));
#25662=CARTESIAN_POINT('Ctrl Pts',(-2.29057274957865,1.63322634504617,13.553361932451));
#25663=CARTESIAN_POINT('Ctrl Pts',(-2.28075528400572,1.62797785312041,13.660259932391));
#25664=CARTESIAN_POINT('Ctrl Pts',(-2.26602905363386,1.60443102075799,13.8190521615535));
#25665=CARTESIAN_POINT('Ctrl Pts',(-2.25498440062962,1.57518246629865,13.9358468917031));
#25666=CARTESIAN_POINT('Ctrl Pts',(-2.24843941314017,1.55366106765359,14.0037857560899));
#25667=CARTESIAN_POINT('Ctrl Pts',(-2.24353067492705,1.53669419003256,14.0544676889874));
#25668=CARTESIAN_POINT('Ctrl Pts',(-2.23984912098126,1.52256174880168,14.0920025777527));
#25669=CARTESIAN_POINT('Ctrl Pts',(-2.21448730515743,1.41694703492178,14.3471327348479));
#25670=CARTESIAN_POINT('Ctrl Pts',(-2.17030865839431,1.13314767767377,14.7501030896063));
#25671=CARTESIAN_POINT('Ctrl Pts',(-2.10404068838079,0.48985529256926,15.1145875274289));
#25672=CARTESIAN_POINT('Ctrl Pts',(-2.03777271837396,-0.247486882538813,
15.1690540813149));
#25673=CARTESIAN_POINT('Ctrl Pts',(-1.97395911763629,-0.911798832807848,
14.9127364048317));
#25674=CARTESIAN_POINT('Ctrl Pts',(-1.91259988616224,-1.39310996057585,
14.4310578285023));
#25675=CARTESIAN_POINT('Ctrl Pts',(-1.84878628545668,-1.66479795157223,
13.7766219771277));
#25676=CARTESIAN_POINT('Ctrl Pts',(-1.78988142317389,-1.63248593599747,
13.1166990702497));
#25677=CARTESIAN_POINT('Ctrl Pts',(-1.74324840727158,-1.41224995598874,
12.6527853330733));
#25678=CARTESIAN_POINT('Ctrl Pts',(-1.71870471460997,-1.24755228455272,
12.4415496621475));
#25679=CARTESIAN_POINT('Ctrl Pts',(-1.70888723755622,-1.17378817419318,
12.3641095389944));
#25680=CARTESIAN_POINT('Ctrl Pts',(-1.70152412968286,-1.11711290300786,
12.30741090743));
#25681=CARTESIAN_POINT('Ctrl Pts',(-1.68679791418894,-0.998163120888784,
12.1996368857678));
#25682=CARTESIAN_POINT('Ctrl Pts',(-1.6524367445998,-0.685665906795594,
11.9905518057572));
#25683=CARTESIAN_POINT('Ctrl Pts',(-1.60334935950164,-0.164421556499146,
11.8323643050256));
#25684=CARTESIAN_POINT('Ctrl Pts',(-1.53953575865813,0.540747957468112,
11.901617685449));
#25685=CARTESIAN_POINT('Ctrl Pts',(-1.49535711192252,0.965883684423983,
12.1560379983072));
#25686=CARTESIAN_POINT('Ctrl Pts',(-1.4536328344594,1.28717780938966,12.4773646847382));
#25687=CARTESIAN_POINT('Ctrl Pts',(-1.41927166486658,1.50525376566623,12.7876189220491));
#25688=CARTESIAN_POINT('Ctrl Pts',(-1.35545806402325,1.69493846692438,13.4676051398953));
#25689=CARTESIAN_POINT('Ctrl Pts',(-1.29164446321183,1.55357584047738,14.1783939299935));
#25690=CARTESIAN_POINT('Ctrl Pts',(-1.22783086237105,1.11817335073225,14.734117053682));
#25691=CARTESIAN_POINT('Ctrl Pts',(-1.19346969277715,0.797965353074917,
14.9372224500198));
#25692=CARTESIAN_POINT('Ctrl Pts',(-1.14683667684874,0.328840193056562,
15.1320794625458));
#25693=CARTESIAN_POINT('Ctrl Pts',(-1.10265803009968,-0.170461188953638,
15.1805232343716));
#25694=CARTESIAN_POINT('Ctrl Pts',(-1.04375316786571,-0.781072783835267,
14.9610508385942));
#25695=CARTESIAN_POINT('Ctrl Pts',(-1.01430073671879,-1.04140710776821,
14.7683279748065));
#25696=CARTESIAN_POINT('Ctrl Pts',(-0.979939567130956,-1.30597646868345,
14.5036867373158));
#25697=CARTESIAN_POINT('Ctrl Pts',(-0.960304613064202,-1.4270605691062,
14.3226287109822));
#25698=CARTESIAN_POINT('Ctrl Pts',(-0.935760920374095,-1.52930100872486,
14.0756739209351));
#25699=CARTESIAN_POINT('Ctrl Pts',(-0.928397812551484,-1.55636742199646,
14.0001138510484));
#25700=CARTESIAN_POINT('Ctrl Pts',(-0.913671597093866,-1.59911265933892,
13.8455369235439));
#25701=CARTESIAN_POINT('Ctrl Pts',(-0.88421916601447,-1.65431209129421,
13.5287124742323));
#25702=CARTESIAN_POINT('Ctrl Pts',(-0.847403627128462,-1.61421626509089,
13.1221241103553));
#25703=CARTESIAN_POINT('Ctrl Pts',(-0.808133718938854,-1.44962467809318,
12.7251977888485));
#25704=CARTESIAN_POINT('Ctrl Pts',(-0.78359002629623,-1.30052263608422,
12.5019186100426));
#25705=CARTESIAN_POINT('Ctrl Pts',(-0.76886381077922,-1.19269127101649,
12.3829668682071));
#25706=CARTESIAN_POINT('Ctrl Pts',(-0.754137595149626,-1.07932525044337,
12.2696043978058));
#25707=CARTESIAN_POINT('Ctrl Pts',(-0.734502641072207,-0.913282101181525,
12.1332231457686));
#25708=CARTESIAN_POINT('Ctrl Pts',(-0.714867686988017,-0.723821617740119,
12.0320856016891));
#25709=CARTESIAN_POINT('Ctrl Pts',(-0.675597778820173,-0.32887384745749,
11.8678982144759));
#25710=CARTESIAN_POINT('Ctrl Pts',(-0.628964762829318,0.19826785403632,
11.8168787027133));
#25711=CARTESIAN_POINT('Ctrl Pts',(-0.565151162002638,0.856314278625342,
12.0715613404292));
#25712=CARTESIAN_POINT('Ctrl Pts',(-0.516063776796385,1.2669674670857,12.4254554520173));
#25713=CARTESIAN_POINT('Ctrl Pts',(-0.484156976433268,1.44749830932253,
12.7268633891509));
#25714=CARTESIAN_POINT('Ctrl Pts',(-0.454704545415558,1.57023839812038,
13.0230879375965));
#25715=CARTESIAN_POINT('Ctrl Pts',(-0.430160852743294,1.63585223537756,
13.285143483846));
#25716=CARTESIAN_POINT('Ctrl Pts',(-0.400708421628965,1.63580953116395,
13.6073742665564));
#25717=CARTESIAN_POINT('Ctrl Pts',(-0.376164728954184,1.59657052806564,
13.8720348170695));
#25718=CARTESIAN_POINT('Ctrl Pts',(-0.361438513458364,1.54982470601694,
14.026220050662));
#25719=CARTESIAN_POINT('Ctrl Pts',(-0.349166667134025,1.49869362646351,
14.1496661593144));
#25720=CARTESIAN_POINT('Ctrl Pts',(-0.344257928557389,1.4770370638121,14.1985479979232));
#25721=CARTESIAN_POINT('Ctrl Pts',(-0.334440451474348,1.42895428828331,
14.2940474291423));
#25722=CARTESIAN_POINT('Ctrl Pts',(-0.317259866709618,1.332717968861,14.4547305965666));
#25723=CARTESIAN_POINT('Ctrl Pts',(-0.302533651204796,1.23046378536219,
14.5792352145037));
#25724=CARTESIAN_POINT('Ctrl Pts',(-0.26571811232627,0.947273180307621,
14.86293984835));
#25725=CARTESIAN_POINT('Ctrl Pts',(-0.211721988644085,0.416651601106899,
15.1631715574816));
#25726=CARTESIAN_POINT('Ctrl Pts',(-0.128273433716417,-0.525303820823094,
15.1403331888213));
#25727=CARTESIAN_POINT('Ctrl Pts',(-0.0374617710681013,-1.38485327505203,
14.5670907032476));
#25728=CARTESIAN_POINT('Ctrl Pts',(0.0263518297750454,-1.63379435128198,
13.8742842613791));
#25729=CARTESIAN_POINT('Ctrl Pts',(0.0950741689632889,-1.63382972703326,
13.1258710146013));
#25730=CARTESIAN_POINT('Ctrl Pts',(0.158887769808821,-1.38495508123797,
12.4330413982481));
#25731=CARTESIAN_POINT('Ctrl Pts',(0.249699432452321,-0.52545935207591,
11.8597170827633));
#25732=CARTESIAN_POINT('Ctrl Pts',(0.333147987387138,0.416491690732399,
11.8367914807877));
#25733=CARTESIAN_POINT('Ctrl Pts',(0.387144111066703,0.947143527898697,
12.1369717461611));
#25734=CARTESIAN_POINT('Ctrl Pts',(0.423959649936313,1.23035674071828,12.4206532587168));
#25735=CARTESIAN_POINT('Ctrl Pts',(0.436231496205733,1.31559067564619,12.5243893912344));
#25736=CARTESIAN_POINT('Ctrl Pts',(0.450957711741397,1.4013704881953,12.6599178389611));
#25737=CARTESIAN_POINT('Ctrl Pts',(0.4607751887345,1.45409117498363,12.7529378493789));
#25738=CARTESIAN_POINT('Ctrl Pts',(0.468138296558858,1.48840440040474,12.8255047097806));
#25739=CARTESIAN_POINT('Ctrl Pts',(0.477955773727791,1.52931520386143,12.9242574281315));
#25740=CARTESIAN_POINT('Ctrl Pts',(0.492681989231907,1.58341885399309,13.0754019220946));
#25741=CARTESIAN_POINT('Ctrl Pts',(0.51722568191251,1.6358025154813,13.3387617413545));
#25742=CARTESIAN_POINT('Ctrl Pts',(0.551586851479718,1.6358622587284,13.7147015657294));
#25743=CARTESIAN_POINT('Ctrl Pts',(0.576130544154049,1.57028636551549,13.9767616281306));
#25744=CARTESIAN_POINT('Ctrl Pts',(0.605582975172473,1.44757211442134,14.272998526345));
#25745=CARTESIAN_POINT('Ctrl Pts',(0.637489775533693,1.26707042745046,14.5744235528787));
#25746=CARTESIAN_POINT('Ctrl Pts',(0.686577160741821,0.856450056310684,
14.9283569884486));
#25747=CARTESIAN_POINT('Ctrl Pts',(0.750390761567867,0.198427790429692,
15.1831021639917));
#25748=CARTESIAN_POINT('Ctrl Pts',(0.797023777559325,-0.328719012736018,
15.1321327619175));
#25749=CARTESIAN_POINT('Ctrl Pts',(0.83629368572729,-0.723682311592208,
14.9679828445898));
#25750=CARTESIAN_POINT('Ctrl Pts',(0.85592863981007,-0.913152446732621,
14.8668632900606));
#25751=CARTESIAN_POINT('Ctrl Pts',(0.875563593888921,-1.07920850799294,
14.7304977869275));
#25752=CARTESIAN_POINT('Ctrl Pts',(0.890289809517802,-1.19258529192622,
14.6171460730064));
#25753=CARTESIAN_POINT('Ctrl Pts',(0.905016025034186,-1.30042793054723,
14.4982045532945));
#25754=CARTESIAN_POINT('Ctrl Pts',(0.929559717682546,-1.44955115512858,
14.2749395277779));
#25755=CARTESIAN_POINT('Ctrl Pts',(0.968829625859914,-1.61418037039209,
13.8780288156127));
#25756=CARTESIAN_POINT('Ctrl Pts',(1.00564516475731,-1.65431477124166,13.4714442854307));
#25757=CARTESIAN_POINT('Ctrl Pts',(1.03509759583151,-1.59914537217458,13.1546146181273));
#25758=CARTESIAN_POINT('Ctrl Pts',(1.04982381129091,-1.55641478567852,13.0000336344831));
#25759=CARTESIAN_POINT('Ctrl Pts',(1.0571869191131,-1.52935553879155,12.9244710046119));
#25760=CARTESIAN_POINT('Ctrl Pts',(1.08173061180252,-1.42713848945209,12.6775065180917));
#25761=CARTESIAN_POINT('Ctrl Pts',(1.10136556586942,-1.30607158736917,12.4964370303868));
#25762=CARTESIAN_POINT('Ctrl Pts',(1.13572673545794,-1.04152729433169,12.2317707234624));
#25763=CARTESIAN_POINT('Ctrl Pts',(1.16517916660448,-0.781211253495427,
12.0390231851748));
#25764=CARTESIAN_POINT('Ctrl Pts',(1.22408402883849,-0.170620462432981,
11.8194929249613));
#25765=CARTESIAN_POINT('Ctrl Pts',(1.26826267558795,0.328685516234155,11.8678893662407));
#25766=CARTESIAN_POINT('Ctrl Pts',(1.31489569151535,0.79782912167651,12.0627019246719));
#25767=CARTESIAN_POINT('Ctrl Pts',(1.34925686111136,1.11805638087561,12.2657769596875));
#25768=CARTESIAN_POINT('Ctrl Pts',(1.41307046195049,1.55351153230628,12.8214588224151));
#25769=CARTESIAN_POINT('Ctrl Pts',(1.47688406276225,1.69494153596926,13.532234210352));
#25770=CARTESIAN_POINT('Ctrl Pts',(1.54069766360644,1.50532127692099,14.2122383972142));
#25771=CARTESIAN_POINT('Ctrl Pts',(1.5750588332008,1.28727474124243,14.5225133116529));
#25772=CARTESIAN_POINT('Ctrl Pts',(1.61678311066043,0.966011054182616,14.8438704467015));
#25773=CARTESIAN_POINT('Ctrl Pts',(1.66096175739847,0.540899461717136,15.0983310548197));
#25774=CARTESIAN_POINT('Ctrl Pts',(1.72477535823702,-0.164263490526999,
15.1676512711812));
#25775=CARTESIAN_POINT('Ctrl Pts',(1.77386274333832,-0.685522828652171,
15.0095131764614));
#25776=CARTESIAN_POINT('Ctrl Pts',(1.80822391292843,-0.998039852607216,
14.8004577179364));
#25777=CARTESIAN_POINT('Ctrl Pts',(1.82295012842216,-1.11699985285216,14.6926949691893));
#25778=CARTESIAN_POINT('Ctrl Pts',(1.83031323629589,-1.17368049582136,14.6360017121857));
#25779=CARTESIAN_POINT('Ctrl Pts',(1.84013071334923,-1.24745194660516,14.5585685740192));
#25780=CARTESIAN_POINT('Ctrl Pts',(1.86467440601124,-1.41216963612087,14.3473485268086));
#25781=CARTESIAN_POINT('Ctrl Pts',(1.91130742191433,-1.63244957724005,13.8834556582109));
#25782=CARTESIAN_POINT('Ctrl Pts',(1.97021228419637,-1.66482413385211,13.2235358241412));
#25783=CARTESIAN_POINT('Ctrl Pts',(2.03402588490596,-1.39319814356631,12.5690742212523));
#25784=CARTESIAN_POINT('Ctrl Pts',(2.09538511638032,-0.911932631418002,
12.0873500335917));
#25785=CARTESIAN_POINT('Ctrl Pts',(2.15919871712108,-0.247644919118781,
11.8309693962473));
#25786=CARTESIAN_POINT('Ctrl Pts',(2.2254666871376,0.489702547485788,11.8853660789399));
#25787=CARTESIAN_POINT('Ctrl Pts',(2.29173465714865,1.13302959529792,12.2497895468869));
#25788=CARTESIAN_POINT('Ctrl Pts',(2.33591330392835,1.41686742328557,12.6527330373133));
#25789=CARTESIAN_POINT('Ctrl Pts',(2.36127511975716,1.52250637166547,12.9078531761878));
#25790=CARTESIAN_POINT('Ctrl Pts',(2.36495667370317,1.53664238670787,12.9453867337541));
#25791=CARTESIAN_POINT('Ctrl Pts',(2.36986541191653,1.5536140512705,12.9960670500936));
#25792=CARTESIAN_POINT('Ctrl Pts',(2.37641039940547,1.57514194868161,13.0640038860603));
#25793=CARTESIAN_POINT('Ctrl Pts',(2.38745505241297,1.60440147660552,13.1807958197083));
#25794=CARTESIAN_POINT('Ctrl Pts',(2.40218128278599,1.62796365750789,13.3395858727675));
#25795=CARTESIAN_POINT('Ctrl Pts',(2.41199874836342,1.63322205640795,13.4464832900758));
#25796=CARTESIAN_POINT('Ctrl Pts',(2.43654243007502,1.63322976252623,13.7136965402967));
#25797=CARTESIAN_POINT('Ctrl Pts',(2.45617743206558,1.59079533728359,13.9274562422369));
#25798=CARTESIAN_POINT('Ctrl Pts',(2.4782667196338,1.49871212944699,14.1496275339613));
#25799=CARTESIAN_POINT('Ctrl Pts',(2.5028103600564,1.39052109086099,14.3941006888739));
#25800=CARTESIAN_POINT('Ctrl Pts',(2.54698916595512,1.08724369463858,14.7824338036398));
#25801=CARTESIAN_POINT('Ctrl Pts',(2.61080254255296,0.462464018280852,15.1165555131629));
#25802=CARTESIAN_POINT('Ctrl Pts',(2.67461634115977,-0.247393003196471,
15.1690039491515));
#25803=CARTESIAN_POINT('Ctrl Pts',(2.74333874625233,-0.963000910327539,
14.8932808228982));
#25804=CARTESIAN_POINT('Ctrl Pts',(2.80960599038935,-1.46231188778867,14.3423162383898));
#25805=CARTESIAN_POINT('Ctrl Pts',(2.87342139427634,-1.66731758164261,13.6644668612195));
#25806=CARTESIAN_POINT('Ctrl Pts',(2.9421397828027,-1.59347520441855,12.9048899504509));
#25807=CARTESIAN_POINT('Ctrl Pts',(2.99543686361548,-1.25774848826549,12.4010519912542));
#25808=CARTESIAN_POINT('Ctrl Pts',(3.02908986191469,-0.964147003153576,
12.1810042236116));
#25809=CARTESIAN_POINT('Ctrl Pts',(3.03329287307245,-0.92648238051196,12.1550256572553));
#25810=CARTESIAN_POINT('Ctrl Pts',(-3.08759528491809,0.0023500709696575,
15.3669112794954));
#25811=CARTESIAN_POINT('Ctrl Pts',(-3.070364778818,-0.212646371255907,15.3671449067253));
#25812=CARTESIAN_POINT('Ctrl Pts',(-3.03594205588516,-0.640224871273036,
15.2930636162465));
#25813=CARTESIAN_POINT('Ctrl Pts',(-2.97203928859788,-1.34405177464685,
14.8959035131867));
#25814=CARTESIAN_POINT('Ctrl Pts',(-2.90579059611891,-1.82179168220255,
14.180783442706));
#25815=CARTESIAN_POINT('Ctrl Pts',(-2.8370582186335,-1.90595073708206,13.3119961697794));
#25816=CARTESIAN_POINT('Ctrl Pts',(-2.77324913208513,-1.67174130404843,
12.5373404820452));
#25817=CARTESIAN_POINT('Ctrl Pts',(-2.70697934869721,-1.1009493781795,11.9073944503979));
#25818=CARTESIAN_POINT('Ctrl Pts',(-2.63825717411256,-0.282964643060395,
11.5921720805156));
#25819=CARTESIAN_POINT('Ctrl Pts',(-2.57444406802585,0.528477611992774,
11.6520800065705));
#25820=CARTESIAN_POINT('Ctrl Pts',(-2.51062990712246,1.24274101975633,12.0339183867967));
#25821=CARTESIAN_POINT('Ctrl Pts',(-2.46645165807834,1.58936201945163,12.4778870234411));
#25822=CARTESIAN_POINT('Ctrl Pts',(-2.44190783487501,1.71315248791266,12.7572594832551));
#25823=CARTESIAN_POINT('Ctrl Pts',(-2.41981842205487,1.8183263300599,13.0112815736336));
#25824=CARTESIAN_POINT('Ctrl Pts',(-2.40018358765284,1.86696052951785,13.255540997676));
#25825=CARTESIAN_POINT('Ctrl Pts',(-2.37563986763414,1.86695758479274,13.5610368182778));
#25826=CARTESIAN_POINT('Ctrl Pts',(-2.36582236194615,1.86095970736867,13.6832217734386));
#25827=CARTESIAN_POINT('Ctrl Pts',(-2.35109618359108,1.8340383937764,13.8647453356404));
#25828=CARTESIAN_POINT('Ctrl Pts',(-2.34005150062928,1.80060082651263,13.9982489249835));
#25829=CARTESIAN_POINT('Ctrl Pts',(-2.33350652305318,1.77600090529121,14.0759124271069));
#25830=CARTESIAN_POINT('Ctrl Pts',(-2.32859778355624,1.75659799293553,14.1338445204053));
#25831=CARTESIAN_POINT('Ctrl Pts',(-2.32491622964828,1.74045665369918,14.1767545198982));
#25832=CARTESIAN_POINT('Ctrl Pts',(-2.29955441405339,1.61964487367634,14.4683693759585));
#25833=CARTESIAN_POINT('Ctrl Pts',(-2.25537576737961,1.29530781396324,14.929025377181));
#25834=CARTESIAN_POINT('Ctrl Pts',(-2.18910779718202,0.559905905457109,
15.3456504769967));
#25835=CARTESIAN_POINT('Ctrl Pts',(-2.12283982719947,-0.282930359999273,
15.4078999941006));
#25836=CARTESIAN_POINT('Ctrl Pts',(-2.05902622653861,-1.04231549003814,
15.1148878618827));
#25837=CARTESIAN_POINT('Ctrl Pts',(-1.99766699502949,-1.59247938955606,
14.564272017216));
#25838=CARTESIAN_POINT('Ctrl Pts',(-1.93385339428798,-1.90307453898268,
13.8161699129123));
#25839=CARTESIAN_POINT('Ctrl Pts',(-1.87494853210476,-1.86608125873476,
13.0618174246178));
#25840=CARTESIAN_POINT('Ctrl Pts',(-1.82831551613341,-1.61438776389863,
12.5315095874762));
#25841=CARTESIAN_POINT('Ctrl Pts',(-1.80377182346193,-1.42602447023497,
12.2900559477824));
#25842=CARTESIAN_POINT('Ctrl Pts',(-1.79395434644624,-1.34175398647389,
12.201528824612));
#25843=CARTESIAN_POINT('Ctrl Pts',(-1.78659123858441,-1.27694850031384,
12.1367313966333));
#25844=CARTESIAN_POINT('Ctrl Pts',(-1.77186502305241,-1.14098738956333,
12.013506241682));
#25845=CARTESIAN_POINT('Ctrl Pts',(-1.7375038534634,-0.783756830443404,
11.7745426475921));
#25846=CARTESIAN_POINT('Ctrl Pts',(-1.68841646838521,-0.187913082298619,
11.5937304847702));
#25847=CARTESIAN_POINT('Ctrl Pts',(-1.62460286756024,0.61815658478922,11.6728608723269));
#25848=CARTESIAN_POINT('Ctrl Pts',(-1.58042422078084,1.10413623186327,11.9638185378979));
#25849=CARTESIAN_POINT('Ctrl Pts',(-1.53869994331994,1.47138001066433,12.3309861788527));
#25850=CARTESIAN_POINT('Ctrl Pts',(-1.50433877374192,1.72072186236973,12.6857382584471));
#25851=CARTESIAN_POINT('Ctrl Pts',(-1.44052517292936,1.93748562326409,13.4629729665557));
#25852=CARTESIAN_POINT('Ctrl Pts',(-1.37671157203573,1.77587122939508,14.2755365403217));
#25853=CARTESIAN_POINT('Ctrl Pts',(-1.31289797121347,1.27821103918419,14.910720784742));
#25854=CARTESIAN_POINT('Ctrl Pts',(-1.27853680163774,0.912087345431337,
15.1429840770779));
#25855=CARTESIAN_POINT('Ctrl Pts',(-1.23190378572754,0.37589996465958,15.3655639266512));
#25856=CARTESIAN_POINT('Ctrl Pts',(-1.18772513897687,-0.194914574603933,
15.4210130110031));
#25857=CARTESIAN_POINT('Ctrl Pts',(-1.12882027666981,-0.892860720439233,
15.1701471113649));
#25858=CARTESIAN_POINT('Ctrl Pts',(-1.09936784558967,-1.19047435017082,
14.9497506527899));
#25859=CARTESIAN_POINT('Ctrl Pts',(-1.06500667599683,-1.49288243745837,
14.6473828402657));
#25860=CARTESIAN_POINT('Ctrl Pts',(-1.04537172186518,-1.63124495617839,
14.440195073271));
#25861=CARTESIAN_POINT('Ctrl Pts',(-1.02082802926375,-1.74818285448208,
14.1580460636463));
#25862=CARTESIAN_POINT('Ctrl Pts',(-1.01346492148097,-1.77908694402207,
14.0716427230622));
#25863=CARTESIAN_POINT('Ctrl Pts',(-0.998738705857055,-1.82799370925915,
13.8949520830598));
#25864=CARTESIAN_POINT('Ctrl Pts',(-0.969286275024268,-1.89101395941206,
13.5327858149411));
#25865=CARTESIAN_POINT('Ctrl Pts',(-0.932470735954739,-1.84521085036033,
13.0680056680855));
#25866=CARTESIAN_POINT('Ctrl Pts',(-0.89320082783347,-1.65706813257767,
12.6142812638122));
#25867=CARTESIAN_POINT('Ctrl Pts',(-0.868657135111634,-1.48660805742424,
12.3590420738917));
#25868=CARTESIAN_POINT('Ctrl Pts',(-0.853930919637501,-1.36335663025442,
12.2230840215225));
#25869=CARTESIAN_POINT('Ctrl Pts',(-0.839204704031034,-1.23376026936314,
12.0934568578651));
#25870=CARTESIAN_POINT('Ctrl Pts',(-0.8195697499311,-1.04394701268137,11.9376775261929));
#25871=CARTESIAN_POINT('Ctrl Pts',(-0.7999347958418,-0.827386737992478,
11.8219078046918));
#25872=CARTESIAN_POINT('Ctrl Pts',(-0.760664887668704,-0.375884998960593,
11.6344876086694));
#25873=CARTESIAN_POINT('Ctrl Pts',(-0.714031871708202,0.226667196248288,
11.5759533828502));
#25874=CARTESIAN_POINT('Ctrl Pts',(-0.65021827085275,0.97889333543878,11.8671971878041));
#25875=CARTESIAN_POINT('Ctrl Pts',(-0.601130885626391,1.44829992606202,
12.2717276845478));
#25876=CARTESIAN_POINT('Ctrl Pts',(-0.569224085280087,1.65466780097147,
12.6162485693903));
#25877=CARTESIAN_POINT('Ctrl Pts',(-0.53977165428826,1.79495718711597,12.9548992928255));
#25878=CARTESIAN_POINT('Ctrl Pts',(-0.515227961643534,1.86996301017078,
13.2544352024425));
#25879=CARTESIAN_POINT('Ctrl Pts',(-0.485775530482349,1.86990635043761,
13.6227923522052));
#25880=CARTESIAN_POINT('Ctrl Pts',(-0.461231837841324,1.82504811787028,
13.9253227089901));
#25881=CARTESIAN_POINT('Ctrl Pts',(-0.446505622315567,1.77160362358178,
14.1015741272446));
#25882=CARTESIAN_POINT('Ctrl Pts',(-0.434233775961515,1.71316198986504,
14.2426890400414));
#25883=CARTESIAN_POINT('Ctrl Pts',(-0.429325037372163,1.68839398250032,
14.2985571130423));
#25884=CARTESIAN_POINT('Ctrl Pts',(-0.419507560431212,1.6334513413436,14.4077416262965));
#25885=CARTESIAN_POINT('Ctrl Pts',(-0.40232697556216,1.52339204904435,14.5913779147532));
#25886=CARTESIAN_POINT('Ctrl Pts',(-0.387600760055443,1.40657398765396,
14.7337625495905));
#25887=CARTESIAN_POINT('Ctrl Pts',(-0.350785221174236,1.08273851420154,
15.0579597690902));
#25888=CARTESIAN_POINT('Ctrl Pts',(-0.296789097516509,0.476285039428357,
15.4012909875185));
#25889=CARTESIAN_POINT('Ctrl Pts',(-0.213340542615734,-0.600556246952718,
15.3749620338903));
#25890=CARTESIAN_POINT('Ctrl Pts',(-0.122528879886235,-1.58304430910793,
14.7197956084861));
#25891=CARTESIAN_POINT('Ctrl Pts',(-0.0587152790700956,-1.8675942981973,
13.927777469134));
#25892=CARTESIAN_POINT('Ctrl Pts',(0.0100070600863068,-1.86761983033918,
13.0723336751479));
#25893=CARTESIAN_POINT('Ctrl Pts',(0.0738206608959717,-1.58311665986085,
12.2802987218011));
#25894=CARTESIAN_POINT('Ctrl Pts',(0.164632323640247,-0.600668197270314,
11.6250749647134));
#25895=CARTESIAN_POINT('Ctrl Pts',(0.248080878521423,0.476171360890716,
11.5986828860266));
#25896=CARTESIAN_POINT('Ctrl Pts',(0.302077002185279,1.08264277791298,11.9419808031196));
#25897=CARTESIAN_POINT('Ctrl Pts',(0.338892541089085,1.40649893417158,12.266157604826));
#25898=CARTESIAN_POINT('Ctrl Pts',(0.351164387374828,1.50384840958494,12.3848125514054));
#25899=CARTESIAN_POINT('Ctrl Pts',(0.365890602801437,1.60195104912399,12.5396951787418));
#25900=CARTESIAN_POINT('Ctrl Pts',(0.375708079966948,1.66219089380516,12.6460487393483));
#25901=CARTESIAN_POINT('Ctrl Pts',(0.383071187745898,1.70142775366068,12.7289881483073));
#25902=CARTESIAN_POINT('Ctrl Pts',(0.392888664884959,1.74818788890808,12.8418781801734));
#25903=CARTESIAN_POINT('Ctrl Pts',(0.407614880391224,1.81002885866779,13.0146550273087));
#25904=CARTESIAN_POINT('Ctrl Pts',(0.432158573017531,1.86990438259484,13.3157009880243));
#25905=CARTESIAN_POINT('Ctrl Pts',(0.466519742664319,1.8699655452867,13.7454525475317));
#25906=CARTESIAN_POINT('Ctrl Pts',(0.491063435304432,1.79499221766936,14.0449929131399));
#25907=CARTESIAN_POINT('Ctrl Pts',(0.520515866293551,1.65472151719971,14.3836519320234));
#25908=CARTESIAN_POINT('Ctrl Pts',(0.552422666642926,1.44837375641488,14.7281855842315));
#25909=CARTESIAN_POINT('Ctrl Pts',(0.60151005186875,0.978990666418381,15.1327440801011));
#25910=CARTESIAN_POINT('Ctrl Pts',(0.665323652724684,0.226781365827923,
15.4240327960859));
#25911=CARTESIAN_POINT('Ctrl Pts',(0.71195666868146,-0.375774382679836,
15.3655342908919));
#25912=CARTESIAN_POINT('Ctrl Pts',(0.751226576855593,-0.827287339935277,
15.1781408845209));
#25913=CARTESIAN_POINT('Ctrl Pts',(0.770861530946073,-1.0438544481067,15.0623839856104));
#25914=CARTESIAN_POINT('Ctrl Pts',(0.790496485045808,-1.23367697134313,
14.9066159119171));
#25915=CARTESIAN_POINT('Ctrl Pts',(0.805222700653011,-1.36328099370934,
14.776996415965));
#25916=CARTESIAN_POINT('Ctrl Pts',(0.819948916128669,-1.48654046797679,
14.6410456587964));
#25917=CARTESIAN_POINT('Ctrl Pts',(0.844492608835747,-1.65701565369615,
14.3858165693403));
#25918=CARTESIAN_POINT('Ctrl Pts',(0.883762516987446,-1.84518520703327,
13.932103302506));
#25919=CARTESIAN_POINT('Ctrl Pts',(0.920578056028856,-1.89101584313679,
13.4673259234246));
#25920=CARTESIAN_POINT('Ctrl Pts',(0.950030486875574,-1.82801700727461,
13.1051559267996));
#25921=CARTESIAN_POINT('Ctrl Pts',(0.964756702494275,-1.77912068879012,
12.9284624028924));
#25922=CARTESIAN_POINT('Ctrl Pts',(0.972119810278298,-1.74822170447994,
12.8420572325272));
#25923=CARTESIAN_POINT('Ctrl Pts',(0.996663502882085,-1.63130050620839,
12.5599013225452));
#25924=CARTESIAN_POINT('Ctrl Pts',(1.01629845701254,-1.49295022231228,12.352705383945));
#25925=CARTESIAN_POINT('Ctrl Pts',(1.05065962660513,-1.19056003230052,12.050319698693));
#25926=CARTESIAN_POINT('Ctrl Pts',(1.08011205768541,-0.892959426854112,
11.8299056561741));
#25927=CARTESIAN_POINT('Ctrl Pts',(1.13901691999234,-0.195028119944808,
11.5789984993715));
#25928=CARTESIAN_POINT('Ctrl Pts',(1.18319556674322,0.375789682526766,11.634413850994));
#25929=CARTESIAN_POINT('Ctrl Pts',(1.22982858265304,0.911990235958854,11.856961997154));
#25930=CARTESIAN_POINT('Ctrl Pts',(1.26418975222758,1.27812764581854,12.0892036582747));
#25931=CARTESIAN_POINT('Ctrl Pts',(1.3280033530514,1.77582538844162,12.7243584776999));
#25932=CARTESIAN_POINT('Ctrl Pts',(1.39181695394423,1.93748780829106,13.5369124982985));
#25933=CARTESIAN_POINT('Ctrl Pts',(1.45563055475692,1.72077000069959,14.3141600253852));
#25934=CARTESIAN_POINT('Ctrl Pts',(1.48999172433415,1.47144910986013,14.6689268368013));
#25935=CARTESIAN_POINT('Ctrl Pts',(1.53171600179601,1.10422705446681,15.0361161891462));
#25936=CARTESIAN_POINT('Ctrl Pts',(1.57589464857577,0.618264596492589,15.3271025815264));
#25937=CARTESIAN_POINT('Ctrl Pts',(1.6397082494017,-0.187800383852184,15.4062806204875));
#25938=CARTESIAN_POINT('Ctrl Pts',(1.68879563447951,-0.78365481480013,15.2255036805631));
#25939=CARTESIAN_POINT('Ctrl Pts',(1.72315680406778,-1.14089950151332,14.9865612032227));
#25940=CARTESIAN_POINT('Ctrl Pts',(1.73788301959999,-1.27686789199295,14.8633440871825));
#25941=CARTESIAN_POINT('Ctrl Pts',(1.74524612746181,-1.34167720988981,14.7985504880953));
#25942=CARTESIAN_POINT('Ctrl Pts',(1.75506360447765,-1.4259529256506,14.7100283526174));
#25943=CARTESIAN_POINT('Ctrl Pts',(1.77960729714949,-1.6143304908496,14.4685858375326));
#25944=CARTESIAN_POINT('Ctrl Pts',(1.82624031312,-1.86605531676253,13.9382928885807));
#25945=CARTESIAN_POINT('Ctrl Pts',(1.8851451753049,-1.90309317982369,13.1839425839232));
#25946=CARTESIAN_POINT('Ctrl Pts',(1.94895877604335,-1.5925422036829,12.4358221265291));
#25947=CARTESIAN_POINT('Ctrl Pts',(2.01031800755653,-1.04241078847366,11.8851737608717));
#25948=CARTESIAN_POINT('Ctrl Pts',(2.07413160821739,-0.283042883570731,
11.5921167431507));
#25949=CARTESIAN_POINT('Ctrl Pts',(2.14039957820167,0.559797274712904,11.6543164405991));
#25950=CARTESIAN_POINT('Ctrl Pts',(2.20666754840405,1.29522400889582,12.0708980789732));
#25951=CARTESIAN_POINT('Ctrl Pts',(2.25084619508075,1.6195887412875,12.5315349098769));
#25952=CARTESIAN_POINT('Ctrl Pts',(2.27620801067512,1.74041786042992,12.8231426370461));
#25953=CARTESIAN_POINT('Ctrl Pts',(2.27988956458325,1.75656173412752,12.8660516752081));
#25954=CARTESIAN_POINT('Ctrl Pts',(2.28479830407995,1.77596808494156,12.9239826309265));
#25955=CARTESIAN_POINT('Ctrl Pts',(2.29134328165695,1.80057259257038,13.0016446570642));
#25956=CARTESIAN_POINT('Ctrl Pts',(2.30238796461873,1.8340181463693,13.1351463223963));
#25957=CARTESIAN_POINT('Ctrl Pts',(2.31711414297562,1.8609502466527,13.3166682127696));
#25958=CARTESIAN_POINT('Ctrl Pts',(2.32693164866254,1.86695551980756,13.4388529249682));
#25959=CARTESIAN_POINT('Ctrl Pts',(2.35147536869532,1.8669761579952,13.7443483740352));
#25960=CARTESIAN_POINT('Ctrl Pts',(2.37111020309486,1.81835939666339,13.9886114325472));
#25961=CARTESIAN_POINT('Ctrl Pts',(2.3931996159295,1.71319995454039,14.2426393076694));
#25962=CARTESIAN_POINT('Ctrl Pts',(2.41774343911922,1.58942689168338,14.5220193282036));
#25963=CARTESIAN_POINT('Ctrl Pts',(2.46192168824902,1.24283702002585,14.9660103282504));
#25964=CARTESIAN_POINT('Ctrl Pts',(2.52573584912865,0.528597455391128,15.3478865186278));
#25965=CARTESIAN_POINT('Ctrl Pts',(2.58954895542082,-0.282823439666157,
15.407853412087));
#25966=CARTESIAN_POINT('Ctrl Pts',(2.65827112993319,-1.10083352415133,15.0926576029327));
#25967=CARTESIAN_POINT('Ctrl Pts',(2.7245409139849,-1.67158419892642,14.4627976259999));
#25968=CARTESIAN_POINT('Ctrl Pts',(2.78835000017331,-1.90590776116979,13.6880601642426));
#25969=CARTESIAN_POINT('Ctrl Pts',(2.85708237956506,-1.821479964611,12.8195313357051));
#25970=CARTESIAN_POINT('Ctrl Pts',(2.91035772328115,-1.4376982387087,12.2440093096638));
#25971=CARTESIAN_POINT('Ctrl Pts',(2.94402092726701,-1.10215653765364,11.9922029531339));
#25972=CARTESIAN_POINT('Ctrl Pts',(2.94822541613613,-1.05904260584525,11.9625368481551));
#25973=CARTESIAN_POINT('Ctrl Pts',(-3.17266220035259,0.00264184562465942,
15.6006308241626));
#25974=CARTESIAN_POINT('Ctrl Pts',(-3.15544971768883,-0.239046808317434,
15.6009202622642));
#25975=CARTESIAN_POINT('Ctrl Pts',(-3.12102872579492,-0.720158267641467,
15.5176257131219));
#25976=CARTESIAN_POINT('Ctrl Pts',(-3.05708907174061,-1.51248273306104,
15.0705362781659));
#25977=CARTESIAN_POINT('Ctrl Pts',(-2.99086741120179,-2.04980411836316,
14.2660656413471));
#25978=CARTESIAN_POINT('Ctrl Pts',(-2.92212104198698,-2.1445664440175,13.288402600722));
#25979=CARTESIAN_POINT('Ctrl Pts',(-2.8583182735956,-1.88101160882473,12.4168213143143));
#25980=CARTESIAN_POINT('Ctrl Pts',(-2.7920459500128,-1.23875968366752,11.7079913692117));
#25981=CARTESIAN_POINT('Ctrl Pts',(-2.72332400615456,-0.318351097498607,
11.3533357827765));
#25982=CARTESIAN_POINT('Ctrl Pts',(-2.65951159229766,0.594666833883564,
11.420732594117));
#25983=CARTESIAN_POINT('Ctrl Pts',(-2.59569664716482,1.39833550923656,11.8504187872197));
#25984=CARTESIAN_POINT('Ctrl Pts',(-2.55151895485121,1.78838606602427,12.3499173356549));
#25985=CARTESIAN_POINT('Ctrl Pts',(-2.5269749488977,1.92762083664646,12.6643104262796));
#25986=CARTESIAN_POINT('Ctrl Pts',(-2.50488541080207,2.04601496321456,12.9501032916501));
#25987=CARTESIAN_POINT('Ctrl Pts',(-2.48525074400365,2.10067625814384,13.2249852988262));
#25988=CARTESIAN_POINT('Ctrl Pts',(-2.46070698565595,2.10067806416113,13.5687043580597));
#25989=CARTESIAN_POINT('Ctrl Pts',(-2.45088943986216,2.09392530800916,13.7061920430449));
#25990=CARTESIAN_POINT('Ctrl Pts',(-2.43616331352013,2.063631791612,13.9104351957971));
#25991=CARTESIAN_POINT('Ctrl Pts',(-2.42511860060563,2.02600652422355,14.0606546557986));
#25992=CARTESIAN_POINT('Ctrl Pts',(-2.41857363294159,1.99832432702032,14.1480389593073));
#25993=CARTESIAN_POINT('Ctrl Pts',(-2.41366489216172,1.97649509446574,14.2132245903546));
#25994=CARTESIAN_POINT('Ctrl Pts',(-2.40998333829098,1.95832480905997,14.2615042017653));
#25995=CARTESIAN_POINT('Ctrl Pts',(-2.38462152292895,1.82242492077781,14.5896371766628));
#25996=CARTESIAN_POINT('Ctrl Pts',(-2.34044287635804,1.4574325852988,15.1079453504089));
#25997=CARTESIAN_POINT('Ctrl Pts',(-2.2741749059696,0.629981383084626,15.5767198045092));
#25998=CARTESIAN_POINT('Ctrl Pts',(-2.20790693601996,-0.318384334109432,
15.646747379099));
#25999=CARTESIAN_POINT('Ctrl Pts',(-2.14409333543653,-1.17282687254162,
15.317041154053));
#26000=CARTESIAN_POINT('Ctrl Pts',(-2.08273410389093,-1.79186597979423,
14.6974827997507));
#26001=CARTESIAN_POINT('Ctrl Pts',(-2.01892050311859,-2.14131186029559,
13.8557240815807));
#26002=CARTESIAN_POINT('Ctrl Pts',(-1.96001564103395,-2.09969863559914,
13.0069296488875));
#26003=CARTESIAN_POINT('Ctrl Pts',(-1.91338262499469,-1.81645082636161,
12.4102412367691));
#26004=CARTESIAN_POINT('Ctrl Pts',(-1.88883893231528,-1.6045509056256,12.1385586862707));
#26005=CARTESIAN_POINT('Ctrl Pts',(-1.87902145533625,-1.50970215352713,
12.0389534490745));
#26006=CARTESIAN_POINT('Ctrl Pts',(-1.87165834748703,-1.43679234243196,
11.9660376433793));
#26007=CARTESIAN_POINT('Ctrl Pts',(-1.85693213191582,-1.28380123614643,
11.8274039902691));
#26008=CARTESIAN_POINT('Ctrl Pts',(-1.82257096232786,-0.881849651288155,
11.558510752652));
#26009=CARTESIAN_POINT('Ctrl Pts',(-1.77348357727153,-0.21141052754035,
11.3550706699088));
#26010=CARTESIAN_POINT('Ctrl Pts',(-1.70966997646036,0.695576906938657,
11.4441452651285));
#26011=CARTESIAN_POINT('Ctrl Pts',(-1.66549132964107,1.24238709858536,11.771472748311));
#26012=CARTESIAN_POINT('Ctrl Pts',(-1.62376705217685,1.655612733367,12.1846907466758));
#26013=CARTESIAN_POINT('Ctrl Pts',(-1.58940588261669,1.93613052167727,12.5838088251675));
#26014=CARTESIAN_POINT('Ctrl Pts',(-1.52559228183367,2.18004640024346,13.4583839812046));
#26015=CARTESIAN_POINT('Ctrl Pts',(-1.46177868085939,1.99819061811832,14.3726391361564));
#26016=CARTESIAN_POINT('Ctrl Pts',(-1.39796508005353,1.43818525007012,15.0873649788857));
#26017=CARTESIAN_POINT('Ctrl Pts',(-1.36360391049841,1.02626889486372,15.3486477476018));
#26018=CARTESIAN_POINT('Ctrl Pts',(-1.31697089460524,0.422912135353946,
15.599164614062));
#26019=CARTESIAN_POINT('Ctrl Pts',(-1.27279224785391,-0.219332827926,15.6615028656883));
#26020=CARTESIAN_POINT('Ctrl Pts',(-1.2138873854739,-1.00467417934464,15.3792058981596));
#26021=CARTESIAN_POINT('Ctrl Pts',(-1.18443495446031,-1.33952818945933,
15.1312597853418));
#26022=CARTESIAN_POINT('Ctrl Pts',(-1.15007378486252,-1.67979938218662,
14.7909543366238));
#26023=CARTESIAN_POINT('Ctrl Pts',(-1.13043883066505,-1.83550446245088,
14.5579405445852));
#26024=CARTESIAN_POINT('Ctrl Pts',(-1.10589513815342,-1.96703997856123,
14.240389049116));
#26025=CARTESIAN_POINT('Ctrl Pts',(-1.09853203041032,-2.00182960412185,
14.1431839218754));
#26026=CARTESIAN_POINT('Ctrl Pts',(-1.08380581461998,-2.05683123962386,
13.9443682479003));
#26027=CARTESIAN_POINT('Ctrl Pts',(-1.05435338403389,-2.12777334415797,
13.536861775514));
#26028=CARTESIAN_POINT('Ctrl Pts',(-1.0175378447822,-2.0762083485259,13.0139000451585));
#26029=CARTESIAN_POINT('Ctrl Pts',(-0.978267936728251,-1.864499032025,12.5033759025148));
#26030=CARTESIAN_POINT('Ctrl Pts',(-0.953724243927657,-1.67270341789268,
12.2161912935285));
#26031=CARTESIAN_POINT('Ctrl Pts',(-0.93899802849587,-1.5340127312506,12.0632069998174));
#26032=CARTESIAN_POINT('Ctrl Pts',(-0.924271812912939,-1.38819254281156,
11.9173769826473));
#26033=CARTESIAN_POINT('Ctrl Pts',(-0.904636858791085,-1.17461691688123,
11.7420376710293));
#26034=CARTESIAN_POINT('Ctrl Pts',(-0.885001904695471,-0.930935491319084,
11.6118636578801));
#26035=CARTESIAN_POINT('Ctrl Pts',(-0.84573199651817,-0.422923427845423,
11.4008528077841));
#26036=CARTESIAN_POINT('Ctrl Pts',(-0.799098980586865,0.255078212786275,
11.3351181015767));
#26037=CARTESIAN_POINT('Ctrl Pts',(-0.735285379702259,1.10146391779465,
11.6627814277576));
#26038=CARTESIAN_POINT('Ctrl Pts',(-0.686197994457681,1.6296328843616,12.1179713327371));
#26039=CARTESIAN_POINT('Ctrl Pts',(-0.654291194127137,1.86182645070982,
12.5056389077366));
#26040=CARTESIAN_POINT('Ctrl Pts',(-0.624838763160051,2.01967849078206,
12.8866708235145));
#26041=CARTESIAN_POINT('Ctrl Pts',(-0.60029507054379,2.10406567799361,13.2237189739029));
#26042=CARTESIAN_POINT('Ctrl Pts',(-0.57084263933558,2.10399684935638,13.6381840752747));
#26043=CARTESIAN_POINT('Ctrl Pts',(-0.546298946728076,2.05351727011022,
13.9785897887072));
#26044=CARTESIAN_POINT('Ctrl Pts',(-0.531572731173083,1.99338238766352,
14.1769042061779));
#26045=CARTESIAN_POINT('Ctrl Pts',(-0.519300884788924,1.92761739567746,
14.3356823998713));
#26046=CARTESIAN_POINT('Ctrl Pts',(-0.514392146187137,1.89975372144083,
14.3985487843327));
#26047=CARTESIAN_POINT('Ctrl Pts',(-0.504574669387815,1.83791895148544,
14.5213910515937));
#26048=CARTESIAN_POINT('Ctrl Pts',(-0.487394084415219,1.71410350172111,
14.7280360584275));
#26049=CARTESIAN_POINT('Ctrl Pts',(-0.472667868905623,1.58262085472758,
14.888210024574));
#26050=CARTESIAN_POINT('Ctrl Pts',(-0.435852330022712,1.21829850806929,
15.2530421057079));
#26051=CARTESIAN_POINT('Ctrl Pts',(-0.381856206388399,0.535859744814445,
15.6392692230569));
#26052=CARTESIAN_POINT('Ctrl Pts',(-0.298407651514801,-0.67574596699535,
15.6097342394618));
#26053=CARTESIAN_POINT('Ctrl Pts',(-0.20759598870574,-1.78125190703748,
14.8724643137972));
#26054=CARTESIAN_POINT('Ctrl Pts',(-0.143782387914756,-2.10141357731427,
13.9813209628623));
#26055=CARTESIAN_POINT('Ctrl Pts',(-0.0750600487909853,-2.10142877451732,
13.018745682568));
#26056=CARTESIAN_POINT('Ctrl Pts',(-0.0112464480162327,-1.78129552929104,
12.127592539261));
#26057=CARTESIAN_POINT('Ctrl Pts',(0.079565214828448,-0.67581288028697,
11.3902881479926));
#26058=CARTESIAN_POINT('Ctrl Pts',(0.163013769655459,0.53579047445301,11.3607166917808));
#26059=CARTESIAN_POINT('Ctrl Pts',(0.217009893304003,1.21824103378077,11.7469232259717));
#26060=CARTESIAN_POINT('Ctrl Pts',(0.253825432241908,1.58257316404802,12.1117453517784));
#26061=CARTESIAN_POINT('Ctrl Pts',(0.266097278544301,1.69215006954595,12.2452185124881));
#26062=CARTESIAN_POINT('Ctrl Pts',(0.280823493861359,1.80250551956799,12.4195149158672));
#26063=CARTESIAN_POINT('Ctrl Pts',(0.290640971199572,1.87029759818536,12.5391729746263));
#26064=CARTESIAN_POINT('Ctrl Pts',(0.298004078932886,1.91443752392828,12.6325030347934));
#26065=CARTESIAN_POINT('Ctrl Pts',(0.307821556042263,1.96705153765617,12.7595242806143));
#26066=CARTESIAN_POINT('Ctrl Pts',(0.322547771550418,2.03663286377444,12.9539313301886));
#26067=CARTESIAN_POINT('Ctrl Pts',(0.347091464122481,2.10399912325221,13.2926681274472));
#26068=CARTESIAN_POINT('Ctrl Pts',(0.381452633849436,2.10406095745389,13.7762140318887));
#26069=CARTESIAN_POINT('Ctrl Pts',(0.405996326453825,2.01970108901493,14.1132638203997));
#26070=CARTESIAN_POINT('Ctrl Pts',(0.435448757415273,1.86185886016731,14.4943011233421));
#26071=CARTESIAN_POINT('Ctrl Pts',(0.467355557750643,1.62967766233521,14.8819763128389));
#26072=CARTESIAN_POINT('Ctrl Pts',(0.516442942996658,1.10152229544305,15.3371831862365));
#26073=CARTESIAN_POINT('Ctrl Pts',(0.580256543880559,0.255146656090134,
15.6648734409929));
#26074=CARTESIAN_POINT('Ctrl Pts',(0.626889559804317,-0.422857263281462,
15.5991601609565));
#26075=CARTESIAN_POINT('Ctrl Pts',(0.66615946798391,-0.930876015826006,
15.3881653339733));
#26076=CARTESIAN_POINT('Ctrl Pts',(0.685794422082415,-1.17456155931576,
15.2579989996418));
#26077=CARTESIAN_POINT('Ctrl Pts',(0.705429376203152,-1.38814271520269,
15.0826664192684));
#26078=CARTESIAN_POINT('Ctrl Pts',(0.720155591788415,-1.5339674905036,14.9368409887842));
#26079=CARTESIAN_POINT('Ctrl Pts',(0.734881807223654,-1.67266298412755,
14.7838610537252));
#26080=CARTESIAN_POINT('Ctrl Pts',(0.759425499988951,-1.86446763640772,
14.4966824904347));
#26081=CARTESIAN_POINT('Ctrl Pts',(0.798695408116211,-2.07619298774507,
13.9861650044251));
#26082=CARTESIAN_POINT('Ctrl Pts',(0.83551094730015,-2.1277744490612,13.4632049483027));
#26083=CARTESIAN_POINT('Ctrl Pts',(0.864963377919054,-2.05684513787007,
13.0556962539315));
#26084=CARTESIAN_POINT('Ctrl Pts',(0.879689593697196,-2.00184974289138,
12.856878855445));
#26085=CARTESIAN_POINT('Ctrl Pts',(0.88705270144308,-1.96706316877626,12.7596726372977));
#26086=CARTESIAN_POINT('Ctrl Pts',(0.911596393960796,-1.83553762188005,
12.4421170175806));
#26087=CARTESIAN_POINT('Ctrl Pts',(0.931231348155162,-1.67983986643869,
12.2090983517141));
#26088=CARTESIAN_POINT('Ctrl Pts',(0.96559251775177,-1.33957935861203,11.8687822298386));
#26089=CARTESIAN_POINT('Ctrl Pts',(0.99504494876616,-1.00473313541158,11.620825614142));
#26090=CARTESIAN_POINT('Ctrl Pts',(1.05394981114623,-0.219400648575714,
11.3385040063844));
#26091=CARTESIAN_POINT('Ctrl Pts',(1.09812845789801,0.422846266856786,11.4008221062241));
#26092=CARTESIAN_POINT('Ctrl Pts',(1.14476147379055,1.02621088612219,11.6513200396668));
#26093=CARTESIAN_POINT('Ctrl Pts',(1.17912264334457,1.43813543913076,11.9125898832225));
#26094=CARTESIAN_POINT('Ctrl Pts',(1.24293624415171,1.99816323522134,12.6272981531672));
#26095=CARTESIAN_POINT('Ctrl Pts',(1.30674984512595,2.18004770840565,13.5415476016066));
#26096=CARTESIAN_POINT('Ctrl Pts',(1.37056344590792,1.93615927629818,14.4161304124479));
#26097=CARTESIAN_POINT('Ctrl Pts',(1.40492461546698,1.6556540141085,14.8152572944509));
#26098=CARTESIAN_POINT('Ctrl Pts',(1.44664889293198,1.24244134800518,15.2284882608853));
#26099=CARTESIAN_POINT('Ctrl Pts',(1.49082753975291,0.695641431593744,15.5558329045212));
#26100=CARTESIAN_POINT('Ctrl Pts',(1.55464114056533,-0.211343205044639,
15.6449359634957));
#26101=CARTESIAN_POINT('Ctrl Pts',(1.60372852562089,-0.881788707995604,
15.4415169212182));
#26102=CARTESIAN_POINT('Ctrl Pts',(1.63808969520711,-1.28374872909566,15.1726362981186));
#26103=CARTESIAN_POINT('Ctrl Pts',(1.65281591077819,-1.43674418522118,15.0340074462966));
#26104=CARTESIAN_POINT('Ctrl Pts',(1.66017901862767,-1.5096562843569,14.9610939287589));
#26105=CARTESIAN_POINT('Ctrl Pts',(1.66999649560661,-1.60450816196902,14.8614916681869));
#26106=CARTESIAN_POINT('Ctrl Pts',(1.6945401882874,-1.81641660638884,14.5898157678553));
#26107=CARTESIAN_POINT('Ctrl Pts',(1.74117320432588,-2.09968312529506,13.993136245687));
#26108=CARTESIAN_POINT('Ctrl Pts',(1.80007806641223,-2.14132297639453,13.1443431199714));
#26109=CARTESIAN_POINT('Ctrl Pts',(1.86389166718199,-1.79190346307116,12.3025734370431));
#26110=CARTESIAN_POINT('Ctrl Pts',(1.92525089873163,-1.1728837333095,11.6829956582692));
#26111=CARTESIAN_POINT('Ctrl Pts',(1.9890644993147,-0.318451445307582,11.353262621575));
#26112=CARTESIAN_POINT('Ctrl Pts',(2.05533246926636,0.629916684121097,11.4232604409134));
#26113=CARTESIAN_POINT('Ctrl Pts',(2.12160043965998,1.45738279440301,11.8920089333997));
#26114=CARTESIAN_POINT('Ctrl Pts',(2.16577908623353,1.82239184147097,12.4103056664616));
#26115=CARTESIAN_POINT('Ctrl Pts',(2.19114090159337,1.95830212268135,12.7384343791443));
#26116=CARTESIAN_POINT('Ctrl Pts',(2.19482245546371,1.97647393187141,12.7867134206883));
#26117=CARTESIAN_POINT('Ctrl Pts',(2.19973119624365,1.99830521034253,12.8518983669964));
#26118=CARTESIAN_POINT('Ctrl Pts',(2.20627616390887,2.02599016863268,12.9392817993886));
#26119=CARTESIAN_POINT('Ctrl Pts',(2.21732087682484,2.06362019625161,13.0895000864374));
#26120=CARTESIAN_POINT('Ctrl Pts',(2.23204700316566,2.09392025952937,13.2937422834945));
#26121=CARTESIAN_POINT('Ctrl Pts',(2.24186454896205,2.10067736162775,13.4312297636866));
#26122=CARTESIAN_POINT('Ctrl Pts',(2.26640830731602,2.1006866380108,13.7749488306902));
#26123=CARTESIAN_POINT('Ctrl Pts',(2.286042974127,2.04603571825695,14.0498326403604));
#26124=CARTESIAN_POINT('Ctrl Pts',(2.30813251222673,1.9276507441991,14.3356292078984));
#26125=CARTESIAN_POINT('Ctrl Pts',(2.33267651818434,1.78842576055076,14.6500263621867));
#26126=CARTESIAN_POINT('Ctrl Pts',(2.37685421054368,1.39839795140035,15.1495402659449));
#26127=CARTESIAN_POINT('Ctrl Pts',(2.44066915571005,0.594740868894852,15.5792454847316));
#26128=CARTESIAN_POINT('Ctrl Pts',(2.50448156968343,-0.318252030767666,
15.6466850868822));
#26129=CARTESIAN_POINT('Ctrl Pts',(2.5732035136348,-1.23868770045141,15.2920299004919));
#26130=CARTESIAN_POINT('Ctrl Pts',(2.63947583757363,-1.88086695443964,14.5832859786279));
#26131=CARTESIAN_POINT('Ctrl Pts',(2.70327860614168,-2.14454478615246,13.7115935900664));
#26132=CARTESIAN_POINT('Ctrl Pts',(2.77202497624202,-2.04943982851017,12.7342369759876));
#26133=CARTESIAN_POINT('Ctrl Pts',(2.82527858318522,-1.61782105646327,12.0867954330277));
#26134=CARTESIAN_POINT('Ctrl Pts',(2.8589519925713,-1.24010853015882,11.8034581198931));
#26135=CARTESIAN_POINT('Ctrl Pts',(2.8631579592014,-1.19160472684239,11.7700461798512));
#26136=CARTESIAN_POINT('',(-2.91382504120091,0.,14.89));
#26137=CARTESIAN_POINT('Origin',(-3.29867228626928,0.,15.245));
#26138=CARTESIAN_POINT('Ctrl Pts',(-2.86395232247026,1.18339323898477,11.7647413855289));
#26139=CARTESIAN_POINT('Ctrl Pts',(-2.85951639598233,1.23470680988399,11.799740100392));
#26140=CARTESIAN_POINT('Ctrl Pts',(-2.83299103552865,1.5324114987355,12.0225088821029));
#26141=CARTESIAN_POINT('Ctrl Pts',(-2.8040120778353,1.78814814342653,12.3501521071371));
#26142=CARTESIAN_POINT('Ctrl Pts',(-2.77946807208677,1.92737178398469,12.6645011910224));
#26143=CARTESIAN_POINT('Ctrl Pts',(-2.75737853413057,2.04574294616347,12.9502605082012));
#26144=CARTESIAN_POINT('Ctrl Pts',(-2.73774386712553,2.10040352107426,13.2250982876992));
#26145=CARTESIAN_POINT('Ctrl Pts',(-2.71320010881799,2.10039759285345,13.5687716283892));
#26146=CARTESIAN_POINT('Ctrl Pts',(-2.703382563069,2.0936420873127,13.7062412062418));
#26147=CARTESIAN_POINT('Ctrl Pts',(-2.68865643666704,2.06334666234638,13.9104570270601));
#26148=CARTESIAN_POINT('Ctrl Pts',(-2.67761172378578,2.02572215584014,14.0606557808409));
#26149=CARTESIAN_POINT('Ctrl Pts',(-2.67106675611039,1.99804077971579,14.1480281091204));
#26150=CARTESIAN_POINT('Ctrl Pts',(-2.66615801533196,1.97621227192314,14.2132048011292));
#26151=CARTESIAN_POINT('Ctrl Pts',(-2.66247646146109,1.95804284955894,14.2614776811265));
#26152=CARTESIAN_POINT('Ctrl Pts',(-2.63711464609784,1.82215054249416,14.5895642078971));
#26153=CARTESIAN_POINT('Ctrl Pts',(-2.59293599952233,1.45719179411054,15.107792259493));
#26154=CARTESIAN_POINT('Ctrl Pts',(-2.52666802913216,0.629832203340271,
15.5764801682427));
#26155=CARTESIAN_POINT('Ctrl Pts',(-2.46040005918036,-0.318413945911626,
15.6464676527716));
#26156=CARTESIAN_POINT('Ctrl Pts',(-2.39658645859582,-1.17273725777722,
15.3167756828035));
#26157=CARTESIAN_POINT('Ctrl Pts',(-2.33522722704962,-1.79167816896257,
14.6972758001249));
#26158=CARTESIAN_POINT('Ctrl Pts',(-2.27141362627676,-2.14105325390368,
13.855612208645));
#26159=CARTESIAN_POINT('Ctrl Pts',(-2.21250876419197,-2.09941852228509,
13.0069263498048));
#26160=CARTESIAN_POINT('Ctrl Pts',(-2.16587574815266,-1.81618760322336,
12.4103221850427));
#26161=CARTESIAN_POINT('Ctrl Pts',(-2.14133205547323,-1.60430579232672,
12.13868064052));
#26162=CARTESIAN_POINT('Ctrl Pts',(-2.13151457849414,-1.50946592983573,
12.0390909700533));
#26163=CARTESIAN_POINT('Ctrl Pts',(-2.12415147064491,-1.43656303221216,
11.9661866807793));
#26164=CARTESIAN_POINT('Ctrl Pts',(-2.10942525507374,-1.28358690527117,
11.8275753375537));
#26165=CARTESIAN_POINT('Ctrl Pts',(-2.07506408548576,-0.881677639438382,
11.5587288109207));
#26166=CARTESIAN_POINT('Ctrl Pts',(-2.02597670042933,-0.211316719569808,
11.3553356115629));
#26167=CARTESIAN_POINT('Ctrl Pts',(-1.96216309961809,0.695553256549286,
11.4444274965203));
#26168=CARTESIAN_POINT('Ctrl Pts',(-1.91798445279889,1.24228418885524,11.7717307237019));
#26169=CARTESIAN_POINT('Ctrl Pts',(-1.87626017533466,1.65544468008186,12.1849091373921));
#26170=CARTESIAN_POINT('Ctrl Pts',(-1.84189900577446,1.93591474668381,12.5839855411706));
#26171=CARTESIAN_POINT('Ctrl Pts',(-1.77808540499141,2.17977217767513,13.4584576635979));
#26172=CARTESIAN_POINT('Ctrl Pts',(-1.71427180401722,1.99791066935068,14.3725915504926));
#26173=CARTESIAN_POINT('Ctrl Pts',(-1.65045820321132,1.43795381725481,15.0872093791297));
#26174=CARTESIAN_POINT('Ctrl Pts',(-1.61609703365616,1.02608112988485,15.3484460912615));
#26175=CARTESIAN_POINT('Ctrl Pts',(-1.56946401776296,0.422792880231089,
15.5989118787714));
#26176=CARTESIAN_POINT('Ctrl Pts',(-1.52528537101175,-0.219372883281587,
15.6612220798083));
#26177=CARTESIAN_POINT('Ctrl Pts',(-1.46638050863173,-1.00460604457137,
15.3789362729773));
#26178=CARTESIAN_POINT('Ctrl Pts',(-1.43692807761804,-1.33940996924325,
15.1310108721175));
#26179=CARTESIAN_POINT('Ctrl Pts',(-1.40256690802025,-1.67962743720217,
14.790737877859));
#26180=CARTESIAN_POINT('Ctrl Pts',(-1.38293195382286,-1.83530555995113,
14.5577485921235));
#26181=CARTESIAN_POINT('Ctrl Pts',(-1.35838826131112,-1.96681455751747,
14.2402332233263));
#26182=CARTESIAN_POINT('Ctrl Pts',(-1.35102515356799,-2.00159671759724,
14.1430392814066));
#26183=CARTESIAN_POINT('Ctrl Pts',(-1.33629893777783,-2.05658519035004,
13.9442470225823));
#26184=CARTESIAN_POINT('Ctrl Pts',(-1.30684650719147,-2.12750545897677,
13.5367898517779));
#26185=CARTESIAN_POINT('Ctrl Pts',(-1.27003096793995,-2.07593057890912,
13.0138958671947));
#26186=CARTESIAN_POINT('Ctrl Pts',(-1.23076105988595,-1.86423205700168,
12.5034429312468));
#26187=CARTESIAN_POINT('Ctrl Pts',(-1.20621736708542,-1.67245166038405,
12.2163007047761));
#26188=CARTESIAN_POINT('Ctrl Pts',(-1.1914911516536,-1.53377371678283,12.0633401357287));
#26189=CARTESIAN_POINT('Ctrl Pts',(-1.17676493607063,-1.38796737947216,
11.9175331486101));
#26190=CARTESIAN_POINT('Ctrl Pts',(-1.15712998194875,-1.17441323673287,
11.7422228942938));
#26191=CARTESIAN_POINT('Ctrl Pts',(-1.1374950278532,-0.930758522391391,
11.6120730373285));
#26192=CARTESIAN_POINT('Ctrl Pts',(-1.09822511967589,-0.422803967350463,
11.4011055450012));
#26193=CARTESIAN_POINT('Ctrl Pts',(-1.05159210374468,0.255114060124627,
11.3354006658051));
#26194=CARTESIAN_POINT('Ctrl Pts',(-0.987778502859985,1.10138252402949,
11.6630493850669));
#26195=CARTESIAN_POINT('Ctrl Pts',(-0.938691117615512,1.62947047446097,
12.1181985558448));
#26196=CARTESIAN_POINT('Ctrl Pts',(-0.906784317284843,1.86162252844231,
12.505824402897));
#26197=CARTESIAN_POINT('Ctrl Pts',(-0.877331886317726,2.01944264609616,
12.8868131774084));
#26198=CARTESIAN_POINT('Ctrl Pts',(-0.852788193701485,2.10380859651136,
13.2238214133424));
#26199=CARTESIAN_POINT('Ctrl Pts',(-0.823335762493315,2.10372675620362,
13.6382341331381));
#26200=CARTESIAN_POINT('Ctrl Pts',(-0.798792069885758,2.05324287076447,
13.9785952306268));
#26201=CARTESIAN_POINT('Ctrl Pts',(-0.784065854330827,1.99310933344462,
14.1768826785089));
#26202=CARTESIAN_POINT('Ctrl Pts',(-0.7717940079467,1.92734766933172,14.335638732088));
#26203=CARTESIAN_POINT('Ctrl Pts',(-0.766885269344943,1.89948553670055,
14.3984962882538));
#26204=CARTESIAN_POINT('Ctrl Pts',(-0.757067792545443,1.8376547328267,14.5213210863396));
#26205=CARTESIAN_POINT('Ctrl Pts',(-0.739887207572969,1.71384840296856,
14.7279360406703));
#26206=CARTESIAN_POINT('Ctrl Pts',(-0.725160992063393,1.5823773053324,14.8880855588829));
#26207=CARTESIAN_POINT('Ctrl Pts',(-0.688345453180475,1.21808924244413,
15.2528597399623));
#26208=CARTESIAN_POINT('Ctrl Pts',(-0.63434932954611,0.535724535273187,
15.6390163094263));
#26209=CARTESIAN_POINT('Ctrl Pts',(-0.550900774672618,-0.6757274452496,
15.609444965228));
#26210=CARTESIAN_POINT('Ctrl Pts',(-0.460089111863575,-1.78107000044726,
14.8722340315906));
#26211=CARTESIAN_POINT('Ctrl Pts',(-0.396275511072554,-2.10116286876526,
13.9811937613502));
#26212=CARTESIAN_POINT('Ctrl Pts',(-0.327553171948746,-2.10114784905051,
13.018740961484));
#26213=CARTESIAN_POINT('Ctrl Pts',(-0.263739571173964,-1.78102745715508,
12.1277110014121));
#26214=CARTESIAN_POINT('Ctrl Pts',(-0.172927908329469,-0.675661904576781,
11.3905350167616));
#26215=CARTESIAN_POINT('Ctrl Pts',(-0.0894793535022535,0.535789576569599,
11.3610032710076));
#26216=CARTESIAN_POINT('Ctrl Pts',(-0.0354832298537147,1.21814183783093,
11.747182094498));
#26217=CARTESIAN_POINT('Ctrl Pts',(0.00133230908414512,1.58241678739983,
12.1119691836169));
#26218=CARTESIAN_POINT('Ctrl Pts',(0.0136041553865288,1.69197569693335,
12.2454288356657));
#26219=CARTESIAN_POINT('Ctrl Pts',(0.0283303707037281,1.80231176016096,
12.4197066355812));
#26220=CARTESIAN_POINT('Ctrl Pts',(0.0381478480417329,1.87009150500503,
12.5393516987898));
#26221=CARTESIAN_POINT('Ctrl Pts',(0.0455109557751048,1.91422294038976,
12.6326713282807));
#26222=CARTESIAN_POINT('Ctrl Pts',(0.0553284328845138,1.96682631953794,
12.7596781644253));
#26223=CARTESIAN_POINT('Ctrl Pts',(0.0700546483926733,2.03639275364112,
12.9540628133223));
#26224=CARTESIAN_POINT('Ctrl Pts',(0.0945983409647811,2.10373988430058,
13.2927589040249));
#26225=CARTESIAN_POINT('Ctrl Pts',(0.128959510691625,2.1037865350476,13.7762436940241));
#26226=CARTESIAN_POINT('Ctrl Pts',(0.153503203296114,2.01942674468552,14.1132482690728));
#26227=CARTESIAN_POINT('Ctrl Pts',(0.182955634257591,1.86159251610715,14.4942325177201));
#26228=CARTESIAN_POINT('Ctrl Pts',(0.214862434592872,1.62942849097079,14.8818513989961));
#26229=CARTESIAN_POINT('Ctrl Pts',(0.263949819838949,1.10132555773969,15.3369843770367));
#26230=CARTESIAN_POINT('Ctrl Pts',(0.327763420722699,0.255046583726186,
15.6646068840464));
#26231=CARTESIAN_POINT('Ctrl Pts',(0.374396436646611,-0.422869598616443,
15.5988808622999));
#26232=CARTESIAN_POINT('Ctrl Pts',(0.413666344826193,-0.93081759534357,
15.3878974965819));
#26233=CARTESIAN_POINT('Ctrl Pts',(0.433301298924743,-1.17446825510573,
15.2577400181351));
#26234=CARTESIAN_POINT('Ctrl Pts',(0.452936253045398,-1.38801691891332,
15.0824230855869));
#26235=CARTESIAN_POINT('Ctrl Pts',(0.467662468630681,-1.53381868681228,
14.9366115293155));
#26236=CARTESIAN_POINT('Ctrl Pts',(0.482388684065977,-1.67249183188709,
14.7836466105238));
#26237=CARTESIAN_POINT('Ctrl Pts',(0.506932376831184,-1.86426323547285,
14.4964983877605));
#26238=CARTESIAN_POINT('Ctrl Pts',(0.546202284958494,-2.07594573733582,
13.9860388151222));
#26239=CARTESIAN_POINT('Ctrl Pts',(0.58301782414224,-2.12750424881575,13.463143268723));
#26240=CARTESIAN_POINT('Ctrl Pts',(0.61247025476142,-2.05657118613531,13.0556883300511));
#26241=CARTESIAN_POINT('Ctrl Pts',(0.62719647053937,-2.00157647080744,12.8568978000849));
#26242=CARTESIAN_POINT('Ctrl Pts',(0.634559578285301,-1.96679125863703,
12.7597049515784));
#26243=CARTESIAN_POINT('Ctrl Pts',(0.659103270803122,-1.83527229136505,
12.4421937174885));
#26244=CARTESIAN_POINT('Ctrl Pts',(0.67873822499742,-1.67958686286578,12.2092093349896));
#26245=CARTESIAN_POINT('Ctrl Pts',(0.713099394594027,-1.33935871215268,
11.8689470329008));
#26246=CARTESIAN_POINT('Ctrl Pts',(0.742551825608453,-1.0045470059286,11.6210321549827));
#26247=CARTESIAN_POINT('Ctrl Pts',(0.801456687988358,-0.219304983886525,
11.33877101901));
#26248=CARTESIAN_POINT('Ctrl Pts',(0.845635334740273,0.422858819730382,
11.4011013952));
#26249=CARTESIAN_POINT('Ctrl Pts',(0.892268350632809,1.02613920072941,11.6515861350263));
#26250=CARTESIAN_POINT('Ctrl Pts',(0.926629520186844,1.43800368130773,11.9128357874006));
#26251=CARTESIAN_POINT('Ctrl Pts',(0.99044312099397,1.99793808743644,12.6274712081551));
#26252=CARTESIAN_POINT('Ctrl Pts',(1.05425672196811,2.17977088478312,13.5416108112303));
#26253=CARTESIAN_POINT('Ctrl Pts',(1.11807032275011,1.93588599253454,14.4160752800524));
#26254=CARTESIAN_POINT('Ctrl Pts',(1.15243149230917,1.65540339740651,14.8151428801159));
#26255=CARTESIAN_POINT('Ctrl Pts',(1.19415576977416,1.2422299359489,15.2283083230172));
#26256=CARTESIAN_POINT('Ctrl Pts',(1.23833441659508,0.695488745466205,15.5555943973105));
#26257=CARTESIAN_POINT('Ctrl Pts',(1.30214801740745,-0.211384009584384,
15.6446578133189));
#26258=CARTESIAN_POINT('Ctrl Pts',(1.35123540246295,-0.881738497810867,
15.4412435944634));
#26259=CARTESIAN_POINT('Ctrl Pts',(1.38559657204916,-1.28363930202604,15.172384458236));
#26260=CARTESIAN_POINT('Ctrl Pts',(1.40032278762018,-1.43661106863639,15.0337683155675));
#26261=CARTESIAN_POINT('Ctrl Pts',(1.40768589546967,-1.50951167457381,14.9608617378445));
#26262=CARTESIAN_POINT('Ctrl Pts',(1.41750337244863,-1.60434840567024,14.8612690911551));
#26263=CARTESIAN_POINT('Ctrl Pts',(1.44204706512938,-1.81622166540711,14.5896209074415));
#26264=CARTESIAN_POINT('Ctrl Pts',(1.48868008116764,-2.09943371647049,13.9930079562618));
#26265=CARTESIAN_POINT('Ctrl Pts',(1.54758494325403,-2.14104170095398,13.144320866245));
#26266=CARTESIAN_POINT('Ctrl Pts',(1.61139854402315,-1.79163977666453,12.3026685936186));
#26267=CARTESIAN_POINT('Ctrl Pts',(1.672757775572,-1.17267887511365,11.6831886072225));
#26268=CARTESIAN_POINT('Ctrl Pts',(1.73657137615399,-0.318344426567643,
11.3535241406746));
#26269=CARTESIAN_POINT('Ctrl Pts',(1.80283934610328,0.629901232782519,11.4235428712566));
#26270=CARTESIAN_POINT('Ctrl Pts',(1.86910731649445,1.45724767055709,11.8922581094627));
#26271=CARTESIAN_POINT('Ctrl Pts',(1.9132859630631,1.82219364420109,12.4105006201815));
#26272=CARTESIAN_POINT('Ctrl Pts',(1.93864777842214,1.958076391633,12.7385920533271));
#26273=CARTESIAN_POINT('Ctrl Pts',(1.94232933229241,1.97624436428055,12.786865560793));
#26274=CARTESIAN_POINT('Ctrl Pts',(1.9472380730709,1.9980708388772,12.8520429490877));
#26275=CARTESIAN_POINT('Ctrl Pts',(1.95378304074728,2.02574952526818,12.9394162047849));
#26276=CARTESIAN_POINT('Ctrl Pts',(1.96482775362835,2.06336995074317,13.0896166528483));
#26277=CARTESIAN_POINT('Ctrl Pts',(1.97955388002742,2.09365953804166,13.2938339723862));
#26278=CARTESIAN_POINT('Ctrl Pts',(1.9893714257774,2.10041134743223,13.4313042539146));
#26279=CARTESIAN_POINT('Ctrl Pts',(2.01391518408421,2.10040911756558,13.7749798122416));
#26280=CARTESIAN_POINT('Ctrl Pts',(2.03354985106829,2.04575275009202,14.0498267163717));
#26281=CARTESIAN_POINT('Ctrl Pts',(2.05563938902259,1.92737336277738,14.3355834398345));
#26282=CARTESIAN_POINT('Ctrl Pts',(2.08018339476934,1.78815549053371,14.6499365896423));
#26283=CARTESIAN_POINT('Ctrl Pts',(2.12436108771495,1.39815247612617,15.1493719808017));
#26284=CARTESIAN_POINT('Ctrl Pts',(2.1881760319483,0.594574019921796,15.5790015900282));
#26285=CARTESIAN_POINT('Ctrl Pts',(2.25198844660101,-0.318322870616011,
15.6463919965956));
#26286=CARTESIAN_POINT('Ctrl Pts',(2.32071039067994,-1.23866577243641,15.2917708772129));
#26287=CARTESIAN_POINT('Ctrl Pts',(2.38698271143203,-1.88078189450323,14.5830446809642));
#26288=CARTESIAN_POINT('Ctrl Pts',(2.450785486869,-2.14449521632646,13.7115329395622));
#26289=CARTESIAN_POINT('Ctrl Pts',(2.51953184050711,-2.04937889610162,12.7340785859711));
#26290=CARTESIAN_POINT('Ctrl Pts',(2.58575353157662,-1.51228301440999,11.9296669778702));
#26291=CARTESIAN_POINT('Ctrl Pts',(2.64970641129486,-0.719879659816408,
11.482543891491));
#26292=CARTESIAN_POINT('Ctrl Pts',(2.68414064416519,-0.238646463251669,
11.3992812306547));
#26293=CARTESIAN_POINT('Ctrl Pts',(2.70136633287573,0.00319878278718031,
11.3996354935645));
#26294=CARTESIAN_POINT('Ctrl Pts',(-2.94898729103638,1.05177980826717,11.9577756495737));
#26295=CARTESIAN_POINT('Ctrl Pts',(-2.94455138545693,1.09739106504139,11.9888760681277));
#26296=CARTESIAN_POINT('Ctrl Pts',(-2.918026110446,1.3619620785344,12.186884227221));
#26297=CARTESIAN_POINT('Ctrl Pts',(-2.88904678767022,1.58922760362333,12.4781026097179));
#26298=CARTESIAN_POINT('Ctrl Pts',(-2.86450296461958,1.71300194233482,12.7574567944657));
#26299=CARTESIAN_POINT('Ctrl Pts',(-2.84241355188039,1.8181539629972,13.0114540002238));
#26300=CARTESIAN_POINT('Ctrl Pts',(-2.82277871735286,1.86678055104444,13.2556912711833));
#26301=CARTESIAN_POINT('Ctrl Pts',(-2.79823499734993,1.86676441116482,13.5611506108829));
#26302=CARTESIAN_POINT('Ctrl Pts',(-2.78841749169422,1.86076014318703,13.6833245219451));
#26303=CARTESIAN_POINT('Ctrl Pts',(-2.77369131329709,1.83383161817478,13.8648277310688));
#26304=CARTESIAN_POINT('Ctrl Pts',(-2.76264663035824,1.8003898778738,13.9983167301413));
#26305=CARTESIAN_POINT('Ctrl Pts',(-2.75610165277409,1.77578783700224,14.0759711000829));
#26306=CARTESIAN_POINT('Ctrl Pts',(-2.75119291327835,1.75638332024967,14.1338966609949));
#26307=CARTESIAN_POINT('Ctrl Pts',(-2.74751135937009,1.74024106899155,14.1768014870589));
#26308=CARTESIAN_POINT('Ctrl Pts',(-2.72214954377412,1.61942429167451,14.4683809016479));
#26309=CARTESIAN_POINT('Ctrl Pts',(-2.67797089709577,1.29509438279977,14.9289708470309));
#26310=CARTESIAN_POINT('Ctrl Pts',(-2.6117029268964,0.559739361759716,15.3455116670227));
#26311=CARTESIAN_POINT('Ctrl Pts',(-2.54543495691169,-0.283018800514111,
15.4077039754452));
#26312=CARTESIAN_POINT('Ctrl Pts',(-2.48162135624977,-1.04231371404291,
15.1146741383994));
#26313=CARTESIAN_POINT('Ctrl Pts',(-2.42026212474002,-1.59239241227961,
14.5640775634698));
#26314=CARTESIAN_POINT('Ctrl Pts',(-2.356448523998,-1.90291363513159,13.8160277442462));
#26315=CARTESIAN_POINT('Ctrl Pts',(-2.29754366181465,-1.8658791953148,13.0617489355256));
#26316=CARTESIAN_POINT('Ctrl Pts',(-2.25091064584323,-1.61417795247039,
12.5315062166412));
#26317=CARTESIAN_POINT('Ctrl Pts',(-2.22636695317173,-1.42581820826996,
12.2900866009581));
#26318=CARTESIAN_POINT('Ctrl Pts',(-2.216549476156,-1.34155044848788,12.2015728667815));
#26319=CARTESIAN_POINT('Ctrl Pts',(-2.20918636829416,-1.27674728353269,
12.1367854064728));
#26320=CARTESIAN_POINT('Ctrl Pts',(-2.19446015276218,-1.14079176069474,
12.0135799955576));
#26321=CARTESIAN_POINT('Ctrl Pts',(-2.16009898317316,-0.783580906846267,
11.7746602397536));
#26322=CARTESIAN_POINT('Ctrl Pts',(-2.11101159809488,-0.187782817615464,
11.5939005667503));
#26323=CARTESIAN_POINT('Ctrl Pts',(-2.04719799726984,0.618205729404025,
11.6730712407523));
#26324=CARTESIAN_POINT('Ctrl Pts',(-2.00301935049051,1.10412222965747,11.9640298571025));
#26325=CARTESIAN_POINT('Ctrl Pts',(-1.96129507302961,1.47130954923465,12.331184249062));
#26326=CARTESIAN_POINT('Ctrl Pts',(-1.92693390345156,1.72060698460052,12.6859172796413));
#26327=CARTESIAN_POINT('Ctrl Pts',(-1.86312030263897,1.93730413467564,13.463091044457));
#26328=CARTESIAN_POINT('Ctrl Pts',(-1.7993067017454,1.77565703033136,14.2755679481243));
#26329=CARTESIAN_POINT('Ctrl Pts',(-1.7354931009231,1.27800656389494,14.9106625105529));
#26330=CARTESIAN_POINT('Ctrl Pts',(-1.70113193134735,0.911903775153735,
15.1428819271019));
#26331=CARTESIAN_POINT('Ctrl Pts',(-1.6544989154371,0.375754078194938,15.3654086726963));
#26332=CARTESIAN_POINT('Ctrl Pts',(-1.61032026868658,-0.195009556823064,
15.4208186513374));
#26333=CARTESIAN_POINT('Ctrl Pts',(-1.55141540637949,-0.89287467908256,
15.1699353718112));
#26334=CARTESIAN_POINT('Ctrl Pts',(-1.52196297529924,-1.19044705982738,
14.9495422087379));
#26335=CARTESIAN_POINT('Ctrl Pts',(-1.48760180570641,-1.49280856824171,
14.6471851287901));
#26336=CARTESIAN_POINT('Ctrl Pts',(-1.46796685157482,-1.63114583675639,
14.4400090223007));
#26337=CARTESIAN_POINT('Ctrl Pts',(-1.44342315897332,-1.74805594016706,
14.1578798012588));
#26338=CARTESIAN_POINT('Ctrl Pts',(-1.43606005119052,-1.77895201880203,
14.0714828485797));
#26339=CARTESIAN_POINT('Ctrl Pts',(-1.42133383556671,-1.82784367389418,
13.8948060786019));
#26340=CARTESIAN_POINT('Ctrl Pts',(-1.39188140473377,-1.89083654696875,
13.532670438544));
#26341=CARTESIAN_POINT('Ctrl Pts',(-1.35506586566434,-1.84501027253879,
13.0679371083961));
#26342=CARTESIAN_POINT('Ctrl Pts',(-1.31579595754304,-1.65685861831594,
12.6142668799998));
#26343=CARTESIAN_POINT('Ctrl Pts',(-1.29125226482124,-1.4863996270751,12.3590620417495));
#26344=CARTESIAN_POINT('Ctrl Pts',(-1.27652604934709,-1.36315184596167,
12.223124185907));
#26345=CARTESIAN_POINT('Ctrl Pts',(-1.26179983374059,-1.23356011807307,
12.0935170469981));
#26346=CARTESIAN_POINT('Ctrl Pts',(-1.24216487964064,-1.04375563480033,
11.9377637595064));
#26347=CARTESIAN_POINT('Ctrl Pts',(-1.22252992555137,-0.827209047354781,
11.8220180667511));
#26348=CARTESIAN_POINT('Ctrl Pts',(-1.18326001737828,-0.375738967230657,
11.6346427649014));
#26349=CARTESIAN_POINT('Ctrl Pts',(-1.13662700141788,0.226759583587447,
11.5761502172032));
#26350=CARTESIAN_POINT('Ctrl Pts',(-1.07281340056232,0.978897200444188,
11.867410994966));
#26351=CARTESIAN_POINT('Ctrl Pts',(-1.02372601533608,1.44823540529516,12.2719311266445));
#26352=CARTESIAN_POINT('Ctrl Pts',(-0.991819214989638,1.65456333844798,
12.6164315560303));
#26353=CARTESIAN_POINT('Ctrl Pts',(-0.962366783997792,1.79481940789023,
12.9550584907526));
#26354=CARTESIAN_POINT('Ctrl Pts',(-0.937823091353101,1.86980040908937,
13.2545704979585));
#26355=CARTESIAN_POINT('Ctrl Pts',(-0.908370660191932,1.86972197127684,
13.6228927098112));
#26356=CARTESIAN_POINT('Ctrl Pts',(-0.883826967550878,1.82485010373173,
13.9253917288496));
#26357=CARTESIAN_POINT('Ctrl Pts',(-0.869100752025165,1.77140023412798,
14.1016232582535));
#26358=CARTESIAN_POINT('Ctrl Pts',(-0.856828905671129,1.71295578839072,
14.2427213235411));
#26359=CARTESIAN_POINT('Ctrl Pts',(-0.851920167081815,1.6881868322722,14.2985826390753));
#26360=CARTESIAN_POINT('Ctrl Pts',(-0.842102690140726,1.63324292701848,
14.4077535244));
#26361=CARTESIAN_POINT('Ctrl Pts',(-0.824922105271772,1.52318322321949,
14.5913659007489));
#26362=CARTESIAN_POINT('Ctrl Pts',(-0.81019588976506,1.40636770077858,14.7337299682696));
#26363=CARTESIAN_POINT('Ctrl Pts',(-0.773380350883849,1.08254357632472,
15.0578770878186));
#26364=CARTESIAN_POINT('Ctrl Pts',(-0.719384227226075,0.476127115050851,
15.4011394060682));
#26365=CARTESIAN_POINT('Ctrl Pts',(-0.635935672325424,-0.600610770607247,
15.3747474794605));
#26366=CARTESIAN_POINT('Ctrl Pts',(-0.545124009595912,-1.58296648710691,
14.7195854393962));
#26367=CARTESIAN_POINT('Ctrl Pts',(-0.481310408779742,-1.86744232190721,
13.9276261419255));
#26368=CARTESIAN_POINT('Ctrl Pts',(-0.412588069623317,-1.8674172716517,
13.0722641862657));
#26369=CARTESIAN_POINT('Ctrl Pts',(-0.348774468813634,-1.58289462307497,
12.2803217206137));
#26370=CARTESIAN_POINT('Ctrl Pts',(-0.257962806069509,-0.60050100556019,
11.625218534854));
#26371=CARTESIAN_POINT('Ctrl Pts',(-0.174514251188141,0.476238220638283,
11.5988907922679));
#26372=CARTESIAN_POINT('Ctrl Pts',(-0.1205181275243,1.08263207658234,11.9421915291005));
#26373=CARTESIAN_POINT('Ctrl Pts',(-0.083702588620523,1.40643852814198,
12.266356491699));
#26374=CARTESIAN_POINT('Ctrl Pts',(-0.0714307423348015,1.50377190616919,
12.3850057885532));
#26375=CARTESIAN_POINT('Ctrl Pts',(-0.056704526908075,1.60185605597705,
12.5398795378693));
#26376=CARTESIAN_POINT('Ctrl Pts',(-0.0468870497427143,1.66208392322534,
12.6462265542716));
#26377=CARTESIAN_POINT('Ctrl Pts',(-0.0395239419637206,1.70131215898071,
12.7291604128228));
#26378=CARTESIAN_POINT('Ctrl Pts',(-0.0297064648246382,1.74806119403677,
12.8420424941069));
#26379=CARTESIAN_POINT('Ctrl Pts',(-0.0149802493183748,1.80988609416315,
13.01480660082));
#26380=CARTESIAN_POINT('Ctrl Pts',(0.00956344330796528,1.86973816150673,
13.3158275547878));
#26381=CARTESIAN_POINT('Ctrl Pts',(0.0439246129546704,1.86977391645042,
13.7455383573357));
#26382=CARTESIAN_POINT('Ctrl Pts',(0.0684683055948698,1.7947899917414,14.0450459514158));
#26383=CARTESIAN_POINT('Ctrl Pts',(0.0979207365840127,1.65451257187983,
14.3836645907943));
#26384=CARTESIAN_POINT('Ctrl Pts',(0.129827536933279,1.44816401155227,14.7281533863918));
#26385=CARTESIAN_POINT('Ctrl Pts',(0.178914922159187,0.978801466284751,
15.1326460137714));
#26386=CARTESIAN_POINT('Ctrl Pts',(0.242728523014966,0.226646269966196,
15.4238627618682));
#26387=CARTESIAN_POINT('Ctrl Pts',(0.289361538971896,-0.375848970264699,
15.3653346814543));
#26388=CARTESIAN_POINT('Ctrl Pts',(0.32863144714602,-0.827308050222727,
15.177932788993));
#26389=CARTESIAN_POINT('Ctrl Pts',(0.348266401236533,-1.0438478212656,15.0621743080247));
#26390=CARTESIAN_POINT('Ctrl Pts',(0.367901355336211,-1.2336431249768,14.9064098355125));
#26391=CARTESIAN_POINT('Ctrl Pts',(0.38262757094342,-1.36322719731575,14.7767950409474));
#26392=CARTESIAN_POINT('Ctrl Pts',(0.397353786419115,-1.48646694621212,
14.6408499027268));
#26393=CARTESIAN_POINT('Ctrl Pts',(0.42189747912613,-1.65691087093242,14.3856350125846));
#26394=CARTESIAN_POINT('Ctrl Pts',(0.461167387277872,-1.84503571034646,
13.9319536706252));
#26395=CARTESIAN_POINT('Ctrl Pts',(0.497982926319137,-1.8908345576629,13.4672176837265));
#26396=CARTESIAN_POINT('Ctrl Pts',(0.527435357166049,-1.82782027363552,
13.1050857826764));
#26397=CARTESIAN_POINT('Ctrl Pts',(0.542161572784617,-1.77891817099809,
12.9284119001505));
#26398=CARTESIAN_POINT('Ctrl Pts',(0.549524680568676,-1.74801698741632,
12.8420167796121));
#26399=CARTESIAN_POINT('Ctrl Pts',(0.574068373172529,-1.63109018601349,
12.5598944683743));
#26400=CARTESIAN_POINT('Ctrl Pts',(0.59370332730294,-1.49274070366298,12.3527265616716));
#26401=CARTESIAN_POINT('Ctrl Pts',(0.628064496895538,-1.19036130281273,
12.0503873706824));
#26402=CARTESIAN_POINT('Ctrl Pts',(0.657516927975823,-0.892775905160294,
11.8300118089703));
#26403=CARTESIAN_POINT('Ctrl Pts',(0.716421790282611,-0.194895950072102,
11.5791698109191));
#26404=CARTESIAN_POINT('Ctrl Pts',(0.760600437033626,0.375864414459618,
11.6346135405221));
#26405=CARTESIAN_POINT('Ctrl Pts',(0.807233452943446,0.912000931911337,
11.8571720039664));
#26406=CARTESIAN_POINT('Ctrl Pts',(0.84159462251798,1.27808999763,12.0894130635292));
#26407=CARTESIAN_POINT('Ctrl Pts',(0.905408223341798,1.77570289947956,12.7245370657824));
#26408=CARTESIAN_POINT('Ctrl Pts',(0.969221824234544,1.93730196525167,13.5370235308092));
#26409=CARTESIAN_POINT('Ctrl Pts',(1.03303542504725,1.72055885411322,14.3141844798476));
#26410=CARTESIAN_POINT('Ctrl Pts',(1.06739659462448,1.47124045864297,14.6689027806501));
#26411=CARTESIAN_POINT('Ctrl Pts',(1.10912087208633,1.10403141746053,15.0360354618146));
#26412=CARTESIAN_POINT('Ctrl Pts',(1.1532995188661,0.618097747792482,15.3269653632982));
#26413=CARTESIAN_POINT('Ctrl Pts',(1.21711311969197,-0.187895466307751,
15.4060883879997));
#26414=CARTESIAN_POINT('Ctrl Pts',(1.26620050476972,-0.783682821932288,
15.2252935184613));
#26415=CARTESIAN_POINT('Ctrl Pts',(1.30056167435797,-1.14087952499533,14.9863526540441));
#26416=CARTESIAN_POINT('Ctrl Pts',(1.31528788989013,-1.27682775871608,14.8631392072867));
#26417=CARTESIAN_POINT('Ctrl Pts',(1.32265099775196,-1.34162708887353,14.7983479183875));
#26418=CARTESIAN_POINT('Ctrl Pts',(1.33246847476781,-1.42588961157989,14.709829197654));
#26419=CARTESIAN_POINT('Ctrl Pts',(1.35701216743962,-1.61423505890897,14.4683984701231));
#26420=CARTESIAN_POINT('Ctrl Pts',(1.40364518340993,-1.86590481711679,13.9381409687645));
#26421=CARTESIAN_POINT('Ctrl Pts',(1.46255004559483,-1.90289456011376,13.1838600527939));
#26422=CARTESIAN_POINT('Ctrl Pts',(1.52636364633265,-1.59232869850008,12.4358289376896));
#26423=CARTESIAN_POINT('Ctrl Pts',(1.58772287784506,-1.04221690767433,11.8852653514821));
#26424=CARTESIAN_POINT('Ctrl Pts',(1.65153647850482,-0.282903885450296,
11.5922810835848));
#26425=CARTESIAN_POINT('Ctrl Pts',(1.71780444848671,0.559852308259102,11.6545246982156));
#26426=CARTESIAN_POINT('Ctrl Pts',(1.78407241868674,1.29518426159801,12.0711103352848));
#26427=CARTESIAN_POINT('Ctrl Pts',(1.82825106535847,1.61949044289959,12.5317224786145));
#26428=CARTESIAN_POINT('Ctrl Pts',(1.85361288095202,1.74029071256228,12.8233096457127));
#26429=CARTESIAN_POINT('Ctrl Pts',(1.85729443485987,1.7564305234626,12.8662155716377));
#26430=CARTESIAN_POINT('Ctrl Pts',(1.86220317435584,1.77583158789889,12.9241421695384));
#26431=CARTESIAN_POINT('Ctrl Pts',(1.86874815193976,1.80042917108278,13.0017983055331));
#26432=CARTESIAN_POINT('Ctrl Pts',(1.87979283487919,1.83386347459296,13.135289209121));
#26433=CARTESIAN_POINT('Ctrl Pts',(1.89451901327258,1.86078214523026,13.3167955468064));
#26434=CARTESIAN_POINT('Ctrl Pts',(1.90433651893123,1.86677935000811,13.4389688837803));
#26435=CARTESIAN_POINT('Ctrl Pts',(1.92888023892041,1.86678190805501,13.7444357101596));
#26436=CARTESIAN_POINT('Ctrl Pts',(1.9485150734491,1.8181503635251,13.9886715771723));
#26437=CARTESIAN_POINT('Ctrl Pts',(1.97060448617354,1.71298620579008,14.2426695760738));
#26438=CARTESIAN_POINT('Ctrl Pts',(1.99514830924029,1.58920678796943,14.5220153067922));
#26439=CARTESIAN_POINT('Ctrl Pts',(2.03932655870192,1.24261702068429,14.9659420203183));
#26440=CARTESIAN_POINT('Ctrl Pts',(2.10314071900831,0.528409678047588,15.347741546511));
#26441=CARTESIAN_POINT('Ctrl Pts',(2.16695382561945,-0.282949484886631,
15.4076465636485));
#26442=CARTESIAN_POINT('Ctrl Pts',(2.23567600035159,-1.10090827734288,15.0924424888951));
#26443=CARTESIAN_POINT('Ctrl Pts',(2.30194578184805,-1.6715898090538,14.4625725258841));
#26444=CARTESIAN_POINT('Ctrl Pts',(2.36575487307431,-1.90597096237174,13.6879468659033));
#26445=CARTESIAN_POINT('Ctrl Pts',(2.43448724036195,-1.82145805582818,12.8193214271364));
#26446=CARTESIAN_POINT('Ctrl Pts',(2.50073595296765,-1.34391225562139,12.104238216233));
#26447=CARTESIAN_POINT('Ctrl Pts',(2.56465195236451,-0.63999730751846,11.7070280736045));
#26448=CARTESIAN_POINT('Ctrl Pts',(2.59908792453329,-0.212295699473147,
11.6329768668928));
#26449=CARTESIAN_POINT('Ctrl Pts',(2.61633167011827,0.00284556929259513,
11.6332663792972));
#26450=CARTESIAN_POINT('Ctrl Pts',(-3.03402225960255,0.920169500289213,
12.1508069720949));
#26451=CARTESIAN_POINT('Ctrl Pts',(-3.02958637493129,0.960060201874113,
12.1780263141219));
#26452=CARTESIAN_POINT('Ctrl Pts',(-3.00306118536422,1.1915446741207,12.3512259484075));
#26453=CARTESIAN_POINT('Ctrl Pts',(-2.97408149750605,1.39040704521766,12.6059785856818));
#26454=CARTESIAN_POINT('Ctrl Pts',(-2.94953785715269,1.49860681286232,12.8504237378315));
#26455=CARTESIAN_POINT('Ctrl Pts',(-2.92744856963118,1.59068454416991,13.072587592917));
#26456=CARTESIAN_POINT('Ctrl Pts',(-2.90781356757833,1.63313005912254,13.2863194450445));
#26457=CARTESIAN_POINT('Ctrl Pts',(-2.88326988588137,1.63312353621953,13.553521441343));
#26458=CARTESIAN_POINT('Ctrl Pts',(-2.87345242031875,1.62786623540166,13.6604114149956));
#26459=CARTESIAN_POINT('Ctrl Pts',(-2.85872618992664,1.60430567893626,13.8191933720227));
#26460=CARTESIAN_POINT('Ctrl Pts',(-2.84768153693031,1.57504838849142,13.9359780710016));
#26461=CARTESIAN_POINT('Ctrl Pts',(-2.84113654943735,1.55352166107146,14.0039114130109));
#26462=CARTESIAN_POINT('Ctrl Pts',(-2.83622781122445,1.53655095176889,14.0545888622835));
#26463=CARTESIAN_POINT('Ctrl Pts',(-2.83254625727853,1.52241574345267,14.0921204234963));
#26464=CARTESIAN_POINT('Ctrl Pts',(-2.80718444145174,1.41678309361852,14.347226232301));
#26465=CARTESIAN_POINT('Ctrl Pts',(-2.76300579467544,1.1329635040614,14.7501457186005));
#26466=CARTESIAN_POINT('Ctrl Pts',(-2.6967378246562,0.489672671131416,15.114548514947));
#26467=CARTESIAN_POINT('Ctrl Pts',(-2.63046985464307,-0.247633377770316,
15.1689412363303));
#26468=CARTESIAN_POINT('Ctrl Pts',(-2.56665625390239,-0.911884404744357,
14.912574079968));
#26469=CARTESIAN_POINT('Ctrl Pts',(-2.50529702242643,-1.39312343471216,
14.4308757228267));
#26470=CARTESIAN_POINT('Ctrl Pts',(-2.44148342171928,-1.66473450900518,
13.7764493906401));
#26471=CARTESIAN_POINT('Ctrl Pts',(-2.38257855943633,-1.63236162107275,
13.1165653158355));
#26472=CARTESIAN_POINT('Ctrl Pts',(-2.33594554353368,-1.41209346995343,
12.6526975531263));
#26473=CARTESIAN_POINT('Ctrl Pts',(-2.31140185087204,-1.24738462820272,
12.441488964872));
#26474=CARTESIAN_POINT('Ctrl Pts',(-2.30158437381822,-1.17361718385254,
12.3640600256991));
#26475=CARTESIAN_POINT('Ctrl Pts',(-2.29422126594484,-1.11693960792093,
12.3073698470986));
#26476=CARTESIAN_POINT('Ctrl Pts',(-2.27949505045088,-0.997986048126505,
12.1996129366123));
#26477=CARTESIAN_POINT('Ctrl Pts',(-2.24513388086172,-0.685485933856807,
11.990568875841));
#26478=CARTESIAN_POINT('Ctrl Pts',(-2.19604649576334,-0.164254747381628,
11.8324394379657));
#26479=CARTESIAN_POINT('Ctrl Pts',(-2.13223289491963,0.540869967667105,
11.9017559617062));
#26480=CARTESIAN_POINT('Ctrl Pts',(-2.08805424818418,0.96595860097193,12.15620272179));
#26481=CARTESIAN_POINT('Ctrl Pts',(-2.04632997072101,1.28720491445197,12.4775422504944));
#26482=CARTESIAN_POINT('Ctrl Pts',(-2.01196880112813,1.50523979116393,12.787800305018));
#26483=CARTESIAN_POINT('Ctrl Pts',(-1.9481552002848,1.69484966835682,13.4677675453008));
#26484=CARTESIAN_POINT('Ctrl Pts',(-1.88434159947337,1.55342731976602,14.1785043884778));
#26485=CARTESIAN_POINT('Ctrl Pts',(-1.82052799863252,1.11799586960201,14.734156071574));
#26486=CARTESIAN_POINT('Ctrl Pts',(-1.78616682903858,0.797785855142485,
14.9372200074867));
#26487=CARTESIAN_POINT('Ctrl Pts',(-1.73953381311012,0.328667738149594,
15.1320217157569));
#26488=CARTESIAN_POINT('Ctrl Pts',(-1.69535516636144,-0.170611178336508,
15.1804155041868));
#26489=CARTESIAN_POINT('Ctrl Pts',(-1.63645030412725,-0.781168837678439,
14.9608972194216));
#26490=CARTESIAN_POINT('Ctrl Pts',(-1.60699787298018,-1.04147077861518,
14.7681600649693));
#26491=CARTESIAN_POINT('Ctrl Pts',(-1.57263670339236,-1.30600071406174,
14.5035081513716));
#26492=CARTESIAN_POINT('Ctrl Pts',(-1.55300174932564,-1.42706109438727,
14.3224484754254));
#26493=CARTESIAN_POINT('Ctrl Pts',(-1.52845805663552,-1.52927263928429,
14.0754974223444));
#26494=CARTESIAN_POINT('Ctrl Pts',(-1.5210949488129,-1.55633041503445,13.9999388879625));
#26495=CARTESIAN_POINT('Ctrl Pts',(-1.50636873335532,-1.59905869561866,
13.8453662892381));
#26496=CARTESIAN_POINT('Ctrl Pts',(-1.47691630227588,-1.6542250679665,13.5285538081163));
#26497=CARTESIAN_POINT('Ctrl Pts',(-1.44010076338987,-1.61409287864128,
13.1219913011565));
#26498=CARTESIAN_POINT('Ctrl Pts',(-1.40083085520029,-1.44947263129895,
12.7251021192302));
#26499=CARTESIAN_POINT('Ctrl Pts',(-1.37628716255761,-1.30035750492487,
12.5018492233465));
#26500=CARTESIAN_POINT('Ctrl Pts',(-1.36156094704064,-1.19252072049869,
12.3829141693026));
#26501=CARTESIAN_POINT('Ctrl Pts',(-1.34683473141102,-1.07915009456125,
12.2695686129219));
#26502=CARTESIAN_POINT('Ctrl Pts',(-1.32719977733342,-0.913103031170408,
12.133210596805));
#26503=CARTESIAN_POINT('Ctrl Pts',(-1.30756482324941,-0.723643206763342,
12.0320965600779));
#26504=CARTESIAN_POINT('Ctrl Pts',(-1.26829491508155,-0.328701273622561,
11.8679559538835));
#26505=CARTESIAN_POINT('Ctrl Pts',(-1.22166189909103,0.198416733304813,
11.8169893707361));
#26506=CARTESIAN_POINT('Ctrl Pts',(-1.157848298264,0.856403344125254,12.0717207142664));
#26507=CARTESIAN_POINT('Ctrl Pts',(-1.10876091305799,1.26700075008309,12.4256347119853));
#26508=CARTESIAN_POINT('Ctrl Pts',(-1.07685411269456,1.44749324226499,12.7270434153079));
#26509=CARTESIAN_POINT('Ctrl Pts',(-1.04740168167682,1.57019859096341,13.0232635734239));
#26510=CARTESIAN_POINT('Ctrl Pts',(-1.0228579890047,1.63578404034369,13.2853111623653));
#26511=CARTESIAN_POINT('Ctrl Pts',(-0.993405557890351,1.63571078832615,
13.6075244739282));
#26512=CARTESIAN_POINT('Ctrl Pts',(-0.968861865215506,1.59644882660007,
13.8721669546422));
#26513=CARTESIAN_POINT('Ctrl Pts',(-0.954135649719787,1.54969090536267,
14.0263393865899));
#26514=CARTESIAN_POINT('Ctrl Pts',(-0.941863803395456,1.49855089459867,
14.1497739523841));
#26515=CARTESIAN_POINT('Ctrl Pts',(-0.936955064818857,1.47689087177173,
14.1986510834065));
#26516=CARTESIAN_POINT('Ctrl Pts',(-0.927137587735728,1.42880164807781,
14.2941407780118));
#26517=CARTESIAN_POINT('Ctrl Pts',(-0.909957002971033,1.33255530220944,
14.4548060833212));
#26518=CARTESIAN_POINT('Ctrl Pts',(-0.895230787466278,1.23029481064996,
14.579294205637));
#26519=CARTESIAN_POINT('Ctrl Pts',(-0.858415248587724,0.947092495740584,
14.8629563894098));
#26520=CARTESIAN_POINT('Ctrl Pts',(-0.804419124905459,0.416471133153839,
15.1631213076161));
#26521=CARTESIAN_POINT('Ctrl Pts',(-0.720970569978194,-0.525431236881228,
15.140193552971));
#26522=CARTESIAN_POINT('Ctrl Pts',(-0.630158907329698,-1.38487944782349,
14.566900993129));
#26523=CARTESIAN_POINT('Ctrl Pts',(-0.566345306486509,-1.63374111356011,
13.8741088568859));
#26524=CARTESIAN_POINT('Ctrl Pts',(-0.497622967298252,-1.63370556065679,
13.1257367092235));
#26525=CARTESIAN_POINT('Ctrl Pts',(-0.433809366452732,-1.3847789726291,
12.4329685854038));
#26526=CARTESIAN_POINT('Ctrl Pts',(-0.342997703809482,-0.52527584557229,
11.8597571249176));
#26527=CARTESIAN_POINT('Ctrl Pts',(-0.259549148874224,0.416626540888193,
11.836920727128));
#26528=CARTESIAN_POINT('Ctrl Pts',(-0.205553025194717,0.947221216760767,
12.1371347585086));
#26529=CARTESIAN_POINT('Ctrl Pts',(-0.168737486325147,1.23039239167878,
12.4208275322826));
#26530=CARTESIAN_POINT('Ctrl Pts',(-0.156465640055685,1.31561190938362,
12.5245660427945));
#26531=CARTESIAN_POINT('Ctrl Pts',(-0.141739424519946,1.40137424309293,
12.6600952641544));
#26532=CARTESIAN_POINT('Ctrl Pts',(-0.131921947526936,1.45408325127083,
12.7531152215987));
#26533=CARTESIAN_POINT('Ctrl Pts',(-0.124558839702545,1.48838774933109,
12.8256813917505));
#26534=CARTESIAN_POINT('Ctrl Pts',(-0.114741362533611,1.52928697674707,
12.9244326285369));
#26535=CARTESIAN_POINT('Ctrl Pts',(-0.100015147029465,1.58337337161512,
13.0755740476735));
#26536=CARTESIAN_POINT('Ctrl Pts',(-0.0754714543489009,1.63572924411331,
13.3389245508721));
#26537=CARTESIAN_POINT('Ctrl Pts',(-0.0411102847817865,1.63575335187083,
13.7148439986148));
#26538=CARTESIAN_POINT('Ctrl Pts',(-0.0165665921072617,1.5701561760943,
13.9768836663726));
#26539=CARTESIAN_POINT('Ctrl Pts',(0.0128858389111597,1.44742050019548,
14.2730929097655));
#26540=CARTESIAN_POINT('Ctrl Pts',(0.0447926392720795,1.26690003118422,
14.5744844766074));
#26541=CARTESIAN_POINT('Ctrl Pts',(0.0938800244804459,0.856268351960268,
14.9283599556911));
#26542=CARTESIAN_POINT('Ctrl Pts',(0.157693625306139,0.198257586748516,
15.1830290881431));
#26543=CARTESIAN_POINT('Ctrl Pts',(0.204326641297953,-0.328855799025312,
15.132012690545));
#26544=CARTESIAN_POINT('Ctrl Pts',(0.243596549465899,-0.723782207149813,
14.9678346732507));
#26545=CARTESIAN_POINT('Ctrl Pts',(0.263231503548857,-0.913232470143678,
14.8667027120325));
#26546=CARTESIAN_POINT('Ctrl Pts',(0.282866457627509,-1.07926662259235,
14.7303289658635));
#26547=CARTESIAN_POINT('Ctrl Pts',(0.297592673256385,-1.19262651054228,
14.6169726725508));
#26548=CARTESIAN_POINT('Ctrl Pts',(0.312318888772827,-1.30045202310849,
14.4980274007988));
#26549=CARTESIAN_POINT('Ctrl Pts',(0.336862581421082,-1.44954600310508,
14.2747603872182));
#26550=CARTESIAN_POINT('Ctrl Pts',(0.376132489598524,-1.61412863338867,
13.8778556113047));
#26551=CARTESIAN_POINT('Ctrl Pts',(0.412948028495775,-1.65422231886617,
13.4712893453838));
#26552=CARTESIAN_POINT('Ctrl Pts',(0.442400459570104,-1.59902591563155,
13.1544820886784));
#26553=CARTESIAN_POINT('Ctrl Pts',(0.457126675029423,-1.55628298468981,
12.9999135484931));
#26554=CARTESIAN_POINT('Ctrl Pts',(0.464489782851631,-1.52921804275104,
12.9243575754456));
#26555=CARTESIAN_POINT('Ctrl Pts',(0.489033475541114,-1.42698310993751,
12.6774162249364));
#26556=CARTESIAN_POINT('Ctrl Pts',(0.508668429607991,-1.305905545711,12.4963680285754));
#26557=CARTESIAN_POINT('Ctrl Pts',(0.543029599196515,-1.04135054659198,
12.2317411943687));
#26558=CARTESIAN_POINT('Ctrl Pts',(0.572482030342974,-0.781030328084433,
12.0390287250993));
#26559=CARTESIAN_POINT('Ctrl Pts',(0.631386892576705,-0.170451869762501,
11.8195683188816));
#26560=CARTESIAN_POINT('Ctrl Pts',(0.675565539326545,0.328822445454624,
11.8680094482727));
#26561=CARTESIAN_POINT('Ctrl Pts',(0.722198555253912,0.79792211316962,12.062855618652));
#26562=CARTESIAN_POINT('Ctrl Pts',(0.756559724849884,1.11811286227706,12.2659499226733));
#26563=CARTESIAN_POINT('Ctrl Pts',(0.82037332568896,1.55349164464191,12.8216428751273));
#26564=CARTESIAN_POINT('Ctrl Pts',(0.884186926500656,1.69484661024464,13.5323931254781));
#26565=CARTESIAN_POINT('Ctrl Pts',(0.948000527344836,1.5051722882597,14.2123423996626));
#26566=CARTESIAN_POINT('Ctrl Pts',(0.982361696939161,1.28710799282076,14.5225797792344));
#26567=CARTESIAN_POINT('Ctrl Pts',(1.02408597439874,0.965831243986841,14.8438888609862));
#26568=CARTESIAN_POINT('Ctrl Pts',(1.0682646211369,0.540718491046902,15.0982953355625));
#26569=CARTESIAN_POINT('Ctrl Pts',(1.13207822197524,-0.164412771655819,
15.1675450274765));
#26570=CARTESIAN_POINT('Ctrl Pts',(1.1811656070763,-0.685628935442496,15.0093662035735));
#26571=CARTESIAN_POINT('Ctrl Pts',(1.2155267766664,-0.9981092245177,14.8002925280399));
#26572=CARTESIAN_POINT('Ctrl Pts',(1.23025299216004,-1.11705256006795,14.6925243471944));
#26573=CARTESIAN_POINT('Ctrl Pts',(1.23761610003377,-1.17372476231246,14.6358287944356));
#26574=CARTESIAN_POINT('Ctrl Pts',(1.24743357708706,-1.24748486299388,14.5583928713913));
#26575=CARTESIAN_POINT('Ctrl Pts',(1.27197726974902,-1.41217366984488,14.3471686686388));
#26576=CARTESIAN_POINT('Ctrl Pts',(1.31861028565164,-1.63239775437311,13.8832801106741));
#26577=CARTESIAN_POINT('Ctrl Pts',(1.37751514793352,-1.66470802437629,13.2233930149844));
#26578=CARTESIAN_POINT('Ctrl Pts',(1.44132874864127,-1.39303462659156,12.5689926739555));
#26579=CARTESIAN_POINT('Ctrl Pts',(1.50268798011341,-0.911749558144166,
12.0873402447523));
#26580=CARTESIAN_POINT('Ctrl Pts',(1.56650158085077,-0.247473676131264,
11.8310365165478));
#26581=CARTESIAN_POINT('Ctrl Pts',(1.63276955086017,0.489828424940365,11.8855001177392));
#26582=CARTESIAN_POINT('Ctrl Pts',(1.69903752086455,1.1330858275586,12.2499648183537));
#26583=CARTESIAN_POINT('Ctrl Pts',(1.7432161676295,1.4168696997825,12.6529132192007));
#26584=CARTESIAN_POINT('Ctrl Pts',(1.76857798345518,1.52247870518676,12.9080295053983));
#26585=CARTESIAN_POINT('Ctrl Pts',(1.77225953740107,1.53661037226812,12.9455623561621));
#26586=CARTESIAN_POINT('Ctrl Pts',(1.77716827561365,1.55357633118333,12.9962415414666));
#26587=CARTESIAN_POINT('Ctrl Pts',(1.78371326310664,1.57509655384721,13.0641767165963));
#26588=CARTESIAN_POINT('Ctrl Pts',(1.79475791609898,1.60434347759022,13.1809651080057));
#26589=CARTESIAN_POINT('Ctrl Pts',(1.80948414649115,1.62788896182785,13.3397487002929));
#26590=CARTESIAN_POINT('Ctrl Pts',(1.819301612048,1.63313712936035,13.4466409112928));
#26591=CARTESIAN_POINT('Ctrl Pts',(1.84384529374514,1.63311844824755,13.7138391645349));
#26592=CARTESIAN_POINT('Ctrl Pts',(1.8634802957282,1.59066474212537,13.9275836013987));
#26593=CARTESIAN_POINT('Ctrl Pts',(1.8855695832519,1.49856463863765,14.1497336983763));
#26594=CARTESIAN_POINT('Ctrl Pts',(1.91011322357714,1.39035745604533,14.394184386848));
#26595=CARTESIAN_POINT('Ctrl Pts',(1.9542920295924,1.08705021048906,14.7824621967109));
#26596=CARTESIAN_POINT('Ctrl Pts',(2.01810540570555,0.462273209156912,15.1165143307525));
#26597=CARTESIAN_POINT('Ctrl Pts',(2.08191920435414,-0.247571374664457,
15.1688755025031));
#26598=CARTESIAN_POINT('Ctrl Pts',(2.15064160895298,-0.96311444391493,14.8931256206334));
#26599=CARTESIAN_POINT('Ctrl Pts',(2.2169088515672,-1.46241536607307,14.3420807405149));
#26600=CARTESIAN_POINT('Ctrl Pts',(2.28072425635766,-1.66732177281756,13.6643462346872));
#26601=CARTESIAN_POINT('Ctrl Pts',(2.34944263886444,-1.59359430353533,12.9045702858734));
#26602=CARTESIAN_POINT('Ctrl Pts',(2.41571836748289,-1.17545546442057,12.2787031132114));
#26603=CARTESIAN_POINT('Ctrl Pts',(2.47959749132094,-0.560059618033885,
11.9315903996426));
#26604=CARTESIAN_POINT('Ctrl Pts',(2.51403518517295,-0.185684347821608,
11.86658222976));
#26605=CARTESIAN_POINT('Ctrl Pts',(2.53129700762356,0.00248888451629452,
11.8668984646848));
#26606=CARTESIAN_POINT('Ctrl Pts',(-3.11905722816867,0.788556068408818,
12.3438412372351));
#26607=CARTESIAN_POINT('Ctrl Pts',(-3.1146213644059,0.822744462661041,12.3671622765409));
#26608=CARTESIAN_POINT('Ctrl Pts',(-3.08809626028157,1.02109524199808,12.515601306046));
#26609=CARTESIAN_POINT('Ctrl Pts',(-3.05911620734098,1.19148646818497,12.7339291160136));
#26610=CARTESIAN_POINT('Ctrl Pts',(-3.0345727496855,1.28423698062874,12.9433793370522));
#26611=CARTESIAN_POINT('Ctrl Pts',(-3.012483587381,1.36309551648216,13.1337811072441));
#26612=CARTESIAN_POINT('Ctrl Pts',(-2.99284841780566,1.39950709934089,13.316912415425));
#26613=CARTESIAN_POINT('Ctrl Pts',(-2.96830477441331,1.3994903573956,13.5459004268723));
#26614=CARTESIAN_POINT('Ctrl Pts',(-2.95848734894396,1.39498429573084,13.6374947293668));
#26615=CARTESIAN_POINT('Ctrl Pts',(-2.94376106655668,1.3747906388216,13.7735640779168));
#26616=CARTESIAN_POINT('Ctrl Pts',(-2.93271644350277,1.34971611395508,13.8736390201562));
#26617=CARTESIAN_POINT('Ctrl Pts',(-2.92617144610105,1.3312687232855,13.9318544049706));
#26618=CARTESIAN_POINT('Ctrl Pts',(-2.92126270917083,1.31672200136771,13.975280722022));
#26619=CARTESIAN_POINT('Ctrl Pts',(-2.91758115518753,1.30461397165259,14.0074442312418));
#26620=CARTESIAN_POINT('Ctrl Pts',(-2.89221933912803,1.21405681112827,14.2260429153886));
#26621=CARTESIAN_POINT('Ctrl Pts',(-2.84804069224887,0.970866105212703,
14.571324307522));
#26622=CARTESIAN_POINT('Ctrl Pts',(-2.78177272242044,0.419579819813183,
14.8835800117351));
#26623=CARTESIAN_POINT('Ctrl Pts',(-2.71550475237441,-0.212238228752434,
14.9301775586545));
#26624=CARTESIAN_POINT('Ctrl Pts',(-2.65169115155633,-0.781460863156941,
14.7104725350107));
#26625=CARTESIAN_POINT('Ctrl Pts',(-2.59033192011683,-1.19383767178126,
14.2976774875137));
#26626=CARTESIAN_POINT('Ctrl Pts',(-2.52651831944052,-1.42659490494421,
13.7368649239659));
#26627=CARTESIAN_POINT('Ctrl Pts',(-2.46761345705901,-1.39882228600251,
13.1713879038669));
#26628=CARTESIAN_POINT('Ctrl Pts',(-2.42098044122426,-1.21008384706513,
12.7738815820048));
#26629=CARTESIAN_POINT('Ctrl Pts',(-2.39643674857055,-1.0688970240368,12.5928949266493));
#26630=CARTESIAN_POINT('Ctrl Pts',(-2.38661927148008,-1.00570170912655,
12.5265419204679));
#26631=CARTESIAN_POINT('Ctrl Pts',(-2.37925616359409,-0.957123856235339,
12.4779685781114));
#26632=CARTESIAN_POINT('Ctrl Pts',(-2.36452994813932,-0.855190907485222,
12.3856175840845));
#26633=CARTESIAN_POINT('Ctrl Pts',(-2.33016877854912,-0.587389200609479,
12.206500313161));
#26634=CARTESIAN_POINT('Ctrl Pts',(-2.2810813934289,-0.14072084325576,12.0710044028659));
#26635=CARTESIAN_POINT('Ctrl Pts',(-2.21726779257138,0.463522436140825,
12.13039969068));
#26636=CARTESIAN_POINT('Ctrl Pts',(-2.1730891458758,0.827796642395821,12.3485019022086));
#26637=CARTESIAN_POINT('Ctrl Pts',(-2.13136486841596,1.10306977224913,12.6238173312992));
#26638=CARTESIAN_POINT('Ctrl Pts',(-2.09700369880523,1.28993205121074,12.8897320616277));
#26639=CARTESIAN_POINT('Ctrl Pts',(-2.03319009793237,1.45238162030186,13.4724009101037));
#26640=CARTESIAN_POINT('Ctrl Pts',(-1.96937649720154,1.3311736718366,14.0814808009882));
#26641=CARTESIAN_POINT('Ctrl Pts',(-1.9055628963443,0.958048639865271,14.5576091879427));
#26642=CARTESIAN_POINT('Ctrl Pts',(-1.87120172672977,0.683608478280005,
14.7316558797277));
#26643=CARTESIAN_POINT('Ctrl Pts',(-1.82456871078427,0.281628953814897,
14.8985184663949));
#26644=CARTESIAN_POINT('Ctrl Pts',(-1.78039006403628,-0.146247864930105,
14.9400120756112));
#26645=CARTESIAN_POINT('Ctrl Pts',(-1.72148520187501,-0.669437462685373,
14.7518963321265));
#26646=CARTESIAN_POINT('Ctrl Pts',(-1.6920327706614,-0.892507874178498,
14.5866913693728));
#26647=CARTESIAN_POINT('Ctrl Pts',(-1.65767160107852,-1.11918184099976,
14.3599554485608));
#26648=CARTESIAN_POINT('Ctrl Pts',(-1.6380366470776,-1.22290134327235,14.2047088389408));
#26649=CARTESIAN_POINT('Ctrl Pts',(-1.61349295429772,-1.31051403112513,
13.9931440110592));
#26650=CARTESIAN_POINT('Ctrl Pts',(-1.60612984643543,-1.33368570763948,
13.9283824504914));
#26651=CARTESIAN_POINT('Ctrl Pts',(-1.59140363114421,-1.37031719534642,
13.7959253448278));
#26652=CARTESIAN_POINT('Ctrl Pts',(-1.56195119981817,-1.41755613457247,
13.5244343938463));
#26653=CARTESIAN_POINT('Ctrl Pts',(-1.52513566111425,-1.38317257118645,
13.1760325375352));
#26654=CARTESIAN_POINT('Ctrl Pts',(-1.48586575285738,-1.24209919728576,
12.8359260637791));
#26655=CARTESIAN_POINT('Ctrl Pts',(-1.46132206029344,-1.11430546792535,
12.6446105506962));
#26656=CARTESIAN_POINT('Ctrl Pts',(-1.44659584473411,-1.02189885312362,
12.5426982172715));
#26657=CARTESIAN_POINT('Ctrl Pts',(-1.43186962908097,-0.924742834190651,
12.445552486113));
#26658=CARTESIAN_POINT('Ctrl Pts',(-1.4122346750253,-0.782445427376674,
12.3287514970302));
#26659=CARTESIAN_POINT('Ctrl Pts',(-1.39259972094758,-0.620093737820679,
12.2420415398033));
#26660=CARTESIAN_POINT('Ctrl Pts',(-1.35332981278393,-0.281636263334788,
12.1014932572049));
#26661=CARTESIAN_POINT('Ctrl Pts',(-1.30669679676423,0.17006225243843,12.0577388887696));
#26662=CARTESIAN_POINT('Ctrl Pts',(-1.24288319596633,0.733918023717241,
12.2760823434877));
#26663=CARTESIAN_POINT('Ctrl Pts',(-1.19379581077855,1.08576568076314,12.5793672935782));
#26664=CARTESIAN_POINT('Ctrl Pts',(-1.16188901039935,1.24043405633174,12.8376505666888));
#26665=CARTESIAN_POINT('Ctrl Pts',(-1.13243657935689,1.34557535185587,13.0915089017486));
#26666=CARTESIAN_POINT('Ctrl Pts',(-1.10789288665632,1.40177585596813,13.3160602501166));
#26667=CARTESIAN_POINT('Ctrl Pts',(-1.07844045558897,1.40170600578177,13.5921830605853));
#26668=CARTESIAN_POINT('Ctrl Pts',(-1.05389676288062,1.36805606273619,13.8189634607861));
#26669=CARTESIAN_POINT('Ctrl Pts',(-1.03917054741413,1.32798180613147,13.9510799754394));
#26670=CARTESIAN_POINT('Ctrl Pts',(-1.02689870111988,1.2841590185032,14.0568565549943));
#26671=CARTESIAN_POINT('Ctrl Pts',(-1.02198996255573,1.26559216632164,14.0987374408959));
#26672=CARTESIAN_POINT('Ctrl Pts',(-1.01217248533102,1.22438985324433,14.1805732328973));
#26673=CARTESIAN_POINT('Ctrl Pts',(-0.994991900669837,1.14189010858655,
14.318235939556));
#26674=CARTESIAN_POINT('Ctrl Pts',(-0.980265685167946,1.05428522966142,
14.424938644877));
#26675=CARTESIAN_POINT('Ctrl Pts',(-0.943450146291098,0.811546794400914,
14.6679737141968));
#26676=CARTESIAN_POINT('Ctrl Pts',(-0.889454022585424,0.356873734737775,
14.9252444568342));
#26677=CARTESIAN_POINT('Ctrl Pts',(-0.806005467631,-0.450314585645347,14.9054960137471));
#26678=CARTESIAN_POINT('Ctrl Pts',(-0.715193805062034,-1.1867759283488,
14.4142524142852));
#26679=CARTESIAN_POINT('Ctrl Pts',(-0.651380204193698,-1.40002055950109,
13.8205412187184));
#26680=CARTESIAN_POINT('Ctrl Pts',(-0.582657864972822,-1.39997497623281,
13.1792599528847));
#26681=CARTESIAN_POINT('Ctrl Pts',(-0.518844264092402,-1.18664613215041,
12.585579291146));
#26682=CARTESIAN_POINT('Ctrl Pts',(-0.428032601549523,-0.450114970484183,
12.094440696976));
#26683=CARTESIAN_POINT('Ctrl Pts',(-0.344584046560112,0.357075207419309,
12.0748081953586));
#26684=CARTESIAN_POINT('Ctrl Pts',(-0.290587922865303,0.811711418684831,
12.3321442177636));
#26685=CARTESIAN_POINT('Ctrl Pts',(-0.253772384029816,1.05441415769597,
12.5752148091857));
#26686=CARTESIAN_POINT('Ctrl Pts',(-0.241500537777015,1.12740810231216,
12.6641430019001));
#26687=CARTESIAN_POINT('Ctrl Pts',(-0.226774322131749,1.20091854863098,
12.7802681504964));
#26688=CARTESIAN_POINT('Ctrl Pts',(-0.216956845311384,1.24607566691818,
12.8599900719375));
#26689=CARTESIAN_POINT('Ctrl Pts',(-0.20959373744137,1.2754769729967,12.9221704644164));
#26690=CARTESIAN_POINT('Ctrl Pts',(-0.199776260242763,1.31052185463136,
13.0067969486097));
#26691=CARTESIAN_POINT('Ctrl Pts',(-0.185050044740512,1.35686671439483,
13.1363178263613));
#26692=CARTESIAN_POINT('Ctrl Pts',(-0.160506352005717,1.40172752399848,
13.3619931910802));
#26693=CARTESIAN_POINT('Ctrl Pts',(-0.126145182518741,1.40174073623245,
13.6841386578387));
#26694=CARTESIAN_POINT('Ctrl Pts',(-0.101601489808506,1.34551942205644,
13.908681333809));
#26695=CARTESIAN_POINT('Ctrl Pts',(-0.072149058762419,1.240340560484,14.1625249842377));
#26696=CARTESIAN_POINT('Ctrl Pts',(-0.0402422583875128,1.08563555157988,
14.4207864531663));
#26697=CARTESIAN_POINT('Ctrl Pts',(0.00884512680068361,0.733744263865131,
14.7240215729494));
#26698=CARTESIAN_POINT('Ctrl Pts',(0.0726587275984066,0.169857268657729,
14.9422849993108));
#26699=CARTESIAN_POINT('Ctrl Pts',(0.119291743623238,-0.281835160449523,
14.8984664262192));
#26700=CARTESIAN_POINT('Ctrl Pts',(0.158561651785726,-0.620272668097745,
14.7578700153382));
#26701=CARTESIAN_POINT('Ctrl Pts',(0.178196605860647,-0.78261203441093,
14.6711369668772));
#26702=CARTESIAN_POINT('Ctrl Pts',(0.197831559918322,-0.924892829664357,
14.5543157409681));
#26703=CARTESIAN_POINT('Ctrl Pts',(0.212557775569124,-1.02203502447049,
14.4571561863723));
#26704=CARTESIAN_POINT('Ctrl Pts',(0.227283991125964,-1.11442713372381,
14.3552307026066));
#26705=CARTESIAN_POINT('Ctrl Pts',(0.251827683716028,-1.24219364322043,
14.1638970162314));
#26706=CARTESIAN_POINT('Ctrl Pts',(0.291097591917902,-1.38321860530081,
13.8237704716166));
#26707=CARTESIAN_POINT('Ctrl Pts',(0.327913130672672,-1.41755260632012,
13.4753637614126));
#26708=CARTESIAN_POINT('Ctrl Pts',(0.357365561974734,-1.3702750193093,13.2038795417306));
#26709=CARTESIAN_POINT('Ctrl Pts',(0.372091777274669,-1.33362467627383,
13.0714276531952));
#26710=CARTESIAN_POINT('Ctrl Pts',(0.379454885135005,-1.31044378071783,
13.0066693926929));
#26711=CARTESIAN_POINT('Ctrl Pts',(0.403998577910522,-1.22280097664773,
12.7951170424732));
#26712=CARTESIAN_POINT('Ctrl Pts',(0.423633531913512,-1.11905938241173,
12.6398852089949));
#26713=CARTESIAN_POINT('Ctrl Pts',(0.457994701498026,-0.892353142221933,
12.4131815643651));
#26714=CARTESIAN_POINT('Ctrl Pts',(0.487447132710345,-0.66925921781202,
12.2480083652116));
#26715=CARTESIAN_POINT('Ctrl Pts',(0.546351994870958,-0.146042848998138,
12.0599671108965));
#26716=CARTESIAN_POINT('Ctrl Pts',(0.590530641619899,0.281828057894891,
12.1015216368775));
#26717=CARTESIAN_POINT('Ctrl Pts',(0.637163657564549,0.683783822214472,
12.2684414511951));
#26718=CARTESIAN_POINT('Ctrl Pts',(0.67152482718102,0.958199202226451,12.4425272138518));
#26719=CARTESIAN_POINT('Ctrl Pts',(0.735338428036789,1.33125644777318,12.9187087178781));
#26720=CARTESIAN_POINT('Ctrl Pts',(0.799152028767091,1.45237768566226,13.5278058611153));
#26721=CARTESIAN_POINT('Ctrl Pts',(0.862965629641978,1.28984517196703,14.1104515813163));
#26722=CARTESIAN_POINT('Ctrl Pts',(0.897326799254478,1.10294504271018,14.3763397106384));
#26723=CARTESIAN_POINT('Ctrl Pts',(0.93905107671091,0.827632726114737,14.6516159527686));
#26724=CARTESIAN_POINT('Ctrl Pts',(0.983229723407923,0.463327489001278,
14.8696663168148));
#26725=CARTESIAN_POINT('Ctrl Pts',(1.04704332425977,-0.140924226201367,
14.9289755924517));
#26726=CARTESIAN_POINT('Ctrl Pts',(1.09613070938308,-0.587573258897613,
14.793416119096));
#26727=CARTESIAN_POINT('Ctrl Pts',(1.13049187897521,-0.855349451405556,
14.614260734394));
#26728=CARTESIAN_POINT('Ctrl Pts',(1.14521809443,-0.957269247127293,14.5218952336081));
#26729=CARTESIAN_POINT('Ctrl Pts',(1.15258120231606,-1.00584018321824,14.4733149769537));
#26730=CARTESIAN_POINT('Ctrl Pts',(1.16239867940624,-1.06902604877892,14.4069529765618));
#26731=CARTESIAN_POINT('Ctrl Pts',(1.18694237205925,-1.21018709119309,14.2259462340624));
#26732=CARTESIAN_POINT('Ctrl Pts',(1.23357538789392,-1.39886884688823,13.8284131208944));
#26733=CARTESIAN_POINT('Ctrl Pts',(1.29248025027432,-1.42656089820532,13.2629322038511));
#26734=CARTESIAN_POINT('Ctrl Pts',(1.35629385095077,-1.19372354209459,12.7021530167634));
#26735=CARTESIAN_POINT('Ctrl Pts',(1.41765308238647,-0.781287592708931,
12.2894169897012));
#26736=CARTESIAN_POINT('Ctrl Pts',(1.4814666832016,-0.212033131166725,12.0697934600203));
#26737=CARTESIAN_POINT('Ctrl Pts',(1.5477346532436,0.419779491092501,12.1164819470839));
#26738=CARTESIAN_POINT('Ctrl Pts',(1.61400262305684,0.971022431641602,12.4288170433353));
#26739=CARTESIAN_POINT('Ctrl Pts',(1.65818126992488,1.21416646777651,12.774135089221));
#26740=CARTESIAN_POINT('Ctrl Pts',(1.68354308598506,1.30469303591977,12.9927470969396));
#26741=CARTESIAN_POINT('Ctrl Pts',(1.68722463996854,1.31679653379992,13.0249123682082));
#26742=CARTESIAN_POINT('Ctrl Pts',(1.69213337689861,1.33133708616498,13.0683407618607));
#26743=CARTESIAN_POINT('Ctrl Pts',(1.69867837429913,1.34977620422811,13.1265588187185));
#26744=CARTESIAN_POINT('Ctrl Pts',(1.70972299734984,1.37483700647468,13.2266376630337));
#26745=CARTESIAN_POINT('Ctrl Pts',(1.72444927973632,1.3950115748963,13.3627102778487));
#26746=CARTESIAN_POINT('Ctrl Pts',(1.73426670520185,1.39950513574301,13.4543055384039));
#26747=CARTESIAN_POINT('Ctrl Pts',(1.75881034858134,1.39949125223529,13.6832950819811));
#26748=CARTESIAN_POINT('Ctrl Pts',(1.77844551810905,1.36306231207927,13.86642843719));
#26749=CARTESIAN_POINT('Ctrl Pts',(1.80053468040288,1.28417749446346,14.0568198428129));
#26750=CARTESIAN_POINT('Ctrl Pts',(1.82507813804813,1.19140871647897,14.26626307035));
#26751=CARTESIAN_POINT('Ctrl Pts',(1.8692575005794,0.931514766722571,14.5990322547947));
#26752=CARTESIAN_POINT('Ctrl Pts',(1.93307009276571,0.396108856903805,14.8852542750114));
#26753=CARTESIAN_POINT('Ctrl Pts',(1.99688458337269,-0.212197990694309,
14.9301300790991));
#26754=CARTESIAN_POINT('Ctrl Pts',(2.06560721862504,-0.825356962352493,
14.693797228026));
#26755=CARTESIAN_POINT('Ctrl Pts',(2.13187192198348,-1.25322327405421,14.2216085927445));
#26756=CARTESIAN_POINT('Ctrl Pts',(2.19569364256406,-1.42879756538438,13.6407601664489));
#26757=CARTESIAN_POINT('Ctrl Pts',(2.26439803871978,-1.36567344200437,12.989813124798));
#26758=CARTESIAN_POINT('Ctrl Pts',(2.33070078887648,-1.00708473766736,12.453274391172));
#26759=CARTESIAN_POINT('Ctrl Pts',(2.39454303239137,-0.480177286341525,
12.1560745526581));
#26760=CARTESIAN_POINT('Ctrl Pts',(2.42898246554838,-0.159333681076682,
12.1002778996127));
#26761=CARTESIAN_POINT('Ctrl Pts',(2.44626234486601,0.00213567231429039,
12.1005293499708));
#26762=CARTESIAN_POINT('',(2.62767578687551,5.23816853614149E-11,11.6014703833234));
#26763=CARTESIAN_POINT('Origin',(2.82743338823081,4.5822835629755E-15,11.8));
#26764=CARTESIAN_POINT('Origin',(6.2,0.,14.67));
#26765=CARTESIAN_POINT('',(6.2,-1.4328367550024E-16,12.33));
#26766=CARTESIAN_POINT('Origin',(6.2,0.,13.5));
#26767=CARTESIAN_POINT('Origin',(6.16,0.,13.5));
#26768=CARTESIAN_POINT('',(6.12,-1.53080849893419E-16,12.25));
#26769=CARTESIAN_POINT('Origin',(6.12,0.,13.5));
#26770=CARTESIAN_POINT('',(6.16,-1.4818226269683E-16,12.29));
#26771=CARTESIAN_POINT('Origin',(5.3225,0.,13.5));
#26772=CARTESIAN_POINT('',(4.525,-1.53080849893419E-16,12.25));
#26773=CARTESIAN_POINT('Origin',(4.525,0.,13.5));
#26774=CARTESIAN_POINT('',(5.3225,-1.53080849893419E-16,12.25));
#26775=CARTESIAN_POINT('Origin',(4.525,0.,15.));
#26776=CARTESIAN_POINT('',(4.525,-1.83697019872103E-16,12.));
#26777=CARTESIAN_POINT('Origin',(4.525,0.,13.5));
#26778=CARTESIAN_POINT('Origin',(4.5,0.,13.5));
#26779=CARTESIAN_POINT('',(4.475,-1.8982025386784E-16,11.95));
#26780=CARTESIAN_POINT('Origin',(4.475,0.,13.5));
#26781=CARTESIAN_POINT('',(4.5,-1.86758636869971E-16,11.975));
#26782=CARTESIAN_POINT('Origin',(4.2875,0.,13.5));
#26783=CARTESIAN_POINT('',(4.1,-1.8982025386784E-16,11.95));
#26784=CARTESIAN_POINT('Origin',(4.1,0.,13.5));
#26785=CARTESIAN_POINT('',(4.2875,-1.8982025386784E-16,11.95));
#26786=CARTESIAN_POINT('Origin',(4.1,0.,14.9));
#26787=CARTESIAN_POINT('Origin',(-4.1,0.,15.05));
#26788=CARTESIAN_POINT('',(-4.1,-1.8982025386784E-16,11.95));
#26789=CARTESIAN_POINT('Origin',(-4.1,0.,13.5));
#26790=CARTESIAN_POINT('Origin',(-4.2875,0.,13.5));
#26791=CARTESIAN_POINT('',(-4.475,-1.8982025386784E-16,11.95));
#26792=CARTESIAN_POINT('Origin',(-4.475,0.,13.5));
#26793=CARTESIAN_POINT('',(-4.2875,-1.8982025386784E-16,11.95));
#26794=CARTESIAN_POINT('Origin',(-4.5,0.,13.5));
#26795=CARTESIAN_POINT('',(-4.525,-1.83697019872103E-16,12.));
#26796=CARTESIAN_POINT('',(-4.5,1.86758636869971E-16,11.975));
#26797=CARTESIAN_POINT('Origin',(-4.525,0.,13.5));
#26798=CARTESIAN_POINT('Origin',(-4.525,0.,14.75));
#26799=CARTESIAN_POINT('',(-4.525,-1.53080849893419E-16,12.25));
#26800=CARTESIAN_POINT('Origin',(-4.525,0.,13.5));
#26801=CARTESIAN_POINT('Origin',(-5.8225,0.,13.5));
#26802=CARTESIAN_POINT('',(-7.12,-1.53080849893419E-16,12.25));
#26803=CARTESIAN_POINT('Origin',(-7.12,0.,13.5));
#26804=CARTESIAN_POINT('',(-5.8225,-1.53080849893419E-16,12.25));
#26805=CARTESIAN_POINT('Origin',(-7.16,0.,13.5));
#26806=CARTESIAN_POINT('',(-7.2,-1.4328367550024E-16,12.33));
#26807=CARTESIAN_POINT('',(-7.16,1.4818226269683E-16,12.29));
#26808=CARTESIAN_POINT('Origin',(-7.2,0.,13.5));
#26809=CARTESIAN_POINT('Origin',(-7.2,0.,13.5));
#26810=CARTESIAN_POINT('',(0.,0.,0.));
#26811=CARTESIAN_POINT('Origin',(0.,-1.275,7.2));
#26812=CARTESIAN_POINT('',(-4.04133443718627E-16,-1.25,3.9));
#26813=CARTESIAN_POINT('',(-4.04133443718627E-16,-1.25,10.5));
#26814=CARTESIAN_POINT('Origin',(0.,-1.25,7.2));
#26815=CARTESIAN_POINT('',(-4.10256677714363E-16,-1.3,10.55));
#26816=CARTESIAN_POINT('',(-4.07195060716495E-16,-1.275,10.525));
#26817=CARTESIAN_POINT('Origin',(0.,-1.3,7.2));
#26818=CARTESIAN_POINT('Origin',(0.,-1.25,7.2));
#26819=CARTESIAN_POINT('Origin',(0.,0.,7.2));
#26820=CARTESIAN_POINT('',(-4.04133443718627E-16,1.25,3.9));
#26821=CARTESIAN_POINT('',(-4.04133443718627E-16,0.,3.9));
#26822=CARTESIAN_POINT('',(-4.04133443718627E-16,1.25,10.5));
#26823=CARTESIAN_POINT('Origin',(0.,1.25,7.2));
#26824=CARTESIAN_POINT('Origin',(0.,1.25,7.2));
#26825=CARTESIAN_POINT('Origin',(0.,-1.3,12.05));
#26826=CARTESIAN_POINT('',(-1.16079736048698,-1.3,11.6306327026976));
#26827=CARTESIAN_POINT('',(-1.35212230766397,-1.30000000000017,11.857710302833));
#26828=CARTESIAN_POINT('Ctrl Pts',(-1.16079736048698,-1.3,11.6306327026976));
#26829=CARTESIAN_POINT('Ctrl Pts',(-1.16756547280972,-1.3,11.6361811764316));
#26830=CARTESIAN_POINT('Ctrl Pts',(-1.17433759800592,-1.30000000000001,
11.6464116794416));
#26831=CARTESIAN_POINT('Ctrl Pts',(-1.18440586374552,-1.30000000000002,
11.6613628993828));
#26832=CARTESIAN_POINT('Ctrl Pts',(-1.19298536144484,-1.30000000000003,
11.6736347004975));
#26833=CARTESIAN_POINT('Ctrl Pts',(-1.2010525651233,-1.30000000000005,11.6846776130522));
#26834=CARTESIAN_POINT('Ctrl Pts',(-1.20689949924857,-1.30000000000005,
11.6917782430971));
#26835=CARTESIAN_POINT('Ctrl Pts',(-1.21290364438206,-1.30000000000005,
11.6988352552442));
#26836=CARTESIAN_POINT('Ctrl Pts',(-1.22618519864767,-1.30000000000005,
11.7171839141227));
#26837=CARTESIAN_POINT('Ctrl Pts',(-1.24813860795808,-1.30000000000018,
11.742992785695));
#26838=CARTESIAN_POINT('Ctrl Pts',(-1.26978166142649,-1.30000000000021,
11.7689185967307));
#26839=CARTESIAN_POINT('Ctrl Pts',(-1.28621507340024,-1.30000000000022,
11.7874440086064));
#26840=CARTESIAN_POINT('Ctrl Pts',(-1.29884778522716,-1.30000000000025,
11.8011898160839));
#26841=CARTESIAN_POINT('Ctrl Pts',(-1.30959903943822,-1.30000000000028,
11.8125295228686));
#26842=CARTESIAN_POINT('Ctrl Pts',(-1.31760194267198,-1.30000000000028,
11.8218663161003));
#26843=CARTESIAN_POINT('Ctrl Pts',(-1.33044578595539,-1.30000000000034,
11.835492648863));
#26844=CARTESIAN_POINT('Ctrl Pts',(-1.34223778779766,-1.30000000000035,
11.8472929513181));
#26845=CARTESIAN_POINT('Ctrl Pts',(-1.35147403673712,-1.30000000000039,
11.857025688592));
#26846=CARTESIAN_POINT('Ctrl Pts',(-1.3521223074938,-1.30000000000039,11.8577103026533));
#26847=CARTESIAN_POINT('',(-1.85488174067955,-1.30000000000031,11.6812848300933));
#26848=CARTESIAN_POINT('Origin',(0.,-1.3,7.2));
#26849=CARTESIAN_POINT('',(-1.84783999216022,-1.3,11.390889146273));
#26850=CARTESIAN_POINT('Ctrl Pts',(-1.85488174055135,-1.29999999999962,
11.6812848304777));
#26851=CARTESIAN_POINT('Ctrl Pts',(-1.85492628499207,-1.29999999999962,
11.6802652801082));
#26852=CARTESIAN_POINT('Ctrl Pts',(-1.85520261176984,-1.29999999999962,
11.6731568182642));
#26853=CARTESIAN_POINT('Ctrl Pts',(-1.85517328864456,-1.29999999999968,
11.6601079860047));
#26854=CARTESIAN_POINT('Ctrl Pts',(-1.85677772263879,-1.29999999999968,
11.6415847248257));
#26855=CARTESIAN_POINT('Ctrl Pts',(-1.8559372933276,-1.29999999999972,11.6267230412807));
#26856=CARTESIAN_POINT('Ctrl Pts',(-1.85699869963993,-1.29999999999972,
11.6143622964798));
#26857=CARTESIAN_POINT('Ctrl Pts',(-1.85707299808147,-1.29999999999975,
11.5962359591743));
#26858=CARTESIAN_POINT('Ctrl Pts',(-1.85782405239374,-1.29999999999978,
11.5718563713308));
#26859=CARTESIAN_POINT('Ctrl Pts',(-1.85678181360665,-1.29999999999981,
11.5479686431211));
#26860=CARTESIAN_POINT('Ctrl Pts',(-1.85646792992201,-1.29999999999983,
11.5238562660423));
#26861=CARTESIAN_POINT('Ctrl Pts',(-1.85497966222552,-1.29999999999992,
11.5031261449632));
#26862=CARTESIAN_POINT('Ctrl Pts',(-1.85439311555543,-1.29999999999991,
11.4790463022061));
#26863=CARTESIAN_POINT('Ctrl Pts',(-1.85283978068161,-1.29999999999994,
11.4613539877648));
#26864=CARTESIAN_POINT('Ctrl Pts',(-1.85127630062445,-1.29999999999995,
11.4435752287495));
#26865=CARTESIAN_POINT('Ctrl Pts',(-1.84999209718951,-1.29999999999997,
11.42887504109));
#26866=CARTESIAN_POINT('Ctrl Pts',(-1.84771283470267,-1.29999999999997,
11.411322510041));
#26867=CARTESIAN_POINT('Ctrl Pts',(-1.84624880074883,-1.3,11.3993427675272));
#26868=CARTESIAN_POINT('Ctrl Pts',(-1.84783999216022,-1.3,11.390889146273));
#26869=CARTESIAN_POINT('',(-2.05661148970878,-1.3,11.2924694059607));
#26870=CARTESIAN_POINT('',(-1.84783999216022,-1.3,11.390889146273));
#26871=CARTESIAN_POINT('',(-2.29123854954719,-1.29999999999661,11.4746609113891));
#26872=CARTESIAN_POINT('Ctrl Pts',(-2.05661148970878,-1.3,11.2924694059607));
#26873=CARTESIAN_POINT('Ctrl Pts',(-2.06438529509424,-1.3,11.2964894625547));
#26874=CARTESIAN_POINT('Ctrl Pts',(-2.07310405152088,-1.29999999999976,
11.3051109272566));
#26875=CARTESIAN_POINT('Ctrl Pts',(-2.08604767365932,-1.29999999999967,
11.3176494774367));
#26876=CARTESIAN_POINT('Ctrl Pts',(-2.09697218826213,-1.2999999999995,11.3278871439685));
#26877=CARTESIAN_POINT('Ctrl Pts',(-2.10826479557385,-1.29999999999936,
11.3380338755579));
#26878=CARTESIAN_POINT('Ctrl Pts',(-2.11798686606834,-1.29999999999925,
11.3455803565384));
#26879=CARTESIAN_POINT('Ctrl Pts',(-2.12751552334166,-1.29999999999917,
11.353305425036));
#26880=CARTESIAN_POINT('Ctrl Pts',(-2.14304910682454,-1.2999999999991,11.3675618927394));
#26881=CARTESIAN_POINT('Ctrl Pts',(-2.16816701100081,-1.29999999999791,
11.3858847423419));
#26882=CARTESIAN_POINT('Ctrl Pts',(-2.19197084033902,-1.2999999999976,11.4050757262928));
#26883=CARTESIAN_POINT('Ctrl Pts',(-2.21194072996125,-1.29999999999725,
11.4197523880556));
#26884=CARTESIAN_POINT('Ctrl Pts',(-2.22718477672532,-1.2999999999971,11.4305479831049));
#26885=CARTESIAN_POINT('Ctrl Pts',(-2.24236803062252,-1.29999999999635,
11.4413662490843));
#26886=CARTESIAN_POINT('Ctrl Pts',(-2.26249397180294,-1.29999999999583,
11.4558744789577));
#26887=CARTESIAN_POINT('Ctrl Pts',(-2.27915093949768,-1.29999999999501,
11.4666835569465));
#26888=CARTESIAN_POINT('Ctrl Pts',(-2.29043543302869,-1.29999999999466,
11.4741293822945));
#26889=CARTESIAN_POINT('Ctrl Pts',(-2.29123854934731,-1.29999999999464,
11.4746609111665));
#26890=CARTESIAN_POINT('',(-2.74606098184731,-1.30000000000043,11.1977054774281));
#26891=CARTESIAN_POINT('Origin',(0.,-1.3,7.2));
#26892=CARTESIAN_POINT('',(-2.67879510330291,-1.3,10.9151206262376));
#26893=CARTESIAN_POINT('Ctrl Pts',(-2.74606098180075,-1.30000000000052,
11.1977054778115));
#26894=CARTESIAN_POINT('Ctrl Pts',(-2.74589257547025,-1.30000000000052,
11.1966989891297));
#26895=CARTESIAN_POINT('Ctrl Pts',(-2.74468488647704,-1.30000000000052,
11.1896884723293));
#26896=CARTESIAN_POINT('Ctrl Pts',(-2.74194313468275,-1.30000000000045,
11.1769309522019));
#26897=CARTESIAN_POINT('Ctrl Pts',(-2.73966116432262,-1.30000000000044,
11.1584789426609));
#26898=CARTESIAN_POINT('Ctrl Pts',(-2.73574909450226,-1.30000000000039,
11.1441167944129));
#26899=CARTESIAN_POINT('Ctrl Pts',(-2.73421733091279,-1.30000000000039,
11.1318054961784));
#26900=CARTESIAN_POINT('Ctrl Pts',(-2.73052114637807,-1.30000000000036,
11.1140598974805));
#26901=CARTESIAN_POINT('Ctrl Pts',(-2.72618669292026,-1.3000000000003,11.0900570416951));
#26902=CARTESIAN_POINT('Ctrl Pts',(-2.72020047826994,-1.30000000000025,
11.0669081106693));
#26903=CARTESIAN_POINT('Ctrl Pts',(-2.71488010558258,-1.30000000000023,
11.0433879560159));
#26904=CARTESIAN_POINT('Ctrl Pts',(-2.70911402584219,-1.30000000000012,
11.0234204248471));
#26905=CARTESIAN_POINT('Ctrl Pts',(-2.70353383063923,-1.30000000000011,
10.9999887293472));
#26906=CARTESIAN_POINT('Ctrl Pts',(-2.69833596654804,-1.30000000000008,
10.983006039634));
#26907=CARTESIAN_POINT('Ctrl Pts',(-2.69311023072124,-1.30000000000006,
10.9659408795863));
#26908=CARTESIAN_POINT('Ctrl Pts',(-2.6887977871431,-1.30000000000005,10.9518289492138));
#26909=CARTESIAN_POINT('Ctrl Pts',(-2.6829189620321,-1.30000000000003,10.9351338813408));
#26910=CARTESIAN_POINT('Ctrl Pts',(-2.67899628993004,-1.3,10.9237203428817));
#26911=CARTESIAN_POINT('Ctrl Pts',(-2.67879510330291,-1.3,10.9151206262376));
#26912=CARTESIAN_POINT('',(-2.86254182811346,-1.3,10.7754455583364));
#26913=CARTESIAN_POINT('',(-2.67879510330291,-1.3,10.9151206262376));
#26914=CARTESIAN_POINT('',(-3.12979327626143,-1.29999999999956,10.9049823276056));
#26915=CARTESIAN_POINT('Ctrl Pts',(-2.86254182811346,-1.3,10.7754455583364));
#26916=CARTESIAN_POINT('Ctrl Pts',(-2.87098157396347,-1.3,10.7777615020268));
#26917=CARTESIAN_POINT('Ctrl Pts',(-2.88130799910635,-1.29999999999995,
10.7843752712055));
#26918=CARTESIAN_POINT('Ctrl Pts',(-2.89657675896672,-1.29999999999994,
10.7939475114029));
#26919=CARTESIAN_POINT('Ctrl Pts',(-2.90939733936898,-1.29999999999989,
10.8016830781138));
#26920=CARTESIAN_POINT('Ctrl Pts',(-2.92255067730088,-1.29999999999988,
10.8092626647234));
#26921=CARTESIAN_POINT('Ctrl Pts',(-2.93364134797163,-1.29999999999984,
10.8146096561709));
#26922=CARTESIAN_POINT('Ctrl Pts',(-2.94454127932451,-1.29999999999984,
10.8202105050095));
#26923=CARTESIAN_POINT('Ctrl Pts',(-2.96280984633302,-1.29999999999977,
10.8308072518358));
#26924=CARTESIAN_POINT('Ctrl Pts',(-2.99104878850524,-1.29999999999969,
10.8436673431889));
#26925=CARTESIAN_POINT('Ctrl Pts',(-3.01834269857632,-1.29999999999954,
10.8574591123471));
#26926=CARTESIAN_POINT('Ctrl Pts',(-3.04099809512408,-1.29999999999947,
10.8675872666515));
#26927=CARTESIAN_POINT('Ctrl Pts',(-3.05375053744491,-1.29999999999936,
10.8732488581604));
#26928=CARTESIAN_POINT('Ctrl Pts',(-3.06242055860219,-1.29999999999936,
10.8768361729214));
#26929=CARTESIAN_POINT('Ctrl Pts',(-3.06815466520311,-1.29999999999934,
10.879276631911));
#26930=CARTESIAN_POINT('Ctrl Pts',(-3.07523784637398,-1.29999999999934,
10.8824189159387));
#26931=CARTESIAN_POINT('Ctrl Pts',(-3.0835896561049,-1.29999999999931,10.8863527724723));
#26932=CARTESIAN_POINT('Ctrl Pts',(-3.10080971693874,-1.29999999999922,
10.893634162511));
#26933=CARTESIAN_POINT('Ctrl Pts',(-3.11640268293853,-1.29999999999909,
10.899617481341));
#26934=CARTESIAN_POINT('Ctrl Pts',(-3.12890931112008,-1.29999999999898,
10.9046274841548));
#26935=CARTESIAN_POINT('Ctrl Pts',(-3.12979327620054,-1.29999999999897,
10.9049823275812));
#26936=CARTESIAN_POINT('',(-3.51715555718115,-1.30000000000215,10.5394702475537));
#26937=CARTESIAN_POINT('Origin',(0.,-1.3,7.2));
#26938=CARTESIAN_POINT('',(-3.39267401414619,-1.3,10.2769835077089));
#26939=CARTESIAN_POINT('Ctrl Pts',(-3.51715323192894,-1.30000000000206,
10.5394644239228));
#26940=CARTESIAN_POINT('Ctrl Pts',(-3.5167751163261,-1.30000000000204,10.5385174606946));
#26941=CARTESIAN_POINT('Ctrl Pts',(-3.51412021591145,-1.30000000000197,
10.5319251070686));
#26942=CARTESIAN_POINT('Ctrl Pts',(-3.51014479419029,-1.30000000000177,
10.5226552577284));
#26943=CARTESIAN_POINT('Ctrl Pts',(-3.50627111332769,-1.30000000000177,
10.51267580137));
#26944=CARTESIAN_POINT('Ctrl Pts',(-3.50442220663016,-1.30000000000176,
10.5076132694342));
#26945=CARTESIAN_POINT('Ctrl Pts',(-3.50332286786836,-1.30000000000176,
10.5047548383451));
#26946=CARTESIAN_POINT('Ctrl Pts',(-3.49802816243003,-1.30000000000167,
10.4921711193908));
#26947=CARTESIAN_POINT('Ctrl Pts',(-3.48397706310364,-1.30000000000133,
10.4576138699548));
#26948=CARTESIAN_POINT('Ctrl Pts',(-3.46377916361693,-1.30000000000061,
10.4138557361379));
#26949=CARTESIAN_POINT('Ctrl Pts',(-3.44488287358282,-1.30000000000045,
10.3765723257512));
#26950=CARTESIAN_POINT('Ctrl Pts',(-3.43444272475379,-1.30000000000036,
10.3549066020539));
#26951=CARTESIAN_POINT('Ctrl Pts',(-3.4258722715172,-1.30000000000023,10.3393534519172));
#26952=CARTESIAN_POINT('Ctrl Pts',(-3.41721009436118,-1.30000000000019,
10.3237432942191));
#26953=CARTESIAN_POINT('Ctrl Pts',(-3.41007224859402,-1.30000000000012,
10.3108264414936));
#26954=CARTESIAN_POINT('Ctrl Pts',(-3.4008540684495,-1.30000000000008,10.2957145443332));
#26955=CARTESIAN_POINT('Ctrl Pts',(-3.39465878599086,-1.3,10.2853534708595));
#26956=CARTESIAN_POINT('Ctrl Pts',(-3.39267401414619,-1.3,10.2769835077089));
#26957=CARTESIAN_POINT('',(-3.54336535262991,-1.3,10.1021575829215));
#26958=CARTESIAN_POINT('',(-3.39267401414619,-1.3,10.2769835077089));
#26959=CARTESIAN_POINT('',(-3.83170332429324,-1.30000000000003,10.1733061790875));
#26960=CARTESIAN_POINT('Ctrl Pts',(-3.54336535262991,-1.3,10.1021575829215));
#26961=CARTESIAN_POINT('Ctrl Pts',(-3.55210218155242,-1.3,10.1026681958559));
#26962=CARTESIAN_POINT('Ctrl Pts',(-3.56359990094073,-1.3,10.1069613837583));
#26963=CARTESIAN_POINT('Ctrl Pts',(-3.58052453593301,-1.3,10.1131512829018));
#26964=CARTESIAN_POINT('Ctrl Pts',(-3.5947099922829,-1.30000000000002,10.1179996604393));
#26965=CARTESIAN_POINT('Ctrl Pts',(-3.6091175106494,-1.30000000000001,10.122729572639));
#26966=CARTESIAN_POINT('Ctrl Pts',(-3.62418184228238,-1.30000000000001,
10.1262166523165));
#26967=CARTESIAN_POINT('Ctrl Pts',(-3.64724297519883,-1.30000000000001,
10.1335969392187));
#26968=CARTESIAN_POINT('Ctrl Pts',(-3.67397691592533,-1.30000000000002,
10.1404382070294));
#26969=CARTESIAN_POINT('Ctrl Pts',(-3.70101609997419,-1.30000000000003,
10.1467971727461));
#26970=CARTESIAN_POINT('Ctrl Pts',(-3.71878759513276,-1.30000000000003,
10.1514335393157));
#26971=CARTESIAN_POINT('Ctrl Pts',(-3.73401038434217,-1.30000000000004,
10.1545818971217));
#26972=CARTESIAN_POINT('Ctrl Pts',(-3.74458338262459,-1.30000000000004,
10.1569162443582));
#26973=CARTESIAN_POINT('Ctrl Pts',(-3.75070071224819,-1.30000000000004,
10.1581177840759));
#26974=CARTESIAN_POINT('Ctrl Pts',(-3.76607211082019,-1.30000000000004,
10.1609742455453));
#26975=CARTESIAN_POINT('Ctrl Pts',(-3.79159121371509,-1.30000000000004,
10.166868855423));
#26976=CARTESIAN_POINT('Ctrl Pts',(-3.81751020820494,-1.30000000000005,
10.1708055317158));
#26977=CARTESIAN_POINT('Ctrl Pts',(-3.83076636902639,-1.30000000000006,
10.1731399950341));
#26978=CARTESIAN_POINT('Ctrl Pts',(-3.83170332419124,-1.30000000000006,
10.1733061790695));
#26979=CARTESIAN_POINT('',(-4.13458745388079,-1.30000000000005,9.73526890803374));
#26980=CARTESIAN_POINT('Origin',(0.,-1.3,7.2));
#26981=CARTESIAN_POINT('',(-3.95827679071515,-1.3,9.50436744488836));
#26982=CARTESIAN_POINT('Ctrl Pts',(-4.13458133514455,-1.30000000000001,
9.73525952971052));
#26983=CARTESIAN_POINT('Ctrl Pts',(-4.13402211860173,-1.30000000000001,
9.73440240093009));
#26984=CARTESIAN_POINT('Ctrl Pts',(-4.12678253409857,-1.30000000000001,
9.7232969089459));
#26985=CARTESIAN_POINT('Ctrl Pts',(-4.11635470812671,-1.30000000000001,
9.70687190739251));
#26986=CARTESIAN_POINT('Ctrl Pts',(-4.10202300360556,-1.30000000000001,
9.68751099507706));
#26987=CARTESIAN_POINT('Ctrl Pts',(-4.0922355048406,-1.30000000000001,9.6718006770301));
#26988=CARTESIAN_POINT('Ctrl Pts',(-4.08088288391458,-1.29999999999999,
9.65800792817637));
#26989=CARTESIAN_POINT('Ctrl Pts',(-4.07272838886398,-1.3,9.64488009164316));
#26990=CARTESIAN_POINT('Ctrl Pts',(-4.06138621253064,-1.3,9.63106202969796));
#26991=CARTESIAN_POINT('Ctrl Pts',(-4.04716422159604,-1.3,9.61149186781034));
#26992=CARTESIAN_POINT('Ctrl Pts',(-4.02999794901947,-1.3,9.59094278729833));
#26993=CARTESIAN_POINT('Ctrl Pts',(-4.01715577671304,-1.3,9.57427610753465));
#26994=CARTESIAN_POINT('Ctrl Pts',(-4.01049046738455,-1.3,9.56625472662842));
#26995=CARTESIAN_POINT('Ctrl Pts',(-4.00659335599276,-1.3,9.56178696274009));
#26996=CARTESIAN_POINT('Ctrl Pts',(-4.00072166766439,-1.3,9.55514362730498));
#26997=CARTESIAN_POINT('Ctrl Pts',(-3.99198996060064,-1.3,9.54496247330593));
#26998=CARTESIAN_POINT('Ctrl Pts',(-3.98223602054924,-1.3,9.53389065551681));
#26999=CARTESIAN_POINT('Ctrl Pts',(-3.97422670435759,-1.3,9.52527149172313));
#27000=CARTESIAN_POINT('Ctrl Pts',(-3.96589174422145,-1.3,9.51663189767497));
#27001=CARTESIAN_POINT('Ctrl Pts',(-3.96073119938755,-1.3,9.50955037962426));
#27002=CARTESIAN_POINT('Ctrl Pts',(-3.95827679071515,-1.3,9.50436744488836));
#27003=CARTESIAN_POINT('',(-4.06932680828303,-1.3,9.30203139503569));
#27004=CARTESIAN_POINT('',(-3.95827679071515,-1.3,9.50436744488836));
#27005=CARTESIAN_POINT('',(-4.36615556544121,-1.29999999999999,9.31167837948083));
#27006=CARTESIAN_POINT('Ctrl Pts',(-4.06932680828303,-1.3,9.30203139503569));
#27007=CARTESIAN_POINT('Ctrl Pts',(-4.07797887893014,-1.3,9.30071436097879));
#27008=CARTESIAN_POINT('Ctrl Pts',(-4.09011797873215,-1.3,9.30252364569424));
#27009=CARTESIAN_POINT('Ctrl Pts',(-4.10795972277923,-1.3,9.30505955869223));
#27010=CARTESIAN_POINT('Ctrl Pts',(-4.12284323459949,-1.3,9.30685293138333));
#27011=CARTESIAN_POINT('Ctrl Pts',(-4.13791931153359,-1.3,9.30848411321574));
#27012=CARTESIAN_POINT('Ctrl Pts',(-4.15337942684459,-1.3,9.30876317496534));
#27013=CARTESIAN_POINT('Ctrl Pts',(-4.177471105744,-1.3,9.3111874364075));
#27014=CARTESIAN_POINT('Ctrl Pts',(-4.2050428800799,-1.29999999999999,9.31232210003487));
#27015=CARTESIAN_POINT('Ctrl Pts',(-4.23281323594795,-1.29999999999999,
9.31292054619228));
#27016=CARTESIAN_POINT('Ctrl Pts',(-4.25116029379092,-1.29999999999997,
9.31376081103432));
#27017=CARTESIAN_POINT('Ctrl Pts',(-4.26670499109767,-1.29999999999998,
9.31367542306717));
#27018=CARTESIAN_POINT('Ctrl Pts',(-4.27753228080538,-1.29999999999998,
9.31376050379772));
#27019=CARTESIAN_POINT('Ctrl Pts',(-4.28376574468317,-1.29999999999998,
9.31366392579328));
#27020=CARTESIAN_POINT('Ctrl Pts',(-4.29939513404249,-1.29999999999998,
9.31326205030653));
#27021=CARTESIAN_POINT('Ctrl Pts',(-4.32558216921343,-1.29999999999998,
9.31372186269267));
#27022=CARTESIAN_POINT('Ctrl Pts',(-4.35175307577712,-1.29999999999997,
9.31218345558017));
#27023=CARTESIAN_POINT('Ctrl Pts',(-4.36520473933644,-1.29999999999997,
9.31171063592312));
#27024=CARTESIAN_POINT('Ctrl Pts',(-4.36615556533234,-1.29999999999997,
9.31167837948453));
#27025=CARTESIAN_POINT('',(-4.57138092645551,-1.29999999999936,8.82016913292346));
#27026=CARTESIAN_POINT('Origin',(0.,-1.3,7.2));
#27027=CARTESIAN_POINT('',(-4.35088387761047,-1.3,8.63103946714436));
#27028=CARTESIAN_POINT('Ctrl Pts',(-4.57137830133415,-1.29999999999872,
8.82016777346892));
#27029=CARTESIAN_POINT('Ctrl Pts',(-4.5706499710557,-1.29999999999873,8.81945142449021));
#27030=CARTESIAN_POINT('Ctrl Pts',(-4.56555294905792,-1.2999999999988,8.81448624478641));
#27031=CARTESIAN_POINT('Ctrl Pts',(-4.55583799175273,-1.29999999999884,
8.80577096598508));
#27032=CARTESIAN_POINT('Ctrl Pts',(-4.54314694081162,-1.29999999999898,
8.79218277495142));
#27033=CARTESIAN_POINT('Ctrl Pts',(-4.53154583913746,-1.29999999999902,
8.78285112053941));
#27034=CARTESIAN_POINT('Ctrl Pts',(-4.5230641316617,-1.29999999999905,8.77380443519591));
#27035=CARTESIAN_POINT('Ctrl Pts',(-4.50966808728349,-1.29999999999912,
8.76156795041169));
#27036=CARTESIAN_POINT('Ctrl Pts',(-4.48972114667047,-1.29999999999927,
8.7428644163535));
#27037=CARTESIAN_POINT('Ctrl Pts',(-4.46225757065887,-1.29999999999944,
8.71958453597246));
#27038=CARTESIAN_POINT('Ctrl Pts',(-4.43911310247342,-1.29999999999973,
8.70074230118687));
#27039=CARTESIAN_POINT('Ctrl Pts',(-4.42075431675779,-1.29999999999974,
8.68521657502575));
#27040=CARTESIAN_POINT('Ctrl Pts',(-4.4065970852679,-1.29999999999981,8.6744687837598));
#27041=CARTESIAN_POINT('Ctrl Pts',(-4.39232901723895,-1.29999999999987,
8.663754809807));
#27042=CARTESIAN_POINT('Ctrl Pts',(-4.38055136998726,-1.29999999999991,
8.65486034483265));
#27043=CARTESIAN_POINT('Ctrl Pts',(-4.36598120515464,-1.29999999999993,
8.64481132314781));
#27044=CARTESIAN_POINT('Ctrl Pts',(-4.35610142762816,-1.3,8.63787852952385));
#27045=CARTESIAN_POINT('Ctrl Pts',(-4.35088387761047,-1.3,8.63103946714436));
#27046=CARTESIAN_POINT('',(-4.41743915561768,-1.3,8.41003634852114));
#27047=CARTESIAN_POINT('',(-4.35088387761047,-1.3,8.63103946714436));
#27048=CARTESIAN_POINT('',(-4.70981757133242,-1.29999999999615,8.35763484922072));
#27049=CARTESIAN_POINT('Ctrl Pts',(-4.41743915561768,-1.3,8.41003634852114));
#27050=CARTESIAN_POINT('Ctrl Pts',(-4.42289860586251,-1.3,8.40797826829437));
#27051=CARTESIAN_POINT('Ctrl Pts',(-4.4316817112443,-1.29999999999974,8.40635777334174));
#27052=CARTESIAN_POINT('Ctrl Pts',(-4.44386598092803,-1.29999999999974,
8.40580624828125));
#27053=CARTESIAN_POINT('Ctrl Pts',(-4.45581389180353,-1.29999999999952,
8.40486348086199));
#27054=CARTESIAN_POINT('Ctrl Pts',(-4.47075640156682,-1.29999999999934,
8.4036633250798));
#27055=CARTESIAN_POINT('Ctrl Pts',(-4.48584345896485,-1.29999999999907,
8.40202163820225));
#27056=CARTESIAN_POINT('Ctrl Pts',(-4.49796178305987,-1.29999999999891,
8.39985529775274));
#27057=CARTESIAN_POINT('Ctrl Pts',(-4.51007860939437,-1.29999999999879,
8.39793835227947));
#27058=CARTESIAN_POINT('Ctrl Pts',(-4.53106911976877,-1.29999999999867,
8.39593541505635));
#27059=CARTESIAN_POINT('Ctrl Pts',(-4.56150565653829,-1.29999999999687,
8.3894994098264));
#27060=CARTESIAN_POINT('Ctrl Pts',(-4.5916993973255,-1.29999999999631,8.38463466234546));
#27061=CARTESIAN_POINT('Ctrl Pts',(-4.6159708325463,-1.29999999999587,8.37961235158075));
#27062=CARTESIAN_POINT('Ctrl Pts',(-4.63419695389511,-1.29999999999542,
8.37547771778002));
#27063=CARTESIAN_POINT('Ctrl Pts',(-4.65239690742476,-1.29999999999488,
8.37146876966047));
#27064=CARTESIAN_POINT('Ctrl Pts',(-4.67662765556342,-1.29999999999398,
8.36638064005625));
#27065=CARTESIAN_POINT('Ctrl Pts',(-4.69579249083398,-1.29999999999256,
8.36144353805949));
#27066=CARTESIAN_POINT('Ctrl Pts',(-4.70888530574064,-1.29999999999208,
8.35788592377707));
#27067=CARTESIAN_POINT('Ctrl Pts',(-4.70981757125868,-1.29999999999204,
8.3576348491941));
#27068=CARTESIAN_POINT('',(-4.80833510396185,-1.3000000000003,7.83433302999821));
#27069=CARTESIAN_POINT('Origin',(0.,-1.3,7.2));
#27070=CARTESIAN_POINT('',(-4.55333646119701,-1.3,7.69516819779691));
#27071=CARTESIAN_POINT('Ctrl Pts',(-4.80833173373481,-1.30000000000022,
7.83433088232518));
#27072=CARTESIAN_POINT('Ctrl Pts',(-4.80747027295148,-1.30000000000022,
7.83378193252291));
#27073=CARTESIAN_POINT('Ctrl Pts',(-4.80145165647202,-1.30000000000022,
7.82998687887007));
#27074=CARTESIAN_POINT('Ctrl Pts',(-4.79013869260298,-1.30000000000018,
7.82347634664022));
#27075=CARTESIAN_POINT('Ctrl Pts',(-4.77489914987298,-1.30000000000019,
7.81282546636897));
#27076=CARTESIAN_POINT('Ctrl Pts',(-4.76161182290262,-1.30000000000016,
7.80610825536316));
#27077=CARTESIAN_POINT('Ctrl Pts',(-4.75143447025795,-1.30000000000017,
7.79902289403953));
#27078=CARTESIAN_POINT('Ctrl Pts',(-4.7357871929817,-1.30000000000014,7.78983839804539));
#27079=CARTESIAN_POINT('Ctrl Pts',(-4.71238759485038,-1.30000000000014,
7.77568997553474));
#27080=CARTESIAN_POINT('Ctrl Pts',(-4.68068425748567,-1.30000000000009,
7.75862761062045));
#27081=CARTESIAN_POINT('Ctrl Pts',(-4.65412859982376,-1.30000000000005,
7.74500676190757));
#27082=CARTESIAN_POINT('Ctrl Pts',(-4.63294304514747,-1.30000000000005,
7.73363723320237));
#27083=CARTESIAN_POINT('Ctrl Pts',(-4.61686083285171,-1.30000000000004,
7.72606704168879));
#27084=CARTESIAN_POINT('Ctrl Pts',(-4.60067713755889,-1.30000000000003,
7.71855328487673));
#27085=CARTESIAN_POINT('Ctrl Pts',(-4.58730781279961,-1.30000000000002,
7.71230138859932));
#27086=CARTESIAN_POINT('Ctrl Pts',(-4.57096682812081,-1.3,7.70550102152382));
#27087=CARTESIAN_POINT('Ctrl Pts',(-4.55986191625143,-1.3,7.70077302060858));
#27088=CARTESIAN_POINT('Ctrl Pts',(-4.55333646119701,-1.3,7.69516819779691));
#27089=CARTESIAN_POINT('',(-4.57248821462698,-1.3,7.4651569071776));
#27090=CARTESIAN_POINT('',(-4.55333646119701,-1.3,7.69516819779691));
#27091=CARTESIAN_POINT('',(-4.84757993445123,-1.30000000000002,7.35319523199426));
#27092=CARTESIAN_POINT('Ctrl Pts',(-4.57248821462698,-1.3,7.4651569071776));
#27093=CARTESIAN_POINT('Ctrl Pts',(-4.57985658845472,-1.3,7.46043462252668));
#27094=CARTESIAN_POINT('Ctrl Pts',(-4.59168342474763,-1.3,7.45718163914689));
#27095=CARTESIAN_POINT('Ctrl Pts',(-4.60901429870377,-1.3,7.45223840664112));
#27096=CARTESIAN_POINT('Ctrl Pts',(-4.6233426492548,-1.3,7.44788165467972));
#27097=CARTESIAN_POINT('Ctrl Pts',(-4.63777744145292,-1.30000000000001,
7.44317884815646));
#27098=CARTESIAN_POINT('Ctrl Pts',(-4.64917211308579,-1.30000000000001,
7.43850439917718));
#27099=CARTESIAN_POINT('Ctrl Pts',(-4.66062967398901,-1.30000000000001,
7.4341698631728));
#27100=CARTESIAN_POINT('Ctrl Pts',(-4.68072279072001,-1.30000000000001,
7.427597316889));
#27101=CARTESIAN_POINT('Ctrl Pts',(-4.72058200346441,-1.30000000000001,
7.41055955717716));
#27102=CARTESIAN_POINT('Ctrl Pts',(-4.75619240536045,-1.30000000000002,
7.39667294505808));
#27103=CARTESIAN_POINT('Ctrl Pts',(-4.78159245634837,-1.30000000000002,
7.3845295394818));
#27104=CARTESIAN_POINT('Ctrl Pts',(-4.78724263544855,-1.30000000000002,
7.38189848275632));
#27105=CARTESIAN_POINT('Ctrl Pts',(-4.79573463031575,-1.30000000000002,
7.37812243727754));
#27106=CARTESIAN_POINT('Ctrl Pts',(-4.80424392564078,-1.30000000000002,
7.37453487689564));
#27107=CARTESIAN_POINT('Ctrl Pts',(-4.82116392366521,-1.30000000000002,
7.3664890641967));
#27108=CARTESIAN_POINT('Ctrl Pts',(-4.83462057271346,-1.30000000000004,
7.35948972770122));
#27109=CARTESIAN_POINT('Ctrl Pts',(-4.84672316806408,-1.30000000000005,
7.35361004877818));
#27110=CARTESIAN_POINT('Ctrl Pts',(-4.84757993437554,-1.30000000000005,
7.3531952320309));
#27111=CARTESIAN_POINT('',(-4.83515073502711,-1.30000000000003,6.82076739205056));
#27112=CARTESIAN_POINT('Origin',(0.,-1.3,7.2));
#27113=CARTESIAN_POINT('',(-4.55678639209675,-1.3,6.73765570212511));
#27114=CARTESIAN_POINT('Ctrl Pts',(-4.83515073557977,-1.30000000000001,
6.82076739235878));
#27115=CARTESIAN_POINT('Ctrl Pts',(-4.83419429812713,-1.30000000000001,
6.82040545606944));
#27116=CARTESIAN_POINT('Ctrl Pts',(-4.82180430644273,-1.30000000000001,
6.81574194544304));
#27117=CARTESIAN_POINT('Ctrl Pts',(-4.79795229094081,-1.29999999999999,
6.80742687526405));
#27118=CARTESIAN_POINT('Ctrl Pts',(-4.77218237162954,-1.3,6.79773450848217));
#27119=CARTESIAN_POINT('Ctrl Pts',(-4.75492703857423,-1.3,6.79270521874687));
#27120=CARTESIAN_POINT('Ctrl Pts',(-4.74343177047669,-1.3,6.78894839353199));
#27121=CARTESIAN_POINT('Ctrl Pts',(-4.72910106576434,-1.3,6.78356480038482));
#27122=CARTESIAN_POINT('Ctrl Pts',(-4.71179979755839,-1.3,6.77906526523394));
#27123=CARTESIAN_POINT('Ctrl Pts',(-4.6859192007466,-1.3,6.77087890474239));
#27124=CARTESIAN_POINT('Ctrl Pts',(-4.65706796695327,-1.3,6.76297007363099));
#27125=CARTESIAN_POINT('Ctrl Pts',(-4.62824128498159,-1.3,6.75514249224118));
#27126=CARTESIAN_POINT('Ctrl Pts',(-4.60795779379671,-1.3,6.75077046400056));
#27127=CARTESIAN_POINT('Ctrl Pts',(-4.59357758309321,-1.3,6.7473262596935));
#27128=CARTESIAN_POINT('Ctrl Pts',(-4.57618074025563,-1.3,6.74410801342416));
#27129=CARTESIAN_POINT('Ctrl Pts',(-4.56433455848945,-1.3,6.74178132771716));
#27130=CARTESIAN_POINT('Ctrl Pts',(-4.55678639209675,-1.3,6.73765570212511));
#27131=CARTESIAN_POINT('',(-4.52769759742429,-1.3,6.50868883662639));
#27132=CARTESIAN_POINT('',(-4.55678639209675,-1.3,6.73765570212511));
#27133=CARTESIAN_POINT('',(-4.77349769916151,-1.30000000000004,6.34196753202475));
#27134=CARTESIAN_POINT('Ctrl Pts',(-4.52769759742428,-1.3,6.50868883662639));
#27135=CARTESIAN_POINT('Ctrl Pts',(-4.53392313641892,-1.3,6.50253777416401));
#27136=CARTESIAN_POINT('Ctrl Pts',(-4.54481358953488,-1.3,6.49689772508412));
#27137=CARTESIAN_POINT('Ctrl Pts',(-4.56073742191181,-1.30000000000001,
6.48845909030186));
#27138=CARTESIAN_POINT('Ctrl Pts',(-4.57384637687987,-1.30000000000001,
6.48122083117138));
#27139=CARTESIAN_POINT('Ctrl Pts',(-4.58698656110021,-1.30000000000001,
6.47361713730408));
#27140=CARTESIAN_POINT('Ctrl Pts',(-4.5971617191533,-1.30000000000001,6.46668272213463));
#27141=CARTESIAN_POINT('Ctrl Pts',(-4.60746225289102,-1.30000000000001,
6.46004353502867));
#27142=CARTESIAN_POINT('Ctrl Pts',(-4.62576982567744,-1.30000000000001,
6.449508799198));
#27143=CARTESIAN_POINT('Ctrl Pts',(-4.65102959463077,-1.30000000000003,
6.43149214233013));
#27144=CARTESIAN_POINT('Ctrl Pts',(-4.67660141835911,-1.30000000000004,
6.4146923842508));
#27145=CARTESIAN_POINT('Ctrl Pts',(-4.69671938666191,-1.30000000000004,
6.40019410542733));
#27146=CARTESIAN_POINT('Ctrl Pts',(-4.70923780804923,-1.30000000000005,
6.39102177259885));
#27147=CARTESIAN_POINT('Ctrl Pts',(-4.71915423906947,-1.30000000000005,
6.38338868641418));
#27148=CARTESIAN_POINT('Ctrl Pts',(-4.72667488592069,-1.30000000000005,
6.37792955793699));
#27149=CARTESIAN_POINT('Ctrl Pts',(-4.73425539759128,-1.30000000000006,
6.37265708709588));
#27150=CARTESIAN_POINT('Ctrl Pts',(-4.74915526276079,-1.30000000000005,
6.36133152319305));
#27151=CARTESIAN_POINT('Ctrl Pts',(-4.76218569011346,-1.30000000000008,
6.35098992646152));
#27152=CARTESIAN_POINT('Ctrl Pts',(-4.77274896536852,-1.30000000000009,
6.34256409538153));
#27153=CARTESIAN_POINT('Ctrl Pts',(-4.77349769914136,-1.30000000000009,
6.34196753204081));
#27154=CARTESIAN_POINT('',(-4.65066919172074,-1.3000000000019,5.8238996459718));
#27155=CARTESIAN_POINT('Origin',(0.,-1.3,7.2));
#27156=CARTESIAN_POINT('',(-4.36108289177477,-1.3,5.80034987084453));
#27157=CARTESIAN_POINT('Ctrl Pts',(-4.65065521504301,-1.30000000000123,
5.82389742331003));
#27158=CARTESIAN_POINT('Ctrl Pts',(-4.64964365411225,-1.30000000000123,
5.82373656278459));
#27159=CARTESIAN_POINT('Ctrl Pts',(-4.63654304374248,-1.30000000000123,
5.82165956670231));
#27160=CARTESIAN_POINT('Ctrl Pts',(-4.61140095727319,-1.30000000000098,
5.81803205132024));
#27161=CARTESIAN_POINT('Ctrl Pts',(-4.57222382486577,-1.30000000000091,
5.81294014075723));
#27162=CARTESIAN_POINT('Ctrl Pts',(-4.54217763126687,-1.30000000000045,
5.80967119057755));
#27163=CARTESIAN_POINT('Ctrl Pts',(-4.51828305614626,-1.30000000000046,
5.8081247804399));
#27164=CARTESIAN_POINT('Ctrl Pts',(-4.49429427127261,-1.30000000000038,
5.80593985674244));
#27165=CARTESIAN_POINT('Ctrl Pts',(-4.46442169461025,-1.30000000000015,
5.80418837180128));
#27166=CARTESIAN_POINT('Ctrl Pts',(-4.43460530968231,-1.30000000000015,
5.80256316172568));
#27167=CARTESIAN_POINT('Ctrl Pts',(-4.41385708995417,-1.30000000000008,
5.80251373424002));
#27168=CARTESIAN_POINT('Ctrl Pts',(-4.39907707321173,-1.30000000000007,
5.80214342814169));
#27169=CARTESIAN_POINT('Ctrl Pts',(-4.38139208292371,-1.30000000000003,
5.80261733027065));
#27170=CARTESIAN_POINT('Ctrl Pts',(-4.36932387841423,-1.3,5.80281598958163));
#27171=CARTESIAN_POINT('Ctrl Pts',(-4.36108289177477,-1.3,5.80034987084453));
#27172=CARTESIAN_POINT('',(-4.28502486891058,-1.3,5.58243438119362));
#27173=CARTESIAN_POINT('',(-4.36108289177477,-1.3,5.80034987084453));
#27174=CARTESIAN_POINT('',(-4.49074858706858,-1.30000000000336,5.36815088613614));
#27175=CARTESIAN_POINT('Ctrl Pts',(-4.28502486891058,-1.3,5.58243438119362));
#27176=CARTESIAN_POINT('Ctrl Pts',(-4.28983548714458,-1.3,5.57512337186545));
#27177=CARTESIAN_POINT('Ctrl Pts',(-4.29926460392035,-1.30000000000005,
5.56730754668058));
#27178=CARTESIAN_POINT('Ctrl Pts',(-4.31087898979562,-1.30000000000006,
5.55775119234793));
#27179=CARTESIAN_POINT('Ctrl Pts',(-4.31756355119799,-1.30000000000007,
5.55178320730578));
#27180=CARTESIAN_POINT('Ctrl Pts',(-4.32673222276919,-1.30000000000009,
5.54396284373672));
#27181=CARTESIAN_POINT('Ctrl Pts',(-4.33567044487514,-1.30000000000012,
5.53578209594158));
#27182=CARTESIAN_POINT('Ctrl Pts',(-4.34632504743019,-1.30000000000015,
5.52463757271538));
#27183=CARTESIAN_POINT('Ctrl Pts',(-4.35515498779034,-1.30000000000018,
5.51626230029439));
#27184=CARTESIAN_POINT('Ctrl Pts',(-4.37078301239806,-1.30000000000019,
5.50197740006243));
#27185=CARTESIAN_POINT('Ctrl Pts',(-4.3895491469188,-1.30000000000043,5.48121690616271));
#27186=CARTESIAN_POINT('Ctrl Pts',(-4.41112472456535,-1.30000000000049,
5.45954571059707));
#27187=CARTESIAN_POINT('Ctrl Pts',(-4.42782422204148,-1.30000000000057,
5.44124473191616));
#27188=CARTESIAN_POINT('Ctrl Pts',(-4.44012243041892,-1.3000000000006,5.42715703615339));
#27189=CARTESIAN_POINT('Ctrl Pts',(-4.45464562208433,-1.30000000000083,
5.41105919281666));
#27190=CARTESIAN_POINT('Ctrl Pts',(-4.47094525801375,-1.30000000000091,
5.3921662715124));
#27191=CARTESIAN_POINT('Ctrl Pts',(-4.48355136291131,-1.30000000000109,
5.37693009060612));
#27192=CARTESIAN_POINT('Ctrl Pts',(-4.49013572864496,-1.30000000000116,
5.36889672578802));
#27193=CARTESIAN_POINT('Ctrl Pts',(-4.49074754412175,-1.30000000000116,
5.36815157839931));
#27194=CARTESIAN_POINT('',(-4.26288026203271,-1.30000000000046,4.88691723606622));
#27195=CARTESIAN_POINT('Origin',(0.,-1.3,7.2));
#27196=CARTESIAN_POINT('',(-3.97477914228473,-1.3,4.92421546647452));
#27197=CARTESIAN_POINT('Ctrl Pts',(-4.26288026262664,-1.30000000000002,
4.88691723612453));
#27198=CARTESIAN_POINT('Ctrl Pts',(-4.26185925374181,-1.30000000000002,
4.88697560743987));
#27199=CARTESIAN_POINT('Ctrl Pts',(-4.24864351689439,-1.30000000000002,
4.88775469182251));
#27200=CARTESIAN_POINT('Ctrl Pts',(-4.22347137391457,-1.30000000000002,
4.8898598443532));
#27201=CARTESIAN_POINT('Ctrl Pts',(-4.19598697828258,-1.30000000000001,
4.89148680791329));
#27202=CARTESIAN_POINT('Ctrl Pts',(-4.17817781145144,-1.30000000000001,
4.89391064073123));
#27203=CARTESIAN_POINT('Ctrl Pts',(-4.16614832183902,-1.30000000000001,
4.89515416503415));
#27204=CARTESIAN_POINT('Ctrl Pts',(-4.15086691685344,-1.30000000000001,
4.89606494834232));
#27205=CARTESIAN_POINT('Ctrl Pts',(-4.13323139050141,-1.30000000000001,
4.89899172467465));
#27206=CARTESIAN_POINT('Ctrl Pts',(-4.10625889988789,-1.30000000000001,
4.90204030255357));
#27207=CARTESIAN_POINT('Ctrl Pts',(-4.07668616191853,-1.30000000000001,
4.90655222883004));
#27208=CARTESIAN_POINT('Ctrl Pts',(-4.04716803737915,-1.30000000000001,
4.9111262375198));
#27209=CARTESIAN_POINT('Ctrl Pts',(-4.02686024311824,-1.30000000000001,
4.91538283693502));
#27210=CARTESIAN_POINT('Ctrl Pts',(-4.01232252274933,-1.3,4.91808539201506));
#27211=CARTESIAN_POINT('Ctrl Pts',(-3.99512086302587,-1.3,4.92222147175324));
#27212=CARTESIAN_POINT('Ctrl Pts',(-3.98335277851019,-1.3,4.92491429713412));
#27213=CARTESIAN_POINT('Ctrl Pts',(-3.97477914228473,-1.3,4.92421546647452));
#27214=CARTESIAN_POINT('',(-3.85507599179486,-1.3,4.7268753052437));
#27215=CARTESIAN_POINT('',(-3.97477914228473,-1.3,4.92421546647452));
#27216=CARTESIAN_POINT('',(-4.01183482598956,-1.30000000000004,4.47462271804852));
#27217=CARTESIAN_POINT('Ctrl Pts',(-3.85507599179486,-1.3,4.7268753052437));
#27218=CARTESIAN_POINT('Ctrl Pts',(-3.85719962537661,-1.3,4.72144101857423));
#27219=CARTESIAN_POINT('Ctrl Pts',(-3.86187573129448,-1.3,4.71383403293719));
#27220=CARTESIAN_POINT('Ctrl Pts',(-3.86961810893469,-1.3,4.70440940889751));
#27221=CARTESIAN_POINT('Ctrl Pts',(-3.87691755596589,-1.3,4.69490664118851));
#27222=CARTESIAN_POINT('Ctrl Pts',(-3.88601526735224,-1.3,4.68298671678656));
#27223=CARTESIAN_POINT('Ctrl Pts',(-3.89491361629376,-1.30000000000001,
4.67070753187996));
#27224=CARTESIAN_POINT('Ctrl Pts',(-3.90299367365694,-1.30000000000001,
4.65757823073424));
#27225=CARTESIAN_POINT('Ctrl Pts',(-3.90989779693671,-1.30000000000001,
4.64755288062265));
#27226=CARTESIAN_POINT('Ctrl Pts',(-3.92221206525842,-1.30000000000001,
4.6303305021881));
#27227=CARTESIAN_POINT('Ctrl Pts',(-3.93623661697013,-1.30000000000003,
4.60609932986893));
#27228=CARTESIAN_POINT('Ctrl Pts',(-3.95284745610302,-1.30000000000004,
4.58042969910381));
#27229=CARTESIAN_POINT('Ctrl Pts',(-3.96535170192481,-1.30000000000004,
4.55902748517642));
#27230=CARTESIAN_POINT('Ctrl Pts',(-3.97449901676931,-1.30000000000004,
4.54274237531139));
#27231=CARTESIAN_POINT('Ctrl Pts',(-3.98365558285502,-1.30000000000005,
4.52648867384939));
#27232=CARTESIAN_POINT('Ctrl Pts',(-3.99622589356068,-1.30000000000007,
4.50522626952481));
#27233=CARTESIAN_POINT('Ctrl Pts',(-4.0051093795642,-1.30000000000007,4.48739495292359));
#27234=CARTESIAN_POINT('Ctrl Pts',(-4.01138931711436,-1.30000000000008,
4.47546647684066));
#27235=CARTESIAN_POINT('Ctrl Pts',(-4.01183482595518,-1.30000000000008,
4.47462271811364));
#27236=CARTESIAN_POINT('',(-3.68874885777913,-1.30000000000003,4.05109036897819));
#27237=CARTESIAN_POINT('Origin',(0.,-1.3,7.2));
#27238=CARTESIAN_POINT('',(-3.4147584711704,-1.3,4.14754376664537));
#27239=CARTESIAN_POINT('Ctrl Pts',(-3.68874885789501,-1.29999999999998,
4.05109036897745));
#27240=CARTESIAN_POINT('Ctrl Pts',(-3.68777058327918,-1.29999999999998,
4.0513661006271));
#27241=CARTESIAN_POINT('Ctrl Pts',(-3.68094176684541,-1.29999999999998,
4.05331905207122));
#27242=CARTESIAN_POINT('Ctrl Pts',(-3.67135789241846,-1.29999999999998,
4.05637552490222));
#27243=CARTESIAN_POINT('Ctrl Pts',(-3.65953806887845,-1.29999999999998,
4.05956467038679));
#27244=CARTESIAN_POINT('Ctrl Pts',(-3.64763149426095,-1.29999999999998,
4.06262355022671));
#27245=CARTESIAN_POINT('Ctrl Pts',(-3.63356070629898,-1.29999999999998,
4.06771912618173));
#27246=CARTESIAN_POINT('Ctrl Pts',(-3.61556442432801,-1.29999999999998,
4.07212390020612));
#27247=CARTESIAN_POINT('Ctrl Pts',(-3.58711823022726,-1.29999999999998,
4.08187617918609));
#27248=CARTESIAN_POINT('Ctrl Pts',(-3.55260469525794,-1.29999999999999,
4.0930731351417));
#27249=CARTESIAN_POINT('Ctrl Pts',(-3.51930456141974,-1.29999999999999,
4.10610119875621));
#27250=CARTESIAN_POINT('Ctrl Pts',(-3.49661091395695,-1.3,4.11413655268901));
#27251=CARTESIAN_POINT('Ctrl Pts',(-3.48026786811637,-1.3,4.12106457332588));
#27252=CARTESIAN_POINT('Ctrl Pts',(-3.46382778992352,-1.3,4.12803241400126));
#27253=CARTESIAN_POINT('Ctrl Pts',(-3.45023815468816,-1.3,4.1337844199917));
#27254=CARTESIAN_POINT('Ctrl Pts',(-3.4342434803328,-1.3,4.14136931465002));
#27255=CARTESIAN_POINT('Ctrl Pts',(-3.42329004793791,-1.3,4.14644476697428));
#27256=CARTESIAN_POINT('Ctrl Pts',(-3.4147584711704,-1.3,4.14754376664537));
#27257=CARTESIAN_POINT('',(-3.2566417951307,-1.3,3.97940364582357));
#27258=CARTESIAN_POINT('',(-3.4147584711704,-1.3,4.14754376664537));
#27259=CARTESIAN_POINT('',(-3.35764585633179,-1.3,3.70018367575412));
#27260=CARTESIAN_POINT('Ctrl Pts',(-3.2566417951307,-1.3,3.97940364582357));
#27261=CARTESIAN_POINT('Ctrl Pts',(-3.25806285817519,-1.3,3.97076805174943));
#27262=CARTESIAN_POINT('Ctrl Pts',(-3.26355683793739,-1.3,3.9597981722457));
#27263=CARTESIAN_POINT('Ctrl Pts',(-3.27139143944837,-1.3,3.94354916079683));
#27264=CARTESIAN_POINT('Ctrl Pts',(-3.2779598506316,-1.3,3.93013440106242));
#27265=CARTESIAN_POINT('Ctrl Pts',(-3.2859599492917,-1.3,3.91027551688124));
#27266=CARTESIAN_POINT('Ctrl Pts',(-3.29748931314118,-1.3,3.88213052763898));
#27267=CARTESIAN_POINT('Ctrl Pts',(-3.30875979616856,-1.3,3.85378158569074));
#27268=CARTESIAN_POINT('Ctrl Pts',(-3.32193490364989,-1.3,3.81588673765676));
#27269=CARTESIAN_POINT('Ctrl Pts',(-3.33101474967438,-1.3,3.78965575124683));
#27270=CARTESIAN_POINT('Ctrl Pts',(-3.33990624483581,-1.30000000000001,
3.7596865043912));
#27271=CARTESIAN_POINT('Ctrl Pts',(-3.34788849600103,-1.30000000000001,
3.73634894724736));
#27272=CARTESIAN_POINT('Ctrl Pts',(-3.35378355466238,-1.30000000000001,
3.71409631543785));
#27273=CARTESIAN_POINT('Ctrl Pts',(-3.35739217057375,-1.30000000000001,
3.70109535582529));
#27274=CARTESIAN_POINT('Ctrl Pts',(-3.35764585626408,-1.30000000000001,
3.70018367599751));
#27275=CARTESIAN_POINT('',(-2.95346134572195,-1.29999999999997,3.35297958421177));
#27276=CARTESIAN_POINT('Origin',(0.,-1.3,7.2));
#27277=CARTESIAN_POINT('',(-2.70549646903679,-1.3,3.50427905152391));
#27278=CARTESIAN_POINT('Ctrl Pts',(-2.95346134606173,-1.29999999999991,
3.35297958415421));
#27279=CARTESIAN_POINT('Ctrl Pts',(-2.95255499004324,-1.29999999999991,
3.3534507668553));
#27280=CARTESIAN_POINT('Ctrl Pts',(-2.94625709387801,-1.29999999999991,
3.35676322322326));
#27281=CARTESIAN_POINT('Ctrl Pts',(-2.93496317665334,-1.29999999999991,
3.36330631593411));
#27282=CARTESIAN_POINT('Ctrl Pts',(-2.91812360584104,-1.29999999999993,
3.37118251970181));
#27283=CARTESIAN_POINT('Ctrl Pts',(-2.9056493229959,-1.29999999999993,3.37931771926192));
#27284=CARTESIAN_POINT('Ctrl Pts',(-2.89444547446341,-1.29999999999993,
3.38460967377963));
#27285=CARTESIAN_POINT('Ctrl Pts',(-2.87330971922866,-1.29999999999993,
3.39645550931664));
#27286=CARTESIAN_POINT('Ctrl Pts',(-2.84986342692002,-1.29999999999996,
3.41016373782286));
#27287=CARTESIAN_POINT('Ctrl Pts',(-2.81674957134943,-1.29999999999996,
3.43070471365395));
#27288=CARTESIAN_POINT('Ctrl Pts',(-2.7913038555555,-1.29999999999999,3.44659963092752));
#27289=CARTESIAN_POINT('Ctrl Pts',(-2.76631964265224,-1.29999999999999,
3.46290077644007));
#27290=CARTESIAN_POINT('Ctrl Pts',(-2.74946991434189,-1.29999999999999,
3.47502052021695));
#27291=CARTESIAN_POINT('Ctrl Pts',(-2.73730164354868,-1.3,3.48341371040722));
#27292=CARTESIAN_POINT('Ctrl Pts',(-2.72326627312498,-1.3,3.49418507966832));
#27293=CARTESIAN_POINT('Ctrl Pts',(-2.71361311550261,-1.3,3.50143025308134));
#27294=CARTESIAN_POINT('Ctrl Pts',(-2.70549646903679,-1.3,3.50427905152391));
#27295=CARTESIAN_POINT('',(-2.5158767249182,-1.3,3.37268750121688));
#27296=CARTESIAN_POINT('',(-2.70549646903679,-1.3,3.50427905152391));
#27297=CARTESIAN_POINT('',(-2.55662924076281,-1.30000000000006,3.07857464882883));
#27298=CARTESIAN_POINT('Ctrl Pts',(-2.5158767249182,-1.3,3.37268750121688));
#27299=CARTESIAN_POINT('Ctrl Pts',(-2.51547129336049,-1.3,3.36394515997202));
#27300=CARTESIAN_POINT('Ctrl Pts',(-2.51853827080766,-1.3,3.35206487686083));
#27301=CARTESIAN_POINT('Ctrl Pts',(-2.52292752087393,-1.3,3.33458767675194));
#27302=CARTESIAN_POINT('Ctrl Pts',(-2.52626319062591,-1.30000000000002,
3.31997332758446));
#27303=CARTESIAN_POINT('Ctrl Pts',(-2.52947109631152,-1.30000000000001,
3.30515554054866));
#27304=CARTESIAN_POINT('Ctrl Pts',(-2.53134877776937,-1.30000000000001,
3.28980202777013));
#27305=CARTESIAN_POINT('Ctrl Pts',(-2.53635588003665,-1.30000000000001,
3.26613435433942));
#27306=CARTESIAN_POINT('Ctrl Pts',(-2.54098117524229,-1.30000000000006,
3.23262551129745));
#27307=CARTESIAN_POINT('Ctrl Pts',(-2.54607194775842,-1.30000000000005,
3.19608939128866));
#27308=CARTESIAN_POINT('Ctrl Pts',(-2.54893825527277,-1.30000000000007,
3.1715295558732));
#27309=CARTESIAN_POINT('Ctrl Pts',(-2.5504386619693,-1.30000000000007,3.15283126618667));
#27310=CARTESIAN_POINT('Ctrl Pts',(-2.55358415559025,-1.3000000000001,3.12519350169639));
#27311=CARTESIAN_POINT('Ctrl Pts',(-2.55521193746924,-1.30000000000012,
3.09918410423394));
#27312=CARTESIAN_POINT('Ctrl Pts',(-2.55656438877201,-1.30000000000014,
3.07951611690942));
#27313=CARTESIAN_POINT('Ctrl Pts',(-2.55662924075641,-1.30000000000014,
3.07857464892167));
#27314=CARTESIAN_POINT('',(-2.08924672297676,-1.30000000000088,2.82308040495193));
#27315=CARTESIAN_POINT('Origin',(0.,-1.3,7.2));
#27316=CARTESIAN_POINT('',(-1.87799128879384,-1.3,3.02253507588753));
#27317=CARTESIAN_POINT('Ctrl Pts',(-2.08923581516041,-1.29999999999997,
2.82308924799323));
#27318=CARTESIAN_POINT('Ctrl Pts',(-2.08844045325633,-1.29999999999997,
2.82373405682108));
#27319=CARTESIAN_POINT('Ctrl Pts',(-2.07814240117949,-1.29999999999997,
2.83208780541099));
#27320=CARTESIAN_POINT('Ctrl Pts',(-2.05852013350784,-1.29999999999997,
2.84828080309984));
#27321=CARTESIAN_POINT('Ctrl Pts',(-2.0312350900644,-1.29999999999999,2.87227242206314));
#27322=CARTESIAN_POINT('Ctrl Pts',(-2.00791251142451,-1.29999999999999,
2.89191456471751));
#27323=CARTESIAN_POINT('Ctrl Pts',(-1.99091305460766,-1.29999999999999,
2.90872364328326));
#27324=CARTESIAN_POINT('Ctrl Pts',(-1.96891126495497,-1.29999999999999,
2.92924299368149));
#27325=CARTESIAN_POINT('Ctrl Pts',(-1.94765865101366,-1.3,2.95030374733538));
#27326=CARTESIAN_POINT('Ctrl Pts',(-1.92692142534669,-1.3,2.97161824960676));
#27327=CARTESIAN_POINT('Ctrl Pts',(-1.91488873767411,-1.3,2.98475844866707));
#27328=CARTESIAN_POINT('Ctrl Pts',(-1.90476633611182,-1.3,2.99551287590898));
#27329=CARTESIAN_POINT('Ctrl Pts',(-1.89326780681826,-1.3,3.00896395652652));
#27330=CARTESIAN_POINT('Ctrl Pts',(-1.8853382685594,-1.3,3.01806098483551));
#27331=CARTESIAN_POINT('Ctrl Pts',(-1.87799128879384,-1.3,3.02253507588753));
#27332=CARTESIAN_POINT('',(-1.66515576931082,-1.3,2.93324327829));
#27333=CARTESIAN_POINT('',(-1.87799128879384,-1.3,3.02253507588753));
#27334=CARTESIAN_POINT('',(-1.64377746965492,-1.30000000000001,2.63705187074685));
#27335=CARTESIAN_POINT('Ctrl Pts',(-1.66515576931082,-1.3,2.93324327829));
#27336=CARTESIAN_POINT('Ctrl Pts',(-1.66294156245546,-1.3,2.9247762721372));
#27337=CARTESIAN_POINT('Ctrl Pts',(-1.66343058758897,-1.3,2.91253818382604));
#27338=CARTESIAN_POINT('Ctrl Pts',(-1.66409924349391,-1.3,2.89751233934794));
#27339=CARTESIAN_POINT('Ctrl Pts',(-1.66413304228543,-1.3,2.88855088157155));
#27340=CARTESIAN_POINT('Ctrl Pts',(-1.66445586874793,-1.3,2.87650429183671));
#27341=CARTESIAN_POINT('Ctrl Pts',(-1.664349847888,-1.3,2.86438665854254));
#27342=CARTESIAN_POINT('Ctrl Pts',(-1.66319395735112,-1.3,2.84901103609996));
#27343=CARTESIAN_POINT('Ctrl Pts',(-1.66287285385496,-1.3,2.83684381205863));
#27344=CARTESIAN_POINT('Ctrl Pts',(-1.66271526553416,-1.3,2.81567174026611));
#27345=CARTESIAN_POINT('Ctrl Pts',(-1.65979832631147,-1.3,2.78782357681355));
#27346=CARTESIAN_POINT('Ctrl Pts',(-1.65813795427161,-1.30000000000001,
2.75729053581771));
#27347=CARTESIAN_POINT('Ctrl Pts',(-1.65570779467889,-1.30000000000001,
2.7326332827021));
#27348=CARTESIAN_POINT('Ctrl Pts',(-1.65357606588014,-1.30000000000001,
2.71409163860543));
#27349=CARTESIAN_POINT('Ctrl Pts',(-1.65142819925291,-1.30000000000001,
2.69555803570244));
#27350=CARTESIAN_POINT('Ctrl Pts',(-1.64970395610008,-1.30000000000003,
2.67712374665253));
#27351=CARTESIAN_POINT('Ctrl Pts',(-1.6466789368294,-1.30000000000002,2.65843106406553));
#27352=CARTESIAN_POINT('Ctrl Pts',(-1.64484418585986,-1.30000000000002,
2.64511356192673));
#27353=CARTESIAN_POINT('Ctrl Pts',(-1.64390164626195,-1.30000000000002,
2.63799122361867));
#27354=CARTESIAN_POINT('Ctrl Pts',(-1.6437774696566,-1.30000000000002,2.63705187075953));
#27355=CARTESIAN_POINT('',(-1.13359858633549,-1.30000000000068,2.48435531028948));
#27356=CARTESIAN_POINT('Origin',(0.,-1.3,7.2));
#27357=CARTESIAN_POINT('',(-0.96840887762858,-1.3,2.72336636313561));
#27358=CARTESIAN_POINT('Ctrl Pts',(-1.13358785818362,-1.30000000000001,
2.48436857277337));
#27359=CARTESIAN_POINT('Ctrl Pts',(-1.13294391371556,-1.30000000000001,
2.48516464283889));
#27360=CARTESIAN_POINT('Ctrl Pts',(-1.12460746651562,-1.30000000000001,
2.49547678508334));
#27361=CARTESIAN_POINT('Ctrl Pts',(-1.10877976373829,-1.30000000000001,
2.51539512337677));
#27362=CARTESIAN_POINT('Ctrl Pts',(-1.08708000619847,-1.30000000000001,
2.54453579145496));
#27363=CARTESIAN_POINT('Ctrl Pts',(-1.06835320849415,-1.30000000000001,
2.56859872678717));
#27364=CARTESIAN_POINT('Ctrl Pts',(-1.05521937382472,-1.3,2.58857464167053));
#27365=CARTESIAN_POINT('Ctrl Pts',(-1.03796310307449,-1.30000000000001,
2.61321937129878));
#27366=CARTESIAN_POINT('Ctrl Pts',(-1.02154978498818,-1.3,2.63823699667523));
#27367=CARTESIAN_POINT('Ctrl Pts',(-1.00569178470079,-1.3,2.66339442294084));
#27368=CARTESIAN_POINT('Ctrl Pts',(-0.996652854808831,-1.3,2.67874859209711));
#27369=CARTESIAN_POINT('Ctrl Pts',(-0.988985336877536,-1.3,2.69137107011216));
#27370=CARTESIAN_POINT('Ctrl Pts',(-0.980533804017512,-1.3,2.7069183409826));
#27371=CARTESIAN_POINT('Ctrl Pts',(-0.974665092423394,-1.3,2.71746251872214));
#27372=CARTESIAN_POINT('Ctrl Pts',(-0.96840887762858,-1.3,2.72336636313561));
#27373=CARTESIAN_POINT('',(-0.741659516280667,-1.3,2.68027679827216));
#27374=CARTESIAN_POINT('',(-0.96840887762858,-1.3,2.72336636313561));
#27375=CARTESIAN_POINT('',(-0.65920976572758,-1.3,2.39500858640003));
#27376=CARTESIAN_POINT('Ctrl Pts',(-0.741659516280667,-1.3,2.68027679827216));
#27377=CARTESIAN_POINT('Ctrl Pts',(-0.737733305592168,-1.3,2.67245517600954));
#27378=CARTESIAN_POINT('Ctrl Pts',(-0.735709753270853,-1.3,2.66035632699759));
#27379=CARTESIAN_POINT('Ctrl Pts',(-0.732581199673119,-1.3,2.64260536769193));
#27380=CARTESIAN_POINT('Ctrl Pts',(-0.729771743392392,-1.3,2.62789816097751));
#27381=CARTESIAN_POINT('Ctrl Pts',(-0.726505469227191,-1.3,2.61305804659458));
#27382=CARTESIAN_POINT('Ctrl Pts',(-0.718203659447295,-1.3,2.58347432518374));
#27383=CARTESIAN_POINT('Ctrl Pts',(-0.711759248151159,-1.3,2.55392799989943));
#27384=CARTESIAN_POINT('Ctrl Pts',(-0.701409308678931,-1.3,2.52143083639189));
#27385=CARTESIAN_POINT('Ctrl Pts',(-0.695015042608168,-1.3,2.49781259678565));
#27386=CARTESIAN_POINT('Ctrl Pts',(-0.684471546903469,-1.3,2.46831190594928));
#27387=CARTESIAN_POINT('Ctrl Pts',(-0.67426120931563,-1.3,2.43590191982579));
#27388=CARTESIAN_POINT('Ctrl Pts',(-0.665650684226192,-1.3,2.41236448965118));
#27389=CARTESIAN_POINT('Ctrl Pts',(-0.660928574120142,-1.3,2.3997238538199));
#27390=CARTESIAN_POINT('Ctrl Pts',(-0.659532670840085,-1.3,2.39589740264602));
#27391=CARTESIAN_POINT('Ctrl Pts',(-0.659209765837711,-1.3,2.39500858670318));
#27392=CARTESIAN_POINT('',(-0.128233641545422,-1.30000000000026,2.35170117785791));
#27393=CARTESIAN_POINT('Origin',(0.,-1.3,7.2));
#27394=CARTESIAN_POINT('',(-0.0165023515695832,-1.3,2.61984802158616));
#27395=CARTESIAN_POINT('Ctrl Pts',(-0.128230808431501,-1.3,2.35170674040144));
#27396=CARTESIAN_POINT('Ctrl Pts',(-0.12776606171,-1.3,2.35261922867771));
#27397=CARTESIAN_POINT('Ctrl Pts',(-0.116201754712566,-1.3,2.37534516765435));
#27398=CARTESIAN_POINT('Ctrl Pts',(-0.10245981594267,-1.3,2.40364627470203));
#27399=CARTESIAN_POINT('Ctrl Pts',(-0.0865550189115516,-1.3,2.43952180316647));
#27400=CARTESIAN_POINT('Ctrl Pts',(-0.0768451818344749,-1.3,2.46162868799538));
#27401=CARTESIAN_POINT('Ctrl Pts',(-0.0646419694895632,-1.3,2.49219986215438));
#27402=CARTESIAN_POINT('Ctrl Pts',(-0.0519913323925687,-1.3,2.52275042090917));
#27403=CARTESIAN_POINT('Ctrl Pts',(-0.0414484880037243,-1.3,2.55063756703338));
#27404=CARTESIAN_POINT('Ctrl Pts',(-0.0349002835201714,-1.3,2.57033915626984));
#27405=CARTESIAN_POINT('Ctrl Pts',(-0.0299922130720366,-1.3,2.58428069475804));
#27406=CARTESIAN_POINT('Ctrl Pts',(-0.0249600309789548,-1.3,2.60124271611068));
#27407=CARTESIAN_POINT('Ctrl Pts',(-0.0213943747864753,-1.3,2.6127724501419));
#27408=CARTESIAN_POINT('Ctrl Pts',(-0.0165023515695832,-1.3,2.61984802158616));
#27409=CARTESIAN_POINT('',(0.214250816488161,-1.3,2.62484391020801));
#27410=CARTESIAN_POINT('',(-0.0165023515695832,-1.3,2.61984802158616));
#27411=CARTESIAN_POINT('',(0.35416429646195,-1.3,2.36294845478037));
#27412=CARTESIAN_POINT('Ctrl Pts',(0.214250816488161,-1.3,2.62484391020801));
#27413=CARTESIAN_POINT('Ctrl Pts',(0.219717436762652,-1.3,2.61800951426072));
#27414=CARTESIAN_POINT('Ctrl Pts',(0.224226242429556,-1.3,2.60660085910045));
#27415=CARTESIAN_POINT('Ctrl Pts',(0.230949458773341,-1.3,2.58988253450941));
#27416=CARTESIAN_POINT('Ctrl Pts',(0.236845399224574,-1.3,2.57610161912971));
#27417=CARTESIAN_POINT('Ctrl Pts',(0.242960861231531,-1.3,2.56222898063722));
#27418=CARTESIAN_POINT('Ctrl Pts',(0.250471543071847,-1.3,2.54870591804817));
#27419=CARTESIAN_POINT('Ctrl Pts',(0.260324786692121,-1.30000000000003,
2.52661415542702));
#27420=CARTESIAN_POINT('Ctrl Pts',(0.276326377533022,-1.29999999999998,
2.49679480815956));
#27421=CARTESIAN_POINT('Ctrl Pts',(0.292202396494612,-1.3,2.46694851625356));
#27422=CARTESIAN_POINT('Ctrl Pts',(0.304272576971148,-1.3,2.44537989334913));
#27423=CARTESIAN_POINT('Ctrl Pts',(0.313919337066705,-1.3,2.42933896783766));
#27424=CARTESIAN_POINT('Ctrl Pts',(0.329357357760238,-1.3,2.40248830163039));
#27425=CARTESIAN_POINT('Ctrl Pts',(0.343163853228179,-1.3,2.3804482950595));
#27426=CARTESIAN_POINT('Ctrl Pts',(0.353661239603825,-1.3,2.3637484532088));
#27427=CARTESIAN_POINT('Ctrl Pts',(0.354164296458132,-1.3,2.36294845478644));
#27428=CARTESIAN_POINT('',(0.882693729895366,-1.30000000000117,2.43100096678543));
#27429=CARTESIAN_POINT('Origin',(0.,-1.3,7.2));
#27430=CARTESIAN_POINT('',(0.936125406440075,-1.3,2.71650429950101));
#27431=CARTESIAN_POINT('Ctrl Pts',(0.88269372985561,-1.30000000000001,2.43100096679471));
#27432=CARTESIAN_POINT('Ctrl Pts',(0.882952787962226,-1.30000000000001,
2.43198921795854));
#27433=CARTESIAN_POINT('Ctrl Pts',(0.884755223318824,-1.30000000000001,
2.43888799591159));
#27434=CARTESIAN_POINT('Ctrl Pts',(0.889558734078043,-1.30000000000001,
2.45759430808911));
#27435=CARTESIAN_POINT('Ctrl Pts',(0.89478682500609,-1.3,2.4812180822005));
#27436=CARTESIAN_POINT('Ctrl Pts',(0.900920744454363,-1.3,2.5048946782523));
#27437=CARTESIAN_POINT('Ctrl Pts',(0.903919282745227,-1.3,2.52258106593104));
#27438=CARTESIAN_POINT('Ctrl Pts',(0.909809170318803,-1.3,2.54627243685644));
#27439=CARTESIAN_POINT('Ctrl Pts',(0.915082652483101,-1.3,2.57870764115585));
#27440=CARTESIAN_POINT('Ctrl Pts',(0.920469044817052,-1.3,2.60822457195672));
#27441=CARTESIAN_POINT('Ctrl Pts',(0.923992559502828,-1.3,2.62890061695527));
#27442=CARTESIAN_POINT('Ctrl Pts',(0.92529189916004,-1.3,2.63775451220869));
#27443=CARTESIAN_POINT('Ctrl Pts',(0.926611318159081,-1.3,2.64948665818481));
#27444=CARTESIAN_POINT('Ctrl Pts',(0.928513761893331,-1.3,2.66427335298964));
#27445=CARTESIAN_POINT('Ctrl Pts',(0.930286002589081,-1.3,2.67890363859173));
#27446=CARTESIAN_POINT('Ctrl Pts',(0.931729064678959,-1.3,2.69655002042693));
#27447=CARTESIAN_POINT('Ctrl Pts',(0.932811379690214,-1.3,2.70856623745045));
#27448=CARTESIAN_POINT('Ctrl Pts',(0.936125406440075,-1.3,2.71650429950101));
#27449=CARTESIAN_POINT('',(1.16079736048698,-1.3,2.76936729730244));
#27450=CARTESIAN_POINT('',(0.936125406440075,-1.3,2.71650429950101));
#27451=CARTESIAN_POINT('',(1.35237060322927,-1.30000000000175,2.54236178404915));
#27452=CARTESIAN_POINT('Ctrl Pts',(1.16079736048698,-1.3,2.76936729730244));
#27453=CARTESIAN_POINT('Ctrl Pts',(1.16756547280971,-1.3,2.76381882356845));
#27454=CARTESIAN_POINT('Ctrl Pts',(1.17429750653111,-1.3,2.75357268161998));
#27455=CARTESIAN_POINT('Ctrl Pts',(1.18440293490914,-1.3,2.73864158445797));
#27456=CARTESIAN_POINT('Ctrl Pts',(1.19282025714294,-1.3,2.72628875413437));
#27457=CARTESIAN_POINT('Ctrl Pts',(1.20387629867366,-1.3,2.71172082727262));
#27458=CARTESIAN_POINT('Ctrl Pts',(1.22295971290217,-1.3,2.68787251266423));
#27459=CARTESIAN_POINT('Ctrl Pts',(1.24182813440028,-1.3,2.66390221260837));
#27460=CARTESIAN_POINT('Ctrl Pts',(1.26205481118708,-1.3,2.6405729968529));
#27461=CARTESIAN_POINT('Ctrl Pts',(1.2776175603498,-1.3,2.62164579396719));
#27462=CARTESIAN_POINT('Ctrl Pts',(1.2989775139145,-1.30000000000002,2.59886823472894));
#27463=CARTESIAN_POINT('Ctrl Pts',(1.32380250697419,-1.30000000000001,2.57121941147867));
#27464=CARTESIAN_POINT('Ctrl Pts',(1.34201514395952,-1.30000000000001,2.55258581820719));
#27465=CARTESIAN_POINT('Ctrl Pts',(1.35168394483177,-1.30000000000001,2.54304278699951));
#27466=CARTESIAN_POINT('Ctrl Pts',(1.35237060320572,-1.30000000000001,2.54236178414845));
#27467=CARTESIAN_POINT('',(1.8548768629636,-1.30000000000053,2.71871315099399));
#27468=CARTESIAN_POINT('Origin',(0.,-1.3,7.2));
#27469=CARTESIAN_POINT('',(1.84783999216022,-1.3,3.009110853727));
#27470=CARTESIAN_POINT('Ctrl Pts',(1.85487686288809,-1.3,2.71871315085827));
#27471=CARTESIAN_POINT('Ctrl Pts',(1.8549270845609,-1.3,2.71973140281124));
#27472=CARTESIAN_POINT('Ctrl Pts',(1.85584912980544,-1.3,2.73905781529638));
#27473=CARTESIAN_POINT('Ctrl Pts',(1.85622336316485,-1.3,2.76429054728935));
#27474=CARTESIAN_POINT('Ctrl Pts',(1.85720708657456,-1.3,2.79473457766745));
#27475=CARTESIAN_POINT('Ctrl Pts',(1.85717700294328,-1.3,2.82191251964874));
#27476=CARTESIAN_POINT('Ctrl Pts',(1.85685021732853,-1.3,2.84599119375483));
#27477=CARTESIAN_POINT('Ctrl Pts',(1.85632123702888,-1.3,2.87004577464698));
#27478=CARTESIAN_POINT('Ctrl Pts',(1.85516825338145,-1.3,2.89087649959048));
#27479=CARTESIAN_POINT('Ctrl Pts',(1.85462998338858,-1.3,2.91496806145217));
#27480=CARTESIAN_POINT('Ctrl Pts',(1.85283789437454,-1.3,2.9386502765753));
#27481=CARTESIAN_POINT('Ctrl Pts',(1.85121289296164,-1.3,2.956407355506));
#27482=CARTESIAN_POINT('Ctrl Pts',(1.84997378187088,-1.3,2.97112153527195));
#27483=CARTESIAN_POINT('Ctrl Pts',(1.84769026538568,-1.3,2.98867205329545));
#27484=CARTESIAN_POINT('Ctrl Pts',(1.84624880074882,-1.3,3.00065723247277));
#27485=CARTESIAN_POINT('Ctrl Pts',(1.84783999216022,-1.3,3.009110853727));
#27486=CARTESIAN_POINT('',(2.05661148970878,-1.3,3.10753059403928));
#27487=CARTESIAN_POINT('',(1.84783999216022,-1.3,3.009110853727));
#27488=CARTESIAN_POINT('',(2.29124606287429,-1.30000000000005,2.92534725798923));
#27489=CARTESIAN_POINT('Ctrl Pts',(2.05661148970878,-1.3,3.10753059403928));
#27490=CARTESIAN_POINT('Ctrl Pts',(2.06438529509424,-1.3,3.10351053744535));
#27491=CARTESIAN_POINT('Ctrl Pts',(2.07311117400896,-1.3,3.09489607890758));
#27492=CARTESIAN_POINT('Ctrl Pts',(2.08606699867075,-1.3,3.08237024088461));
#27493=CARTESIAN_POINT('Ctrl Pts',(2.09696957937697,-1.3,3.07210722196283));
#27494=CARTESIAN_POINT('Ctrl Pts',(2.11058813200124,-1.3,3.06000397880414));
#27495=CARTESIAN_POINT('Ctrl Pts',(2.12535537170441,-1.3,3.04879480129421));
#27496=CARTESIAN_POINT('Ctrl Pts',(2.14303983420991,-1.3,3.03242748668087));
#27497=CARTESIAN_POINT('Ctrl Pts',(2.16828207977003,-1.30000000000002,3.01421432900305));
#27498=CARTESIAN_POINT('Ctrl Pts',(2.19672991623475,-1.30000000000001,2.99108833318567));
#27499=CARTESIAN_POINT('Ctrl Pts',(2.22228736155764,-1.30000000000002,2.97318805622786));
#27500=CARTESIAN_POINT('Ctrl Pts',(2.24737536599506,-1.30000000000003,2.95499905098218));
#27501=CARTESIAN_POINT('Ctrl Pts',(2.26798132103125,-1.30000000000003,2.94084734176461));
#27502=CARTESIAN_POINT('Ctrl Pts',(2.28447669320673,-1.30000000000004,2.92993182453429));
#27503=CARTESIAN_POINT('Ctrl Pts',(2.29044867842997,-1.30000000000004,2.92588845519796));
#27504=CARTESIAN_POINT('Ctrl Pts',(2.29124265273508,-1.30000000000004,2.92534957251983));
#27505=CARTESIAN_POINT('',(2.74606318254088,-1.30000000000086,3.20229603426228));
#27506=CARTESIAN_POINT('Origin',(0.,-1.3,7.2));
#27507=CARTESIAN_POINT('',(2.67879510330291,-1.3,3.48487937376242));
#27508=CARTESIAN_POINT('Ctrl Pts',(2.74606318249062,-1.29999999999992,3.20229603390921));
#27509=CARTESIAN_POINT('Ctrl Pts',(2.74589513931379,-1.29999999999992,3.20330365007811));
#27510=CARTESIAN_POINT('Ctrl Pts',(2.74469097079251,-1.29999999999992,3.2103169281617));
#27511=CARTESIAN_POINT('Ctrl Pts',(2.74195814600035,-1.29999999999994,3.22308002651851));
#27512=CARTESIAN_POINT('Ctrl Pts',(2.73967118082232,-1.29999999999994,3.24152929711112));
#27513=CARTESIAN_POINT('Ctrl Pts',(2.73578893667096,-1.29999999999994,3.25590696673797));
#27514=CARTESIAN_POINT('Ctrl Pts',(2.73421818102307,-1.29999999999994,3.26819776747556));
#27515=CARTESIAN_POINT('Ctrl Pts',(2.72948351347016,-1.29999999999994,3.29195966295173));
#27516=CARTESIAN_POINT('Ctrl Pts',(2.72369170179234,-1.29999999999997,3.3184945491252));
#27517=CARTESIAN_POINT('Ctrl Pts',(2.7143890244755,-1.29999999999997,3.35633531279436));
#27518=CARTESIAN_POINT('Ctrl Pts',(2.70713559815793,-1.29999999999998,3.38544760191399));
#27519=CARTESIAN_POINT('Ctrl Pts',(2.69935280611399,-1.29999999999999,3.41424635971549));
#27520=CARTESIAN_POINT('Ctrl Pts',(2.6930331868878,-1.3,3.43401667925856));
#27521=CARTESIAN_POINT('Ctrl Pts',(2.68881095174019,-1.3,3.44818305017517));
#27522=CARTESIAN_POINT('Ctrl Pts',(2.68290395206009,-1.3,3.46486003904829));
#27523=CARTESIAN_POINT('Ctrl Pts',(2.67899628993004,-1.3,3.47627965711833));
#27524=CARTESIAN_POINT('Ctrl Pts',(2.67879510330291,-1.3,3.48487937376242));
#27525=CARTESIAN_POINT('',(2.86254182811346,-1.3,3.62455444166361));
#27526=CARTESIAN_POINT('',(2.67879510330291,-1.3,3.48487937376242));
#27527=CARTESIAN_POINT('',(3.12987662692929,-1.30000000000176,3.49508808472698));
#27528=CARTESIAN_POINT('Ctrl Pts',(2.86254182811346,-1.3,3.62455444166361));
#27529=CARTESIAN_POINT('Ctrl Pts',(2.87098157396346,-1.3,3.62223849797319));
#27530=CARTESIAN_POINT('Ctrl Pts',(2.88130082124863,-1.3,3.61561587077067));
#27531=CARTESIAN_POINT('Ctrl Pts',(2.89657701929705,-1.3,3.60605436272742));
#27532=CARTESIAN_POINT('Ctrl Pts',(2.90936639790833,-1.29999999999998,3.59827482204039));
#27533=CARTESIAN_POINT('Ctrl Pts',(2.92520978215673,-1.29999999999999,3.58926377762022));
#27534=CARTESIAN_POINT('Ctrl Pts',(2.94195211701841,-1.29999999999997,3.58135635188596));
#27535=CARTESIAN_POINT('Ctrl Pts',(2.96275287235917,-1.29999999999999,3.56912187057544));
#27536=CARTESIAN_POINT('Ctrl Pts',(2.99103081011587,-1.29999999999996,3.55633083166688));
#27537=CARTESIAN_POINT('Ctrl Pts',(3.02374000248103,-1.29999999999995,3.53970490348805));
#27538=CARTESIAN_POINT('Ctrl Pts',(3.0581134518176,-1.29999999999992,3.52497819970328));
#27539=CARTESIAN_POINT('Ctrl Pts',(3.09205625616746,-1.2999999999999,3.50984328348542));
#27540=CARTESIAN_POINT('Ctrl Pts',(3.11631138545393,-1.29999999999988,3.50027215599398));
#27541=CARTESIAN_POINT('Ctrl Pts',(3.12897487608527,-1.29999999999987,3.49543223771777));
#27542=CARTESIAN_POINT('Ctrl Pts',(3.12987662694986,-1.29999999999987,3.495088084751));
#27543=CARTESIAN_POINT('',(3.5171326127652,-1.30000000000045,3.86049731487559));
#27544=CARTESIAN_POINT('Origin',(0.,-1.3,7.2));
#27545=CARTESIAN_POINT('',(3.39267401414619,-1.3,4.12301649229108));
#27546=CARTESIAN_POINT('Ctrl Pts',(3.51713261273951,-1.3,3.86049731486587));
#27547=CARTESIAN_POINT('Ctrl Pts',(3.51688288217038,-1.3,3.86115709724913));
#27548=CARTESIAN_POINT('Ctrl Pts',(3.51650668153201,-1.3,3.86212544904999));
#27549=CARTESIAN_POINT('Ctrl Pts',(3.5160121348391,-1.3,3.86337613530466));
#27550=CARTESIAN_POINT('Ctrl Pts',(3.51367923070723,-1.3,3.86927594450976));
#27551=CARTESIAN_POINT('Ctrl Pts',(3.50890708207116,-1.3,3.88153385811727));
#27552=CARTESIAN_POINT('Ctrl Pts',(3.50248870255892,-1.3,3.89738608899958));
#27553=CARTESIAN_POINT('Ctrl Pts',(3.49843132749079,-1.3,3.90740706800735));
#27554=CARTESIAN_POINT('Ctrl Pts',(3.49368714677763,-1.3,3.91885284427876));
#27555=CARTESIAN_POINT('Ctrl Pts',(3.48842221216129,-1.3,3.93100743587123));
#27556=CARTESIAN_POINT('Ctrl Pts',(3.48607767189504,-1.3,3.93642002529257));
#27557=CARTESIAN_POINT('Ctrl Pts',(3.48362945784637,-1.3,3.94197283731675));
#27558=CARTESIAN_POINT('Ctrl Pts',(3.48111675437825,-1.3,3.94761334202975));
#27559=CARTESIAN_POINT('Ctrl Pts',(3.47392079620689,-1.3,3.96376679447454));
#27560=CARTESIAN_POINT('Ctrl Pts',(3.46610202845713,-1.3,3.98081946477663));
#27561=CARTESIAN_POINT('Ctrl Pts',(3.45829100003881,-1.3,3.99674657305018));
#27562=CARTESIAN_POINT('Ctrl Pts',(3.45203318383949,-1.3,4.00950659782858));
#27563=CARTESIAN_POINT('Ctrl Pts',(3.44681974798713,-1.3,4.01966078645757));
#27564=CARTESIAN_POINT('Ctrl Pts',(3.44229346403023,-1.3,4.02889359280264));
#27565=CARTESIAN_POINT('Ctrl Pts',(3.43952648034535,-1.3,4.03453774256563));
#27566=CARTESIAN_POINT('Ctrl Pts',(3.43698933358003,-1.3,4.03982671919313));
#27567=CARTESIAN_POINT('Ctrl Pts',(3.4343179304055,-1.3,4.04500372655646));
#27568=CARTESIAN_POINT('Ctrl Pts',(3.43163432866176,-1.3,4.05020437396154));
#27569=CARTESIAN_POINT('Ctrl Pts',(3.42878588057214,-1.3,4.05534933711627));
#27570=CARTESIAN_POINT('Ctrl Pts',(3.42583988757771,-1.3,4.060679557033));
#27571=CARTESIAN_POINT('Ctrl Pts',(3.42266805467712,-1.3,4.06641839175911));
#27572=CARTESIAN_POINT('Ctrl Pts',(3.41981353336582,-1.3,4.07159530558462));
#27573=CARTESIAN_POINT('Ctrl Pts',(3.417220711055,-1.3,4.07625699048129));
#27574=CARTESIAN_POINT('Ctrl Pts',(3.41568434131801,-1.3,4.07901925905972));
#27575=CARTESIAN_POINT('Ctrl Pts',(3.4142406922337,-1.3,4.08160108673217));
#27576=CARTESIAN_POINT('Ctrl Pts',(3.41288349055858,-1.3,4.08401513033096));
#27577=CARTESIAN_POINT('Ctrl Pts',(3.41132416451107,-1.3,4.08678869090963));
#27578=CARTESIAN_POINT('Ctrl Pts',(3.4098759552894,-1.3,4.08933910003031));
#27579=CARTESIAN_POINT('Ctrl Pts',(3.40850271524696,-1.3,4.09167097319111));
#27580=CARTESIAN_POINT('Ctrl Pts',(3.40683923872879,-1.3,4.09449569146794));
#27581=CARTESIAN_POINT('Ctrl Pts',(3.40529659274212,-1.3,4.09700575372786));
#27582=CARTESIAN_POINT('Ctrl Pts',(3.403919606175,-1.3,4.09926954672169));
#27583=CARTESIAN_POINT('Ctrl Pts',(3.39276510850083,-1.3,4.11760776024346));
#27584=CARTESIAN_POINT('Ctrl Pts',(3.39333976027048,-1.3,4.12020898041362));
#27585=CARTESIAN_POINT('Ctrl Pts',(3.39267401414619,-1.3,4.12301649229108));
#27586=CARTESIAN_POINT('',(3.54336535262991,-1.3,4.29784241707854));
#27587=CARTESIAN_POINT('',(3.39267401414619,-1.3,4.12301649229108));
#27588=CARTESIAN_POINT('',(3.83160559593893,-1.30000000000002,4.22656788267061));
#27589=CARTESIAN_POINT('Ctrl Pts',(3.54336535262991,-1.3,4.29784241707854));
#27590=CARTESIAN_POINT('Ctrl Pts',(3.5521021815524,-1.3,4.29733180414408));
#27591=CARTESIAN_POINT('Ctrl Pts',(3.56358560401283,-1.3,4.29301250933079));
#27592=CARTESIAN_POINT('Ctrl Pts',(3.58056423090154,-1.3,4.28691857619117));
#27593=CARTESIAN_POINT('Ctrl Pts',(3.59459177663706,-1.3,4.2817873486781));
#27594=CARTESIAN_POINT('Ctrl Pts',(3.61517717129019,-1.3,4.27590496591539));
#27595=CARTESIAN_POINT('Ctrl Pts',(3.64437267289781,-1.30000000000002,4.26737943677047));
#27596=CARTESIAN_POINT('Ctrl Pts',(3.67374206987082,-1.30000000000001,4.25912999654611));
#27597=CARTESIAN_POINT('Ctrl Pts',(3.71280539583391,-1.30000000000003,4.24998612818397));
#27598=CARTESIAN_POINT('Ctrl Pts',(3.73984169575344,-1.30000000000003,4.24369792702497));
#27599=CARTESIAN_POINT('Ctrl Pts',(3.77057621024761,-1.30000000000003,4.23798792710164));
#27600=CARTESIAN_POINT('Ctrl Pts',(3.79462037248639,-1.30000000000005,4.23248904186298));
#27601=CARTESIAN_POINT('Ctrl Pts',(3.81736692655516,-1.30000000000004,4.22895365433709));
#27602=CARTESIAN_POINT('Ctrl Pts',(3.83067329395874,-1.30000000000005,4.22672467388769));
#27603=CARTESIAN_POINT('Ctrl Pts',(3.83160559566069,-1.30000000000005,4.2265678827174));
#27604=CARTESIAN_POINT('',(4.13470146325513,-1.3,4.66489767272486));
#27605=CARTESIAN_POINT('Origin',(0.,-1.3,7.2));
#27606=CARTESIAN_POINT('',(3.95827679071515,-1.3,4.89563255511164));
#27607=CARTESIAN_POINT('Ctrl Pts',(4.1347014632565,-1.30000000000001,4.66489767272278));
#27608=CARTESIAN_POINT('Ctrl Pts',(4.13414034057423,-1.30000000000001,4.66574651526749));
#27609=CARTESIAN_POINT('Ctrl Pts',(4.1301921985072,-1.30000000000001,4.67166339544529));
#27610=CARTESIAN_POINT('Ctrl Pts',(4.1225478980385,-1.30000000000001,4.68226017949025));
#27611=CARTESIAN_POINT('Ctrl Pts',(4.11277136635636,-1.30000000000001,4.69795681868009));
#27612=CARTESIAN_POINT('Ctrl Pts',(4.10185652815243,-1.30000000000001,4.71227111163331));
#27613=CARTESIAN_POINT('Ctrl Pts',(4.08853169252855,-1.30000000000001,4.73287853781571));
#27614=CARTESIAN_POINT('Ctrl Pts',(4.07049950580513,-1.29999999999999,4.75697072422904));
#27615=CARTESIAN_POINT('Ctrl Pts',(4.04694899362191,-1.3,4.7882155432056));
#27616=CARTESIAN_POINT('Ctrl Pts',(4.02820350434482,-1.3,4.8114248769198));
#27617=CARTESIAN_POINT('Ctrl Pts',(4.01343459617974,-1.3,4.83038036764205));
#27618=CARTESIAN_POINT('Ctrl Pts',(4.00369573333177,-1.3,4.84150363159022));
#27619=CARTESIAN_POINT('Ctrl Pts',(3.99200513405257,-1.3,4.855004766164));
#27620=CARTESIAN_POINT('Ctrl Pts',(3.9823266250081,-1.3,4.86614166803621));
#27621=CARTESIAN_POINT('Ctrl Pts',(3.97017242189078,-1.3,4.87901196281535));
#27622=CARTESIAN_POINT('Ctrl Pts',(3.96195840372374,-1.3,4.88785815300778));
#27623=CARTESIAN_POINT('Ctrl Pts',(3.95827679071515,-1.3,4.89563255511164));
#27624=CARTESIAN_POINT('',(4.06932680828302,-1.3,5.09796860496431));
#27625=CARTESIAN_POINT('',(3.95827679071515,-1.3,4.89563255511164));
#27626=CARTESIAN_POINT('',(4.36619448174045,-1.30000000000001,5.08840208666063));
#27627=CARTESIAN_POINT('Ctrl Pts',(4.06932680828302,-1.3,5.09796860496431));
#27628=CARTESIAN_POINT('Ctrl Pts',(4.07797887893015,-1.3,5.09928563902122));
#27629=CARTESIAN_POINT('Ctrl Pts',(4.09010264837494,-1.3,5.09742818248793));
#27630=CARTESIAN_POINT('Ctrl Pts',(4.10794777737397,-1.3,5.09490870018088));
#27631=CARTESIAN_POINT('Ctrl Pts',(4.1227984853887,-1.3,5.092996965449));
#27632=CARTESIAN_POINT('Ctrl Pts',(4.14093676471961,-1.3,5.09122327296695));
#27633=CARTESIAN_POINT('Ctrl Pts',(4.15945674239661,-1.3,5.09077853240722));
#27634=CARTESIAN_POINT('Ctrl Pts',(4.18342557961069,-1.3,5.08805332370513));
#27635=CARTESIAN_POINT('Ctrl Pts',(4.22679133883137,-1.3,5.0875445379173));
#27636=CARTESIAN_POINT('Ctrl Pts',(4.26662860959371,-1.30000000000001,5.08602638006159));
#27637=CARTESIAN_POINT('Ctrl Pts',(4.3041267131296,-1.30000000000001,5.08697688034838));
#27638=CARTESIAN_POINT('Ctrl Pts',(4.32877752354222,-1.30000000000001,5.08656709641376));
#27639=CARTESIAN_POINT('Ctrl Pts',(4.35175885165174,-1.30000000000001,5.08779880743945));
#27640=CARTESIAN_POINT('Ctrl Pts',(4.36524030569969,-1.30000000000002,5.08836278683076));
#27641=CARTESIAN_POINT('Ctrl Pts',(4.3661944817394,-1.30000000000002,5.08840208666059));
#27642=CARTESIAN_POINT('',(4.5712854650164,-1.30000000000092,5.57960782188225));
#27643=CARTESIAN_POINT('Origin',(0.,-1.3,7.2));
#27644=CARTESIAN_POINT('',(4.35088387761047,-1.3,5.76896053285564));
#27645=CARTESIAN_POINT('Ctrl Pts',(4.57127105643491,-1.30000000000025,5.57962221793917));
#27646=CARTESIAN_POINT('Ctrl Pts',(4.57054672674967,-1.30000000000025,5.58034591264246));
#27647=CARTESIAN_POINT('Ctrl Pts',(4.56116348515715,-1.30000000000025,5.58971564859421));
#27648=CARTESIAN_POINT('Ctrl Pts',(4.54301380784618,-1.30000000000019,5.60754561873787));
#27649=CARTESIAN_POINT('Ctrl Pts',(4.51629897299144,-1.30000000000017,5.63216227364949));
#27650=CARTESIAN_POINT('Ctrl Pts',(4.49433855488318,-1.30000000000009,5.65331652551982));
#27651=CARTESIAN_POINT('Ctrl Pts',(4.47582949985366,-1.3000000000001,5.66843433384021));
#27652=CARTESIAN_POINT('Ctrl Pts',(4.45542493556535,-1.30000000000008,5.68625771326949));
#27653=CARTESIAN_POINT('Ctrl Pts',(4.43225268787841,-1.30000000000004,5.70516072474142));
#27654=CARTESIAN_POINT('Ctrl Pts',(4.40908517600157,-1.30000000000003,5.72400020051142));
#27655=CARTESIAN_POINT('Ctrl Pts',(4.39231891341255,-1.30000000000002,5.73621537749316));
#27656=CARTESIAN_POINT('Ctrl Pts',(4.38057663395205,-1.30000000000002,5.74519668890453));
#27657=CARTESIAN_POINT('Ctrl Pts',(4.36598759938307,-1.3,5.75520187083905));
#27658=CARTESIAN_POINT('Ctrl Pts',(4.35610142762816,-1.3,5.76212147047616));
#27659=CARTESIAN_POINT('Ctrl Pts',(4.35088387761047,-1.3,5.76896053285564));
#27660=CARTESIAN_POINT('',(4.41743915561768,-1.3,5.98996365147886));
#27661=CARTESIAN_POINT('',(4.35088387761047,-1.3,5.76896053285564));
#27662=CARTESIAN_POINT('',(4.70981332849669,-1.30000000000085,6.04234788887652));
#27663=CARTESIAN_POINT('Ctrl Pts',(4.41743915561768,-1.3,5.98996365147887));
#27664=CARTESIAN_POINT('Ctrl Pts',(4.42562833098492,-1.3,5.99305077181904));
#27665=CARTESIAN_POINT('Ctrl Pts',(4.43787121888721,-1.29999999999999,5.99376524194451));
#27666=CARTESIAN_POINT('Ctrl Pts',(4.45585041430517,-1.29999999999998,5.99501197237366));
#27667=CARTESIAN_POINT('Ctrl Pts',(4.47077112054749,-1.29999999999998,5.99624136741251));
#27668=CARTESIAN_POINT('Ctrl Pts',(4.48888549481281,-1.29999999999996,5.99826902796312));
#27669=CARTESIAN_POINT('Ctrl Pts',(4.50708052400253,-1.29999999999994,6.00172835399205));
#27670=CARTESIAN_POINT('Ctrl Pts',(4.53109886254277,-1.29999999999994,6.00406302153201));
#27671=CARTESIAN_POINT('Ctrl Pts',(4.5554207795094,-1.29999999999991,6.00910658184204));
#27672=CARTESIAN_POINT('Ctrl Pts',(4.57961335592168,-1.2999999999999,6.01326169023657));
#27673=CARTESIAN_POINT('Ctrl Pts',(4.60381579105576,-1.29999999999988,6.01754841177145));
#27674=CARTESIAN_POINT('Ctrl Pts',(4.62354611479138,-1.29999999999983,6.02187971789091));
#27675=CARTESIAN_POINT('Ctrl Pts',(4.63874413860124,-1.29999999999982,6.02548249806524));
#27676=CARTESIAN_POINT('Ctrl Pts',(4.6448207916927,-1.29999999999982,6.02690740127392));
#27677=CARTESIAN_POINT('Ctrl Pts',(4.65541484816387,-1.29999999999982,6.02904115986987));
#27678=CARTESIAN_POINT('Ctrl Pts',(4.67663673184222,-1.2999999999998,6.03366080550892));
#27679=CARTESIAN_POINT('Ctrl Pts',(4.6957990883815,-1.29999999999975,6.03866730859026));
#27680=CARTESIAN_POINT('Ctrl Pts',(4.70888266080627,-1.29999999999972,6.04210425716953));
#27681=CARTESIAN_POINT('Ctrl Pts',(4.70981332848442,-1.29999999999972,6.04234788890545));
#27682=CARTESIAN_POINT('',(4.80833879015672,-1.30000000000006,6.56566721647533));
#27683=CARTESIAN_POINT('Origin',(0.,-1.3,7.2));
#27684=CARTESIAN_POINT('',(4.55333646119701,-1.3,6.70483180220308));
#27685=CARTESIAN_POINT('Ctrl Pts',(4.80833879058776,-1.30000000000005,6.56566721608982));
#27686=CARTESIAN_POINT('Ctrl Pts',(4.80747844806735,-1.30000000000005,6.56622014166603));
#27687=CARTESIAN_POINT('Ctrl Pts',(4.79632873311919,-1.30000000000005,6.5733579152029));
#27688=CARTESIAN_POINT('Ctrl Pts',(4.77472662307004,-1.30000000000003,6.58645074781878));
#27689=CARTESIAN_POINT('Ctrl Pts',(4.7515349646246,-1.30000000000003,6.60128956561561));
#27690=CARTESIAN_POINT('Ctrl Pts',(4.73570235451819,-1.30000000000002,6.60979664855893));
#27691=CARTESIAN_POINT('Ctrl Pts',(4.72523936468665,-1.30000000000002,6.61586137002473));
#27692=CARTESIAN_POINT('Ctrl Pts',(4.71234108790908,-1.30000000000002,6.62410664981093));
#27693=CARTESIAN_POINT('Ctrl Pts',(4.69635329463586,-1.30000000000002,6.63210460558043));
#27694=CARTESIAN_POINT('Ctrl Pts',(4.67274012394597,-1.30000000000002,6.64549193416047));
#27695=CARTESIAN_POINT('Ctrl Pts',(4.64616298310549,-1.30000000000001,6.65922290148753));
#27696=CARTESIAN_POINT('Ctrl Pts',(4.61959384082978,-1.30000000000001,6.67287273622477));
#27697=CARTESIAN_POINT('Ctrl Pts',(4.60066248946865,-1.30000000000001,6.68136532610089));
#27698=CARTESIAN_POINT('Ctrl Pts',(4.58731275561843,-1.3,6.68772391623228));
#27699=CARTESIAN_POINT('Ctrl Pts',(4.57096519811773,-1.3,6.69448853267874));
#27700=CARTESIAN_POINT('Ctrl Pts',(4.55986191625143,-1.3,6.69922697939143));
#27701=CARTESIAN_POINT('Ctrl Pts',(4.55333646119701,-1.3,6.70483180220308));
#27702=CARTESIAN_POINT('',(4.57248821462698,-1.3,6.9348430928224));
#27703=CARTESIAN_POINT('',(4.55333646119701,-1.3,6.70483180220308));
#27704=CARTESIAN_POINT('',(4.84757809483801,-1.3,7.04674656791213));
#27705=CARTESIAN_POINT('Ctrl Pts',(4.57248821462698,-1.3,6.9348430928224));
#27706=CARTESIAN_POINT('Ctrl Pts',(4.58686099902111,-1.3,6.94405440331263));
#27707=CARTESIAN_POINT('Ctrl Pts',(4.60907421143989,-1.30000000000024,6.94591557225086));
#27708=CARTESIAN_POINT('Ctrl Pts',(4.66591701788673,-1.30000000000024,6.9677865529423));
#27709=CARTESIAN_POINT('Ctrl Pts',(4.68947396446559,-1.30000000000016,6.97660500882556));
#27710=CARTESIAN_POINT('Ctrl Pts',(4.75859274645512,-1.30000000000016,7.00421340848844));
#27711=CARTESIAN_POINT('Ctrl Pts',(4.80332270094286,-1.3,7.02507116583801));
#27712=CARTESIAN_POINT('Ctrl Pts',(4.84757809483801,-1.3,7.04674656791213));
#27713=CARTESIAN_POINT('',(4.83514958407044,-1.30000000000004,7.57915194386478));
#27714=CARTESIAN_POINT('Origin',(0.,-1.3,7.2));
#27715=CARTESIAN_POINT('',(4.55678639209675,-1.3,7.66234429787489));
#27716=CARTESIAN_POINT('Ctrl Pts',(4.83514187469075,-1.30000000000002,7.57915490962811));
#27717=CARTESIAN_POINT('Ctrl Pts',(4.83418604828034,-1.30000000000002,7.57952260918312));
#27718=CARTESIAN_POINT('Ctrl Pts',(4.8218053910255,-1.30000000000002,7.58427928601273));
#27719=CARTESIAN_POINT('Ctrl Pts',(4.80369703210634,-1.30000000000002,7.59113993557893));
#27720=CARTESIAN_POINT('Ctrl Pts',(4.78072070206189,-1.30000000000001,7.59826996426714));
#27721=CARTESIAN_POINT('Ctrl Pts',(4.76786499505704,-1.30000000000001,7.60368176740184));
#27722=CARTESIAN_POINT('Ctrl Pts',(4.75923927618335,-1.30000000000001,7.60624853723847));
#27723=CARTESIAN_POINT('Ctrl Pts',(4.75348070600745,-1.30000000000001,7.60784584718063));
#27724=CARTESIAN_POINT('Ctrl Pts',(4.74343057879298,-1.30000000000001,7.61127081391062));
#27725=CARTESIAN_POINT('Ctrl Pts',(4.7290926957189,-1.30000000000001,7.61656804117484));
#27726=CARTESIAN_POINT('Ctrl Pts',(4.71179724858882,-1.30000000000001,7.62108876395165));
#27727=CARTESIAN_POINT('Ctrl Pts',(4.68590468587277,-1.30000000000001,7.62938620214825));
#27728=CARTESIAN_POINT('Ctrl Pts',(4.65997285225601,-1.3,7.63611399060629));
#27729=CARTESIAN_POINT('Ctrl Pts',(4.63687848316794,-1.3,7.64278362359797));
#27730=CARTESIAN_POINT('Ctrl Pts',(4.62245430981319,-1.3,7.64588206265252));
#27731=CARTESIAN_POINT('Ctrl Pts',(4.60795019531382,-1.30000000000002,7.64934885674979));
#27732=CARTESIAN_POINT('Ctrl Pts',(4.59357906309857,-1.3,7.65261768781225));
#27733=CARTESIAN_POINT('Ctrl Pts',(4.57617941896521,-1.3,7.65590048748505));
#27734=CARTESIAN_POINT('Ctrl Pts',(4.56433455848945,-1.3,7.65821867228284));
#27735=CARTESIAN_POINT('Ctrl Pts',(4.55678639209675,-1.3,7.66234429787489));
#27736=CARTESIAN_POINT('',(4.52769759742429,-1.3,7.89131116337361));
#27737=CARTESIAN_POINT('',(4.55678639209675,-1.3,7.66234429787489));
#27738=CARTESIAN_POINT('',(4.77352143851607,-1.29999999999998,8.05790038817306));
#27739=CARTESIAN_POINT('Ctrl Pts',(4.52769759742428,-1.3,7.89131116337361));
#27740=CARTESIAN_POINT('Ctrl Pts',(4.53392313641892,-1.3,7.89746222583599));
#27741=CARTESIAN_POINT('Ctrl Pts',(4.54480756131904,-1.3,7.90313131042928));
#27742=CARTESIAN_POINT('Ctrl Pts',(4.56073300810662,-1.3,7.91156448348519));
#27743=CARTESIAN_POINT('Ctrl Pts',(4.57382741729707,-1.3,7.91886372538035));
#27744=CARTESIAN_POINT('Ctrl Pts',(4.58698548913663,-1.29999999999999,7.92639668444809));
#27745=CARTESIAN_POINT('Ctrl Pts',(4.59965290245868,-1.29999999999999,7.93527268020086));
#27746=CARTESIAN_POINT('Ctrl Pts',(4.62058857472471,-1.29999999999999,7.94740044967715));
#27747=CARTESIAN_POINT('Ctrl Pts',(4.64859413441977,-1.29999999999999,7.96634699488997));
#27748=CARTESIAN_POINT('Ctrl Pts',(4.6816555228702,-1.29999999999997,7.98886506857447));
#27749=CARTESIAN_POINT('Ctrl Pts',(4.70425563008658,-1.29999999999998,8.00520911535576));
#27750=CARTESIAN_POINT('Ctrl Pts',(4.71911478157114,-1.29999999999997,8.01670270298284));
#27751=CARTESIAN_POINT('Ctrl Pts',(4.72917527752168,-1.29999999999997,8.02388370350348));
#27752=CARTESIAN_POINT('Ctrl Pts',(4.74172894757691,-1.29999999999997,8.03290675645269));
#27753=CARTESIAN_POINT('Ctrl Pts',(4.75646184909153,-1.29999999999997,8.04470262929097));
#27754=CARTESIAN_POINT('Ctrl Pts',(4.7670715443958,-1.29999999999996,8.05295673069625));
#27755=CARTESIAN_POINT('Ctrl Pts',(4.77277075263192,-1.29999999999996,8.05732553818437));
#27756=CARTESIAN_POINT('Ctrl Pts',(4.77352143846884,-1.29999999999996,8.05790038813689));
#27757=CARTESIAN_POINT('',(4.65060554698675,-1.30000000000011,8.57636043474658));
#27758=CARTESIAN_POINT('Origin',(0.,-1.3,7.2));
#27759=CARTESIAN_POINT('',(4.36108289177477,-1.3,8.59965012915547));
#27760=CARTESIAN_POINT('Ctrl Pts',(4.65060554698679,-1.30000000000024,8.57636043474659));
#27761=CARTESIAN_POINT('Ctrl Pts',(4.64959949726022,-1.30000000000024,8.57651340723713));
#27762=CARTESIAN_POINT('Ctrl Pts',(4.63651671604971,-1.30000000000024,8.57849253071906));
#27763=CARTESIAN_POINT('Ctrl Pts',(4.62194387170408,-1.30000000000018,8.58059186454646));
#27764=CARTESIAN_POINT('Ctrl Pts',(4.60387932238256,-1.30000000000017,8.58288177294578));
#27765=CARTESIAN_POINT('Ctrl Pts',(4.5949397787931,-1.30000000000016,8.58342037655297));
#27766=CARTESIAN_POINT('Ctrl Pts',(4.58581707049659,-1.30000000000016,8.58509868341759));
#27767=CARTESIAN_POINT('Ctrl Pts',(4.57976379072862,-1.30000000000016,8.5860410540558));
#27768=CARTESIAN_POINT('Ctrl Pts',(4.5527239583302,-1.30000000000016,8.58902013595488));
#27769=CARTESIAN_POINT('Ctrl Pts',(4.51519255717782,-1.30000000000006,8.59274412866406));
#27770=CARTESIAN_POINT('Ctrl Pts',(4.47343222775836,-1.30000000000005,8.59504533441449));
#27771=CARTESIAN_POINT('Ctrl Pts',(4.45248023997978,-1.30000000000004,8.59655638746876));
#27772=CARTESIAN_POINT('Ctrl Pts',(4.44055346921642,-1.30000000000004,8.59708300700705));
#27773=CARTESIAN_POINT('Ctrl Pts',(4.42874610728168,-1.30000000000002,8.59716779009615));
#27774=CARTESIAN_POINT('Ctrl Pts',(4.41383823973776,-1.30000000000004,8.59752605734575));
#27775=CARTESIAN_POINT('Ctrl Pts',(4.39909825262232,-1.30000000000002,8.59776299484744));
#27776=CARTESIAN_POINT('Ctrl Pts',(4.38139541625276,-1.3,8.59735867632484));
#27777=CARTESIAN_POINT('Ctrl Pts',(4.36932387841423,-1.3,8.59718401041836));
#27778=CARTESIAN_POINT('Ctrl Pts',(4.36108289177477,-1.3,8.59965012915547));
#27779=CARTESIAN_POINT('',(4.28502486891058,-1.3,8.81756561880638));
#27780=CARTESIAN_POINT('',(4.36108289177477,-1.3,8.59965012915547));
#27781=CARTESIAN_POINT('',(4.4908419881269,-1.30000000000001,9.03162175071067));
#27782=CARTESIAN_POINT('Ctrl Pts',(4.28502486891058,-1.3,8.81756561880638));
#27783=CARTESIAN_POINT('Ctrl Pts',(4.28983548714458,-1.3,8.82487662813455));
#27784=CARTESIAN_POINT('Ctrl Pts',(4.29930376072647,-1.3,8.8326846148834));
#27785=CARTESIAN_POINT('Ctrl Pts',(4.31312792074243,-1.3,8.84424454248958));
#27786=CARTESIAN_POINT('Ctrl Pts',(4.32441879715599,-1.3,8.85410663225913));
#27787=CARTESIAN_POINT('Ctrl Pts',(4.33572321977293,-1.3,8.86421064164099));
#27788=CARTESIAN_POINT('Ctrl Pts',(4.34626852229515,-1.3,8.87552627071934));
#27789=CARTESIAN_POINT('Ctrl Pts',(4.3642252122643,-1.3,8.89174180979169));
#27790=CARTESIAN_POINT('Ctrl Pts',(4.38767994763106,-1.3,8.91609640196863));
#27791=CARTESIAN_POINT('Ctrl Pts',(4.41533706763616,-1.30000000000001,8.94499626631874));
#27792=CARTESIAN_POINT('Ctrl Pts',(4.43404520828785,-1.30000000000001,8.96568188496965));
#27793=CARTESIAN_POINT('Ctrl Pts',(4.44619000963143,-1.30000000000001,8.98001366847381));
#27794=CARTESIAN_POINT('Ctrl Pts',(4.45453765168017,-1.30000000000001,8.9891294252702));
#27795=CARTESIAN_POINT('Ctrl Pts',(4.46494103395469,-1.30000000000001,9.00056527592794));
#27796=CARTESIAN_POINT('Ctrl Pts',(4.47689956689865,-1.30000000000001,9.0151663505764));
#27797=CARTESIAN_POINT('Ctrl Pts',(4.48556119107646,-1.30000000000001,9.02544560667773));
#27798=CARTESIAN_POINT('Ctrl Pts',(4.49022739352167,-1.30000000000001,9.0309035988107));
#27799=CARTESIAN_POINT('Ctrl Pts',(4.49084198808645,-1.30000000000001,9.0316217506634));
#27800=CARTESIAN_POINT('',(4.2628448153366,-1.30000000000019,9.51314808875148));
#27801=CARTESIAN_POINT('Origin',(0.,-1.3,7.2));
#27802=CARTESIAN_POINT('',(3.97477914228473,-1.3,9.47578453352548));
#27803=CARTESIAN_POINT('Ctrl Pts',(4.26284481543292,-1.29999999999937,9.5131480887536));
#27804=CARTESIAN_POINT('Ctrl Pts',(4.26220643334429,-1.29999999999937,9.51311720919109));
#27805=CARTESIAN_POINT('Ctrl Pts',(4.26156824485443,-1.29999999999937,9.51308588793707));
#27806=CARTESIAN_POINT('Ctrl Pts',(4.26054883619775,-1.29999999999937,9.51303248016318));
#27807=CARTESIAN_POINT('Ctrl Pts',(4.260166989794,-1.29999999999937,9.5130120882434));
#27808=CARTESIAN_POINT('Ctrl Pts',(4.25368275115679,-1.29999999999938,9.51264762263276));
#27809=CARTESIAN_POINT('Ctrl Pts',(4.24178124330855,-1.29999999999946,9.51117036285086));
#27810=CARTESIAN_POINT('Ctrl Pts',(4.22320612684214,-1.2999999999995,9.51079938881588));
#27811=CARTESIAN_POINT('Ctrl Pts',(4.20544580882674,-1.29999999999956,9.50826165136631));
#27812=CARTESIAN_POINT('Ctrl Pts',(4.186869367981,-1.29999999999961,9.50784799049426));
#27813=CARTESIAN_POINT('Ctrl Pts',(4.16917315735985,-1.29999999999964,9.50510377777432));
#27814=CARTESIAN_POINT('Ctrl Pts',(4.15072826469995,-1.2999999999997,9.50428049865621));
#27815=CARTESIAN_POINT('Ctrl Pts',(4.13311774283479,-1.29999999999972,9.50129808886395));
#27816=CARTESIAN_POINT('Ctrl Pts',(4.10903671786789,-1.29999999999976,9.49882516426723));
#27817=CARTESIAN_POINT('Ctrl Pts',(4.08562660246456,-1.29999999999985,9.49464937055402));
#27818=CARTESIAN_POINT('Ctrl Pts',(4.06476527097454,-1.29999999999987,9.49189931303716));
#27819=CARTESIAN_POINT('Ctrl Pts',(4.05300830437223,-1.29999999999988,9.48988652188621));
#27820=CARTESIAN_POINT('Ctrl Pts',(4.04144316270787,-1.2999999999999,9.48751020962115));
#27821=CARTESIAN_POINT('Ctrl Pts',(4.02679641464904,-1.29999999999993,9.48473812544654));
#27822=CARTESIAN_POINT('Ctrl Pts',(4.01233725084337,-1.29999999999994,9.4818865708566));
#27823=CARTESIAN_POINT('Ctrl Pts',(3.99511068658323,-1.29999999999998,9.47779791444728));
#27824=CARTESIAN_POINT('Ctrl Pts',(3.98335277851019,-1.3,9.47508570286587));
#27825=CARTESIAN_POINT('Ctrl Pts',(3.97477914228473,-1.3,9.47578453352548));
#27826=CARTESIAN_POINT('',(3.85507599179486,-1.3,9.6731246947563));
#27827=CARTESIAN_POINT('',(3.97477914228473,-1.3,9.47578453352548));
#27828=CARTESIAN_POINT('',(4.01179369694655,-1.29999999999766,9.92543782412063));
#27829=CARTESIAN_POINT('Ctrl Pts',(3.85507599179486,-1.3,9.6731246947563));
#27830=CARTESIAN_POINT('Ctrl Pts',(3.85826144216748,-1.3,9.6812761247605));
#27831=CARTESIAN_POINT('Ctrl Pts',(3.86592075441167,-1.29999999999977,9.69085660595971));
#27832=CARTESIAN_POINT('Ctrl Pts',(3.87702049239362,-1.29999999999969,9.70505728721368));
#27833=CARTESIAN_POINT('Ctrl Pts',(3.88609751225379,-1.29999999999954,9.71696191407332));
#27834=CARTESIAN_POINT('Ctrl Pts',(3.89668925414945,-1.29999999999939,9.73180622961143));
#27835=CARTESIAN_POINT('Ctrl Pts',(3.90634129735435,-1.29999999999907,9.74759065323404));
#27836=CARTESIAN_POINT('Ctrl Pts',(3.92055275904235,-1.29999999999887,9.76714384265834));
#27837=CARTESIAN_POINT('Ctrl Pts',(3.9429340522804,-1.29999999999834,9.80416499781408));
#27838=CARTESIAN_POINT('Ctrl Pts',(3.96875291306392,-1.29999999999679,9.84603918270465));
#27839=CARTESIAN_POINT('Ctrl Pts',(3.9873515828036,-1.29999999999548,9.87931932511112));
#27840=CARTESIAN_POINT('Ctrl Pts',(3.99403512297734,-1.29999999999538,9.89169252950719));
#27841=CARTESIAN_POINT('Ctrl Pts',(3.99548245121696,-1.29999999999538,9.89448355290195));
#27842=CARTESIAN_POINT('Ctrl Pts',(3.99797166780201,-1.29999999999536,9.89941379417338));
#27843=CARTESIAN_POINT('Ctrl Pts',(4.00320446632786,-1.29999999999526,9.90899225940416));
#27844=CARTESIAN_POINT('Ctrl Pts',(4.00794236274215,-1.29999999999492,9.91824630352297));
#27845=CARTESIAN_POINT('Ctrl Pts',(4.01134148578579,-1.29999999999461,9.92459663707328));
#27846=CARTESIAN_POINT('Ctrl Pts',(4.01179369694582,-1.29999999999457,9.92543782411959));
#27847=CARTESIAN_POINT('',(3.68876499470921,-1.2999999999998,10.3488907275642));
#27848=CARTESIAN_POINT('Origin',(0.,-1.3,7.2));
#27849=CARTESIAN_POINT('',(3.4147584711704,-1.3,10.2524562333546));
#27850=CARTESIAN_POINT('Ctrl Pts',(3.68876499511134,-1.29999999999967,10.3488907275609));
#27851=CARTESIAN_POINT('Ctrl Pts',(3.68778157068785,-1.29999999999968,10.3486180302189));
#27852=CARTESIAN_POINT('Ctrl Pts',(3.68093562331016,-1.29999999999968,10.34668418986));
#27853=CARTESIAN_POINT('Ctrl Pts',(3.66853450170539,-1.29999999999972,10.342623977583));
#27854=CARTESIAN_POINT('Ctrl Pts',(3.65042204492734,-1.29999999999974,10.3384258601431));
#27855=CARTESIAN_POINT('Ctrl Pts',(3.63654746083435,-1.29999999999975,10.333034031973));
#27856=CARTESIAN_POINT('Ctrl Pts',(3.62446370502866,-1.29999999999976,10.3302238019511));
#27857=CARTESIAN_POINT('Ctrl Pts',(3.60720160452375,-1.29999999999979,10.3246930658666));
#27858=CARTESIAN_POINT('Ctrl Pts',(3.58378319929591,-1.29999999999981,10.3178735693703));
#27859=CARTESIAN_POINT('Ctrl Pts',(3.5613867219776,-1.29999999999984,10.309500573553));
#27860=CARTESIAN_POINT('Ctrl Pts',(3.53855149764872,-1.29999999999986,10.3017508966992));
#27861=CARTESIAN_POINT('Ctrl Pts',(3.51929591785349,-1.29999999999993,10.2939294651204));
#27862=CARTESIAN_POINT('Ctrl Pts',(3.49657587699449,-1.29999999999993,10.2859305508819));
#27863=CARTESIAN_POINT('Ctrl Pts',(3.48022950006539,-1.29999999999995,10.2789860295796));
#27864=CARTESIAN_POINT('Ctrl Pts',(3.46380404043213,-1.29999999999997,10.2720051436094));
#27865=CARTESIAN_POINT('Ctrl Pts',(3.4502201710553,-1.29999999999997,10.2662412177574));
#27866=CARTESIAN_POINT('Ctrl Pts',(3.43423105359296,-1.29999999999999,10.258649491102));
#27867=CARTESIAN_POINT('Ctrl Pts',(3.42329004793793,-1.3,10.2535552330257));
#27868=CARTESIAN_POINT('Ctrl Pts',(3.4147584711704,-1.3,10.2524562333546));
#27869=CARTESIAN_POINT('',(3.2566417951307,-1.3,10.4205963541764));
#27870=CARTESIAN_POINT('',(3.4147584711704,-1.3,10.2524562333546));
#27871=CARTESIAN_POINT('',(3.35750201349686,-1.30000000000001,10.6999543181825));
#27872=CARTESIAN_POINT('Ctrl Pts',(3.2566417951307,-1.3,10.4205963541764));
#27873=CARTESIAN_POINT('Ctrl Pts',(3.25806285817521,-1.3,10.4292319482506));
#27874=CARTESIAN_POINT('Ctrl Pts',(3.26356969889493,-1.3,10.4401936173529));
#27875=CARTESIAN_POINT('Ctrl Pts',(3.27142362945852,-1.3,10.4564287702392));
#27876=CARTESIAN_POINT('Ctrl Pts',(3.27796208619394,-1.3,10.4698652030682));
#27877=CARTESIAN_POINT('Ctrl Pts',(3.2860779275434,-1.3,10.4896409410859));
#27878=CARTESIAN_POINT('Ctrl Pts',(3.29502533151807,-1.3,10.5123524713942));
#27879=CARTESIAN_POINT('Ctrl Pts',(3.30450367753534,-1.3,10.5347011036463));
#27880=CARTESIAN_POINT('Ctrl Pts',(3.31134556628297,-1.30000000000001,10.5553067937749));
#27881=CARTESIAN_POINT('Ctrl Pts',(3.31769888764456,-1.30000000000001,10.5725971040919));
#27882=CARTESIAN_POINT('Ctrl Pts',(3.32402656077159,-1.30000000000001,10.5898959986511));
#27883=CARTESIAN_POINT('Ctrl Pts',(3.32983519550124,-1.30000000000001,10.6075611244656));
#27884=CARTESIAN_POINT('Ctrl Pts',(3.33543431689405,-1.30000000000001,10.6253660208349));
#27885=CARTESIAN_POINT('Ctrl Pts',(3.34094149524616,-1.30000000000001,10.6432126996063));
#27886=CARTESIAN_POINT('Ctrl Pts',(3.34862517899022,-1.30000000000001,10.6667657263109));
#27887=CARTESIAN_POINT('Ctrl Pts',(3.35346931197927,-1.30000000000001,10.6861420881869));
#27888=CARTESIAN_POINT('Ctrl Pts',(3.35723434756309,-1.30000000000001,10.6990438624022));
#27889=CARTESIAN_POINT('Ctrl Pts',(3.35750201347149,-1.30000000000001,10.6999543180962));
#27890=CARTESIAN_POINT('',(2.95346386085648,-1.30000000000038,11.0470184848632));
#27891=CARTESIAN_POINT('Origin',(0.,-1.3,7.2));
#27892=CARTESIAN_POINT('',(2.70549646903679,-1.3,10.8957209484761));
#27893=CARTESIAN_POINT('Ctrl Pts',(2.95346386122922,-1.30000000000034,11.0470184849348));
#27894=CARTESIAN_POINT('Ctrl Pts',(2.95255855788318,-1.30000000000034,11.046547241464));
#27895=CARTESIAN_POINT('Ctrl Pts',(2.9462642246173,-1.30000000000027,11.0432322378643));
#27896=CARTESIAN_POINT('Ctrl Pts',(2.93497824004344,-1.30000000000034,11.0366822995913));
#27897=CARTESIAN_POINT('Ctrl Pts',(2.91813452753453,-1.30000000000025,11.0288099698744));
#27898=CARTESIAN_POINT('Ctrl Pts',(2.90568427085911,-1.30000000000026,11.0206511408273));
#27899=CARTESIAN_POINT('Ctrl Pts',(2.8944488945071,-1.30000000000025,11.0153899166468));
#27900=CARTESIAN_POINT('Ctrl Pts',(2.87871424024048,-1.30000000000023,11.0063906910495));
#27901=CARTESIAN_POINT('Ctrl Pts',(2.85722596337419,-1.3000000000002,10.994850673871));
#27902=CARTESIAN_POINT('Ctrl Pts',(2.83706008972697,-1.30000000000017,10.9820037922093));
#27903=CARTESIAN_POINT('Ctrl Pts',(2.81633525801823,-1.30000000000013,10.9696756101453));
#27904=CARTESIAN_POINT('Ctrl Pts',(2.7991269778593,-1.30000000000009,10.9580213491863));
#27905=CARTESIAN_POINT('Ctrl Pts',(2.77856646432003,-1.30000000000008,10.9454735069678));
#27906=CARTESIAN_POINT('Ctrl Pts',(2.76402116993851,-1.30000000000005,10.9352822600267));
#27907=CARTESIAN_POINT('Ctrl Pts',(2.74940605748609,-1.30000000000005,10.9250389677111));
#27908=CARTESIAN_POINT('Ctrl Pts',(2.73731735276373,-1.30000000000003,10.9165770042152));
#27909=CARTESIAN_POINT('Ctrl Pts',(2.72325603000415,-1.30000000000001,10.9058269403026));
#27910=CARTESIAN_POINT('Ctrl Pts',(2.71361311550261,-1.3,10.8985697469187));
#27911=CARTESIAN_POINT('Ctrl Pts',(2.70549646903679,-1.3,10.8957209484761));
#27912=CARTESIAN_POINT('',(2.5158767249182,-1.3,11.0273124987831));
#27913=CARTESIAN_POINT('',(2.70549646903679,-1.3,10.8957209484761));
#27914=CARTESIAN_POINT('',(2.55649102449489,-1.30000000000196,11.3215110871707));
#27915=CARTESIAN_POINT('Ctrl Pts',(2.5158767249182,-1.3,11.0273124987831));
#27916=CARTESIAN_POINT('Ctrl Pts',(2.51547129336049,-1.3,11.036054840028));
#27917=CARTESIAN_POINT('Ctrl Pts',(2.5185714677897,-1.30000000000023,11.0479195112411));
#27918=CARTESIAN_POINT('Ctrl Pts',(2.52295716596346,-1.30000000000031,11.06539891157));
#27919=CARTESIAN_POINT('Ctrl Pts',(2.52635301603749,-1.30000000000046,11.0799823544973));
#27920=CARTESIAN_POINT('Ctrl Pts',(2.52949729038838,-1.30000000000058,11.0948340954078));
#27921=CARTESIAN_POINT('Ctrl Pts',(2.53115568101867,-1.3000000000007,11.1070342157947));
#27922=CARTESIAN_POINT('Ctrl Pts',(2.53311426036291,-1.30000000000078,11.1191314014661));
#27923=CARTESIAN_POINT('Ctrl Pts',(2.53754735173857,-1.30000000000096,11.139780364975));
#27924=CARTESIAN_POINT('Ctrl Pts',(2.54105191070822,-1.30000000000149,11.1706110977417));
#27925=CARTESIAN_POINT('Ctrl Pts',(2.54573452006113,-1.30000000000204,11.2008309367231));
#27926=CARTESIAN_POINT('Ctrl Pts',(2.54836608072526,-1.30000000000237,11.2255071987807));
#27927=CARTESIAN_POINT('Ctrl Pts',(2.54980989363996,-1.30000000000288,11.2393849186443));
#27928=CARTESIAN_POINT('Ctrl Pts',(2.55054244654306,-1.30000000000289,11.2487391367418));
#27929=CARTESIAN_POINT('Ctrl Pts',(2.55109152476666,-1.30000000000291,11.2549467364804));
#27930=CARTESIAN_POINT('Ctrl Pts',(2.55189116477319,-1.30000000000301,11.262654253516));
#27931=CARTESIAN_POINT('Ctrl Pts',(2.55305163254523,-1.30000000000305,11.2718129170801));
#27932=CARTESIAN_POINT('Ctrl Pts',(2.55465518880789,-1.30000000000349,11.2904402301689));
#27933=CARTESIAN_POINT('Ctrl Pts',(2.55552695808368,-1.30000000000399,11.3071186494231));
#27934=CARTESIAN_POINT('Ctrl Pts',(2.55642674563612,-1.30000000000449,11.3205610386322));
#27935=CARTESIAN_POINT('Ctrl Pts',(2.55649102449025,-1.30000000000453,11.3215110871003));
#27936=CARTESIAN_POINT('',(2.08915688129593,-1.30000000000187,11.576970137216));
#27937=CARTESIAN_POINT('Origin',(0.,-1.3,7.2));
#27938=CARTESIAN_POINT('',(1.87799128879385,-1.3,11.3774649241125));
#27939=CARTESIAN_POINT('Ctrl Pts',(2.08915200586581,-1.30000000000102,11.576966073662));
#27940=CARTESIAN_POINT('Ctrl Pts',(2.08836889275514,-1.30000000000101,11.5763133523961));
#27941=CARTESIAN_POINT('Ctrl Pts',(2.0829231840913,-1.30000000000101,11.5717486188595));
#27942=CARTESIAN_POINT('Ctrl Pts',(2.07532697621286,-1.30000000000088,11.5651096373284));
#27943=CARTESIAN_POINT('Ctrl Pts',(2.0670360910251,-1.30000000000089,11.5583394095983));
#27944=CARTESIAN_POINT('Ctrl Pts',(2.06279202116117,-1.30000000000088,11.5550170835899));
#27945=CARTESIAN_POINT('Ctrl Pts',(2.06041334439402,-1.30000000000088,11.5530881430355));
#27946=CARTESIAN_POINT('Ctrl Pts',(2.05008175662487,-1.30000000000087,11.5441639496953));
#27947=CARTESIAN_POINT('Ctrl Pts',(2.02156140521154,-1.3000000000006,11.5201193794785));
#27948=CARTESIAN_POINT('Ctrl Pts',(1.98618970204262,-1.30000000000032,11.4873857546922));
#27949=CARTESIAN_POINT('Ctrl Pts',(1.95657107896346,-1.30000000000022,11.4578927873005));
#27950=CARTESIAN_POINT('Ctrl Pts',(1.9391923383441,-1.30000000000018,11.4412683292772));
#27951=CARTESIAN_POINT('Ctrl Pts',(1.9270492632946,-1.30000000000012,11.4283111506914));
#27952=CARTESIAN_POINT('Ctrl Pts',(1.91488011008762,-1.30000000000009,11.4152490614082));
#27953=CARTESIAN_POINT('Ctrl Pts',(1.90480129625264,-1.30000000000006,11.4044692218263));
#27954=CARTESIAN_POINT('Ctrl Pts',(1.89327770969982,-1.30000000000004,11.3910324012891));
#27955=CARTESIAN_POINT('Ctrl Pts',(1.88533826855939,-1.3,11.3819390151645));
#27956=CARTESIAN_POINT('Ctrl Pts',(1.87799128879384,-1.3,11.3774649241125));
#27957=CARTESIAN_POINT('',(1.66515576931082,-1.3,11.46675672171));
#27958=CARTESIAN_POINT('',(1.87799128879384,-1.3,11.3774649241125));
#27959=CARTESIAN_POINT('',(1.64376583932815,-1.3,11.7629523189989));
#27960=CARTESIAN_POINT('Ctrl Pts',(1.66515576931082,-1.3,11.46675672171));
#27961=CARTESIAN_POINT('Ctrl Pts',(1.66294156245546,-1.3,11.4752237278628));
#27962=CARTESIAN_POINT('Ctrl Pts',(1.66352992364857,-1.3,11.4874744137729));
#27963=CARTESIAN_POINT('Ctrl Pts',(1.66410716288398,-1.3,11.505499322124));
#27964=CARTESIAN_POINT('Ctrl Pts',(1.66462615833061,-1.3,11.5204313880075));
#27965=CARTESIAN_POINT('Ctrl Pts',(1.66400832169345,-1.3,11.5417962198324));
#27966=CARTESIAN_POINT('Ctrl Pts',(1.6629753934554,-1.3,11.5661771710961));
#27967=CARTESIAN_POINT('Ctrl Pts',(1.66253954923371,-1.29999999999999,11.5904501135858));
#27968=CARTESIAN_POINT('Ctrl Pts',(1.66047989040796,-1.29999999999999,11.6120422433131));
#27969=CARTESIAN_POINT('Ctrl Pts',(1.65917440129576,-1.29999999999999,11.6304388748568));
#27970=CARTESIAN_POINT('Ctrl Pts',(1.65825661873327,-1.29999999999999,11.6457250585537));
#27971=CARTESIAN_POINT('Ctrl Pts',(1.65692536543947,-1.3,11.6580787419226));
#27972=CARTESIAN_POINT('Ctrl Pts',(1.65574912520357,-1.3,11.6703942470278));
#27973=CARTESIAN_POINT('Ctrl Pts',(1.6519973873214,-1.29999999999997,11.704362262037));
#27974=CARTESIAN_POINT('Ctrl Pts',(1.64727440390851,-1.29999999999999,11.7363420669453));
#27975=CARTESIAN_POINT('Ctrl Pts',(1.64388919338363,-1.29999999999999,11.7620157535565));
#27976=CARTESIAN_POINT('Ctrl Pts',(1.64376583933432,-1.29999999999999,11.7629523189521));
#27977=CARTESIAN_POINT('',(1.13367999186515,-1.30000000000007,11.9156231271707));
#27978=CARTESIAN_POINT('Origin',(0.,-1.3,7.2));
#27979=CARTESIAN_POINT('',(0.968408877628581,-1.3,11.6766336368644));
#27980=CARTESIAN_POINT('Ctrl Pts',(1.13366791254867,-1.30000000000001,11.9156081970114));
#27981=CARTESIAN_POINT('Ctrl Pts',(1.13302390437827,-1.30000000000001,11.9148121906901));
#27982=CARTESIAN_POINT('Ctrl Pts',(1.12468637038362,-1.30000000000001,11.9045010017064));
#27983=CARTESIAN_POINT('Ctrl Pts',(1.10885180968865,-1.30000000000001,11.884587008504));
#27984=CARTESIAN_POINT('Ctrl Pts',(1.08716165682344,-1.3,11.855446045349));
#27985=CARTESIAN_POINT('Ctrl Pts',(1.06841695418305,-1.3,11.8313959298596));
#27986=CARTESIAN_POINT('Ctrl Pts',(1.05531692441144,-1.3,11.8114079524741));
#27987=CARTESIAN_POINT('Ctrl Pts',(1.03972439720481,-1.3,11.7892518976243));
#27988=CARTESIAN_POINT('Ctrl Pts',(1.0233484645155,-1.3,11.7642300009282));
#27989=CARTESIAN_POINT('Ctrl Pts',(1.00703467199694,-1.3,11.739219370099));
#27990=CARTESIAN_POINT('Ctrl Pts',(0.996639789377799,-1.3,11.7212674543396));
#27991=CARTESIAN_POINT('Ctrl Pts',(0.988936150867075,-1.3,11.7086498444923));
#27992=CARTESIAN_POINT('Ctrl Pts',(0.980511229803915,-1.3,11.6930945208311));
#27993=CARTESIAN_POINT('Ctrl Pts',(0.974665092423395,-1.3,11.6825374812779));
#27994=CARTESIAN_POINT('Ctrl Pts',(0.968408877628581,-1.3,11.6766336368644));
#27995=CARTESIAN_POINT('',(0.741659516280668,-1.3,11.7197232017278));
#27996=CARTESIAN_POINT('',(0.968408877628581,-1.3,11.6766336368644));
#27997=CARTESIAN_POINT('',(0.659062828598954,-1.29999999999948,12.0050115700132));
#27998=CARTESIAN_POINT('Ctrl Pts',(0.741659516280668,-1.3,11.7197232017278));
#27999=CARTESIAN_POINT('Ctrl Pts',(0.739042042488337,-1.3,11.7249376165696));
#28000=CARTESIAN_POINT('Ctrl Pts',(0.736513353027037,-1.29999999999997,
11.7335029101655));
#28001=CARTESIAN_POINT('Ctrl Pts',(0.734690372091585,-1.29999999999996,
11.7455625251115));
#28002=CARTESIAN_POINT('Ctrl Pts',(0.732507359893533,-1.29999999999992,
11.7573468723061));
#28003=CARTESIAN_POINT('Ctrl Pts',(0.729739714965371,-1.2999999999999,11.7720784210858));
#28004=CARTESIAN_POINT('Ctrl Pts',(0.726871111169886,-1.29999999999987,
11.7854327933035));
#28005=CARTESIAN_POINT('Ctrl Pts',(0.724391632493095,-1.29999999999985,
11.7943012189907));
#28006=CARTESIAN_POINT('Ctrl Pts',(0.722742798682037,-1.29999999999985,
11.8002248077555));
#28007=CARTESIAN_POINT('Ctrl Pts',(0.719941170551377,-1.2999999999998,11.8105870027121));
#28008=CARTESIAN_POINT('Ctrl Pts',(0.715773049841678,-1.29999999999985,
11.8312567595427));
#28009=CARTESIAN_POINT('Ctrl Pts',(0.708106339592658,-1.29999999999956,
11.854933747163));
#28010=CARTESIAN_POINT('Ctrl Pts',(0.701392717589497,-1.29999999999949,
11.8785605604877));
#28011=CARTESIAN_POINT('Ctrl Pts',(0.696379212651565,-1.29999999999946,
11.896276690909));
#28012=CARTESIAN_POINT('Ctrl Pts',(0.690660095299637,-1.29999999999939,
11.9139835115396));
#28013=CARTESIAN_POINT('Ctrl Pts',(0.68477416176603,-1.29999999999933,11.9316792283626));
#28014=CARTESIAN_POINT('Ctrl Pts',(0.678549186698806,-1.29999999999919,
11.9493585018481));
#28015=CARTESIAN_POINT('Ctrl Pts',(0.674222718308847,-1.29999999999909,
11.9640876094411));
#28016=CARTESIAN_POINT('Ctrl Pts',(0.667369721617829,-1.29999999999903,
11.9817468175655));
#28017=CARTESIAN_POINT('Ctrl Pts',(0.663034818602077,-1.29999999999887,
11.9943987309871));
#28018=CARTESIAN_POINT('Ctrl Pts',(0.659399632431257,-1.29999999999879,
12.0041138042021));
#28019=CARTESIAN_POINT('Ctrl Pts',(0.659062828590475,-1.29999999999879,
12.0050115700357));
#28020=CARTESIAN_POINT('',(0.128218778230027,-1.30000000000009,12.0483048527994));
#28021=CARTESIAN_POINT('Origin',(0.,-1.3,7.2));
#28022=CARTESIAN_POINT('',(0.0165023515695838,-1.3,11.7801519784138));
#28023=CARTESIAN_POINT('Ctrl Pts',(0.12821877865013,-1.30000000000002,12.0483048532947));
#28024=CARTESIAN_POINT('Ctrl Pts',(0.127767437989379,-1.30000000000002,
12.0473919903599));
#28025=CARTESIAN_POINT('Ctrl Pts',(0.124640289790951,-1.30000000000002,
12.0410103084665));
#28026=CARTESIAN_POINT('Ctrl Pts',(0.120462273527711,-1.30000000000002,
12.0318473446916));
#28027=CARTESIAN_POINT('Ctrl Pts',(0.114879864456106,-1.30000000000002,
12.0209362197056));
#28028=CARTESIAN_POINT('Ctrl Pts',(0.109188261488994,-1.30000000000002,
12.0100407684408));
#28029=CARTESIAN_POINT('Ctrl Pts',(0.103562192797069,-1.3,11.996174288113));
#28030=CARTESIAN_POINT('Ctrl Pts',(0.0947946336556477,-1.30000000000001,
11.9798529787365));
#28031=CARTESIAN_POINT('Ctrl Pts',(0.0830130309314115,-1.3,11.9521871509241));
#28032=CARTESIAN_POINT('Ctrl Pts',(0.0682437123210014,-1.30000000000001,
11.9190458604758));
#28033=CARTESIAN_POINT('Ctrl Pts',(0.0556483962277135,-1.3,11.8855803936));
#28034=CARTESIAN_POINT('Ctrl Pts',(0.0464357783186146,-1.3,11.8633387174799));
#28035=CARTESIAN_POINT('Ctrl Pts',(0.0406518797624009,-1.3,11.8465564726808));
#28036=CARTESIAN_POINT('Ctrl Pts',(0.0348304131678258,-1.3,11.8296763358228));
#28037=CARTESIAN_POINT('Ctrl Pts',(0.0300137202382597,-1.3,11.8157274242518));
#28038=CARTESIAN_POINT('Ctrl Pts',(0.0249486472265611,-1.3,11.798765411714));
#28039=CARTESIAN_POINT('Ctrl Pts',(0.0213943747864759,-1.3,11.7872275498581));
#28040=CARTESIAN_POINT('Ctrl Pts',(0.0165023515695838,-1.3,11.7801519784138));
#28041=CARTESIAN_POINT('',(-0.214250816488161,-1.3,11.775156089792));
#28042=CARTESIAN_POINT('',(0.0165023515695838,-1.3,11.7801519784138));
#28043=CARTESIAN_POINT('',(-0.354232945953444,-1.3,12.0370465182796));
#28044=CARTESIAN_POINT('Ctrl Pts',(-0.214250816488157,-1.3,11.775156089792));
#28045=CARTESIAN_POINT('Ctrl Pts',(-0.226776816940669,-1.3,11.7908161580662));
#28046=CARTESIAN_POINT('Ctrl Pts',(-0.229117821703532,-1.29999999999933,
11.816545516841));
#28047=CARTESIAN_POINT('Ctrl Pts',(-0.314361841081013,-1.29999999999933,
11.9736092487021));
#28048=CARTESIAN_POINT('Ctrl Pts',(-0.33156106808883,-1.3,11.9999679942315));
#28049=CARTESIAN_POINT('Ctrl Pts',(-0.354232945953442,-1.3,12.0370465182796));
#28050=CARTESIAN_POINT('',(-0.882581877102588,-1.30000000000383,11.9690197346898));
#28051=CARTESIAN_POINT('Origin',(0.,-1.3,7.2));
#28052=CARTESIAN_POINT('',(-0.936125406440075,-1.3,11.683495700499));
#28053=CARTESIAN_POINT('Ctrl Pts',(-0.882581877071048,-1.3,11.9690197346817));
#28054=CARTESIAN_POINT('Ctrl Pts',(-0.882808795626795,-1.3,11.9681439377607));
#28055=CARTESIAN_POINT('Ctrl Pts',(-0.883062784706584,-1.3,11.9671488844407));
#28056=CARTESIAN_POINT('Ctrl Pts',(-0.88333561661655,-1.3,11.9660476844872));
#28057=CARTESIAN_POINT('Ctrl Pts',(-0.88444610261044,-1.3,11.96156555802));
#28058=CARTESIAN_POINT('Ctrl Pts',(-0.885768767111217,-1.3,11.955301283602));
#28059=CARTESIAN_POINT('Ctrl Pts',(-0.887564373833532,-1.3,11.9483389250401));
#28060=CARTESIAN_POINT('Ctrl Pts',(-0.889007412258535,-1.3,11.942743629139));
#28061=CARTESIAN_POINT('Ctrl Pts',(-0.890845883878463,-1.3,11.9367181788242));
#28062=CARTESIAN_POINT('Ctrl Pts',(-0.89225592342973,-1.3,11.9305935570264));
#28063=CARTESIAN_POINT('Ctrl Pts',(-0.893647676455054,-1.3,11.9245483642455));
#28064=CARTESIAN_POINT('Ctrl Pts',(-0.894627819898128,-1.3,11.9184090511601));
#28065=CARTESIAN_POINT('Ctrl Pts',(-0.896030179377485,-1.3,11.912883875931));
#28066=CARTESIAN_POINT('Ctrl Pts',(-0.896833031705652,-1.3,11.9097207070992));
#28067=CARTESIAN_POINT('Ctrl Pts',(-0.89773423291985,-1.3,11.9067490121674));
#28068=CARTESIAN_POINT('Ctrl Pts',(-0.898453790759213,-1.3,11.9039975125493));
#28069=CARTESIAN_POINT('Ctrl Pts',(-0.899333475274128,-1.3,11.9006337084541));
#28070=CARTESIAN_POINT('Ctrl Pts',(-0.89998356318908,-1.3,11.8976091563924));
#28071=CARTESIAN_POINT('Ctrl Pts',(-0.900535947202928,-1.3,11.8951297300085));
#28072=CARTESIAN_POINT('Ctrl Pts',(-0.901673468155476,-1.3,11.8900238627289));
#28073=CARTESIAN_POINT('Ctrl Pts',(-0.902046559818047,-1.3,11.8883980818041));
#28074=CARTESIAN_POINT('Ctrl Pts',(-0.902341267799144,-1.3,11.8870932461531));
#28075=CARTESIAN_POINT('Ctrl Pts',(-0.902635975780242,-1.3,11.8857884105021));
#28076=CARTESIAN_POINT('Ctrl Pts',(-0.902931032114102,-1.3,11.8844836710949));
#28077=CARTESIAN_POINT('Ctrl Pts',(-0.903225882890785,-1.3,11.8831788717348));
#28078=CARTESIAN_POINT('Ctrl Pts',(-0.903815584444153,-1.3,11.8805692730148));
#28079=CARTESIAN_POINT('Ctrl Pts',(-0.904404468432412,-1.3,11.8779594230048));
#28080=CARTESIAN_POINT('Ctrl Pts',(-0.904988061452789,-1.3,11.8753482266002));
#28081=CARTESIAN_POINT('Ctrl Pts',(-0.906155247493544,-1.3,11.8701258337912));
#28082=CARTESIAN_POINT('Ctrl Pts',(-0.907301396337968,-1.3,11.8648979451309));
#28083=CARTESIAN_POINT('Ctrl Pts',(-0.908389551665395,-1.3,11.8596576184927));
#28084=CARTESIAN_POINT('Ctrl Pts',(-0.910831876163998,-1.3,11.8478958986293));
#28085=CARTESIAN_POINT('Ctrl Pts',(-0.912979520196815,-1.3,11.8360733641414));
#28086=CARTESIAN_POINT('Ctrl Pts',(-0.915007770053264,-1.3,11.8242316349802));
#28087=CARTESIAN_POINT('Ctrl Pts',(-0.917028179777949,-1.3,11.8124356796258));
#28088=CARTESIAN_POINT('Ctrl Pts',(-0.918931529702551,-1.3,11.8006199242949));
#28089=CARTESIAN_POINT('Ctrl Pts',(-0.920981332184873,-1.3,11.7888327519991));
#28090=CARTESIAN_POINT('Ctrl Pts',(-0.921072479857284,-1.3,11.7883086169527));
#28091=CARTESIAN_POINT('Ctrl Pts',(-0.92116391556169,-1.3,11.7877845386678));
#28092=CARTESIAN_POINT('Ctrl Pts',(-0.921255506017709,-1.3,11.7872604942856));
#28093=CARTESIAN_POINT('Ctrl Pts',(-0.921599708986489,-1.3,11.785291100967));
#28094=CARTESIAN_POINT('Ctrl Pts',(-0.922341321043407,-1.3,11.781792726034));
#28095=CARTESIAN_POINT('Ctrl Pts',(-0.923980128118824,-1.3,11.7711124286227));
#28096=CARTESIAN_POINT('Ctrl Pts',(-0.924788538415726,-1.3,11.7658439241533));
#28097=CARTESIAN_POINT('Ctrl Pts',(-0.925589291106062,-1.3,11.7596504825016));
#28098=CARTESIAN_POINT('Ctrl Pts',(-0.92635697777491,-1.3,11.7534461585483));
#28099=CARTESIAN_POINT('Ctrl Pts',(-0.927121899806116,-1.3,11.7472641779653));
#28100=CARTESIAN_POINT('Ctrl Pts',(-0.927871372060883,-1.3,11.741073829877));
#28101=CARTESIAN_POINT('Ctrl Pts',(-0.928520999957708,-1.3,11.7357687097838));
#28102=CARTESIAN_POINT('Ctrl Pts',(-0.929364645543441,-1.3,11.7288791639835));
#28103=CARTESIAN_POINT('Ctrl Pts',(-0.930049426493481,-1.3,11.7231571743506));
#28104=CARTESIAN_POINT('Ctrl Pts',(-0.93052372837535,-1.3,11.7181547759627));
#28105=CARTESIAN_POINT('Ctrl Pts',(-0.930834677160099,-1.3,11.7148752407995));
#28106=CARTESIAN_POINT('Ctrl Pts',(-0.931065957287747,-1.3,11.7119438225555));
#28107=CARTESIAN_POINT('Ctrl Pts',(-0.931282157598271,-1.3,11.7093208443881));
#28108=CARTESIAN_POINT('Ctrl Pts',(-0.932829264363458,-1.3,11.6905510875003));
#28109=CARTESIAN_POINT('Ctrl Pts',(-0.934376840494585,-1.3,11.6876840266721));
#28110=CARTESIAN_POINT('Ctrl Pts',(-0.936125406440076,-1.3,11.683495700499));
#28111=CARTESIAN_POINT('',(-0.936125406440075,-1.3,11.683495700499));
#28112=CARTESIAN_POINT('Origin',(0.,1.275,7.2));
#28113=CARTESIAN_POINT('',(4.10256677714363E-16,1.3,10.55));
#28114=CARTESIAN_POINT('',(4.07195060716495E-16,1.275,10.525));
#28115=CARTESIAN_POINT('Origin',(0.,1.3,7.2));
#28116=CARTESIAN_POINT('Origin',(0.,1.3,10.5));
#28117=CARTESIAN_POINT('',(-1.13329432476672,1.3,11.9157336622684));
#28118=CARTESIAN_POINT('',(-0.968408877628584,1.3,11.6766336368644));
#28119=CARTESIAN_POINT('Ctrl Pts',(-1.13329432476672,1.3,11.9157336622684));
#28120=CARTESIAN_POINT('Ctrl Pts',(-1.09357982029352,1.3,11.8656069040482));
#28121=CARTESIAN_POINT('Ctrl Pts',(-1.03481352213628,1.30000000000027,11.78447477828));
#28122=CARTESIAN_POINT('Ctrl Pts',(-0.993644753278957,1.30000000000027,
11.7162670765878));
#28123=CARTESIAN_POINT('Ctrl Pts',(-0.992137613505443,1.30000000000026,
11.7141259017487));
#28124=CARTESIAN_POINT('Ctrl Pts',(-0.980066579642223,1.30000000000026,
11.6923013287743));
#28125=CARTESIAN_POINT('Ctrl Pts',(-0.975396089277502,1.3,11.6832273059784));
#28126=CARTESIAN_POINT('Ctrl Pts',(-0.968408877628581,1.3,11.6766336368644));
#28127=CARTESIAN_POINT('',(-0.741659516280671,1.3,11.7197232017278));
#28128=CARTESIAN_POINT('',(-0.968408877628584,1.3,11.6766336368644));
#28129=CARTESIAN_POINT('',(-0.659151153699352,1.29999999999999,12.0049994543784));
#28130=CARTESIAN_POINT('Ctrl Pts',(-0.741659516280671,1.3,11.7197232017278));
#28131=CARTESIAN_POINT('Ctrl Pts',(-0.737733305603289,1.3,11.727544824049));
#28132=CARTESIAN_POINT('Ctrl Pts',(-0.735751588984198,1.3,11.7396469846747));
#28133=CARTESIAN_POINT('Ctrl Pts',(-0.732635446296485,1.3,11.7573965790848));
#28134=CARTESIAN_POINT('Ctrl Pts',(-0.72985761739672,1.3,11.7721099993479));
#28135=CARTESIAN_POINT('Ctrl Pts',(-0.725954358660486,1.3,11.7899072742885));
#28136=CARTESIAN_POINT('Ctrl Pts',(-0.720616710375773,1.3,11.8076573420007));
#28137=CARTESIAN_POINT('Ctrl Pts',(-0.715898913230529,1.3,11.8312928575073));
#28138=CARTESIAN_POINT('Ctrl Pts',(-0.706317872537295,1.29999999999998,
11.8608672626166));
#28139=CARTESIAN_POINT('Ctrl Pts',(-0.696599728536621,1.29999999999999,
11.8962911605939));
#28140=CARTESIAN_POINT('Ctrl Pts',(-0.687924960193452,1.29999999999998,
11.9228443737029));
#28141=CARTESIAN_POINT('Ctrl Pts',(-0.681633248701518,1.29999999999998,
11.9405257597102));
#28142=CARTESIAN_POINT('Ctrl Pts',(-0.677918881824272,1.29999999999998,
11.9523134141152));
#28143=CARTESIAN_POINT('Ctrl Pts',(-0.673216514165749,1.29999999999998,
11.9670400942954));
#28144=CARTESIAN_POINT('Ctrl Pts',(-0.666547092405337,1.29999999999998,
11.9846968609246));
#28145=CARTESIAN_POINT('Ctrl Pts',(-0.661903094886713,1.29999999999998,
11.9973370975437));
#28146=CARTESIAN_POINT('Ctrl Pts',(-0.659471134965142,1.29999999999998,
12.00410729267));
#28147=CARTESIAN_POINT('Ctrl Pts',(-0.659151153717024,1.29999999999998,
12.0049994543292));
#28148=CARTESIAN_POINT('',(-0.128158081915158,1.30000000000259,12.0483064575425));
#28149=CARTESIAN_POINT('Origin',(0.,1.3,7.2));
#28150=CARTESIAN_POINT('',(-0.0165023515695838,1.3,11.7801519784138));
#28151=CARTESIAN_POINT('Ctrl Pts',(-0.128158082004638,1.30000000000001,
12.0483064576567));
#28152=CARTESIAN_POINT('Ctrl Pts',(-0.127706543597735,1.30000000000001,
12.0473941560219));
#28153=CARTESIAN_POINT('Ctrl Pts',(-0.124585249997123,1.30000000000001,
12.0410104377584));
#28154=CARTESIAN_POINT('Ctrl Pts',(-0.119344627363001,1.30000000000001,
12.0290727474592));
#28155=CARTESIAN_POINT('Ctrl Pts',(-0.110353620477029,1.30000000000001,
12.0128019553342));
#28156=CARTESIAN_POINT('Ctrl Pts',(-0.10505905347749,1.30000000000001,11.9988853872125));
#28157=CARTESIAN_POINT('Ctrl Pts',(-0.0990805943072033,1.30000000000001,
11.9880225704775));
#28158=CARTESIAN_POINT('Ctrl Pts',(-0.0915248950042503,1.30000000000001,
11.9715091494637));
#28159=CARTESIAN_POINT('Ctrl Pts',(-0.0802434788763688,1.29999999999999,
11.946707478996));
#28160=CARTESIAN_POINT('Ctrl Pts',(-0.065394987617947,1.30000000000001,
11.9106252544473));
#28161=CARTESIAN_POINT('Ctrl Pts',(-0.0532333790268668,1.3,11.8800519932815));
#28162=CARTESIAN_POINT('Ctrl Pts',(-0.0443578084944021,1.3,11.8577582069453));
#28163=CARTESIAN_POINT('Ctrl Pts',(-0.039728294969975,1.3,11.8437419949466));
#28164=CARTESIAN_POINT('Ctrl Pts',(-0.0347820509500467,1.3,11.8296771141586));
#28165=CARTESIAN_POINT('Ctrl Pts',(-0.0300196112300812,1.3,11.8157273049924));
#28166=CARTESIAN_POINT('Ctrl Pts',(-0.0249390517352318,1.3,11.798765550829));
#28167=CARTESIAN_POINT('Ctrl Pts',(-0.0213943747864967,1.3,11.7872275498223));
#28168=CARTESIAN_POINT('Ctrl Pts',(-0.0165023515695838,1.3,11.7801519784138));
#28169=CARTESIAN_POINT('',(0.214250816488161,1.3,11.775156089792));
#28170=CARTESIAN_POINT('',(-0.0165023515695838,1.3,11.7801519784138));
#28171=CARTESIAN_POINT('',(0.354270609538462,1.30000000000001,12.0370437599031));
#28172=CARTESIAN_POINT('Ctrl Pts',(0.214250816488161,1.3,11.775156089792));
#28173=CARTESIAN_POINT('Ctrl Pts',(0.219717436763954,1.3,11.7819904857988));
#28174=CARTESIAN_POINT('Ctrl Pts',(0.224173980653817,1.3,11.7934174209104));
#28175=CARTESIAN_POINT('Ctrl Pts',(0.23091560441885,1.3,11.8101320480681));
#28176=CARTESIAN_POINT('Ctrl Pts',(0.236687800958387,1.3,11.8239457500398));
#28177=CARTESIAN_POINT('Ctrl Pts',(0.244221948540284,1.3,11.8405462034363));
#28178=CARTESIAN_POINT('Ctrl Pts',(0.253104343833752,1.3,11.8567896804809));
#28179=CARTESIAN_POINT('Ctrl Pts',(0.262803958219338,1.3,11.8789010314179));
#28180=CARTESIAN_POINT('Ctrl Pts',(0.281070358318964,1.3,11.9113009100025));
#28181=CARTESIAN_POINT('Ctrl Pts',(0.29785247370303,1.30000000000001,11.9439420582747));
#28182=CARTESIAN_POINT('Ctrl Pts',(0.313963477925296,1.30000000000001,11.9706688915201));
#28183=CARTESIAN_POINT('Ctrl Pts',(0.323566005429044,1.30000000000001,11.9867005582315));
#28184=CARTESIAN_POINT('Ctrl Pts',(0.330874530740489,1.30000000000001,12.000206898768));
#28185=CARTESIAN_POINT('Ctrl Pts',(0.337855133813077,1.30000000000001,12.0107554280267));
#28186=CARTESIAN_POINT('Ctrl Pts',(0.344387552689543,1.30000000000001,12.0213987101841));
#28187=CARTESIAN_POINT('Ctrl Pts',(0.349955872658189,1.30000000000001,12.0301352547577));
#28188=CARTESIAN_POINT('Ctrl Pts',(0.353770133775808,1.30000000000001,12.03624110066));
#28189=CARTESIAN_POINT('Ctrl Pts',(0.354270609436508,1.30000000000001,12.0370437597396));
#28190=CARTESIAN_POINT('',(0.882649956952474,1.30000000000121,11.9690071349479));
#28191=CARTESIAN_POINT('Origin',(0.,1.3,7.2));
#28192=CARTESIAN_POINT('',(0.936125406440073,1.3,11.683495700499));
#28193=CARTESIAN_POINT('Ctrl Pts',(0.88264995692282,1.3,11.96900713494));
#28194=CARTESIAN_POINT('Ctrl Pts',(0.882911955670296,1.3,11.968026127732));
#28195=CARTESIAN_POINT('Ctrl Pts',(0.883173297900691,1.3,11.9670365544159));
#28196=CARTESIAN_POINT('Ctrl Pts',(0.883432313455179,1.3,11.9660383664123));
#28197=CARTESIAN_POINT('Ctrl Pts',(0.885606849944969,1.3,11.9576581892382));
#28198=CARTESIAN_POINT('Ctrl Pts',(0.887575729343874,1.3,11.9486660469659));
#28199=CARTESIAN_POINT('Ctrl Pts',(0.890061999938986,1.3,11.9394534486077));
#28200=CARTESIAN_POINT('Ctrl Pts',(0.890851962988844,1.3,11.9365263286432));
#28201=CARTESIAN_POINT('Ctrl Pts',(0.891699082744094,1.3,11.9335773147197));
#28202=CARTESIAN_POINT('Ctrl Pts',(0.892445456246523,1.3,11.9305767538767));
#28203=CARTESIAN_POINT('Ctrl Pts',(0.893884265071105,1.3,11.9247924737467));
#28204=CARTESIAN_POINT('Ctrl Pts',(0.894920505793652,1.3,11.9188138340153));
#28205=CARTESIAN_POINT('Ctrl Pts',(0.896299792001618,1.3,11.9128615900811));
#28206=CARTESIAN_POINT('Ctrl Pts',(0.897667983545716,1.3,11.9069572246403));
#28207=CARTESIAN_POINT('Ctrl Pts',(0.899382403484439,1.3,11.9010763914123));
#28208=CARTESIAN_POINT('Ctrl Pts',(0.9007277698223,1.3,11.8951124219187));
#28209=CARTESIAN_POINT('Ctrl Pts',(0.902056064238301,1.3,11.8892241317537));
#28210=CARTESIAN_POINT('Ctrl Pts',(0.903014046033323,1.3,11.883255972996));
#28211=CARTESIAN_POINT('Ctrl Pts',(0.904274193813204,1.3,11.8773973930454));
#28212=CARTESIAN_POINT('Ctrl Pts',(0.905564059685733,1.3,11.8714006500757));
#28213=CARTESIAN_POINT('Ctrl Pts',(0.907156121579215,1.3,11.8655127074693));
#28214=CARTESIAN_POINT('Ctrl Pts',(0.908366580665661,1.3,11.8596450271036));
#28215=CARTESIAN_POINT('Ctrl Pts',(0.909600827504593,1.3,11.8536620360018));
#28216=CARTESIAN_POINT('Ctrl Pts',(0.910447978388727,1.3,11.8477046062916));
#28217=CARTESIAN_POINT('Ctrl Pts',(0.911488139022433,1.3,11.8419426014754));
#28218=CARTESIAN_POINT('Ctrl Pts',(0.912592827853641,1.3,11.8358231405388));
#28219=CARTESIAN_POINT('Ctrl Pts',(0.913887769999808,1.3,11.8299167744627));
#28220=CARTESIAN_POINT('Ctrl Pts',(0.914982579148,1.3,11.8242119452305));
#28221=CARTESIAN_POINT('Ctrl Pts',(0.917527897789361,1.3,11.8109488041483));
#28222=CARTESIAN_POINT('Ctrl Pts',(0.919180222565221,1.3,11.7988189649137));
#28223=CARTESIAN_POINT('Ctrl Pts',(0.920881722724676,1.3,11.7888075686438));
#28224=CARTESIAN_POINT('Ctrl Pts',(0.922057503612529,1.3,11.7818894332975));
#28225=CARTESIAN_POINT('Ctrl Pts',(0.923102561601193,1.3,11.7762464130738));
#28226=CARTESIAN_POINT('Ctrl Pts',(0.923921465389292,1.3,11.771085056656));
#28227=CARTESIAN_POINT('Ctrl Pts',(0.924403404177455,1.3,11.7680475107398));
#28228=CARTESIAN_POINT('Ctrl Pts',(0.924828219757713,1.3,11.7651004509153));
#28229=CARTESIAN_POINT('Ctrl Pts',(0.925198336031033,1.3,11.7622401659214));
#28230=CARTESIAN_POINT('Ctrl Pts',(0.925391797231251,1.3,11.7607450839491));
#28231=CARTESIAN_POINT('Ctrl Pts',(0.92557043456165,1.3,11.7592737494426));
#28232=CARTESIAN_POINT('Ctrl Pts',(0.925741442489917,1.3,11.7578264931109));
#28233=CARTESIAN_POINT('Ctrl Pts',(0.925918111930927,1.3,11.7563313228593));
#28234=CARTESIAN_POINT('Ctrl Pts',(0.926086696269529,1.3,11.754861862917));
#28235=CARTESIAN_POINT('Ctrl Pts',(0.926256816181442,1.3,11.7534184302241));
#28236=CARTESIAN_POINT('Ctrl Pts',(0.927007261063928,1.3,11.7470510587308));
#28237=CARTESIAN_POINT('Ctrl Pts',(0.927774594433632,1.3,11.7411851682608));
#28238=CARTESIAN_POINT('Ctrl Pts',(0.928446980256554,1.3,11.7357385420547));
#28239=CARTESIAN_POINT('Ctrl Pts',(0.929240499769501,1.3,11.7293106787253));
#28240=CARTESIAN_POINT('Ctrl Pts',(0.929908251832915,1.3,11.7234706008434));
#28241=CARTESIAN_POINT('Ctrl Pts',(0.930436366319506,1.3,11.7181271863582));
#28242=CARTESIAN_POINT('Ctrl Pts',(0.930742894038522,1.3,11.7150257666936));
#28243=CARTESIAN_POINT('Ctrl Pts',(0.931003610509611,1.3,11.7120920765099));
#28244=CARTESIAN_POINT('Ctrl Pts',(0.931226895192046,1.3,11.7093048944438));
#28245=CARTESIAN_POINT('Ctrl Pts',(0.931479130591859,1.3,11.7061563310262));
#28246=CARTESIAN_POINT('Ctrl Pts',(0.931693185616966,1.3,11.7031937822063));
#28247=CARTESIAN_POINT('Ctrl Pts',(0.932017858608567,1.3,11.7004007314288));
#28248=CARTESIAN_POINT('Ctrl Pts',(0.932766403025875,1.3,11.69396125965));
#28249=CARTESIAN_POINT('Ctrl Pts',(0.934064984191208,1.3,11.6884310135751));
#28250=CARTESIAN_POINT('Ctrl Pts',(0.936125406440064,1.3,11.683495700499));
#28251=CARTESIAN_POINT('',(1.16079736048698,1.3,11.6306327026976));
#28252=CARTESIAN_POINT('',(0.936125406440074,1.3,11.683495700499));
#28253=CARTESIAN_POINT('',(1.35226619965017,1.3,11.8576685288847));
#28254=CARTESIAN_POINT('Ctrl Pts',(1.16079736048698,1.3,11.6306327026976));
#28255=CARTESIAN_POINT('Ctrl Pts',(1.16756547282336,1.3,11.6361811764895));
#28256=CARTESIAN_POINT('Ctrl Pts',(1.17431337124345,1.3,11.6464259698444));
#28257=CARTESIAN_POINT('Ctrl Pts',(1.1844641184857,1.3,11.6613370682762));
#28258=CARTESIAN_POINT('Ctrl Pts',(1.19279885226841,1.3,11.6737320721675));
#28259=CARTESIAN_POINT('Ctrl Pts',(1.20597861208497,1.3,11.6905975515117));
#28260=CARTESIAN_POINT('Ctrl Pts',(1.22462455149233,1.3,11.7146389274155));
#28261=CARTESIAN_POINT('Ctrl Pts',(1.24342566547099,1.3,11.7386228662457));
#28262=CARTESIAN_POINT('Ctrl Pts',(1.26170958390841,1.30000000000001,11.7595856095273));
#28263=CARTESIAN_POINT('Ctrl Pts',(1.27727352044057,1.30000000000001,11.7785119326797));
#28264=CARTESIAN_POINT('Ctrl Pts',(1.29877215077146,1.30000000000001,11.8012267330547));
#28265=CARTESIAN_POINT('Ctrl Pts',(1.32365521531308,1.30000000000001,11.8288485325488));
#28266=CARTESIAN_POINT('Ctrl Pts',(1.34190888454235,1.30000000000001,11.8474571703315));
#28267=CARTESIAN_POINT('Ctrl Pts',(1.35158289478778,1.30000000000001,11.856991850512));
#28268=CARTESIAN_POINT('Ctrl Pts',(1.35226619956941,1.30000000000001,11.8576685288047));
#28269=CARTESIAN_POINT('',(1.85479302526307,1.30000000000044,11.6813215498401));
#28270=CARTESIAN_POINT('Origin',(0.,1.3,7.2));
#28271=CARTESIAN_POINT('',(1.84783999216022,1.3,11.390889146273));
#28272=CARTESIAN_POINT('Ctrl Pts',(1.85479302522491,1.3,11.6813215498385));
#28273=CARTESIAN_POINT('Ctrl Pts',(1.85749249844584,1.3,11.6158578696262));
#28274=CARTESIAN_POINT('Ctrl Pts',(1.85870424358163,1.3,11.5263025468982));
#28275=CARTESIAN_POINT('Ctrl Pts',(1.84829934772273,1.3,11.4112520763645));
#28276=CARTESIAN_POINT('Ctrl Pts',(1.8458590678981,1.3,11.4014133252669));
#28277=CARTESIAN_POINT('Ctrl Pts',(1.84783999216022,1.3,11.390889146273));
#28278=CARTESIAN_POINT('',(2.05661148970878,1.3,11.2924694059607));
#28279=CARTESIAN_POINT('',(1.84783999216022,1.3,11.390889146273));
#28280=CARTESIAN_POINT('',(2.2911613629891,1.30000000000044,11.4747022830537));
#28281=CARTESIAN_POINT('Ctrl Pts',(2.05661148970878,1.3,11.2924694059607));
#28282=CARTESIAN_POINT('Ctrl Pts',(2.06438529511966,1.3,11.2964894626086));
#28283=CARTESIAN_POINT('Ctrl Pts',(2.07311280409283,1.30000000000005,11.3051080086582));
#28284=CARTESIAN_POINT('Ctrl Pts',(2.08607547837362,1.30000000000005,11.3176312713285));
#28285=CARTESIAN_POINT('Ctrl Pts',(2.09696615016092,1.3000000000001,11.3279028086908));
#28286=CARTESIAN_POINT('Ctrl Pts',(2.11062203159441,1.30000000000011,11.3399881418636));
#28287=CARTESIAN_POINT('Ctrl Pts',(2.12531111485264,1.30000000000018,11.3512371203303));
#28288=CARTESIAN_POINT('Ctrl Pts',(2.14327171669124,1.30000000000022,11.3674145634971));
#28289=CARTESIAN_POINT('Ctrl Pts',(2.17775045539098,1.30000000000032,11.3935430635717));
#28290=CARTESIAN_POINT('Ctrl Pts',(2.21669657645957,1.30000000000061,11.4235975293954));
#28291=CARTESIAN_POINT('Ctrl Pts',(2.24785024885108,1.30000000000087,11.4455731525381));
#28292=CARTESIAN_POINT('Ctrl Pts',(2.25945701905641,1.30000000000088,11.4535134605502));
#28293=CARTESIAN_POINT('Ctrl Pts',(2.26208146734059,1.30000000000088,11.4552446005424));
#28294=CARTESIAN_POINT('Ctrl Pts',(2.2667245028145,1.3000000000009,11.4582355351721));
#28295=CARTESIAN_POINT('Ctrl Pts',(2.27570351210482,1.30000000000087,11.4644408982048));
#28296=CARTESIAN_POINT('Ctrl Pts',(2.28441167791373,1.30000000000097,11.4701202167479));
#28297=CARTESIAN_POINT('Ctrl Pts',(2.2903719830358,1.30000000000101,11.4741645710873));
#28298=CARTESIAN_POINT('Ctrl Pts',(2.29116136298823,1.30000000000102,11.4747022830531));
#28299=CARTESIAN_POINT('',(2.74612652659283,1.3,11.1976604533081));
#28300=CARTESIAN_POINT('Origin',(0.,1.3,7.2));
#28301=CARTESIAN_POINT('',(2.67879510330291,1.3,10.9151206262376));
#28302=CARTESIAN_POINT('Ctrl Pts',(2.74612652659282,1.3,11.1976604533081));
#28303=CARTESIAN_POINT('Ctrl Pts',(2.74596451589451,1.3,11.19665402888));
#28304=CARTESIAN_POINT('Ctrl Pts',(2.74580163938371,1.3,11.1956477001141));
#28305=CARTESIAN_POINT('Ctrl Pts',(2.74563797152551,1.3,11.1946414582487));
#28306=CARTESIAN_POINT('Ctrl Pts',(2.74368370235821,1.3,11.1826264696363));
#28307=CARTESIAN_POINT('Ctrl Pts',(2.74161741958818,1.3,11.1706227867786));
#28308=CARTESIAN_POINT('Ctrl Pts',(2.73928525122789,1.3,11.1586662116773));
#28309=CARTESIAN_POINT('Ctrl Pts',(2.73870662877036,1.3,11.1556997265013));
#28310=CARTESIAN_POINT('Ctrl Pts',(2.7381117435708,1.3,11.1527361231565));
#28311=CARTESIAN_POINT('Ctrl Pts',(2.73746409185162,1.3,11.1497825766952));
#28312=CARTESIAN_POINT('Ctrl Pts',(2.73681764724266,1.3,11.1468345351311));
#28313=CARTESIAN_POINT('Ctrl Pts',(2.73611954983319,1.3,11.1438967384406));
#28314=CARTESIAN_POINT('Ctrl Pts',(2.73557366467298,1.3,11.1409300364769));
#28315=CARTESIAN_POINT('Ctrl Pts',(2.73501877686395,1.3,11.1379144081495));
#28316=CARTESIAN_POINT('Ctrl Pts',(2.73461628430988,1.3,11.1348691468756));
#28317=CARTESIAN_POINT('Ctrl Pts',(2.73415960583626,1.3,11.1318333756012));
#28318=CARTESIAN_POINT('Ctrl Pts',(2.73393195089181,1.3,11.1303200387992));
#28319=CARTESIAN_POINT('Ctrl Pts',(2.73369124569482,1.3,11.1288090442376));
#28320=CARTESIAN_POINT('Ctrl Pts',(2.73341248846247,1.3,11.1273055115503));
#28321=CARTESIAN_POINT('Ctrl Pts',(2.73313667795592,1.3,11.1258178726158));
#28322=CARTESIAN_POINT('Ctrl Pts',(2.73282314053844,1.3,11.1243376848035));
#28323=CARTESIAN_POINT('Ctrl Pts',(2.73250766432533,1.3,11.1228579486607));
#28324=CARTESIAN_POINT('Ctrl Pts',(2.73124858845734,1.3,11.1169522733956));
#28325=CARTESIAN_POINT('Ctrl Pts',(2.72996157700056,1.3,11.1110529795643));
#28326=CARTESIAN_POINT('Ctrl Pts',(2.72872025058404,1.3,11.1051442288111));
#28327=CARTESIAN_POINT('Ctrl Pts',(2.72747735620529,1.3,11.099228014511));
#28328=CARTESIAN_POINT('Ctrl Pts',(2.72628009813441,1.3,11.0933015722916));
#28329=CARTESIAN_POINT('Ctrl Pts',(2.72498683323779,1.3,11.0873959758342));
#28330=CARTESIAN_POINT('Ctrl Pts',(2.72241841329655,1.3,11.0756674801904));
#28331=CARTESIAN_POINT('Ctrl Pts',(2.71946779623975,1.3,11.0640269669922));
#28332=CARTESIAN_POINT('Ctrl Pts',(2.71652343305083,1.3,11.0523920562829));
#28333=CARTESIAN_POINT('Ctrl Pts',(2.71358373997865,1.3,11.0407755999517));
#28334=CARTESIAN_POINT('Ctrl Pts',(2.71065147471426,1.3,11.0291615051628));
#28335=CARTESIAN_POINT('Ctrl Pts',(2.70771716723947,1.3,11.0175458216236));
#28336=CARTESIAN_POINT('Ctrl Pts',(2.70625043780106,1.3,11.0117396594745));
#28337=CARTESIAN_POINT('Ctrl Pts',(2.70478323191785,1.3,11.0059327406934));
#28338=CARTESIAN_POINT('Ctrl Pts',(2.70323987718174,1.3,11.0001465555415));
#28339=CARTESIAN_POINT('Ctrl Pts',(2.70247147803797,1.3,10.9972657533433));
#28340=CARTESIAN_POINT('Ctrl Pts',(2.70168438254399,1.3,10.9943900335713));
#28341=CARTESIAN_POINT('Ctrl Pts',(2.70083970447103,1.3,10.9915311919127));
#28342=CARTESIAN_POINT('Ctrl Pts',(2.70000086668158,1.3,10.9886921168923));
#28343=CARTESIAN_POINT('Ctrl Pts',(2.69910470091314,1.3,10.9858700981927));
#28344=CARTESIAN_POINT('Ctrl Pts',(2.69822575948921,1.3,10.98304354175));
#28345=CARTESIAN_POINT('Ctrl Pts',(2.69625160085045,1.3,10.9766949152462));
#28346=CARTESIAN_POINT('Ctrl Pts',(2.69437215817735,1.3,10.9703739764371));
#28347=CARTESIAN_POINT('Ctrl Pts',(2.69304746703953,1.3,10.9659932897602));
#28348=CARTESIAN_POINT('Ctrl Pts',(2.69119548416497,1.3,10.9598688759457));
#28349=CARTESIAN_POINT('Ctrl Pts',(2.68998601190985,1.3,10.9558289925951));
#28350=CARTESIAN_POINT('Ctrl Pts',(2.68772315303807,1.3,10.9490869229178));
#28351=CARTESIAN_POINT('Ctrl Pts',(2.68687354912832,1.3,10.9465555724969));
#28352=CARTESIAN_POINT('Ctrl Pts',(2.68580897072893,1.3,10.9435039196507));
#28353=CARTESIAN_POINT('Ctrl Pts',(2.68483500056766,1.3,10.9407017314786));
#28354=CARTESIAN_POINT('Ctrl Pts',(2.68164275703609,1.3,10.9315173976843));
#28355=CARTESIAN_POINT('Ctrl Pts',(2.67898731875167,1.3,10.9233368709496));
#28356=CARTESIAN_POINT('Ctrl Pts',(2.67879510330291,1.3,10.9151206262376));
#28357=CARTESIAN_POINT('',(2.86254182811346,1.3,10.7754455583364));
#28358=CARTESIAN_POINT('',(2.67879510330291,1.3,10.9151206262376));
#28359=CARTESIAN_POINT('',(3.1297306010244,1.30000000000014,10.9050352717634));
#28360=CARTESIAN_POINT('Ctrl Pts',(2.86254182811346,1.3,10.7754455583364));
#28361=CARTESIAN_POINT('Ctrl Pts',(2.87098157399952,1.3,10.7777615020743));
#28362=CARTESIAN_POINT('Ctrl Pts',(2.88129518337835,1.30000000000003,10.7843931284862));
#28363=CARTESIAN_POINT('Ctrl Pts',(2.89656867358042,1.30000000000002,10.7939563838538));
#28364=CARTESIAN_POINT('Ctrl Pts',(2.90935734036008,1.30000000000004,10.8017417133146));
#28365=CARTESIAN_POINT('Ctrl Pts',(2.92519160082833,1.30000000000006,10.8107532722469));
#28366=CARTESIAN_POINT('Ctrl Pts',(2.94194585038891,1.30000000000006,10.8186721958535));
#28367=CARTESIAN_POINT('Ctrl Pts',(2.96266976928765,1.30000000000008,10.8309787346033));
#28368=CARTESIAN_POINT('Ctrl Pts',(2.98251244358946,1.30000000000014,10.8398773562819));
#28369=CARTESIAN_POINT('Ctrl Pts',(3.00474611284772,1.30000000000016,10.8505077189706));
#28370=CARTESIAN_POINT('Ctrl Pts',(3.02671111250602,1.3000000000002,10.8614078746728));
#28371=CARTESIAN_POINT('Ctrl Pts',(3.04946200615208,1.30000000000022,10.8714147740806));
#28372=CARTESIAN_POINT('Ctrl Pts',(3.06679325766632,1.30000000000024,10.8785906567429));
#28373=CARTESIAN_POINT('Ctrl Pts',(3.07804152851698,1.30000000000026,10.8837146344997));
#28374=CARTESIAN_POINT('Ctrl Pts',(3.09212660927841,1.30000000000026,10.8900802463094));
#28375=CARTESIAN_POINT('Ctrl Pts',(3.10970701250653,1.30000000000029,10.8969430220631));
#28376=CARTESIAN_POINT('Ctrl Pts',(3.12220207956528,1.30000000000031,10.9019527342208));
#28377=CARTESIAN_POINT('Ctrl Pts',(3.12885620798913,1.30000000000033,10.9046768064315));
#28378=CARTESIAN_POINT('Ctrl Pts',(3.12973060094966,1.30000000000033,10.9050352717328));
#28379=CARTESIAN_POINT('',(3.51702417252248,1.30000000000004,10.5396168896264));
#28380=CARTESIAN_POINT('Origin',(0.,1.3,7.2));
#28381=CARTESIAN_POINT('',(3.39267401414619,1.3,10.2769835077089));
#28382=CARTESIAN_POINT('Ctrl Pts',(3.51702417248271,1.3,10.5396168896419));
#28383=CARTESIAN_POINT('Ctrl Pts',(3.49672647112758,1.3,10.4875123140426));
#28384=CARTESIAN_POINT('Ctrl Pts',(3.46275940082978,1.3,10.4051664173467));
#28385=CARTESIAN_POINT('Ctrl Pts',(3.4011770434785,1.3,10.2950140468319));
#28386=CARTESIAN_POINT('Ctrl Pts',(3.39510833417347,1.3,10.2872492564874));
#28387=CARTESIAN_POINT('Ctrl Pts',(3.39267401414619,1.3,10.276983507709));
#28388=CARTESIAN_POINT('',(3.54336535262991,1.3,10.1021575829215));
#28389=CARTESIAN_POINT('',(3.39267401414619,1.3,10.2769835077089));
#28390=CARTESIAN_POINT('',(3.8316570030416,1.29999999999986,10.1733658723814));
#28391=CARTESIAN_POINT('Ctrl Pts',(3.54336535262991,1.3,10.1021575829215));
#28392=CARTESIAN_POINT('Ctrl Pts',(3.55210218159755,1.3,10.1026681958948));
#28393=CARTESIAN_POINT('Ctrl Pts',(3.56356899629571,1.29999999999999,10.1070114760009));
#28394=CARTESIAN_POINT('Ctrl Pts',(3.58049697517908,1.29999999999998,10.113190435319));
#28395=CARTESIAN_POINT('Ctrl Pts',(3.59462471573536,1.29999999999995,10.1181472229321));
#28396=CARTESIAN_POINT('Ctrl Pts',(3.61198647845491,1.29999999999995,10.12367003144));
#28397=CARTESIAN_POINT('Ctrl Pts',(3.63002093128387,1.29999999999992,10.1279329457953));
#28398=CARTESIAN_POINT('Ctrl Pts',(3.65285062374733,1.29999999999992,10.1356618793807));
#28399=CARTESIAN_POINT('Ctrl Pts',(3.67410984172058,1.29999999999985,10.1402406910406));
#28400=CARTESIAN_POINT('Ctrl Pts',(3.6980678619775,1.29999999999983,10.1460160834464));
#28401=CARTESIAN_POINT('Ctrl Pts',(3.72181914762373,1.29999999999981,10.1521112671248));
#28402=CARTESIAN_POINT('Ctrl Pts',(3.74615344929343,1.29999999999978,10.1571692337866));
#28403=CARTESIAN_POINT('Ctrl Pts',(3.76459792690676,1.29999999999976,10.1605848969376));
#28404=CARTESIAN_POINT('Ctrl Pts',(3.77666573049054,1.29999999999974,10.1632582465006));
#28405=CARTESIAN_POINT('Ctrl Pts',(3.79176649230709,1.29999999999974,10.1665562922193));
#28406=CARTESIAN_POINT('Ctrl Pts',(3.81038957161618,1.2999999999997,10.1696138666325));
#28407=CARTESIAN_POINT('Ctrl Pts',(3.82365280763186,1.29999999999968,10.1719161377918));
#28408=CARTESIAN_POINT('Ctrl Pts',(3.83072754430228,1.29999999999967,10.173197107173));
#28409=CARTESIAN_POINT('Ctrl Pts',(3.83165700295789,1.29999999999967,10.1733658723663));
#28410=CARTESIAN_POINT('',(4.13460022854383,1.2999999999976,9.7352069526073));
#28411=CARTESIAN_POINT('Origin',(0.,1.3,7.2));
#28412=CARTESIAN_POINT('',(3.95827679071515,1.3,9.50436744488836));
#28413=CARTESIAN_POINT('Ctrl Pts',(4.13458086813857,1.3,9.73517804740468));
#28414=CARTESIAN_POINT('Ctrl Pts',(4.08546280420686,1.3,9.66185452740355));
#28415=CARTESIAN_POINT('Ctrl Pts',(4.04234444364633,1.3,9.6029319619877));
#28416=CARTESIAN_POINT('Ctrl Pts',(3.96268006345613,1.3,9.511257093339));
#28417=CARTESIAN_POINT('Ctrl Pts',(3.96053997251118,1.3,9.50914656897965));
#28418=CARTESIAN_POINT('Ctrl Pts',(3.95827679071515,1.3,9.50436744488836));
#28419=CARTESIAN_POINT('',(4.06932680828303,1.3,9.30203139503569));
#28420=CARTESIAN_POINT('',(3.95827679071515,1.3,9.50436744488836));
#28421=CARTESIAN_POINT('',(4.36609756959125,1.29999999999973,9.31179828885486));
#28422=CARTESIAN_POINT('Ctrl Pts',(4.06932680828303,1.3,9.30203139503569));
#28423=CARTESIAN_POINT('Ctrl Pts',(4.07797887898238,1.3,9.30071436100745));
#28424=CARTESIAN_POINT('Ctrl Pts',(4.09011069171085,1.29999999999996,9.30253751130118));
#28425=CARTESIAN_POINT('Ctrl Pts',(4.10795583415653,1.29999999999994,9.30506364957931));
#28426=CARTESIAN_POINT('Ctrl Pts',(4.12281928798903,1.29999999999992,9.30690417832915));
#28427=CARTESIAN_POINT('Ctrl Pts',(4.13792366935278,1.29999999999991,9.30846318087845));
#28428=CARTESIAN_POINT('Ctrl Pts',(4.15023209615125,1.29999999999988,9.3088328818803));
#28429=CARTESIAN_POINT('Ctrl Pts',(4.16247876162117,1.29999999999988,9.30949047140628));
#28430=CARTESIAN_POINT('Ctrl Pts',(4.18345672109247,1.29999999999984,9.31179756901066));
#28431=CARTESIAN_POINT('Ctrl Pts',(4.20827437817346,1.29999999999976,9.31201935419063));
#28432=CARTESIAN_POINT('Ctrl Pts',(4.23283302083266,1.29999999999972,9.3128856552204));
#28433=CARTESIAN_POINT('Ctrl Pts',(4.25122160285819,1.29999999999969,9.31361866027968));
#28434=CARTESIAN_POINT('Ctrl Pts',(4.26981671664902,1.29999999999964,9.31368244807499));
#28435=CARTESIAN_POINT('Ctrl Pts',(4.28847502205149,1.29999999999959,9.31351820624347));
#28436=CARTESIAN_POINT('Ctrl Pts',(4.30716480650586,1.29999999999956,9.31320732627316));
#28437=CARTESIAN_POINT('Ctrl Pts',(4.32563404344978,1.29999999999949,9.31355938218807));
#28438=CARTESIAN_POINT('Ctrl Pts',(4.34458714565271,1.29999999999946,9.31234956827253));
#28439=CARTESIAN_POINT('Ctrl Pts',(4.35714349439214,1.29999999999938,9.31234301972474));
#28440=CARTESIAN_POINT('Ctrl Pts',(4.36384001426254,1.29999999999937,9.31193092960279));
#28441=CARTESIAN_POINT('Ctrl Pts',(4.36462701760224,1.29999999999937,9.31188523907631));
#28442=CARTESIAN_POINT('Ctrl Pts',(4.3653799997326,1.29999999999937,9.31183950868406));
#28443=CARTESIAN_POINT('Ctrl Pts',(4.36593552968483,1.29999999999937,9.31180750976769));
#28444=CARTESIAN_POINT('Ctrl Pts',(4.36609756959125,1.29999999999937,9.31179828885486));
#28445=CARTESIAN_POINT('',(4.57140911793407,1.30000000000128,8.82009835380608));
#28446=CARTESIAN_POINT('Origin',(0.,1.3,7.2));
#28447=CARTESIAN_POINT('',(4.35088387761047,1.3,8.63103946714436));
#28448=CARTESIAN_POINT('Ctrl Pts',(4.57140911790143,1.3,8.82009835383949));
#28449=CARTESIAN_POINT('Ctrl Pts',(4.5706814231909,1.3,8.81938742440423));
#28450=CARTESIAN_POINT('Ctrl Pts',(4.56995109704004,1.3,8.81868077650572));
#28451=CARTESIAN_POINT('Ctrl Pts',(4.56921748737933,1.3,8.81797917609138));
#28452=CARTESIAN_POINT('Ctrl Pts',(4.56480235883729,1.3,8.81375669078291));
#28453=CARTESIAN_POINT('Ctrl Pts',(4.56027147065103,1.3,8.80971586453579));
#28454=CARTESIAN_POINT('Ctrl Pts',(4.55597042156158,1.3,8.80551114442447));
#28455=CARTESIAN_POINT('Ctrl Pts',(4.5515560546328,1.3,8.80119564441083));
#28456=CARTESIAN_POINT('Ctrl Pts',(4.54737114764275,1.3,8.79671564866395));
#28457=CARTESIAN_POINT('Ctrl Pts',(4.54294046767687,1.3,8.79259015797614));
#28458=CARTESIAN_POINT('Ctrl Pts',(4.53847171520424,1.3,8.78842921725059));
#28459=CARTESIAN_POINT('Ctrl Pts',(4.53376239388215,1.3,8.78462570418076));
#28460=CARTESIAN_POINT('Ctrl Pts',(4.52949040409136,1.3,8.78046646176674));
#28461=CARTESIAN_POINT('Ctrl Pts',(4.52727670177039,1.3,8.77831118400713));
#28462=CARTESIAN_POINT('Ctrl Pts',(4.52517288265194,1.3,8.77606700032968));
#28463=CARTESIAN_POINT('Ctrl Pts',(4.52300760269494,1.3,8.77392186038719));
#28464=CARTESIAN_POINT('Ctrl Pts',(4.52083180190261,1.3,8.77176629746728));
#28465=CARTESIAN_POINT('Ctrl Pts',(4.51859492702336,1.3,8.76971040774127));
#28466=CARTESIAN_POINT('Ctrl Pts',(4.51637518841834,1.3,8.76767197520911));
#28467=CARTESIAN_POINT('Ctrl Pts',(4.50713124681152,1.3,8.7591830696893));
#28468=CARTESIAN_POINT('Ctrl Pts',(4.49817607520628,1.3,8.75100076229712));
#28469=CARTESIAN_POINT('Ctrl Pts',(4.48948341155244,1.3,8.74333183809486));
#28470=CARTESIAN_POINT('Ctrl Pts',(4.47994963627258,1.3,8.73492086041367));
#28471=CARTESIAN_POINT('Ctrl Pts',(4.47074451497491,1.3,8.72711603709132));
#28472=CARTESIAN_POINT('Ctrl Pts',(4.46212271757076,1.3,8.71986344315658));
#28473=CARTESIAN_POINT('Ctrl Pts',(4.4491396707095,1.3,8.70894219756165));
#28474=CARTESIAN_POINT('Ctrl Pts',(4.43747485629493,1.3,8.69927577567235));
#28475=CARTESIAN_POINT('Ctrl Pts',(4.42761872805175,1.3,8.69109174442388));
#28476=CARTESIAN_POINT('Ctrl Pts',(4.42252179250726,1.3,8.68685950649654));
#28477=CARTESIAN_POINT('Ctrl Pts',(4.41788967791717,1.3,8.68304533279346));
#28478=CARTESIAN_POINT('Ctrl Pts',(4.41368050107165,1.3,8.6798232258243));
#28479=CARTESIAN_POINT('Ctrl Pts',(4.4111202398016,1.3,8.67786335671357));
#28480=CARTESIAN_POINT('Ctrl Pts',(4.4087266150474,1.3,8.67611069656105));
#28481=CARTESIAN_POINT('Ctrl Pts',(4.40656831116804,1.3,8.67450505586071));
#28482=CARTESIAN_POINT('Ctrl Pts',(4.40006247096172,1.3,8.66966512487367));
#28483=CARTESIAN_POINT('Ctrl Pts',(4.39588688861348,1.3,8.6664490557388));
#28484=CARTESIAN_POINT('Ctrl Pts',(4.39234740865121,1.3,8.66377079335119));
#28485=CARTESIAN_POINT('Ctrl Pts',(4.38738609061361,1.3,8.66001665103798));
#28486=CARTESIAN_POINT('Ctrl Pts',(4.38385031613455,1.3,8.65733159560148));
#28487=CARTESIAN_POINT('Ctrl Pts',(4.37809180956932,1.3,8.65323937484063));
#28488=CARTESIAN_POINT('Ctrl Pts',(4.37589487582872,1.3,8.65167814750474));
#28489=CARTESIAN_POINT('Ctrl Pts',(4.37324823329501,1.3,8.64984331524573));
#28490=CARTESIAN_POINT('Ctrl Pts',(4.3708229365894,1.3,8.64815914175065));
#28491=CARTESIAN_POINT('Ctrl Pts',(4.36278432406233,1.3,8.64257697189741));
#28492=CARTESIAN_POINT('Ctrl Pts',(4.35585193117194,1.3,8.63755149448732));
#28493=CARTESIAN_POINT('Ctrl Pts',(4.35088387761047,1.3,8.63103946714436));
#28494=CARTESIAN_POINT('',(4.41743915561768,1.3,8.41003634852114));
#28495=CARTESIAN_POINT('',(4.35088387761047,1.3,8.63103946714436));
#28496=CARTESIAN_POINT('',(4.70979663593526,1.3000000000001,8.35772002147866));
#28497=CARTESIAN_POINT('Ctrl Pts',(4.41743915561768,1.3,8.41003634852114));
#28498=CARTESIAN_POINT('Ctrl Pts',(4.42562833104196,1.3,8.40694922819813));
#28499=CARTESIAN_POINT('Ctrl Pts',(4.43787350489845,1.30000000000001,8.40622766486505));
#28500=CARTESIAN_POINT('Ctrl Pts',(4.45585351305901,1.30000000000001,8.40499606910573));
#28501=CARTESIAN_POINT('Ctrl Pts',(4.47077483084096,1.30000000000003,8.40371437127723));
#28502=CARTESIAN_POINT('Ctrl Pts',(4.48587205596936,1.30000000000003,8.40211582040918));
#28503=CARTESIAN_POINT('Ctrl Pts',(4.4979897136352,1.30000000000004,8.39991299338427));
#28504=CARTESIAN_POINT('Ctrl Pts',(4.51009815468572,1.30000000000004,8.39805546525287));
#28505=CARTESIAN_POINT('Ctrl Pts',(4.53111879558693,1.30000000000004,8.39580460547943));
#28506=CARTESIAN_POINT('Ctrl Pts',(4.57364955024891,1.30000000000008,8.38742647237147));
#28507=CARTESIAN_POINT('Ctrl Pts',(4.61136873806362,1.30000000000014,8.38124836466501));
#28508=CARTESIAN_POINT('Ctrl Pts',(4.63873844454836,1.30000000000016,8.37465149171448));
#28509=CARTESIAN_POINT('Ctrl Pts',(4.64481218242238,1.30000000000016,8.37325265104856));
#28510=CARTESIAN_POINT('Ctrl Pts',(4.65390368130274,1.30000000000016,8.37132464930544));
#28511=CARTESIAN_POINT('Ctrl Pts',(4.66297291571428,1.30000000000017,8.36958456723215));
#28512=CARTESIAN_POINT('Ctrl Pts',(4.68119597547622,1.30000000000017,8.36523210052763));
#28513=CARTESIAN_POINT('Ctrl Pts',(4.6958131149506,1.30000000000022,8.3611827857283));
#28514=CARTESIAN_POINT('Ctrl Pts',(4.70887301296434,1.30000000000024,8.35794751342532));
#28515=CARTESIAN_POINT('Ctrl Pts',(4.70979663583784,1.30000000000024,8.35772002150267));
#28516=CARTESIAN_POINT('',(4.80835060743154,1.3,7.83424319963977));
#28517=CARTESIAN_POINT('Origin',(0.,1.3,7.2));
#28518=CARTESIAN_POINT('',(4.55333646119701,1.3,7.69516819779692));
#28519=CARTESIAN_POINT('Ctrl Pts',(4.80835060754372,1.29999999999996,7.8342431997438));
#28520=CARTESIAN_POINT('Ctrl Pts',(4.80749051866453,1.29999999999996,7.83369878716171));
#28521=CARTESIAN_POINT('Ctrl Pts',(4.80146805113317,1.29999999999996,7.8299273448685));
#28522=CARTESIAN_POINT('Ctrl Pts',(4.79014356570026,1.29999999999996,7.82346765255662));
#28523=CARTESIAN_POINT('Ctrl Pts',(4.7749017311504,1.29999999999998,7.81282514770577));
#28524=CARTESIAN_POINT('Ctrl Pts',(4.76161483790886,1.29999999999997,7.80610490563682));
#28525=CARTESIAN_POINT('Ctrl Pts',(4.75143645340678,1.29999999999997,7.79902370870334));
#28526=CARTESIAN_POINT('Ctrl Pts',(4.73580330060841,1.29999999999997,7.78978321737489));
#28527=CARTESIAN_POINT('Ctrl Pts',(4.7123168197138,1.29999999999999,7.77597081284977));
#28528=CARTESIAN_POINT('Ctrl Pts',(4.67798440200463,1.29999999999997,7.75743185110967));
#28529=CARTESIAN_POINT('Ctrl Pts',(4.64884999722387,1.29999999999999,7.74214044075126));
#28530=CARTESIAN_POINT('Ctrl Pts',(4.62760606760101,1.29999999999999,7.73098319622892));
#28531=CARTESIAN_POINT('Ctrl Pts',(4.61415054115611,1.29999999999999,7.72491389336459));
#28532=CARTESIAN_POINT('Ctrl Pts',(4.60067972068881,1.29999999999999,7.71852453663296));
#28533=CARTESIAN_POINT('Ctrl Pts',(4.5873040871705,1.29999999999999,7.71233002722669));
#28534=CARTESIAN_POINT('Ctrl Pts',(4.5709662969739,1.29999999999999,7.70550430059969));
#28535=CARTESIAN_POINT('Ctrl Pts',(4.55986191621585,1.3,7.70077302060486));
#28536=CARTESIAN_POINT('Ctrl Pts',(4.55333646119701,1.3,7.69516819779692));
#28537=CARTESIAN_POINT('',(4.57248821462698,1.3,7.4651569071776));
#28538=CARTESIAN_POINT('',(4.55333646119701,1.3,7.69516819779692));
#28539=CARTESIAN_POINT('',(4.84757646506369,1.30000000000001,7.35330497500277));
#28540=CARTESIAN_POINT('Ctrl Pts',(4.57248821462698,1.3,7.4651569071776));
#28541=CARTESIAN_POINT('Ctrl Pts',(4.5798565885141,1.3,7.46043462253162));
#28542=CARTESIAN_POINT('Ctrl Pts',(4.59168078261245,1.3,7.45714429554202));
#28543=CARTESIAN_POINT('Ctrl Pts',(4.60901113594043,1.3,7.45220225290281));
#28544=CARTESIAN_POINT('Ctrl Pts',(4.62333650359118,1.3,7.44778282836643));
#28545=CARTESIAN_POINT('Ctrl Pts',(4.63777227980167,1.3,7.44313876891633));
#28546=CARTESIAN_POINT('Ctrl Pts',(4.65200864708552,1.3,7.4371009858883));
#28547=CARTESIAN_POINT('Ctrl Pts',(4.67500366927394,1.3,7.42951895371871));
#28548=CARTESIAN_POINT('Ctrl Pts',(4.70065028211382,1.3,7.41931266872196));
#28549=CARTESIAN_POINT('Ctrl Pts',(4.72626264033617,1.30000000000001,7.40855923000075));
#28550=CARTESIAN_POINT('Ctrl Pts',(4.74336478500948,1.30000000000001,7.40185875322679));
#28551=CARTESIAN_POINT('Ctrl Pts',(4.75753064369248,1.30000000000001,7.39545690322073));
#28552=CARTESIAN_POINT('Ctrl Pts',(4.76745636601093,1.3,7.39112846433222));
#28553=CARTESIAN_POINT('Ctrl Pts',(4.77311161413793,1.30000000000001,7.38850648431319));
#28554=CARTESIAN_POINT('Ctrl Pts',(4.78158028238953,1.3,7.38446389233093));
#28555=CARTESIAN_POINT('Ctrl Pts',(4.79431947529819,1.30000000000002,7.37881277574729));
#28556=CARTESIAN_POINT('Ctrl Pts',(4.81695502355809,1.3,7.36871994814812));
#28557=CARTESIAN_POINT('Ctrl Pts',(4.8346427283241,1.30000000000002,7.35972960775616));
#28558=CARTESIAN_POINT('Ctrl Pts',(4.84672489359485,1.30000000000002,7.35372750798776));
#28559=CARTESIAN_POINT('Ctrl Pts',(4.84757646497524,1.30000000000002,7.35330497504666));
#28560=CARTESIAN_POINT('',(4.83514813889957,1.30000000000181,6.82074434979023));
#28561=CARTESIAN_POINT('Origin',(0.,1.3,7.2));
#28562=CARTESIAN_POINT('',(4.55678639209675,1.3,6.73765570212511));
#28563=CARTESIAN_POINT('Ctrl Pts',(4.83514655110529,1.30000000000047,6.82074421646102));
#28564=CARTESIAN_POINT('Ctrl Pts',(4.83418984233378,1.30000000000046,6.82039257937535));
#28565=CARTESIAN_POINT('Ctrl Pts',(4.8275141099345,1.30000000000046,6.8179659614836));
#28566=CARTESIAN_POINT('Ctrl Pts',(4.81795999365544,1.30000000000042,6.81478799676167));
#28567=CARTESIAN_POINT('Ctrl Pts',(4.80653088510641,1.30000000000041,6.81028270647152));
#28568=CARTESIAN_POINT('Ctrl Pts',(4.78936219347766,1.30000000000041,6.80389947355039));
#28569=CARTESIAN_POINT('Ctrl Pts',(4.75783769436201,1.30000000000029,6.79269374504301));
#28570=CARTESIAN_POINT('Ctrl Pts',(4.72334918205181,1.30000000000017,6.78192834281718));
#28571=CARTESIAN_POINT('Ctrl Pts',(4.68878647838757,1.30000000000016,6.77165051357849));
#28572=CARTESIAN_POINT('Ctrl Pts',(4.66573214590264,1.30000000000009,6.76556506981444));
#28573=CARTESIAN_POINT('Ctrl Pts',(4.64264412228767,1.30000000000009,6.75875338894064));
#28574=CARTESIAN_POINT('Ctrl Pts',(4.62535152074713,1.30000000000006,6.7547381568986));
#28575=CARTESIAN_POINT('Ctrl Pts',(4.60795448968299,1.30000000000004,6.75071584500925));
#28576=CARTESIAN_POINT('Ctrl Pts',(4.59357902902068,1.30000000000003,6.74737894430936));
#28577=CARTESIAN_POINT('Ctrl Pts',(4.576180400044,1.30000000000001,6.74411411083726));
#28578=CARTESIAN_POINT('Ctrl Pts',(4.56433455845385,1.3,6.74178132772091));
#28579=CARTESIAN_POINT('Ctrl Pts',(4.55678639209675,1.3,6.73765570212512));
#28580=CARTESIAN_POINT('',(4.52769759742429,1.3,6.50868883662639));
#28581=CARTESIAN_POINT('',(4.55678639209675,1.3,6.73765570212511));
#28582=CARTESIAN_POINT('',(4.77352764767188,1.30000000000002,6.34213416147271));
#28583=CARTESIAN_POINT('Ctrl Pts',(4.52769759742429,1.3,6.50868883662639));
#28584=CARTESIAN_POINT('Ctrl Pts',(4.53392313647801,1.3,6.50253777415649));
#28585=CARTESIAN_POINT('Ctrl Pts',(4.54481208542156,1.3,6.49688052366386));
#28586=CARTESIAN_POINT('Ctrl Pts',(4.56070008160091,1.3,6.488336502504));
#28587=CARTESIAN_POINT('Ctrl Pts',(4.57389579341099,1.3,6.48133398930416));
#28588=CARTESIAN_POINT('Ctrl Pts',(4.59203923906489,1.30000000000002,6.46996823620903));
#28589=CARTESIAN_POINT('Ctrl Pts',(4.61789381187435,1.3,6.45392159180597));
#28590=CARTESIAN_POINT('Ctrl Pts',(4.64368961597031,1.30000000000002,6.43767322775346));
#28591=CARTESIAN_POINT('Ctrl Pts',(4.66641984978595,1.30000000000002,6.42158632818792));
#28592=CARTESIAN_POINT('Ctrl Pts',(4.68178015411769,1.30000000000002,6.41154489129323));
#28593=CARTESIAN_POINT('Ctrl Pts',(4.69428702464384,1.30000000000003,6.40228578094019));
#28594=CARTESIAN_POINT('Ctrl Pts',(4.70437021285367,1.30000000000003,6.39513336563024));
#28595=CARTESIAN_POINT('Ctrl Pts',(4.71922603638813,1.30000000000003,6.38361239688257));
#28596=CARTESIAN_POINT('Ctrl Pts',(4.74196049006546,1.30000000000003,6.36773979185516));
#28597=CARTESIAN_POINT('Ctrl Pts',(4.76217237674818,1.30000000000005,6.35099061182857));
#28598=CARTESIAN_POINT('Ctrl Pts',(4.77278114106614,1.30000000000005,6.34271479237717));
#28599=CARTESIAN_POINT('Ctrl Pts',(4.77352764741212,1.30000000000005,6.34213416167476));
#28600=CARTESIAN_POINT('',(4.65067750872513,1.30000000000116,5.82388274136382));
#28601=CARTESIAN_POINT('Origin',(0.,1.3,7.2));
#28602=CARTESIAN_POINT('',(4.36108289177478,1.3,5.80034987084453));
#28603=CARTESIAN_POINT('Ctrl Pts',(4.65067750872023,1.3,5.8238827413956));
#28604=CARTESIAN_POINT('Ctrl Pts',(4.57567439558732,1.3,5.8123200324086));
#28605=CARTESIAN_POINT('Ctrl Pts',(4.49988238082424,1.3,5.80395796558544));
#28606=CARTESIAN_POINT('Ctrl Pts',(4.40454586996321,1.3,5.80228572656157));
#28607=CARTESIAN_POINT('Ctrl Pts',(4.40191545967668,1.3,5.80217462217108));
#28608=CARTESIAN_POINT('Ctrl Pts',(4.38054048224239,1.3,5.80258762524379));
#28609=CARTESIAN_POINT('Ctrl Pts',(4.3703146143467,1.3,5.80311246775222));
#28610=CARTESIAN_POINT('Ctrl Pts',(4.36108289177478,1.3,5.80034987084453));
#28611=CARTESIAN_POINT('',(4.28502486891058,1.3,5.58243438119362));
#28612=CARTESIAN_POINT('',(4.36108289177478,1.3,5.80034987084453));
#28613=CARTESIAN_POINT('',(4.49080284932952,1.30000000000011,5.368282290184));
#28614=CARTESIAN_POINT('Ctrl Pts',(4.28502486891058,1.3,5.58243438119362));
#28615=CARTESIAN_POINT('Ctrl Pts',(4.2898354872008,1.3,5.57512337184582));
#28616=CARTESIAN_POINT('Ctrl Pts',(4.29931642282797,1.30000000000001,5.56733888639131));
#28617=CARTESIAN_POINT('Ctrl Pts',(4.3130840388909,1.30000000000001,5.55568404800534));
#28618=CARTESIAN_POINT('Ctrl Pts',(4.32453875212957,1.30000000000003,5.54609803841767));
#28619=CARTESIAN_POINT('Ctrl Pts',(4.33993231883246,1.30000000000003,5.53122457501866));
#28620=CARTESIAN_POINT('Ctrl Pts',(4.36189159450452,1.30000000000003,5.51016616730234));
#28621=CARTESIAN_POINT('Ctrl Pts',(4.38377554191331,1.30000000000007,5.48895426241472));
#28622=CARTESIAN_POINT('Ctrl Pts',(4.40271175336488,1.3000000000001,5.46857812868943));
#28623=CARTESIAN_POINT('Ctrl Pts',(4.41990733032772,1.3000000000001,5.45112073570275));
#28624=CARTESIAN_POINT('Ctrl Pts',(4.44025594115488,1.30000000000016,5.4273732287603));
#28625=CARTESIAN_POINT('Ctrl Pts',(4.46512770529739,1.3000000000002,5.39974222775974));
#28626=CARTESIAN_POINT('Ctrl Pts',(4.48173090221287,1.30000000000024,5.37965091509962));
#28627=CARTESIAN_POINT('Ctrl Pts',(4.49020148419593,1.30000000000025,5.36903242764666));
#28628=CARTESIAN_POINT('Ctrl Pts',(4.49080284925142,1.30000000000025,5.36828229028143));
#28629=CARTESIAN_POINT('',(4.26287719558135,1.3000000000006,4.88691158511914));
#28630=CARTESIAN_POINT('Origin',(0.,1.3,7.2));
#28631=CARTESIAN_POINT('',(3.97477914228473,1.3,4.92421546647452));
#28632=CARTESIAN_POINT('Ctrl Pts',(4.26287719558322,1.3,4.88691158515324));
#28633=CARTESIAN_POINT('Ctrl Pts',(4.16750758322341,1.3,4.89212562971692));
#28634=CARTESIAN_POINT('Ctrl Pts',(4.09236051848986,1.3,4.90259779459969));
#28635=CARTESIAN_POINT('Ctrl Pts',(3.98404709074897,1.3,4.92363634735652));
#28636=CARTESIAN_POINT('Ctrl Pts',(3.98077132219638,1.3,4.92470388458002));
#28637=CARTESIAN_POINT('Ctrl Pts',(3.97477914228474,1.3,4.92421546647452));
#28638=CARTESIAN_POINT('',(3.85507599179487,1.3,4.7268753052437));
#28639=CARTESIAN_POINT('',(3.97477914228474,1.3,4.92421546647452));
#28640=CARTESIAN_POINT('',(4.01191463394249,1.3,4.47474020138297));
#28641=CARTESIAN_POINT('Ctrl Pts',(3.85507599179487,1.3,4.7268753052437));
#28642=CARTESIAN_POINT('Ctrl Pts',(3.85826144221842,1.3,4.7187238752086));
#28643=CARTESIAN_POINT('Ctrl Pts',(3.86591529009691,1.3,4.70913672804832));
#28644=CARTESIAN_POINT('Ctrl Pts',(3.87702448920013,1.3,4.69494766196105));
#28645=CARTESIAN_POINT('Ctrl Pts',(3.88606867189398,1.3,4.68300308818325));
#28646=CARTESIAN_POINT('Ctrl Pts',(3.89672887394469,1.3,4.66824246157762));
#28647=CARTESIAN_POINT('Ctrl Pts',(3.90461453552397,1.3,4.65489605906055));
#28648=CARTESIAN_POINT('Ctrl Pts',(3.91888415578993,1.3,4.63540334932576));
#28649=CARTESIAN_POINT('Ctrl Pts',(3.93483759407892,1.3,4.60896349398333));
#28650=CARTESIAN_POINT('Ctrl Pts',(3.9561473127133,1.3,4.57524814942806));
#28651=CARTESIAN_POINT('Ctrl Pts',(3.97147745303166,1.30000000000001,4.54819353159721));
#28652=CARTESIAN_POINT('Ctrl Pts',(3.98359299015971,1.30000000000001,4.52641657168413));
#28653=CARTESIAN_POINT('Ctrl Pts',(3.99308905203255,1.3,4.51055005634327));
#28654=CARTESIAN_POINT('Ctrl Pts',(4.00172238876483,1.3,4.49374975302448));
#28655=CARTESIAN_POINT('Ctrl Pts',(4.00805516521168,1.30000000000001,4.48189586303462));
#28656=CARTESIAN_POINT('Ctrl Pts',(4.01146644254775,1.3,4.47557094656382));
#28657=CARTESIAN_POINT('Ctrl Pts',(4.01191463393987,1.3,4.47474020138783));
#28658=CARTESIAN_POINT('',(3.68882920336369,1.30000000000049,4.05118449127588));
#28659=CARTESIAN_POINT('Origin',(0.,1.3,7.2));
#28660=CARTESIAN_POINT('',(3.4147584711704,1.3,4.14754376664537));
#28661=CARTESIAN_POINT('Ctrl Pts',(3.68882920337514,1.3,4.05118449131822));
#28662=CARTESIAN_POINT('Ctrl Pts',(3.65850555103085,1.3,4.05938588383362));
#28663=CARTESIAN_POINT('Ctrl Pts',(3.55713888853847,1.3,4.08790905610615));
#28664=CARTESIAN_POINT('Ctrl Pts',(3.43637430894292,1.3,4.13982506353119));
#28665=CARTESIAN_POINT('Ctrl Pts',(3.42618793094316,1.3,4.1460714746367));
#28666=CARTESIAN_POINT('Ctrl Pts',(3.4147584711704,1.3,4.14754376664537));
#28667=CARTESIAN_POINT('',(3.25664179513071,1.3,3.97940364582358));
#28668=CARTESIAN_POINT('',(3.4147584711704,1.3,4.14754376664537));
#28669=CARTESIAN_POINT('',(3.35740649851691,1.30000000000134,3.69995637892978));
#28670=CARTESIAN_POINT('Ctrl Pts',(3.25664179513071,1.3,3.97940364582358));
#28671=CARTESIAN_POINT('Ctrl Pts',(3.25806285821859,1.3,3.9707680517086));
#28672=CARTESIAN_POINT('Ctrl Pts',(3.26349509695928,1.3,3.95978804109145));
#28673=CARTESIAN_POINT('Ctrl Pts',(3.2702247202651,1.3,3.94633814773344));
#28674=CARTESIAN_POINT('Ctrl Pts',(3.27389249918462,1.3,3.93815813999823));
#28675=CARTESIAN_POINT('Ctrl Pts',(3.27911491145038,1.3,3.92730408899227));
#28676=CARTESIAN_POINT('Ctrl Pts',(3.28506288912775,1.3,3.91334417124239));
#28677=CARTESIAN_POINT('Ctrl Pts',(3.29127623046883,1.3,3.8959033209131));
#28678=CARTESIAN_POINT('Ctrl Pts',(3.30120174405925,1.30000000000002,3.87389948305366));
#28679=CARTESIAN_POINT('Ctrl Pts',(3.31308542169651,1.3,3.83865271317822));
#28680=CARTESIAN_POINT('Ctrl Pts',(3.32618522651639,1.30000000000001,3.80439139269443));
#28681=CARTESIAN_POINT('Ctrl Pts',(3.33701682672449,1.30000000000001,3.76851394130066));
#28682=CARTESIAN_POINT('Ctrl Pts',(3.34674839854031,1.30000000000003,3.73916815385308));
#28683=CARTESIAN_POINT('Ctrl Pts',(3.3533947067203,1.30000000000002,3.71491322535318));
#28684=CARTESIAN_POINT('Ctrl Pts',(3.3569075990033,1.30000000000002,3.70182795548531));
#28685=CARTESIAN_POINT('Ctrl Pts',(3.3571574986747,1.30000000000002,3.70089472823323));
#28686=CARTESIAN_POINT('Ctrl Pts',(3.35740469928613,1.30000000000002,3.69995929704989));
#28687=CARTESIAN_POINT('',(2.95357407114036,1.30000000000001,3.35306612923546));
#28688=CARTESIAN_POINT('Origin',(0.,1.3,7.2));
#28689=CARTESIAN_POINT('',(2.70549646903679,1.3,3.50427905152391));
#28690=CARTESIAN_POINT('Ctrl Pts',(2.95357407115217,1.3,3.35306612925858));
#28691=CARTESIAN_POINT('Ctrl Pts',(2.88599776229586,1.3,3.38758551557036));
#28692=CARTESIAN_POINT('Ctrl Pts',(2.8198851485551,1.3,3.42559236828672));
#28693=CARTESIAN_POINT('Ctrl Pts',(2.71359164015416,1.3,3.50008522613048));
#28694=CARTESIAN_POINT('Ctrl Pts',(2.71105385687628,1.3,3.50232850732212));
#28695=CARTESIAN_POINT('Ctrl Pts',(2.7054964690368,1.3,3.50427905152391));
#28696=CARTESIAN_POINT('',(2.5158767249182,1.3,3.37268750121688));
#28697=CARTESIAN_POINT('',(2.70549646903679,1.3,3.50427905152391));
#28698=CARTESIAN_POINT('',(2.55661739137892,1.29999999999997,3.0785672983659));
#28699=CARTESIAN_POINT('Ctrl Pts',(2.5158767249182,1.3,3.37268750121688));
#28700=CARTESIAN_POINT('Ctrl Pts',(2.51547129339445,1.3,3.36394515992304));
#28701=CARTESIAN_POINT('Ctrl Pts',(2.51855424420958,1.3,3.35207075092507));
#28702=CARTESIAN_POINT('Ctrl Pts',(2.52283590576821,1.3,3.33454697355417));
#28703=CARTESIAN_POINT('Ctrl Pts',(2.52646568091669,1.29999999999998,3.32005827780177));
#28704=CARTESIAN_POINT('Ctrl Pts',(2.53015462701597,1.3,3.29896774216744));
#28705=CARTESIAN_POINT('Ctrl Pts',(2.53556382481435,1.29999999999996,3.26903445978772));
#28706=CARTESIAN_POINT('Ctrl Pts',(2.54069414220718,1.29999999999997,3.23896280698673));
#28707=CARTESIAN_POINT('Ctrl Pts',(2.54562846964274,1.29999999999995,3.19912449820451));
#28708=CARTESIAN_POINT('Ctrl Pts',(2.5491865482161,1.29999999999994,3.17163804176601));
#28709=CARTESIAN_POINT('Ctrl Pts',(2.55097589650377,1.29999999999994,3.14662539106063));
#28710=CARTESIAN_POINT('Ctrl Pts',(2.55239378124017,1.29999999999994,3.13435370671797));
#28711=CARTESIAN_POINT('Ctrl Pts',(2.55405997194999,1.29999999999994,3.11897444393603));
#28712=CARTESIAN_POINT('Ctrl Pts',(2.55513657431493,1.29999999999992,3.1001254150743));
#28713=CARTESIAN_POINT('Ctrl Pts',(2.55602160759642,1.29999999999992,3.08668496437601));
#28714=CARTESIAN_POINT('Ctrl Pts',(2.55654773472364,1.29999999999992,3.07951048822781));
#28715=CARTESIAN_POINT('Ctrl Pts',(2.55661739137288,1.29999999999992,3.0785672984477));
#28716=CARTESIAN_POINT('',(2.08911835436551,1.30000000000047,2.82300508328796));
#28717=CARTESIAN_POINT('Origin',(0.,1.3,7.2));
#28718=CARTESIAN_POINT('',(1.87799128879385,1.3,3.02253507588753));
#28719=CARTESIAN_POINT('Ctrl Pts',(2.08911835439991,1.3,2.82300508332989));
#28720=CARTESIAN_POINT('Ctrl Pts',(2.03046284013333,1.3,2.87112862669476));
#28721=CARTESIAN_POINT('Ctrl Pts',(1.97359865399671,1.3,2.92188244262196));
#28722=CARTESIAN_POINT('Ctrl Pts',(1.88576178563236,1.3,3.01598267558689));
#28723=CARTESIAN_POINT('Ctrl Pts',(1.8835507587602,1.3,3.01914952488677));
#28724=CARTESIAN_POINT('Ctrl Pts',(1.87799128879385,1.3,3.02253507588753));
#28725=CARTESIAN_POINT('',(1.66515576931082,1.3,2.93324327828999));
#28726=CARTESIAN_POINT('',(1.87799128879385,1.3,3.02253507588753));
#28727=CARTESIAN_POINT('',(1.64381178161171,1.3,2.63706423159009));
#28728=CARTESIAN_POINT('Ctrl Pts',(1.66515576931082,1.3,2.93324327829));
#28729=CARTESIAN_POINT('Ctrl Pts',(1.66294156247849,1.3,2.92477627208227));
#28730=CARTESIAN_POINT('Ctrl Pts',(1.66351030995394,1.3,2.9125249551468));
#28731=CARTESIAN_POINT('Ctrl Pts',(1.66412261980249,1.3,2.89450855944385));
#28732=CARTESIAN_POINT('Ctrl Pts',(1.66452629020269,1.3,2.87955334577841));
#28733=CARTESIAN_POINT('Ctrl Pts',(1.66423539774643,1.3,2.86129400510938));
#28734=CARTESIAN_POINT('Ctrl Pts',(1.66273115025757,1.3,2.83678667555902));
#28735=CARTESIAN_POINT('Ctrl Pts',(1.6626944242077,1.3,2.81260856801406));
#28736=CARTESIAN_POINT('Ctrl Pts',(1.6605733140711,1.3,2.79100115316553));
#28737=CARTESIAN_POINT('Ctrl Pts',(1.65871139278267,1.3,2.76644084839449));
#28738=CARTESIAN_POINT('Ctrl Pts',(1.65715322685088,1.3,2.74196829601108));
#28739=CARTESIAN_POINT('Ctrl Pts',(1.65352500342455,1.3,2.71406419108784));
#28740=CARTESIAN_POINT('Ctrl Pts',(1.6504187223115,1.3,2.68327445254122));
#28741=CARTESIAN_POINT('Ctrl Pts',(1.64675072801477,1.3,2.65752408921042));
#28742=CARTESIAN_POINT('Ctrl Pts',(1.64394619751435,1.3,2.63799905453949));
#28743=CARTESIAN_POINT('Ctrl Pts',(1.64381178161338,1.3,2.63706423160175));
#28744=CARTESIAN_POINT('',(1.13357773497359,1.30000000000006,2.48433445646712));
#28745=CARTESIAN_POINT('Origin',(0.,1.3,7.2));
#28746=CARTESIAN_POINT('',(0.968408877628583,1.3,2.72336636313561));
#28747=CARTESIAN_POINT('Ctrl Pts',(1.13357773499831,1.3,2.4843344564871));
#28748=CARTESIAN_POINT('Ctrl Pts',(1.13293652139485,1.3,2.48512733677124));
#28749=CARTESIAN_POINT('Ctrl Pts',(1.1322867097125,1.3,2.48593132009101));
#28750=CARTESIAN_POINT('Ctrl Pts',(1.13162887637119,1.3,2.48674634991899));
#28751=CARTESIAN_POINT('Ctrl Pts',(1.12479465001758,1.3,2.49521368956197));
#28752=CARTESIAN_POINT('Ctrl Pts',(1.11708786724918,1.3,2.5048693306749));
#28753=CARTESIAN_POINT('Ctrl Pts',(1.10893902398972,1.3,2.51546374956644));
#28754=CARTESIAN_POINT('Ctrl Pts',(1.10193451489362,1.3,2.52457040447816));
#28755=CARTESIAN_POINT('Ctrl Pts',(1.09462362918233,1.3,2.53438290697181));
#28756=CARTESIAN_POINT('Ctrl Pts',(1.08693530229986,1.3,2.54448550662487));
#28757=CARTESIAN_POINT('Ctrl Pts',(1.07978720725581,1.3,2.55387823193637));
#28758=CARTESIAN_POINT('Ctrl Pts',(1.07228148729113,1.3,2.56350592466692));
#28759=CARTESIAN_POINT('Ctrl Pts',(1.06521521123111,1.3,2.57365000947087));
#28760=CARTESIAN_POINT('Ctrl Pts',(1.06180540316093,1.3,2.57854500393971));
#28761=CARTESIAN_POINT('Ctrl Pts',(1.05850493335534,1.3,2.58356304708329));
#28762=CARTESIAN_POINT('Ctrl Pts',(1.05512786151265,1.3,2.5885393160823));
#28763=CARTESIAN_POINT('Ctrl Pts',(1.0517557761572,1.3,2.5935082372655));
#28764=CARTESIAN_POINT('Ctrl Pts',(1.04830595503031,1.3,2.59843593972442));
#28765=CARTESIAN_POINT('Ctrl Pts',(1.04490139855508,1.3,2.6033778059502));
#28766=CARTESIAN_POINT('Ctrl Pts',(1.0345032720822,1.3,2.61847115229406));
#28767=CARTESIAN_POINT('Ctrl Pts',(1.02453521099312,1.3,2.63369301355648));
#28768=CARTESIAN_POINT('Ctrl Pts',(1.01523157341463,1.3,2.648306025813));
#28769=CARTESIAN_POINT('Ctrl Pts',(1.01197415980419,1.3,2.65342237139422));
#28770=CARTESIAN_POINT('Ctrl Pts',(1.0087985257201,1.3,2.65846528371442));
#28771=CARTESIAN_POINT('Ctrl Pts',(1.00576925730934,1.3,2.66343712573536));
#28772=CARTESIAN_POINT('Ctrl Pts',(1.00250701753485,1.3,2.66879133625551));
#28773=CARTESIAN_POINT('Ctrl Pts',(0.99938314075874,1.3,2.67410046903923));
#28774=CARTESIAN_POINT('Ctrl Pts',(0.996624580065918,1.3,2.67871368637101));
#28775=CARTESIAN_POINT('Ctrl Pts',(0.993116511760298,1.3,2.68458032601054));
#28776=CARTESIAN_POINT('Ctrl Pts',(0.990100803084034,1.3,2.68958524992309));
#28777=CARTESIAN_POINT('Ctrl Pts',(0.987617586884602,1.3,2.6939842956337));
#28778=CARTESIAN_POINT('Ctrl Pts',(0.986011479870618,1.3,2.69682953245692));
#28779=CARTESIAN_POINT('Ctrl Pts',(0.984612560913104,1.3,2.69941205955226));
#28780=CARTESIAN_POINT('Ctrl Pts',(0.983335702194529,1.3,2.70174695396398));
#28781=CARTESIAN_POINT('Ctrl Pts',(0.976916590415545,1.3,2.713485095391));
#28782=CARTESIAN_POINT('Ctrl Pts',(0.973272619642238,1.3,2.7187765629255));
#28783=CARTESIAN_POINT('Ctrl Pts',(0.968408877628585,1.3,2.72336636313561));
#28784=CARTESIAN_POINT('',(0.74165951628067,1.3,2.68027679827216));
#28785=CARTESIAN_POINT('',(0.968408877628583,1.3,2.72336636313561));
#28786=CARTESIAN_POINT('',(0.659051978146154,1.3,2.39498694173454));
#28787=CARTESIAN_POINT('Ctrl Pts',(0.74165951628067,1.3,2.68027679827216));
#28788=CARTESIAN_POINT('Ctrl Pts',(0.737733305603287,1.3,2.67245517595099));
#28789=CARTESIAN_POINT('Ctrl Pts',(0.735713875635836,1.3,2.66035957958182));
#28790=CARTESIAN_POINT('Ctrl Pts',(0.732597760872633,1.3,2.64260793958377));
#28791=CARTESIAN_POINT('Ctrl Pts',(0.729765699114481,1.3,2.62790692781172));
#28792=CARTESIAN_POINT('Ctrl Pts',(0.726557820517931,1.3,2.61305934494932));
#28793=CARTESIAN_POINT('Ctrl Pts',(0.723151878203878,1.3,2.60124260806693));
#28794=CARTESIAN_POINT('Ctrl Pts',(0.720709138865025,1.3,2.59235073662494));
#28795=CARTESIAN_POINT('Ctrl Pts',(0.71634712092609,1.3,2.57167599474918));
#28796=CARTESIAN_POINT('Ctrl Pts',(0.707491994511335,1.3,2.54210786089461));
#28797=CARTESIAN_POINT('Ctrl Pts',(0.69816516774291,1.3,2.50962744616599));
#28798=CARTESIAN_POINT('Ctrl Pts',(0.690779760699569,1.3,2.48601858192387));
#28799=CARTESIAN_POINT('Ctrl Pts',(0.684623565179564,1.3,2.46832269985239));
#28800=CARTESIAN_POINT('Ctrl Pts',(0.676935095157866,1.3,2.44474912633269));
#28801=CARTESIAN_POINT('Ctrl Pts',(0.669050883568352,1.3,2.42118640333502));
#28802=CARTESIAN_POINT('Ctrl Pts',(0.661798923496942,1.30000000000001,2.40266552561176));
#28803=CARTESIAN_POINT('Ctrl Pts',(0.659371426705916,1.30000000000001,2.39588686093049));
#28804=CARTESIAN_POINT('Ctrl Pts',(0.659051978154449,1.30000000000001,2.39498694175791));
#28805=CARTESIAN_POINT('',(0.128170675781554,1.30000000000107,2.35169387542681));
#28806=CARTESIAN_POINT('Origin',(0.,1.3,7.2));
#28807=CARTESIAN_POINT('',(0.0165023515695843,1.3,2.61984802158616));
#28808=CARTESIAN_POINT('Ctrl Pts',(0.128170675807936,1.3,2.35169387544013));
#28809=CARTESIAN_POINT('Ctrl Pts',(0.10619951312427,1.3,2.39523277512288));
#28810=CARTESIAN_POINT('Ctrl Pts',(0.0854073494869826,1.29999999999995,
2.43946186308817));
#28811=CARTESIAN_POINT('Ctrl Pts',(0.0585207374510833,1.29999999999995,
2.50734591272452));
#28812=CARTESIAN_POINT('Ctrl Pts',(0.0487206764552959,1.29999999999993,
2.52957674635612));
#28813=CARTESIAN_POINT('Ctrl Pts',(0.0354428122597672,1.29999999999993,
2.56889180573038));
#28814=CARTESIAN_POINT('Ctrl Pts',(0.0324836161788516,1.29999999999993,
2.5767603968036));
#28815=CARTESIAN_POINT('Ctrl Pts',(0.0251452812246871,1.29999999999993,
2.60004278591798));
#28816=CARTESIAN_POINT('Ctrl Pts',(0.022543073780594,1.3,2.61111103088363));
#28817=CARTESIAN_POINT('Ctrl Pts',(0.0165023515695844,1.3,2.61984802158616));
#28818=CARTESIAN_POINT('',(-0.214250816488161,1.3,2.624843910208));
#28819=CARTESIAN_POINT('',(0.0165023515695843,1.3,2.61984802158616));
#28820=CARTESIAN_POINT('',(-0.354392897366409,1.3,2.36296519815122));
#28821=CARTESIAN_POINT('Ctrl Pts',(-0.21425081648816,1.3,2.624843910208));
#28822=CARTESIAN_POINT('Ctrl Pts',(-0.219717436763953,1.3,2.61800951420116));
#28823=CARTESIAN_POINT('Ctrl Pts',(-0.224209275765746,1.3,2.606595622045));
#28824=CARTESIAN_POINT('Ctrl Pts',(-0.231052456917044,1.3,2.58990382504299));
#28825=CARTESIAN_POINT('Ctrl Pts',(-0.236623358264727,1.3,2.57604856509846));
#28826=CARTESIAN_POINT('Ctrl Pts',(-0.2460751938082,1.3,2.55682624237417));
#28827=CARTESIAN_POINT('Ctrl Pts',(-0.259183769683128,1.3,2.52940909662549));
#28828=CARTESIAN_POINT('Ctrl Pts',(-0.274355810881998,1.3,2.49938890693942));
#28829=CARTESIAN_POINT('Ctrl Pts',(-0.290586106563452,1.3,2.46962310770296));
#28830=CARTESIAN_POINT('Ctrl Pts',(-0.302397069786213,1.29999999999999,
2.44799378564757));
#28831=CARTESIAN_POINT('Ctrl Pts',(-0.323310367858908,1.3,2.41324546052299));
#28832=CARTESIAN_POINT('Ctrl Pts',(-0.33939401831521,1.3,2.38564120596506));
#28833=CARTESIAN_POINT('Ctrl Pts',(-0.353861208044329,1.3,2.36377256592943));
#28834=CARTESIAN_POINT('Ctrl Pts',(-0.354392897361749,1.3,2.3629651981583));
#28835=CARTESIAN_POINT('',(-0.882736269392908,1.3,2.43100884057243));
#28836=CARTESIAN_POINT('Origin',(0.,1.3,7.2));
#28837=CARTESIAN_POINT('',(-0.936125406440072,1.3,2.71650429950101));
#28838=CARTESIAN_POINT('Ctrl Pts',(-0.882736269392908,1.3,2.43100884057243));
#28839=CARTESIAN_POINT('Ctrl Pts',(-0.890585516016561,1.3,2.46173198670934));
#28840=CARTESIAN_POINT('Ctrl Pts',(-0.914120009049791,1.29999999996271,
2.56513894027015));
#28841=CARTESIAN_POINT('Ctrl Pts',(-0.931163753333676,1.29999999996271,
2.67599020345154));
#28842=CARTESIAN_POINT('Ctrl Pts',(-0.929449820781408,1.3,2.70051432210213));
#28843=CARTESIAN_POINT('Ctrl Pts',(-0.936125406440074,1.3,2.716504299501));
#28844=CARTESIAN_POINT('',(-1.16079736048697,1.3,2.76936729730244));
#28845=CARTESIAN_POINT('',(-0.936125406440072,1.3,2.71650429950101));
#28846=CARTESIAN_POINT('',(-1.3523957842154,1.30000000000138,2.54237068259109));
#28847=CARTESIAN_POINT('Ctrl Pts',(-1.16079736048697,1.3,2.76936729730244));
#28848=CARTESIAN_POINT('Ctrl Pts',(-1.16756547282336,1.3,2.76381882351047));
#28849=CARTESIAN_POINT('Ctrl Pts',(-1.17429793045071,1.3,2.75357283179475));
#28850=CARTESIAN_POINT('Ctrl Pts',(-1.18440354486965,1.3,2.7386418212914));
#28851=CARTESIAN_POINT('Ctrl Pts',(-1.19282120230342,1.3,2.72628912988518));
#28852=CARTESIAN_POINT('Ctrl Pts',(-1.20387759611253,1.3,2.71172137984579));
#28853=CARTESIAN_POINT('Ctrl Pts',(-1.22296240651216,1.3,2.68787374759291));
#28854=CARTESIAN_POINT('Ctrl Pts',(-1.24183231204913,1.3,2.66390421538196));
#28855=CARTESIAN_POINT('Ctrl Pts',(-1.26206094764912,1.30000000000001,2.64057600636631));
#28856=CARTESIAN_POINT('Ctrl Pts',(-1.27762376107936,1.30000000000001,2.62164883825251));
#28857=CARTESIAN_POINT('Ctrl Pts',(-1.29899075380456,1.29999999999999,2.59887488144818));
#28858=CARTESIAN_POINT('Ctrl Pts',(-1.32381937982074,1.3,2.57122791399148));
#28859=CARTESIAN_POINT('Ctrl Pts',(-1.34203682692771,1.30000000000001,2.55259610655428));
#28860=CARTESIAN_POINT('Ctrl Pts',(-1.35170736374796,1.30000000000001,2.5430533015253));
#28861=CARTESIAN_POINT('Ctrl Pts',(-1.3523945461556,1.30000000000001,2.54237191022484));
#28862=CARTESIAN_POINT('',(-1.85490568625463,1.30000000000046,2.7187250815555));
#28863=CARTESIAN_POINT('Origin',(0.,1.3,7.2));
#28864=CARTESIAN_POINT('',(-1.84783999216021,1.3,3.00911085372699));
#28865=CARTESIAN_POINT('Ctrl Pts',(-1.85490568621173,1.3,2.71872508155732));
#28866=CARTESIAN_POINT('Ctrl Pts',(-1.85494906266401,1.3,2.71974586259111));
#28867=CARTESIAN_POINT('Ctrl Pts',(-1.85498765318356,1.3,2.7207652106144));
#28868=CARTESIAN_POINT('Ctrl Pts',(-1.85502062869155,1.3,2.72178310517736));
#28869=CARTESIAN_POINT('Ctrl Pts',(-1.85521915454548,1.3,2.72791124086604));
#28870=CARTESIAN_POINT('Ctrl Pts',(-1.85521812104922,1.3,2.73398519666606));
#28871=CARTESIAN_POINT('Ctrl Pts',(-1.85546360136794,1.3,2.73998240712142));
#28872=CARTESIAN_POINT('Ctrl Pts',(-1.85571689038058,1.3,2.74617038798602));
#28873=CARTESIAN_POINT('Ctrl Pts',(-1.85621651005613,1.3,2.75228028849141));
#28874=CARTESIAN_POINT('Ctrl Pts',(-1.85637531506373,1.3,2.75831933810552));
#28875=CARTESIAN_POINT('Ctrl Pts',(-1.85653649953747,1.3,2.76444887424915));
#28876=CARTESIAN_POINT('Ctrl Pts',(-1.85635497434812,1.3,2.77050160335946));
#28877=CARTESIAN_POINT('Ctrl Pts',(-1.85649256135086,1.3,2.77645639068877));
#28878=CARTESIAN_POINT('Ctrl Pts',(-1.85663595615561,1.3,2.7826625406115));
#28879=CARTESIAN_POINT('Ctrl Pts',(-1.85709812605095,1.3,2.7887665601669));
#28880=CARTESIAN_POINT('Ctrl Pts',(-1.85723117976892,1.3,2.79476573133978));
#28881=CARTESIAN_POINT('Ctrl Pts',(-1.85736766436802,1.3,2.80091959524531));
#28882=CARTESIAN_POINT('Ctrl Pts',(-1.85717181951977,1.3,2.80695968052047));
#28883=CARTESIAN_POINT('Ctrl Pts',(-1.85717055652404,1.3,2.81287274002393));
#28884=CARTESIAN_POINT('Ctrl Pts',(-1.85716923144163,1.3,2.8190764753326));
#28885=CARTESIAN_POINT('Ctrl Pts',(-1.85736110288761,1.3,2.82514297239297));
#28886=CARTESIAN_POINT('Ctrl Pts',(-1.85737655537845,1.3,2.83105817463949));
#28887=CARTESIAN_POINT('Ctrl Pts',(-1.85740983197251,1.3,2.84379643062085));
#28888=CARTESIAN_POINT('Ctrl Pts',(-1.85670509444853,1.3,2.85582368886185));
#28889=CARTESIAN_POINT('Ctrl Pts',(-1.85623323659832,1.3,2.86702301390781));
#28890=CARTESIAN_POINT('Ctrl Pts',(-1.85567755293928,1.3,2.88021190526076));
#28891=CARTESIAN_POINT('Ctrl Pts',(-1.85534153484999,1.3,2.89225944470745));
#28892=CARTESIAN_POINT('Ctrl Pts',(-1.85491006186869,1.3,2.90295344320832));
#28893=CARTESIAN_POINT('Ctrl Pts',(-1.85478465332402,1.3,2.90606167674066));
#28894=CARTESIAN_POINT('Ctrl Pts',(-1.85465444606568,1.3,2.90905549205128));
#28895=CARTESIAN_POINT('Ctrl Pts',(-1.85453421931241,1.3,2.91193055999209));
#28896=CARTESIAN_POINT('Ctrl Pts',(-1.85425731305134,1.3,2.91855241654326));
#28897=CARTESIAN_POINT('Ctrl Pts',(-1.85400169649198,1.3,2.92454378031362));
#28898=CARTESIAN_POINT('Ctrl Pts',(-1.85357635954475,1.3,2.92982815978896));
#28899=CARTESIAN_POINT('Ctrl Pts',(-1.85331787482462,1.3,2.93303956984536));
#28900=CARTESIAN_POINT('Ctrl Pts',(-1.85301417358302,1.3,2.9359903706631));
#28901=CARTESIAN_POINT('Ctrl Pts',(-1.85276389577182,1.3,2.93867303583745));
#28902=CARTESIAN_POINT('Ctrl Pts',(-1.85203942456943,1.3,2.9464384612068));
#28903=CARTESIAN_POINT('Ctrl Pts',(-1.85165865380786,1.3,2.95166509583937));
#28904=CARTESIAN_POINT('Ctrl Pts',(-1.85124074681822,1.3,2.95641359523244));
#28905=CARTESIAN_POINT('Ctrl Pts',(-1.85096598292866,1.3,2.9595356204562));
#28906=CARTESIAN_POINT('Ctrl Pts',(-1.85069885767855,1.3,2.96237084157569));
#28907=CARTESIAN_POINT('Ctrl Pts',(-1.85042671469841,1.3,2.96526229133589));
#28908=CARTESIAN_POINT('Ctrl Pts',(-1.85016557442577,1.3,2.96803684013488));
#28909=CARTESIAN_POINT('Ctrl Pts',(-1.84990350496385,1.3,2.9708641856712));
#28910=CARTESIAN_POINT('Ctrl Pts',(-1.84954418939433,1.3,2.97403920416527));
#28911=CARTESIAN_POINT('Ctrl Pts',(-1.84923315994381,1.3,2.97678755225074));
#28912=CARTESIAN_POINT('Ctrl Pts',(-1.84882683041588,1.3,2.97989392199881));
#28913=CARTESIAN_POINT('Ctrl Pts',(-1.84844777243925,1.3,2.98284440587253));
#28914=CARTESIAN_POINT('Ctrl Pts',(-1.84725567213586,1.3,2.99212338939983));
#28915=CARTESIAN_POINT('Ctrl Pts',(-1.8462860297191,1.3,3.00085502123862));
#28916=CARTESIAN_POINT('Ctrl Pts',(-1.84783999216021,1.3,3.00911085372699));
#28917=CARTESIAN_POINT('',(-2.05661148970878,1.3,3.10753059403928));
#28918=CARTESIAN_POINT('',(-1.84783999216022,1.3,3.00911085372699));
#28919=CARTESIAN_POINT('',(-2.29120499210816,1.30000000000064,2.92532110174576));
#28920=CARTESIAN_POINT('Ctrl Pts',(-2.05661148970878,1.3,3.10753059403928));
#28921=CARTESIAN_POINT('Ctrl Pts',(-2.06438529511965,1.3,3.10351053739145));
#28922=CARTESIAN_POINT('Ctrl Pts',(-2.07309811100438,1.3,3.09488481470888));
#28923=CARTESIAN_POINT('Ctrl Pts',(-2.08608645028851,1.3,3.08238039314201));
#28924=CARTESIAN_POINT('Ctrl Pts',(-2.09688680253806,1.3,3.07204590157201));
#28925=CARTESIAN_POINT('Ctrl Pts',(-2.11072923711644,1.3,3.06009427260729));
#28926=CARTESIAN_POINT('Ctrl Pts',(-2.13435227632379,1.3,3.0407328914854));
#28927=CARTESIAN_POINT('Ctrl Pts',(-2.15779105518433,1.29999999999999,3.02120880625423));
#28928=CARTESIAN_POINT('Ctrl Pts',(-2.18242600362798,1.29999999999999,3.00259488826929));
#28929=CARTESIAN_POINT('Ctrl Pts',(-2.20158377310446,1.29999999999999,2.98731694105395));
#28930=CARTESIAN_POINT('Ctrl Pts',(-2.22721864903229,1.29999999999999,2.96948359344277));
#28931=CARTESIAN_POINT('Ctrl Pts',(-2.25725367801875,1.29999999999997,2.94760389756073));
#28932=CARTESIAN_POINT('Ctrl Pts',(-2.27894790606329,1.29999999999997,2.93316799584485));
#28933=CARTESIAN_POINT('Ctrl Pts',(-2.29039127170519,1.29999999999997,2.92584463101117));
#28934=CARTESIAN_POINT('Ctrl Pts',(-2.29120499200655,1.29999999999997,2.92532110186514));
#28935=CARTESIAN_POINT('',(-2.74608525937212,1.30000000000049,3.202311199222));
#28936=CARTESIAN_POINT('Origin',(0.,1.3,7.2));
#28937=CARTESIAN_POINT('',(-2.67879510330291,1.3,3.48487937376242));
#28938=CARTESIAN_POINT('Ctrl Pts',(-2.74608525933252,1.3,3.20231119921555));
#28939=CARTESIAN_POINT('Ctrl Pts',(-2.74592314706517,1.3,3.20330586994931));
#28940=CARTESIAN_POINT('Ctrl Pts',(-2.74575725588899,1.3,3.20431266911));
#28941=CARTESIAN_POINT('Ctrl Pts',(-2.745587413402,1.3,3.20533113938524));
#28942=CARTESIAN_POINT('Ctrl Pts',(-2.74297531402366,1.3,3.22099474405838));
#28943=CARTESIAN_POINT('Ctrl Pts',(-2.73928848452582,1.3,3.23938453120443));
#28944=CARTESIAN_POINT('Ctrl Pts',(-2.73586109861741,1.3,3.25921559597869));
#28945=CARTESIAN_POINT('Ctrl Pts',(-2.73484312557184,1.3,3.26510565036547));
#28946=CARTESIAN_POINT('Ctrl Pts',(-2.73386685344387,1.3,3.2711284112336));
#28947=CARTESIAN_POINT('Ctrl Pts',(-2.73254890665973,1.3,3.27716215918157));
#28948=CARTESIAN_POINT('Ctrl Pts',(-2.73191131995472,1.3,3.28008112185844));
#28949=CARTESIAN_POINT('Ctrl Pts',(-2.73119017390953,1.3,3.28300152537924));
#28950=CARTESIAN_POINT('Ctrl Pts',(-2.73051127150851,1.3,3.28594500588927));
#28951=CARTESIAN_POINT('Ctrl Pts',(-2.72849187055887,1.3,3.29470041363015));
#28952=CARTESIAN_POINT('Ctrl Pts',(-2.72685428417164,1.3,3.30366556692271));
#28953=CARTESIAN_POINT('Ctrl Pts',(-2.72492380642212,1.3,3.31257530148778));
#28954=CARTESIAN_POINT('Ctrl Pts',(-2.72236580737704,1.3,3.32438123528583));
#28955=CARTESIAN_POINT('Ctrl Pts',(-2.71928291517288,1.3,3.33607991251617));
#28956=CARTESIAN_POINT('Ctrl Pts',(-2.71638775539464,1.3,3.34754495029874));
#28957=CARTESIAN_POINT('Ctrl Pts',(-2.71255125582638,1.3,3.36273776032373));
#28958=CARTESIAN_POINT('Ctrl Pts',(-2.70901769291549,1.3,3.377521969348));
#28959=CARTESIAN_POINT('Ctrl Pts',(-2.70554870841793,1.3,3.39118652568365));
#28960=CARTESIAN_POINT('Ctrl Pts',(-2.7040218274528,1.3,3.39720100945563));
#28961=CARTESIAN_POINT('Ctrl Pts',(-2.70250594885501,1.3,3.40299854130969));
#28962=CARTESIAN_POINT('Ctrl Pts',(-2.70087427516177,1.3,3.40848409353771));
#28963=CARTESIAN_POINT('Ctrl Pts',(-2.70000778040026,1.3,3.41139717737869));
#28964=CARTESIAN_POINT('Ctrl Pts',(-2.69911190347081,1.3,3.41422269682275));
#28965=CARTESIAN_POINT('Ctrl Pts',(-2.69825737393594,1.3,3.41697217111659));
#28966=CARTESIAN_POINT('Ctrl Pts',(-2.69618031045467,1.3,3.4236551848866));
#28967=CARTESIAN_POINT('Ctrl Pts',(-2.69436074527778,1.3,3.42976051800602));
#28968=CARTESIAN_POINT('Ctrl Pts',(-2.69306997616279,1.3,3.43401819985236));
#28969=CARTESIAN_POINT('Ctrl Pts',(-2.69114011425413,1.3,3.44038396884935));
#28970=CARTESIAN_POINT('Ctrl Pts',(-2.68999653222302,1.3,3.44420087101193));
#28971=CARTESIAN_POINT('Ctrl Pts',(-2.68773832472882,1.3,3.45092138645622));
#28972=CARTESIAN_POINT('Ctrl Pts',(-2.68689484823012,1.3,3.45343160611094));
#28973=CARTESIAN_POINT('Ctrl Pts',(-2.68582412772417,1.3,3.45649798649749));
#28974=CARTESIAN_POINT('Ctrl Pts',(-2.68484689460198,1.3,3.4593048285032));
#28975=CARTESIAN_POINT('Ctrl Pts',(-2.68164638744206,1.3,3.46849743335057));
#28976=CARTESIAN_POINT('Ctrl Pts',(-2.67898720638086,1.3,3.47666793233799));
#28977=CARTESIAN_POINT('Ctrl Pts',(-2.6787951033029,1.3,3.48487937376242));
#28978=CARTESIAN_POINT('',(-2.86254182811346,1.3,3.6245544416636));
#28979=CARTESIAN_POINT('',(-2.67879510330291,1.3,3.48487937376242));
#28980=CARTESIAN_POINT('',(-3.12967817046588,1.29999999999996,3.49492043954391));
#28981=CARTESIAN_POINT('Ctrl Pts',(-2.86254182811346,1.3,3.6245544416636));
#28982=CARTESIAN_POINT('Ctrl Pts',(-2.87098157399952,1.3,3.62223849792578));
#28983=CARTESIAN_POINT('Ctrl Pts',(-2.88132223312521,1.3,3.61563726783235));
#28984=CARTESIAN_POINT('Ctrl Pts',(-2.8966652799432,1.3,3.60615009400148));
#28985=CARTESIAN_POINT('Ctrl Pts',(-2.90932323850128,1.29999999999998,3.59822082837081));
#28986=CARTESIAN_POINT('Ctrl Pts',(-2.92824173701722,1.29999999999999,3.58819528871223));
#28987=CARTESIAN_POINT('Ctrl Pts',(-2.95503853269752,1.29999999999997,3.57380109025187));
#28988=CARTESIAN_POINT('Ctrl Pts',(-2.98205336859788,1.29999999999997,3.55962955254953));
#28989=CARTESIAN_POINT('Ctrl Pts',(-3.01841720312939,1.29999999999995,3.54262615901524));
#28990=CARTESIAN_POINT('Ctrl Pts',(-3.0434588220131,1.29999999999994,3.53074835161772));
#28991=CARTESIAN_POINT('Ctrl Pts',(-3.06669431743405,1.29999999999993,3.52131722426942));
#28992=CARTESIAN_POINT('Ctrl Pts',(-3.07792722226869,1.29999999999993,3.51617656284746));
#28993=CARTESIAN_POINT('Ctrl Pts',(-3.0920388719552,1.29999999999991,3.50983944286351));
#28994=CARTESIAN_POINT('Ctrl Pts',(-3.10963261570923,1.29999999999992,3.50299078553603));
#28995=CARTESIAN_POINT('Ctrl Pts',(-3.12214179520417,1.29999999999991,3.49799566328401));
#28996=CARTESIAN_POINT('Ctrl Pts',(-3.12880259493956,1.29999999999991,3.4952781850355));
#28997=CARTESIAN_POINT('Ctrl Pts',(-3.12967817039088,1.29999999999991,3.49492043957456));
#28998=CARTESIAN_POINT('',(-3.51715936790342,1.30000000000004,3.86052549337951));
#28999=CARTESIAN_POINT('Origin',(0.,1.3,7.2));
#29000=CARTESIAN_POINT('',(-3.39267401414619,1.3,4.12301649229107));
#29001=CARTESIAN_POINT('Ctrl Pts',(-3.51715936786488,1.3,3.86052549336462));
#29002=CARTESIAN_POINT('Ctrl Pts',(-3.50582685066179,1.3,3.88984355757898));
#29003=CARTESIAN_POINT('Ctrl Pts',(-3.46685584273537,1.3,3.98767483334669));
#29004=CARTESIAN_POINT('Ctrl Pts',(-3.40261508876044,1.3,4.10231519737892));
#29005=CARTESIAN_POINT('Ctrl Pts',(-3.39533368135243,1.3,4.11180043398003));
#29006=CARTESIAN_POINT('Ctrl Pts',(-3.3926740141462,1.3,4.12301649229107));
#29007=CARTESIAN_POINT('',(-3.54336535262991,1.3,4.29784241707854));
#29008=CARTESIAN_POINT('',(-3.39267401414619,1.3,4.12301649229107));
#29009=CARTESIAN_POINT('',(-3.83164255228946,1.29999999999999,4.22661550568205));
#29010=CARTESIAN_POINT('Ctrl Pts',(-3.54336535262991,1.3,4.29784241707854));
#29011=CARTESIAN_POINT('Ctrl Pts',(-3.55210218159752,1.3,4.29733180410519));
#29012=CARTESIAN_POINT('Ctrl Pts',(-3.56357804858823,1.3,4.29300353001696));
#29013=CARTESIAN_POINT('Ctrl Pts',(-3.58051111276238,1.3,4.28683090345647));
#29014=CARTESIAN_POINT('Ctrl Pts',(-3.5946404397042,1.3,4.281881159061));
#29015=CARTESIAN_POINT('Ctrl Pts',(-3.61201924717445,1.3,4.27637436927279));
#29016=CARTESIAN_POINT('Ctrl Pts',(-3.63003664337434,1.3,4.27211248343673));
#29017=CARTESIAN_POINT('Ctrl Pts',(-3.65295986932128,1.29999999999998,4.26452737687587));
#29018=CARTESIAN_POINT('Ctrl Pts',(-3.6892645645786,1.3,4.25643069318791));
#29019=CARTESIAN_POINT('Ctrl Pts',(-3.72475552906397,1.29999999999999,4.24706883683854));
#29020=CARTESIAN_POINT('Ctrl Pts',(-3.75540297439471,1.29999999999998,4.24116675613968));
#29021=CARTESIAN_POINT('Ctrl Pts',(-3.77374429985487,1.29999999999998,4.23757924625996));
#29022=CARTESIAN_POINT('Ctrl Pts',(-3.78867292218785,1.29999999999998,4.23397473293131));
#29023=CARTESIAN_POINT('Ctrl Pts',(-3.80118619929376,1.29999999999998,4.23210976365254));
#29024=CARTESIAN_POINT('Ctrl Pts',(-3.81344027727322,1.29999999999998,4.22979565281318));
#29025=CARTESIAN_POINT('Ctrl Pts',(-3.82363173700113,1.29999999999997,4.2280429461226));
#29026=CARTESIAN_POINT('Ctrl Pts',(-3.83071366500148,1.29999999999997,4.22678143362433));
#29027=CARTESIAN_POINT('Ctrl Pts',(-3.83164255214012,1.29999999999997,4.22661550570873));
#29028=CARTESIAN_POINT('',(-4.13466409677445,1.30000000000152,4.66483672982034));
#29029=CARTESIAN_POINT('Origin',(0.,1.3,7.2));
#29030=CARTESIAN_POINT('',(-3.95827679071515,1.3,4.89563255511164));
#29031=CARTESIAN_POINT('Ctrl Pts',(-4.13466409674311,1.3,4.66483672979985));
#29032=CARTESIAN_POINT('Ctrl Pts',(-4.09315488056353,1.3,4.72833921195976));
#29033=CARTESIAN_POINT('Ctrl Pts',(-4.0481896741846,1.30000000000031,4.78987080268933));
#29034=CARTESIAN_POINT('Ctrl Pts',(-3.99253637143538,1.30000000000031,4.85426406366701));
#29035=CARTESIAN_POINT('Ctrl Pts',(-3.98559379871555,1.3000000000003,4.86240513433244));
#29036=CARTESIAN_POINT('Ctrl Pts',(-3.96923168411537,1.3000000000003,4.88009738329383));
#29037=CARTESIAN_POINT('Ctrl Pts',(-3.96254124756276,1.3,4.88662737113017));
#29038=CARTESIAN_POINT('Ctrl Pts',(-3.95827679071516,1.3,4.89563255511163));
#29039=CARTESIAN_POINT('',(-4.06932680828303,1.3,5.09796860496431));
#29040=CARTESIAN_POINT('',(-3.95827679071515,1.3,4.89563255511164));
#29041=CARTESIAN_POINT('',(-4.36610424565707,1.30000000000001,5.0882155138236));
#29042=CARTESIAN_POINT('Ctrl Pts',(-4.06932680828303,1.3,5.09796860496431));
#29043=CARTESIAN_POINT('Ctrl Pts',(-4.07797887898237,1.3,5.09928563899255));
#29044=CARTESIAN_POINT('Ctrl Pts',(-4.09011340671472,1.3,5.09746151167884));
#29045=CARTESIAN_POINT('Ctrl Pts',(-4.10798906787033,1.3,5.09503481582656));
#29046=CARTESIAN_POINT('Ctrl Pts',(-4.12278056955995,1.3,5.09294345303559));
#29047=CARTESIAN_POINT('Ctrl Pts',(-4.14413938009718,1.3,5.091473450798));
#29048=CARTESIAN_POINT('Ctrl Pts',(-4.17448812907648,1.3,5.08925827165076));
#29049=CARTESIAN_POINT('Ctrl Pts',(-4.20490736605425,1.3,5.08723936162841));
#29050=CARTESIAN_POINT('Ctrl Pts',(-4.23275200389569,1.30000000000001,5.08689293279717));
#29051=CARTESIAN_POINT('Ctrl Pts',(-4.25108091289331,1.30000000000001,5.08598794103597));
#29052=CARTESIAN_POINT('Ctrl Pts',(-4.26664152659686,1.30000000000001,5.08612728928339));
#29053=CARTESIAN_POINT('Ctrl Pts',(-4.27900308121979,1.30000000000001,5.08598697165463));
#29054=CARTESIAN_POINT('Ctrl Pts',(-4.29779355786982,1.30000000000001,5.08657564277857));
#29055=CARTESIAN_POINT('Ctrl Pts',(-4.32551587266611,1.30000000000003,5.08605420816759));
#29056=CARTESIAN_POINT('Ctrl Pts',(-4.35171241440574,1.30000000000002,5.08772479474994));
#29057=CARTESIAN_POINT('Ctrl Pts',(-4.36515927599734,1.30000000000002,5.08818455598542));
#29058=CARTESIAN_POINT('Ctrl Pts',(-4.36610424531595,1.30000000000002,5.08821551381243));
#29059=CARTESIAN_POINT('',(-4.57136452277826,1.30000000000254,5.57977581816781));
#29060=CARTESIAN_POINT('Origin',(0.,1.3,7.2));
#29061=CARTESIAN_POINT('',(-4.35088387761047,1.3,5.76896053285564));
#29062=CARTESIAN_POINT('Ctrl Pts',(-4.57136452274418,1.3,5.57977581813352));
#29063=CARTESIAN_POINT('Ctrl Pts',(-4.51754002640381,1.3,5.63325957053971));
#29064=CARTESIAN_POINT('Ctrl Pts',(-4.46083948717456,1.30000000000647,5.68419491725153));
#29065=CARTESIAN_POINT('Ctrl Pts',(-4.38996093886439,1.30000000000647,5.73802002909746));
#29066=CARTESIAN_POINT('Ctrl Pts',(-4.38483171389866,1.30000000000651,5.74208126366599));
#29067=CARTESIAN_POINT('Ctrl Pts',(-4.36574496082626,1.30000000000651,5.75538076255523));
#29068=CARTESIAN_POINT('Ctrl Pts',(-4.35689160691752,1.3,5.76108571890034));
#29069=CARTESIAN_POINT('Ctrl Pts',(-4.35088387761047,1.3,5.76896053285564));
#29070=CARTESIAN_POINT('',(-4.41743915561768,1.3,5.98996365147886));
#29071=CARTESIAN_POINT('',(-4.35088387761047,1.3,5.76896053285564));
#29072=CARTESIAN_POINT('',(-4.70979325221238,1.30000000000053,6.04226621306406));
#29073=CARTESIAN_POINT('Ctrl Pts',(-4.41743915561768,1.3,5.98996365147886));
#29074=CARTESIAN_POINT('Ctrl Pts',(-4.42562833104198,1.3,5.99305077180187));
#29075=CARTESIAN_POINT('Ctrl Pts',(-4.43787410397313,1.30000000000004,5.99377070921043));
#29076=CARTESIAN_POINT('Ctrl Pts',(-4.45586248406724,1.30000000000007,5.99510260510018));
#29077=CARTESIAN_POINT('Ctrl Pts',(-4.47076472138646,1.30000000000009,5.99612876774796));
#29078=CARTESIAN_POINT('Ctrl Pts',(-4.49195835498715,1.30000000000015,5.99908948996134));
#29079=CARTESIAN_POINT('Ctrl Pts',(-4.52210835638369,1.30000000000015,6.00327770721702));
#29080=CARTESIAN_POINT('Ctrl Pts',(-4.55226320816141,1.30000000000036,6.00741263999137));
#29081=CARTESIAN_POINT('Ctrl Pts',(-4.57654950949712,1.30000000000046,6.01237589346951));
#29082=CARTESIAN_POINT('Ctrl Pts',(-4.60070795159453,1.30000000000046,6.0162343787984));
#29083=CARTESIAN_POINT('Ctrl Pts',(-4.6311368113507,1.30000000000088,6.02353250784579));
#29084=CARTESIAN_POINT('Ctrl Pts',(-4.67053008929459,1.30000000000101,6.0319106295725));
#29085=CARTESIAN_POINT('Ctrl Pts',(-4.69577141109484,1.30000000000119,6.0384019209567));
#29086=CARTESIAN_POINT('Ctrl Pts',(-4.70886570174723,1.30000000000123,6.04201282916357));
#29087=CARTESIAN_POINT('Ctrl Pts',(-4.70979325209678,1.30000000000123,6.04226621303244));
#29088=CARTESIAN_POINT('',(-4.80835019122325,1.30000000000007,6.56575364560707));
#29089=CARTESIAN_POINT('Origin',(0.,1.3,7.2));
#29090=CARTESIAN_POINT('',(-4.55333646119701,1.3,6.70483180220308));
#29091=CARTESIAN_POINT('Ctrl Pts',(-4.80835019119519,1.3,6.56575364556359));
#29092=CARTESIAN_POINT('Ctrl Pts',(-4.7434061141498,1.3,6.60767583956299));
#29093=CARTESIAN_POINT('Ctrl Pts',(-4.72650779342684,1.29999999999997,6.61707548172361));
#29094=CARTESIAN_POINT('Ctrl Pts',(-4.6403689076869,1.29999999999997,6.66208434195179));
#29095=CARTESIAN_POINT('Ctrl Pts',(-4.63296554263347,1.29999999999999,6.66644578587599));
#29096=CARTESIAN_POINT('Ctrl Pts',(-4.57698227389077,1.29999999999999,6.69210759502936));
#29097=CARTESIAN_POINT('Ctrl Pts',(-4.56282896282898,1.3,6.6966785332743));
#29098=CARTESIAN_POINT('Ctrl Pts',(-4.55333646119701,1.3,6.70483180220308));
#29099=CARTESIAN_POINT('',(-4.57248821462698,1.3,6.9348430928224));
#29100=CARTESIAN_POINT('',(-4.55333646119701,1.3,6.70483180220308));
#29101=CARTESIAN_POINT('',(-4.84757460734146,1.3,7.04663629419473));
#29102=CARTESIAN_POINT('Ctrl Pts',(-4.57248821462698,1.3,6.9348430928224));
#29103=CARTESIAN_POINT('Ctrl Pts',(-4.5798565885141,1.3,6.93956537746838));
#29104=CARTESIAN_POINT('Ctrl Pts',(-4.59168429755987,1.3,6.94283346090675));
#29105=CARTESIAN_POINT('Ctrl Pts',(-4.60900164344958,1.3,6.94788682421139));
#29106=CARTESIAN_POINT('Ctrl Pts',(-4.62336514575569,1.3,6.95199202349994));
#29107=CARTESIAN_POINT('Ctrl Pts',(-4.64347549796415,1.3,6.95933528312236));
#29108=CARTESIAN_POINT('Ctrl Pts',(-4.67210160956593,1.3,6.96965511487844));
#29109=CARTESIAN_POINT('Ctrl Pts',(-4.70071250038716,1.3,6.98017995874042));
#29110=CARTESIAN_POINT('Ctrl Pts',(-4.72629088154586,1.3,6.99118791773456));
#29111=CARTESIAN_POINT('Ctrl Pts',(-4.74340328278023,1.3,6.99781595031789));
#29112=CARTESIAN_POINT('Ctrl Pts',(-4.75756194704263,1.3,7.00427217122634));
#29113=CARTESIAN_POINT('Ctrl Pts',(-4.76891185654316,1.3,7.00917189133043));
#29114=CARTESIAN_POINT('Ctrl Pts',(-4.78583835543268,1.3,7.01735252591455));
#29115=CARTESIAN_POINT('Ctrl Pts',(-4.81137590685574,1.3,7.02815247242249));
#29116=CARTESIAN_POINT('Ctrl Pts',(-4.83462754895962,1.3,7.04033440400255));
#29117=CARTESIAN_POINT('Ctrl Pts',(-4.84672437123211,1.3,7.04622385103896));
#29118=CARTESIAN_POINT('Ctrl Pts',(-4.84757460701277,1.3,7.04663629403529));
#29119=CARTESIAN_POINT('',(-4.83514000566344,1.30000000008923,7.57936937611262));
#29120=CARTESIAN_POINT('Origin',(0.,1.3,7.2));
#29121=CARTESIAN_POINT('',(-4.55678639209675,1.3,7.66234429787488));
#29122=CARTESIAN_POINT('Ctrl Pts',(-4.83514000561781,1.3,7.57936937599151));
#29123=CARTESIAN_POINT('Ctrl Pts',(-4.83419097024645,1.3,7.57972696234589));
#29124=CARTESIAN_POINT('Ctrl Pts',(-4.83323821194189,1.3,7.58008513247196));
#29125=CARTESIAN_POINT('Ctrl Pts',(-4.83228194790045,1.3,7.58044402446448));
#29126=CARTESIAN_POINT('Ctrl Pts',(-4.82124539004742,1.3,7.58458611500299));
#29127=CARTESIAN_POINT('Ctrl Pts',(-4.80974201417162,1.3,7.58882670514177));
#29128=CARTESIAN_POINT('Ctrl Pts',(-4.79795307756342,1.3,7.59296283947731));
#29129=CARTESIAN_POINT('Ctrl Pts',(-4.79652635944612,1.3,7.59346340182557));
#29130=CARTESIAN_POINT('Ctrl Pts',(-4.79509548726416,1.3,7.59396253106982));
#29131=CARTESIAN_POINT('Ctrl Pts',(-4.7936535395449,1.3,7.59443920076872));
#29132=CARTESIAN_POINT('Ctrl Pts',(-4.78938085605041,1.3,7.59585163668968));
#29133=CARTESIAN_POINT('Ctrl Pts',(-4.78501089289788,1.3,7.59706283538183));
#29134=CARTESIAN_POINT('Ctrl Pts',(-4.78073579922085,1.3,7.5985929666076));
#29135=CARTESIAN_POINT('Ctrl Pts',(-4.77785428940659,1.3,7.59962430965578));
#29136=CARTESIAN_POINT('Ctrl Pts',(-4.77501388452526,1.3,7.60079734333637));
#29137=CARTESIAN_POINT('Ctrl Pts',(-4.77215073536344,1.3,7.60191808577717));
#29138=CARTESIAN_POINT('Ctrl Pts',(-4.77072659903648,1.3,7.60247554538996));
#29139=CARTESIAN_POINT('Ctrl Pts',(-4.769296968437,1.3,7.6030202762138));
#29140=CARTESIAN_POINT('Ctrl Pts',(-4.76785580911974,1.3,7.60353277750965));
#29141=CARTESIAN_POINT('Ctrl Pts',(-4.76642912909357,1.3,7.60404012971798));
#29142=CARTESIAN_POINT('Ctrl Pts',(-4.76499106435748,1.3,7.60451551720438));
#29143=CARTESIAN_POINT('Ctrl Pts',(-4.76355258318755,1.3,7.60498986104352));
#29144=CARTESIAN_POINT('Ctrl Pts',(-4.74038334903627,1.3,7.61262999127744));
#29145=CARTESIAN_POINT('Ctrl Pts',(-4.71743823325545,1.3,7.61992997683004));
#29146=CARTESIAN_POINT('Ctrl Pts',(-4.69454547239695,1.3,7.62649274471369));
#29147=CARTESIAN_POINT('Ctrl Pts',(-4.68209916288128,1.3,7.6300607827002));
#29148=CARTESIAN_POINT('Ctrl Pts',(-4.67003039171006,1.3,7.63333245595284));
#29149=CARTESIAN_POINT('Ctrl Pts',(-4.65995652632322,1.3,7.63618341831681));
#29150=CARTESIAN_POINT('Ctrl Pts',(-4.65313633315566,1.3,7.6381135725614));
#29151=CARTESIAN_POINT('Ctrl Pts',(-4.64721746850589,1.3,7.63980698908736));
#29152=CARTESIAN_POINT('Ctrl Pts',(-4.64265064572876,1.3,7.64103597342789));
#29153=CARTESIAN_POINT('Ctrl Pts',(-4.63895509819979,1.3,7.6420304876152));
#29154=CARTESIAN_POINT('Ctrl Pts',(-4.63651780229139,1.3,7.64264706904322));
#29155=CARTESIAN_POINT('Ctrl Pts',(-4.63398843337283,1.3,7.64325317280513));
#29156=CARTESIAN_POINT('Ctrl Pts',(-4.63111165446774,1.3,7.64394252519803));
#29157=CARTESIAN_POINT('Ctrl Pts',(-4.62821644281675,1.3,7.64457987313622));
#29158=CARTESIAN_POINT('Ctrl Pts',(-4.62533042545875,1.3,7.64523212643175));
#29159=CARTESIAN_POINT('Ctrl Pts',(-4.61948156938312,1.3,7.64655399500605));
#29160=CARTESIAN_POINT('Ctrl Pts',(-4.6136656043277,1.3,7.64793750472749));
#29161=CARTESIAN_POINT('Ctrl Pts',(-4.60797408626637,1.3,7.64926722192711));
#29162=CARTESIAN_POINT('Ctrl Pts',(-4.60203015483469,1.3,7.65065591080993));
#29163=CARTESIAN_POINT('Ctrl Pts',(-4.59622578392498,1.3,7.65198073034883));
#29164=CARTESIAN_POINT('Ctrl Pts',(-4.59066919321539,1.3,7.65310460254942));
#29165=CARTESIAN_POINT('Ctrl Pts',(-4.58768770325936,1.3,7.65370763664947));
#29166=CARTESIAN_POINT('Ctrl Pts',(-4.58477730158393,1.3,7.65425612837712));
#29167=CARTESIAN_POINT('Ctrl Pts',(-4.58196278725844,1.3,7.65479373462267));
#29168=CARTESIAN_POINT('Ctrl Pts',(-4.57189339261782,1.3,7.65671711067325));
#29169=CARTESIAN_POINT('Ctrl Pts',(-4.56309464195952,1.3,7.65889637743072));
#29170=CARTESIAN_POINT('Ctrl Pts',(-4.55678639209676,1.3,7.66234429787489));
#29171=CARTESIAN_POINT('',(-4.52769759742429,1.3,7.89131116337361));
#29172=CARTESIAN_POINT('',(-4.55678639209675,1.3,7.66234429787488));
#29173=CARTESIAN_POINT('',(-4.77350315750453,1.30000000000009,8.05800210098462));
#29174=CARTESIAN_POINT('Ctrl Pts',(-4.52769759742429,1.3,7.89131116337361));
#29175=CARTESIAN_POINT('Ctrl Pts',(-4.53392313647801,1.3,7.8974622258435));
#29176=CARTESIAN_POINT('Ctrl Pts',(-4.54481935244901,1.30000000000001,7.90309006287113));
#29177=CARTESIAN_POINT('Ctrl Pts',(-4.56073685668485,1.30000000000002,7.91153981038679));
#29178=CARTESIAN_POINT('Ctrl Pts',(-4.57387095253533,1.30000000000002,7.91873059084141));
#29179=CARTESIAN_POINT('Ctrl Pts',(-4.58959025693521,1.30000000000004,7.927944597891));
#29180=CARTESIAN_POINT('Ctrl Pts',(-4.60482087637025,1.30000000000004,7.93850976730446));
#29181=CARTESIAN_POINT('Ctrl Pts',(-4.62584154984425,1.30000000000006,7.95030089779444));
#29182=CARTESIAN_POINT('Ctrl Pts',(-4.65100328639092,1.30000000000009,7.96856552395811));
#29183=CARTESIAN_POINT('Ctrl Pts',(-4.68168781869127,1.30000000000013,7.98876229901975));
#29184=CARTESIAN_POINT('Ctrl Pts',(-4.70425849103461,1.30000000000015,8.00522489773813));
#29185=CARTESIAN_POINT('Ctrl Pts',(-4.71912910902609,1.30000000000016,8.0166759369683));
#29186=CARTESIAN_POINT('Ctrl Pts',(-4.72919200083095,1.30000000000016,8.02385128590682));
#29187=CARTESIAN_POINT('Ctrl Pts',(-4.74174314804138,1.30000000000018,8.03287907296244));
#29188=CARTESIAN_POINT('Ctrl Pts',(-4.75647533498549,1.3000000000002,8.04467732548915));
#29189=CARTESIAN_POINT('Ctrl Pts',(-4.76705952279732,1.30000000000021,8.05301621943483));
#29190=CARTESIAN_POINT('Ctrl Pts',(-4.77275066854619,1.30000000000022,8.05742047528334));
#29191=CARTESIAN_POINT('Ctrl Pts',(-4.77350315748042,1.30000000000022,8.05800210096597));
#29192=CARTESIAN_POINT('',(-4.65061125535824,1.29999999999665,8.57625414053201));
#29193=CARTESIAN_POINT('Origin',(0.,1.3,7.2));
#29194=CARTESIAN_POINT('',(-4.36108289177478,1.3,8.59965012915547));
#29195=CARTESIAN_POINT('Ctrl Pts',(-4.65058430230005,1.3,8.57625821131574));
#29196=CARTESIAN_POINT('Ctrl Pts',(-4.6495875835157,1.3,8.57640874172956));
#29197=CARTESIAN_POINT('Ctrl Pts',(-4.6485907689512,1.3,8.57655893939737));
#29198=CARTESIAN_POINT('Ctrl Pts',(-4.6475939573955,1.3,8.57670945662017));
#29199=CARTESIAN_POINT('Ctrl Pts',(-4.6355533009042,1.3,8.57852757978046));
#29200=CARTESIAN_POINT('Ctrl Pts',(-4.6235110513442,1.3,8.58039535440588));
#29201=CARTESIAN_POINT('Ctrl Pts',(-4.61140829826703,1.3,8.58183234538072));
#29202=CARTESIAN_POINT('Ctrl Pts',(-4.60539370804484,1.3,8.58254647313426));
#29203=CARTESIAN_POINT('Ctrl Pts',(-4.59936562178916,1.3,8.58315349116365));
#29204=CARTESIAN_POINT('Ctrl Pts',(-4.59336338090833,1.3,8.58396597893305));
#29205=CARTESIAN_POINT('Ctrl Pts',(-4.58732043535485,1.3,8.5847839766527));
#29206=CARTESIAN_POINT('Ctrl Pts',(-4.58130099734447,1.3,8.58580835441553));
#29207=CARTESIAN_POINT('Ctrl Pts',(-4.57524472399301,1.3,8.58653298671471));
#29208=CARTESIAN_POINT('Ctrl Pts',(-4.56925971555996,1.3,8.5872490921759));
#29209=CARTESIAN_POINT('Ctrl Pts',(-4.56324090758591,1.3,8.58766473828875));
#29210=CARTESIAN_POINT('Ctrl Pts',(-4.55724511852431,1.3,8.58827649344112));
#29211=CARTESIAN_POINT('Ctrl Pts',(-4.5512176382313,1.3,8.58889148207517));
#29212=CARTESIAN_POINT('Ctrl Pts',(-4.54521048860568,1.3,8.58970340650068));
#29213=CARTESIAN_POINT('Ctrl Pts',(-4.53918575032511,1.3,8.590349951669));
#29214=CARTESIAN_POINT('Ctrl Pts',(-4.52725372665985,1.3,8.59163043754072));
#29215=CARTESIAN_POINT('Ctrl Pts',(-4.51526184714999,1.3,8.59224977873498));
#29216=CARTESIAN_POINT('Ctrl Pts',(-4.5032919926851,1.3,8.59300958029857));
#29217=CARTESIAN_POINT('Ctrl Pts',(-4.49132452209666,1.3,8.5937692305426));
#29218=CARTESIAN_POINT('Ctrl Pts',(-4.47937209380073,1.3,8.59467395052153));
#29219=CARTESIAN_POINT('Ctrl Pts',(-4.46741124492339,1.3,8.59549545051039));
#29220=CARTESIAN_POINT('Ctrl Pts',(-4.46143603156469,1.3,8.59590584259527));
#29221=CARTESIAN_POINT('Ctrl Pts',(-4.45545887627245,1.3,8.596295629844));
#29222=CARTESIAN_POINT('Ctrl Pts',(-4.44947791681133,1.3,8.59660698982628));
#29223=CARTESIAN_POINT('Ctrl Pts',(-4.44650105055845,1.3,8.59676196111973));
#29224=CARTESIAN_POINT('Ctrl Pts',(-4.44352321944155,1.3,8.59689768988603));
#29225=CARTESIAN_POINT('Ctrl Pts',(-4.44054357105003,1.3,8.59697309156111));
#29226=CARTESIAN_POINT('Ctrl Pts',(-4.43758401047722,1.3,8.59704798490266));
#29227=CARTESIAN_POINT('Ctrl Pts',(-4.43462290252627,1.3,8.5970627433161));
#29228=CARTESIAN_POINT('Ctrl Pts',(-4.43166289976314,1.3,8.59709880909697));
#29229=CARTESIAN_POINT('Ctrl Pts',(-4.4258852251388,1.3,8.59716920644575));
#29230=CARTESIAN_POINT('Ctrl Pts',(-4.42019491457939,1.3,8.59732137622975));
#29231=CARTESIAN_POINT('Ctrl Pts',(-4.41384885731029,1.3,8.59744228461716));
#29232=CARTESIAN_POINT('Ctrl Pts',(-4.40828798224256,1.3,8.59754823330444));
#29233=CARTESIAN_POINT('Ctrl Pts',(-4.40235627801372,1.3,8.5976248940948));
#29234=CARTESIAN_POINT('Ctrl Pts',(-4.3961230007992,1.3,8.59759099519588));
#29235=CARTESIAN_POINT('Ctrl Pts',(-4.39315805428831,1.3,8.59757487070492));
#29236=CARTESIAN_POINT('Ctrl Pts',(-4.39009395819138,1.3,8.59753057587581));
#29237=CARTESIAN_POINT('Ctrl Pts',(-4.38726532243509,1.3,8.59746198288177));
#29238=CARTESIAN_POINT('Ctrl Pts',(-4.38411848835464,1.3,8.59738567373845));
#29239=CARTESIAN_POINT('Ctrl Pts',(-4.38116136924875,1.3,8.59728836610966));
#29240=CARTESIAN_POINT('Ctrl Pts',(-4.37832669149765,1.3,8.59732091390751));
#29241=CARTESIAN_POINT('Ctrl Pts',(-4.3722147640682,1.3,8.59739109111845));
#29242=CARTESIAN_POINT('Ctrl Pts',(-4.36669022745341,1.3,8.59797213156775));
#29243=CARTESIAN_POINT('Ctrl Pts',(-4.36108289177478,1.3,8.59965012915547));
#29244=CARTESIAN_POINT('',(-4.28502486891058,1.3,8.81756561880638));
#29245=CARTESIAN_POINT('',(-4.36108289177478,1.3,8.59965012915547));
#29246=CARTESIAN_POINT('',(-4.49082727704381,1.29999999999945,9.03165781950697));
#29247=CARTESIAN_POINT('Ctrl Pts',(-4.28502486891058,1.3,8.81756561880638));
#29248=CARTESIAN_POINT('Ctrl Pts',(-4.2898354872008,1.3,8.8248766281542));
#29249=CARTESIAN_POINT('Ctrl Pts',(-4.29932549685833,1.29999999999993,8.83264384777641));
#29250=CARTESIAN_POINT('Ctrl Pts',(-4.31313904561508,1.29999999999991,8.84421728449725));
#29251=CARTESIAN_POINT('Ctrl Pts',(-4.32449237549068,1.29999999999986,8.8539796218888));
#29252=CARTESIAN_POINT('Ctrl Pts',(-4.33795366492192,1.29999999999982,8.86625855451921));
#29253=CARTESIAN_POINT('Ctrl Pts',(-4.35065688898753,1.29999999999975,8.87975609279067));
#29254=CARTESIAN_POINT('Ctrl Pts',(-4.36876695393333,1.29999999999971,8.89565957397917));
#29255=CARTESIAN_POINT('Ctrl Pts',(-4.38958862281826,1.29999999999944,8.91874421566872));
#29256=CARTESIAN_POINT('Ctrl Pts',(-4.41540753427271,1.29999999999926,8.94487233749321));
#29257=CARTESIAN_POINT('Ctrl Pts',(-4.43406590057313,1.29999999999911,8.96566151560513));
#29258=CARTESIAN_POINT('Ctrl Pts',(-4.44623256960715,1.29999999999905,8.97995099359928));
#29259=CARTESIAN_POINT('Ctrl Pts',(-4.45458379296231,1.29999999999901,8.98906155763134));
#29260=CARTESIAN_POINT('Ctrl Pts',(-4.46498628653592,1.29999999999898,9.00049726618221));
#29261=CARTESIAN_POINT('Ctrl Pts',(-4.47694277519802,1.29999999999885,9.01510154466921));
#29262=CARTESIAN_POINT('Ctrl Pts',(-4.48556751235134,1.29999999999877,9.02544344919194));
#29263=CARTESIAN_POINT('Ctrl Pts',(-4.49021466107917,1.29999999999873,9.03093465841783));
#29264=CARTESIAN_POINT('Ctrl Pts',(-4.4908272770097,1.29999999999872,9.03165781946676));
#29265=CARTESIAN_POINT('',(-4.26286793815783,1.30000000000209,9.51310547565977));
#29266=CARTESIAN_POINT('Origin',(0.,1.3,7.2));
#29267=CARTESIAN_POINT('',(-3.97477914228474,1.3,9.47578453352548));
#29268=CARTESIAN_POINT('Ctrl Pts',(-4.2628679381595,1.3,9.51310547563085));
#29269=CARTESIAN_POINT('Ctrl Pts',(-4.18712155066313,1.3,9.50872478499194));
#29270=CARTESIAN_POINT('Ctrl Pts',(-4.11130619555387,1.30000000000629,9.5009205299035));
#29271=CARTESIAN_POINT('Ctrl Pts',(-4.02380326491958,1.30000000000629,9.48408990538011));
#29272=CARTESIAN_POINT('Ctrl Pts',(-4.01872677589918,1.3000000000063,9.4833016605151));
#29273=CARTESIAN_POINT('Ctrl Pts',(-3.99411124458743,1.3000000000063,9.47759067102414));
#29274=CARTESIAN_POINT('Ctrl Pts',(-3.98430478699325,1.3,9.47500810534561));
#29275=CARTESIAN_POINT('Ctrl Pts',(-3.97477914228474,1.3,9.47578453352547));
#29276=CARTESIAN_POINT('',(-3.85507599179487,1.3,9.6731246947563));
#29277=CARTESIAN_POINT('',(-3.97477914228474,1.3,9.47578453352548));
#29278=CARTESIAN_POINT('',(-4.01176129273638,1.30000000000074,9.92548471807191));
#29279=CARTESIAN_POINT('Ctrl Pts',(-3.85507599179487,1.3,9.6731246947563));
#29280=CARTESIAN_POINT('Ctrl Pts',(-3.85719962541057,1.3,9.67855898144637));
#29281=CARTESIAN_POINT('Ctrl Pts',(-3.86187591307552,1.3,9.68616633802149));
#29282=CARTESIAN_POINT('Ctrl Pts',(-3.86961829094849,1.3,9.69559038157922));
#29283=CARTESIAN_POINT('Ctrl Pts',(-3.87691775533033,1.3,9.70509517032314));
#29284=CARTESIAN_POINT('Ctrl Pts',(-3.88601575983783,1.3,9.71700697516693));
#29285=CARTESIAN_POINT('Ctrl Pts',(-3.89402362564178,1.3,9.72807138563928));
#29286=CARTESIAN_POINT('Ctrl Pts',(-3.89895590723415,1.3,9.73584729023011));
#29287=CARTESIAN_POINT('Ctrl Pts',(-3.90225564380959,1.3,9.74103523695475));
#29288=CARTESIAN_POINT('Ctrl Pts',(-3.90808032589377,1.3,9.75005250397545));
#29289=CARTESIAN_POINT('Ctrl Pts',(-3.92066850316574,1.3,9.76696249005104));
#29290=CARTESIAN_POINT('Ctrl Pts',(-3.93465792264323,1.3,9.79123516446284));
#29291=CARTESIAN_POINT('Ctrl Pts',(-3.94790798782012,1.3,9.8118165641029));
#29292=CARTESIAN_POINT('Ctrl Pts',(-3.95754151618004,1.30000000000002,9.82759293428611));
#29293=CARTESIAN_POINT('Ctrl Pts',(-3.96543595276435,1.29999999999999,9.84087661025074));
#29294=CARTESIAN_POINT('Ctrl Pts',(-3.97449492745696,1.3,9.8572589811272));
#29295=CARTESIAN_POINT('Ctrl Pts',(-3.98377635983763,1.3,9.87337467813515));
#29296=CARTESIAN_POINT('Ctrl Pts',(-3.99612389890649,1.30000000000002,9.89487963847089));
#29297=CARTESIAN_POINT('Ctrl Pts',(-4.00523044215879,1.30000000000001,9.91248203324778));
#29298=CARTESIAN_POINT('Ctrl Pts',(-4.01132444103615,1.30000000000001,9.92462053118691));
#29299=CARTESIAN_POINT('Ctrl Pts',(-4.01176063670267,1.30000000000001,9.92548407605884));
#29300=CARTESIAN_POINT('',(-3.68879127699578,1.3000000000002,10.3488599388502));
#29301=CARTESIAN_POINT('Origin',(0.,1.3,7.2));
#29302=CARTESIAN_POINT('',(-3.4147584711704,1.3,10.2524562333546));
#29303=CARTESIAN_POINT('Ctrl Pts',(-3.68879127700292,1.3,10.3488599388241));
#29304=CARTESIAN_POINT('Ctrl Pts',(-3.61561107823774,1.3,10.3288266201356));
#29305=CARTESIAN_POINT('Ctrl Pts',(-3.5430756359792,1.30000000000053,10.3054288287531));
#29306=CARTESIAN_POINT('Ctrl Pts',(-3.46098540050118,1.30000000000053,10.270773167704));
#29307=CARTESIAN_POINT('Ctrl Pts',(-3.45618327613316,1.30000000000052,10.2689465255546));
#29308=CARTESIAN_POINT('Ctrl Pts',(-3.43329266685346,1.30000000000052,10.2582422684741));
#29309=CARTESIAN_POINT('Ctrl Pts',(-3.42423747329421,1.3,10.2536772761121));
#29310=CARTESIAN_POINT('Ctrl Pts',(-3.4147584711704,1.3,10.2524562333546));
#29311=CARTESIAN_POINT('',(-3.25664179513071,1.3,10.4205963541764));
#29312=CARTESIAN_POINT('',(-3.4147584711704,1.3,10.2524562333546));
#29313=CARTESIAN_POINT('',(-3.35750281628615,1.30000000000089,10.6999535480671));
#29314=CARTESIAN_POINT('Ctrl Pts',(-3.25664179513071,1.3,10.4205963541764));
#29315=CARTESIAN_POINT('Ctrl Pts',(-3.25806285821861,1.3,10.4292319482914));
#29316=CARTESIAN_POINT('Ctrl Pts',(-3.26356414651618,1.30000000000008,10.4401950374537));
#29317=CARTESIAN_POINT('Ctrl Pts',(-3.27146918596613,1.30000000000012,10.4563930038539));
#29318=CARTESIAN_POINT('Ctrl Pts',(-3.27787351976156,1.30000000000018,10.4699243752486));
#29319=CARTESIAN_POINT('Ctrl Pts',(-3.2851479844364,1.30000000000024,10.486646198898));
#29320=CARTESIAN_POINT('Ctrl Pts',(-3.29130852430374,1.30000000000035,10.5040919019837));
#29321=CARTESIAN_POINT('Ctrl Pts',(-3.30114479310941,1.30000000000045,10.5261721228317));
#29322=CARTESIAN_POINT('Ctrl Pts',(-3.31534105722496,1.30000000000063,10.5670370259464));
#29323=CARTESIAN_POINT('Ctrl Pts',(-3.33189443614984,1.30000000000123,10.6133610002865));
#29324=CARTESIAN_POINT('Ctrl Pts',(-3.34316994757927,1.30000000000171,10.649779142451));
#29325=CARTESIAN_POINT('Ctrl Pts',(-3.34713592831131,1.30000000000175,10.6632708594138));
#29326=CARTESIAN_POINT('Ctrl Pts',(-3.34797075229533,1.30000000000177,10.6663022138394));
#29327=CARTESIAN_POINT('Ctrl Pts',(-3.34938363968462,1.30000000000175,10.6716401187348));
#29328=CARTESIAN_POINT('Ctrl Pts',(-3.35249794888383,1.30000000000182,10.6821059278266));
#29329=CARTESIAN_POINT('Ctrl Pts',(-3.35524625903208,1.30000000000193,10.6921138091528));
#29330=CARTESIAN_POINT('Ctrl Pts',(-3.35723820844024,1.30000000000204,10.6990377857127));
#29331=CARTESIAN_POINT('Ctrl Pts',(-3.35750281627144,1.30000000000205,10.699953548016));
#29332=CARTESIAN_POINT('',(-2.95338171769359,1.3,11.0470815470423));
#29333=CARTESIAN_POINT('Origin',(0.,1.3,7.2));
#29334=CARTESIAN_POINT('',(-2.70549646903679,1.3,10.8957209484761));
#29335=CARTESIAN_POINT('Ctrl Pts',(-2.95338171769359,1.3,11.0470815470423));
#29336=CARTESIAN_POINT('Ctrl Pts',(-2.95247588339834,1.3,11.0466168870669));
#29337=CARTESIAN_POINT('Ctrl Pts',(-2.95157040531699,1.3,11.0461514383438));
#29338=CARTESIAN_POINT('Ctrl Pts',(-2.95066525202913,1.3,11.0456852690531));
#29339=CARTESIAN_POINT('Ctrl Pts',(-2.93984365977446,1.3,11.0401119655544));
#29340=CARTESIAN_POINT('Ctrl Pts',(-2.92906721124797,1.3,11.0344361051911));
#29341=CARTESIAN_POINT('Ctrl Pts',(-2.9184176123353,1.3,11.028522211404));
#29342=CARTESIAN_POINT('Ctrl Pts',(-2.91577535418661,1.3,11.0270549229007));
#29343=CARTESIAN_POINT('Ctrl Pts',(-2.91314085605255,1.3,11.0255730743499));
#29344=CARTESIAN_POINT('Ctrl Pts',(-2.91053216609454,1.3,11.0240442761547));
#29345=CARTESIAN_POINT('Ctrl Pts',(-2.90792830457153,1.3,11.0225183076183));
#29346=CARTESIAN_POINT('Ctrl Pts',(-2.9053500848189,1.3,11.0209465056074));
#29347=CARTESIAN_POINT('Ctrl Pts',(-2.90269735027348,1.3,11.0195104701681));
#29348=CARTESIAN_POINT('Ctrl Pts',(-2.90000088688124,1.3,11.0180507624869));
#29349=CARTESIAN_POINT('Ctrl Pts',(-2.89722916133843,1.3,11.0167267722398));
#29350=CARTESIAN_POINT('Ctrl Pts',(-2.89448316298046,1.3,11.0153542728071));
#29351=CARTESIAN_POINT('Ctrl Pts',(-2.89311426908746,1.3,11.0146700749867));
#29352=CARTESIAN_POINT('Ctrl Pts',(-2.8917516247831,1.3,11.0139742120426));
#29353=CARTESIAN_POINT('Ctrl Pts',(-2.89040783878869,1.3,11.0132444682025));
#29354=CARTESIAN_POINT('Ctrl Pts',(-2.88907825445049,1.3,11.012522436581));
#29355=CARTESIAN_POINT('Ctrl Pts',(-2.88776741760646,1.3,11.0117668298678));
#29356=CARTESIAN_POINT('Ctrl Pts',(-2.88645763555239,1.3,11.0110094722585));
#29357=CARTESIAN_POINT('Ctrl Pts',(-2.88123035456337,1.3,11.0079868922648));
#29358=CARTESIAN_POINT('Ctrl Pts',(-2.87601819521636,1.3,11.0049389767175));
#29359=CARTESIAN_POINT('Ctrl Pts',(-2.87078275582546,1.3,11.001931888515));
#29360=CARTESIAN_POINT('Ctrl Pts',(-2.86554067077328,1.3,10.9989209832329));
#29361=CARTESIAN_POINT('Ctrl Pts',(-2.86027458446436,1.3,10.9959506173958));
#29362=CARTESIAN_POINT('Ctrl Pts',(-2.85505801286341,1.3,10.992895365571));
#29363=CARTESIAN_POINT('Ctrl Pts',(-2.84469787685817,1.3,10.9868276209185));
#29364=CARTESIAN_POINT('Ctrl Pts',(-2.83453960901062,1.3,10.9804234935907));
#29365=CARTESIAN_POINT('Ctrl Pts',(-2.82438475466521,1.3,10.9740270330777));
#29366=CARTESIAN_POINT('Ctrl Pts',(-2.81424599834958,1.3,10.9676407125833));
#29367=CARTESIAN_POINT('Ctrl Pts',(-2.80410721467228,1.3,10.9612621771574));
#29368=CARTESIAN_POINT('Ctrl Pts',(-2.79396737066265,1.3,10.9548814931131));
#29369=CARTESIAN_POINT('Ctrl Pts',(-2.78889889682822,1.3,10.9516920623789));
#29370=CARTESIAN_POINT('Ctrl Pts',(-2.78382980480467,1.3,10.9485020149995));
#29371=CARTESIAN_POINT('Ctrl Pts',(-2.77880393234839,1.3,10.945245998842));
#29372=CARTESIAN_POINT('Ctrl Pts',(-2.77630166727939,1.3,10.9436249040836));
#29373=CARTESIAN_POINT('Ctrl Pts',(-2.77381000561899,1.3,10.9419876101408));
#29374=CARTESIAN_POINT('Ctrl Pts',(-2.77135220271479,1.3,10.9403007518256));
#29375=CARTESIAN_POINT('Ctrl Pts',(-2.76891140135738,1.3,10.9386255621437));
#29376=CARTESIAN_POINT('Ctrl Pts',(-2.76650454967012,1.3,10.9369011054413));
#29377=CARTESIAN_POINT('Ctrl Pts',(-2.76408805554562,1.3,10.9351916308035));
#29378=CARTESIAN_POINT('Ctrl Pts',(-2.75866098844093,1.3,10.9313524186659));
#29379=CARTESIAN_POINT('Ctrl Pts',(-2.75323113168416,1.3,10.9276119632866));
#29380=CARTESIAN_POINT('Ctrl Pts',(-2.74947315280486,1.3,10.9249974102865));
#29381=CARTESIAN_POINT('Ctrl Pts',(-2.74422322745703,1.3,10.9213448596709));
#29382=CARTESIAN_POINT('Ctrl Pts',(-2.740751784517,1.3,10.9189437652169));
#29383=CARTESIAN_POINT('Ctrl Pts',(-2.73504020153367,1.3,10.9147088809601));
#29384=CARTESIAN_POINT('Ctrl Pts',(-2.73289496744276,1.3,10.9131182854797));
#29385=CARTESIAN_POINT('Ctrl Pts',(-2.73032184179771,1.3,10.9111628383304));
#29386=CARTESIAN_POINT('Ctrl Pts',(-2.72795814059379,1.3,10.9093707518815));
#29387=CARTESIAN_POINT('Ctrl Pts',(-2.720208752911,1.3,10.9034954015496));
#29388=CARTESIAN_POINT('Ctrl Pts',(-2.71325047752261,1.3,10.8984424674216));
#29389=CARTESIAN_POINT('Ctrl Pts',(-2.70549646903679,1.3,10.8957209484761));
#29390=CARTESIAN_POINT('',(-2.5158767249182,1.3,11.0273124987831));
#29391=CARTESIAN_POINT('',(-2.70549646903679,1.3,10.8957209484761));
#29392=CARTESIAN_POINT('',(-2.55655914734361,1.30000000000023,11.321468831149));
#29393=CARTESIAN_POINT('Ctrl Pts',(-2.5158767249182,1.3,11.0273124987831));
#29394=CARTESIAN_POINT('Ctrl Pts',(-2.51547129339445,1.3,11.036054840077));
#29395=CARTESIAN_POINT('Ctrl Pts',(-2.51859198142745,1.30000000000003,11.0479128654031));
#29396=CARTESIAN_POINT('Ctrl Pts',(-2.52296758356098,1.30000000000005,11.0653939986377));
#29397=CARTESIAN_POINT('Ctrl Pts',(-2.5264203539551,1.30000000000005,11.079962490987));
#29398=CARTESIAN_POINT('Ctrl Pts',(-2.53009803158022,1.30000000000008,11.0978064517128));
#29399=CARTESIAN_POINT('Ctrl Pts',(-2.53245235259751,1.30000000000011,11.116187731106));
#29400=CARTESIAN_POINT('Ctrl Pts',(-2.53775258378681,1.30000000000011,11.1397002573066));
#29401=CARTESIAN_POINT('Ctrl Pts',(-2.54008393448627,1.30000000000022,11.1613216668819));
#29402=CARTESIAN_POINT('Ctrl Pts',(-2.54332335680958,1.30000000000025,11.1857521422222));
#29403=CARTESIAN_POINT('Ctrl Pts',(-2.5469023959529,1.30000000000031,11.2100104540124));
#29404=CARTESIAN_POINT('Ctrl Pts',(-2.54938896734332,1.30000000000036,11.2347401697883));
#29405=CARTESIAN_POINT('Ctrl Pts',(-2.55085790609064,1.30000000000038,11.2534406531382));
#29406=CARTESIAN_POINT('Ctrl Pts',(-2.55225517129,1.3000000000004,11.2657217926828));
#29407=CARTESIAN_POINT('Ctrl Pts',(-2.55395665763029,1.30000000000042,11.2810845819828));
#29408=CARTESIAN_POINT('Ctrl Pts',(-2.55505077960984,1.30000000000047,11.2999252661264));
#29409=CARTESIAN_POINT('Ctrl Pts',(-2.55595402588115,1.30000000000049,11.3133566528398));
#29410=CARTESIAN_POINT('Ctrl Pts',(-2.55648845398831,1.30000000000052,11.3205266804514));
#29411=CARTESIAN_POINT('Ctrl Pts',(-2.5565591473374,1.30000000000052,11.3214688310659));
#29412=CARTESIAN_POINT('',(-2.08914039445814,1.29999999999929,11.5769470743903));
#29413=CARTESIAN_POINT('Origin',(0.,1.3,7.2));
#29414=CARTESIAN_POINT('',(-1.87799128879385,1.3,11.3774649241125));
#29415=CARTESIAN_POINT('Ctrl Pts',(-2.08911157607092,1.3,11.5769235068739));
#29416=CARTESIAN_POINT('Ctrl Pts',(-2.03039281675241,1.3,11.5289034585235));
#29417=CARTESIAN_POINT('Ctrl Pts',(-1.97366330051107,1.30000000000335,11.4780295569611));
#29418=CARTESIAN_POINT('Ctrl Pts',(-1.91186458013702,1.30000000000335,11.4120146246155));
#29419=CARTESIAN_POINT('Ctrl Pts',(-1.90903631482672,1.30000000000332,11.4092617389519));
#29420=CARTESIAN_POINT('Ctrl Pts',(-1.8926160488693,1.30000000000332,11.390333398815));
#29421=CARTESIAN_POINT('Ctrl Pts',(-1.88617869194126,1.3,11.3824508078545));
#29422=CARTESIAN_POINT('Ctrl Pts',(-1.87799128879385,1.3,11.3774649241125));
#29423=CARTESIAN_POINT('',(-1.66515576931083,1.3,11.46675672171));
#29424=CARTESIAN_POINT('',(-1.87799128879385,1.3,11.3774649241125));
#29425=CARTESIAN_POINT('',(-1.64379217587214,1.29999999999984,11.7629428313909));
#29426=CARTESIAN_POINT('Ctrl Pts',(-1.66515576931083,1.3,11.46675672171));
#29427=CARTESIAN_POINT('Ctrl Pts',(-1.6629415624785,1.3,11.4752237279177));
#29428=CARTESIAN_POINT('Ctrl Pts',(-1.66352894105859,1.29999999999999,11.4874714735657));
#29429=CARTESIAN_POINT('Ctrl Pts',(-1.66417447630822,1.29999999999996,11.5054803428951));
#29430=CARTESIAN_POINT('Ctrl Pts',(-1.66452301405315,1.29999999999996,11.5204483587987));
#29431=CARTESIAN_POINT('Ctrl Pts',(-1.66441047704251,1.29999999999995,11.5386670191183));
#29432=CARTESIAN_POINT('Ctrl Pts',(-1.66289185486147,1.29999999999991,11.5571361197397));
#29433=CARTESIAN_POINT('Ctrl Pts',(-1.66318775374981,1.29999999999991,11.5812368181191));
#29434=CARTESIAN_POINT('Ctrl Pts',(-1.66097302460095,1.29999999999983,11.6028704763946));
#29435=CARTESIAN_POINT('Ctrl Pts',(-1.65906230940226,1.29999999999982,11.6274406048554));
#29436=CARTESIAN_POINT('Ctrl Pts',(-1.65751962363572,1.29999999999978,11.6519129358666));
#29437=CARTESIAN_POINT('Ctrl Pts',(-1.65481031308637,1.29999999999973,11.6766192287848));
#29438=CARTESIAN_POINT('Ctrl Pts',(-1.65235914007452,1.29999999999972,11.6952164665527));
#29439=CARTESIAN_POINT('Ctrl Pts',(-1.6511724890373,1.29999999999972,11.7075197398047));
#29440=CARTESIAN_POINT('Ctrl Pts',(-1.6496427241954,1.29999999999968,11.7229005682395));
#29441=CARTESIAN_POINT('Ctrl Pts',(-1.64679579483565,1.29999999999966,11.7415570091161));
#29442=CARTESIAN_POINT('Ctrl Pts',(-1.64488682205169,1.29999999999964,11.7548824893073));
#29443=CARTESIAN_POINT('Ctrl Pts',(-1.64391888364001,1.29999999999962,11.7620067583755));
#29444=CARTESIAN_POINT('Ctrl Pts',(-1.64379217588362,1.29999999999962,11.7629428313061));
#29445=CARTESIAN_POINT('Origin',(0.,1.3,7.2));
#29446=CARTESIAN_POINT('Ctrl Pts',(-0.815761714370199,-1.30000000001152,
12.1782561896344));
#29447=CARTESIAN_POINT('Ctrl Pts',(-0.774949037065984,-1.18514270861958,
12.1904765350853));
#29448=CARTESIAN_POINT('Ctrl Pts',(-0.740987950522033,-1.06847604194908,
12.1899531249505));
#29449=CARTESIAN_POINT('Ctrl Pts',(-0.678359592026837,-0.794772684000851,
12.1593033180494));
#29450=CARTESIAN_POINT('Ctrl Pts',(-0.662111769290086,-0.636309800095197,
12.0912247185297));
#29451=CARTESIAN_POINT('Ctrl Pts',(-0.623796234000798,-0.319434907277159,
12.0277447643888));
#29452=CARTESIAN_POINT('Ctrl Pts',(-0.614857791974962,-0.158333333333332,
11.9827589718232));
#29453=CARTESIAN_POINT('Ctrl Pts',(-0.581221077760458,0.158333333333334,
11.9868187308147));
#29454=CARTESIAN_POINT('Ctrl Pts',(-0.55498717214331,0.319434907277167,
12.0359668790066));
#29455=CARTESIAN_POINT('Ctrl Pts',(-0.527915117225984,0.636309800095206,
12.1075072879431));
#29456=CARTESIAN_POINT('Ctrl Pts',(-0.508441992410805,0.79477268400084,
12.1792483945391));
#29457=CARTESIAN_POINT('Ctrl Pts',(-0.5254047727039,1.06847604194527,12.2173269808048));
#29458=CARTESIAN_POINT('Ctrl Pts',(-0.542940786614001,1.1851427086121,12.2211942845391));
#29459=CARTESIAN_POINT('Ctrl Pts',(-0.570670255378274,1.30000000000048,
12.2124460829639));
#29460=CARTESIAN_POINT('Ctrl Pts',(-0.82013686250475,-1.30000000001152,
12.1665018705585));
#29461=CARTESIAN_POINT('Ctrl Pts',(-0.780090946642151,-1.18514270861958,
12.1764721061336));
#29462=CARTESIAN_POINT('Ctrl Pts',(-0.746715246716433,-1.06847604194908,
12.1743051424724));
#29463=CARTESIAN_POINT('Ctrl Pts',(-0.685020236289605,-0.794772684000851,
12.141259664642));
#29464=CARTESIAN_POINT('Ctrl Pts',(-0.66882498757232,-0.636309800095197,
12.0736176643627));
#29465=CARTESIAN_POINT('Ctrl Pts',(-0.630650969306314,-0.319434907277159,
12.0100782700739));
#29466=CARTESIAN_POINT('Ctrl Pts',(-0.621210414483327,-0.158333333333332,
11.9658130254479));
#29467=CARTESIAN_POINT('Ctrl Pts',(-0.588041432022333,0.158333333333334,
11.9699175322922));
#29468=CARTESIAN_POINT('Ctrl Pts',(-0.562926419586644,0.319434907277167,
12.0183993675339));
#29469=CARTESIAN_POINT('Ctrl Pts',(-0.53636198222106,0.636309800095206,
12.0900710401584));
#29470=CARTESIAN_POINT('Ctrl Pts',(-0.517059899028168,0.79477268400084,
12.161414267525));
#29471=CARTESIAN_POINT('Ctrl Pts',(-0.533012642916803,1.06847604194527,
12.2018952309815));
#29472=CARTESIAN_POINT('Ctrl Pts',(-0.54980559533789,1.1851427086121,12.2073958498195));
#29473=CARTESIAN_POINT('Ctrl Pts',(-0.576486148458089,1.30000000000048,
12.2008743783825));
#29474=CARTESIAN_POINT('Ctrl Pts',(-0.828301885813206,-1.3000000000115,
12.1430419168349));
#29475=CARTESIAN_POINT('Ctrl Pts',(-0.791470154233991,-1.18514270861957,
12.148526329752));
#29476=CARTESIAN_POINT('Ctrl Pts',(-0.760221087829436,-1.06847604194906,
12.1430741928524));
#29477=CARTESIAN_POINT('Ctrl Pts',(-0.700926566443512,-0.794772684000842,
12.1052130479931));
#29478=CARTESIAN_POINT('Ctrl Pts',(-0.682086780735323,-0.636309800095188,
12.0383657208095));
#29479=CARTESIAN_POINT('Ctrl Pts',(-0.643454278021432,-0.319434907277154,
11.9746814174566));
#29480=CARTESIAN_POINT('Ctrl Pts',(-0.634003199425879,-0.15833333333333,
11.9319085201582));
#29481=CARTESIAN_POINT('Ctrl Pts',(-0.601473370738099,0.158333333333332,
11.9360713376515));
#29482=CARTESIAN_POINT('Ctrl Pts',(-0.57745577938292,0.319434907277162,
11.9831275324594));
#29483=CARTESIAN_POINT('Ctrl Pts',(-0.551739715339017,0.636309800095197,
12.0550457861955));
#29484=CARTESIAN_POINT('Ctrl Pts',(-0.533839936831245,0.794772684000831,
12.1256672596271));
#29485=CARTESIAN_POINT('Ctrl Pts',(-0.547735885685927,1.06847604194526,
12.1709700838584));
#29486=CARTESIAN_POINT('Ctrl Pts',(-0.562829352204696,1.18514270861208,
12.1797357114804));
#29487=CARTESIAN_POINT('Ctrl Pts',(-0.587001243878688,1.30000000000045,
12.1776570527497));
#29488=CARTESIAN_POINT('Ctrl Pts',(-0.836707147794769,-1.30000000001149,
12.1192702708369));
#29489=CARTESIAN_POINT('Ctrl Pts',(-0.80043188440398,-1.18514270861956,
12.1201835583254));
#29490=CARTESIAN_POINT('Ctrl Pts',(-0.769771336481297,-1.06847604194905,
12.1113955021284));
#29491=CARTESIAN_POINT('Ctrl Pts',(-0.711910453110691,-0.794772684000834,
12.068681289609));
#29492=CARTESIAN_POINT('Ctrl Pts',(-0.694489271114953,-0.636309800095183,
12.0027480164002));
#29493=CARTESIAN_POINT('Ctrl Pts',(-0.656588678792395,-0.319434907277153,
11.9389505469321));
#29494=CARTESIAN_POINT('Ctrl Pts',(-0.64612829689688,-0.158333333333329,
11.8976409947032));
#29495=CARTESIAN_POINT('Ctrl Pts',(-0.614289353194816,0.15833333333333,
11.9018599735325));
#29496=CARTESIAN_POINT('Ctrl Pts',(-0.591653888851498,0.319434907277157,
11.9474876088037));
#29497=CARTESIAN_POINT('Ctrl Pts',(-0.567261065300381,0.636309800095191,
12.0196769662247));
#29498=CARTESIAN_POINT('Ctrl Pts',(-0.551340534525828,0.794772684000825,
12.0895982646898));
#29499=CARTESIAN_POINT('Ctrl Pts',(-0.563310045646076,1.06847604194525,
12.139782144358));
#29500=CARTESIAN_POINT('Ctrl Pts',(-0.576630193529321,1.18514270861207,
12.1518448274832));
#29501=CARTESIAN_POINT('Ctrl Pts',(-0.598089331445952,1.30000000000045,
12.1542474517214));
#29502=CARTESIAN_POINT('Ctrl Pts',(-0.840896249733202,-1.30000000001149,
12.1071345222084));
#29503=CARTESIAN_POINT('Ctrl Pts',(-0.80590565072756,-1.18514270861955,
12.1057161795362));
#29504=CARTESIAN_POINT('Ctrl Pts',(-0.776118041671117,-1.06847604194905,
12.0952223523448));
#29505=CARTESIAN_POINT('Ctrl Pts',(-0.719322653398249,-0.794772684000831,
12.0500133274667));
#29506=CARTESIAN_POINT('Ctrl Pts',(-0.701147360363495,-0.636309800095182,
11.9845133106775));
#29507=CARTESIAN_POINT('Ctrl Pts',(-0.662937063965583,-0.319434907277152,
11.9206373392581));
#29508=CARTESIAN_POINT('Ctrl Pts',(-0.651850096865466,-0.158333333333328,
11.880076238071));
#29509=CARTESIAN_POINT('Ctrl Pts',(-0.620348320308299,0.15833333333333,
11.8843214312355));
#29510=CARTESIAN_POINT('Ctrl Pts',(-0.598936484134056,0.319434907277156,
11.929235417687));
#29511=CARTESIAN_POINT('Ctrl Pts',(-0.575010801522814,0.636309800095188,
12.0015391808645));
#29512=CARTESIAN_POINT('Ctrl Pts',(-0.559119512271139,0.794772684000824,
12.0710311232064));
#29513=CARTESIAN_POINT('Ctrl Pts',(-0.57010620639343,1.06847604194525,12.1237185482583));
#29514=CARTESIAN_POINT('Ctrl Pts',(-0.582732606004582,1.18514270861207,
12.1374883996074));
#29515=CARTESIAN_POINT('Ctrl Pts',(-0.60322967243848,1.30000000000044,12.1422216682623));
#29516=CARTESIAN_POINT('Ctrl Pts',(-0.84108366557138,-1.30000000001149,
12.106582879579));
#29517=CARTESIAN_POINT('Ctrl Pts',(-0.806151169153311,-1.18514270861955,
12.1050584818237));
#29518=CARTESIAN_POINT('Ctrl Pts',(-0.776403200212559,-1.06847604194905,
12.0944870720756));
#29519=CARTESIAN_POINT('Ctrl Pts',(-0.719656736533463,-0.794772684000831,
12.0491645932037));
#29520=CARTESIAN_POINT('Ctrl Pts',(-0.701449230989593,-0.636309800095182,
11.9836843524763));
#29521=CARTESIAN_POINT('Ctrl Pts',(-0.663224451229675,-0.319434907277152,
11.9198047781588));
#29522=CARTESIAN_POINT('Ctrl Pts',(-0.652106150378969,-0.158333333333328,
11.8792775941036));
#29523=CARTESIAN_POINT('Ctrl Pts',(-0.62061947737185,0.15833333333333,11.8835239547376));
#29524=CARTESIAN_POINT('Ctrl Pts',(-0.599265114264511,0.319434907277156,
11.9284055424065));
#29525=CARTESIAN_POINT('Ctrl Pts',(-0.575362200797949,0.636309800095188,
12.0007145718174));
#29526=CARTESIAN_POINT('Ctrl Pts',(-0.559473301158497,0.794772684000824,
12.07018707444));
#29527=CARTESIAN_POINT('Ctrl Pts',(-0.570415763160731,1.06847604194525,
12.1229883507983));
#29528=CARTESIAN_POINT('Ctrl Pts',(-0.583010559332848,1.18514270861207,
12.1368358144636));
#29529=CARTESIAN_POINT('Ctrl Pts',(-0.603463565334488,1.30000000000044,
12.1416750257389));
#29530=CARTESIAN_POINT('Ctrl Pts',(-0.841271106653579,-1.30000000001149,
12.1060312225867));
#29531=CARTESIAN_POINT('Ctrl Pts',(-0.806396138358098,-1.18514270861955,
12.1044007736908));
#29532=CARTESIAN_POINT('Ctrl Pts',(-0.776687427737685,-1.06847604194905,
12.0937517836326));
#29533=CARTESIAN_POINT('Ctrl Pts',(-0.719989451734108,-0.794772684000831,
12.0483158520383));
#29534=CARTESIAN_POINT('Ctrl Pts',(-0.701749841759635,-0.636309800095182,
11.9828553699663));
#29535=CARTESIAN_POINT('Ctrl Pts',(-0.66351134192088,-0.319434907277152,
11.9189722126188));
#29536=CARTESIAN_POINT('Ctrl Pts',(-0.652363265515954,-0.158333333333328,
11.8784790007643));
#29537=CARTESIAN_POINT('Ctrl Pts',(-0.620891783947901,0.15833333333333,
11.8827265264074));
#29538=CARTESIAN_POINT('Ctrl Pts',(-0.599593227881866,0.319434907277156,
11.9275756469084));
#29539=CARTESIAN_POINT('Ctrl Pts',(-0.575712897964395,0.636309800095188,
11.9998899397845));
#29540=CARTESIAN_POINT('Ctrl Pts',(-0.559827649734273,0.794772684000824,
12.06934306953));
#29541=CARTESIAN_POINT('Ctrl Pts',(-0.570726051352478,1.06847604194525,
12.1222582011948));
#29542=CARTESIAN_POINT('Ctrl Pts',(-0.583289129579976,1.18514270861207,
12.1361832670831));
#29543=CARTESIAN_POINT('Ctrl Pts',(-0.603697771800025,1.30000000000044,
12.141128399061));
#29544=CARTESIAN_POINT('Ctrl Pts',(-0.8416433382849,-1.30000000001149,12.1049278686445));
#29545=CARTESIAN_POINT('Ctrl Pts',(-0.806882159906077,-1.18514270861955,
12.1030852573022));
#29546=CARTESIAN_POINT('Ctrl Pts',(-0.777251289156161,-1.06847604194905,
12.0922810672687));
#29547=CARTESIAN_POINT('Ctrl Pts',(-0.720650087026833,-0.794772684000831,
12.0466181873869));
#29548=CARTESIAN_POINT('Ctrl Pts',(-0.702348630569117,-0.636309800095182,
11.981197280085));
#29549=CARTESIAN_POINT('Ctrl Pts',(-0.66408356520117,-0.319434907277152,
11.9173069588674));
#29550=CARTESIAN_POINT('Ctrl Pts',(-0.652875601867588,-0.158333333333328,
11.8768816785607));
#29551=CARTESIAN_POINT('Ctrl Pts',(-0.621434367058539,0.15833333333333,
11.8811315066939));
#29552=CARTESIAN_POINT('Ctrl Pts',(-0.600246478406182,0.319434907277156,
11.9259156187069));
#29553=CARTESIAN_POINT('Ctrl Pts',(-0.576412498766739,0.636309800095188,
11.998240501404));
#29554=CARTESIAN_POINT('Ctrl Pts',(-0.560537751889447,0.794772684000824,
12.0676550804845));
#29555=CARTESIAN_POINT('Ctrl Pts',(-0.571348643291286,1.06847604194525,
12.1207979754241));
#29556=CARTESIAN_POINT('Ctrl Pts',(-0.583847946343261,1.18514270861207,
12.1348782360536));
#29557=CARTESIAN_POINT('Ctrl Pts',(-0.604166918142359,1.30000000000044,
12.1400351672316));
#29558=CARTESIAN_POINT('Ctrl Pts',(-0.842440411811635,-1.30000000001149,
12.1025370321507));
#29559=CARTESIAN_POINT('Ctrl Pts',(-0.807917893314191,-1.18514270861955,
12.1002345213527));
#29560=CARTESIAN_POINT('Ctrl Pts',(-0.778451084354395,-1.06847604194905,
12.0890939250708));
#29561=CARTESIAN_POINT('Ctrl Pts',(-0.722056561266581,-0.794772684000831,
12.0429391734713));
#29562=CARTESIAN_POINT('Ctrl Pts',(-0.703631014770677,-0.636309800095182,
11.9776041650572));
#29563=CARTESIAN_POINT('Ctrl Pts',(-0.665315562999388,-0.319434907277152,
11.9136984391799));
#29564=CARTESIAN_POINT('Ctrl Pts',(-0.653984050577437,-0.158333333333328,
11.8734205623712));
#29565=CARTESIAN_POINT('Ctrl Pts',(-0.622608333470667,0.15833333333333,
11.8776752669074));
#29566=CARTESIAN_POINT('Ctrl Pts',(-0.60164873732673,0.319434907277157,
11.9223179126499));
#29567=CARTESIAN_POINT('Ctrl Pts',(-0.577918698969977,0.636309800095188,
11.9946659720654));
#29568=CARTESIAN_POINT('Ctrl Pts',(-0.562084540976334,0.794772684000824,
12.0639981026217));
#29569=CARTESIAN_POINT('Ctrl Pts',(-0.572709027367301,1.06847604194525,
12.1176347043536));
#29570=CARTESIAN_POINT('Ctrl Pts',(-0.58506843023964,1.18514270861207,12.13205113149));
#29571=CARTESIAN_POINT('Ctrl Pts',(-0.605188289501683,1.30000000000044,
12.1376666883049));
#29572=CARTESIAN_POINT('Ctrl Pts',(-0.8436279850576,-1.30000000001149,12.098857420753));
#29573=CARTESIAN_POINT('Ctrl Pts',(-0.8094239679675,-1.18514270861955,12.0958463896222));
#29574=CARTESIAN_POINT('Ctrl Pts',(-0.780181208795663,-1.06847604194905,
12.0841876400619));
#29575=CARTESIAN_POINT('Ctrl Pts',(-0.724086083403273,-0.794772684000831,
12.0372756367114));
#29576=CARTESIAN_POINT('Ctrl Pts',(-0.705529966296978,-0.636309800095182,
11.9720736371635));
#29577=CARTESIAN_POINT('Ctrl Pts',(-0.667182604758452,-0.319434907277152,
11.9081451757437));
#29578=CARTESIAN_POINT('Ctrl Pts',(-0.655703716817061,-0.158333333333328,
11.8680957195148));
#29579=CARTESIAN_POINT('Ctrl Pts',(-0.624426688156065,0.15833333333333,
11.872357314027));
#29580=CARTESIAN_POINT('Ctrl Pts',(-0.603741085139811,0.319434907277157,
11.9167783358466));
#29581=CARTESIAN_POINT('Ctrl Pts',(-0.580187088115549,0.636309800095188,
11.9891633552736));
#29582=CARTESIAN_POINT('Ctrl Pts',(-0.564525011791283,0.794772684000824,
12.0583754013928));
#29583=CARTESIAN_POINT('Ctrl Pts',(-0.574876802233916,1.06847604194525,
12.1127725326272));
#29584=CARTESIAN_POINT('Ctrl Pts',(-0.587007286654078,1.18514270861207,
12.1277053380453));
#29585=CARTESIAN_POINT('Ctrl Pts',(-0.606787348983421,1.30000000000044,
12.1340244463825));
#29586=CARTESIAN_POINT('Ctrl Pts',(-0.844998182644887,-1.30000000001148,
12.0944389846615));
#29587=CARTESIAN_POINT('Ctrl Pts',(-0.81108280355128,-1.18514270861955,
12.090576012288));
#29588=CARTESIAN_POINT('Ctrl Pts',(-0.782053207345806,-1.06847604194905,
12.0782944298942));
#29589=CARTESIAN_POINT('Ctrl Pts',(-0.726276168630486,-0.794772684000832,
12.0304728443595));
#29590=CARTESIAN_POINT('Ctrl Pts',(-0.707666075200391,-0.636309800095182,
11.9654317870864));
#29591=CARTESIAN_POINT('Ctrl Pts',(-0.669369958673357,-0.319434907277152,
11.9014782233589));
#29592=CARTESIAN_POINT('Ctrl Pts',(-0.65781344964472,-0.158333333333328,
11.8617068390375));
#29593=CARTESIAN_POINT('Ctrl Pts',(-0.626654186829892,0.15833333333333,
11.8659756293417));
#29594=CARTESIAN_POINT('Ctrl Pts',(-0.606142384063235,0.319434907277157,
11.9101225137041));
#29595=CARTESIAN_POINT('Ctrl Pts',(-0.582820993097351,0.636309800095189,
11.982553935868));
#29596=CARTESIAN_POINT('Ctrl Pts',(-0.567560619655728,0.794772684000824,
12.0516344476837));
#29597=CARTESIAN_POINT('Ctrl Pts',(-0.577613545939296,1.06847604194525,
12.1069460957049));
#29598=CARTESIAN_POINT('Ctrl Pts',(-0.589447841868061,1.18514270861207,
12.1224971408499));
#29599=CARTESIAN_POINT('Ctrl Pts',(-0.608764894435061,1.30000000000044,
12.1296568682101));
#29600=CARTESIAN_POINT('Ctrl Pts',(-0.846782212613889,-1.30000000001149,
12.0885449248653));
#29601=CARTESIAN_POINT('Ctrl Pts',(-0.813168584017232,-1.18514270861955,
12.0835445222219));
#29602=CARTESIAN_POINT('Ctrl Pts',(-0.784372570115393,-1.06847604194905,
12.0704315727545));
#29603=CARTESIAN_POINT('Ctrl Pts',(-0.728977671085883,-0.794772684000831,
12.0213964301765));
#29604=CARTESIAN_POINT('Ctrl Pts',(-0.710379940056297,-0.636309800095182,
11.9565711544317));
#29605=CARTESIAN_POINT('Ctrl Pts',(-0.672221392006236,-0.319434907277152,
11.8925859612815));
#29606=CARTESIAN_POINT('Ctrl Pts',(-0.660639528873272,-0.158333333333328,
11.8531887947527));
#29607=CARTESIAN_POINT('Ctrl Pts',(-0.629635528222297,0.15833333333333,
11.8574659748541));
#29608=CARTESIAN_POINT('Ctrl Pts',(-0.609228998788056,0.319434907277157,
11.9012398803746));
#29609=CARTESIAN_POINT('Ctrl Pts',(-0.586239765328994,0.636309800095188,
11.9737345871329));
#29610=CARTESIAN_POINT('Ctrl Pts',(-0.571684072982041,0.794772684000824,
12.0426503161413));
#29611=CARTESIAN_POINT('Ctrl Pts',(-0.581362316142963,1.06847604194525,
12.0991830970244));
#29612=CARTESIAN_POINT('Ctrl Pts',(-0.592782232184672,1.18514270861207,
12.1155574251084));
#29613=CARTESIAN_POINT('Ctrl Pts',(-0.611432711417976,1.30000000000044,
12.1238351351779));
#29614=CARTESIAN_POINT('Ctrl Pts',(-0.849022524491501,-1.30000000001149,
12.0811753213131));
#29615=CARTESIAN_POINT('Ctrl Pts',(-0.815790792839271,-1.18514270861955,
12.0747521792439));
#29616=CARTESIAN_POINT('Ctrl Pts',(-0.7872803364692,-1.06847604194905,12.0605992294231));
#29617=CARTESIAN_POINT('Ctrl Pts',(-0.732322569147779,-0.794772684000832,
12.0100456818012));
#29618=CARTESIAN_POINT('Ctrl Pts',(-0.713659524061526,-0.636309800095182,
11.9454896346112));
#29619=CARTESIAN_POINT('Ctrl Pts',(-0.675628672060576,-0.319434907277152,
11.881464252745));
#29620=CARTESIAN_POINT('Ctrl Pts',(-0.664012556063606,-0.158333333333328,
11.8425350941018));
#29621=CARTESIAN_POINT('Ctrl Pts',(-0.633230004184434,0.15833333333333,
11.8468222411214));
#29622=CARTESIAN_POINT('Ctrl Pts',(-0.613036617821267,0.319434907277157,
11.890130257037));
#29623=CARTESIAN_POINT('Ctrl Pts',(-0.590457452248467,0.636309800095189,
11.9627014415155));
#29624=CARTESIAN_POINT('Ctrl Pts',(-0.576648844760399,0.794772684000824,
12.0314043836306));
#29625=CARTESIAN_POINT('Ctrl Pts',(-0.585895284402455,1.06847604194525,
12.0894658356194));
#29626=CARTESIAN_POINT('Ctrl Pts',(-0.596847578942501,1.18514270861207,
12.1068723220005));
#29627=CARTESIAN_POINT('Ctrl Pts',(-0.614749726915899,1.30000000000044,
12.1165526435854));
#29628=CARTESIAN_POINT('Ctrl Pts',(-0.852869513329444,-1.30000000001149,
12.0693893749476));
#29629=CARTESIAN_POINT('Ctrl Pts',(-0.820647185601926,-1.18514270861956,
12.0606941221766));
#29630=CARTESIAN_POINT('Ctrl Pts',(-0.792815469737626,-1.06847604194905,
12.0448792800955));
#29631=CARTESIAN_POINT('Ctrl Pts',(-0.738661830119352,-0.794772684000832,
11.9918961555659));
#29632=CARTESIAN_POINT('Ctrl Pts',(-0.719381690621249,-0.636309800095182,
11.927765607536));
#29633=CARTESIAN_POINT('Ctrl Pts',(-0.681009666211855,-0.319434907277152,
11.8636640896346));
#29634=CARTESIAN_POINT('Ctrl Pts',(-0.668721509130177,-0.158333333333328,
11.8254656175414));
#29635=CARTESIAN_POINT('Ctrl Pts',(-0.638266505472543,0.15833333333333,
11.8297692452917));
#29636=CARTESIAN_POINT('Ctrl Pts',(-0.619251838548418,0.319434907277157,
11.8723633623647));
#29637=CARTESIAN_POINT('Ctrl Pts',(-0.597316162344372,0.636309800095189,
11.9450436276509));
#29638=CARTESIAN_POINT('Ctrl Pts',(-0.583841371506697,0.794772684000823,
12.0133455370274));
#29639=CARTESIAN_POINT('Ctrl Pts',(-0.59230706893329,1.06847604194525,12.0738508224656));
#29640=CARTESIAN_POINT('Ctrl Pts',(-0.602621019135524,1.18514270861207,
12.0929205048113));
#29641=CARTESIAN_POINT('Ctrl Pts',(-0.619584432809021,1.30000000000044,
12.1048693733783));
#29642=CARTESIAN_POINT('Ctrl Pts',(-0.857756263455172,-1.30000000001149,
12.0546463002434));
#29643=CARTESIAN_POINT('Ctrl Pts',(-0.826777915563002,-1.18514270861955,
12.0431077053763));
#29644=CARTESIAN_POINT('Ctrl Pts',(-0.799791193187777,-1.06847604194905,
12.0252135500953));
#29645=CARTESIAN_POINT('Ctrl Pts',(-0.746667919292781,-0.794772684000831,
11.9691918557023));
#29646=CARTESIAN_POINT('Ctrl Pts',(-0.726684243680441,-0.636309800095182,
11.9055952862092));
#29647=CARTESIAN_POINT('Ctrl Pts',(-0.687953766670922,-0.319434907277152,
11.8414036063792));
#29648=CARTESIAN_POINT('Ctrl Pts',(-0.674928204569495,-0.158333333333329,
11.8041281373097));
#29649=CARTESIAN_POINT('Ctrl Pts',(-0.644786943020532,0.15833333333333,
11.8084501671754));
#29650=CARTESIAN_POINT('Ctrl Pts',(-0.626886079124035,0.319434907277158,
11.8501324015904));
#29651=CARTESIAN_POINT('Ctrl Pts',(-0.605820300049983,0.63630980009519,
11.9229551449895));
#29652=CARTESIAN_POINT('Ctrl Pts',(-0.593236695086667,0.794772684000823,
11.9907870809948));
#29653=CARTESIAN_POINT('Ctrl Pts',(-0.600902941546169,1.06847604194525,
12.0543534139577));
#29654=CARTESIAN_POINT('Ctrl Pts',(-0.610435718320796,1.18514270861207,
12.0754994900718));
#29655=CARTESIAN_POINT('Ctrl Pts',(-0.626182837840153,1.30000000000045,
12.090276132125));
#29656=CARTESIAN_POINT('Ctrl Pts',(-0.864644628449034,-1.3000000000115,
12.0310472553246));
#29657=CARTESIAN_POINT('Ctrl Pts',(-0.834955202509833,-1.18514270861956,
12.0149459412788));
#29658=CARTESIAN_POINT('Ctrl Pts',(-0.808856027738995,-1.06847604194906,
11.9937159067301));
#29659=CARTESIAN_POINT('Ctrl Pts',(-0.756855911323515,-0.794772684000833,
11.9328219095113));
#29660=CARTESIAN_POINT('Ctrl Pts',(-0.736034398151118,-0.636309800095184,
11.870088231716));
#29661=CARTESIAN_POINT('Ctrl Pts',(-0.697391884991225,-0.319434907277153,
11.8057563938321));
#29662=CARTESIAN_POINT('Ctrl Pts',(-0.684176003430856,-0.158333333333329,
11.7699635731805));
#29663=CARTESIAN_POINT('Ctrl Pts',(-0.655128309893531,0.158333333333331,
11.7743144927794));
#29664=CARTESIAN_POINT('Ctrl Pts',(-0.639098183310164,0.319434907277159,
11.8145449842146));
#29665=CARTESIAN_POINT('Ctrl Pts',(-0.618976588811999,0.636309800095192,
11.8875626261278));
#29666=CARTESIAN_POINT('Ctrl Pts',(-0.606686062383306,0.794772684000826,
11.9545666974269));
#29667=CARTESIAN_POINT('Ctrl Pts',(-0.612704837274032,1.06847604194525,
12.0230303781235));
#29668=CARTESIAN_POINT('Ctrl Pts',(-0.62101138188125,1.18514270861208,12.0475164781124));
#29669=CARTESIAN_POINT('Ctrl Pts',(-0.635019166463077,1.30000000000045,
12.066853287546));
#29670=CARTESIAN_POINT('Ctrl Pts',(-0.871823313020447,-1.3000000000115,
12.0074165305344));
#29671=CARTESIAN_POINT('Ctrl Pts',(-0.843419365115712,-1.18514270861956,
11.9867520917804));
#29672=CARTESIAN_POINT('Ctrl Pts',(-0.818264588190346,-1.06847604194906,
11.9621852591644));
#29673=CARTESIAN_POINT('Ctrl Pts',(-0.767658256254581,-0.794772684000836,
11.896415650752));
#29674=CARTESIAN_POINT('Ctrl Pts',(-0.746661656345003,-0.636309800095187,
11.8345383396903));
#29675=CARTESIAN_POINT('Ctrl Pts',(-0.708018162750769,-0.319434907277156,
11.7700665973413));
#29676=CARTESIAN_POINT('Ctrl Pts',(-0.694138943110603,-0.15833333333333,
11.7357745430453));
#29677=CARTESIAN_POINT('Ctrl Pts',(-0.665269484383368,0.158333333333332,
11.7401347217955));
#29678=CARTESIAN_POINT('Ctrl Pts',(-0.649849813569892,0.319434907277161,
11.7788574661797));
#29679=CARTESIAN_POINT('Ctrl Pts',(-0.630563019913342,0.636309800095195,
11.8520669521813));
#29680=CARTESIAN_POINT('Ctrl Pts',(-0.619731947798664,0.794772684000831,
11.9182908531853));
#29681=CARTESIAN_POINT('Ctrl Pts',(-0.624903674483712,1.06847604194526,
11.9916814007995));
#29682=CARTESIAN_POINT('Ctrl Pts',(-0.63229108230308,1.18514270861208,12.0195178447586));
#29683=CARTESIAN_POINT('Ctrl Pts',(-0.644827249091217,1.30000000000046,
12.0434226840024));
#29684=CARTESIAN_POINT('Ctrl Pts',(-0.878501924149539,-1.3000000000115,
11.9837919824015));
#29685=CARTESIAN_POINT('Ctrl Pts',(-0.851593849899919,-1.18514270861957,
11.9585435767857));
#29686=CARTESIAN_POINT('Ctrl Pts',(-0.827318970973691,-1.06847604194906,
11.9306273219391));
#29687=CARTESIAN_POINT('Ctrl Pts',(-0.777322352448109,-0.794772684000837,
11.8599719231924));
#29688=CARTESIAN_POINT('Ctrl Pts',(-0.754045433093823,-0.636309800095185,
11.7989833086607));
#29689=CARTESIAN_POINT('Ctrl Pts',(-0.715008483530921,-0.319434907277153,
11.7343686089337));
#29690=CARTESIAN_POINT('Ctrl Pts',(-0.701574831806603,-0.158333333333329,
11.7015525526237));
#29691=CARTESIAN_POINT('Ctrl Pts',(-0.673894849027944,0.158333333333331,
11.7059103525462));
#29692=CARTESIAN_POINT('Ctrl Pts',(-0.65976531894143,0.319434907277161,
11.7431259723976));
#29693=CARTESIAN_POINT('Ctrl Pts',(-0.642182221447585,0.636309800095194,
11.8165321273102));
#29694=CARTESIAN_POINT('Ctrl Pts',(-0.633533642865829,0.794772684000825,
11.8819903817194));
#29695=CARTESIAN_POINT('Ctrl Pts',(-0.637513538252151,1.06847604194525,
11.9603096822764));
#29696=CARTESIAN_POINT('Ctrl Pts',(-0.643530336300666,1.18514270861208,
11.9914944048591));
#29697=CARTESIAN_POINT('Ctrl Pts',(-0.653841183154614,1.30000000000046,
12.0199623268296));
#29698=CARTESIAN_POINT('Ctrl Pts',(-0.883557620031031,-1.3000000000115,
11.9660343263365));
#29699=CARTESIAN_POINT('Ctrl Pts',(-0.856845494787491,-1.18514270861957,
11.9373706087656));
#29700=CARTESIAN_POINT('Ctrl Pts',(-0.832849332419673,-1.06847604194906,
11.9069544151971));
#29701=CARTESIAN_POINT('Ctrl Pts',(-0.78368781450453,-0.794772684000841,
11.8326383531807));
#29702=CARTESIAN_POINT('Ctrl Pts',(-0.761796018154491,-0.63630980009519,
11.7722658357778));
#29703=CARTESIAN_POINT('Ctrl Pts',(-0.722736188073244,-0.319434907277156,
11.7075445931099));
#29704=CARTESIAN_POINT('Ctrl Pts',(-0.707613932029028,-0.158333333333331,
11.6758783453701));
#29705=CARTESIAN_POINT('Ctrl Pts',(-0.679765481684038,0.158333333333332,
11.6802412589297));
#29706=CARTESIAN_POINT('Ctrl Pts',(-0.666795618498137,0.319434907277163,
11.7163157384279));
#29707=CARTESIAN_POINT('Ctrl Pts',(-0.649626496355868,0.636309800095198,
11.7898316119687));
#29708=CARTESIAN_POINT('Ctrl Pts',(-0.64091936790216,0.794772684000834,
11.8546401172946));
#29709=CARTESIAN_POINT('Ctrl Pts',(-0.644477404575823,1.06847604194526,
11.936664901596));
#29710=CARTESIAN_POINT('Ctrl Pts',(-0.650189127781039,1.18514270861208,
11.9703850564661));
#29711=CARTESIAN_POINT('Ctrl Pts',(-0.66007243195369,1.30000000000046,12.0023198763999));
#29712=CARTESIAN_POINT('Ctrl Pts',(-0.887281295441576,-1.3000000000115,
11.9483568191932));
#29713=CARTESIAN_POINT('Ctrl Pts',(-0.861806181848091,-1.18514270861957,
11.9162326705626));
#29714=CARTESIAN_POINT('Ctrl Pts',(-0.838516494444084,-1.06847604194906,
11.8832903206437));
#29715=CARTESIAN_POINT('Ctrl Pts',(-0.789761429146444,-0.79477268400084,
11.8052966935815));
#29716=CARTESIAN_POINT('Ctrl Pts',(-0.765800673218215,-0.636309800095188,
11.7456175979226));
#29717=CARTESIAN_POINT('Ctrl Pts',(-0.726343628275416,-0.319434907277154,
11.6807914709022));
#29718=CARTESIAN_POINT('Ctrl Pts',(-0.711403458489195,-0.15833333333333,
11.6502281095496));
#29719=CARTESIAN_POINT('Ctrl Pts',(-0.685078224489192,0.158333333333332,
11.6545703789146));
#29720=CARTESIAN_POINT('Ctrl Pts',(-0.674269857923319,0.319434907277163,
11.6894882681703));
#29721=CARTESIAN_POINT('Ctrl Pts',(-0.658929605102686,0.636309800095197,
11.7631343154741));
#29722=CARTESIAN_POINT('Ctrl Pts',(-0.651505739224311,0.794772684000829,
11.8273679692787));
#29723=CARTESIAN_POINT('Ctrl Pts',(-0.653946884062025,1.06847604194526,
11.9130946810947));
#29724=CARTESIAN_POINT('Ctrl Pts',(-0.658499180558779,1.18514270861208,
11.9493313800572));
#29725=CARTESIAN_POINT('Ctrl Pts',(-0.666547092405371,1.30000000000046,
11.9846968609247));
#29726=CARTESIAN_POINT('Ctrl Pts',(-0.892703441219226,-1.30000000001151,
11.9305719471507));
#29727=CARTESIAN_POINT('Ctrl Pts',(-0.867861945427389,-1.18514270861957,
11.8950149270867));
#29728=CARTESIAN_POINT('Ctrl Pts',(-0.844983347403223,-1.06847604194906,
11.859564292742));
#29729=CARTESIAN_POINT('Ctrl Pts',(-0.796663895640123,-0.794772684000841,
11.7779120078267));
#29730=CARTESIAN_POINT('Ctrl Pts',(-0.772227335557577,-0.636309800095189,
11.7188940920834));
#29731=CARTESIAN_POINT('Ctrl Pts',(-0.732424394074677,-0.319434907277156,
11.6539705401567));
#29732=CARTESIAN_POINT('Ctrl Pts',(-0.717112193228731,-0.158333333333331,
11.6245378964453));
#29733=CARTESIAN_POINT('Ctrl Pts',(-0.690622206064707,0.158333333333332,
11.6288726611887));
#29734=CARTESIAN_POINT('Ctrl Pts',(-0.679713770617353,0.319434907277163,
11.6626385810088));
#29735=CARTESIAN_POINT('Ctrl Pts',(-0.66500986725975,0.636309800095199,
11.7363947688458));
#29736=CARTESIAN_POINT('Ctrl Pts',(-0.659065939520507,0.794772684000833,
11.7999938191272));
#29737=CARTESIAN_POINT('Ctrl Pts',(-0.661570434056588,1.06847604194526,
11.8894333440492));
#29738=CARTESIAN_POINT('Ctrl Pts',(-0.665813828387652,1.18514270861208,
11.9282072795572));
#29739=CARTESIAN_POINT('Ctrl Pts',(-0.673216514165779,1.30000000000046,
11.9670400942955));
#29740=CARTESIAN_POINT('Ctrl Pts',(-0.894984307098906,-1.3000000000115,
11.9158592698447));
#29741=CARTESIAN_POINT('Ctrl Pts',(-0.87060412226304,-1.18514270861957,
11.877430347329));
#29742=CARTESIAN_POINT('Ctrl Pts',(-0.848070591674411,-1.06847604194906,
11.8398786914086));
#29743=CARTESIAN_POINT('Ctrl Pts',(-0.800279768931258,-0.79477268400084,
11.7551535153833));
#29744=CARTESIAN_POINT('Ctrl Pts',(-0.775870214390773,-0.63630980009519,
11.6966683639025));
#29745=CARTESIAN_POINT('Ctrl Pts',(-0.736016130791778,-0.319434907277156,
11.6316498793278));
#29746=CARTESIAN_POINT('Ctrl Pts',(-0.720069234314568,-0.158333333333331,
11.6031686722742));
#29747=CARTESIAN_POINT('Ctrl Pts',(-0.694043459634896,0.158333333333332,
11.6074850335135));
#29748=CARTESIAN_POINT('Ctrl Pts',(-0.684234636903101,0.319434907277163,
11.6402707573857));
#29749=CARTESIAN_POINT('Ctrl Pts',(-0.67052600784846,0.636309800095199,
11.7141054852488));
#29750=CARTESIAN_POINT('Ctrl Pts',(-0.665408068045094,0.794772684000834,
11.7771791444796));
#29751=CARTESIAN_POINT('Ctrl Pts',(-0.66757080607668,1.06847604194526,11.8697080313361));
#29752=CARTESIAN_POINT('Ctrl Pts',(-0.671332221044731,1.18514270861209,
11.9105939344582));
#29753=CARTESIAN_POINT('Ctrl Pts',(-0.6779188818243,1.30000000000046,11.9523134141154));
#29754=CARTESIAN_POINT('Ctrl Pts',(-0.89857809711787,-1.30000000001151,
11.9039905526542));
#29755=CARTESIAN_POINT('Ctrl Pts',(-0.874603358219584,-1.18514270861957,
11.8632690261007));
#29756=CARTESIAN_POINT('Ctrl Pts',(-0.852274272367022,-1.06847604194906,
11.8240441276441));
#29757=CARTESIAN_POINT('Ctrl Pts',(-0.804491404877559,-0.794772684000842,
11.7368842756001));
#29758=CARTESIAN_POINT('Ctrl Pts',(-0.779337536601101,-0.63630980009519,
11.6788530360347));
#29759=CARTESIAN_POINT('Ctrl Pts',(-0.73892990170289,-0.319434907277156,
11.6137837345045));
#29760=CARTESIAN_POINT('Ctrl Pts',(-0.722441783590277,-0.158333333333331,
11.5860732558579));
#29761=CARTESIAN_POINT('Ctrl Pts',(-0.69673919586524,0.158333333333333,
11.590376212721));
#29762=CARTESIAN_POINT('Ctrl Pts',(-0.687911166797296,0.319434907277164,
11.6223606112703));
#29763=CARTESIAN_POINT('Ctrl Pts',(-0.675177329582872,0.6363098000952,11.6962538723052));
#29764=CARTESIAN_POINT('Ctrl Pts',(-0.671095145736662,0.794772684000834,
11.7589138472138));
#29765=CARTESIAN_POINT('Ctrl Pts',(-0.67283030602288,1.06847604194526,11.8539181159165));
#29766=CARTESIAN_POINT('Ctrl Pts',(-0.676014982447061,1.18514270861209,
11.8964952730699));
#29767=CARTESIAN_POINT('Ctrl Pts',(-0.681633248701541,1.30000000000046,
11.9405257597103));
#29768=CARTESIAN_POINT('Ctrl Pts',(-0.902477105871258,-1.3000000000115,
11.8862709956588));
#29769=CARTESIAN_POINT('Ctrl Pts',(-0.879221148848204,-1.18514270861957,
11.8421011623459));
#29770=CARTESIAN_POINT('Ctrl Pts',(-0.857323211941763,-1.06847604194906,
11.8003577978764));
#29771=CARTESIAN_POINT('Ctrl Pts',(-0.809871895161875,-0.79477268400084,
11.7095279036636));
#29772=CARTESIAN_POINT('Ctrl Pts',(-0.78376380919803,-0.63630980009519,
11.6521754885616));
#29773=CARTESIAN_POINT('Ctrl Pts',(-0.743059579658607,-0.319434907277157,
11.5870018840245));
#29774=CARTESIAN_POINT('Ctrl Pts',(-0.726496099759876,-0.158333333333331,
11.5604077166868));
#29775=CARTESIAN_POINT('Ctrl Pts',(-0.701225272913036,0.158333333333333,
11.564684638206));
#29776=CARTESIAN_POINT('Ctrl Pts',(-0.693057788862471,0.319434907277164,
11.5955056206572));
#29777=CARTESIAN_POINT('Ctrl Pts',(-0.681187501823921,0.6363098000952,11.6694930695212));
#29778=CARTESIAN_POINT('Ctrl Pts',(-0.677908421627274,0.794772684000835,
11.7315085139232));
#29779=CARTESIAN_POINT('Ctrl Pts',(-0.679723677487409,1.06847604194526,
11.830224032349));
#29780=CARTESIAN_POINT('Ctrl Pts',(-0.682719357389429,1.18514270861209,
11.875340909519));
#29781=CARTESIAN_POINT('Ctrl Pts',(-0.687924960193474,1.30000000000046,
11.9228443737031));
#29782=CARTESIAN_POINT('Ctrl Pts',(-0.908701175984222,-1.30000000001151,
11.8596446736958));
#29783=CARTESIAN_POINT('Ctrl Pts',(-0.885597731026704,-1.18514270861958,
11.8103494528277));
#29784=CARTESIAN_POINT('Ctrl Pts',(-0.863726842934849,-1.06847604194907,
11.7648613672129));
#29785=CARTESIAN_POINT('Ctrl Pts',(-0.816048169119225,-0.794772684000848,
11.6685700336343));
#29786=CARTESIAN_POINT('Ctrl Pts',(-0.789297210261759,-0.636309800095195,
11.6122070099515));
#29787=CARTESIAN_POINT('Ctrl Pts',(-0.748080016284346,-0.319434907277159,
11.5468882279858));
#29788=CARTESIAN_POINT('Ctrl Pts',(-0.730922493088147,-0.158333333333332,
11.5219976057089));
#29789=CARTESIAN_POINT('Ctrl Pts',(-0.706296610091351,0.158333333333333,
11.5262284547253));
#29790=CARTESIAN_POINT('Ctrl Pts',(-0.699176918679878,0.319434907277163,
11.5552723030019));
#29791=CARTESIAN_POINT('Ctrl Pts',(-0.68952274971155,0.636309800095202,
11.629367132279));
#29792=CARTESIAN_POINT('Ctrl Pts',(-0.689442245328543,0.794772684000841,
11.6903943283916));
#29793=CARTESIAN_POINT('Ctrl Pts',(-0.691123492164588,1.06847604194527,
11.7946579210228));
#29794=CARTESIAN_POINT('Ctrl Pts',(-0.6931914874416,1.18514270861209,11.843579616181));
#29795=CARTESIAN_POINT('Ctrl Pts',(-0.696599728536635,1.30000000000047,
11.8962911605941));
#29796=CARTESIAN_POINT('Ctrl Pts',(-0.915130190235684,-1.30000000001151,
11.8242205798896));
#29797=CARTESIAN_POINT('Ctrl Pts',(-0.893056339639968,-1.18514270861957,
11.7680209678601));
#29798=CARTESIAN_POINT('Ctrl Pts',(-0.871639908682559,-1.06847604194907,
11.7175023970209));
#29799=CARTESIAN_POINT('Ctrl Pts',(-0.823682439710349,-0.794772684000845,
11.6139187338168));
#29800=CARTESIAN_POINT('Ctrl Pts',(-0.794249766051324,-0.636309800095193,
11.5590155181827));
#29801=CARTESIAN_POINT('Ctrl Pts',(-0.751861014111227,-0.319434907277158,
11.4935377543236));
#29802=CARTESIAN_POINT('Ctrl Pts',(-0.734333408979958,-0.158333333333331,
11.4708919274452));
#29803=CARTESIAN_POINT('Ctrl Pts',(-0.711210673215988,0.158333333333333,
11.474997385459));
#29804=CARTESIAN_POINT('Ctrl Pts',(-0.706934100478653,0.319434907277164,
11.5015762199418));
#29805=CARTESIAN_POINT('Ctrl Pts',(-0.699537697066227,0.636309800095202,
11.5757677752393));
#29806=CARTESIAN_POINT('Ctrl Pts',(-0.70026656533437,0.794772684000837,
11.6355062348343));
#29807=CARTESIAN_POINT('Ctrl Pts',(-0.701961607982734,1.06847604194527,
11.7471880962734));
#29808=CARTESIAN_POINT('Ctrl Pts',(-0.703658269885911,1.18514270861209,
11.80119546492));
#29809=CARTESIAN_POINT('Ctrl Pts',(-0.706317872537308,1.30000000000047,
11.8608672626169));
#29810=CARTESIAN_POINT('Ctrl Pts',(-0.919875601210953,-1.30000000001151,
11.794755777199));
#29811=CARTESIAN_POINT('Ctrl Pts',(-0.897754873416259,-1.18514270861958,
11.7328980381801));
#29812=CARTESIAN_POINT('Ctrl Pts',(-0.876137226977588,-1.06847604194907,
11.6782555736647));
#29813=CARTESIAN_POINT('Ctrl Pts',(-0.827358357683314,-0.794772684000842,
11.5686892769622));
#29814=CARTESIAN_POINT('Ctrl Pts',(-0.796899762965292,-0.636309800095194,
11.5149399801506));
#29815=CARTESIAN_POINT('Ctrl Pts',(-0.753134772148241,-0.319434907277159,
11.449386078349));
#29816=CARTESIAN_POINT('Ctrl Pts',(-0.734068291732325,-0.158333333333332,
11.4287191254146));
#29817=CARTESIAN_POINT('Ctrl Pts',(-0.711489212968676,0.158333333333334,
11.4327379611124));
#29818=CARTESIAN_POINT('Ctrl Pts',(-0.708878543676851,0.319434907277166,
11.4572226251063));
#29819=CARTESIAN_POINT('Ctrl Pts',(-0.704814412254138,0.636309800095204,
11.5313722822653));
#29820=CARTESIAN_POINT('Ctrl Pts',(-0.709558684665683,0.794772684000838,
11.5898828461728));
#29821=CARTESIAN_POINT('Ctrl Pts',(-0.712685057867134,1.06847604194527,
11.7076289689314));
#29822=CARTESIAN_POINT('Ctrl Pts',(-0.714207440026723,1.1851427086121,11.7658395763296));
#29823=CARTESIAN_POINT('Ctrl Pts',(-0.715898913230535,1.30000000000048,
11.8312928575076));
#29824=CARTESIAN_POINT('Ctrl Pts',(-0.924141876334402,-1.30000000001151,
11.77109374108));
#29825=CARTESIAN_POINT('Ctrl Pts',(-0.902128626336287,-1.18514270861958,
11.7046408337731));
#29826=CARTESIAN_POINT('Ctrl Pts',(-0.880266737286765,-1.06847604194907,
11.6466664975652));
#29827=CARTESIAN_POINT('Ctrl Pts',(-0.830111074198288,-0.794772684000846,
11.5323213785717));
#29828=CARTESIAN_POINT('Ctrl Pts',(-0.796780342020798,-0.636309800095194,
11.4796953438876));
#29829=CARTESIAN_POINT('Ctrl Pts',(-0.752031508840179,-0.319434907277159,
11.414066913023));
#29830=CARTESIAN_POINT('Ctrl Pts',(-0.733948122062509,-0.158333333333332,
11.3947980763829));
#29831=CARTESIAN_POINT('Ctrl Pts',(-0.712402467902627,0.158333333333334,
11.3986851071608));
#29832=CARTESIAN_POINT('Ctrl Pts',(-0.710570449880107,0.319434907277166,
11.4215419748185));
#29833=CARTESIAN_POINT('Ctrl Pts',(-0.708111636311791,0.636309800095204,
11.4956970484854));
#29834=CARTESIAN_POINT('Ctrl Pts',(-0.714522758116903,0.794772684000838,
11.5532469192424));
#29835=CARTESIAN_POINT('Ctrl Pts',(-0.718124410207019,1.06847604194527,
11.6759178206841));
#29836=CARTESIAN_POINT('Ctrl Pts',(-0.719474850841755,1.1851427086121,11.7375308903995));
#29837=CARTESIAN_POINT('Ctrl Pts',(-0.720616710375778,1.30000000000048,
11.8076573420011));
#29838=CARTESIAN_POINT('Ctrl Pts',(-0.926371093396794,-1.30000000001152,
11.753459339287));
#29839=CARTESIAN_POINT('Ctrl Pts',(-0.904090435631733,-1.18514270861958,
11.6836508049185));
#29840=CARTESIAN_POINT('Ctrl Pts',(-0.881916612865422,-1.06847604194907,
11.623236534169));
#29841=CARTESIAN_POINT('Ctrl Pts',(-0.830937456637536,-0.794772684000847,
11.5053701111827));
#29842=CARTESIAN_POINT('Ctrl Pts',(-0.796952716130588,-0.636309800095196,
11.4534698280134));
#29843=CARTESIAN_POINT('Ctrl Pts',(-0.751203299623306,-0.31943490727716,
11.3878331944127));
#29844=CARTESIAN_POINT('Ctrl Pts',(-0.732079387725648,-0.158333333333332,
11.3697640959159));
#29845=CARTESIAN_POINT('Ctrl Pts',(-0.710840218192551,0.158333333333334,
11.3735847534848));
#29846=CARTESIAN_POINT('Ctrl Pts',(-0.71018123879766,0.319434907277167,
11.395154921514));
#29847=CARTESIAN_POINT('Ctrl Pts',(-0.709701662316501,0.636309800095206,
11.4692249373051));
#29848=CARTESIAN_POINT('Ctrl Pts',(-0.717994743494202,0.79477268400084,
11.5259919854094));
#29849=CARTESIAN_POINT('Ctrl Pts',(-0.723001082445735,1.06847604194527,
11.6522344970941));
#29850=CARTESIAN_POINT('Ctrl Pts',(-0.72470786072698,1.1851427086121,11.7163406580131));
#29851=CARTESIAN_POINT('Ctrl Pts',(-0.725954358660491,1.30000000000048,
11.7899072742888));
#29852=CARTESIAN_POINT('Ctrl Pts',(-0.928515616741265,-1.30000000001152,
11.7357458531039));
#29853=CARTESIAN_POINT('Ctrl Pts',(-0.906220595951806,-1.18514270861958,
11.6624050656068));
#29854=CARTESIAN_POINT('Ctrl Pts',(-0.883726917173569,-1.06847604194907,
11.5994386109857));
#29855=CARTESIAN_POINT('Ctrl Pts',(-0.831303079656328,-0.794772684000849,
11.4779402887388));
#29856=CARTESIAN_POINT('Ctrl Pts',(-0.79401622890383,-0.636309800095196,
11.4270499306769));
#29857=CARTESIAN_POINT('Ctrl Pts',(-0.748443991722638,-0.31943490727716,
11.3612517013318));
#29858=CARTESIAN_POINT('Ctrl Pts',(-0.732895889171905,-0.158333333333333,
11.3439307342967));
#29859=CARTESIAN_POINT('Ctrl Pts',(-0.712854812281222,0.158333333333334,
11.3475845935226));
#29860=CARTESIAN_POINT('Ctrl Pts',(-0.710580569151887,0.319434907277167,
11.3681203190846));
#29861=CARTESIAN_POINT('Ctrl Pts',(-0.710811179990112,0.636309800095207,
11.4422556130938));
#29862=CARTESIAN_POINT('Ctrl Pts',(-0.721190875660884,0.794772684000841,
11.4982216430212));
#29863=CARTESIAN_POINT('Ctrl Pts',(-0.727041576108211,1.06847604194527,
11.6282345327963));
#29864=CARTESIAN_POINT('Ctrl Pts',(-0.728824440348993,1.1851427086121,11.6949522758241));
#29865=CARTESIAN_POINT('Ctrl Pts',(-0.729857617396724,1.30000000000048,
11.7721099993483));
#29866=CARTESIAN_POINT('Ctrl Pts',(-0.930329635621813,-1.30000000001152,
11.7210988980544));
#29867=CARTESIAN_POINT('Ctrl Pts',(-0.907076845997319,-1.18514270861958,
11.6451431370766));
#29868=CARTESIAN_POINT('Ctrl Pts',(-0.884085358419116,-1.06847604194908,
11.5802500565896));
#29869=CARTESIAN_POINT('Ctrl Pts',(-0.831574082683346,-0.794772684000852,
11.455891063866));
#29870=CARTESIAN_POINT('Ctrl Pts',(-0.796125283318549,-0.636309800095196,
11.4053623224109));
#29871=CARTESIAN_POINT('Ctrl Pts',(-0.75140068947891,-0.319434907277159,
11.3394432860062));
#29872=CARTESIAN_POINT('Ctrl Pts',(-0.736139894754654,-0.158333333333332,
11.3230376354443));
#29873=CARTESIAN_POINT('Ctrl Pts',(-0.715467336234378,0.158333333333334,
11.3267399924723));
#29874=CARTESIAN_POINT('Ctrl Pts',(-0.711333498127357,0.319434907277167,
11.3464993960691));
#29875=CARTESIAN_POINT('Ctrl Pts',(-0.711346536120014,0.636309800095206,
11.4206699483946));
#29876=CARTESIAN_POINT('Ctrl Pts',(-0.723269722424154,0.794772684000839,
11.4759041572379));
#29877=CARTESIAN_POINT('Ctrl Pts',(-0.729727433914076,1.06847604194527,
11.6087621891132));
#29878=CARTESIAN_POINT('Ctrl Pts',(-0.731628539382279,1.1851427086121,11.6774767588117));
#29879=CARTESIAN_POINT('Ctrl Pts',(-0.73263544629649,1.30000000000048,11.7573965790852));
#29880=CARTESIAN_POINT('Ctrl Pts',(-0.931747258687475,-1.30000000001152,
11.7034562621613));
#29881=CARTESIAN_POINT('Ctrl Pts',(-0.90733877716988,-1.18514270861958,
11.6239757801627));
#29882=CARTESIAN_POINT('Ctrl Pts',(-0.883910231356362,-1.06847604194908,
11.5564438916877));
#29883=CARTESIAN_POINT('Ctrl Pts',(-0.832049451175459,-0.794772684000851,
11.4280353609519));
#29884=CARTESIAN_POINT('Ctrl Pts',(-0.799951516477764,-0.636309800095196,
11.3776840270139));
#29885=CARTESIAN_POINT('Ctrl Pts',(-0.757363875886255,-0.319434907277159,
11.3113557017931));
#29886=CARTESIAN_POINT('Ctrl Pts',(-0.742707262105031,-0.158333333333332,
11.2961489921131));
#29887=CARTESIAN_POINT('Ctrl Pts',(-0.722150626445397,0.158333333333334,
11.299816574206));
#29888=CARTESIAN_POINT('Ctrl Pts',(-0.717216708376096,0.319434907277167,
11.3183579084001));
#29889=CARTESIAN_POINT('Ctrl Pts',(-0.715964078358445,0.636309800095206,
11.3928350448839));
#29890=CARTESIAN_POINT('Ctrl Pts',(-0.726336336909195,0.79477268400084,
11.447716025051));
#29891=CARTESIAN_POINT('Ctrl Pts',(-0.732307490535758,1.06847604194527,
11.5846602431266));
#29892=CARTESIAN_POINT('Ctrl Pts',(-0.734317087069204,1.1851427086121,11.65608184955));
#29893=CARTESIAN_POINT('Ctrl Pts',(-0.735751588984204,1.30000000000048,
11.739646984675));
#29894=CARTESIAN_POINT('Ctrl Pts',(-0.932811379692883,-1.30000000001152,
11.6914337625578));
#29895=CARTESIAN_POINT('Ctrl Pts',(-0.90624835288135,-1.18514270861958,
11.6096869608822));
#29896=CARTESIAN_POINT('Ctrl Pts',(-0.882011643627204,-1.06847604194908,
11.5404979069991));
#29897=CARTESIAN_POINT('Ctrl Pts',(-0.831394255649799,-0.794772684000851,
11.409668260878));
#29898=CARTESIAN_POINT('Ctrl Pts',(-0.805863671216798,-0.636309800095197,
11.3596728386796));
#29899=CARTESIAN_POINT('Ctrl Pts',(-0.76676614190522,-0.319434907277159,
11.2934131620907));
#29900=CARTESIAN_POINT('Ctrl Pts',(-0.7519939500761,-0.158333333333332,
11.2792748470613));
#29901=CARTESIAN_POINT('Ctrl Pts',(-0.731604230888437,0.158333333333334,
11.2829625198157));
#29902=CARTESIAN_POINT('Ctrl Pts',(-0.726824245390955,0.319434907277167,
11.3005329620478));
#29903=CARTESIAN_POINT('Ctrl Pts',(-0.722683372359804,0.636309800095206,
11.3748246904046));
#29904=CARTESIAN_POINT('Ctrl Pts',(-0.72755043150687,0.79477268400084,11.4289715802577));
#29905=CARTESIAN_POINT('Ctrl Pts',(-0.732217053984718,1.06847604194527,
11.5683538364568));
#29906=CARTESIAN_POINT('Ctrl Pts',(-0.734729140509331,1.1851427086121,11.6415286370167));
#29907=CARTESIAN_POINT('Ctrl Pts',(-0.737733305603302,1.30000000000048,
11.7275448240494));
#29908=CARTESIAN_POINT('Ctrl Pts',(-0.936125406442746,-1.30000000001152,
11.6834957005072));
#29909=CARTESIAN_POINT('Ctrl Pts',(-0.909492919288004,-1.18514270861958,
11.6019904180297));
#29910=CARTESIAN_POINT('Ctrl Pts',(-0.885532801702577,-1.06847604194908,
11.5330073325074));
#29911=CARTESIAN_POINT('Ctrl Pts',(-0.836353845186883,-0.794772684000851,
11.4025713849577));
#29912=CARTESIAN_POINT('Ctrl Pts',(-0.813383183475108,-0.636309800095197,
11.3527487599227));
#29913=CARTESIAN_POINT('Ctrl Pts',(-0.77596280188267,-0.319434907277159,
11.2866672191688));
#29914=CARTESIAN_POINT('Ctrl Pts',(-0.761169784372622,-0.158333333333332,
11.2724808787964));
#29915=CARTESIAN_POINT('Ctrl Pts',(-0.74101228662764,0.158333333333334,
11.2762150307074));
#29916=CARTESIAN_POINT('Ctrl Pts',(-0.736764158587383,0.319434907277167,
11.2939064508864));
#29917=CARTESIAN_POINT('Ctrl Pts',(-0.730851239620766,0.636309800095206,
11.368060793598));
#29918=CARTESIAN_POINT('Ctrl Pts',(-0.732075357025827,0.79477268400084,
11.421994282357));
#29919=CARTESIAN_POINT('Ctrl Pts',(-0.735457044102353,1.06847604194527,
11.5609770187779));
#29920=CARTESIAN_POINT('Ctrl Pts',(-0.738012470505655,1.1851427086121,11.6339459053542));
#29921=CARTESIAN_POINT('Ctrl Pts',(-0.741659516280686,1.30000000000048,
11.7197232017282));
#29922=CARTESIAN_POINT('Ctrl Pts',(-0.936125406440075,-1.3,11.683495700499));
#29923=CARTESIAN_POINT('Ctrl Pts',(-0.909492919286402,-1.18514270861178,
11.6019904180251));
#29924=CARTESIAN_POINT('Ctrl Pts',(-0.885532801701866,-1.06847604194512,
11.5330073325055));
#29925=CARTESIAN_POINT('Ctrl Pts',(-0.836353845186883,-0.794772684000851,
11.4025713849577));
#29926=CARTESIAN_POINT('Ctrl Pts',(-0.813383183475108,-0.636309800095197,
11.3527487599227));
#29927=CARTESIAN_POINT('Ctrl Pts',(-0.775962801882671,-0.319434907277159,
11.2866672191688));
#29928=CARTESIAN_POINT('Ctrl Pts',(-0.761169784372622,-0.158333333333332,
11.2724808787964));
#29929=CARTESIAN_POINT('Ctrl Pts',(-0.741012286627641,0.158333333333334,
11.2762150307074));
#29930=CARTESIAN_POINT('Ctrl Pts',(-0.736764158587383,0.319434907277167,
11.2939064508864));
#29931=CARTESIAN_POINT('Ctrl Pts',(-0.730851239620766,0.636309800095206,
11.368060793598));
#29932=CARTESIAN_POINT('Ctrl Pts',(-0.732075357025827,0.79477268400084,
11.421994282357));
#29933=CARTESIAN_POINT('Ctrl Pts',(-0.735457044102351,1.06847604194511,
11.5609770187778));
#29934=CARTESIAN_POINT('Ctrl Pts',(-0.738012470505648,1.18514270861177,
11.633945905354));
#29935=CARTESIAN_POINT('Ctrl Pts',(-0.741659516280671,1.3,11.7197232017278));
#29936=CARTESIAN_POINT('',(-0.818977267421107,-1.2,12.0817800273514));
#29937=CARTESIAN_POINT('Ctrl Pts',(-0.818977267421108,-1.2,12.0817800273514));
#29938=CARTESIAN_POINT('Ctrl Pts',(-0.829590878647036,-1.21693989154628,
12.0628228500606));
#29939=CARTESIAN_POINT('Ctrl Pts',(-0.841157631026617,-1.23347875773062,
12.0440503378966));
#29940=CARTESIAN_POINT('Ctrl Pts',(-0.857159462862295,-1.25898780506585,
12.0153221239789));
#29941=CARTESIAN_POINT('Ctrl Pts',(-0.862316329350737,-1.26708707076649,
12.0061721287558));
#29942=CARTESIAN_POINT('Ctrl Pts',(-0.871215005322769,-1.28134030327299,
11.9900791870324));
#29943=CARTESIAN_POINT('Ctrl Pts',(-0.877883425044479,-1.29212373571783,
11.9778974543232));
#29944=CARTESIAN_POINT('Ctrl Pts',(-0.881788403109014,-1.29865542294387,
11.9705339008578));
#29945=CARTESIAN_POINT('Ctrl Pts',(-0.882187409448981,-1.29932801060554,
11.9697761372506));
#29946=CARTESIAN_POINT('Ctrl Pts',(-0.88258187706403,-1.3000000000115,11.9690197347219));
#29947=CARTESIAN_POINT('',(-0.664237986899246,-0.653834841416763,12.1052306670025));
#29948=CARTESIAN_POINT('Ctrl Pts',(-0.664237986905426,-0.653834841416077,
12.105230667028));
#29949=CARTESIAN_POINT('Ctrl Pts',(-0.680353745117992,-0.717928623971185,
12.1030483641927));
#29950=CARTESIAN_POINT('Ctrl Pts',(-0.693482797353694,-0.763796716852745,
12.1012100657869));
#29951=CARTESIAN_POINT('Ctrl Pts',(-0.744781546673584,-0.949538510163098,
12.0937752011493));
#29952=CARTESIAN_POINT('Ctrl Pts',(-0.772317944299114,-1.0477587126458,
12.0896076895435));
#29953=CARTESIAN_POINT('Ctrl Pts',(-0.818977267421107,-1.2,12.0817800273514));
#29954=CARTESIAN_POINT('',(-0.525742999964556,0.653834841531101,12.1220010461182));
#29955=CARTESIAN_POINT('Ctrl Pts',(-0.525742999964555,0.653834841531117,
12.1220010461182));
#29956=CARTESIAN_POINT('Ctrl Pts',(-0.539180494581549,0.575791384517359,
12.0825525341831));
#29957=CARTESIAN_POINT('Ctrl Pts',(-0.551088168076891,0.493917938905458,
12.0497160696344));
#29958=CARTESIAN_POINT('Ctrl Pts',(-0.570743025184575,0.338198422468042,
12.0029892655978));
#29959=CARTESIAN_POINT('Ctrl Pts',(-0.578836711827597,0.265710408106597,
11.987005961632));
#29960=CARTESIAN_POINT('Ctrl Pts',(-0.593510978022751,0.129738985434452,
11.9674960160308));
#29961=CARTESIAN_POINT('Ctrl Pts',(-0.600113893017226,0.0666402976695767,
11.9624924648463));
#29962=CARTESIAN_POINT('Ctrl Pts',(-0.613310308940931,-0.0595494045754736,
11.9605197921755));
#29963=CARTESIAN_POINT('Ctrl Pts',(-0.620002378829859,-0.122795601055212,
11.9635188907578));
#29964=CARTESIAN_POINT('Ctrl Pts',(-0.633837957101957,-0.260143441971975,
11.9789765523794));
#29965=CARTESIAN_POINT('Ctrl Pts',(-0.640844580997494,-0.333940897156081,
11.9930593600372));
#29966=CARTESIAN_POINT('Ctrl Pts',(-0.653894554419043,-0.491228500515348,
12.0359708867721));
#29967=CARTESIAN_POINT('Ctrl Pts',(-0.659731921577109,-0.574163620766454,
12.0669021452979));
#29968=CARTESIAN_POINT('Ctrl Pts',(-0.664237986928543,-0.653834841428476,
12.1052306669747));
#29969=CARTESIAN_POINT('',(-0.597447978578511,1.2,12.1138127673826));
#29970=CARTESIAN_POINT('Ctrl Pts',(-0.597447978578509,1.2,12.1138127673826));
#29971=CARTESIAN_POINT('Ctrl Pts',(-0.585248394446679,1.13497002128492,
12.1152960589169));
#29972=CARTESIAN_POINT('Ctrl Pts',(-0.568988293295729,1.03881507655241,
12.1172252340192));
#29973=CARTESIAN_POINT('Ctrl Pts',(-0.537251997267457,0.795009267531881,
12.120775755352));
#29974=CARTESIAN_POINT('Ctrl Pts',(-0.53228169119802,0.741767795577442,
12.1213026165338));
#29975=CARTESIAN_POINT('Ctrl Pts',(-0.525742999964558,0.653834841531101,
12.1220010461182));
#29976=CARTESIAN_POINT('Ctrl Pts',(-0.659151153699351,1.29999999999999,
12.0049994543784));
#29977=CARTESIAN_POINT('Ctrl Pts',(-0.649082664482629,1.28244937374245,
12.0240956466888));
#29978=CARTESIAN_POINT('Ctrl Pts',(-0.638073668917069,1.2652022482834,12.0429614950135));
#29979=CARTESIAN_POINT('Ctrl Pts',(-0.622388419312196,1.23914419848352,
12.071260359206));
#29980=CARTESIAN_POINT('Ctrl Pts',(-0.610683834550175,1.2193232684228,12.0927379078));
#29981=CARTESIAN_POINT('Ctrl Pts',(-0.597447978578509,1.2,12.1138127673826));
#29982=CARTESIAN_POINT('Ctrl Pts',(-0.936125406440075,-1.3,11.683495700499));
#29983=CARTESIAN_POINT('Ctrl Pts',(-0.909492919286402,-1.18514270861178,
11.6019904180251));
#29984=CARTESIAN_POINT('Ctrl Pts',(-0.885532801701865,-1.06847604194512,
11.5330073325055));
#29985=CARTESIAN_POINT('Ctrl Pts',(-0.836353845186884,-0.794772684000851,
11.4025713849577));
#29986=CARTESIAN_POINT('Ctrl Pts',(-0.813383183475109,-0.636309800095197,
11.3527487599227));
#29987=CARTESIAN_POINT('Ctrl Pts',(-0.775962801882671,-0.319434907277159,
11.2866672191688));
#29988=CARTESIAN_POINT('Ctrl Pts',(-0.761169784372622,-0.158333333333333,
11.2724808787964));
#29989=CARTESIAN_POINT('Ctrl Pts',(-0.741012286627641,0.158333333333334,
11.2762150307074));
#29990=CARTESIAN_POINT('Ctrl Pts',(-0.736764158587383,0.319434907277167,
11.2939064508864));
#29991=CARTESIAN_POINT('Ctrl Pts',(-0.730851239620767,0.636309800095206,
11.368060793598));
#29992=CARTESIAN_POINT('Ctrl Pts',(-0.732075357025827,0.79477268400084,
11.421994282357));
#29993=CARTESIAN_POINT('Ctrl Pts',(-0.735457044102351,1.06847604194511,
11.5609770187778));
#29994=CARTESIAN_POINT('Ctrl Pts',(-0.738012470505648,1.18514270861178,
11.633945905354));
#29995=CARTESIAN_POINT('Ctrl Pts',(-0.741659516280671,1.3,11.7197232017278));
#29996=CARTESIAN_POINT('Ctrl Pts',(-1.01101605778904,-1.3,11.6658747012318));
#29997=CARTESIAN_POINT('Ctrl Pts',(-0.982742057194053,-1.18514270861178,
11.5849228973736));
#29998=CARTESIAN_POINT('Ctrl Pts',(-0.95765377154039,-1.06847604194512,
11.5163675802146));
#29999=CARTESIAN_POINT('Ctrl Pts',(-0.90705445160062,-0.794772684000851,
11.386629447317));
#30000=CARTESIAN_POINT('Ctrl Pts',(-0.884801197368707,-0.636309800095197,
11.3368248349354));
#30001=CARTESIAN_POINT('Ctrl Pts',(-0.847999940077956,-0.319434907277159,
11.270991020387));
#30002=CARTESIAN_POINT('Ctrl Pts',(-0.834445726094756,-0.158333333333333,
11.2567221110703));
#30003=CARTESIAN_POINT('Ctrl Pts',(-0.814362858626307,0.158333333333334,
11.2608073708274));
#30004=CARTESIAN_POINT('Ctrl Pts',(-0.808949443435951,0.319434907277167,
11.2789272273103));
#30005=CARTESIAN_POINT('Ctrl Pts',(-0.802571685601039,0.636309800095206,
11.3535596997118));
#30006=CARTESIAN_POINT('Ctrl Pts',(-0.803147745067787,0.79477268400084,
11.4078014397586));
#30007=CARTESIAN_POINT('Ctrl Pts',(-0.808110825487516,1.06847604194511,
11.5468439477319));
#30008=CARTESIAN_POINT('Ctrl Pts',(-0.811870873772818,1.18514270861178,
11.6197447528576));
#30009=CARTESIAN_POINT('Ctrl Pts',(-0.817242636729975,1.3,11.70536001344));
#30010=CARTESIAN_POINT('Ctrl Pts',(-1.08590670913801,-1.3,11.6482537019647));
#30011=CARTESIAN_POINT('Ctrl Pts',(-1.05599119510171,-1.18514270861178,
11.5678553767222));
#30012=CARTESIAN_POINT('Ctrl Pts',(-1.02977474137891,-1.06847604194512,
11.4997278279237));
#30013=CARTESIAN_POINT('Ctrl Pts',(-0.977755058014356,-0.794772684000851,
11.3706875096762));
#30014=CARTESIAN_POINT('Ctrl Pts',(-0.956219211262306,-0.636309800095197,
11.3209009099481));
#30015=CARTESIAN_POINT('Ctrl Pts',(-0.920037078273243,-0.319434907277159,
11.2553148216052));
#30016=CARTESIAN_POINT('Ctrl Pts',(-0.90772166781689,-0.158333333333333,
11.2409633433442));
#30017=CARTESIAN_POINT('Ctrl Pts',(-0.887713430624973,0.158333333333334,
11.2453997109473));
#30018=CARTESIAN_POINT('Ctrl Pts',(-0.881134728284519,0.319434907277167,
11.2639480037341));
#30019=CARTESIAN_POINT('Ctrl Pts',(-0.874292131581311,0.636309800095206,
11.3390586058255));
#30020=CARTESIAN_POINT('Ctrl Pts',(-0.874220133109747,0.79477268400084,
11.3936085971601));
#30021=CARTESIAN_POINT('Ctrl Pts',(-0.880764606872681,1.06847604194511,
11.5327108766861));
#30022=CARTESIAN_POINT('Ctrl Pts',(-0.885729277039988,1.18514270861178,
11.6055436003612));
#30023=CARTESIAN_POINT('Ctrl Pts',(-0.892825757179279,1.3,11.6909968251522));
#30024=CARTESIAN_POINT('Ctrl Pts',(-1.16079736048698,-1.3,11.6306327026976));
#30025=CARTESIAN_POINT('Ctrl Pts',(-1.12924033300936,-1.18514270861178,
11.5507878560707));
#30026=CARTESIAN_POINT('Ctrl Pts',(-1.10189571121744,-1.06847604194512,
11.4830880756329));
#30027=CARTESIAN_POINT('Ctrl Pts',(-1.04845566442809,-0.794772684000851,
11.3547455720355));
#30028=CARTESIAN_POINT('Ctrl Pts',(-1.0276372251559,-0.636309800095197,
11.3049769849608));
#30029=CARTESIAN_POINT('Ctrl Pts',(-0.992074216468528,-0.319434907277159,
11.2396386228234));
#30030=CARTESIAN_POINT('Ctrl Pts',(-0.980997609539023,-0.158333333333333,
11.2252045756181));
#30031=CARTESIAN_POINT('Ctrl Pts',(-0.961064002623639,0.158333333333334,
11.2299920510673));
#30032=CARTESIAN_POINT('Ctrl Pts',(-0.953320013133087,0.319434907277167,
11.248968780158));
#30033=CARTESIAN_POINT('Ctrl Pts',(-0.946012577561583,0.636309800095206,
11.3245575119393));
#30034=CARTESIAN_POINT('Ctrl Pts',(-0.945292521151708,0.79477268400084,
11.3794157545617));
#30035=CARTESIAN_POINT('Ctrl Pts',(-0.953418388257847,1.06847604194511,
11.5185778056402));
#30036=CARTESIAN_POINT('Ctrl Pts',(-0.959587680307158,1.18514270861178,
11.5913424478648));
#30037=CARTESIAN_POINT('Ctrl Pts',(-0.968408877628584,1.3,11.6766336368644));
#30038=CARTESIAN_POINT('Ctrl Pts',(-1.16079736048698,-1.3,11.6306327026976));
#30039=CARTESIAN_POINT('Ctrl Pts',(-1.12924033300936,-1.18514270861178,
11.5507878560707));
#30040=CARTESIAN_POINT('Ctrl Pts',(-1.10189571121744,-1.06847604194512,
11.4830880756329));
#30041=CARTESIAN_POINT('Ctrl Pts',(-1.04845566442809,-0.794772684000851,
11.3547455720355));
#30042=CARTESIAN_POINT('Ctrl Pts',(-1.0276372251559,-0.636309800095197,
11.3049769849608));
#30043=CARTESIAN_POINT('Ctrl Pts',(-0.992074216468528,-0.319434907277159,
11.2396386228234));
#30044=CARTESIAN_POINT('Ctrl Pts',(-0.980997609539023,-0.158333333333332,
11.2252045756181));
#30045=CARTESIAN_POINT('Ctrl Pts',(-0.961064002623638,0.158333333333334,
11.2299920510673));
#30046=CARTESIAN_POINT('Ctrl Pts',(-0.953320013133087,0.319434907277167,
11.248968780158));
#30047=CARTESIAN_POINT('Ctrl Pts',(-0.946012577561583,0.636309800095206,
11.3245575119393));
#30048=CARTESIAN_POINT('Ctrl Pts',(-0.945292521151708,0.79477268400084,
11.3794157545617));
#30049=CARTESIAN_POINT('Ctrl Pts',(-0.953418388257847,1.06847604194511,
11.5185778056402));
#30050=CARTESIAN_POINT('Ctrl Pts',(-0.959587680307158,1.18514270861178,
11.5913424478648));
#30051=CARTESIAN_POINT('Ctrl Pts',(-0.968408877628584,1.3,11.6766336368644));
#30052=CARTESIAN_POINT('Ctrl Pts',(-1.16079736048729,-1.30000000000112,
11.6306327026983));
#30053=CARTESIAN_POINT('Ctrl Pts',(-1.12924033300954,-1.18514270861254,
11.5507878560712));
#30054=CARTESIAN_POINT('Ctrl Pts',(-1.10189571121751,-1.0684760419455,11.483088075633));
#30055=CARTESIAN_POINT('Ctrl Pts',(-1.04845566442809,-0.794772684000851,
11.3547455720355));
#30056=CARTESIAN_POINT('Ctrl Pts',(-1.0276372251559,-0.636309800095196,
11.3049769849608));
#30057=CARTESIAN_POINT('Ctrl Pts',(-0.992074216468527,-0.319434907277159,
11.2396386228234));
#30058=CARTESIAN_POINT('Ctrl Pts',(-0.980997609539022,-0.158333333333332,
11.2252045756181));
#30059=CARTESIAN_POINT('Ctrl Pts',(-0.961064002623638,0.158333333333334,
11.2299920510673));
#30060=CARTESIAN_POINT('Ctrl Pts',(-0.953320013133086,0.319434907277167,
11.248968780158));
#30061=CARTESIAN_POINT('Ctrl Pts',(-0.946012577561583,0.636309800095206,
11.3245575119393));
#30062=CARTESIAN_POINT('Ctrl Pts',(-0.945292521151708,0.79477268400084,
11.3794157545617));
#30063=CARTESIAN_POINT('Ctrl Pts',(-0.953418388257849,1.06847604194519,
11.5185778056402));
#30064=CARTESIAN_POINT('Ctrl Pts',(-0.959587680307166,1.18514270861193,
11.5913424478649));
#30065=CARTESIAN_POINT('Ctrl Pts',(-0.968408877628601,1.30000000000022,
11.6766336368646));
#30066=CARTESIAN_POINT('Ctrl Pts',(-1.16756547281003,-1.30000000000112,
11.6361811764323));
#30067=CARTESIAN_POINT('Ctrl Pts',(-1.13532397902382,-1.18514270861254,
11.5563795754664));
#30068=CARTESIAN_POINT('Ctrl Pts',(-1.10785601152158,-1.0684760419455,11.488509311166));
#30069=CARTESIAN_POINT('Ctrl Pts',(-1.05542731230007,-0.794772684000851,
11.3592791977852));
#30070=CARTESIAN_POINT('Ctrl Pts',(-1.03785006786609,-0.636309800095196,
11.3078339412244));
#30071=CARTESIAN_POINT('Ctrl Pts',(-1.00385002391231,-0.319434907277159,
11.2416493150162));
#30072=CARTESIAN_POINT('Ctrl Pts',(-0.992336747169047,-0.158333333333332,
11.2275421125221));
#30073=CARTESIAN_POINT('Ctrl Pts',(-0.972209900186257,0.158333333333334,
11.2324665017675));
#30074=CARTESIAN_POINT('Ctrl Pts',(-0.964465402249317,0.319434907277167,
11.2513908870207));
#30075=CARTESIAN_POINT('Ctrl Pts',(-0.955698270375139,0.636309800095206,
11.3278245114471));
#30076=CARTESIAN_POINT('Ctrl Pts',(-0.952709891127445,0.79477268400084,
11.3838818264982));
#30077=CARTESIAN_POINT('Ctrl Pts',(-0.959681817340565,1.06847604194519,
11.5239886018995));
#30078=CARTESIAN_POINT('Ctrl Pts',(-0.965682205206487,1.18514270861193,
11.5970539055485));
#30079=CARTESIAN_POINT('Ctrl Pts',(-0.974665092415997,1.30000000000022,
11.682537481243));
#30080=CARTESIAN_POINT('Ctrl Pts',(-1.17433759800624,-1.30000000000114,
11.6464116794424));
#30081=CARTESIAN_POINT('Ctrl Pts',(-1.14166436485374,-1.18514270861256,
11.5694808106212));
#30082=CARTESIAN_POINT('Ctrl Pts',(-1.11444976981747,-1.06847604194552,
11.5034134250506));
#30083=CARTESIAN_POINT('Ctrl Pts',(-1.06418915706796,-0.794772684000863,
11.3758813671891));
#30084=CARTESIAN_POINT('Ctrl Pts',(-1.0513091229464,-0.636309800095205,
11.3215414692882));
#30085=CARTESIAN_POINT('Ctrl Pts',(-1.01984359533584,-0.319434907277162,
11.2540237958508));
#30086=CARTESIAN_POINT('Ctrl Pts',(-1.0077743357193,-0.158333333333334,
11.2391008731644));
#30087=CARTESIAN_POINT('Ctrl Pts',(-0.987512099007357,0.158333333333336,
11.2441073694368));
#30088=CARTESIAN_POINT('Ctrl Pts',(-0.980345522160174,0.319434907277171,
11.2639439027508));
#30089=CARTESIAN_POINT('Ctrl Pts',(-0.968447629115628,0.636309800095215,
11.3418486499862));
#30090=CARTESIAN_POINT('Ctrl Pts',(-0.959621049662965,0.79477268400085,
11.4008963472683));
#30091=CARTESIAN_POINT('Ctrl Pts',(-0.964471525893826,1.0684760419452,11.5393026757461));
#30092=CARTESIAN_POINT('Ctrl Pts',(-0.970529496012491,1.18514270861194,
11.610531299113));
#30093=CARTESIAN_POINT('Ctrl Pts',(-0.980545844817339,1.30000000000024,
11.6930775747087));
#30094=CARTESIAN_POINT('Ctrl Pts',(-1.18440586374583,-1.30000000000115,
11.6613628993834));
#30095=CARTESIAN_POINT('Ctrl Pts',(-1.15281179463886,-1.18514270861256,
11.5879487744173));
#30096=CARTESIAN_POINT('Ctrl Pts',(-1.12658990680956,-1.06847604194552,
11.524407622229));
#30097=CARTESIAN_POINT('Ctrl Pts',(-1.07842291370587,-0.794772684000867,
11.4004233915087));
#30098=CARTESIAN_POINT('Ctrl Pts',(-1.06681408259705,-0.636309800095209,
11.3451288299006));
#30099=CARTESIAN_POINT('Ctrl Pts',(-1.03664169893558,-0.319434907277165,
11.2773712449188));
#30100=CARTESIAN_POINT('Ctrl Pts',(-1.02481278861994,-0.158333333333335,
11.2610028855051));
#30101=CARTESIAN_POINT('Ctrl Pts',(-1.0044850652804,0.158333333333337,11.2660078555499));
#30102=CARTESIAN_POINT('Ctrl Pts',(-0.997358728970921,0.319434907277173,
11.2871590926494));
#30103=CARTESIAN_POINT('Ctrl Pts',(-0.983329367588696,0.636309800095218,
11.3655638273867));
#30104=CARTESIAN_POINT('Ctrl Pts',(-0.97135393304074,0.794772684000856,
11.4261862920945));
#30105=CARTESIAN_POINT('Ctrl Pts',(-0.973948227190362,1.06847604194521,
11.5611531693971));
#30106=CARTESIAN_POINT('Ctrl Pts',(-0.979354787992951,1.18514270861195,
11.6297802214725));
#30107=CARTESIAN_POINT('Ctrl Pts',(-0.989044935788829,1.30000000000025,
11.7086121654545));
#30108=CARTESIAN_POINT('Ctrl Pts',(-1.19298536144512,-1.30000000000116,
11.6736347004981));
#30109=CARTESIAN_POINT('Ctrl Pts',(-1.16257956592102,-1.18514270861257,
11.6026906475997));
#30110=CARTESIAN_POINT('Ctrl Pts',(-1.13708399446326,-1.06847604194553,
11.5409940674741));
#30111=CARTESIAN_POINT('Ctrl Pts',(-1.0895277239045,-0.794772684000875,
11.4198261370814));
#30112=CARTESIAN_POINT('Ctrl Pts',(-1.07616291886583,-0.636309800095215,
11.3645178040103));
#30113=CARTESIAN_POINT('Ctrl Pts',(-1.046127413614,-0.319434907277168,11.2967346480581));
#30114=CARTESIAN_POINT('Ctrl Pts',(-1.0356366171024,-0.158333333333337,
11.2789326233998));
#30115=CARTESIAN_POINT('Ctrl Pts',(-1.01578267670476,0.158333333333339,
11.2837609183981));
#30116=CARTESIAN_POINT('Ctrl Pts',(-1.00856388451852,0.319434907277175,
11.3059044815962));
#30117=CARTESIAN_POINT('Ctrl Pts',(-0.993790452697415,0.636309800095223,
11.3845140146692));
#30118=CARTESIAN_POINT('Ctrl Pts',(-0.980710833423847,0.794772684000864,
11.446079999681));
#30119=CARTESIAN_POINT('Ctrl Pts',(-0.982257391046026,1.06847604194522,
11.5784182630752));
#30120=CARTESIAN_POINT('Ctrl Pts',(-0.987267620003271,1.18514270861196,
11.6451250692127));
#30121=CARTESIAN_POINT('Ctrl Pts',(-0.996618630428724,1.30000000000026,
11.7212543508803));
#30122=CARTESIAN_POINT('Ctrl Pts',(-1.20105256512359,-1.30000000000117,
11.6846776130528));
#30123=CARTESIAN_POINT('Ctrl Pts',(-1.17182076003448,-1.18514270861259,
11.6161968728078));
#30124=CARTESIAN_POINT('Ctrl Pts',(-1.14702653796543,-1.06847604194554,
11.5563595354834));
#30125=CARTESIAN_POINT('Ctrl Pts',(-1.0999986294307,-0.794772684000881,
11.4380913056996));
#30126=CARTESIAN_POINT('Ctrl Pts',(-1.08498990472442,-0.636309800095221,
11.3828473439718));
#30127=CARTESIAN_POINT('Ctrl Pts',(-1.05457956671436,-0.319434907277171,
11.3152877377322));
#30128=CARTESIAN_POINT('Ctrl Pts',(-1.04492763006788,-0.158333333333338,
11.2962396194479));
#30129=CARTESIAN_POINT('Ctrl Pts',(-1.02445048342747,0.15833333333334,11.3012437581198));
#30130=CARTESIAN_POINT('Ctrl Pts',(-1.01546159798066,0.319434907277179,
11.3248855867104));
#30131=CARTESIAN_POINT('Ctrl Pts',(-1.00042100180492,0.63630980009523,11.4034742761441));
#30132=CARTESIAN_POINT('Ctrl Pts',(-0.989132095493053,0.794772684000872,
11.4649686187968));
#30133=CARTESIAN_POINT('Ctrl Pts',(-0.990490881115352,1.06847604194523,
11.594349776762));
#30134=CARTESIAN_POINT('Ctrl Pts',(-0.995057162532792,1.18514270861197,
11.6591412225012));
#30135=CARTESIAN_POINT('Ctrl Pts',(-1.00360155741975,1.30000000000027,11.7327198047409));
#30136=CARTESIAN_POINT('Ctrl Pts',(-1.20689949924884,-1.30000000000117,
11.6917782430978));
#30137=CARTESIAN_POINT('Ctrl Pts',(-1.17845243113741,-1.18514270861259,
11.6248282543793));
#30138=CARTESIAN_POINT('Ctrl Pts',(-1.15410150400538,-1.06847604194554,
11.5661579127043));
#30139=CARTESIAN_POINT('Ctrl Pts',(-1.10730889603686,-0.794772684000884,
11.4497453274811));
#30140=CARTESIAN_POINT('Ctrl Pts',(-1.09120924295904,-0.636309800095223,
11.3945642230668));
#30141=CARTESIAN_POINT('Ctrl Pts',(-1.06001205148635,-0.319434907277172,
11.327335922249));
#30142=CARTESIAN_POINT('Ctrl Pts',(-1.05000648532554,-0.158333333333339,
11.3078132435952));
#30143=CARTESIAN_POINT('Ctrl Pts',(-1.0289822678563,0.158333333333341,11.3129700474019));
#30144=CARTESIAN_POINT('Ctrl Pts',(-1.01946870924847,0.31943490727718,11.337318972364));
#30145=CARTESIAN_POINT('Ctrl Pts',(-1.00477531806935,0.636309800095232,
11.4157246330572));
#30146=CARTESIAN_POINT('Ctrl Pts',(-0.995163031930164,0.794772684000874,
11.4770283488341));
#30147=CARTESIAN_POINT('Ctrl Pts',(-0.996348460080219,1.06847604194523,
11.6045910634879));
#30148=CARTESIAN_POINT('Ctrl Pts',(-1.00044163242317,1.18514270861198,11.6682499633972));
#30149=CARTESIAN_POINT('Ctrl Pts',(-1.00811484918735,1.30000000000028,11.7403505907066));
#30150=CARTESIAN_POINT('Ctrl Pts',(-1.21290364438232,-1.30000000000118,
11.698835255245));
#30151=CARTESIAN_POINT('Ctrl Pts',(-1.18517186067427,-1.18514270861259,
11.6334762032491));
#30152=CARTESIAN_POINT('Ctrl Pts',(-1.16120472180641,-1.06847604194555,
11.5760187052981));
#30153=CARTESIAN_POINT('Ctrl Pts',(-1.11453291910748,-0.794772684000885,
11.461534561243));
#30154=CARTESIAN_POINT('Ctrl Pts',(-1.09730001002919,-0.636309800095224,
11.4064183653184));
#30155=CARTESIAN_POINT('Ctrl Pts',(-1.06524461600585,-0.319434907277173,
11.3395345033929));
#30156=CARTESIAN_POINT('Ctrl Pts',(-1.05468161482419,-0.158333333333339,
11.3195732647092));
#30157=CARTESIAN_POINT('Ctrl Pts',(-1.03344222170005,0.158333333333341,
11.3247807857825));
#30158=CARTESIAN_POINT('Ctrl Pts',(-1.02429992110725,0.319434907277181,
11.3495874441969));
#30159=CARTESIAN_POINT('Ctrl Pts',(-1.00996736700274,0.636309800095234,
11.4278162259574));
#30160=CARTESIAN_POINT('Ctrl Pts',(-1.00099482485428,0.794772684000876,
11.489260778002));
#30161=CARTESIAN_POINT('Ctrl Pts',(-1.00187182097402,1.06847604194523,11.6150124880496));
#30162=CARTESIAN_POINT('Ctrl Pts',(-1.00560365754974,1.18514270861198,11.677478729188));
#30163=CARTESIAN_POINT('Ctrl Pts',(-1.01268771157684,1.30000000000028,11.7479779557451));
#30164=CARTESIAN_POINT('Ctrl Pts',(-1.22618519864795,-1.30000000000117,
11.7171839141231));
#30165=CARTESIAN_POINT('Ctrl Pts',(-1.20029820969549,-1.18514270861259,
11.6557804959295));
#30166=CARTESIAN_POINT('Ctrl Pts',(-1.1774891576665,-1.06847604194555,11.6012816521569));
#30167=CARTESIAN_POINT('Ctrl Pts',(-1.13190633457677,-0.794772684000887,
11.491329368754));
#30168=CARTESIAN_POINT('Ctrl Pts',(-1.11309362995195,-0.636309800095223,
11.4359111902228));
#30169=CARTESIAN_POINT('Ctrl Pts',(-1.07962100664597,-0.319434907277172,
11.3696324319088));
#30170=CARTESIAN_POINT('Ctrl Pts',(-1.06755959380154,-0.158333333333339,
11.3486314227978));
#30171=CARTESIAN_POINT('Ctrl Pts',(-1.04563975760617,0.158333333333341,
11.354033649905));
#30172=CARTESIAN_POINT('Ctrl Pts',(-1.03692233361866,0.319434907277181,
11.3801842515533));
#30173=CARTESIAN_POINT('Ctrl Pts',(-1.02342169532662,0.636309800095234,
11.4579815559397));
#30174=CARTESIAN_POINT('Ctrl Pts',(-1.01646829809711,0.794772684000875,
11.5195861143864));
#30175=CARTESIAN_POINT('Ctrl Pts',(-1.01666663265259,1.06847604194523,11.6407453923103));
#30176=CARTESIAN_POINT('Ctrl Pts',(-1.01948091312335,1.18514270861198,11.7002238250183));
#30177=CARTESIAN_POINT('Ctrl Pts',(-1.02502362238482,1.30000000000028,11.7667353284147));
#30178=CARTESIAN_POINT('Ctrl Pts',(-1.24813860795827,-1.30000000000129,
11.7429927856957));
#30179=CARTESIAN_POINT('Ctrl Pts',(-1.2264525293792,-1.18514270861269,11.6866859516542));
#30180=CARTESIAN_POINT('Ctrl Pts',(-1.20615493716576,-1.06847604194564,
11.6361391300789));
#30181=CARTESIAN_POINT('Ctrl Pts',(-1.16247111990375,-0.794772684000951,
11.5326726414666));
#30182=CARTESIAN_POINT('Ctrl Pts',(-1.13883908333676,-0.636309800095283,
11.4779589372101));
#30183=CARTESIAN_POINT('Ctrl Pts',(-1.10197370831211,-0.319434907277205,
11.4131688831434));
#30184=CARTESIAN_POINT('Ctrl Pts',(-1.08738397050814,-0.158333333333354,
11.3908083257058));
#30185=CARTESIAN_POINT('Ctrl Pts',(-1.06439414201174,0.158333333333356,
11.3965200012287));
#30186=CARTESIAN_POINT('Ctrl Pts',(-1.05691133021397,0.319434907277209,
11.4243254506344));
#30187=CARTESIAN_POINT('Ctrl Pts',(-1.04507964885187,0.636309800095292,
11.5012931953789));
#30188=CARTESIAN_POINT('Ctrl Pts',(-1.0416738801892,0.794772684000951,11.562919855076));
#30189=CARTESIAN_POINT('Ctrl Pts',(-1.04039339555115,1.06847604194533,11.6775759855885));
#30190=CARTESIAN_POINT('Ctrl Pts',(-1.04138798256821,1.18514270861209,11.7328848202995));
#30191=CARTESIAN_POINT('Ctrl Pts',(-1.04393143095552,1.3000000000004,11.793872099251));
#30192=CARTESIAN_POINT('Ctrl Pts',(-1.26978166142668,-1.30000000000132,
11.7689185967311));
#30193=CARTESIAN_POINT('Ctrl Pts',(-1.25073245999804,-1.18514270861273,
11.718424664199));
#30194=CARTESIAN_POINT('Ctrl Pts',(-1.23223782137633,-1.06847604194567,
11.6721762443729));
#30195=CARTESIAN_POINT('Ctrl Pts',(-1.19079265734443,-0.794772684000976,
11.575141126273));
#30196=CARTESIAN_POINT('Ctrl Pts',(-1.16623243927054,-0.636309800095297,
11.5195123009208));
#30197=CARTESIAN_POINT('Ctrl Pts',(-1.12774217801638,-0.319434907277209,
11.4555287799354));
#30198=CARTESIAN_POINT('Ctrl Pts',(-1.11016030267911,-0.158333333333357,
11.4320233662326));
#30199=CARTESIAN_POINT('Ctrl Pts',(-1.08625156130612,0.158333333333359,
11.4380535962252));
#30200=CARTESIAN_POINT('Ctrl Pts',(-1.08045831900887,0.319434907277216,
11.4674483189564));
#30201=CARTESIAN_POINT('Ctrl Pts',(-1.06916124243966,0.636309800095305,
11.5440020301027));
#30202=CARTESIAN_POINT('Ctrl Pts',(-1.06704328315777,0.794772684000967,
11.6063846328021));
#30203=CARTESIAN_POINT('Ctrl Pts',(-1.06311483577445,1.06847604194535,11.7148788223867));
#30204=CARTESIAN_POINT('Ctrl Pts',(-1.06207708456856,1.18514270861211,11.7660573346459));
#30205=CARTESIAN_POINT('Ctrl Pts',(-1.06170206146569,1.30000000000043,11.8214512445991));
#30206=CARTESIAN_POINT('Ctrl Pts',(-1.28621507340038,-1.30000000000135,
11.787444008607));
#30207=CARTESIAN_POINT('Ctrl Pts',(-1.27068858339734,-1.18514270861275,
11.7404565922239));
#30208=CARTESIAN_POINT('Ctrl Pts',(-1.25446887060034,-1.06847604194569,
11.6969042378102));
#30209=CARTESIAN_POINT('Ctrl Pts',(-1.21539660596413,-0.794772684000991,
11.6042252668273));
#30210=CARTESIAN_POINT('Ctrl Pts',(-1.1880682889676,-0.636309800095309,
11.5488823476501));
#30211=CARTESIAN_POINT('Ctrl Pts',(-1.14767980214843,-0.319434907277216,
11.4858445626509));
#30212=CARTESIAN_POINT('Ctrl Pts',(-1.1281592556255,-0.15833333333336,11.4614541561878));
#30213=CARTESIAN_POINT('Ctrl Pts',(-1.10345103237585,0.158333333333362,
11.4677753839338));
#30214=CARTESIAN_POINT('Ctrl Pts',(-1.09857321173,0.319434907277223,11.4983919872682));
#30215=CARTESIAN_POINT('Ctrl Pts',(-1.08800167231434,0.636309800095319,
11.574499229092));
#30216=CARTESIAN_POINT('Ctrl Pts',(-1.08784105687488,0.794772684000983,
11.6370517121057));
#30217=CARTESIAN_POINT('Ctrl Pts',(-1.08213675247853,1.06847604194537,11.7410213750434));
#30218=CARTESIAN_POINT('Ctrl Pts',(-1.07948736551723,1.18514270861213,11.7892559936534));
#30219=CARTESIAN_POINT('Ctrl Pts',(-1.07665777360248,1.30000000000045,11.8407206162434));
#30220=CARTESIAN_POINT('Ctrl Pts',(-1.2988477852273,-1.30000000000137,11.8011898160843));
#30221=CARTESIAN_POINT('Ctrl Pts',(-1.28496304689735,-1.18514270861276,
11.7572780526074));
#30222=CARTESIAN_POINT('Ctrl Pts',(-1.26981948734302,-1.0684760419457,11.7160274702605));
#30223=CARTESIAN_POINT('Ctrl Pts',(-1.23192670645918,-0.794772684001,11.626878233666));
#30224=CARTESIAN_POINT('Ctrl Pts',(-1.20339270808647,-0.636309800095317,
11.5713448845443));
#30225=CARTESIAN_POINT('Ctrl Pts',(-1.16227892917472,-0.31943490727722,
11.5087171233327));
#30226=CARTESIAN_POINT('Ctrl Pts',(-1.14202028849874,-0.158333333333362,
11.4833758052458));
#30227=CARTESIAN_POINT('Ctrl Pts',(-1.11698880932356,0.158333333333364,
11.4898111602895));
#30228=CARTESIAN_POINT('Ctrl Pts',(-1.11265992653266,0.319434907277227,
11.5214253283881));
#30229=CARTESIAN_POINT('Ctrl Pts',(-1.10188207887894,0.636309800095326,
11.5974924555126));
#30230=CARTESIAN_POINT('Ctrl Pts',(-1.10178142294354,0.794772684000993,
11.6607002318859));
#30231=CARTESIAN_POINT('Ctrl Pts',(-1.0944826956649,1.06847604194539,11.7613683248178));
#30232=CARTESIAN_POINT('Ctrl Pts',(-1.09080071657814,1.18514270861215,11.8073233566545));
#30233=CARTESIAN_POINT('Ctrl Pts',(-1.08659610699906,1.30000000000047,11.855657933018));
#30234=CARTESIAN_POINT('Ctrl Pts',(-1.30959903943834,-1.3000000000014,11.8125295228691));
#30235=CARTESIAN_POINT('Ctrl Pts',(-1.2975816101224,-1.1851427086128,11.7709505876381));
#30236=CARTESIAN_POINT('Ctrl Pts',(-1.28368627549302,-1.06847604194573,
11.7314592499347));
#30237=CARTESIAN_POINT('Ctrl Pts',(-1.24724693579931,-0.794772684001022,
11.6450491275368));
#30238=CARTESIAN_POINT('Ctrl Pts',(-1.21760067785406,-0.636309800095336,
11.5894346271556));
#30239=CARTESIAN_POINT('Ctrl Pts',(-1.17564743019148,-0.319434907277229,
11.5272668765828));
#30240=CARTESIAN_POINT('Ctrl Pts',(-1.15418812004909,-0.158333333333367,
11.5013861396723));
#30241=CARTESIAN_POINT('Ctrl Pts',(-1.12885531704681,0.158333333333369,
11.5079362390012));
#30242=CARTESIAN_POINT('Ctrl Pts',(-1.12525652825615,0.319434907277237,
11.5402551178548));
#30243=CARTESIAN_POINT('Ctrl Pts',(-1.11504912781576,0.636309800095346,
11.615992998271));
#30244=CARTESIAN_POINT('Ctrl Pts',(-1.11630139094869,0.794772684001016,
11.6792370475013));
#30245=CARTESIAN_POINT('Ctrl Pts',(-1.10760457044329,1.06847604194542,11.7771924105374));
#30246=CARTESIAN_POINT('Ctrl Pts',(-1.10269037666985,1.18514270861218,11.8214012181949));
#30247=CARTESIAN_POINT('Ctrl Pts',(-1.09662652047079,1.3000000000005,11.8674175864555));
#30248=CARTESIAN_POINT('Ctrl Pts',(-1.31760194267207,-1.30000000000141,
11.8218663161006));
#30249=CARTESIAN_POINT('Ctrl Pts',(-1.30740878936986,-1.1851427086128,11.7820012977114));
#30250=CARTESIAN_POINT('Ctrl Pts',(-1.29473728074604,-1.06847604194573,
11.7438139784362));
#30251=CARTESIAN_POINT('Ctrl Pts',(-1.25973806431227,-0.794772684001023,
11.6594694521398));
#30252=CARTESIAN_POINT('Ctrl Pts',(-1.22907848423481,-0.636309800095337,
11.6038553909907));
#30253=CARTESIAN_POINT('Ctrl Pts',(-1.18625025075386,-0.31943490727723,
11.5421425696291));
#30254=CARTESIAN_POINT('Ctrl Pts',(-1.1635032970347,-0.158333333333367,
11.5159615935396));
#30255=CARTESIAN_POINT('Ctrl Pts',(-1.13773612695948,0.158333333333369,
11.5226872205802));
#30256=CARTESIAN_POINT('Ctrl Pts',(-1.13489948120314,0.319434907277237,
11.555508014619));
#30257=CARTESIAN_POINT('Ctrl Pts',(-1.12486792444456,0.636309800095347,
11.6310952409414));
#30258=CARTESIAN_POINT('Ctrl Pts',(-1.12656133963866,0.794772684001018,
11.6946178963244));
#30259=CARTESIAN_POINT('Ctrl Pts',(-1.11669649677285,1.06847604194542,11.7904131544161));
#30260=CARTESIAN_POINT('Ctrl Pts',(-1.11091640428911,1.18514270861219,11.8331719559363));
#30261=CARTESIAN_POINT('Ctrl Pts',(-1.1036263442698,1.30000000000051,11.8772233413129));
#30262=CARTESIAN_POINT('Ctrl Pts',(-1.33044578595549,-1.30000000000145,
11.8354926488634));
#30263=CARTESIAN_POINT('Ctrl Pts',(-1.32211288865797,-1.18514270861284,
11.7986019247905));
#30264=CARTESIAN_POINT('Ctrl Pts',(-1.31068800059481,-1.06847604194577,
11.7626398529816));
#30265=CARTESIAN_POINT('Ctrl Pts',(-1.27715110640868,-0.794772684001048,
11.6817056454209));
#30266=CARTESIAN_POINT('Ctrl Pts',(-1.2453022793547,-0.636309800095356,
11.6259099815901));
#30267=CARTESIAN_POINT('Ctrl Pts',(-1.20186071890905,-0.319434907277239,
11.5645749966149));
#30268=CARTESIAN_POINT('Ctrl Pts',(-1.17821381724787,-0.158333333333372,
11.5375213000565));
#30269=CARTESIAN_POINT('Ctrl Pts',(-1.15255006747905,0.158333333333374,
11.5441900625005));
#30270=CARTESIAN_POINT('Ctrl Pts',(-1.15106019695707,0.319434907277248,
11.577668514768));
#30271=CARTESIAN_POINT('Ctrl Pts',(-1.14115313157659,0.636309800095367,
11.6530843128247));
#30272=CARTESIAN_POINT('Ctrl Pts',(-1.14280855344883,0.794772684001041,
11.7173201381379));
#30273=CARTESIAN_POINT('Ctrl Pts',(-1.13081458063189,1.06847604194545,11.810038109084));
#30274=CARTESIAN_POINT('Ctrl Pts',(-1.12363899130074,1.18514270861222,11.8506655484021));
#30275=CARTESIAN_POINT('Ctrl Pts',(-1.11447955905041,1.30000000000055,11.8917862529552));
#30276=CARTESIAN_POINT('Ctrl Pts',(-1.34601296172094,-1.30000000000148,
11.8510707826578));
#30277=CARTESIAN_POINT('Ctrl Pts',(-1.34132286698166,-1.18514270861287,
11.8169387564616));
#30278=CARTESIAN_POINT('Ctrl Pts',(-1.33229750149764,-1.0684760419458,11.7831228063995));
#30279=CARTESIAN_POINT('Ctrl Pts',(-1.30143175902319,-0.794772684001073,
11.705731395999));
#30280=CARTESIAN_POINT('Ctrl Pts',(-1.26715729948021,-0.636309800095377,
11.6502915199856));
#30281=CARTESIAN_POINT('Ctrl Pts',(-1.22185490916071,-0.31943490727725,
11.5899544953272));
#30282=CARTESIAN_POINT('Ctrl Pts',(-1.19616941707238,-0.158333333333377,
11.5623270871317));
#30283=CARTESIAN_POINT('Ctrl Pts',(-1.16909862965114,0.158333333333379,
11.5695937788591));
#30284=CARTESIAN_POINT('Ctrl Pts',(-1.16747959347913,0.319434907277257,
11.6045326774201));
#30285=CARTESIAN_POINT('Ctrl Pts',(-1.15811685224228,0.636309800095386,
11.679580178308));
#30286=CARTESIAN_POINT('Ctrl Pts',(-1.16292009703033,0.794772684001067,
11.7433177695099));
#30287=CARTESIAN_POINT('Ctrl Pts',(-1.1489448495103,1.06847604194549,11.8322318725625));
#30288=CARTESIAN_POINT('Ctrl Pts',(-1.13981020907389,1.18514270861226,11.8705080987032));
#30289=CARTESIAN_POINT('Ctrl Pts',(-1.12759029501853,1.30000000000059,11.9085729303654));
#30290=CARTESIAN_POINT('Ctrl Pts',(-1.36294346109262,-1.30000000000156,
11.8692837620561));
#30291=CARTESIAN_POINT('Ctrl Pts',(-1.36085923751846,-1.18514270861294,
11.8390475820273));
#30292=CARTESIAN_POINT('Ctrl Pts',(-1.35373219611573,-1.06847604194586,
11.8080843650971));
#30293=CARTESIAN_POINT('Ctrl Pts',(-1.32561738671945,-0.794772684001115,
11.7348735391328));
#30294=CARTESIAN_POINT('Ctrl Pts',(-1.29114039687238,-0.63630980009541,
11.6785797244191));
#30295=CARTESIAN_POINT('Ctrl Pts',(-1.24520756634855,-0.319434907277266,
11.6186826600773));
#30296=CARTESIAN_POINT('Ctrl Pts',(-1.21710945792495,-0.158333333333386,
11.5904617895211));
#30297=CARTESIAN_POINT('Ctrl Pts',(-1.18990665017216,0.158333333333388,
11.5977907775527));
#30298=CARTESIAN_POINT('Ctrl Pts',(-1.19077150633563,0.319434907277275,
11.6332977744102));
#30299=CARTESIAN_POINT('Ctrl Pts',(-1.18135618940353,0.636309800095421,
11.7082107659264));
#30300=CARTESIAN_POINT('Ctrl Pts',(-1.185167714955,0.794772684001107,11.7732961672384));
#30301=CARTESIAN_POINT('Ctrl Pts',(-1.16816485771141,1.06847604194554,11.8582057977702));
#30302=CARTESIAN_POINT('Ctrl Pts',(-1.15725060624733,1.18514270861232,11.8936182187079));
#30303=CARTESIAN_POINT('Ctrl Pts',(-1.14278201020198,1.30000000000066,11.9276888277378));
#30304=CARTESIAN_POINT('Ctrl Pts',(-1.38080148305821,-1.30000000000158,
11.8870097673586));
#30305=CARTESIAN_POINT('Ctrl Pts',(-1.38268370064567,-1.18514270861296,
11.8599975752852));
#30306=CARTESIAN_POINT('Ctrl Pts',(-1.37819135820682,-1.06847604194587,
11.8315245282412));
#30307=CARTESIAN_POINT('Ctrl Pts',(-1.35308663959594,-0.794772684001128,
11.7623712263315));
#30308=CARTESIAN_POINT('Ctrl Pts',(-1.31591355523754,-0.636309800095421,
11.7064557387738));
#30309=CARTESIAN_POINT('Ctrl Pts',(-1.26851148105121,-0.319434907277273,
11.6474327241946));
#30310=CARTESIAN_POINT('Ctrl Pts',(-1.23889908635022,-0.158333333333388,
11.6182288910649));
#30311=CARTESIAN_POINT('Ctrl Pts',(-1.21089672311666,0.15833333333339,11.6259113968901));
#30312=CARTESIAN_POINT('Ctrl Pts',(-1.2122289967891,0.319434907277279,11.6628308932153));
#30313=CARTESIAN_POINT('Ctrl Pts',(-1.20315804593487,0.636309800095431,
11.7374350798258));
#30314=CARTESIAN_POINT('Ctrl Pts',(-1.20910091955257,0.794772684001122,
11.8025396611556));
#30315=CARTESIAN_POINT('Ctrl Pts',(-1.1894709900496,1.06847604194556,11.8832732309525));
#30316=CARTESIAN_POINT('Ctrl Pts',(-1.1763930513816,1.18514270861235,11.9159850016308));
#30317=CARTESIAN_POINT('Ctrl Pts',(-1.15873424316685,1.30000000000068,11.9464619720958));
#30318=CARTESIAN_POINT('Ctrl Pts',(-1.40367537834943,-1.30000000000185,
11.9089012603341));
#30319=CARTESIAN_POINT('Ctrl Pts',(-1.40935748512326,-1.18514270861321,
11.8864595634616));
#30320=CARTESIAN_POINT('Ctrl Pts',(-1.40753829200455,-1.0684760419461,11.8613849877698));
#30321=CARTESIAN_POINT('Ctrl Pts',(-1.38600608859034,-0.794772684001295,
11.797375224992));
#30322=CARTESIAN_POINT('Ctrl Pts',(-1.34749195158982,-0.636309800095552,
11.7409488864709));
#30323=CARTESIAN_POINT('Ctrl Pts',(-1.29928584878208,-0.319434907277337,
11.6825333798681));
#30324=CARTESIAN_POINT('Ctrl Pts',(-1.26776917595437,-0.158333333333421,
11.652128053469));
#30325=CARTESIAN_POINT('Ctrl Pts',(-1.23919953259728,0.158333333333423,
11.6600812250877));
#30326=CARTESIAN_POINT('Ctrl Pts',(-1.24175730414977,0.319434907277347,
11.6985117560777));
#30327=CARTESIAN_POINT('Ctrl Pts',(-1.23256199087342,0.636309800095563,
11.7729805746429));
#30328=CARTESIAN_POINT('Ctrl Pts',(-1.23944606917772,0.794772684001284,
11.8388334060565));
#30329=CARTESIAN_POINT('Ctrl Pts',(-1.21591616791004,1.06847604194578,11.9146313246069));
#30330=CARTESIAN_POINT('Ctrl Pts',(-1.20012062657232,1.18514270861259,11.9439876297299));
#30331=CARTESIAN_POINT('Ctrl Pts',(-1.17871476628688,1.30000000000095,11.9698901296249));
#30332=CARTESIAN_POINT('Ctrl Pts',(-1.42403899407475,-1.30000000000203,
11.928642082633));
#30333=CARTESIAN_POINT('Ctrl Pts',(-1.43380199579919,-1.18514270861337,
11.9099752094577));
#30334=CARTESIAN_POINT('Ctrl Pts',(-1.43486664397214,-1.06847604194625,
11.8877166093531));
#30335=CARTESIAN_POINT('Ctrl Pts',(-1.41723125743024,-0.794772684001406,
11.8279971825649));
#30336=CARTESIAN_POINT('Ctrl Pts',(-1.37753694095029,-0.636309800095641,
11.7711162197193));
#30337=CARTESIAN_POINT('Ctrl Pts',(-1.32822206778928,-0.319434907277382,
11.7134532616262));
#30338=CARTESIAN_POINT('Ctrl Pts',(-1.29406704705413,-0.158333333333443,
11.6824351194661));
#30339=CARTESIAN_POINT('Ctrl Pts',(-1.26458135603709,0.158333333333445,
11.6908365801527));
#30340=CARTESIAN_POINT('Ctrl Pts',(-1.26843559089466,0.319434907277389,
11.7305157631943));
#30341=CARTESIAN_POINT('Ctrl Pts',(-1.2593505240363,0.63630980009565,11.8047631456141));
#30342=CARTESIAN_POINT('Ctrl Pts',(-1.26759011506683,0.794772684001396,
11.8710693152954));
#30343=CARTESIAN_POINT('Ctrl Pts',(-1.24048368122056,1.06847604194593,11.9424659259234));
#30344=CARTESIAN_POINT('Ctrl Pts',(-1.22207813922907,1.18514270861276,11.9688815272328));
#30345=CARTESIAN_POINT('Ctrl Pts',(-1.19700042606577,1.30000000000113,11.9908077826161));
#30346=CARTESIAN_POINT('Ctrl Pts',(-1.43801335595633,-1.30000000000206,
11.9415958604667));
#30347=CARTESIAN_POINT('Ctrl Pts',(-1.45045410381386,-1.1851427086134,11.9254578817525));
#30348=CARTESIAN_POINT('Ctrl Pts',(-1.4533968558968,-1.06847604194628,11.9050925216825));
#30349=CARTESIAN_POINT('Ctrl Pts',(-1.43825293159713,-0.794772684001427,
11.8482783692284));
#30350=CARTESIAN_POINT('Ctrl Pts',(-1.39770343358077,-0.63630980009566,
11.7911317326));
#30351=CARTESIAN_POINT('Ctrl Pts',(-1.34753037301524,-0.319434907277392,
11.7340335593344));
#30352=CARTESIAN_POINT('Ctrl Pts',(-1.31138241616195,-0.158333333333447,
11.7027255806159));
#30353=CARTESIAN_POINT('Ctrl Pts',(-1.2815345070826,0.158333333333449,11.7113147339748));
#30354=CARTESIAN_POINT('Ctrl Pts',(-1.28684467285541,0.319434907277397,
11.7515472889145));
#30355=CARTESIAN_POINT('Ctrl Pts',(-1.27823601010953,0.636309800095668,
11.8254577169132));
#30356=CARTESIAN_POINT('Ctrl Pts',(-1.2875886999882,0.79477268400142,11.8919654946004));
#30357=CARTESIAN_POINT('Ctrl Pts',(-1.25784477511212,1.06847604194596,11.9605474333257));
#30358=CARTESIAN_POINT('Ctrl Pts',(-1.23745341248982,1.18514270861279,11.9851188877207));
#30359=CARTESIAN_POINT('Ctrl Pts',(-1.20954573020305,1.30000000000117,12.0045752164476));
#30360=CARTESIAN_POINT('Ctrl Pts',(-1.44396187751701,-1.30000000000207,
11.9469208090408));
#30361=CARTESIAN_POINT('Ctrl Pts',(-1.45765536941502,-1.18514270861341,
11.9317612245756));
#30362=CARTESIAN_POINT('Ctrl Pts',(-1.46144721273248,-1.06847604194628,
11.9121479982828));
#30363=CARTESIAN_POINT('Ctrl Pts',(-1.44733234031239,-0.794772684001432,
11.8565487183647));
#30364=CARTESIAN_POINT('Ctrl Pts',(-1.4060424781856,-0.636309800095663,
11.7994964200841));
#30365=CARTESIAN_POINT('Ctrl Pts',(-1.35553317450774,-0.319434907277393,
11.742630923621));
#30366=CARTESIAN_POINT('Ctrl Pts',(-1.31898795487292,-0.158333333333448,
11.7109906847985));
#30367=CARTESIAN_POINT('Ctrl Pts',(-1.28892906680916,0.15833333333345,11.7196848459155));
#30368=CARTESIAN_POINT('Ctrl Pts',(-1.29444895487496,0.319434907277399,
11.7603361927813));
#30369=CARTESIAN_POINT('Ctrl Pts',(-1.28569904371272,0.636309800095671,
11.8342654713718));
#30370=CARTESIAN_POINT('Ctrl Pts',(-1.29521836752735,0.794772684001424,
11.9009938121065));
#30371=CARTESIAN_POINT('Ctrl Pts',(-1.26446650997392,1.06847604194597,11.9683622590465));
#30372=CARTESIAN_POINT('Ctrl Pts',(-1.2433984560899,1.18514270861279,11.9920964705687));
#30373=CARTESIAN_POINT('Ctrl Pts',(-1.21457368798812,1.30000000000117,12.0104035891798));
#30374=CARTESIAN_POINT('Ctrl Pts',(-1.44878160869613,-1.30000000000208,
11.9511471654546));
#30375=CARTESIAN_POINT('Ctrl Pts',(-1.46353970026319,-1.18514270861342,
11.9367371319072));
#30376=CARTESIAN_POINT('Ctrl Pts',(-1.46804432840997,-1.06847604194629,
11.9177076628513));
#30377=CARTESIAN_POINT('Ctrl Pts',(-1.45476336887771,-0.794772684001439,
11.8630739623605));
#30378=CARTESIAN_POINT('Ctrl Pts',(-1.41275083453451,-0.636309800095669,
11.8061639179291));
#30379=CARTESIAN_POINT('Ctrl Pts',(-1.36196014505706,-0.319434907277397,
11.7494932131841));
#30380=CARTESIAN_POINT('Ctrl Pts',(-1.32517039522566,-0.158333333333449,
11.7175531446848));
#30381=CARTESIAN_POINT('Ctrl Pts',(-1.29497962595988,0.158333333333452,
11.7263151673183));
#30382=CARTESIAN_POINT('Ctrl Pts',(-1.30068393443965,0.319434907277402,
11.7672942672444));
#30383=CARTESIAN_POINT('Ctrl Pts',(-1.29180058335059,0.636309800095677,
11.8412483342407));
#30384=CARTESIAN_POINT('Ctrl Pts',(-1.30139627601783,0.794772684001432,
11.9081786650871));
#30385=CARTESIAN_POINT('Ctrl Pts',(-1.26979718785685,1.06847604194598,11.9745958920687));
#30386=CARTESIAN_POINT('Ctrl Pts',(-1.2481741555375,1.18514270861281,11.9976671741239));
#30387=CARTESIAN_POINT('Ctrl Pts',(-1.21860616530208,1.30000000000119,12.0150601816748));
#30388=CARTESIAN_POINT('Ctrl Pts',(-1.45176259299563,-1.30000000000209,
11.9538042732137));
#30389=CARTESIAN_POINT('Ctrl Pts',(-1.46715758972206,-1.18514270861342,
11.9398775948973));
#30390=CARTESIAN_POINT('Ctrl Pts',(-1.47209725699402,-1.0684760419463,11.9212184413938));
#30391=CARTESIAN_POINT('Ctrl Pts',(-1.45935497394801,-0.794772684001442,
11.867179099639));
#30392=CARTESIAN_POINT('Ctrl Pts',(-1.41699570354255,-0.636309800095672,
11.8103031424495));
#30393=CARTESIAN_POINT('Ctrl Pts',(-1.36604424570276,-0.319434907277398,
11.7537462514445));
#30394=CARTESIAN_POINT('Ctrl Pts',(-1.32902683726316,-0.15833333333345,
11.7216575833153));
#30395=CARTESIAN_POINT('Ctrl Pts',(-1.29874790973121,0.158333333333452,
11.7304654392766));
#30396=CARTESIAN_POINT('Ctrl Pts',(-1.30460577039528,0.319434907277404,
11.7716298189423));
#30397=CARTESIAN_POINT('Ctrl Pts',(-1.29567499303704,0.63630980009568,11.8455820758332));
#30398=CARTESIAN_POINT('Ctrl Pts',(-1.30536656523558,0.794772684001435,
11.9126164899123));
#30399=CARTESIAN_POINT('Ctrl Pts',(-1.27321744712993,1.06847604194598,11.9784488600289));
#30400=CARTESIAN_POINT('Ctrl Pts',(-1.25122125180277,1.18514270861281,12.0011181309178));
#30401=CARTESIAN_POINT('Ctrl Pts',(-1.22114502313416,1.30000000000119,12.0179602790019));
#30402=CARTESIAN_POINT('Ctrl Pts',(-1.45412628658392,-1.30000000000209,
11.9559408461953));
#30403=CARTESIAN_POINT('Ctrl Pts',(-1.47000738429716,-1.18514270861343,
11.9424131581336));
#30404=CARTESIAN_POINT('Ctrl Pts',(-1.47528578223223,-1.0684760419463,11.9240551310158));
#30405=CARTESIAN_POINT('Ctrl Pts',(-1.46298557985177,-0.794772684001444,
11.8704853663371));
#30406=CARTESIAN_POINT('Ctrl Pts',(-1.42043011327194,-0.636309800095673,
11.8135940727104));
#30407=CARTESIAN_POINT('Ctrl Pts',(-1.3693582354536,-0.319434907277399,
11.7571235736978));
#30408=CARTESIAN_POINT('Ctrl Pts',(-1.33209230895348,-0.15833333333345,
11.7249498649193));
#30409=CARTESIAN_POINT('Ctrl Pts',(-1.30174447208215,0.158333333333453,
11.7337942228324));
#30410=CARTESIAN_POINT('Ctrl Pts',(-1.30777075626328,0.319434907277404,
11.7750844319782));
#30411=CARTESIAN_POINT('Ctrl Pts',(-1.29884281897625,0.636309800095681,
11.8490159166609));
#30412=CARTESIAN_POINT('Ctrl Pts',(-1.30865687160089,0.794772684001436,
11.9161124935271));
#30413=CARTESIAN_POINT('Ctrl Pts',(-1.27604818827047,1.06847604194599,11.9814861394346));
#30414=CARTESIAN_POINT('Ctrl Pts',(-1.25372777969796,1.18514270861281,12.0038457928843));
#30415=CARTESIAN_POINT('Ctrl Pts',(-1.22320205329589,1.30000000000119,12.0202672708026));
#30416=CARTESIAN_POINT('Ctrl Pts',(-1.45559309281896,-1.30000000000209,
11.9572815917638));
#30417=CARTESIAN_POINT('Ctrl Pts',(-1.47176684857772,-1.18514270861343,
11.9440091015764));
#30418=CARTESIAN_POINT('Ctrl Pts',(-1.47725243245924,-1.0684760419463,11.9258416345089));
#30419=CARTESIAN_POINT('Ctrl Pts',(-1.46523341341502,-0.794772684001445,
11.8725627753639));
#30420=CARTESIAN_POINT('Ctrl Pts',(-1.42259258598767,-0.636309800095674,
11.8156424353714));
#30421=CARTESIAN_POINT('Ctrl Pts',(-1.37145024444862,-0.319434907277399,
11.7592232784206));
#30422=CARTESIAN_POINT('Ctrl Pts',(-1.3340014901361,-0.158333333333451,
11.7270104289212));
#30423=CARTESIAN_POINT('Ctrl Pts',(-1.30360964329911,0.158333333333453,
11.7358782684999));
#30424=CARTESIAN_POINT('Ctrl Pts',(-1.30975675245054,0.319434907277405,
11.7772393990036));
#30425=CARTESIAN_POINT('Ctrl Pts',(-1.30084628394672,0.636309800095682,
11.8511504676796));
#30426=CARTESIAN_POINT('Ctrl Pts',(-1.31075692417128,0.794772684001437,
11.9182766599752));
#30427=CARTESIAN_POINT('Ctrl Pts',(-1.27785446166952,1.06847604194599,11.9833667142888));
#30428=CARTESIAN_POINT('Ctrl Pts',(-1.2553216991526,1.18514270861281,12.0055374169981));
#30429=CARTESIAN_POINT('Ctrl Pts',(-1.22449843097937,1.3000000000012,12.0217037497287));
#30430=CARTESIAN_POINT('Ctrl Pts',(-1.45676183409782,-1.30000000000209,
11.9583565852924));
#30431=CARTESIAN_POINT('Ctrl Pts',(-1.47316443878281,-1.18514270861343,
11.9452909967571));
#30432=CARTESIAN_POINT('Ctrl Pts',(-1.47881367935989,-1.0684760419463,11.9272770581855));
#30433=CARTESIAN_POINT('Ctrl Pts',(-1.46702213292725,-0.794772684001445,
11.8742295779112));
#30434=CARTESIAN_POINT('Ctrl Pts',(-1.42433097171468,-0.636309800095674,
11.8172766283104));
#30435=CARTESIAN_POINT('Ctrl Pts',(-1.37313484211759,-0.319434907277399,
11.7608971357158));
#30436=CARTESIAN_POINT('Ctrl Pts',(-1.33552682586702,-0.158333333333451,
11.728659596914));
#30437=CARTESIAN_POINT('Ctrl Pts',(-1.3050996718648,0.158333333333453,11.7375463919935));
#30438=CARTESIAN_POINT('Ctrl Pts',(-1.31135108710863,0.319434907277405,
11.7789604974073));
#30439=CARTESIAN_POINT('Ctrl Pts',(-1.30246251145676,0.636309800095682,
11.8528515079605));
#30440=CARTESIAN_POINT('Ctrl Pts',(-1.31246056688986,0.794772684001438,
11.9199967060572));
#30441=CARTESIAN_POINT('Ctrl Pts',(-1.27931974389209,1.06847604194599,11.9848614994968));
#30442=CARTESIAN_POINT('Ctrl Pts',(-1.25661216601513,1.18514270861282,12.0068833729769));
#30443=CARTESIAN_POINT('Ctrl Pts',(-1.22554244454843,1.3000000000012,12.0228495543345));
#30444=CARTESIAN_POINT('Ctrl Pts',(-1.4576362468158,-1.3000000000021,11.959163908753));
#30445=CARTESIAN_POINT('Ctrl Pts',(-1.4742081978252,-1.18514270861343,11.9462546785736));
#30446=CARTESIAN_POINT('Ctrl Pts',(-1.4799792929871,-1.0684760419463,11.9283563400937));
#30447=CARTESIAN_POINT('Ctrl Pts',(-1.46835953960324,-0.794772684001445,
11.8754817594131));
#30448=CARTESIAN_POINT('Ctrl Pts',(-1.42563846320108,-0.636309800095674,
11.8185002733194));
#30449=CARTESIAN_POINT('Ctrl Pts',(-1.37440343715322,-0.319434907277399,
11.7621497596797));
#30450=CARTESIAN_POINT('Ctrl Pts',(-1.33667091322058,-0.158333333333451,
11.7298962906598));
#30451=CARTESIAN_POINT('Ctrl Pts',(-1.30621714597304,0.158333333333453,
11.7387974184199));
#30452=CARTESIAN_POINT('Ctrl Pts',(-1.31254933061953,0.319434907277405,
11.7802500019729));
#30453=CARTESIAN_POINT('Ctrl Pts',(-1.30368032461536,0.636309800095682,
11.8541244943568));
#30454=CARTESIAN_POINT('Ctrl Pts',(-1.31374852051673,0.794772684001438,
11.9212818216884));
#30455=CARTESIAN_POINT('Ctrl Pts',(-1.28042768257437,1.06847604194599,11.9859782900626));
#30456=CARTESIAN_POINT('Ctrl Pts',(-1.25758697978893,1.18514270861282,12.0078895053538));
#30457=CARTESIAN_POINT('Ctrl Pts',(-1.22632893030456,1.3000000000012,12.0237072320175));
#30458=CARTESIAN_POINT('Ctrl Pts',(-1.45836365863242,-1.3000000000021,11.9598373036628));
#30459=CARTESIAN_POINT('Ctrl Pts',(-1.47507522896852,-1.18514270861343,
11.9470591421206));
#30460=CARTESIAN_POINT('Ctrl Pts',(-1.48094730564884,-1.0684760419463,11.9292574217479));
#30461=CARTESIAN_POINT('Ctrl Pts',(-1.46947157870716,-0.794772684001446,
11.8765264606078));
#30462=CARTESIAN_POINT('Ctrl Pts',(-1.42673088476929,-0.636309800095674,
11.819518434425));
#30463=CARTESIAN_POINT('Ctrl Pts',(-1.37546443483945,-0.319434907277399,
11.7631915487841));
#30464=CARTESIAN_POINT('Ctrl Pts',(-1.33762471405457,-0.158333333333451,
11.7309265675717));
#30465=CARTESIAN_POINT('Ctrl Pts',(-1.30714867482229,0.158333333333453,
11.7398397251137));
#30466=CARTESIAN_POINT('Ctrl Pts',(-1.31354993392347,0.319434907277405,
11.7813235032592));
#30467=CARTESIAN_POINT('Ctrl Pts',(-1.30469927152157,0.636309800095682,
11.8551832836116));
#30468=CARTESIAN_POINT('Ctrl Pts',(-1.31482873251949,0.794772684001438,
11.922349417857));
#30469=CARTESIAN_POINT('Ctrl Pts',(-1.28135710266374,1.06847604194599,11.9869060154245));
#30470=CARTESIAN_POINT('Ctrl Pts',(-1.2584042056035,1.18514270861282,12.0087256230431));
#30471=CARTESIAN_POINT('Ctrl Pts',(-1.22698703980146,1.3000000000012,12.0244206792509));
#30472=CARTESIAN_POINT('Ctrl Pts',(-1.45887229050876,-1.3000000000021,11.9603089447196));
#30473=CARTESIAN_POINT('Ctrl Pts',(-1.47568111425946,-1.18514270861343,
11.9476227686205));
#30474=CARTESIAN_POINT('Ctrl Pts',(-1.4816237270335,-1.0684760419463,11.9298887510696));
#30475=CARTESIAN_POINT('Ctrl Pts',(-1.47024923022303,-0.794772684001445,
11.8772580992783));
#30476=CARTESIAN_POINT('Ctrl Pts',(-1.42749660001604,-0.636309800095674,
11.8202305657825));
#30477=CARTESIAN_POINT('Ctrl Pts',(-1.37620887221738,-0.319434907277399,
11.7639198533448));
#30478=CARTESIAN_POINT('Ctrl Pts',(-1.33829358685617,-0.158333333333451,
11.7316470933858));
#30479=CARTESIAN_POINT('Ctrl Pts',(-1.3078020088344,0.158333333333453,11.7405686639439));
#30480=CARTESIAN_POINT('Ctrl Pts',(-1.31425157265155,0.319434907277405,
11.7820743088889));
#30481=CARTESIAN_POINT('Ctrl Pts',(-1.30541441170054,0.636309800095682,
11.8559234931048));
#30482=CARTESIAN_POINT('Ctrl Pts',(-1.31558828822311,0.794772684001438,
11.9230950654863));
#30483=CARTESIAN_POINT('Ctrl Pts',(-1.28201086412561,1.06847604194599,11.9875538956265));
#30484=CARTESIAN_POINT('Ctrl Pts',(-1.25897891196976,1.18514270861282,12.0093096412464));
#30485=CARTESIAN_POINT('Ctrl Pts',(-1.22744943038369,1.3000000000012,12.0249192933534));
#30486=CARTESIAN_POINT('Ctrl Pts',(-1.45916293603873,-1.3000000000021,11.9605784516738));
#30487=CARTESIAN_POINT('Ctrl Pts',(-1.47602712731174,-1.18514270861343,
11.9479449470715));
#30488=CARTESIAN_POINT('Ctrl Pts',(-1.4820099641168,-1.0684760419463,11.9302496611076));
#30489=CARTESIAN_POINT('Ctrl Pts',(-1.47069340837042,-0.794772684001446,
11.8776762830501));
#30490=CARTESIAN_POINT('Ctrl Pts',(-1.42793473453064,-0.636309800095675,
11.8206372037096));
#30491=CARTESIAN_POINT('Ctrl Pts',(-1.3766347835925,-0.319434907277399,
11.7643357655358));
#30492=CARTESIAN_POINT('Ctrl Pts',(-1.33867549238525,-0.158333333333451,
11.7320589818148));
#30493=CARTESIAN_POINT('Ctrl Pts',(-1.30817489300452,0.158333333333453,
11.7409854326848));
#30494=CARTESIAN_POINT('Ctrl Pts',(-1.31465257256766,0.319434907277405,
11.7825033107204));
#30495=CARTESIAN_POINT('Ctrl Pts',(-1.30582325002853,0.636309800095683,
11.8563463805486));
#30496=CARTESIAN_POINT('Ctrl Pts',(-1.31602229180613,0.794772684001438,
11.9235211783992));
#30497=CARTESIAN_POINT('Ctrl Pts',(-1.28238440586926,1.06847604194599,11.9879241441032));
#30498=CARTESIAN_POINT('Ctrl Pts',(-1.25930730372606,1.18514270861282,12.0096433818638));
#30499=CARTESIAN_POINT('Ctrl Pts',(-1.22771369385523,1.3000000000012,12.025204199897));
#30500=CARTESIAN_POINT('Ctrl Pts',(-1.46859907610557,-1.30000000000203,
11.9693420881502));
#30501=CARTESIAN_POINT('Ctrl Pts',(-1.48726728132861,-1.18514270861337,
11.9584176006989));
#30502=CARTESIAN_POINT('Ctrl Pts',(-1.49456034141824,-1.06847604194625,
11.9419792378749));
#30503=CARTESIAN_POINT('Ctrl Pts',(-1.48512990834886,-0.794772684001404,
11.8912651761098));
#30504=CARTESIAN_POINT('Ctrl Pts',(-1.44215958086142,-0.636309800095641,
11.8338586014427));
#30505=CARTESIAN_POINT('Ctrl Pts',(-1.3904826145155,-0.319434907277382,
11.777848370173));
#30506=CARTESIAN_POINT('Ctrl Pts',(-1.35113949190814,-0.158333333333443,
11.7454174913081));
#30507=CARTESIAN_POINT('Ctrl Pts',(-1.32035617945323,0.158333333333445,
11.7544976139884));
#30508=CARTESIAN_POINT('Ctrl Pts',(-1.3277105057882,0.319434907277389,11.796432143158));
#30509=CARTESIAN_POINT('Ctrl Pts',(-1.31913956487404,0.636309800095649,
11.8700752352614));
#30510=CARTESIAN_POINT('Ctrl Pts',(-1.33020018471009,0.794772684001394,
11.9373330247913));
#30511=CARTESIAN_POINT('Ctrl Pts',(-1.29459393804896,1.06847604194593,11.999922806806));
#30512=CARTESIAN_POINT('Ctrl Pts',(-1.27003842655761,1.18514270861275,12.0204614781535));
#30513=CARTESIAN_POINT('Ctrl Pts',(-1.23634002841306,1.30000000000113,12.0344460233943));
#30514=CARTESIAN_POINT('Ctrl Pts',(-1.48344548007622,-1.30000000000141,
11.9818935927946));
#30515=CARTESIAN_POINT('Ctrl Pts',(-1.50529278229764,-1.18514270861281,
11.9732243738687));
#30516=CARTESIAN_POINT('Ctrl Pts',(-1.51477839333627,-1.06847604194574,
11.9585096316802));
#30517=CARTESIAN_POINT('Ctrl Pts',(-1.50813407284541,-0.794772684001029,
11.9105492654116));
#30518=CARTESIAN_POINT('Ctrl Pts',(-1.46364588916581,-0.636309800095337,
11.8532367545533));
#30519=CARTESIAN_POINT('Ctrl Pts',(-1.41117822787962,-0.319434907277229,
11.7977990691333));
#30520=CARTESIAN_POINT('Ctrl Pts',(-1.37050240246276,-0.158333333333367,
11.7647942347192));
#30521=CARTESIAN_POINT('Ctrl Pts',(-1.33921855852028,0.15833333333337,11.7741509880921));
#30522=CARTESIAN_POINT('Ctrl Pts',(-1.34760773600743,0.319434907277239,
11.8168336365887));
#30523=CARTESIAN_POINT('Ctrl Pts',(-1.33839509921198,0.636309800095348,
11.8906763773722));
#30524=CARTESIAN_POINT('Ctrl Pts',(-1.34861122908608,0.794772684001016,
11.9590558215034));
#30525=CARTESIAN_POINT('Ctrl Pts',(-1.31066005266653,1.06847604194542,12.0187173448594));
#30526=CARTESIAN_POINT('Ctrl Pts',(-1.28480044480139,1.18514270861219,12.0371059865518));
#30527=CARTESIAN_POINT('Ctrl Pts',(-1.24950888711346,1.30000000000051,12.0480580071529));
#30528=CARTESIAN_POINT('Ctrl Pts',(-1.50230543268038,-1.3000000000014,11.9989352575912));
#30529=CARTESIAN_POINT('Ctrl Pts',(-1.52838553185008,-1.1851427086128,11.9932437652798));
#30530=CARTESIAN_POINT('Ctrl Pts',(-1.54081146658877,-1.06847604194573,
11.9807964322698));
#30531=CARTESIAN_POINT('Ctrl Pts',(-1.537974010293,-0.794772684001022,11.9364332594215));
#30532=CARTESIAN_POINT('Ctrl Pts',(-1.49159955480665,-0.636309800095334,
11.8791998869732));
#30533=CARTESIAN_POINT('Ctrl Pts',(-1.43824443615658,-0.319434907277227,
11.8244360270167));
#30534=CARTESIAN_POINT('Ctrl Pts',(-1.39578979224414,-0.158333333333366,
11.7906539395304));
#30535=CARTESIAN_POINT('Ctrl Pts',(-1.36413285231675,0.158333333333369,
11.8002225466957));
#30536=CARTESIAN_POINT('Ctrl Pts',(-1.37377190540379,0.319434907277236,
11.8439539537967));
#30537=CARTESIAN_POINT('Ctrl Pts',(-1.36500420525066,0.636309800095344,
11.9174328937395));
#30538=CARTESIAN_POINT('Ctrl Pts',(-1.37741180114805,0.794772684001012,
11.9857353250915));
#30539=CARTESIAN_POINT('Ctrl Pts',(-1.33520760996577,1.06847604194542,12.0420131895444));
#30540=CARTESIAN_POINT('Ctrl Pts',(-1.30610077108674,1.18514270861218,12.0582428261529));
#30541=CARTESIAN_POINT('Ctrl Pts',(-1.26615572387209,1.3000000000005,12.0663414971487));
#30542=CARTESIAN_POINT('Ctrl Pts',(-1.51240241427839,-1.30000000000112,
12.007106984072));
#30543=CARTESIAN_POINT('Ctrl Pts',(-1.54036079622444,-1.18514270861254,
12.0030164794702));
#30544=CARTESIAN_POINT('Ctrl Pts',(-1.5541361931653,-1.0684760419455,11.9917560436576));
#30545=CARTESIAN_POINT('Ctrl Pts',(-1.55319458319894,-0.794772684000851,
11.9491782088514));
#30546=CARTESIAN_POINT('Ctrl Pts',(-1.50638430478292,-0.636309800095196,
11.8917068361181));
#30547=CARTESIAN_POINT('Ctrl Pts',(-1.45275981718469,-0.319434907277159,
11.8371994262208));
#30548=CARTESIAN_POINT('Ctrl Pts',(-1.40945018590222,-0.158333333333332,
11.8030474555539));
#30549=CARTESIAN_POINT('Ctrl Pts',(-1.37727481249132,0.158333333333334,
11.8129044039714));
#30550=CARTESIAN_POINT('Ctrl Pts',(-1.3870306215781,0.319434907277167,11.8574095495264));
#30551=CARTESIAN_POINT('Ctrl Pts',(-1.37792399116514,0.636309800095206,
11.9309840760347));
#30552=CARTESIAN_POINT('Ctrl Pts',(-1.39070615145891,0.79477268400084,11.9995754377232));
#30553=CARTESIAN_POINT('Ctrl Pts',(-1.34687223012689,1.06847604194519,12.0539531416098));
#30554=CARTESIAN_POINT('Ctrl Pts',(-1.31666175922729,1.18514270861193,12.0688762002392));
#30555=CARTESIAN_POINT('Ctrl Pts',(-1.27521489776587,1.30000000000022,12.075184224378));
#30556=CARTESIAN_POINT('Ctrl Pts',(-1.51741227377083,-1.30000000000112,
12.0112098547444));
#30557=CARTESIAN_POINT('Ctrl Pts',(-1.54630261814581,-1.18514270861254,
12.0079231435191));
#30558=CARTESIAN_POINT('Ctrl Pts',(-1.56074958986041,-1.0684760419455,11.99725764633));
#30559=CARTESIAN_POINT('Ctrl Pts',(-1.56075790439565,-0.794772684000851,
11.9555717425004));
#30560=CARTESIAN_POINT('Ctrl Pts',(-1.51378858280601,-0.636309800095196,
11.8979534138563));
#30561=CARTESIAN_POINT('Ctrl Pts',(-1.45995892423166,-0.319434907277159,
11.8436091949709));
#30562=CARTESIAN_POINT('Ctrl Pts',(-1.41600270611002,-0.158333333333332,
11.8093804181447));
#30563=CARTESIAN_POINT('Ctrl Pts',(-1.38362278588542,0.158333333333334,
11.8193529279827));
#30564=CARTESIAN_POINT('Ctrl Pts',(-1.39375448302884,0.319434907277167,
11.8640850863445));
#30565=CARTESIAN_POINT('Ctrl Pts',(-1.38457112325774,0.636309800095206,
11.9376612423013));
#30566=CARTESIAN_POINT('Ctrl Pts',(-1.39741805963304,0.79477268400084,12.0064627225285));
#30567=CARTESIAN_POINT('Ctrl Pts',(-1.3526706067805,1.06847604194519,12.0599359626955));
#30568=CARTESIAN_POINT('Ctrl Pts',(-1.32185850051433,1.18514270861193,12.0742273399833));
#30569=CARTESIAN_POINT('Ctrl Pts',(-1.27960380226532,1.30000000000022,12.0796635102695));
#30570=CARTESIAN_POINT('',(-1.2373438536101,1.2,11.9928572050431));
#30571=CARTESIAN_POINT('Ctrl Pts',(-1.2373438536101,1.2,11.9928572050431));
#30572=CARTESIAN_POINT('Ctrl Pts',(-1.22007242234924,1.21680886307926,11.9799560961046));
#30573=CARTESIAN_POINT('Ctrl Pts',(-1.20198017112036,1.23320396068793,11.9676320090486));
#30574=CARTESIAN_POINT('Ctrl Pts',(-1.17510185254842,1.25911304880667,11.9476275708389));
#30575=CARTESIAN_POINT('Ctrl Pts',(-1.15950113852676,1.27356500001449,11.9366232467277));
#30576=CARTESIAN_POINT('Ctrl Pts',(-1.13329432476672,1.3,11.9157336622684));
#30577=CARTESIAN_POINT('',(-1.38832547963881,0.653834841382538,11.9513211175694));
#30578=CARTESIAN_POINT('Ctrl Pts',(-1.38832547962899,0.653834841377511,
11.9513211176064));
#30579=CARTESIAN_POINT('Ctrl Pts',(-1.37327925638861,0.715637047620691,
11.9557175906252));
#30580=CARTESIAN_POINT('Ctrl Pts',(-1.35934876819983,0.767437339736555,
11.9597189842502));
#30581=CARTESIAN_POINT('Ctrl Pts',(-1.32827629350109,0.882054338936367,
11.9684850281746));
#30582=CARTESIAN_POINT('Ctrl Pts',(-1.31342061390376,0.939294188357158,
11.9726076783957));
#30583=CARTESIAN_POINT('Ctrl Pts',(-1.28552565669992,1.03700621393207,11.9801698223984));
#30584=CARTESIAN_POINT('Ctrl Pts',(-1.28427849821935,1.04065632268877,11.9805295350603));
#30585=CARTESIAN_POINT('Ctrl Pts',(-1.2563560598427,1.13599421849374,11.9879204304765));
#30586=CARTESIAN_POINT('Ctrl Pts',(-1.24755393031006,1.16618572853348,11.9902213293829));
#30587=CARTESIAN_POINT('Ctrl Pts',(-1.2373438536101,1.2,11.9928572050431));
#30588=CARTESIAN_POINT('',(-1.52166805320966,-0.653834841531101,11.9103106411192));
#30589=CARTESIAN_POINT('Ctrl Pts',(-1.52166805320967,-0.653834841531079,
11.9103106411192));
#30590=CARTESIAN_POINT('Ctrl Pts',(-1.49332370940493,-0.575726829001172,
11.8797128649133));
#30591=CARTESIAN_POINT('Ctrl Pts',(-1.46878742733875,-0.493694691894675,
11.8546066668147));
#30592=CARTESIAN_POINT('Ctrl Pts',(-1.43181654628555,-0.338084133530092,
11.8199726365178));
#30593=CARTESIAN_POINT('Ctrl Pts',(-1.4178771777781,-0.26562576409014,11.8086841555559));
#30594=CARTESIAN_POINT('Ctrl Pts',(-1.3965041256658,-0.129694174089561,
11.7968486800664));
#30595=CARTESIAN_POINT('Ctrl Pts',(-1.38847548152787,-0.0666412200678742,
11.794956151289));
#30596=CARTESIAN_POINT('Ctrl Pts',(-1.37567108574927,0.0594771285402088,
11.7985011872496));
#30597=CARTESIAN_POINT('Ctrl Pts',(-1.37080511110895,0.122680285497012,
11.8039458214053));
#30598=CARTESIAN_POINT('Ctrl Pts',(-1.36460604093124,0.260050375630151,
11.8236401506711));
#30599=CARTESIAN_POINT('Ctrl Pts',(-1.36403934238603,0.333912938648628,
11.8393326465065));
#30600=CARTESIAN_POINT('Ctrl Pts',(-1.36976405159761,0.491493501735914,
11.8838745599282));
#30601=CARTESIAN_POINT('Ctrl Pts',(-1.37696041957445,0.574885173904325,
11.914805991444));
#30602=CARTESIAN_POINT('Ctrl Pts',(-1.38832547957248,0.653834841398299,
11.9513211175559));
#30603=CARTESIAN_POINT('',(-1.45267111627981,-1.2,11.9320446561636));
#30604=CARTESIAN_POINT('Ctrl Pts',(-1.45267111627981,-1.2,11.9320446561636));
#30605=CARTESIAN_POINT('Ctrl Pts',(-1.46243409420727,-1.14592853623335,
11.9290475593324));
#30606=CARTESIAN_POINT('Ctrl Pts',(-1.47710331673422,-1.06261597021533,
11.9245259227913));
#30607=CARTESIAN_POINT('Ctrl Pts',(-1.50949341520291,-0.803846334503223,
11.9142418008359));
#30608=CARTESIAN_POINT('Ctrl Pts',(-1.51508125140246,-0.746395744507367,
11.9124385105203));
#30609=CARTESIAN_POINT('Ctrl Pts',(-1.52166805320967,-0.653834841531101,
11.9103106411192));
#30610=CARTESIAN_POINT('Ctrl Pts',(-1.35212230766396,-1.30000000000011,
11.857710302833));
#30611=CARTESIAN_POINT('Ctrl Pts',(-1.36853533305804,-1.28287864461177,
11.8707738366094));
#30612=CARTESIAN_POINT('Ctrl Pts',(-1.38567851507679,-1.26604242834882,
11.88327852373));
#30613=CARTESIAN_POINT('Ctrl Pts',(-1.42483729732607,-1.22709161555245,
11.9122329332583));
#30614=CARTESIAN_POINT('Ctrl Pts',(-1.43804978907626,-1.21370565301587,
11.9221962700843));
#30615=CARTESIAN_POINT('Ctrl Pts',(-1.45267111627981,-1.2,11.9320446561636));
#30616=CARTESIAN_POINT('Origin',(0.,1.25,7.2));
#30617=CARTESIAN_POINT('',(-0.213828345914065,1.2,12.1453794028855));
#30618=CARTESIAN_POINT('Origin',(0.,1.2,7.2));
#30619=CARTESIAN_POINT('Ctrl Pts',(-0.213828345914065,1.2,12.1453794028855));
#30620=CARTESIAN_POINT('Ctrl Pts',(-0.195742251015914,1.22112918552691,
12.1250124824944));
#30621=CARTESIAN_POINT('Ctrl Pts',(-0.177075057844756,1.24197036598625,
12.1048648021315));
#30622=CARTESIAN_POINT('Ctrl Pts',(-0.148630873366042,1.27532127191025,
12.0724226989563));
#30623=CARTESIAN_POINT('Ctrl Pts',(-0.138144362293013,1.28756858937727,
12.0604782373989));
#30624=CARTESIAN_POINT('Ctrl Pts',(-0.128158081937606,1.2999999999995,12.0483064575209));
#30625=CARTESIAN_POINT('Origin',(0.,0.92691742076555,7.2));
#30626=CARTESIAN_POINT('',(-0.370132012290736,0.653834841366703,12.1361424506498));
#30627=CARTESIAN_POINT('Origin',(0.,0.653834841531101,7.2));
#30628=CARTESIAN_POINT('Ctrl Pts',(-0.370132012288497,0.653834841365421,
12.1361424506875));
#30629=CARTESIAN_POINT('Ctrl Pts',(-0.354138141111788,0.717049709819526,
12.1373417361178));
#30630=CARTESIAN_POINT('Ctrl Pts',(-0.332832873908772,0.792929369312527,
12.1388326360144));
#30631=CARTESIAN_POINT('Ctrl Pts',(-0.30692609112432,0.885929226741259,
12.1404808169553));
#30632=CARTESIAN_POINT('Ctrl Pts',(-0.300394671658448,0.909292265434727,
12.1408823708037));
#30633=CARTESIAN_POINT('Ctrl Pts',(-0.267850169499559,1.02405695792837,
12.1428118183178));
#30634=CARTESIAN_POINT('Ctrl Pts',(-0.241222096346408,1.1121531011995,12.1441949517309));
#30635=CARTESIAN_POINT('Ctrl Pts',(-0.213828345914064,1.2,12.1453794028854));
#30636=CARTESIAN_POINT('Origin',(0.,0.,7.2));
#30637=CARTESIAN_POINT('',(-0.509087305688324,-0.653834841531101,12.1237516301279));
#30638=CARTESIAN_POINT('Origin',(0.,-0.653834841531101,7.2));
#30639=CARTESIAN_POINT('Ctrl Pts',(-0.509087305688305,-0.65383484153111,
12.1237516301279));
#30640=CARTESIAN_POINT('Ctrl Pts',(-0.487796603721125,-0.575992320405206,
12.0880511292075));
#30641=CARTESIAN_POINT('Ctrl Pts',(-0.469123782926452,-0.493632669726353,
12.05824203318));
#30642=CARTESIAN_POINT('Ctrl Pts',(-0.440222124607192,-0.338115839260951,
12.0166878970055));
#30643=CARTESIAN_POINT('Ctrl Pts',(-0.42902720878148,-0.265637866641146,
12.0027380166553));
#30644=CARTESIAN_POINT('Ctrl Pts',(-0.410675091361661,-0.129696817563903,
11.9867099771911));
#30645=CARTESIAN_POINT('Ctrl Pts',(-0.403190326971112,-0.0666113386779936,
11.9831897465878));
#30646=CARTESIAN_POINT('Ctrl Pts',(-0.389888857045734,0.0595467574157433,
11.9840034138292));
#30647=CARTESIAN_POINT('Ctrl Pts',(-0.38397462719954,0.122772045581972,
11.9883261664178));
#30648=CARTESIAN_POINT('Ctrl Pts',(-0.373658687761304,0.260120772719706,
12.0063186578358));
#30649=CARTESIAN_POINT('Ctrl Pts',(-0.369728507767857,0.33394176338759,
12.0215544969233));
#30650=CARTESIAN_POINT('Ctrl Pts',(-0.365884250931941,0.49120341452778,
12.0662377985978));
#30651=CARTESIAN_POINT('Ctrl Pts',(-0.366579556882535,0.574345839355596,
12.0978024686969));
#30652=CARTESIAN_POINT('Ctrl Pts',(-0.370132012239985,0.653834841383583,
12.1361424506195));
#30653=CARTESIAN_POINT('Origin',(0.,-0.926917420765551,7.2));
#30654=CARTESIAN_POINT('',(-0.437059572605786,-1.2,12.1306671891331));
#30655=CARTESIAN_POINT('Origin',(0.,-1.2,7.2));
#30656=CARTESIAN_POINT('Ctrl Pts',(-0.43705957260579,-1.2,12.1306671891331));
#30657=CARTESIAN_POINT('Ctrl Pts',(-0.449850978802582,-1.13143558342973,
12.1295333453122));
#30658=CARTESIAN_POINT('Ctrl Pts',(-0.463535154438354,-1.05442944320354,
12.1282924278181));
#30659=CARTESIAN_POINT('Ctrl Pts',(-0.497848612890372,-0.79255450235333,
12.1249197851749));
#30660=CARTESIAN_POINT('Ctrl Pts',(-0.50276625626291,-0.738810704696317,
12.1244051899056));
#30661=CARTESIAN_POINT('Ctrl Pts',(-0.509087305688302,-0.6538348415311,
12.1237516301279));
#30662=CARTESIAN_POINT('Origin',(0.,-1.25,7.2));
#30663=CARTESIAN_POINT('Ctrl Pts',(-0.354232945953443,-1.3,12.0370465182796));
#30664=CARTESIAN_POINT('Ctrl Pts',(-0.369830978971964,-1.27998847667344,
12.0559693362845));
#30665=CARTESIAN_POINT('Ctrl Pts',(-0.383310654693955,-1.26450440150284,
12.0704526234879));
#30666=CARTESIAN_POINT('Ctrl Pts',(-0.410365222815302,-1.23095282611831,
12.1019135168529));
#30667=CARTESIAN_POINT('Ctrl Pts',(-0.423468395372474,-1.21538387848804,
12.1164277278777));
#30668=CARTESIAN_POINT('Ctrl Pts',(-0.43705957260579,-1.2,12.1306671891331));
#30669=CARTESIAN_POINT('Ctrl Pts',(-1.83297302538937,-1.30000000000171,
11.8998629503917));
#30670=CARTESIAN_POINT('Ctrl Pts',(-1.7955929556911,-1.18514270861294,11.9203016847184));
#30671=CARTESIAN_POINT('Ctrl Pts',(-1.76226517728477,-1.0684760419457,11.9268506192756));
#30672=CARTESIAN_POINT('Ctrl Pts',(-1.69463294550958,-0.794772684000851,
11.9098917521005));
#30673=CARTESIAN_POINT('Ctrl Pts',(-1.66458583994784,-0.636309800095197,
11.8466789456163));
#30674=CARTESIAN_POINT('Ctrl Pts',(-1.61390936643532,-0.319434907277159,
11.7925524285052));
#30675=CARTESIAN_POINT('Ctrl Pts',(-1.59581317861837,-0.158333333333332,
11.750408090035));
#30676=CARTESIAN_POINT('Ctrl Pts',(-1.56375557866912,0.158333333333334,
11.761372599678));
#30677=CARTESIAN_POINT('Ctrl Pts',(-1.54831342142296,0.319434907277167,
11.814901078586));
#30678=CARTESIAN_POINT('Ctrl Pts',(-1.53670704324243,0.636309800095206,
11.8905067546545));
#30679=CARTESIAN_POINT('Ctrl Pts',(-1.53257526769918,0.79477268400084,11.9647288362512));
#30680=CARTESIAN_POINT('Ctrl Pts',(-1.55708435379914,1.0684760419458,11.9984485537147));
#30681=CARTESIAN_POINT('Ctrl Pts',(-1.57504122139016,1.18514270861313,11.9985854052814));
#30682=CARTESIAN_POINT('Ctrl Pts',(-1.60034588135063,1.300000000002,11.9842630921634));
#30683=CARTESIAN_POINT('Ctrl Pts',(-1.83389086553798,-1.30000000000171,
11.8936593986674));
#30684=CARTESIAN_POINT('Ctrl Pts',(-1.79665188669752,-1.18514270861294,
11.912917953872));
#30685=CARTESIAN_POINT('Ctrl Pts',(-1.76343954855294,-1.0684760419457,11.9186022150992));
#30686=CARTESIAN_POINT('Ctrl Pts',(-1.69601474886784,-0.794772684000853,
11.9003746610507));
#30687=CARTESIAN_POINT('Ctrl Pts',(-1.66603874292474,-0.636309800095198,
11.8373699184396));
#30688=CARTESIAN_POINT('Ctrl Pts',(-1.6154253025298,-0.319434907277159,
11.7831996191878));
#30689=CARTESIAN_POINT('Ctrl Pts',(-1.59715844966913,-0.158333333333333,
11.7414598793969));
#30690=CARTESIAN_POINT('Ctrl Pts',(-1.56533425686699,0.158333333333334,
11.7523976505925));
#30691=CARTESIAN_POINT('Ctrl Pts',(-1.55037005383525,0.319434907277167,
11.8054839378072));
#30692=CARTESIAN_POINT('Ctrl Pts',(-1.53902558372754,0.636309800095206,
11.8811010416947));
#30693=CARTESIAN_POINT('Ctrl Pts',(-1.53493609828886,0.794772684000841,
11.9551107502081));
#30694=CARTESIAN_POINT('Ctrl Pts',(-1.55920094319785,1.0684760419458,11.9901104066026));
#30695=CARTESIAN_POINT('Ctrl Pts',(-1.57696419153494,1.18514270861314,11.9911233153795));
#30696=CARTESIAN_POINT('Ctrl Pts',(-1.60198733594911,1.30000000000201,11.9779990785452));
#30697=CARTESIAN_POINT('Ctrl Pts',(-1.83599972161534,-1.30000000000147,
11.8811871414573));
#30698=CARTESIAN_POINT('Ctrl Pts',(-1.79892582936594,-1.18514270861273,
11.8981141035431));
#30699=CARTESIAN_POINT('Ctrl Pts',(-1.76583960086258,-1.06847604194551,
11.9020927398455));
#30700=CARTESIAN_POINT('Ctrl Pts',(-1.69861609512545,-0.794772684000711,
11.8813709627645));
#30701=CARTESIAN_POINT('Ctrl Pts',(-1.66849527243313,-0.636309800095083,
11.8188239975564));
#30702=CARTESIAN_POINT('Ctrl Pts',(-1.61822051779594,-0.319434907277102,
11.7645294437215));
#30703=CARTESIAN_POINT('Ctrl Pts',(-1.60033540285054,-0.158333333333304,
11.7234771864337));
#30704=CARTESIAN_POINT('Ctrl Pts',(-1.56911125276349,0.158333333333306,
11.7343403832408));
#30705=CARTESIAN_POINT('Ctrl Pts',(-1.55462119255688,0.31943490727711,11.7866261268805));
#30706=CARTESIAN_POINT('Ctrl Pts',(-1.54363915686094,0.636309800095092,
11.862293977294));
#30707=CARTESIAN_POINT('Ctrl Pts',(-1.53974920062094,0.794772684000699,
11.9358578924444));
#30708=CARTESIAN_POINT('Ctrl Pts',(-1.56351982816593,1.06847604194561,11.9734175763765));
#30709=CARTESIAN_POINT('Ctrl Pts',(-1.58088572421911,1.18514270861292,11.9761840272521));
#30710=CARTESIAN_POINT('Ctrl Pts',(-1.60532809244977,1.30000000000177,11.9654587335524));
#30711=CARTESIAN_POINT('Ctrl Pts',(-1.83871875022158,-1.30000000000147,
11.8566111165687));
#30712=CARTESIAN_POINT('Ctrl Pts',(-1.80373143478885,-1.18514270861272,
11.8684945970647));
#30713=CARTESIAN_POINT('Ctrl Pts',(-1.77200267054075,-1.06847604194551,
11.8688179909996));
#30714=CARTESIAN_POINT('Ctrl Pts',(-1.70623078291767,-0.794772684000706,
11.8428589831409));
#30715=CARTESIAN_POINT('Ctrl Pts',(-1.67429344241067,-0.636309800095081,
11.7815375882988));
#30716=CARTESIAN_POINT('Ctrl Pts',(-1.62344550695782,-0.3194349072771,11.7272100904621));
#30717=CARTESIAN_POINT('Ctrl Pts',(-1.60516508839733,-0.158333333333303,
11.6877409305584));
#30718=CARTESIAN_POINT('Ctrl Pts',(-1.5743680048027,0.158333333333305,11.6985560603514));
#30719=CARTESIAN_POINT('Ctrl Pts',(-1.56086158634495,0.319434907277107,
11.7491672409098));
#30720=CARTESIAN_POINT('Ctrl Pts',(-1.55099413643843,0.636309800095088,
11.8248585262712));
#30721=CARTESIAN_POINT('Ctrl Pts',(-1.54867609147355,0.794772684000694,
11.897377874003));
#30722=CARTESIAN_POINT('Ctrl Pts',(-1.57148108477577,1.0684760419456,11.9400854010788));
#30723=CARTESIAN_POINT('Ctrl Pts',(-1.58780090005551,1.18514270861292,11.9464145067419));
#30724=CARTESIAN_POINT('Ctrl Pts',(-1.61056909402271,1.30000000000177,11.9405862120668));
#30725=CARTESIAN_POINT('Ctrl Pts',(-1.84133699429135,-1.30000000000095,
11.8377753162936));
#30726=CARTESIAN_POINT('Ctrl Pts',(-1.80586113471466,-1.18514270861225,
11.8462507052803));
#30727=CARTESIAN_POINT('Ctrl Pts',(-1.77392632328359,-1.06847604194508,
11.8440552614294));
#30728=CARTESIAN_POINT('Ctrl Pts',(-1.70833104994145,-0.794772684000392,
11.8143315883892));
#30729=CARTESIAN_POINT('Ctrl Pts',(-1.67771417480332,-0.636309800094828,
11.7534325233558));
#30730=CARTESIAN_POINT('Ctrl Pts',(-1.62752369412159,-0.319434907276974,
11.6988831504611));
#30731=CARTESIAN_POINT('Ctrl Pts',(-1.60889275025167,-0.158333333333241,
11.6606177782961));
#30732=CARTESIAN_POINT('Ctrl Pts',(-1.57869038857939,0.158333333333243,
11.6713553018697));
#30733=CARTESIAN_POINT('Ctrl Pts',(-1.56592675366209,0.319434907276982,
11.7207153472662));
#30734=CARTESIAN_POINT('Ctrl Pts',(-1.55702565868022,0.636309800094838,
11.7964087944155));
#30735=CARTESIAN_POINT('Ctrl Pts',(-1.55596803316826,0.79477268400038,11.8681143540736));
#30736=CARTESIAN_POINT('Ctrl Pts',(-1.57811230023751,1.06847604194518,11.9147102504626));
#30737=CARTESIAN_POINT('Ctrl Pts',(-1.5936603129417,1.18514270861245,11.9237367188749));
#30738=CARTESIAN_POINT('Ctrl Pts',(-1.61517090566172,1.30000000000125,11.9216200187009));
#30739=CARTESIAN_POINT('Ctrl Pts',(-1.84289452093225,-1.30000000000092,
11.8250381337617));
#30740=CARTESIAN_POINT('Ctrl Pts',(-1.80820933111375,-1.18514270861222,
11.8309617575969));
#30741=CARTESIAN_POINT('Ctrl Pts',(-1.77678593741475,-1.06847604194505,
11.8269137155766));
#30742=CARTESIAN_POINT('Ctrl Pts',(-1.71172701329799,-0.794772684000369,
11.7945253857508));
#30743=CARTESIAN_POINT('Ctrl Pts',(-1.68045048611224,-0.636309800094811,
11.7342095024028));
#30744=CARTESIAN_POINT('Ctrl Pts',(-1.62992587645071,-0.319434907276965,
11.6796502838771));
#30745=CARTESIAN_POINT('Ctrl Pts',(-1.61081717316368,-0.158333333333236,
11.642250753783));
#30746=CARTESIAN_POINT('Ctrl Pts',(-1.58094261327684,0.158333333333238,
11.6529448537923));
#30747=CARTESIAN_POINT('Ctrl Pts',(-1.56923788348696,0.319434907276973,
11.7013502469139));
#30748=CARTESIAN_POINT('Ctrl Pts',(-1.56082258278577,0.63630980009482,11.7770575383374));
#30749=CARTESIAN_POINT('Ctrl Pts',(-1.55970762511443,0.794772684000359,
11.8483368173369));
#30750=CARTESIAN_POINT('Ctrl Pts',(-1.58141110711112,1.06847604194515,11.8975860362724));
#30751=CARTESIAN_POINT('Ctrl Pts',(-1.59663434811504,1.18514270861241,11.9084268380449));
#30752=CARTESIAN_POINT('Ctrl Pts',(-1.61768619695974,1.30000000000122,11.908790279576));
#30753=CARTESIAN_POINT('Ctrl Pts',(-1.84296348521904,-1.30000000000092,
11.8244594935074));
#30754=CARTESIAN_POINT('Ctrl Pts',(-1.80831270159826,-1.18514270861222,
11.8302673795263));
#30755=CARTESIAN_POINT('Ctrl Pts',(-1.77691170768193,-1.06847604194505,
11.8261352609154));
#30756=CARTESIAN_POINT('Ctrl Pts',(-1.71187679432357,-0.794772684000369,
11.7936258411106));
#30757=CARTESIAN_POINT('Ctrl Pts',(-1.68057311228323,-0.636309800094812,
11.7333359468922));
#30758=CARTESIAN_POINT('Ctrl Pts',(-1.63003388390691,-0.319434907276965,
11.6787761644253));
#30759=CARTESIAN_POINT('Ctrl Pts',(-1.61090199228311,-0.158333333333236,
11.6414162554122));
#30760=CARTESIAN_POINT('Ctrl Pts',(-1.58104259750264,0.158333333333238,
11.6521083364588));
#30761=CARTESIAN_POINT('Ctrl Pts',(-1.56938714187537,0.319434907276973,
11.7004701333277));
#30762=CARTESIAN_POINT('Ctrl Pts',(-1.56099510539947,0.636309800094821,
11.7761778608677));
#30763=CARTESIAN_POINT('Ctrl Pts',(-1.55987837436003,0.794772684000359,
11.8474376330947));
#30764=CARTESIAN_POINT('Ctrl Pts',(-1.58156226067329,1.06847604194515,11.8968074087413));
#30765=CARTESIAN_POINT('Ctrl Pts',(-1.59677074811116,1.18514270861241,11.9077306927128));
#30766=CARTESIAN_POINT('Ctrl Pts',(-1.61780157206904,1.30000000000122,11.9082069141089));
#30767=CARTESIAN_POINT('Ctrl Pts',(-1.84303196081658,-1.30000000000092,
11.8238809650216));
#30768=CARTESIAN_POINT('Ctrl Pts',(-1.80841559259507,-1.18514270861222,
11.8295731157283));
#30769=CARTESIAN_POINT('Ctrl Pts',(-1.77703699467618,-1.06847604194505,
11.8253569231424));
#30770=CARTESIAN_POINT('Ctrl Pts',(-1.71202605332952,-0.794772684000369,
11.7927264196592));
#30771=CARTESIAN_POINT('Ctrl Pts',(-1.68069495255617,-0.636309800094811,
11.7324625538845));
#30772=CARTESIAN_POINT('Ctrl Pts',(-1.63014140611213,-0.319434907276965,
11.677902145418));
#30773=CARTESIAN_POINT('Ctrl Pts',(-1.61098724178691,-0.158333333333236,
11.6405816925744));
#30774=CARTESIAN_POINT('Ctrl Pts',(-1.5811428723139,0.158333333333238,11.6512717653135));
#30775=CARTESIAN_POINT('Ctrl Pts',(-1.56953536178466,0.319434907276973,
11.6995901789837));
#30776=CARTESIAN_POINT('Ctrl Pts',(-1.56116656149189,0.63630980009482,11.7752983500434));
#30777=CARTESIAN_POINT('Ctrl Pts',(-1.56004940665739,0.794772684000359,
11.8465384115319));
#30778=CARTESIAN_POINT('Ctrl Pts',(-1.58171386737888,1.06847604194515,11.8960287165786));
#30779=CARTESIAN_POINT('Ctrl Pts',(-1.59690745305271,1.18514270861241,11.9070345037863));
#30780=CARTESIAN_POINT('Ctrl Pts',(-1.61791688210141,1.30000000000122,11.9076235589435));
#30781=CARTESIAN_POINT('Ctrl Pts',(-1.84316669728488,-1.30000000000092,
11.8227243210795));
#30782=CARTESIAN_POINT('Ctrl Pts',(-1.80861747574687,-1.18514270861222,
11.8281852976434));
#30783=CARTESIAN_POINT('Ctrl Pts',(-1.77728271948137,-1.06847604194505,
11.8238011194843));
#30784=CARTESIAN_POINT('Ctrl Pts',(-1.71231922184277,-0.794772684000369,
11.7909285139586));
#30785=CARTESIAN_POINT('Ctrl Pts',(-1.68093588515833,-0.636309800094812,
11.7307162099497));
#30786=CARTESIAN_POINT('Ctrl Pts',(-1.63035490044341,-0.319434907276966,
11.6761543109724));
#30787=CARTESIAN_POINT('Ctrl Pts',(-1.61115632950736,-0.158333333333236,
11.6389127476635));
#30788=CARTESIAN_POINT('Ctrl Pts',(-1.58134204256666,0.158333333333238,
11.6495987813934));
#30789=CARTESIAN_POINT('Ctrl Pts',(-1.56982924289939,0.319434907276973,
11.697830603521));
#30790=CARTESIAN_POINT('Ctrl Pts',(-1.56150796664459,0.636309800094821,
11.7735394991853));
#30791=CARTESIAN_POINT('Ctrl Pts',(-1.56039305183889,0.794772684000359,
11.8447396712156));
#30792=CARTESIAN_POINT('Ctrl Pts',(-1.58201926842724,1.06847604194515,11.8944709559761));
#30793=CARTESIAN_POINT('Ctrl Pts',(-1.59718274353702,1.18514270861241,11.9056418049324));
#30794=CARTESIAN_POINT('Ctrl Pts',(-1.61814850592577,1.30000000000122,11.9064566723979));
#30795=CARTESIAN_POINT('Ctrl Pts',(-1.84344888288028,-1.30000000000092,
11.8202201103828));
#30796=CARTESIAN_POINT('Ctrl Pts',(-1.80903791412077,-1.18514270861222,
11.8251815293551));
#30797=CARTESIAN_POINT('Ctrl Pts',(-1.77779396859234,-1.06847604194506,
11.8204341284388));
#30798=CARTESIAN_POINT('Ctrl Pts',(-1.71293066131657,-0.79477268400037,
11.7870373664222));
#30799=CARTESIAN_POINT('Ctrl Pts',(-1.68144353848663,-0.636309800094812,
11.7269349411184));
#30800=CARTESIAN_POINT('Ctrl Pts',(-1.63080972946727,-0.319434907276966,
11.6723685067135));
#30801=CARTESIAN_POINT('Ctrl Pts',(-1.61152048533865,-0.158333333333237,
11.6352968905261));
#30802=CARTESIAN_POINT('Ctrl Pts',(-1.58177113039119,0.158333333333239,
11.6459740954571));
#30803=CARTESIAN_POINT('Ctrl Pts',(-1.57045247065589,0.319434907276973,
11.6940200284722));
#30804=CARTESIAN_POINT('Ctrl Pts',(-1.56223778799716,0.636309800094821,
11.7697299649961));
#30805=CARTESIAN_POINT('Ctrl Pts',(-1.56114547527118,0.79477268400036,11.8408410521061));
#30806=CARTESIAN_POINT('Ctrl Pts',(-1.58269200483603,1.06847604194515,11.8910940125196));
#30807=CARTESIAN_POINT('Ctrl Pts',(-1.59778850945841,1.18514270861242,11.9026227716686));
#30808=CARTESIAN_POINT('Ctrl Pts',(-1.61865482443213,1.30000000000122,11.9039276454594));
#30809=CARTESIAN_POINT('Ctrl Pts',(-1.84384438076087,-1.30000000000093,
11.8163742850652));
#30810=CARTESIAN_POINT('Ctrl Pts',(-1.80959881413743,-1.18514270861223,
11.8205762115273));
#30811=CARTESIAN_POINT('Ctrl Pts',(-1.77846705385221,-1.06847604194506,
11.8152752438931));
#30812=CARTESIAN_POINT('Ctrl Pts',(-1.71373997526232,-0.794772684000375,
11.781075361793));
#30813=CARTESIAN_POINT('Ctrl Pts',(-1.68215207565877,-0.636309800094816,
11.7211303361575));
#30814=CARTESIAN_POINT('Ctrl Pts',(-1.63148140929813,-0.319434907276968,
11.6665484490828));
#30815=CARTESIAN_POINT('Ctrl Pts',(-1.61209419825319,-0.158333333333238,
11.6297311120483));
#30816=CARTESIAN_POINT('Ctrl Pts',(-1.58244234073241,0.15833333333324,11.6403946024421));
#30817=CARTESIAN_POINT('Ctrl Pts',(-1.57134630363325,0.319434907276975,
11.6881666550633));
#30818=CARTESIAN_POINT('Ctrl Pts',(-1.56331175406625,0.636309800094825,
11.763876099524));
#30819=CARTESIAN_POINT('Ctrl Pts',(-1.56236283053004,0.794772684000365,
11.8348339670287));
#30820=CARTESIAN_POINT('Ctrl Pts',(-1.58380073924108,1.06847604194516,11.8858875342653));
#30821=CARTESIAN_POINT('Ctrl Pts',(-1.59878065247063,1.18514270861242,11.8979689831355));
#30822=CARTESIAN_POINT('Ctrl Pts',(-1.61946080260151,1.30000000000122,11.9000326833401));
#30823=CARTESIAN_POINT('Ctrl Pts',(-1.84426494116142,-1.30000000000093,
11.8117677988858));
#30824=CARTESIAN_POINT('Ctrl Pts',(-1.8101257178847,-1.18514270861223,11.8150761584175));
#30825=CARTESIAN_POINT('Ctrl Pts',(-1.77907371003347,-1.06847604194507,
11.8091214978874));
#30826=CARTESIAN_POINT('Ctrl Pts',(-1.71446944519264,-0.794772684000379,
11.7739656114336));
#30827=CARTESIAN_POINT('Ctrl Pts',(-1.68286150667179,-0.63630980009482,
11.7141893826815));
#30828=CARTESIAN_POINT('Ctrl Pts',(-1.63223484958063,-0.31943490727697,
11.6595724368514));
#30829=CARTESIAN_POINT('Ctrl Pts',(-1.61282826183454,-0.158333333333238,
11.6230434385891));
#30830=CARTESIAN_POINT('Ctrl Pts',(-1.5832926406303,0.15833333333324,11.6336895451472));
#30831=CARTESIAN_POINT('Ctrl Pts',(-1.57231028315703,0.319434907276977,
11.6811571847545));
#30832=CARTESIAN_POINT('Ctrl Pts',(-1.56451316606789,0.636309800094828,
11.7568636108008));
#30833=CARTESIAN_POINT('Ctrl Pts',(-1.56392988574138,0.79477268400037,11.8276093111329));
#30834=CARTESIAN_POINT('Ctrl Pts',(-1.58526559199745,1.06847604194516,11.8796195501203));
#30835=CARTESIAN_POINT('Ctrl Pts',(-1.60008428456176,1.18514270861243,11.892367313324));
#30836=CARTESIAN_POINT('Ctrl Pts',(-1.62048623301792,1.30000000000123,11.8953495344429));
#30837=CARTESIAN_POINT('Ctrl Pts',(-1.84478245665894,-1.30000000000094,
11.8056321709388));
#30838=CARTESIAN_POINT('Ctrl Pts',(-1.81070410073275,-1.18514270861224,
11.8077647834726));
#30839=CARTESIAN_POINT('Ctrl Pts',(-1.77970915118711,-1.06847604194508,
11.8009480735919));
#30840=CARTESIAN_POINT('Ctrl Pts',(-1.71522790279083,-0.794772684000385,
11.7645253850059));
#30841=CARTESIAN_POINT('Ctrl Pts',(-1.68367560268276,-0.636309800094825,
11.7049579257604));
#30842=CARTESIAN_POINT('Ctrl Pts',(-1.63317521611877,-0.319434907276972,
11.6502817193305));
#30843=CARTESIAN_POINT('Ctrl Pts',(-1.61381918122407,-0.15833333333324,
11.6141244214084));
#30844=CARTESIAN_POINT('Ctrl Pts',(-1.58443628392345,0.158333333333242,
11.6247465764964));
#30845=CARTESIAN_POINT('Ctrl Pts',(-1.57348065202961,0.31943490727698,11.6718272551794));
#30846=CARTESIAN_POINT('Ctrl Pts',(-1.56602202900427,0.636309800094834,
11.7475264516963));
#30847=CARTESIAN_POINT('Ctrl Pts',(-1.5660937604962,0.794772684000376,11.8179645101958));
#30848=CARTESIAN_POINT('Ctrl Pts',(-1.58731685620065,1.06847604194517,11.8712470930887));
#30849=CARTESIAN_POINT('Ctrl Pts',(-1.60190135100444,1.18514270861244,11.8848862965936));
#30850=CARTESIAN_POINT('Ctrl Pts',(-1.62188364887474,1.30000000000124,11.8891006477833));
#30851=CARTESIAN_POINT('Ctrl Pts',(-1.84544014297006,-1.30000000000095,
11.7979582048086));
#30852=CARTESIAN_POINT('Ctrl Pts',(-1.81144108841217,-1.18514270861225,
11.7986194547981));
#30853=CARTESIAN_POINT('Ctrl Pts',(-1.78051023879179,-1.06847604194508,
11.7907258958039));
#30854=CARTESIAN_POINT('Ctrl Pts',(-1.71614195567161,-0.794772684000391,
11.7527268752903));
#30855=CARTESIAN_POINT('Ctrl Pts',(-1.68458079263209,-0.636309800094829,
11.6934365417342));
#30856=CARTESIAN_POINT('Ctrl Pts',(-1.63419573725037,-0.319434907276974,
11.6386946770248));
#30857=CARTESIAN_POINT('Ctrl Pts',(-1.6149017766345,-0.158333333333241,
11.6030025586446));
#30858=CARTESIAN_POINT('Ctrl Pts',(-1.58573694252356,0.158333333333243,
11.6135885063308));
#30859=CARTESIAN_POINT('Ctrl Pts',(-1.57489385088498,0.319434907276982,
11.6601689843851));
#30860=CARTESIAN_POINT('Ctrl Pts',(-1.56785257747679,0.636309800094838,
11.7358576708726));
#30861=CARTESIAN_POINT('Ctrl Pts',(-1.56861088718507,0.79477268400038,11.8059322870055));
#30862=CARTESIAN_POINT('Ctrl Pts',(-1.58972943387026,1.06847604194518,11.8607999137329));
#30863=CARTESIAN_POINT('Ctrl Pts',(-1.60407107161093,1.18514270861245,11.8755459464035));
#30864=CARTESIAN_POINT('Ctrl Pts',(-1.62361291075149,1.30000000000125,11.8812878491803));
#30865=CARTESIAN_POINT('Ctrl Pts',(-1.84674828898009,-1.30000000000098,
11.7856311373012));
#30866=CARTESIAN_POINT('Ctrl Pts',(-1.81326855991173,-1.18514270861227,
11.7838592214465));
#30867=CARTESIAN_POINT('Ctrl Pts',(-1.78265895673732,-1.0684760419451,11.774198415806));
#30868=CARTESIAN_POINT('Ctrl Pts',(-1.71857521495619,-0.794772684000405,
11.7336551085668));
#30869=CARTESIAN_POINT('Ctrl Pts',(-1.6864963870894,-0.63630980009484,11.6749097837805));
#30870=CARTESIAN_POINT('Ctrl Pts',(-1.63575839200298,-0.31943490727698,
11.6201649167908));
#30871=CARTESIAN_POINT('Ctrl Pts',(-1.61595406457843,-0.158333333333244,
11.5853280034014));
#30872=CARTESIAN_POINT('Ctrl Pts',(-1.58711121341717,0.158333333333246,
11.595862223947));
#30873=CARTESIAN_POINT('Ctrl Pts',(-1.57727524413475,0.319434907276988,
11.6414988656436));
#30874=CARTESIAN_POINT('Ctrl Pts',(-1.57088676731849,0.636309800094849,
11.7171603612028));
#30875=CARTESIAN_POINT('Ctrl Pts',(-1.57188783305683,0.794772684000394,
11.786773485769));
#30876=CARTESIAN_POINT('Ctrl Pts',(-1.5927508350306,1.0684760419452,11.8441938322081));
#30877=CARTESIAN_POINT('Ctrl Pts',(-1.60681390531366,1.18514270861247,11.8606993865044));
#30878=CARTESIAN_POINT('Ctrl Pts',(-1.62590922537573,1.30000000000128,11.868855354757));
#30879=CARTESIAN_POINT('Ctrl Pts',(-1.84845170421517,-1.30000000000104,
11.7701972347928));
#30880=CARTESIAN_POINT('Ctrl Pts',(-1.81560919139068,-1.18514270861233,
11.7653832284769));
#30881=CARTESIAN_POINT('Ctrl Pts',(-1.78540136955671,-1.06847604194516,
11.7535113896969));
#30882=CARTESIAN_POINT('Ctrl Pts',(-1.72170192132254,-0.794772684000443,
11.709780062255));
#30883=CARTESIAN_POINT('Ctrl Pts',(-1.68903913893573,-0.636309800094871,
11.6517047122135));
#30884=CARTESIAN_POINT('Ctrl Pts',(-1.63792278128934,-0.319434907276996,
11.5969476183648));
#30885=CARTESIAN_POINT('Ctrl Pts',(-1.61757610966211,-0.158333333333251,
11.5631688638252));
#30886=CARTESIAN_POINT('Ctrl Pts',(-1.58903919989458,0.158333333333253,
11.5736565072532));
#30887=CARTESIAN_POINT('Ctrl Pts',(-1.58010994835879,0.319434907277002,
11.6181683609924));
#30888=CARTESIAN_POINT('Ctrl Pts',(-1.57460399261029,0.636309800094879,
11.6937880536352));
#30889=CARTESIAN_POINT('Ctrl Pts',(-1.57637841542004,0.794772684000434,
11.7627565934282));
#30890=CARTESIAN_POINT('Ctrl Pts',(-1.59709589115024,1.06847604194525,11.8233372447497));
#30891=CARTESIAN_POINT('Ctrl Pts',(-1.61082650864359,1.18514270861253,11.8420361414989));
#30892=CARTESIAN_POINT('Ctrl Pts',(-1.6293199160448,1.30000000000134,11.8532108157745));
#30893=CARTESIAN_POINT('Ctrl Pts',(-1.85026481461886,-1.30000000000114,
11.7456866281147));
#30894=CARTESIAN_POINT('Ctrl Pts',(-1.81775194196863,-1.18514270861242,
11.7361383865919));
#30895=CARTESIAN_POINT('Ctrl Pts',(-1.78773023179206,-1.06847604194524,
11.7208168877023));
#30896=CARTESIAN_POINT('Ctrl Pts',(-1.72412915913127,-0.794772684000502,
11.6720837807585));
#30897=CARTESIAN_POINT('Ctrl Pts',(-1.69081671649123,-0.636309800094919,
11.6150284922353));
#30898=CARTESIAN_POINT('Ctrl Pts',(-1.63974375521256,-0.31943490727702,
11.5601180730225));
#30899=CARTESIAN_POINT('Ctrl Pts',(-1.61949910327857,-0.158333333333264,
11.5278321545169));
#30900=CARTESIAN_POINT('Ctrl Pts',(-1.59203020234948,0.158333333333265,
11.5381217576227));
#30901=CARTESIAN_POINT('Ctrl Pts',(-1.58463938153361,0.319434907277029,
11.5808228501109));
#30902=CARTESIAN_POINT('Ctrl Pts',(-1.58009946425156,0.63630980009493,11.6564366711393));
#30903=CARTESIAN_POINT('Ctrl Pts',(-1.58198527480658,0.794772684000494,
11.7245355748381));
#30904=CARTESIAN_POINT('Ctrl Pts',(-1.60210979666633,1.06847604194533,11.7902488369403));
#30905=CARTESIAN_POINT('Ctrl Pts',(-1.61533602454307,1.18514270861261,11.8124693688438));
#30906=CARTESIAN_POINT('Ctrl Pts',(-1.63307732047047,1.30000000000143,11.8284655964033));
#30907=CARTESIAN_POINT('Ctrl Pts',(-1.85235418101203,-1.30000000000125,
11.7210849690256));
#30908=CARTESIAN_POINT('Ctrl Pts',(-1.82016905161149,-1.18514270861252,
11.7068025046435));
#30909=CARTESIAN_POINT('Ctrl Pts',(-1.79038984220925,-1.06847604194533,
11.6880184387967));
#30910=CARTESIAN_POINT('Ctrl Pts',(-1.72715206767857,-0.794772684000574,
11.6342238890251));
#30911=CARTESIAN_POINT('Ctrl Pts',(-1.69383554820921,-0.636309800094973,
11.5780448011396));
#30912=CARTESIAN_POINT('Ctrl Pts',(-1.64271773724477,-0.319434907277046,
11.5230000209639));
#30913=CARTESIAN_POINT('Ctrl Pts',(-1.6221146343507,-0.158333333333276,
11.4923232235877));
#30914=CARTESIAN_POINT('Ctrl Pts',(-1.59481395715236,0.158333333333278,
11.5025859059677));
#30915=CARTESIAN_POINT('Ctrl Pts',(-1.58771839974174,0.319434907277054,
11.5436832251077));
#30916=CARTESIAN_POINT('Ctrl Pts',(-1.58403735989905,0.636309800094981,
11.619310842894));
#30917=CARTESIAN_POINT('Ctrl Pts',(-1.58718536137325,0.794772684000561,
11.6863443221167));
#30918=CARTESIAN_POINT('Ctrl Pts',(-1.60750575379507,1.06847604194542,11.7570527056758));
#30919=CARTESIAN_POINT('Ctrl Pts',(-1.62052991615721,1.18514270861271,11.7827411501694));
#30920=CARTESIAN_POINT('Ctrl Pts',(-1.63778229594682,1.30000000000154,11.8035109999178));
#30921=CARTESIAN_POINT('Ctrl Pts',(-1.85396790840865,-1.30000000000128,
11.6965900695597));
#30922=CARTESIAN_POINT('Ctrl Pts',(-1.82229831568687,-1.18514270861255,
11.6775119375083));
#30923=CARTESIAN_POINT('Ctrl Pts',(-1.79268711193668,-1.06847604194536,
11.6552680903094));
#30924=CARTESIAN_POINT('Ctrl Pts',(-1.72903459787654,-0.794772684000596,
11.5965669181243));
#30925=CARTESIAN_POINT('Ctrl Pts',(-1.69367106033116,-0.63630980009499,
11.5417312925321));
#30926=CARTESIAN_POINT('Ctrl Pts',(-1.64213453885132,-0.319434907277055,
11.4866290091821));
#30927=CARTESIAN_POINT('Ctrl Pts',(-1.62226661781747,-0.158333333333281,
11.4573044263621));
#30928=CARTESIAN_POINT('Ctrl Pts',(-1.59612552676786,0.158333333333283,
11.4673180137663));
#30929=CARTESIAN_POINT('Ctrl Pts',(-1.58998142544728,0.319434907277065,
11.5066725383206));
#30930=CARTESIAN_POINT('Ctrl Pts',(-1.58800752304125,0.636309800095001,
11.5821384656179));
#30931=CARTESIAN_POINT('Ctrl Pts',(-1.5931292840274,0.794772684000582,11.6479698066803));
#30932=CARTESIAN_POINT('Ctrl Pts',(-1.61330891412657,1.06847604194545,11.7237468386099));
#30933=CARTESIAN_POINT('Ctrl Pts',(-1.6256891281828,1.18514270861275,11.7529951111915));
#30934=CARTESIAN_POINT('Ctrl Pts',(-1.64171454215429,1.30000000000158,11.7786905870478));
#30935=CARTESIAN_POINT('Ctrl Pts',(-1.85521388015686,-1.30000000000133,
11.6781712661894));
#30936=CARTESIAN_POINT('Ctrl Pts',(-1.82303326346136,-1.1851427086126,11.6557103919718));
#30937=CARTESIAN_POINT('Ctrl Pts',(-1.79317972753303,-1.0684760419454,11.6309624309223));
#30938=CARTESIAN_POINT('Ctrl Pts',(-1.72958810946243,-0.794772684000624,
11.5685060619735));
#30939=CARTESIAN_POINT('Ctrl Pts',(-1.69570308906305,-0.636309800095015,
11.513986001499));
#30940=CARTESIAN_POINT('Ctrl Pts',(-1.64411605157966,-0.319434907277068,
11.4587851770889));
#30941=CARTESIAN_POINT('Ctrl Pts',(-1.62282683086726,-0.158333333333287,
11.4309375845017));
#30942=CARTESIAN_POINT('Ctrl Pts',(-1.59651906306741,0.158333333333289,
11.4409915305209));
#30943=CARTESIAN_POINT('Ctrl Pts',(-1.59127716910426,0.319434907277074,
11.4789877912314));
#30944=CARTESIAN_POINT('Ctrl Pts',(-1.58973211930582,0.636309800095022,
11.5544748376688));
#30945=CARTESIAN_POINT('Ctrl Pts',(-1.59466018316317,0.794772684000613,
11.6196833551108));
#30946=CARTESIAN_POINT('Ctrl Pts',(-1.61519706666357,1.06847604194549,11.6991726405048));
#30947=CARTESIAN_POINT('Ctrl Pts',(-1.62780582852626,1.18514270861279,11.7309642964648));
#30948=CARTESIAN_POINT('Ctrl Pts',(-1.64413369635081,1.30000000000163,11.7601396421058));
#30949=CARTESIAN_POINT('Ctrl Pts',(-1.85517328864499,-1.30000000000137,
11.6601079860051));
#30950=CARTESIAN_POINT('Ctrl Pts',(-1.82348599895047,-1.18514270861263,
11.6340049138576));
#30951=CARTESIAN_POINT('Ctrl Pts',(-1.79380062463975,-1.06847604194542,
11.6066388522111));
#30952=CARTESIAN_POINT('Ctrl Pts',(-1.72984629646174,-0.794772684000645,
11.5405000168428));
#30953=CARTESIAN_POINT('Ctrl Pts',(-1.69408509803023,-0.63630980009503,
11.4870871937377));
#30954=CARTESIAN_POINT('Ctrl Pts',(-1.64208594211023,-0.319434907277075,
11.4318663463684));
#30955=CARTESIAN_POINT('Ctrl Pts',(-1.62119743812734,-0.158333333333291,
11.4050607229264));
#30956=CARTESIAN_POINT('Ctrl Pts',(-1.59637095195443,0.158333333333293,
11.4147786545005));
#30957=CARTESIAN_POINT('Ctrl Pts',(-1.59300281218603,0.319434907277083,
11.4511946083861));
#30958=CARTESIAN_POINT('Ctrl Pts',(-1.59327147535533,0.636309800095039,
11.5264293584128));
#30959=CARTESIAN_POINT('Ctrl Pts',(-1.59933219948415,0.794772684000632,
11.5908094443692));
#30960=CARTESIAN_POINT('Ctrl Pts',(-1.6195475915525,1.06847604194552,11.674151461135));
#30961=CARTESIAN_POINT('Ctrl Pts',(-1.63154715737108,1.18514270861282,11.7086452007729));
#30962=CARTESIAN_POINT('Ctrl Pts',(-1.64679579483592,1.30000000000166,11.7415570091167));
#30963=CARTESIAN_POINT('Ctrl Pts',(-1.85677772263928,-1.3000000000014,11.6415847248261));
#30964=CARTESIAN_POINT('Ctrl Pts',(-1.82500377440488,-1.18514270861266,
11.611990513213));
#30965=CARTESIAN_POINT('Ctrl Pts',(-1.79520315411112,-1.06847604194545,
11.5820846750055));
#30966=CARTESIAN_POINT('Ctrl Pts',(-1.73091654194481,-0.794772684000666,
11.5122762863304));
#30967=CARTESIAN_POINT('Ctrl Pts',(-1.69481730670943,-0.636309800095046,
11.4596117897729));
#30968=CARTESIAN_POINT('Ctrl Pts',(-1.64245260583326,-0.319434907277083,
11.4043689251971));
#30969=CARTESIAN_POINT('Ctrl Pts',(-1.62142968933603,-0.158333333333295,
11.3787472591335));
#30970=CARTESIAN_POINT('Ctrl Pts',(-1.59644123206918,0.158333333333297,
11.3884914891901));
#30971=CARTESIAN_POINT('Ctrl Pts',(-1.59274409701337,0.319434907277091,
11.4237993865481));
#30972=CARTESIAN_POINT('Ctrl Pts',(-1.59366238655238,0.636309800095055,
11.4990086854437));
#30973=CARTESIAN_POINT('Ctrl Pts',(-1.60104000459311,0.794772684000651,
11.5624606041692));
#30974=CARTESIAN_POINT('Ctrl Pts',(-1.62208616073324,1.06847604194555,11.649421942033));
#30975=CARTESIAN_POINT('Ctrl Pts',(-1.63430838227277,1.18514270861285,11.6864622644108));
#30976=CARTESIAN_POINT('Ctrl Pts',(-1.64964272419568,1.3000000000017,11.7229005682402));
#30977=CARTESIAN_POINT('Ctrl Pts',(-1.85593729332808,-1.30000000000142,
11.6267230412812));
#30978=CARTESIAN_POINT('Ctrl Pts',(-1.82401323334643,-1.18514270861268,
11.5942255222404));
#30979=CARTESIAN_POINT('Ctrl Pts',(-1.79411233921994,-1.06847604194547,
11.5621934861307));
#30980=CARTESIAN_POINT('Ctrl Pts',(-1.72970920999285,-0.794772684000676,
11.4892684334208));
#30981=CARTESIAN_POINT('Ctrl Pts',(-1.69376723753485,-0.636309800095055,
11.4371135776616));
#30982=CARTESIAN_POINT('Ctrl Pts',(-1.64133817124265,-0.319434907277087,
11.3817866822353));
#30983=CARTESIAN_POINT('Ctrl Pts',(-1.6198859209163,-0.158333333333297,
11.3572289053674));
#30984=CARTESIAN_POINT('Ctrl Pts',(-1.59533823300359,0.158333333333299,
11.3668610697367));
#30985=CARTESIAN_POINT('Ctrl Pts',(-1.59250251305007,0.319434907277096,
11.40098490634));
#30986=CARTESIAN_POINT('Ctrl Pts',(-1.59440068043849,0.636309800095065,
11.476066477427));
#30987=CARTESIAN_POINT('Ctrl Pts',(-1.6024690900727,0.794772684000662,11.5388338827361));
#30988=CARTESIAN_POINT('Ctrl Pts',(-1.62382938818921,1.06847604194556,11.6288861795763));
#30989=CARTESIAN_POINT('Ctrl Pts',(-1.63602578233119,1.18514270861287,11.6680908004979));
#30990=CARTESIAN_POINT('Ctrl Pts',(-1.65117248903756,1.30000000000172,11.7075197398054));
#30991=CARTESIAN_POINT('Ctrl Pts',(-1.85699869964041,-1.30000000000142,
11.6143622964803));
#30992=CARTESIAN_POINT('Ctrl Pts',(-1.82500430958963,-1.18514270861268,
11.5795349643121));
#30993=CARTESIAN_POINT('Ctrl Pts',(-1.79495934551754,-1.06847604194547,
11.5458224717731));
#30994=CARTESIAN_POINT('Ctrl Pts',(-1.73005303202881,-0.79477268400068,
11.4705153724133));
#30995=CARTESIAN_POINT('Ctrl Pts',(-1.69344725687642,-0.636309800095058,
11.4189678952462));
#30996=CARTESIAN_POINT('Ctrl Pts',(-1.64045500640219,-0.319434907277089,
11.3637094229155));
#30997=CARTESIAN_POINT('Ctrl Pts',(-1.61863681283758,-0.158333333333298,
11.3400169850387));
#30998=CARTESIAN_POINT('Ctrl Pts',(-1.5944140512909,0.1583333333333,11.3495655171347));
#30999=CARTESIAN_POINT('Ctrl Pts',(-1.59238937323836,0.319434907277097,
11.382696200417));
#31000=CARTESIAN_POINT('Ctrl Pts',(-1.59526779410525,0.636309800095067,
11.4576289911575));
#31001=CARTESIAN_POINT('Ctrl Pts',(-1.60427319996494,0.794772684000666,
11.5197753878327));
#31002=CARTESIAN_POINT('Ctrl Pts',(-1.62572020818096,1.06847604194557,11.6123407970366));
#31003=CARTESIAN_POINT('Ctrl Pts',(-1.63769439053449,1.18514270861288,11.6533220654616));
#31004=CARTESIAN_POINT('Ctrl Pts',(-1.65235914007478,1.30000000000172,11.6952164665535));
#31005=CARTESIAN_POINT('Ctrl Pts',(-1.85707299808195,-1.30000000000145,
11.5962359591747));
#31006=CARTESIAN_POINT('Ctrl Pts',(-1.8250340456161,-1.1851427086127,11.5578966099453));
#31007=CARTESIAN_POINT('Ctrl Pts',(-1.79487638163994,-1.06847604194549,
11.5216352984547));
#31008=CARTESIAN_POINT('Ctrl Pts',(-1.72955229759684,-0.794772684000693,
11.4426650977481));
#31009=CARTESIAN_POINT('Ctrl Pts',(-1.69226227430237,-0.636309800095069,
11.3919488679483));
#31010=CARTESIAN_POINT('Ctrl Pts',(-1.63899399294016,-0.319434907277095,
11.3366395947736));
#31011=CARTESIAN_POINT('Ctrl Pts',(-1.6173140649551,-0.158333333333301,
11.3140597026112));
#31012=CARTESIAN_POINT('Ctrl Pts',(-1.59346344526089,0.158333333333303,
11.323505276146));
#31013=CARTESIAN_POINT('Ctrl Pts',(-1.59178184641142,0.319434907277104,
11.3553793032582));
#31014=CARTESIAN_POINT('Ctrl Pts',(-1.59547188581878,0.636309800095079,
11.4302369991131));
#31015=CARTESIAN_POINT('Ctrl Pts',(-1.60509054103872,0.794772684000681,
11.4915906889066));
#31016=CARTESIAN_POINT('Ctrl Pts',(-1.62742089479516,1.06847604194558,11.5877592904259));
#31017=CARTESIAN_POINT('Ctrl Pts',(-1.63977269513233,1.1851427086129,11.6312552112791));
#31018=CARTESIAN_POINT('Ctrl Pts',(-1.65481031308663,1.30000000000174,11.6766192287855));
#31019=CARTESIAN_POINT('Ctrl Pts',(-1.85782405239422,-1.30000000000149,
11.5718563713316));
#31020=CARTESIAN_POINT('Ctrl Pts',(-1.82511466019596,-1.18514270861274,
11.5289860257926));
#31021=CARTESIAN_POINT('Ctrl Pts',(-1.79433950157869,-1.06847604194552,
11.4894453770448));
#31022=CARTESIAN_POINT('Ctrl Pts',(-1.72771119513777,-0.794772684000718,
11.405790834049));
#31023=CARTESIAN_POINT('Ctrl Pts',(-1.68954961974983,-0.636309800095088,
11.3561967971218));
#31024=CARTESIAN_POINT('Ctrl Pts',(-1.63562300718043,-0.319434907277103,
11.3009078818754));
#31025=CARTESIAN_POINT('Ctrl Pts',(-1.61379601219274,-0.158333333333305,
11.2799023853609));
#31026=CARTESIAN_POINT('Ctrl Pts',(-1.59069699733874,0.158333333333307,
11.2891319462005));
#31027=CARTESIAN_POINT('Ctrl Pts',(-1.58991024511068,0.319434907277113,
11.3191733505662));
#31028=CARTESIAN_POINT('Ctrl Pts',(-1.59579737236803,0.636309800095098,
11.3936566738865));
#31029=CARTESIAN_POINT('Ctrl Pts',(-1.60818428931505,0.794772684000702,
11.4535424940212));
#31030=CARTESIAN_POINT('Ctrl Pts',(-1.63125865236166,1.06847604194561,11.5546095191125));
#31031=CARTESIAN_POINT('Ctrl Pts',(-1.64334165504426,1.18514270861293,11.6016267147841));
#31032=CARTESIAN_POINT('Ctrl Pts',(-1.65751962363596,1.30000000000179,11.6519129358675));
#31033=CARTESIAN_POINT('Ctrl Pts',(-1.85678181360715,-1.30000000000152,
11.5479686431218));
#31034=CARTESIAN_POINT('Ctrl Pts',(-1.82362997352617,-1.18514270861277,
11.5005091509062));
#31035=CARTESIAN_POINT('Ctrl Pts',(-1.79241924785772,-1.06847604194555,
11.457642418012));
#31036=CARTESIAN_POINT('Ctrl Pts',(-1.72480059049101,-0.79477268400074,
11.3692218823769));
#31037=CARTESIAN_POINT('Ctrl Pts',(-1.68579469115041,-0.636309800095108,
11.3207420009397));
#31038=CARTESIAN_POINT('Ctrl Pts',(-1.63138961270452,-0.319434907277114,
11.265422664141));
#31039=CARTESIAN_POINT('Ctrl Pts',(-1.60961523247916,-0.15833333333331,
11.2459371441337));
#31040=CARTESIAN_POINT('Ctrl Pts',(-1.58718054123095,0.158333333333312,
11.2549647313119));
#31041=CARTESIAN_POINT('Ctrl Pts',(-1.58732163867687,0.319434907277123,
11.2831821703496));
#31042=CARTESIAN_POINT('Ctrl Pts',(-1.59439645505399,0.636309800095118,
11.3574923069509));
#31043=CARTESIAN_POINT('Ctrl Pts',(-1.60718994603995,0.79477268400073,11.4163823312034));
#31044=CARTESIAN_POINT('Ctrl Pts',(-1.63150163440477,1.06847604194565,11.5222213562515));
#31045=CARTESIAN_POINT('Ctrl Pts',(-1.64419640242279,1.18514270861297,11.5725657031935));
#31046=CARTESIAN_POINT('Ctrl Pts',(-1.65906230940252,1.30000000000182,11.6274406048564));
#31047=CARTESIAN_POINT('Ctrl Pts',(-1.85646792992249,-1.30000000000154,
11.5238562660431));
#31048=CARTESIAN_POINT('Ctrl Pts',(-1.82287519950759,-1.18514270861279,
11.4717906712953));
#31049=CARTESIAN_POINT('Ctrl Pts',(-1.79110499396969,-1.06847604194556,
11.4256234324653));
#31050=CARTESIAN_POINT('Ctrl Pts',(-1.7219198606302,-0.794772684000747,
11.3325942571756));
#31051=CARTESIAN_POINT('Ctrl Pts',(-1.68117947256001,-0.636309800095115,
11.2855035822367));
#31052=CARTESIAN_POINT('Ctrl Pts',(-1.62549156015531,-0.319434907277118,
11.2303944130328));
#31053=CARTESIAN_POINT('Ctrl Pts',(-1.60321674177326,-0.158333333333312,
11.2125995993871));
#31054=CARTESIAN_POINT('Ctrl Pts',(-1.58171314091487,0.158333333333314,
11.2213342239253));
#31055=CARTESIAN_POINT('Ctrl Pts',(-1.58370410867213,0.319434907277129,
11.247408138762));
#31056=CARTESIAN_POINT('Ctrl Pts',(-1.59310619103803,0.636309800095127,
11.3212369774957));
#31057=CARTESIAN_POINT('Ctrl Pts',(-1.60751436014146,0.794772684000738,
11.3788835799511));
#31058=CARTESIAN_POINT('Ctrl Pts',(-1.63309938464165,1.06847604194566,11.48949665088));
#31059=CARTESIAN_POINT('Ctrl Pts',(-1.6460822009907,1.18514270861298,11.5432480259809));
#31060=CARTESIAN_POINT('Ctrl Pts',(-1.66097302460121,1.30000000000184,11.6028704763956));
#31061=CARTESIAN_POINT('Ctrl Pts',(-1.85497966222603,-1.30000000000162,
11.503126144964));
#31062=CARTESIAN_POINT('Ctrl Pts',(-1.82046411571729,-1.18514270861286,
11.447225295674));
#31063=CARTESIAN_POINT('Ctrl Pts',(-1.78795658628739,-1.06847604194563,
11.3982726438186));
#31064=CARTESIAN_POINT('Ctrl Pts',(-1.71749661135009,-0.794772684000801,
11.3012339511447));
#31065=CARTESIAN_POINT('Ctrl Pts',(-1.67661303372963,-0.636309800095154,
11.2549667049729));
#31066=CARTESIAN_POINT('Ctrl Pts',(-1.62024236111357,-0.319434907277136,
11.1999267400399));
#31067=CARTESIAN_POINT('Ctrl Pts',(-1.59734283762842,-0.158333333333322,
11.1836644064143));
#31068=CARTESIAN_POINT('Ctrl Pts',(-1.57606607100608,0.158333333333324,
11.1922991148789));
#31069=CARTESIAN_POINT('Ctrl Pts',(-1.57850038582121,0.319434907277148,
11.2168226451961));
#31070=CARTESIAN_POINT('Ctrl Pts',(-1.58987873169088,0.636309800095166,
11.2902117061397));
#31071=CARTESIAN_POINT('Ctrl Pts',(-1.6066555036954,0.794772684000786,11.3464567262519));
#31072=CARTESIAN_POINT('Ctrl Pts',(-1.63423517695353,1.06847604194573,11.4609670321102));
#31073=CARTESIAN_POINT('Ctrl Pts',(-1.64786544209433,1.18514270861305,11.517579383574));
#31074=CARTESIAN_POINT('Ctrl Pts',(-1.66318775375007,1.30000000000192,11.5812368181202));
#31075=CARTESIAN_POINT('Ctrl Pts',(-1.85439311555595,-1.30000000000162,
11.479046302207));
#31076=CARTESIAN_POINT('Ctrl Pts',(-1.81905279421378,-1.18514270861286,
11.4186174863998));
#31077=CARTESIAN_POINT('Ctrl Pts',(-1.78561431754195,-1.06847604194563,
11.3664538237022));
#31078=CARTESIAN_POINT('Ctrl Pts',(-1.71275838873707,-0.794772684000798,
11.2650394846877));
#31079=CARTESIAN_POINT('Ctrl Pts',(-1.66915843970215,-0.636309800095153,
11.2205097819443));
#31080=CARTESIAN_POINT('Ctrl Pts',(-1.61171114271454,-0.319434907277136,
11.1656297732224));
#31081=CARTESIAN_POINT('Ctrl Pts',(-1.59001006088378,-0.158333333333322,
11.1505468454814));
#31082=CARTESIAN_POINT('Ctrl Pts',(-1.56976350919437,0.158333333333324,
11.1588237730732));
#31083=CARTESIAN_POINT('Ctrl Pts',(-1.57276507097241,0.319434907277148,
11.181547746742));
#31084=CARTESIAN_POINT('Ctrl Pts',(-1.58582040791484,0.636309800095165,
11.2545825061741));
#31085=CARTESIAN_POINT('Ctrl Pts',(-1.60409543978382,0.794772684000785,
11.3095345616161));
#31086=CARTESIAN_POINT('Ctrl Pts',(-1.63311358253654,1.06847604194572,11.4287799832022));
#31087=CARTESIAN_POINT('Ctrl Pts',(-1.64722663290145,1.18514270861305,11.4887710035572));
#31088=CARTESIAN_POINT('Ctrl Pts',(-1.66289185486174,1.30000000000192,11.5571361197408));
#31089=CARTESIAN_POINT('Ctrl Pts',(-1.85283978068215,-1.30000000000165,
11.4613539877658));
#31090=CARTESIAN_POINT('Ctrl Pts',(-1.81653046021035,-1.18514270861288,
11.3977033856574));
#31091=CARTESIAN_POINT('Ctrl Pts',(-1.78227987318513,-1.06847604194565,
11.3432193821066));
#31092=CARTESIAN_POINT('Ctrl Pts',(-1.70791025146048,-0.794772684000815,
11.2385271108567));
#31093=CARTESIAN_POINT('Ctrl Pts',(-1.66388043844242,-0.636309800095166,
11.1948258070879));
#31094=CARTESIAN_POINT('Ctrl Pts',(-1.60549196134081,-0.319434907277143,
11.1401340976286));
#31095=CARTESIAN_POINT('Ctrl Pts',(-1.58304092552731,-0.158333333333325,
11.1264343755906));
#31096=CARTESIAN_POINT('Ctrl Pts',(-1.56306004713795,0.158333333333327,
11.1345883393377));
#31097=CARTESIAN_POINT('Ctrl Pts',(-1.56688524947397,0.319434907277154,
11.1558281168516));
#31098=CARTESIAN_POINT('Ctrl Pts',(-1.58181398704839,0.636309800095178,
11.2283793503045));
#31099=CARTESIAN_POINT('Ctrl Pts',(-1.60173505635853,0.7947726840008,11.2821786309543));
#31100=CARTESIAN_POINT('Ctrl Pts',(-1.63288796102298,1.06847604194575,11.4046189681354));
#31101=CARTESIAN_POINT('Ctrl Pts',(-1.64789044572972,1.18514270861308,11.4669682801649));
#31102=CARTESIAN_POINT('Ctrl Pts',(-1.6644104770428,1.30000000000195,11.5386670191196));
#31103=CARTESIAN_POINT('Ctrl Pts',(-1.85127630062499,-1.30000000000166,
11.4435752287505));
#31104=CARTESIAN_POINT('Ctrl Pts',(-1.81422237239857,-1.1851427086129,11.3764712734879));
#31105=CARTESIAN_POINT('Ctrl Pts',(-1.77912863126938,-1.06847604194567,
11.3195571370201));
#31106=CARTESIAN_POINT('Ctrl Pts',(-1.70258349311097,-0.794772684000825,
11.2116146160284));
#31107=CARTESIAN_POINT('Ctrl Pts',(-1.65551483630903,-0.636309800095177,
11.1695933113041));
#31108=CARTESIAN_POINT('Ctrl Pts',(-1.5972515116615,-0.319434907277149,
11.1147106253092));
#31109=CARTESIAN_POINT('Ctrl Pts',(-1.57844403382631,-0.158333333333327,
11.1010015815054));
#31110=CARTESIAN_POINT('Ctrl Pts',(-1.55960633153799,0.158333333333329,
11.1087413101428));
#31111=CARTESIAN_POINT('Ctrl Pts',(-1.56165830827601,0.319434907277156,
11.1292984694153));
#31112=CARTESIAN_POINT('Ctrl Pts',(-1.5773092958189,0.636309800095185,11.2017625771917));
#31113=CARTESIAN_POINT('Ctrl Pts',(-1.59911202315622,0.794772684000816,
11.2543443596096));
#31114=CARTESIAN_POINT('Ctrl Pts',(-1.63186631980178,1.06847604194577,11.3802996735384));
#31115=CARTESIAN_POINT('Ctrl Pts',(-1.64747792500286,1.1851427086131,11.4451896980575));
#31116=CARTESIAN_POINT('Ctrl Pts',(-1.66452301405345,1.30000000000196,11.5204483588001));
#31117=CARTESIAN_POINT('Ctrl Pts',(-1.84999209719009,-1.30000000000168,
11.428875041091));
#31118=CARTESIAN_POINT('Ctrl Pts',(-1.81145567664774,-1.18514270861291,
11.3594133583039));
#31119=CARTESIAN_POINT('Ctrl Pts',(-1.77547447896192,-1.06847604194568,
11.3007184692798));
#31120=CARTESIAN_POINT('Ctrl Pts',(-1.69825379026308,-0.794772684000835,
11.1899949812443));
#31121=CARTESIAN_POINT('Ctrl Pts',(-1.65307034145157,-0.636309800095182,
11.1479416751912));
#31122=CARTESIAN_POINT('Ctrl Pts',(-1.59561809421317,-0.319434907277151,
11.0927623076994));
#31123=CARTESIAN_POINT('Ctrl Pts',(-1.57728391425471,-0.158333333333329,
11.0798877614763));
#31124=CARTESIAN_POINT('Ctrl Pts',(-1.55783439338415,0.158333333333331,
11.0878072633641));
#31125=CARTESIAN_POINT('Ctrl Pts',(-1.55789660512953,0.31943490727716,11.1079948388319));
#31126=CARTESIAN_POINT('Ctrl Pts',(-1.57333298878991,0.636309800095192,
11.180541002553));
#31127=CARTESIAN_POINT('Ctrl Pts',(-1.59648543095614,0.794772684000821,
11.2320874284867));
#31128=CARTESIAN_POINT('Ctrl Pts',(-1.63042741542663,1.06847604194577,11.3606986517709));
#31129=CARTESIAN_POINT('Ctrl Pts',(-1.64657384485488,1.18514270861311,11.4275162264943));
#31130=CARTESIAN_POINT('Ctrl Pts',(-1.66417447630853,1.30000000000197,11.5054803428965));
#31131=CARTESIAN_POINT('Ctrl Pts',(-1.84771283470326,-1.30000000000168,
11.4113225100421));
#31132=CARTESIAN_POINT('Ctrl Pts',(-1.80731363076414,-1.18514270861292,
11.3386533475872));
#31133=CARTESIAN_POINT('Ctrl Pts',(-1.77035638698582,-1.06847604194568,
11.2774682075166));
#31134=CARTESIAN_POINT('Ctrl Pts',(-1.69292937712006,-0.794772684000837,
11.1626486829874));
#31135=CARTESIAN_POINT('Ctrl Pts',(-1.65105873820579,-0.636309800095186,
11.120072742534));
#31136=CARTESIAN_POINT('Ctrl Pts',(-1.59560967356912,-0.319434907277153,
11.0640491644009));
#31137=CARTESIAN_POINT('Ctrl Pts',(-1.57811365915877,-0.158333333333329,
11.0522220810441));
#31138=CARTESIAN_POINT('Ctrl Pts',(-1.55877072607704,0.158333333333331,
11.0600832218156));
#31139=CARTESIAN_POINT('Ctrl Pts',(-1.55780038665591,0.319434907277161,
11.0792447767487));
#31140=CARTESIAN_POINT('Ctrl Pts',(-1.57206376052553,0.636309800095195,
11.1523537198416));
#31141=CARTESIAN_POINT('Ctrl Pts',(-1.59362547973182,0.794772684000825,
11.2038774329937));
#31142=CARTESIAN_POINT('Ctrl Pts',(-1.62793948407771,1.06847604194578,11.3365871526014));
#31143=CARTESIAN_POINT('Ctrl Pts',(-1.64475372341218,1.18514270861312,11.4060302996696));
#31144=CARTESIAN_POINT('Ctrl Pts',(-1.66352894105892,1.30000000000199,11.4874714735672));
#31145=CARTESIAN_POINT('Ctrl Pts',(-1.84624880074947,-1.30000000000171,
11.3993427675283));
#31146=CARTESIAN_POINT('Ctrl Pts',(-1.80327012405174,-1.18514270861294,
11.3249050934222));
#31147=CARTESIAN_POINT('Ctrl Pts',(-1.76517783186742,-1.0684760419457,11.2622670815724));
#31148=CARTESIAN_POINT('Ctrl Pts',(-1.68846554232873,-0.794772684000851,
11.1448203238348));
#31149=CARTESIAN_POINT('Ctrl Pts',(-1.65309822965784,-0.636309800095197,
11.1012255285408));
#31150=CARTESIAN_POINT('Ctrl Pts',(-1.60107891377445,-0.319434907277159,
11.0445426182858));
#31151=CARTESIAN_POINT('Ctrl Pts',(-1.58369000879615,-0.158333333333332,
11.0337845707418));
#31152=CARTESIAN_POINT('Ctrl Pts',(-1.56451256417064,0.158333333333334,
11.0416309199903));
#31153=CARTESIAN_POINT('Ctrl Pts',(-1.56349013317763,0.319434907277167,
11.0598112207703));
#31154=CARTESIAN_POINT('Ctrl Pts',(-1.5748858670137,0.636309800095206,11.1333404325303));
#31155=CARTESIAN_POINT('Ctrl Pts',(-1.59090434066293,0.79477268400084,11.1852921644308));
#31156=CARTESIAN_POINT('Ctrl Pts',(-1.62444818679958,1.0684760419458,11.3206583385472));
#31157=CARTESIAN_POINT('Ctrl Pts',(-1.6421192747162,1.18514270861313,11.3917118019926));
#31158=CARTESIAN_POINT('Ctrl Pts',(-1.66294156247886,1.300000000002,11.4752237279192));
#31159=CARTESIAN_POINT('Ctrl Pts',(-1.84783999216086,-1.30000000000171,
11.3908891462741));
#31160=CARTESIAN_POINT('Ctrl Pts',(-1.80484358765992,-1.18514270861294,
11.3167021552094));
#31161=CARTESIAN_POINT('Ctrl Pts',(-1.76706466618289,-1.0684760419457,11.254208104176));
#31162=CARTESIAN_POINT('Ctrl Pts',(-1.69184122946293,-0.794772684000851,
11.1368473750342));
#31163=CARTESIAN_POINT('Ctrl Pts',(-1.65901382561028,-0.636309800095197,
11.0928893630096));
#31164=CARTESIAN_POINT('Ctrl Pts',(-1.60867204426711,-0.319434907277159,
11.0360319972763));
#31165=CARTESIAN_POINT('Ctrl Pts',(-1.59125278366871,-0.158333333333332,
11.0252313037607));
#31166=CARTESIAN_POINT('Ctrl Pts',(-1.57231214945024,0.158333333333334,
11.033074834932));
#31167=CARTESIAN_POINT('Ctrl Pts',(-1.57183510628244,0.319434907277167,
11.0512628906174));
#31168=CARTESIAN_POINT('Ctrl Pts',(-1.58146895355656,0.636309800095206,
11.1250261480047));
#31169=CARTESIAN_POINT('Ctrl Pts',(-1.59387972389892,0.79477268400084,11.1775265523141));
#31170=CARTESIAN_POINT('Ctrl Pts',(-1.62608364872306,1.0684760419458,11.31276909021));
#31171=CARTESIAN_POINT('Ctrl Pts',(-1.64375431751357,1.18514270861313,11.3836121285189));
#31172=CARTESIAN_POINT('Ctrl Pts',(-1.6651557693112,1.300000000002,11.4667567217115));
#31173=CARTESIAN_POINT('Ctrl Pts',(-1.84783999216022,-1.3,11.390889146273));
#31174=CARTESIAN_POINT('Ctrl Pts',(-1.80484358765955,-1.18514270861178,
11.3167021552088));
#31175=CARTESIAN_POINT('Ctrl Pts',(-1.76706466618273,-1.06847604194512,
11.2542081041758));
#31176=CARTESIAN_POINT('Ctrl Pts',(-1.69184122946293,-0.794772684000851,
11.1368473750342));
#31177=CARTESIAN_POINT('Ctrl Pts',(-1.65901382561028,-0.636309800095197,
11.0928893630096));
#31178=CARTESIAN_POINT('Ctrl Pts',(-1.60867204426711,-0.319434907277159,
11.0360319972763));
#31179=CARTESIAN_POINT('Ctrl Pts',(-1.59125278366871,-0.158333333333332,
11.0252313037607));
#31180=CARTESIAN_POINT('Ctrl Pts',(-1.57231214945024,0.158333333333334,
11.0330748349321));
#31181=CARTESIAN_POINT('Ctrl Pts',(-1.57183510628244,0.319434907277167,
11.0512628906174));
#31182=CARTESIAN_POINT('Ctrl Pts',(-1.58146895355656,0.636309800095206,
11.1250261480047));
#31183=CARTESIAN_POINT('Ctrl Pts',(-1.59387972389892,0.79477268400084,11.1775265523141));
#31184=CARTESIAN_POINT('Ctrl Pts',(-1.62608364872298,1.06847604194511,11.3127690902096));
#31185=CARTESIAN_POINT('Ctrl Pts',(-1.64375431751336,1.18514270861178,11.3836121285181));
#31186=CARTESIAN_POINT('Ctrl Pts',(-1.66515576931083,1.3,11.46675672171));
#31187=CARTESIAN_POINT('',(-1.81605431981429,-1.2,11.8048286295457));
#31188=CARTESIAN_POINT('Ctrl Pts',(-1.81605431981429,-1.2,11.8048286295457));
#31189=CARTESIAN_POINT('Ctrl Pts',(-1.8224693082947,-1.21682682923595,11.784210539298));
#31190=CARTESIAN_POINT('Ctrl Pts',(-1.82985488839019,-1.23325265804367,
11.7635755607979));
#31191=CARTESIAN_POINT('Ctrl Pts',(-1.83949601009123,-1.25864666032482,
11.7322887234019));
#31192=CARTESIAN_POINT('Ctrl Pts',(-1.84264810997846,-1.26676758279304,
11.7222392924128));
#31193=CARTESIAN_POINT('Ctrl Pts',(-1.84816644744311,-1.28141938382527,
11.704152355739));
#31194=CARTESIAN_POINT('Ctrl Pts',(-1.85203392632938,-1.2918719144206,11.6912581966035));
#31195=CARTESIAN_POINT('Ctrl Pts',(-1.85435152969323,-1.29845760775963,
11.6831734697223));
#31196=CARTESIAN_POINT('Ctrl Pts',(-1.85461944199808,-1.29922939086495,
11.6822274140474));
#31197=CARTESIAN_POINT('Ctrl Pts',(-1.85488174056831,-1.30000000000132,
11.681284830101));
#31198=CARTESIAN_POINT('',(-1.66957757387615,-0.653834841327789,11.859936772574));
#31199=CARTESIAN_POINT('Ctrl Pts',(-1.66957757394783,-0.653834841312355,
11.8599367725936));
#31200=CARTESIAN_POINT('Ctrl Pts',(-1.68331792633201,-0.711381237877385,
11.855013833653));
#31201=CARTESIAN_POINT('Ctrl Pts',(-1.69787379089,-0.767209767909677,11.8497287246474));
#31202=CARTESIAN_POINT('Ctrl Pts',(-1.72809951098891,-0.881631787835512,
11.8385815155201));
#31203=CARTESIAN_POINT('Ctrl Pts',(-1.7425600255146,-0.939021335919122,
11.8331784821344));
#31204=CARTESIAN_POINT('Ctrl Pts',(-1.7696575090577,-1.03714199995114,11.8228685450684));
#31205=CARTESIAN_POINT('Ctrl Pts',(-1.77053344226464,-1.03956800238679,
11.8225595794184));
#31206=CARTESIAN_POINT('Ctrl Pts',(-1.79854255260691,-1.13871222069374,
11.8117107047821));
#31207=CARTESIAN_POINT('Ctrl Pts',(-1.80621282339748,-1.16608661241795,
11.8087099231875));
#31208=CARTESIAN_POINT('Ctrl Pts',(-1.81605431981429,-1.2,11.8048286295457));
#31209=CARTESIAN_POINT('',(-1.53759581372313,0.653834841531101,11.9051353980115));
#31210=CARTESIAN_POINT('Ctrl Pts',(-1.53759581372313,0.65383484153109,11.9051353980115));
#31211=CARTESIAN_POINT('Ctrl Pts',(-1.54254163045076,0.575731842989942,
11.8637235483156));
#31212=CARTESIAN_POINT('Ctrl Pts',(-1.54764148398872,0.493687693661655,
11.8289822069527));
#31213=CARTESIAN_POINT('Ctrl Pts',(-1.55719804912996,0.338068747436532,
11.77922986672));
#31214=CARTESIAN_POINT('Ctrl Pts',(-1.56183985947927,0.265610792759769,
11.7619048341106));
#31215=CARTESIAN_POINT('Ctrl Pts',(-1.57217181134277,0.129684268044095,
11.7397699428473));
#31216=CARTESIAN_POINT('Ctrl Pts',(-1.57755262396628,0.0666361292480136,
11.7335211393323));
#31217=CARTESIAN_POINT('Ctrl Pts',(-1.58999125690634,-0.0594726585747696,
11.7288642981296));
#31218=CARTESIAN_POINT('Ctrl Pts',(-1.59712426033947,-0.122669256307556,
11.7304095744559));
#31219=CARTESIAN_POINT('Ctrl Pts',(-1.6137045597392,-0.26003767749522,11.7427010308845));
#31220=CARTESIAN_POINT('Ctrl Pts',(-1.62337943103797,-0.333902462181384,
11.7550658391387));
#31221=CARTESIAN_POINT('Ctrl Pts',(-1.64492749970498,-0.491493397975319,
11.7944688143506));
#31222=CARTESIAN_POINT('Ctrl Pts',(-1.65731202392141,-0.574905812515696,
11.8237247520087));
#31223=CARTESIAN_POINT('Ctrl Pts',(-1.66957757397199,-0.653834841350482,
11.8599367724921));
#31224=CARTESIAN_POINT('',(-1.60611120272456,1.2,11.8821903853306));
#31225=CARTESIAN_POINT('Ctrl Pts',(-1.60611120272456,1.2,11.8821903853306));
#31226=CARTESIAN_POINT('Ctrl Pts',(-1.59468073958328,1.13608709176311,11.886111326897));
#31227=CARTESIAN_POINT('Ctrl Pts',(-1.57885340667937,1.03790194753826,11.8914890260236));
#31228=CARTESIAN_POINT('Ctrl Pts',(-1.54889218107653,0.796896277865386,
11.9014466204779));
#31229=CARTESIAN_POINT('Ctrl Pts',(-1.54381784356845,0.741365964363796,
11.9031020947729));
#31230=CARTESIAN_POINT('Ctrl Pts',(-1.53759581372313,0.653834841531101,
11.9051353980115));
#31231=CARTESIAN_POINT('Ctrl Pts',(-1.64379217587217,1.29999999999989,11.762942831391));
#31232=CARTESIAN_POINT('Ctrl Pts',(-1.63815094958981,1.28313650166177,11.7828994633125));
#31233=CARTESIAN_POINT('Ctrl Pts',(-1.63164049333543,1.26654456688836,11.8028295456687));
#31234=CARTESIAN_POINT('Ctrl Pts',(-1.6213586730226,1.23847789472489,11.8361962431637));
#31235=CARTESIAN_POINT('Ctrl Pts',(-1.61473656949771,1.21946613476643,11.858652114516));
#31236=CARTESIAN_POINT('Ctrl Pts',(-1.60611120272456,1.2,11.8821903853306));
#31237=CARTESIAN_POINT('Ctrl Pts',(-1.84783999216022,-1.3,11.390889146273));
#31238=CARTESIAN_POINT('Ctrl Pts',(-1.80484358765955,-1.18514270861178,
11.3167021552088));
#31239=CARTESIAN_POINT('Ctrl Pts',(-1.76706466618273,-1.06847604194512,
11.2542081041758));
#31240=CARTESIAN_POINT('Ctrl Pts',(-1.69184122946293,-0.794772684000851,
11.1368473750342));
#31241=CARTESIAN_POINT('Ctrl Pts',(-1.65901382561028,-0.636309800095197,
11.0928893630096));
#31242=CARTESIAN_POINT('Ctrl Pts',(-1.60867204426711,-0.319434907277159,
11.0360319972763));
#31243=CARTESIAN_POINT('Ctrl Pts',(-1.59125278366871,-0.158333333333332,
11.0252313037607));
#31244=CARTESIAN_POINT('Ctrl Pts',(-1.57231214945024,0.158333333333334,
11.0330748349321));
#31245=CARTESIAN_POINT('Ctrl Pts',(-1.57183510628244,0.319434907277167,
11.0512628906174));
#31246=CARTESIAN_POINT('Ctrl Pts',(-1.58146895355656,0.636309800095206,
11.1250261480047));
#31247=CARTESIAN_POINT('Ctrl Pts',(-1.59387972389892,0.79477268400084,11.1775265523141));
#31248=CARTESIAN_POINT('Ctrl Pts',(-1.62608364872297,1.06847604194511,11.3127690902096));
#31249=CARTESIAN_POINT('Ctrl Pts',(-1.64375431751336,1.18514270861178,11.3836121285181));
#31250=CARTESIAN_POINT('Ctrl Pts',(-1.66515576931083,1.3,11.46675672171));
#31251=CARTESIAN_POINT('Ctrl Pts',(-1.91743049134307,-1.3,11.3580825661689));
#31252=CARTESIAN_POINT('Ctrl Pts',(-1.87294351908303,-1.18514270861178,
11.2847782487198));
#31253=CARTESIAN_POINT('Ctrl Pts',(-1.83415002075929,-1.06847604194512,
11.2229371776131));
#31254=CARTESIAN_POINT('Ctrl Pts',(-1.75768234278715,-0.794772684000851,
11.1065543243585));
#31255=CARTESIAN_POINT('Ctrl Pts',(-1.72556041438092,-0.636309800095197,
11.0624647739656));
#31256=CARTESIAN_POINT('Ctrl Pts',(-1.67587573316224,-0.319434907277159,
11.0057209978454));
#31257=CARTESIAN_POINT('Ctrl Pts',(-1.65965103821258,-0.158333333333332,
10.9945819779792));
#31258=CARTESIAN_POINT('Ctrl Pts',(-1.64085640284598,0.158333333333334,
11.0027534279408));
#31259=CARTESIAN_POINT('Ctrl Pts',(-1.6393286137645,0.319434907277167,11.0216028343905));
#31260=CARTESIAN_POINT('Ctrl Pts',(-1.64860718876712,0.636309800095206,
11.0959304186219));
#31261=CARTESIAN_POINT('Ctrl Pts',(-1.66044815183843,0.79477268400084,11.1488670770106));
#31262=CARTESIAN_POINT('Ctrl Pts',(-1.69421133997152,1.06847604194511,11.283839290143));
#31263=CARTESIAN_POINT('Ctrl Pts',(-1.71304615183609,1.18514270861178,11.3543652797717));
#31264=CARTESIAN_POINT('Ctrl Pts',(-1.73610094247183,1.3,11.4369927891775));
#31265=CARTESIAN_POINT('Ctrl Pts',(-1.98702099052593,-1.3,11.3252759860648));
#31266=CARTESIAN_POINT('Ctrl Pts',(-1.9410434505065,-1.18514270861178,11.2528543422308));
#31267=CARTESIAN_POINT('Ctrl Pts',(-1.90123537533586,-1.06847604194512,
11.1916662510505));
#31268=CARTESIAN_POINT('Ctrl Pts',(-1.82352345611138,-0.794772684000851,
11.0762612736829));
#31269=CARTESIAN_POINT('Ctrl Pts',(-1.79210700315155,-0.636309800095197,
11.0320401849215));
#31270=CARTESIAN_POINT('Ctrl Pts',(-1.74307942205737,-0.319434907277159,
10.9754099984145));
#31271=CARTESIAN_POINT('Ctrl Pts',(-1.72804929275646,-0.158333333333332,
10.9639326521977));
#31272=CARTESIAN_POINT('Ctrl Pts',(-1.70940065624173,0.158333333333334,
10.9724320209495));
#31273=CARTESIAN_POINT('Ctrl Pts',(-1.70682212124656,0.319434907277167,
10.9919427781636));
#31274=CARTESIAN_POINT('Ctrl Pts',(-1.71574542397769,0.636309800095206,
11.0668346892391));
#31275=CARTESIAN_POINT('Ctrl Pts',(-1.72701657977795,0.79477268400084,11.1202076017071));
#31276=CARTESIAN_POINT('Ctrl Pts',(-1.76233903122006,1.06847604194511,11.2549094900764));
#31277=CARTESIAN_POINT('Ctrl Pts',(-1.78233798615881,1.18514270861178,11.3251184310253));
#31278=CARTESIAN_POINT('Ctrl Pts',(-1.80704611563284,1.3,11.407228856645));
#31279=CARTESIAN_POINT('Ctrl Pts',(-2.05661148970878,-1.3,11.2924694059607));
#31280=CARTESIAN_POINT('Ctrl Pts',(-2.00914338192998,-1.18514270861178,
11.2209304357418));
#31281=CARTESIAN_POINT('Ctrl Pts',(-1.96832072991242,-1.06847604194512,
11.1603953244878));
#31282=CARTESIAN_POINT('Ctrl Pts',(-1.88936456943561,-0.794772684000851,
11.0459682230072));
#31283=CARTESIAN_POINT('Ctrl Pts',(-1.85865359192219,-0.636309800095197,
11.0016155958775));
#31284=CARTESIAN_POINT('Ctrl Pts',(-1.8102831109525,-0.319434907277159,
10.9450989989837));
#31285=CARTESIAN_POINT('Ctrl Pts',(-1.79644754730034,-0.158333333333332,
10.9332833264162));
#31286=CARTESIAN_POINT('Ctrl Pts',(-1.77794490963747,0.158333333333334,
10.9421106139582));
#31287=CARTESIAN_POINT('Ctrl Pts',(-1.77431562872862,0.319434907277167,
10.9622827219367));
#31288=CARTESIAN_POINT('Ctrl Pts',(-1.78288365918825,0.636309800095206,
11.0377389598563));
#31289=CARTESIAN_POINT('Ctrl Pts',(-1.79358500771746,0.79477268400084,11.0915481264036));
#31290=CARTESIAN_POINT('Ctrl Pts',(-1.83046672246861,1.06847604194511,11.2259796900098));
#31291=CARTESIAN_POINT('Ctrl Pts',(-1.85162982048154,1.18514270861178,11.2958715822789));
#31292=CARTESIAN_POINT('Ctrl Pts',(-1.87799128879385,1.3,11.3774649241125));
#31293=CARTESIAN_POINT('Ctrl Pts',(-2.05661148970878,-1.3,11.2924694059607));
#31294=CARTESIAN_POINT('Ctrl Pts',(-2.00914338192998,-1.18514270861178,
11.2209304357418));
#31295=CARTESIAN_POINT('Ctrl Pts',(-1.96832072991242,-1.06847604194512,
11.1603953244878));
#31296=CARTESIAN_POINT('Ctrl Pts',(-1.88936456943561,-0.794772684000851,
11.0459682230072));
#31297=CARTESIAN_POINT('Ctrl Pts',(-1.85865359192219,-0.636309800095197,
11.0016155958775));
#31298=CARTESIAN_POINT('Ctrl Pts',(-1.8102831109525,-0.319434907277159,
10.9450989989837));
#31299=CARTESIAN_POINT('Ctrl Pts',(-1.79644754730034,-0.158333333333332,
10.9332833264162));
#31300=CARTESIAN_POINT('Ctrl Pts',(-1.77794490963747,0.158333333333334,
10.9421106139582));
#31301=CARTESIAN_POINT('Ctrl Pts',(-1.77431562872862,0.319434907277167,
10.9622827219367));
#31302=CARTESIAN_POINT('Ctrl Pts',(-1.78288365918825,0.636309800095206,
11.0377389598563));
#31303=CARTESIAN_POINT('Ctrl Pts',(-1.79358500771746,0.79477268400084,11.0915481264036));
#31304=CARTESIAN_POINT('Ctrl Pts',(-1.83046672246861,1.06847604194511,11.2259796900098));
#31305=CARTESIAN_POINT('Ctrl Pts',(-1.85162982048154,1.18514270861178,11.2958715822789));
#31306=CARTESIAN_POINT('Ctrl Pts',(-1.87799128879385,1.3,11.3774649241125));
#31307=CARTESIAN_POINT('Ctrl Pts',(-2.05661148970901,-1.30000000000056,
11.2924694059611));
#31308=CARTESIAN_POINT('Ctrl Pts',(-2.00914338193012,-1.18514270861216,
11.220930435742));
#31309=CARTESIAN_POINT('Ctrl Pts',(-1.96832072991248,-1.06847604194531,
11.1603953244879));
#31310=CARTESIAN_POINT('Ctrl Pts',(-1.88936456943561,-0.794772684000851,
11.0459682230072));
#31311=CARTESIAN_POINT('Ctrl Pts',(-1.85865359192219,-0.636309800095197,
11.0016155958775));
#31312=CARTESIAN_POINT('Ctrl Pts',(-1.8102831109525,-0.319434907277159,
10.9450989989837));
#31313=CARTESIAN_POINT('Ctrl Pts',(-1.79644754730034,-0.158333333333332,
10.9332833264162));
#31314=CARTESIAN_POINT('Ctrl Pts',(-1.77794490963747,0.158333333333334,
10.9421106139582));
#31315=CARTESIAN_POINT('Ctrl Pts',(-1.77431562872862,0.319434907277167,
10.9622827219367));
#31316=CARTESIAN_POINT('Ctrl Pts',(-1.78288365918825,0.636309800095206,
11.0377389598563));
#31317=CARTESIAN_POINT('Ctrl Pts',(-1.79358500771746,0.79477268400084,11.0915481264036));
#31318=CARTESIAN_POINT('Ctrl Pts',(-1.83046672246879,1.06847604194647,11.2259796900104));
#31319=CARTESIAN_POINT('Ctrl Pts',(-1.85162982048202,1.18514270861445,11.2958715822805));
#31320=CARTESIAN_POINT('Ctrl Pts',(-1.87799128879475,1.30000000000394,11.3774649241153));
#31321=CARTESIAN_POINT('Ctrl Pts',(-2.06438529509448,-1.30000000000056,
11.296489462555));
#31322=CARTESIAN_POINT('Ctrl Pts',(-2.01625666951673,-1.18514270861216,
11.2251351015232));
#31323=CARTESIAN_POINT('Ctrl Pts',(-1.9752779216005,-1.06847604194531,11.1644588769034));
#31324=CARTESIAN_POINT('Ctrl Pts',(-1.89712646386988,-0.794772684000851,
11.0489532910601));
#31325=CARTESIAN_POINT('Ctrl Pts',(-1.86923725412316,-0.636309800095197,
11.0022867513961));
#31326=CARTESIAN_POINT('Ctrl Pts',(-1.82221963516386,-0.319434907277159,
10.9446174246915));
#31327=CARTESIAN_POINT('Ctrl Pts',(-1.8080248988176,-0.158333333333332,
10.9332122432533));
#31328=CARTESIAN_POINT('Ctrl Pts',(-1.78936170982529,0.158333333333334,
10.9422136295658));
#31329=CARTESIAN_POINT('Ctrl Pts',(-1.78572104868508,0.319434907277167,
10.9623346432573));
#31330=CARTESIAN_POINT('Ctrl Pts',(-1.79303694376686,0.636309800095206,
11.0389207988169));
#31331=CARTESIAN_POINT('Ctrl Pts',(-1.80176883893061,0.79477268400084,11.0943744460198));
#31332=CARTESIAN_POINT('Ctrl Pts',(-1.83771824839734,1.06847604194647,11.2299700072586));
#31333=CARTESIAN_POINT('Ctrl Pts',(-1.85877864421393,1.18514270861445,11.3001911079339));
#31334=CARTESIAN_POINT('Ctrl Pts',(-1.88533826854578,1.30000000000394,11.3819390151346));
#31335=CARTESIAN_POINT('Ctrl Pts',(-2.07310405152111,-1.30000000000032,
11.3051109272569));
#31336=CARTESIAN_POINT('Ctrl Pts',(-2.02516512349642,-1.18514270861194,
11.236643173689));
#31337=CARTESIAN_POINT('Ctrl Pts',(-1.98482162956526,-1.06847604194511,
11.1776687388379));
#31338=CARTESIAN_POINT('Ctrl Pts',(-1.90916706011344,-0.794772684000704,
11.063357461904));
#31339=CARTESIAN_POINT('Ctrl Pts',(-1.8852824344217,-0.63630980009508,11.0128761490054));
#31340=CARTESIAN_POINT('Ctrl Pts',(-1.84046911413487,-0.319434907277101,
10.953375594764));
#31341=CARTESIAN_POINT('Ctrl Pts',(-1.82555504877143,-0.158333333333303,
10.941293868259));
#31342=CARTESIAN_POINT('Ctrl Pts',(-1.80675081476022,0.158333333333305,
10.9504201941717));
#31343=CARTESIAN_POINT('Ctrl Pts',(-1.80381989210835,0.319434907277107,
10.9713399291468));
#31344=CARTESIAN_POINT('Ctrl Pts',(-1.80837642663847,0.636309800095088,
11.0500174340263));
#31345=CARTESIAN_POINT('Ctrl Pts',(-1.81207156347144,0.794772684000696,
11.1095781698092));
#31346=CARTESIAN_POINT('Ctrl Pts',(-1.8455999431735,1.06847604194627,11.2439466892858));
#31347=CARTESIAN_POINT('Ctrl Pts',(-1.86632992438822,1.18514270861423,11.312362147158));
#31348=CARTESIAN_POINT('Ctrl Pts',(-1.89327669359346,1.3000000000037,11.3910299096651));
#31349=CARTESIAN_POINT('Ctrl Pts',(-2.08604767365955,-1.30000000000023,
11.317649477437));
#31350=CARTESIAN_POINT('Ctrl Pts',(-2.03990164826027,-1.18514270861186,
11.2523901800366));
#31351=CARTESIAN_POINT('Ctrl Pts',(-2.00105983312491,-1.06847604194503,
11.195674735722));
#31352=CARTESIAN_POINT('Ctrl Pts',(-1.92820165679573,-0.794772684000648,
11.0843887232898));
#31353=CARTESIAN_POINT('Ctrl Pts',(-1.90537128487983,-0.636309800095034,
11.0327047049662));
#31354=CARTESIAN_POINT('Ctrl Pts',(-1.86177167481144,-0.319434907277077,
10.9727023630987));
#31355=CARTESIAN_POINT('Ctrl Pts',(-1.84678457427543,-0.158333333333292,
10.9591640112912));
#31356=CARTESIAN_POINT('Ctrl Pts',(-1.82789737514345,0.158333333333294,
10.9683136305511));
#31357=CARTESIAN_POINT('Ctrl Pts',(-1.82524821498833,0.319434907277085,
10.990526740857));
#31358=CARTESIAN_POINT('Ctrl Pts',(-1.82782788881483,0.636309800095043,
11.0701334555425));
#31359=CARTESIAN_POINT('Ctrl Pts',(-1.82881842603555,0.794772684000638,
11.131860745249));
#31360=CARTESIAN_POINT('Ctrl Pts',(-1.85943132258683,1.06847604194619,11.2633328009558));
#31361=CARTESIAN_POINT('Ctrl Pts',(-1.87897774624833,1.18514270861414,11.3293439797425));
#31362=CARTESIAN_POINT('Ctrl Pts',(-1.9048194049738,1.30000000000361,11.4044569559198));
#31363=CARTESIAN_POINT('Ctrl Pts',(-2.09697218826236,-1.30000000000006,
11.3278871439688));
#31364=CARTESIAN_POINT('Ctrl Pts',(-2.05251089756756,-1.18514270861171,
11.2647969922648));
#31365=CARTESIAN_POINT('Ctrl Pts',(-2.0147696008548,-1.0684760419449,11.2097346947087));
#31366=CARTESIAN_POINT('Ctrl Pts',(-1.9431041857565,-0.794772684000548,
11.1010757212276));
#31367=CARTESIAN_POINT('Ctrl Pts',(-1.91854905377933,-0.636309800094954,
11.0497439167426));
#31368=CARTESIAN_POINT('Ctrl Pts',(-1.87508506278343,-0.319434907277038,
10.9896831140813));
#31369=CARTESIAN_POINT('Ctrl Pts',(-1.86111833437904,-0.158333333333272,
10.9744552860704));
#31370=CARTESIAN_POINT('Ctrl Pts',(-1.84266347705537,0.158333333333274,
10.9833318705429));
#31371=CARTESIAN_POINT('Ctrl Pts',(-1.84013583062199,0.319434907277045,
11.0065378896911));
#31372=CARTESIAN_POINT('Ctrl Pts',(-1.84201524437907,0.636309800094964,
11.0865096183245));
#31373=CARTESIAN_POINT('Ctrl Pts',(-1.84208408340377,0.794772684000538,
11.149410442407));
#31374=CARTESIAN_POINT('Ctrl Pts',(-1.87112130174078,1.06847604194606,11.2785244138799));
#31375=CARTESIAN_POINT('Ctrl Pts',(-1.88988682069309,1.185142708614,11.3427315325958));
#31376=CARTESIAN_POINT('Ctrl Pts',(-1.91484872271451,1.30000000000345,11.4152571159209));
#31377=CARTESIAN_POINT('Ctrl Pts',(-2.10826479557406,-1.29999999999992,
11.3380338755581));
#31378=CARTESIAN_POINT('Ctrl Pts',(-2.0656602099202,-1.18514270861158,11.2773274665579));
#31379=CARTESIAN_POINT('Ctrl Pts',(-2.02912223104839,-1.06847604194478,
11.2241061455424));
#31380=CARTESIAN_POINT('Ctrl Pts',(-1.95872726574397,-0.794772684000462,
11.1184462977394));
#31381=CARTESIAN_POINT('Ctrl Pts',(-1.93243426015739,-0.636309800094885,
11.0675486006443));
#31382=CARTESIAN_POINT('Ctrl Pts',(-1.8886049936113,-0.319434907277003,
11.007826746438));
#31383=CARTESIAN_POINT('Ctrl Pts',(-1.87523037933012,-0.158333333333255,
10.9910809152724));
#31384=CARTESIAN_POINT('Ctrl Pts',(-1.8560745914034,0.158333333333257,11.0003296924322));
#31385=CARTESIAN_POINT('Ctrl Pts',(-1.85186465050229,0.319434907277009,
11.0256213410938));
#31386=CARTESIAN_POINT('Ctrl Pts',(-1.85347446833627,0.636309800094893,
11.1056141666609));
#31387=CARTESIAN_POINT('Ctrl Pts',(-1.85565912734136,0.794772684000451,
11.1679143238887));
#31388=CARTESIAN_POINT('Ctrl Pts',(-1.88383366212453,1.06847604194594,11.2938576588064));
#31389=CARTESIAN_POINT('Ctrl Pts',(-1.9016515493598,1.18514270861387,11.3561085364947));
#31390=CARTESIAN_POINT('Ctrl Pts',(-1.92509161169201,1.30000000000331,11.4260940888454));
#31391=CARTESIAN_POINT('Ctrl Pts',(-2.11798686606854,-1.29999999999981,
11.3455803565388));
#31392=CARTESIAN_POINT('Ctrl Pts',(-2.07682357731144,-1.18514270861148,
11.2866450754959));
#31393=CARTESIAN_POINT('Ctrl Pts',(-2.0411712851994,-1.0684760419447,11.2348234956709));
#31394=CARTESIAN_POINT('Ctrl Pts',(-1.97153886292524,-0.794772684000398,
11.1315393523081));
#31395=CARTESIAN_POINT('Ctrl Pts',(-1.94378698956596,-0.636309800094834,
11.0810582859973));
#31396=CARTESIAN_POINT('Ctrl Pts',(-1.89890182412223,-0.319434907276977,
11.0220543656774));
#31397=CARTESIAN_POINT('Ctrl Pts',(-1.88475293497587,-0.158333333333242,
11.0048933339137));
#31398=CARTESIAN_POINT('Ctrl Pts',(-1.86498170941202,0.158333333333244,
11.014460822773));
#31399=CARTESIAN_POINT('Ctrl Pts',(-1.8605942188333,0.319434907276985,11.0406385430365));
#31400=CARTESIAN_POINT('Ctrl Pts',(-1.86269152931723,0.636309800094844,
11.1202526899541));
#31401=CARTESIAN_POINT('Ctrl Pts',(-1.86684619478339,0.794772684000388,
11.1819377459642));
#31402=CARTESIAN_POINT('Ctrl Pts',(-1.89424975777036,1.06847604194586,11.3055989377497));
#31403=CARTESIAN_POINT('Ctrl Pts',(-1.9111333875259,1.18514270861377,11.3665161841555));
#31404=CARTESIAN_POINT('Ctrl Pts',(-1.93303866002193,1.3000000000032,11.4348223291416));
#31405=CARTESIAN_POINT('Ctrl Pts',(-2.12751552334184,-1.29999999999973,
11.3533054250362));
#31406=CARTESIAN_POINT('Ctrl Pts',(-2.08768657842924,-1.1851427086114,11.2962931641647));
#31407=CARTESIAN_POINT('Ctrl Pts',(-2.05287338555443,-1.06847604194463,
11.2459610975741));
#31408=CARTESIAN_POINT('Ctrl Pts',(-1.98403533626337,-0.794772684000345,
11.145116540012));
#31409=CARTESIAN_POINT('Ctrl Pts',(-1.9550943424084,-0.636309800094793,
11.0948592576465));
#31410=CARTESIAN_POINT('Ctrl Pts',(-1.9093049904265,-0.319434907276957,
11.0364660055729));
#31411=CARTESIAN_POINT('Ctrl Pts',(-1.89412945682592,-0.158333333333232,
11.0189783706396));
#31412=CARTESIAN_POINT('Ctrl Pts',(-1.87429743956021,0.158333333333234,
11.0285649155269));
#31413=CARTESIAN_POINT('Ctrl Pts',(-1.87105358272484,0.319434907276963,
11.0549689599644));
#31414=CARTESIAN_POINT('Ctrl Pts',(-1.87356912434942,0.636309800094801,
11.1342543312433));
#31415=CARTESIAN_POINT('Ctrl Pts',(-1.87794784535936,0.794772684000338,
11.1962927526475));
#31416=CARTESIAN_POINT('Ctrl Pts',(-1.90437513697839,1.06847604194579,11.317681492603));
#31417=CARTESIAN_POINT('Ctrl Pts',(-1.92053629934561,1.18514270861369,11.3770784479341));
#31418=CARTESIAN_POINT('Ctrl Pts',(-1.94141922876575,1.30000000000312,11.4433276709655));
#31419=CARTESIAN_POINT('Ctrl Pts',(-2.14304910682474,-1.29999999999967,
11.3675618927398));
#31420=CARTESIAN_POINT('Ctrl Pts',(-2.10599876682301,-1.18514270861135,
11.3135495276944));
#31421=CARTESIAN_POINT('Ctrl Pts',(-2.07304532033494,-1.06847604194458,
11.2655198289767));
#31422=CARTESIAN_POINT('Ctrl Pts',(-2.00638091023047,-0.794772684000311,
11.1683827726755));
#31423=CARTESIAN_POINT('Ctrl Pts',(-1.97576844951589,-0.636309800094764,
11.1183053583916));
#31424=CARTESIAN_POINT('Ctrl Pts',(-1.92881021894933,-0.319434907276942,
11.0607632253031));
#31425=CARTESIAN_POINT('Ctrl Pts',(-1.91226173434354,-0.158333333333225,
11.0425358743185));
#31426=CARTESIAN_POINT('Ctrl Pts',(-1.89148266149804,0.158333333333227,
11.0526393852624));
#31427=CARTESIAN_POINT('Ctrl Pts',(-1.88795508883333,0.319434907276951,
11.0806812541267));
#31428=CARTESIAN_POINT('Ctrl Pts',(-1.89115585204907,0.636309800094775,
11.1593921695946));
#31429=CARTESIAN_POINT('Ctrl Pts',(-1.89858527717453,0.794772684000302,
11.220508860524));
#31430=CARTESIAN_POINT('Ctrl Pts',(-1.92357473296657,1.06847604194574,11.3378270584154));
#31431=CARTESIAN_POINT('Ctrl Pts',(-1.93813670352488,1.18514270861364,11.3948012445658));
#31432=CARTESIAN_POINT('Ctrl Pts',(-1.95644363517964,1.30000000000306,11.4579669160667));
#31433=CARTESIAN_POINT('Ctrl Pts',(-2.16816701100096,-1.29999999999847,
11.3858847423421));
#31434=CARTESIAN_POINT('Ctrl Pts',(-2.13557075152151,-1.18514270861026,
11.3358096331527));
#31435=CARTESIAN_POINT('Ctrl Pts',(-2.10540159865792,-1.06847604194359,
11.2909739036088));
#31436=CARTESIAN_POINT('Ctrl Pts',(-2.04131192204839,-0.794772683999578,
11.1994984141206));
#31437=CARTESIAN_POINT('Ctrl Pts',(-2.00650415050177,-0.636309800094176,
11.1509629672446));
#31438=CARTESIAN_POINT('Ctrl Pts',(-1.95663189844875,-0.319434907276646,
11.0954873096538));
#31439=CARTESIAN_POINT('Ctrl Pts',(-1.93721841919561,-0.158333333333079,
11.0767127352415));
#31440=CARTESIAN_POINT('Ctrl Pts',(-1.91601584542966,0.158333333333081,
11.0870415141348));
#31441=CARTESIAN_POINT('Ctrl Pts',(-1.91530622987097,0.319434907276658,
11.1155647611286));
#31442=CARTESIAN_POINT('Ctrl Pts',(-1.91979154489423,0.636309800094188,
11.1932610324165));
#31443=CARTESIAN_POINT('Ctrl Pts',(-1.92870254854972,0.794772683999565,
11.2546762338425));
#31444=CARTESIAN_POINT('Ctrl Pts',(-1.95083582044778,1.06847604194475,11.3666316540899));
#31445=CARTESIAN_POINT('Ctrl Pts',(-1.96311770202887,1.18514270861255,11.4201456583241));
#31446=CARTESIAN_POINT('Ctrl Pts',(-1.97810079190486,1.30000000000186,11.4787123137243));
#31447=CARTESIAN_POINT('Ctrl Pts',(-2.19197084033917,-1.29999999999816,
11.405075726293));
#31448=CARTESIAN_POINT('Ctrl Pts',(-2.16287598261759,-1.18514270860997,
11.3596211368751));
#31449=CARTESIAN_POINT('Ctrl Pts',(-2.13519097617397,-1.06847604194334,
11.3182138002111));
#31450=CARTESIAN_POINT('Ctrl Pts',(-2.07449011141456,-0.794772683999387,
11.2319045325197));
#31451=CARTESIAN_POINT('Ctrl Pts',(-2.03887330153802,-0.636309800094021,
11.1826114252657));
#31452=CARTESIAN_POINT('Ctrl Pts',(-1.98785020262338,-0.319434907276568,
11.1280752760641));
#31453=CARTESIAN_POINT('Ctrl Pts',(-1.96567353851661,-0.15833333333304,
11.1087999397335));
#31454=CARTESIAN_POINT('Ctrl Pts',(-1.943487830973,0.158333333333042,11.119713787425));
#31455=CARTESIAN_POINT('Ctrl Pts',(-1.94395647822165,0.31943490727658,11.1496725896324));
#31456=CARTESIAN_POINT('Ctrl Pts',(-1.94881586676246,0.636309800094034,
11.2269087319269));
#31457=CARTESIAN_POINT('Ctrl Pts',(-1.95970581148777,0.794772683999372,
11.2883587248095));
#31458=CARTESIAN_POINT('Ctrl Pts',(-1.97841572141238,1.06847604194449,11.3952940028233));
#31459=CARTESIAN_POINT('Ctrl Pts',(-1.98804050414247,1.18514270861226,11.445568000792));
#31460=CARTESIAN_POINT('Ctrl Pts',(-1.99919124286672,1.30000000000154,11.4998276772196));
#31461=CARTESIAN_POINT('Ctrl Pts',(-2.21194072996136,-1.29999999999782,
11.4197523880558));
#31462=CARTESIAN_POINT('Ctrl Pts',(-2.18705625067301,-1.18514270860966,
11.3769694924721));
#31463=CARTESIAN_POINT('Ctrl Pts',(-2.16217394850673,-1.06847604194305,
11.3377137699941));
#31464=CARTESIAN_POINT('Ctrl Pts',(-2.10469588240273,-0.794772683999173,
11.2551736734718));
#31465=CARTESIAN_POINT('Ctrl Pts',(-2.06636629065357,-0.636309800093855,
11.206781684638));
#31466=CARTESIAN_POINT('Ctrl Pts',(-2.01361252053818,-0.319434907276486,
11.1536123775203));
#31467=CARTESIAN_POINT('Ctrl Pts',(-1.98927994229085,-0.158333333332999,
11.1339191974918));
#31468=CARTESIAN_POINT('Ctrl Pts',(-1.96637611505289,0.158333333333001,
11.1452890494184));
#31469=CARTESIAN_POINT('Ctrl Pts',(-1.96811104626271,0.319434907276498,
11.1761945853261));
#31470=CARTESIAN_POINT('Ctrl Pts',(-1.97358770240202,0.636309800093869,
11.2528442702706));
#31471=CARTESIAN_POINT('Ctrl Pts',(-1.98631080264597,0.794772683999164,
11.3141127511188));
#31472=CARTESIAN_POINT('Ctrl Pts',(-2.00232560278451,1.06847604194421,11.416996424493));
#31473=CARTESIAN_POINT('Ctrl Pts',(-2.00977318852491,1.18514270861195,11.4647174726693));
#31474=CARTESIAN_POINT('Ctrl Pts',(-2.01773614643252,1.30000000000121,11.5156250390336));
#31475=CARTESIAN_POINT('Ctrl Pts',(-2.22718477672543,-1.29999999999765,
11.4305479831051));
#31476=CARTESIAN_POINT('Ctrl Pts',(-2.20446821519554,-1.18514270860951,
11.3904908738317));
#31477=CARTESIAN_POINT('Ctrl Pts',(-2.1810698502756,-1.06847604194292,11.3532988193024));
#31478=CARTESIAN_POINT('Ctrl Pts',(-2.12543984425841,-0.794772683999076,
11.2739965827059));
#31479=CARTESIAN_POINT('Ctrl Pts',(-2.08596510327014,-0.636309800093774,
11.2256122840007));
#31480=CARTESIAN_POINT('Ctrl Pts',(-2.03265922940549,-0.319434907276445,
11.1729441026475));
#31481=CARTESIAN_POINT('Ctrl Pts',(-2.00747278411166,-0.158333333332979,
11.1524323973261));
#31482=CARTESIAN_POINT('Ctrl Pts',(-1.98432743759838,0.158333333332981,
11.1639424191239));
#31483=CARTESIAN_POINT('Ctrl Pts',(-1.98680023512611,0.319434907276456,
11.1957039870647));
#31484=CARTESIAN_POINT('Ctrl Pts',(-1.99208136539881,0.636309800093787,
11.2723471795851));
#31485=CARTESIAN_POINT('Ctrl Pts',(-2.0050069749984,0.794772683999063,11.334249214994));
#31486=CARTESIAN_POINT('Ctrl Pts',(-2.01877976488453,1.06847604194408,11.4342362373978));
#31487=CARTESIAN_POINT('Ctrl Pts',(-2.0247430628523,1.1851427086118,11.4799430554902));
#31488=CARTESIAN_POINT('Ctrl Pts',(-2.03070792837825,1.30000000000104,11.5280760145603));
#31489=CARTESIAN_POINT('Ctrl Pts',(-2.24236803062261,-1.29999999999691,
11.4413662490845));
#31490=CARTESIAN_POINT('Ctrl Pts',(-2.22272970222264,-1.18514270860883,
11.4033485923955));
#31491=CARTESIAN_POINT('Ctrl Pts',(-2.20143912424778,-1.0684760419423,11.3677553119689));
#31492=CARTESIAN_POINT('Ctrl Pts',(-2.14843660291098,-0.794772683998616,
11.2911285079329));
#31493=CARTESIAN_POINT('Ctrl Pts',(-2.10748850912162,-0.636309800093407,
11.2430534145239));
#31494=CARTESIAN_POINT('Ctrl Pts',(-2.05311394288683,-0.31943490727626,
11.1912810537758));
#31495=CARTESIAN_POINT('Ctrl Pts',(-2.02616691220347,-0.158333333332887,
11.1705871219805));
#31496=CARTESIAN_POINT('Ctrl Pts',(-2.00238897095407,0.158333333332889,
11.1825197442794));
#31497=CARTESIAN_POINT('Ctrl Pts',(-2.00562061474378,0.319434907276271,
11.2151111091204));
#31498=CARTESIAN_POINT('Ctrl Pts',(-2.01143380800353,0.636309800093419,
11.2912610402889));
#31499=CARTESIAN_POINT('Ctrl Pts',(-2.02628200316612,0.794772683998605,
11.3526445276488));
#31500=CARTESIAN_POINT('Ctrl Pts',(-2.03777139291857,1.06847604194346,11.4497683742301));
#31501=CARTESIAN_POINT('Ctrl Pts',(-2.04181744495932,1.18514270861111,11.4937546572526));
#31502=CARTESIAN_POINT('Ctrl Pts',(-2.04493621794082,1.30000000000029,11.5396859089054));
#31503=CARTESIAN_POINT('Ctrl Pts',(-2.26249397180303,-1.29999999999639,
11.455874478958));
#31504=CARTESIAN_POINT('Ctrl Pts',(-2.24629708411541,-1.18514270860836,
11.421080626451));
#31505=CARTESIAN_POINT('Ctrl Pts',(-2.22739100720034,-1.06847604194188,
11.3879398428267));
#31506=CARTESIAN_POINT('Ctrl Pts',(-2.17745541829201,-0.794772683998302,
11.3151969226777));
#31507=CARTESIAN_POINT('Ctrl Pts',(-2.13502915182882,-0.636309800093156,
11.2671282925831));
#31508=CARTESIAN_POINT('Ctrl Pts',(-2.07969952072822,-0.319434907276135,
11.2161943144671));
#31509=CARTESIAN_POINT('Ctrl Pts',(-2.05070326474499,-0.158333333332825,
11.195046095051));
#31510=CARTESIAN_POINT('Ctrl Pts',(-2.02685371396135,0.158333333332827,
11.2070121729432));
#31511=CARTESIAN_POINT('Ctrl Pts',(-2.03237832409365,0.319434907276143,
11.239855936348));
#31512=CARTESIAN_POINT('Ctrl Pts',(-2.03835837233474,0.636309800093167,
11.3157150116269));
#31513=CARTESIAN_POINT('Ctrl Pts',(-2.05308349031875,0.794772683998294,
11.3782157436242));
#31514=CARTESIAN_POINT('Ctrl Pts',(-2.06112074423417,1.06847604194304,11.4717958121859));
#31515=CARTESIAN_POINT('Ctrl Pts',(-2.06291955728834,1.18514270861065,11.5132794028105));
#31516=CARTESIAN_POINT('Ctrl Pts',(-2.06303815398629,1.29999999999977,11.5557392398623));
#31517=CARTESIAN_POINT('Ctrl Pts',(-2.28098123996243,-1.29999999999548,
11.467871279756));
#31518=CARTESIAN_POINT('Ctrl Pts',(-2.26855348098431,-1.18514270860753,
11.4352971885243));
#31519=CARTESIAN_POINT('Ctrl Pts',(-2.25218384250273,-1.06847604194113,
11.4039495664119));
#31520=CARTESIAN_POINT('Ctrl Pts',(-2.20526017265208,-0.794772683997745,
11.3343636772815));
#31521=CARTESIAN_POINT('Ctrl Pts',(-2.16046735275002,-0.636309800092709,
11.2871715906424));
#31522=CARTESIAN_POINT('Ctrl Pts',(-2.10402724865593,-0.31943490727591,
11.2372344617707));
#31523=CARTESIAN_POINT('Ctrl Pts',(-2.07383776819597,-0.158333333332714,
11.2152981632221));
#31524=CARTESIAN_POINT('Ctrl Pts',(-2.04931561047445,0.158333333332716,
11.2277249232403));
#31525=CARTESIAN_POINT('Ctrl Pts',(-2.05506359872789,0.319434907275921,
11.26198334941));
#31526=CARTESIAN_POINT('Ctrl Pts',(-2.06138952335123,0.636309800092722,
11.3374460223415));
#31527=CARTESIAN_POINT('Ctrl Pts',(-2.07859263583547,0.794772683997734,
11.3991632269327));
#31528=CARTESIAN_POINT('Ctrl Pts',(-2.08373944708755,1.06847604194229,11.4895565975992));
#31529=CARTESIAN_POINT('Ctrl Pts',(-2.08313510061906,1.18514270860981,11.5291502348457));
#31530=CARTESIAN_POINT('Ctrl Pts',(-2.0796985437992,1.29999999999886,11.5692095685813));
#31531=CARTESIAN_POINT('Ctrl Pts',(-2.30191461963453,-1.29999999999489,
11.4817207869872));
#31532=CARTESIAN_POINT('Ctrl Pts',(-2.29295315639335,-1.185142708607,11.4523286421187));
#31533=CARTESIAN_POINT('Ctrl Pts',(-2.27910133602921,-1.06847604194065,
11.4233230213229));
#31534=CARTESIAN_POINT('Ctrl Pts',(-2.23580315667427,-0.794772683997392,
11.3572071826614));
#31535=CARTESIAN_POINT('Ctrl Pts',(-2.1907397046039,-0.636309800092424,
11.3091659470523));
#31536=CARTESIAN_POINT('Ctrl Pts',(-2.13331425086397,-0.319434907275766,
11.2601315080099));
#31537=CARTESIAN_POINT('Ctrl Pts',(-2.0999167008132,-0.158333333332642,
11.2386390748403));
#31538=CARTESIAN_POINT('Ctrl Pts',(-2.07468843330633,0.158333333332644,
11.251579126617));
#31539=CARTESIAN_POINT('Ctrl Pts',(-2.08264523630014,0.319434907275776,
11.2861132674822));
#31540=CARTESIAN_POINT('Ctrl Pts',(-2.08911533116864,0.636309800092434,
11.361298594492));
#31541=CARTESIAN_POINT('Ctrl Pts',(-2.10662134947467,0.794772683997376,
11.4238415251322));
#31542=CARTESIAN_POINT('Ctrl Pts',(-2.10824296875268,1.06847604194181,11.5107554791366));
#31543=CARTESIAN_POINT('Ctrl Pts',(-2.10526319437188,1.18514270860928,11.5479437308975));
#31544=CARTESIAN_POINT('Ctrl Pts',(-2.09860170671175,1.29999999999828,11.5846984042097));
#31545=CARTESIAN_POINT('Ctrl Pts',(-2.31440322914962,-1.29999999999441,
11.4907955972478));
#31546=CARTESIAN_POINT('Ctrl Pts',(-2.30831860217203,-1.18514270860656,
11.4628406234383));
#31547=CARTESIAN_POINT('Ctrl Pts',(-2.29642039607987,-1.06847604194026,
11.4350037608307));
#31548=CARTESIAN_POINT('Ctrl Pts',(-2.25550262902185,-0.794772683997096,
11.3709678999663));
#31549=CARTESIAN_POINT('Ctrl Pts',(-2.2086285196071,-0.63630980009219,11.3236523178589));
#31550=CARTESIAN_POINT('Ctrl Pts',(-2.15072419116017,-0.31943490727565,
11.2751115673957));
#31551=CARTESIAN_POINT('Ctrl Pts',(-2.116801471756,-0.158333333332584,11.2528240808836));
#31552=CARTESIAN_POINT('Ctrl Pts',(-2.09163308515834,0.158333333332586,
11.2657146730607));
#31553=CARTESIAN_POINT('Ctrl Pts',(-2.10047576784667,0.319434907275659,
11.3007542090159));
#31554=CARTESIAN_POINT('Ctrl Pts',(-2.10693394263024,0.636309800092201,
11.3758343691641));
#31555=CARTESIAN_POINT('Ctrl Pts',(-2.1247727595787,0.794772683997086,11.4388074749674));
#31556=CARTESIAN_POINT('Ctrl Pts',(-2.1240277074958,1.06847604194142,11.5236670809836));
#31557=CARTESIAN_POINT('Ctrl Pts',(-2.11943877826403,1.18514270860885,11.559440470131));
#31558=CARTESIAN_POINT('Ctrl Pts',(-2.11058342524029,1.2999999999978,11.5942546693395));
#31559=CARTESIAN_POINT('Ctrl Pts',(-2.33381671126052,-1.29999999999402,
11.5020369773312));
#31560=CARTESIAN_POINT('Ctrl Pts',(-2.33105482008487,-1.1851427086062,11.4766190968446));
#31561=CARTESIAN_POINT('Ctrl Pts',(-2.32150725055883,-1.06847604193994,
11.4507037635032));
#31562=CARTESIAN_POINT('Ctrl Pts',(-2.28377418050927,-0.794772683996859,
11.3896849435304));
#31563=CARTESIAN_POINT('Ctrl Pts',(-2.23600821794575,-0.636309800091998,
11.3421513828582));
#31564=CARTESIAN_POINT('Ctrl Pts',(-2.17711773843962,-0.319434907275552,
11.2945339994663));
#31565=CARTESIAN_POINT('Ctrl Pts',(-2.14099785861747,-0.158333333332536,
11.2722295838866));
#31566=CARTESIAN_POINT('Ctrl Pts',(-2.11471897948203,0.158333333332538,
11.2859386798493));
#31567=CARTESIAN_POINT('Ctrl Pts',(-2.12390517567732,0.319434907275562,
11.3223368294361));
#31568=CARTESIAN_POINT('Ctrl Pts',(-2.1306012601282,0.636309800092009,11.3970951742147));
#31569=CARTESIAN_POINT('Ctrl Pts',(-2.1508023531816,0.794772683996845,11.4593010662695));
#31570=CARTESIAN_POINT('Ctrl Pts',(-2.14716342126206,1.06847604194109,11.5409850223026));
#31571=CARTESIAN_POINT('Ctrl Pts',(-2.1402022302872,1.18514270860849,11.5748651329399));
#31572=CARTESIAN_POINT('Ctrl Pts',(-2.12785500712976,1.29999999999741,11.6072673963366));
#31573=CARTESIAN_POINT('Ctrl Pts',(-2.34670163233748,-1.29999999999275,
11.5107831115056));
#31574=CARTESIAN_POINT('Ctrl Pts',(-2.34671932800519,-1.18514270860504,
11.4868594265423));
#31575=CARTESIAN_POINT('Ctrl Pts',(-2.33907711788905,-1.06847604193889,
11.4621393907479));
#31576=CARTESIAN_POINT('Ctrl Pts',(-2.30372616898224,-0.794772683996075,
11.4031914331071));
#31577=CARTESIAN_POINT('Ctrl Pts',(-2.2542761703362,-0.636309800091375,
11.3563055316114));
#31578=CARTESIAN_POINT('Ctrl Pts',(-2.19515753628339,-0.319434907275241,
11.3090063394001));
#31579=CARTESIAN_POINT('Ctrl Pts',(-2.15873250633772,-0.158333333332381,
11.2857474611326));
#31580=CARTESIAN_POINT('Ctrl Pts',(-2.13280330580729,0.158333333332383,
11.2992036186574));
#31581=CARTESIAN_POINT('Ctrl Pts',(-2.14320558663257,0.319434907275247,
11.3358763363246));
#31582=CARTESIAN_POINT('Ctrl Pts',(-2.14969885791129,0.636309800091384,
11.4106709515121));
#31583=CARTESIAN_POINT('Ctrl Pts',(-2.16955001086733,0.794772683996067,
11.4737915836462));
#31584=CARTESIAN_POINT('Ctrl Pts',(-2.16314946430749,1.06847604194005,11.5537144851381));
#31585=CARTESIAN_POINT('Ctrl Pts',(-2.15447261846925,1.18514270860733,11.5862632140747));
#31586=CARTESIAN_POINT('Ctrl Pts',(-2.13988948623493,1.29999999999614,11.6167650093272));
#31587=CARTESIAN_POINT('Ctrl Pts',(-2.35856865684174,-1.29999999999248,
11.5184481151003));
#31588=CARTESIAN_POINT('Ctrl Pts',(-2.36094102694564,-1.1851427086048,11.4959831014653));
#31589=CARTESIAN_POINT('Ctrl Pts',(-2.35498789299465,-1.06847604193867,
11.4723582444834));
#31590=CARTESIAN_POINT('Ctrl Pts',(-2.32200138276934,-0.794772683995912,
11.4151006285611));
#31591=CARTESIAN_POINT('Ctrl Pts',(-2.27204948957197,-0.636309800091243,
11.3680128505829));
#31592=CARTESIAN_POINT('Ctrl Pts',(-2.21245168235206,-0.319434907275175,
11.3211993476087));
#31593=CARTESIAN_POINT('Ctrl Pts',(-2.17457512814538,-0.158333333332349,
11.297980516356));
#31594=CARTESIAN_POINT('Ctrl Pts',(-2.14813980789209,0.158333333332351,
11.3118224764547));
#31595=CARTESIAN_POINT('Ctrl Pts',(-2.15921124599767,0.319434907275182,
11.3490400011529));
#31596=CARTESIAN_POINT('Ctrl Pts',(-2.16571545678366,0.636309800091253,
11.4237293256518));
#31597=CARTESIAN_POINT('Ctrl Pts',(-2.18633433888062,0.794772683995904,
11.4868936219414));
#31598=CARTESIAN_POINT('Ctrl Pts',(-2.17783123474526,1.06847604193983,11.5649559143081));
#31599=CARTESIAN_POINT('Ctrl Pts',(-2.16763101665763,1.18514270860708,11.5962913793229));
#31600=CARTESIAN_POINT('Ctrl Pts',(-2.15091125919154,1.29999999999587,11.6251720354797));
#31601=CARTESIAN_POINT('Ctrl Pts',(-2.36390892297408,-1.2999999999924,11.5218051266847));
#31602=CARTESIAN_POINT('Ctrl Pts',(-2.36718189067206,-1.18514270860472,
11.5001007762633));
#31603=CARTESIAN_POINT('Ctrl Pts',(-2.36189429107058,-1.0684760419386,11.4770278263546));
#31604=CARTESIAN_POINT('Ctrl Pts',(-2.32990225521314,-0.79477268399586,
11.4205629577346));
#31605=CARTESIAN_POINT('Ctrl Pts',(-2.27992579179333,-0.636309800091202,
11.3732277329024));
#31606=CARTESIAN_POINT('Ctrl Pts',(-2.22021411103163,-0.319434907275154,
11.3265548252099));
#31607=CARTESIAN_POINT('Ctrl Pts',(-2.18172997762361,-0.158333333332338,
11.3033313636279));
#31608=CARTESIAN_POINT('Ctrl Pts',(-2.15506715175217,0.15833333333234,11.3173489222133));
#31609=CARTESIAN_POINT('Ctrl Pts',(-2.16635844001899,0.319434907275161,
11.3548663899172));
#31610=CARTESIAN_POINT('Ctrl Pts',(-2.17283947535757,0.636309800091211,
11.4295289514237));
#31611=CARTESIAN_POINT('Ctrl Pts',(-2.19382952706387,0.794772683995851,
11.4926875929646));
#31612=CARTESIAN_POINT('Ctrl Pts',(-2.18438606802361,1.06847604193976,11.5699268815541));
#31613=CARTESIAN_POINT('Ctrl Pts',(-2.17350190663026,1.18514270860701,11.6007285733569));
#31614=CARTESIAN_POINT('Ctrl Pts',(-2.15582130734746,1.29999999999578,11.6288979309297));
#31615=CARTESIAN_POINT('Ctrl Pts',(-2.3720492133645,-1.29999999999228,11.5267330346446));
#31616=CARTESIAN_POINT('Ctrl Pts',(-2.37680608844054,-1.18514270860461,
11.506060968131));
#31617=CARTESIAN_POINT('Ctrl Pts',(-2.37258429148656,-1.0684760419385,11.4837606717457));
#31618=CARTESIAN_POINT('Ctrl Pts',(-2.34208856738875,-0.794772683995788,
11.4284809892067));
#31619=CARTESIAN_POINT('Ctrl Pts',(-2.29179513196189,-0.636309800091144,
11.3810034797012));
#31620=CARTESIAN_POINT('Ctrl Pts',(-2.23181042817592,-0.319434907275125,
11.334624340559));
#31621=CARTESIAN_POINT('Ctrl Pts',(-2.19245200547176,-0.158333333332324,
11.3113608196081));
#31622=CARTESIAN_POINT('Ctrl Pts',(-2.16549565963411,0.158333333332326,
11.3256061047224));
#31623=CARTESIAN_POINT('Ctrl Pts',(-2.17720846473121,0.319434907275132,
11.3635064325329));
#31624=CARTESIAN_POINT('Ctrl Pts',(-2.18368902993222,0.636309800091154,
11.4381046901535));
#31625=CARTESIAN_POINT('Ctrl Pts',(-2.20520539861963,0.794772683995779,
11.5012787044382));
#31626=CARTESIAN_POINT('Ctrl Pts',(-2.19431129208499,1.06847604193966,11.577314022173));
#31627=CARTESIAN_POINT('Ctrl Pts',(-2.18237753636617,1.1851427086069,11.6073327529529));
#31628=CARTESIAN_POINT('Ctrl Pts',(-2.16322567998097,1.29999999999566,11.6344573428514));
#31629=CARTESIAN_POINT('Ctrl Pts',(-2.38026004860352,-1.29999999999144,
11.5315931029377));
#31630=CARTESIAN_POINT('Ctrl Pts',(-2.38672599277927,-1.18514270860384,
11.5117718614968));
#31631=CARTESIAN_POINT('Ctrl Pts',(-2.38368986891399,-1.06847604193781,
11.4901473215834));
#31632=CARTESIAN_POINT('Ctrl Pts',(-2.35472413735369,-0.794772683995274,
11.4360243281893));
#31633=CARTESIAN_POINT('Ctrl Pts',(-2.30368643572867,-0.636309800090732,
11.3887457787763));
#31634=CARTESIAN_POINT('Ctrl Pts',(-2.24327796333425,-0.319434907274918,
11.3427820318431));
#31635=CARTESIAN_POINT('Ctrl Pts',(-2.20303598723206,-0.158333333332221,
11.3194833619449));
#31636=CARTESIAN_POINT('Ctrl Pts',(-2.17598241412595,0.158333333332223,
11.3338110397047));
#31637=CARTESIAN_POINT('Ctrl Pts',(-2.1885018056849,0.319434907274926,11.3718066355807));
#31638=CARTESIAN_POINT('Ctrl Pts',(-2.19516682571112,0.636309800090742,
11.4462026984505));
#31639=CARTESIAN_POINT('Ctrl Pts',(-2.21716370777384,0.794772683995265,
11.509424941382));
#31640=CARTESIAN_POINT('Ctrl Pts',(-2.20465981764346,1.06847604193897,11.5843771335585));
#31641=CARTESIAN_POINT('Ctrl Pts',(-2.19156314759851,1.18514270860613,11.6136990798478));
#31642=CARTESIAN_POINT('Ctrl Pts',(-2.17078227823132,1.29999999999482,11.6398989456853));
#31643=CARTESIAN_POINT('Ctrl Pts',(-2.38838367499918,-1.29999999999133,
11.5365218435371));
#31644=CARTESIAN_POINT('Ctrl Pts',(-2.39641057934158,-1.18514270860375,
11.5176700758882));
#31645=CARTESIAN_POINT('Ctrl Pts',(-2.39448761826522,-1.06847604193772,
11.4967791690672));
#31646=CARTESIAN_POINT('Ctrl Pts',(-2.36705901391067,-0.794772683995211,
11.4438061756833));
#31647=CARTESIAN_POINT('Ctrl Pts',(-2.31563436231257,-0.636309800090681,
11.3964383534719));
#31648=CARTESIAN_POINT('Ctrl Pts',(-2.25488089277633,-0.319434907274892,
11.3508265038955));
#31649=CARTESIAN_POINT('Ctrl Pts',(-2.21361664280147,-0.158333333332209,
11.3276071052436));
#31650=CARTESIAN_POINT('Ctrl Pts',(-2.18637498304349,0.158333333332211,
11.342086594996));
#31651=CARTESIAN_POINT('Ctrl Pts',(-2.1996222621025,0.3194349072749,11.3802319045307));
#31652=CARTESIAN_POINT('Ctrl Pts',(-2.20646568518064,0.636309800090691,
11.4544281044756));
#31653=CARTESIAN_POINT('Ctrl Pts',(-2.22903619480044,0.794772683995201,
11.5176279418966));
#31654=CARTESIAN_POINT('Ctrl Pts',(-2.21497154076344,1.06847604193888,11.5914610534171));
#31655=CARTESIAN_POINT('Ctrl Pts',(-2.20072648927202,1.18514270860604,11.6200762175823));
#31656=CARTESIAN_POINT('Ctrl Pts',(-2.17832445387503,1.29999999999472,11.6453469277217));
#31657=CARTESIAN_POINT('Ctrl Pts',(-2.39384374823495,-1.29999999999126,
11.5397696257708));
#31658=CARTESIAN_POINT('Ctrl Pts',(-2.40293450860123,-1.18514270860368,
11.5215430360648));
#31659=CARTESIAN_POINT('Ctrl Pts',(-2.40176338657601,-1.06847604193766,
11.5011320141405));
#31660=CARTESIAN_POINT('Ctrl Pts',(-2.37535085920871,-0.794772683995164,
11.4489319948659));
#31661=CARTESIAN_POINT('Ctrl Pts',(-2.32358691483882,-0.636309800090644,
11.4015736207909));
#31662=CARTESIAN_POINT('Ctrl Pts',(-2.26260745230776,-0.319434907274874,
11.3561956820194));
#31663=CARTESIAN_POINT('Ctrl Pts',(-2.22075449856025,-0.158333333332199,
11.3329567614098));
#31664=CARTESIAN_POINT('Ctrl Pts',(-2.1933776976983,0.158333333332201,11.3475446147353));
#31665=CARTESIAN_POINT('Ctrl Pts',(-2.2070297755006,0.319434907274881,11.3858511686716));
#31666=CARTESIAN_POINT('Ctrl Pts',(-2.21392324748015,0.636309800090653,
11.4599662369897));
#31667=CARTESIAN_POINT('Ctrl Pts',(-2.23681589565793,0.794772683995154,
11.5231958510112));
#31668=CARTESIAN_POINT('Ctrl Pts',(-2.22172690592412,1.06847604193882,11.5962713636694));
#31669=CARTESIAN_POINT('Ctrl Pts',(-2.20674534455013,1.18514270860597,11.6243939658985));
#31670=CARTESIAN_POINT('Ctrl Pts',(-2.18331368635577,1.29999999999464,11.6490074886415));
#31671=CARTESIAN_POINT('Ctrl Pts',(-2.3993958962951,-1.29999999999108,11.5429379339209));
#31672=CARTESIAN_POINT('Ctrl Pts',(-2.40963711164426,-1.18514270860352,
11.5252625617807));
#31673=CARTESIAN_POINT('Ctrl Pts',(-2.40925885152419,-1.06847604193752,
11.5052961304459));
#31674=CARTESIAN_POINT('Ctrl Pts',(-2.38385188222345,-0.794772683995057,
11.4538768747274));
#31675=CARTESIAN_POINT('Ctrl Pts',(-2.33150560017621,-0.636309800090558,
11.4067303741552));
#31676=CARTESIAN_POINT('Ctrl Pts',(-2.27029307764192,-0.319434907274831,
11.3615972197224));
#31677=CARTESIAN_POINT('Ctrl Pts',(-2.22806961897634,-0.158333333332178,
11.3381674328317));
#31678=CARTESIAN_POINT('Ctrl Pts',(-2.20055719881342,0.15833333333218,11.3528635379026));
#31679=CARTESIAN_POINT('Ctrl Pts',(-2.21446773311546,0.319434907274838,
11.3914444408506));
#31680=CARTESIAN_POINT('Ctrl Pts',(-2.22127000615627,0.636309800090567,
11.4655856785406));
#31681=CARTESIAN_POINT('Ctrl Pts',(-2.24433616136474,0.794772683995047,
11.5289554442119));
#31682=CARTESIAN_POINT('Ctrl Pts',(-2.22824630643318,1.06847604193868,11.6012567828048));
#31683=CARTESIAN_POINT('Ctrl Pts',(-2.21258638767723,1.18514270860581,11.6288439582938));
#31684=CARTESIAN_POINT('Ctrl Pts',(-2.18823125217736,1.29999999999447,11.6527217388234));
#31685=CARTESIAN_POINT('Ctrl Pts',(-2.40498263771275,-1.2999999999909,11.5460747568237));
#31686=CARTESIAN_POINT('Ctrl Pts',(-2.41641862629916,-1.18514270860336,
11.5289131961289));
#31687=CARTESIAN_POINT('Ctrl Pts',(-2.41685823441742,-1.06847604193737,
11.5093701990312));
#31688=CARTESIAN_POINT('Ctrl Pts',(-2.39246997841415,-0.794772683994947,
11.4587203716772));
#31689=CARTESIAN_POINT('Ctrl Pts',(-2.33945608537769,-0.63630980009047,
11.4118556739238));
#31690=CARTESIAN_POINT('Ctrl Pts',(-2.27801195848589,-0.319434907274787,
11.3669690672671));
#31691=CARTESIAN_POINT('Ctrl Pts',(-2.23548655175409,-0.158333333332156,
11.343297255196));
#31692=CARTESIAN_POINT('Ctrl Pts',(-2.20785175166259,0.158333333332158,
11.3580926156387));
#31693=CARTESIAN_POINT('Ctrl Pts',(-2.22199769074485,0.319434907274794,
11.3969652894081));
#31694=CARTESIAN_POINT('Ctrl Pts',(-2.22866855381979,0.63630980009048,11.4711630031246));
#31695=CARTESIAN_POINT('Ctrl Pts',(-2.25185434580907,0.794772683994938,
11.5347125753992));
#31696=CARTESIAN_POINT('Ctrl Pts',(-2.23474272493949,1.06847604193853,11.6062561397551));
#31697=CARTESIAN_POINT('Ctrl Pts',(-2.21840523355752,1.18514270860564,11.6333079034982));
#31698=CARTESIAN_POINT('Ctrl Pts',(-2.19313723742002,1.29999999999429,11.6564428729249));
#31699=CARTESIAN_POINT('Ctrl Pts',(-2.40914654649501,-1.2999999999908,11.5484482846422));
#31700=CARTESIAN_POINT('Ctrl Pts',(-2.42145246870887,-1.18514270860326,
11.5316937523024));
#31701=CARTESIAN_POINT('Ctrl Pts',(-2.42249597593041,-1.06847604193728,
11.5124761826751));
#31702=CARTESIAN_POINT('Ctrl Pts',(-2.39888825469448,-0.794772683994884,
11.4623896435116));
#31703=CARTESIAN_POINT('Ctrl Pts',(-2.34547205339143,-0.636309800090419,
11.4156545845343));
#31704=CARTESIAN_POINT('Ctrl Pts',(-2.28386607035366,-0.319434907274761,
11.3709429071027));
#31705=CARTESIAN_POINT('Ctrl Pts',(-2.24103624516728,-0.158333333332144,
11.3471534745865));
#31706=CARTESIAN_POINT('Ctrl Pts',(-2.21331083745272,0.158333333332146,
11.3620235089939));
#31707=CARTESIAN_POINT('Ctrl Pts',(-2.22768593270914,0.319434907274768,
11.4010732922679));
#31708=CARTESIAN_POINT('Ctrl Pts',(-2.23430283336779,0.636309800090429,
11.4752791128073));
#31709=CARTESIAN_POINT('Ctrl Pts',(-2.25762873040171,0.794772683994874,
11.5389258277537));
#31710=CARTESIAN_POINT('Ctrl Pts',(-2.23972418478954,1.06847604193844,11.6099211871069));
#31711=CARTESIAN_POINT('Ctrl Pts',(-2.22284695037678,1.18514270860555,11.6365952450213));
#31712=CARTESIAN_POINT('Ctrl Pts',(-2.19684269591802,1.29999999999418,11.6592121004232));
#31713=CARTESIAN_POINT('Ctrl Pts',(-2.41258175685607,-1.29999999999069,
11.5504545132532));
#31714=CARTESIAN_POINT('Ctrl Pts',(-2.42557611387912,-1.18514270860317,
11.5340694313134));
#31715=CARTESIAN_POINT('Ctrl Pts',(-2.42710829624824,-1.0684760419372,11.5151351004672));
#31716=CARTESIAN_POINT('Ctrl Pts',(-2.40416802758222,-0.79477268399482,
11.4655037334637));
#31717=CARTESIAN_POINT('Ctrl Pts',(-2.35054178435821,-0.636309800090368,
11.418772956396));
#31718=CARTESIAN_POINT('Ctrl Pts',(-2.28881475441011,-0.319434907274735,
11.3741949147268));
#31719=CARTESIAN_POINT('Ctrl Pts',(-2.24563279714406,-0.158333333332131,
11.3503872817849));
#31720=CARTESIAN_POINT('Ctrl Pts',(-2.21783129393859,0.158333333332133,
11.3653210871155));
#31721=CARTESIAN_POINT('Ctrl Pts',(-2.2324594281046,0.319434907274742,11.404469400769));
#31722=CARTESIAN_POINT('Ctrl Pts',(-2.23908921925421,0.636309800090377,
11.4786377527717));
#31723=CARTESIAN_POINT('Ctrl Pts',(-2.26260060340433,0.794772683994809,
11.5423141082442));
#31724=CARTESIAN_POINT('Ctrl Pts',(-2.24400853998536,1.06847604193836,11.6128729407444));
#31725=CARTESIAN_POINT('Ctrl Pts',(-2.22664498479955,1.18514270860545,11.6392598442532));
#31726=CARTESIAN_POINT('Ctrl Pts',(-2.1999656897782,1.29999999999408,11.6614913471435));
#31727=CARTESIAN_POINT('Ctrl Pts',(-2.41479985369412,-1.29999999999066,
11.551770597191));
#31728=CARTESIAN_POINT('Ctrl Pts',(-2.42822503947843,-1.18514270860314,
11.5356393929169));
#31729=CARTESIAN_POINT('Ctrl Pts',(-2.43006810827712,-1.06847604193717,
11.5168947157906));
#31730=CARTESIAN_POINT('Ctrl Pts',(-2.40756895867542,-0.794772683994802,
11.4675531166573));
#31731=CARTESIAN_POINT('Ctrl Pts',(-2.35386136455652,-0.636309800090354,
11.4207795398731));
#31732=CARTESIAN_POINT('Ctrl Pts',(-2.29206364242793,-0.319434907274728,
11.3762815092146));
#31733=CARTESIAN_POINT('Ctrl Pts',(-2.24861335875392,-0.158333333332127,
11.3524939667356));
#31734=CARTESIAN_POINT('Ctrl Pts',(-2.2207617827267,0.158333333332129,11.3674701657722));
#31735=CARTESIAN_POINT('Ctrl Pts',(-2.23557703714212,0.319434907274735,
11.406664705906));
#31736=CARTESIAN_POINT('Ctrl Pts',(-2.2422389421051,0.636309800090363,11.4807906699131));
#31737=CARTESIAN_POINT('Ctrl Pts',(-2.26590157058328,0.794772683994792,
11.5444633217759));
#31738=CARTESIAN_POINT('Ctrl Pts',(-2.24685296736716,1.06847604193833,11.6147458579512));
#31739=CARTESIAN_POINT('Ctrl Pts',(-2.22915869582073,1.18514270860543,11.6409572171816));
#31740=CARTESIAN_POINT('Ctrl Pts',(-2.20201558723986,1.29999999999405,11.6629572299565));
#31741=CARTESIAN_POINT('Ctrl Pts',(-2.41582200093143,-1.29999999999066,
11.552379271273));
#31742=CARTESIAN_POINT('Ctrl Pts',(-2.42944422392667,-1.18514270860313,
11.5363667074415));
#31743=CARTESIAN_POINT('Ctrl Pts',(-2.43143011088096,-1.06847604193717,
11.5177100967283));
#31744=CARTESIAN_POINT('Ctrl Pts',(-2.40913564292502,-0.794772683994798,
11.4685013165023));
#31745=CARTESIAN_POINT('Ctrl Pts',(-2.3553968845436,-0.63630980009035,11.4217027331553));
#31746=CARTESIAN_POINT('Ctrl Pts',(-2.2935679446324,-0.319434907274726,
11.3772404685971));
#31747=CARTESIAN_POINT('Ctrl Pts',(-2.24999004172294,-0.158333333332126,
11.3534652817272));
#31748=CARTESIAN_POINT('Ctrl Pts',(-2.22211532483174,0.158333333332128,
11.3684611396057));
#31749=CARTESIAN_POINT('Ctrl Pts',(-2.23701876714905,0.319434907274733,
11.4076755865086));
#31750=CARTESIAN_POINT('Ctrl Pts',(-2.24369793613448,0.636309800090359,
11.4817801555651));
#31751=CARTESIAN_POINT('Ctrl Pts',(-2.26743402756379,0.794772683994788,
11.5454483435967));
#31752=CARTESIAN_POINT('Ctrl Pts',(-2.24817376393022,1.06847604193833,11.6156041394163));
#31753=CARTESIAN_POINT('Ctrl Pts',(-2.23032528206969,1.18514270860542,11.6417357041927));
#31754=CARTESIAN_POINT('Ctrl Pts',(-2.20296537281255,1.29999999999404,11.6636309892633));
#31755=CARTESIAN_POINT('Ctrl Pts',(-2.41633274985894,-1.29999999999066,
11.5526838631196));
#31756=CARTESIAN_POINT('Ctrl Pts',(-2.4300531426528,-1.18514270860313,11.5367309017281));
#31757=CARTESIAN_POINT('Ctrl Pts',(-2.43211031121549,-1.06847604193717,
11.5181184256399));
#31758=CARTESIAN_POINT('Ctrl Pts',(-2.40991840093643,-0.794772683994798,
11.4689758714796));
#31759=CARTESIAN_POINT('Ctrl Pts',(-2.35616528808526,-0.63630980009035,
11.4221637757094));
#31760=CARTESIAN_POINT('Ctrl Pts',(-2.29432104999001,-0.319434907274726,
11.3777191388923));
#31761=CARTESIAN_POINT('Ctrl Pts',(-2.25067868375102,-0.158333333332126,
11.3539506638623));
#31762=CARTESIAN_POINT('Ctrl Pts',(-2.22279239010064,0.158333333332128,
11.3689563687736));
#31763=CARTESIAN_POINT('Ctrl Pts',(-2.23774018786867,0.319434907274733,
11.4081805651302));
#31764=CARTESIAN_POINT('Ctrl Pts',(-2.2444284512897,0.636309800090359,11.4822740913695));
#31765=CARTESIAN_POINT('Ctrl Pts',(-2.26820204945816,0.794772683994787,
11.54593946188));
#31766=CARTESIAN_POINT('Ctrl Pts',(-2.24883578981785,1.06847604193833,11.6160320272022));
#31767=CARTESIAN_POINT('Ctrl Pts',(-2.230909898264,1.18514270860542,11.6421239338287));
#31768=CARTESIAN_POINT('Ctrl Pts',(-2.203441051364,1.29999999999404,11.663967272739));
#31769=CARTESIAN_POINT('Ctrl Pts',(-2.41675820700139,-1.29999999999065,
11.5529378166722));
#31770=CARTESIAN_POINT('Ctrl Pts',(-2.43056017544808,-1.18514270860313,
11.5370347104054));
#31771=CARTESIAN_POINT('Ctrl Pts',(-2.43267666240502,-1.06847604193716,
11.518459078027));
#31772=CARTESIAN_POINT('Ctrl Pts',(-2.41057037076349,-0.794772683994795,
11.4693715812357));
#31773=CARTESIAN_POINT('Ctrl Pts',(-2.35680614313646,-0.636309800090348,
11.4225475297451));
#31774=CARTESIAN_POINT('Ctrl Pts',(-2.29494934815928,-0.319434907274725,
11.3781174269183));
#31775=CARTESIAN_POINT('Ctrl Pts',(-2.25125276855931,-0.158333333332126,
11.3543549505202));
#31776=CARTESIAN_POINT('Ctrl Pts',(-2.22335681619686,0.158333333332128,
11.3693688811036));
#31777=CARTESIAN_POINT('Ctrl Pts',(-2.23834181768131,0.319434907274732,
11.4086010137786));
#31778=CARTESIAN_POINT('Ctrl Pts',(-2.24503793720342,0.636309800090357,
11.4826851317409));
#31779=CARTESIAN_POINT('Ctrl Pts',(-2.26884316755643,0.794772683994785,
11.5463478715594));
#31780=CARTESIAN_POINT('Ctrl Pts',(-2.24938848253282,1.06847604193832,11.6163878284211));
#31781=CARTESIAN_POINT('Ctrl Pts',(-2.23139792006516,1.18514270860542,11.6424468164652));
#31782=CARTESIAN_POINT('Ctrl Pts',(-2.20383800740949,1.29999999999404,11.664247090464));
#31783=CARTESIAN_POINT('Ctrl Pts',(-2.41705590659015,-1.29999999999065,
11.5531156734398));
#31784=CARTESIAN_POINT('Ctrl Pts',(-2.43091492013701,-1.18514270860313,
11.5372475088211));
#31785=CARTESIAN_POINT('Ctrl Pts',(-2.4330729216556,-1.06847604193717,11.5186976709358));
#31786=CARTESIAN_POINT('Ctrl Pts',(-2.41102665830558,-0.794772683994796,
11.4696486328263));
#31787=CARTESIAN_POINT('Ctrl Pts',(-2.3572549218525,-0.636309800090349,
11.4228159918964));
#31788=CARTESIAN_POINT('Ctrl Pts',(-2.29538951710301,-0.319434907274726,
11.3783959181394));
#31789=CARTESIAN_POINT('Ctrl Pts',(-2.25165502805312,-0.158333333332126,
11.3546376119136));
#31790=CARTESIAN_POINT('Ctrl Pts',(-2.22375232379798,0.158333333332128,
11.3696572959091));
#31791=CARTESIAN_POINT('Ctrl Pts',(-2.2387632088314,0.319434907274733,11.4088951096365));
#31792=CARTESIAN_POINT('Ctrl Pts',(-2.24546492778164,0.636309800090358,
11.4829725708656));
#31793=CARTESIAN_POINT('Ctrl Pts',(-2.26929268971541,0.794772683994786,
11.5466331714944));
#31794=CARTESIAN_POINT('Ctrl Pts',(-2.24977607999461,1.06847604193833,11.6166363340987));
#31795=CARTESIAN_POINT('Ctrl Pts',(-2.23174014485318,1.18514270860542,11.6426723646367));
#31796=CARTESIAN_POINT('Ctrl Pts',(-2.20411629175686,1.29999999999404,11.6644426504939));
#31797=CARTESIAN_POINT('Ctrl Pts',(-2.41722606302245,-1.29999999999065,
11.5532172741863));
#31798=CARTESIAN_POINT('Ctrl Pts',(-2.43111759854394,-1.18514270860313,
11.5373691393569));
#31799=CARTESIAN_POINT('Ctrl Pts',(-2.43329928412564,-1.06847604193716,
11.5188340736756));
#31800=CARTESIAN_POINT('Ctrl Pts',(-2.4112873183557,-0.794772683994793,
11.4698070162378));
#31801=CARTESIAN_POINT('Ctrl Pts',(-2.3575115020879,-0.636309800090347,
11.4229692923526));
#31802=CARTESIAN_POINT('Ctrl Pts',(-2.29564112459873,-0.319434907274725,
11.3785549922577));
#31803=CARTESIAN_POINT('Ctrl Pts',(-2.25188468402401,-0.158333333332125,
11.3547993039445));
#31804=CARTESIAN_POINT('Ctrl Pts',(-2.22397810772574,0.158333333332127,
11.3698222911059));
#31805=CARTESIAN_POINT('Ctrl Pts',(-2.23900405544359,0.319434907274732,
11.4090631384977));
#31806=CARTESIAN_POINT('Ctrl Pts',(-2.2457090050593,0.636309800090356,11.4831367708317));
#31807=CARTESIAN_POINT('Ctrl Pts',(-2.26954942789417,0.794772683994783,
11.5467963146545));
#31808=CARTESIAN_POINT('Ctrl Pts',(-2.24999742106405,1.06847604193832,11.6167784568709));
#31809=CARTESIAN_POINT('Ctrl Pts',(-2.23193558967195,1.18514270860541,11.6428013423576));
#31810=CARTESIAN_POINT('Ctrl Pts',(-2.2042752661713,1.29999999999404,11.6645544370595));
#31811=CARTESIAN_POINT('Ctrl Pts',(-2.42819110567103,-1.29999999999132,
11.559777914713));
#31812=CARTESIAN_POINT('Ctrl Pts',(-2.44418755880433,-1.18514270860374,
11.5452153494114));
#31813=CARTESIAN_POINT('Ctrl Pts',(-2.447901541625,-1.06847604193771,11.5276289970943));
#31814=CARTESIAN_POINT('Ctrl Pts',(-2.42810662139858,-0.794772683995203,
11.480015452192));
#31815=CARTESIAN_POINT('Ctrl Pts',(-2.37405249916826,-0.636309800090674,
11.4328626476282));
#31816=CARTESIAN_POINT('Ctrl Pts',(-2.31187591576949,-0.319434907274889,
11.3888090582204));
#31817=CARTESIAN_POINT('Ctrl Pts',(-2.26674213815886,-0.158333333332207,
11.3651910796362));
#31818=CARTESIAN_POINT('Ctrl Pts',(-2.238587891913,0.158333333332209,11.380425036069));
#31819=CARTESIAN_POINT('Ctrl Pts',(-2.25454393150171,0.319434907274896,
11.4198940053948));
#31820=CARTESIAN_POINT('Ctrl Pts',(-2.26145712152465,0.636309800090683,
11.4937212127157));
#31821=CARTESIAN_POINT('Ctrl Pts',(-2.28615700088231,0.794772683995192,
11.5572796140882));
#31822=CARTESIAN_POINT('Ctrl Pts',(-2.26432247843443,1.06847604193887,11.6259065144236));
#31823=CARTESIAN_POINT('Ctrl Pts',(-2.24458242658572,1.18514270860602,11.651088268924));
#31824=CARTESIAN_POINT('Ctrl Pts',(-2.21455367860727,1.2999999999947,11.6717457356466));
#31825=CARTESIAN_POINT('Ctrl Pts',(-2.4452524353986,-1.29999999999661,11.5689626063178));
#31826=CARTESIAN_POINT('Ctrl Pts',(-2.46485785577321,-1.18514270860856,
11.555909053355));
#31827=CARTESIAN_POINT('Ctrl Pts',(-2.47109284500115,-1.06847604194207,
11.5395304089526));
#31828=CARTESIAN_POINT('Ctrl Pts',(-2.45460854672865,-0.794772683998442,
11.4940108374389));
#31829=CARTESIAN_POINT('Ctrl Pts',(-2.39902048241243,-0.636309800093267,
11.4473280503375));
#31830=CARTESIAN_POINT('Ctrl Pts',(-2.33622754359863,-0.31943490727619,
11.4039687597331));
#31831=CARTESIAN_POINT('Ctrl Pts',(-2.28981669923967,-0.158333333332852,
11.3799513324971));
#31832=CARTESIAN_POINT('Ctrl Pts',(-2.26119977660626,0.158333333332854,
11.3955792241029));
#31833=CARTESIAN_POINT('Ctrl Pts',(-2.27812146022787,0.319434907276197,
11.4357148298775));
#31834=CARTESIAN_POINT('Ctrl Pts',(-2.28440047433871,0.636309800093275,
11.509908331257));
#31835=CARTESIAN_POINT('Ctrl Pts',(-2.30861800866693,0.79477268399843,11.5746559944769));
#31836=CARTESIAN_POINT('Ctrl Pts',(-2.28392282923828,1.06847604194322,11.6408880860855));
#31837=CARTESIAN_POINT('Ctrl Pts',(-2.26247078692541,1.18514270861085,11.6642386146762));
#31838=CARTESIAN_POINT('Ctrl Pts',(-2.23025633042783,1.3,11.6822702535409));
#31839=CARTESIAN_POINT('Ctrl Pts',(-2.46724316344813,-1.29999999999784,
11.5817116024117));
#31840=CARTESIAN_POINT('Ctrl Pts',(-2.49156329534275,-1.18514270860968,
11.5707273717748));
#31841=CARTESIAN_POINT('Ctrl Pts',(-2.50112410315566,-1.06847604194307,
11.5559728301234));
#31842=CARTESIAN_POINT('Ctrl Pts',(-2.48911449061508,-0.794772683999187,
11.5131767145811));
#31843=CARTESIAN_POINT('Ctrl Pts',(-2.43184874460611,-0.636309800093867,
11.4668385900733));
#31844=CARTESIAN_POINT('Ctrl Pts',(-2.36827119090855,-0.319434907276493,
11.4243665324868));
#31845=CARTESIAN_POINT('Ctrl Pts',(-2.31971696369294,-0.158333333333001,
11.4001531084736));
#31846=CARTESIAN_POINT('Ctrl Pts',(-2.29076029791301,0.158333333333003,
11.4160813995587));
#31847=CARTESIAN_POINT('Ctrl Pts',(-2.30932133201575,0.319434907276497,
11.4568243292661));
#31848=CARTESIAN_POINT('Ctrl Pts',(-2.31602757401349,0.636309800093875,
11.5305165380476));
#31849=CARTESIAN_POINT('Ctrl Pts',(-2.34232654690967,0.794772683999182,
11.5947733929765));
#31850=CARTESIAN_POINT('Ctrl Pts',(-2.3127375908089,1.06847604194423,11.6586016481313));
#31851=CARTESIAN_POINT('Ctrl Pts',(-2.287642941349,1.18514270861197,11.6805270508448));
#31852=CARTESIAN_POINT('Ctrl Pts',(-2.25026160514642,1.30000000000123,11.696748969685));
#31853=CARTESIAN_POINT('Ctrl Pts',(-2.47880653387082,-1.30000000000056,
11.5876140197912));
#31854=CARTESIAN_POINT('Ctrl Pts',(-2.5053034943636,-1.18514270861216,11.5778000280662));
#31855=CARTESIAN_POINT('Ctrl Pts',(-2.51643668958126,-1.06847604194531,
11.5639215937233));
#31856=CARTESIAN_POINT('Ctrl Pts',(-2.50666322642595,-0.794772684000851,
11.5224699584834));
#31857=CARTESIAN_POINT('Ctrl Pts',(-2.44892689462504,-0.636309800095197,
11.4759868772666));
#31858=CARTESIAN_POINT('Ctrl Pts',(-2.38514150298642,-0.319434907277159,
11.4338197429392));
#31859=CARTESIAN_POINT('Ctrl Pts',(-2.33567769709269,-0.158333333333332,
11.4094186534397));
#31860=CARTESIAN_POINT('Ctrl Pts',(-2.30625480759988,0.158333333333334,
11.4257498401733));
#31861=CARTESIAN_POINT('Ctrl Pts',(-2.32505056891377,0.319434907277167,
11.4672540947557));
#31862=CARTESIAN_POINT('Ctrl Pts',(-2.33143994443199,0.636309800095206,
11.5411142162616));
#31863=CARTESIAN_POINT('Ctrl Pts',(-2.35820372983969,0.79477268400084,11.6055491315694));
#31864=CARTESIAN_POINT('Ctrl Pts',(-2.32663344521572,1.06847604194647,11.667852136859));
#31865=CARTESIAN_POINT('Ctrl Pts',(-2.30018582393963,1.18514270861445,11.6887302009383));
#31866=CARTESIAN_POINT('Ctrl Pts',(-2.26095618780691,1.30000000000395,11.7035176666606));
#31867=CARTESIAN_POINT('Ctrl Pts',(-2.48455995069208,-1.30000000000056,
11.5905856245377));
#31868=CARTESIAN_POINT('Ctrl Pts',(-2.51213562603867,-1.18514270861216,
11.5813640954911));
#31869=CARTESIAN_POINT('Ctrl Pts',(-2.52404941520513,-1.06847604194531,
11.5679279706886));
#31870=CARTESIAN_POINT('Ctrl Pts',(-2.51539056129935,-0.794772684000851,
11.5271512751842));
#31871=CARTESIAN_POINT('Ctrl Pts',(-2.45746810794787,-0.636309800095197,
11.4805575163309));
#31872=CARTESIAN_POINT('Ctrl Pts',(-2.39351595813042,-0.319434907277159,
11.4385926643448));
#31873=CARTESIAN_POINT('Ctrl Pts',(-2.34340372597283,-0.158333333333332,
11.4142508800478));
#31874=CARTESIAN_POINT('Ctrl Pts',(-2.3138047860753,0.158333333333334,11.4307376305815));
#31875=CARTESIAN_POINT('Ctrl Pts',(-2.33301542000644,0.319434907277167,
11.4723857856749));
#31876=CARTESIAN_POINT('Ctrl Pts',(-2.3393300816685,0.636309800095206,11.5462634539526));
#31877=CARTESIAN_POINT('Ctrl Pts',(-2.36620091374559,0.79477268400084,11.6108904285002));
#31878=CARTESIAN_POINT('Ctrl Pts',(-2.33354901187538,1.06847604194647,11.6724986686556));
#31879=CARTESIAN_POINT('Ctrl Pts',(-2.30638156847317,1.18514270861445,11.6928839421724));
#31880=CARTESIAN_POINT('Ctrl Pts',(-2.26618048011623,1.30000000000395,11.706986564853));
#31881=CARTESIAN_POINT('',(-2.20682734928731,1.2,11.6308478929475));
#31882=CARTESIAN_POINT('Ctrl Pts',(-2.20682734928731,1.2,11.6308478929475));
#31883=CARTESIAN_POINT('Ctrl Pts',(-2.18722751564924,1.21680586990626,11.6218348082994));
#31884=CARTESIAN_POINT('Ctrl Pts',(-2.16687973003508,1.23316195266879,11.6136279694703));
#31885=CARTESIAN_POINT('Ctrl Pts',(-2.12794466941964,1.26665720486854,11.5953463142025));
#31886=CARTESIAN_POINT('Ctrl Pts',(-2.11129558646823,1.28061603972248,11.5878883456529));
#31887=CARTESIAN_POINT('Ctrl Pts',(-2.08916921284536,1.29999999999857,11.5769706419067));
#31888=CARTESIAN_POINT('',(-2.34584244559631,0.653834841342843,11.5588442527862));
#31889=CARTESIAN_POINT('Ctrl Pts',(-2.34584244556543,0.653834841328552,
11.5588442528477));
#31890=CARTESIAN_POINT('Ctrl Pts',(-2.33308818544499,0.710941609821211,
11.5657083395222));
#31891=CARTESIAN_POINT('Ctrl Pts',(-2.31925861336638,0.767441603499411,
11.5730759416769));
#31892=CARTESIAN_POINT('Ctrl Pts',(-2.29084677666368,0.881463280997958,
11.5880272054701));
#31893=CARTESIAN_POINT('Ctrl Pts',(-2.27703180365721,0.939232753787813,
11.5952229786298));
#31894=CARTESIAN_POINT('Ctrl Pts',(-2.25131149177042,1.03694567063666,11.6084232885134));
#31895=CARTESIAN_POINT('Ctrl Pts',(-2.25039295349595,1.03976101801352,11.6089199951471));
#31896=CARTESIAN_POINT('Ctrl Pts',(-2.22336742624557,1.1397561733151,11.6225869212586));
#31897=CARTESIAN_POINT('Ctrl Pts',(-2.21631092062426,1.16602124943616,11.6261245070176));
#31898=CARTESIAN_POINT('Ctrl Pts',(-2.20682734928732,1.2,11.6308478929475));
#31899=CARTESIAN_POINT('',(-2.46774460503229,-0.653834841531101,11.4910064745155));
#31900=CARTESIAN_POINT('Ctrl Pts',(-2.4677446050323,-0.653834841531096,
11.4910064745155));
#31901=CARTESIAN_POINT('Ctrl Pts',(-2.43366531823515,-0.575743557741863,
11.466975601479));
#31902=CARTESIAN_POINT('Ctrl Pts',(-2.40440869672623,-0.493700050753892,
11.4475328008353));
#31903=CARTESIAN_POINT('Ctrl Pts',(-2.36105542073859,-0.338105451951495,
11.4213410229621));
#31904=CARTESIAN_POINT('Ctrl Pts',(-2.34510240028127,-0.265657096721669,
11.413182399269));
#31905=CARTESIAN_POINT('Ctrl Pts',(-2.32174616561371,-0.129731483841709,
11.4060384736905));
#31906=CARTESIAN_POINT('Ctrl Pts',(-2.3134924786683,-0.0666595841288654,
11.4058576315973));
#31907=CARTESIAN_POINT('Ctrl Pts',(-2.30170738667741,0.0595017295460707,
11.4119861541816));
#31908=CARTESIAN_POINT('Ctrl Pts',(-2.2980945337294,0.122719333871996,11.4183180474692));
#31909=CARTESIAN_POINT('Ctrl Pts',(-2.29615087668656,0.260098698859542,
11.43886499628));
#31910=CARTESIAN_POINT('Ctrl Pts',(-2.29885542227659,0.333972211087808,
11.4543396536581));
#31911=CARTESIAN_POINT('Ctrl Pts',(-2.31369980548976,0.4915232539199,11.4967249168017));
#31912=CARTESIAN_POINT('Ctrl Pts',(-2.32714440364268,0.574928604049013,
11.525508188405));
#31913=CARTESIAN_POINT('Ctrl Pts',(-2.34584244548056,0.653834841363857,
11.5588442528014));
#31914=CARTESIAN_POINT('',(-2.40481962522456,-1.2,11.5265855556241));
#31915=CARTESIAN_POINT('Ctrl Pts',(-2.40481962522456,-1.2,11.5265855556241));
#31916=CARTESIAN_POINT('Ctrl Pts',(-2.41054630292152,-1.16532760456162,
11.5234025313348));
#31917=CARTESIAN_POINT('Ctrl Pts',(-2.42645100662694,-1.06865554280768,
11.5145509637945));
#31918=CARTESIAN_POINT('Ctrl Pts',(-2.46017068471683,-0.773244824243328,
11.4953835148662));
#31919=CARTESIAN_POINT('Ctrl Pts',(-2.46337028885984,-0.721311495190602,
11.4935221302712));
#31920=CARTESIAN_POINT('Ctrl Pts',(-2.4677446050323,-0.653834841531101,
11.4910064745155));
#31921=CARTESIAN_POINT('Ctrl Pts',(-2.2912385497941,-1.29999999999519,11.4746609114623));
#31922=CARTESIAN_POINT('Ctrl Pts',(-2.31023238688351,-1.28305568231735,
11.4837050274263));
#31923=CARTESIAN_POINT('Ctrl Pts',(-2.32942890430126,-1.26619847603817,
11.4924852393854));
#31924=CARTESIAN_POINT('Ctrl Pts',(-2.3518627461632,-1.24605776992158,11.5031844201827));
#31925=CARTESIAN_POINT('Ctrl Pts',(-2.36202118513148,-1.23682069842138,
11.5081629233068));
#31926=CARTESIAN_POINT('Ctrl Pts',(-2.3803328638717,-1.22104712035176,11.5160864571013));
#31927=CARTESIAN_POINT('Ctrl Pts',(-2.38516684913272,-1.21689694692977,
11.5181587343142));
#31928=CARTESIAN_POINT('Ctrl Pts',(-2.39187438277638,-1.21105168977261,
11.5211282035769));
#31929=CARTESIAN_POINT('Ctrl Pts',(-2.39877337851287,-1.205063204871,11.5241534457709));
#31930=CARTESIAN_POINT('Ctrl Pts',(-2.40481962522456,-1.2,11.5265855556241));
#31931=CARTESIAN_POINT('Origin',(0.,1.25,7.2));
#31932=CARTESIAN_POINT('Origin',(0.,1.2,7.2));
#31933=CARTESIAN_POINT('Origin',(0.,0.92691742076555,7.2));
#31934=CARTESIAN_POINT('Origin',(0.,0.653834841531101,7.2));
#31935=CARTESIAN_POINT('Origin',(0.,0.,7.2));
#31936=CARTESIAN_POINT('Origin',(0.,-0.653834841531101,7.2));
#31937=CARTESIAN_POINT('Origin',(0.,-0.926917420765551,7.2));
#31938=CARTESIAN_POINT('Origin',(0.,-1.2,7.2));
#31939=CARTESIAN_POINT('Origin',(0.,-1.25,7.2));
#31940=CARTESIAN_POINT('Ctrl Pts',(-2.77007461962166,-1.30000000000024,
11.4160631477717));
#31941=CARTESIAN_POINT('Ctrl Pts',(-2.73776084594322,-1.18514270861195,
11.4438270002089));
#31942=CARTESIAN_POINT('Ctrl Pts',(-2.70652295951427,-1.0684760419452,11.457162059593));
#31943=CARTESIAN_POINT('Ctrl Pts',(-2.63684270752248,-0.794772684000851,
11.4546353160166));
#31944=CARTESIAN_POINT('Ctrl Pts',(-2.59430952183081,-0.636309800095197,
11.39905100554));
#31945=CARTESIAN_POINT('Ctrl Pts',(-2.53348691516026,-0.319434907277159,
11.3566435139844));
#31946=CARTESIAN_POINT('Ctrl Pts',(-2.50702387179492,-0.158333333333332,
11.3191825394316));
#31947=CARTESIAN_POINT('Ctrl Pts',(-2.47794645705815,0.158333333333334,
11.3365725980411));
#31948=CARTESIAN_POINT('Ctrl Pts',(-2.47397094455433,0.319434907277167,
11.3921419562788));
#31949=CARTESIAN_POINT('Ctrl Pts',(-2.47833749753066,0.636309800095206,
11.4685085686389));
#31950=CARTESIAN_POINT('Ctrl Pts',(-2.48972764967703,0.79477268400084,11.5419677641134));
#31951=CARTESIAN_POINT('Ctrl Pts',(-2.52071187691362,1.0684760419458,11.5698548993163));
#31952=CARTESIAN_POINT('Ctrl Pts',(-2.53830479690509,1.18514270861313,11.5662553176453));
#31953=CARTESIAN_POINT('Ctrl Pts',(-2.56007871299605,1.300000000002,11.5469848467941));
#31954=CARTESIAN_POINT('Ctrl Pts',(-2.7696826118328,-1.30000000000024,11.4098043288393));
#31955=CARTESIAN_POINT('Ctrl Pts',(-2.73726147280167,-1.18514270861195,
11.436384457461));
#31956=CARTESIAN_POINT('Ctrl Pts',(-2.70595672829373,-1.0684760419452,11.4488497373219));
#31957=CARTESIAN_POINT('Ctrl Pts',(-2.63621560067023,-0.794772684000851,
11.4450389031677));
#31958=CARTESIAN_POINT('Ctrl Pts',(-2.59379521981159,-0.636309800095197,
11.3896433274275));
#31959=CARTESIAN_POINT('Ctrl Pts',(-2.53302516601485,-0.319434907277159,
11.3471799051539));
#31960=CARTESIAN_POINT('Ctrl Pts',(-2.50647930784202,-0.158333333333332,
11.3101501710864));
#31961=CARTESIAN_POINT('Ctrl Pts',(-2.47762464051037,0.158333333333334,
11.3274655474731));
#31962=CARTESIAN_POINT('Ctrl Pts',(-2.47402470095201,0.319434907277167,
11.382503004698));
#31963=CARTESIAN_POINT('Ctrl Pts',(-2.47864981465855,0.636309800095206,
11.4588263414016));
#31964=CARTESIAN_POINT('Ctrl Pts',(-2.49003717792243,0.79477268400084,11.5320690120471));
#31965=CARTESIAN_POINT('Ctrl Pts',(-2.52104861549134,1.0684760419458,11.5612588970434));
#31966=CARTESIAN_POINT('Ctrl Pts',(-2.53863428980996,1.18514270861313,11.5585564843371));
#31967=CARTESIAN_POINT('Ctrl Pts',(-2.56038193621059,1.300000000002,11.5405164393015));
#31968=CARTESIAN_POINT('Ctrl Pts',(-2.76915281737503,-1.30000000000057,
11.3971658160928));
#31969=CARTESIAN_POINT('Ctrl Pts',(-2.73640851043879,-1.18514270861224,
11.4214308270861));
#31970=CARTESIAN_POINT('Ctrl Pts',(-2.70487251583296,-1.06847604194547,
11.4322014493312));
#31971=CARTESIAN_POINT('Ctrl Pts',(-2.63480950274466,-0.794772684001051,
11.425909003821));
#31972=CARTESIAN_POINT('Ctrl Pts',(-2.59234201760466,-0.636309800095355,
11.3709915412348));
#31973=CARTESIAN_POINT('Ctrl Pts',(-2.53187715672899,-0.319434907277237,
11.3283362951877));
#31974=CARTESIAN_POINT('Ctrl Pts',(-2.50584772331639,-0.158333333333372,
11.2918997445371));
#31975=CARTESIAN_POINT('Ctrl Pts',(-2.4775646853384,0.158333333333373,11.309017362706));
#31976=CARTESIAN_POINT('Ctrl Pts',(-2.47426262756895,0.319434907277246,
11.3631728921772));
#31977=CARTESIAN_POINT('Ctrl Pts',(-2.47925260021527,0.636309800095363,
11.439470565577));
#31978=CARTESIAN_POINT('Ctrl Pts',(-2.49074116951473,0.794772684001036,
11.5122361618323));
#31979=CARTESIAN_POINT('Ctrl Pts',(-2.52180172561918,1.06847604194606,11.5440328862475));
#31980=CARTESIAN_POINT('Ctrl Pts',(-2.53936376159819,1.18514270861343,11.5431282164631));
#31981=CARTESIAN_POINT('Ctrl Pts',(-2.56104286972559,1.30000000000233,11.5275552530796));
#31982=CARTESIAN_POINT('Ctrl Pts',(-2.76670318044365,-1.30000000000057,
11.3725613695234));
#31983=CARTESIAN_POINT('Ctrl Pts',(-2.73495204203674,-1.18514270861225,
11.3914589550316));
#31984=CARTESIAN_POINT('Ctrl Pts',(-2.70398432429643,-1.06847604194547,
11.3983717895585));
#31985=CARTESIAN_POINT('Ctrl Pts',(-2.63425255970823,-0.794772684001053,
11.3866546479154));
#31986=CARTESIAN_POINT('Ctrl Pts',(-2.59026178357869,-0.636309800095359,
11.3333141793376));
#31987=CARTESIAN_POINT('Ctrl Pts',(-2.52922897848775,-0.319434907277241,
11.2907460649789));
#31988=CARTESIAN_POINT('Ctrl Pts',(-2.50314228401203,-0.158333333333373,
11.2559401072439));
#31989=CARTESIAN_POINT('Ctrl Pts',(-2.47526690486424,0.158333333333374,
11.2729219488189));
#31990=CARTESIAN_POINT('Ctrl Pts',(-2.4725788014573,0.319434907277247,11.3252350049386));
#31991=CARTESIAN_POINT('Ctrl Pts',(-2.47866351752077,0.636309800095367,
11.4013239975511));
#31992=CARTESIAN_POINT('Ctrl Pts',(-2.49147185773774,0.794772684001045,
11.4727412600865));
#31993=CARTESIAN_POINT('Ctrl Pts',(-2.52265808377612,1.06847604194607,11.5097741407791));
#31994=CARTESIAN_POINT('Ctrl Pts',(-2.53993770890259,1.18514270861343,11.5125717343214));
#31995=CARTESIAN_POINT('Ctrl Pts',(-2.56099759746704,1.30000000000233,11.5021367595577));
#31996=CARTESIAN_POINT('Ctrl Pts',(-2.76535570772393,-1.30000000000129,
11.3536900155371));
#31997=CARTESIAN_POINT('Ctrl Pts',(-2.73242312356743,-1.1851427086129,11.3693724675759));
#31998=CARTESIAN_POINT('Ctrl Pts',(-2.70073315536695,-1.06847604194605,
11.373876973312));
#31999=CARTESIAN_POINT('Ctrl Pts',(-2.63039368071025,-0.794772684001488,
11.3584599905864));
#32000=CARTESIAN_POINT('Ctrl Pts',(-2.58777591208119,-0.636309800095707,
11.30525700494));
#32001=CARTESIAN_POINT('Ctrl Pts',(-2.52733729460958,-0.319434907277415,
11.2623369202654));
#32002=CARTESIAN_POINT('Ctrl Pts',(-2.50115862889893,-0.158333333333459,
11.228775100159));
#32003=CARTESIAN_POINT('Ctrl Pts',(-2.47384647649032,0.158333333333461,
11.2455582419395));
#32004=CARTESIAN_POINT('Ctrl Pts',(-2.47162318313642,0.319434907277424,
11.2964996838724));
#32005=CARTESIAN_POINT('Ctrl Pts',(-2.47864877038137,0.636309800095716,
11.3723908330216));
#32006=CARTESIAN_POINT('Ctrl Pts',(-2.49251384879947,0.794772684001477,
11.4427560053326));
#32007=CARTESIAN_POINT('Ctrl Pts',(-2.523862159101,1.06847604194665,11.4837092803596));
#32008=CARTESIAN_POINT('Ctrl Pts',(-2.54094944198943,1.18514270861408,11.489291196615));
#32009=CARTESIAN_POINT('Ctrl Pts',(-2.56155448580606,1.30000000000305,11.482727873835));
#32010=CARTESIAN_POINT('Ctrl Pts',(-2.76425102958308,-1.30000000000134,
11.3410995400671));
#32011=CARTESIAN_POINT('Ctrl Pts',(-2.7315536663465,-1.18514270861294,11.354163665401));
#32012=CARTESIAN_POINT('Ctrl Pts',(-2.69997469370202,-1.0684760419461,11.3567798466479));
#32013=CARTESIAN_POINT('Ctrl Pts',(-2.62960465554241,-0.794772684001521,
11.3386869077486));
#32014=CARTESIAN_POINT('Ctrl Pts',(-2.58647592708129,-0.636309800095733,
11.2861786420534));
#32015=CARTESIAN_POINT('Ctrl Pts',(-2.52571622593059,-0.319434907277429,
11.2433163704505));
#32016=CARTESIAN_POINT('Ctrl Pts',(-2.4992559721307,-0.158333333333466,
11.2106859315712));
#32017=CARTESIAN_POINT('Ctrl Pts',(-2.47225107092196,0.158333333333468,
11.2273600175278));
#32018=CARTESIAN_POINT('Ctrl Pts',(-2.47085041360708,0.319434907277437,
11.277165815717));
#32019=CARTESIAN_POINT('Ctrl Pts',(-2.47834670595677,0.636309800095743,
11.3529709421115));
#32020=CARTESIAN_POINT('Ctrl Pts',(-2.49207122318901,0.794772684001511,
11.422936527734));
#32021=CARTESIAN_POINT('Ctrl Pts',(-2.52353774137249,1.0684760419467,11.4665362245579));
#32022=CARTESIAN_POINT('Ctrl Pts',(-2.54068299263077,1.18514270861413,11.473932655612));
#32023=CARTESIAN_POINT('Ctrl Pts',(-2.56135280537506,1.3000000000031,11.469852824493));
#32024=CARTESIAN_POINT('Ctrl Pts',(-2.7642249389054,-1.30000000000134,11.3408092309998));
#32025=CARTESIAN_POINT('Ctrl Pts',(-2.73153255481153,-1.18514270861294,
11.3538131019925));
#32026=CARTESIAN_POINT('Ctrl Pts',(-2.69995590010922,-1.0684760419461,11.356385794704));
#32027=CARTESIAN_POINT('Ctrl Pts',(-2.62958506895419,-0.794772684001521,
11.3382311209536));
#32028=CARTESIAN_POINT('Ctrl Pts',(-2.5864454753899,-0.636309800095733,
11.2857385089783));
#32029=CARTESIAN_POINT('Ctrl Pts',(-2.5256784289746,-0.319434907277429,
11.2428775413335));
#32030=CARTESIAN_POINT('Ctrl Pts',(-2.49921092572217,-0.158333333333466,
11.2102689026167));
#32031=CARTESIAN_POINT('Ctrl Pts',(-2.47221323526919,0.158333333333468,
11.2269404266026));
#32032=CARTESIAN_POINT('Ctrl Pts',(-2.47083231477348,0.319434907277437,
11.2767197171004));
#32033=CARTESIAN_POINT('Ctrl Pts',(-2.47833989210166,0.636309800095743,
11.3525226913348));
#32034=CARTESIAN_POINT('Ctrl Pts',(-2.49206109302992,0.794772684001511,
11.4224790800824));
#32035=CARTESIAN_POINT('Ctrl Pts',(-2.52353047072471,1.0684760419467,11.4661398071924));
#32036=CARTESIAN_POINT('Ctrl Pts',(-2.54067711801391,1.18514270861413,11.4735780966765));
#32037=CARTESIAN_POINT('Ctrl Pts',(-2.56134848504356,1.3000000000031,11.4695555646682));
#32038=CARTESIAN_POINT('Ctrl Pts',(-2.76419881448468,-1.30000000000134,
11.3405189439279));
#32039=CARTESIAN_POINT('Ctrl Pts',(-2.73151148373164,-1.18514270861294,
11.3534625344107));
#32040=CARTESIAN_POINT('Ctrl Pts',(-2.69993718519305,-1.0684760419461,11.3559917257283));
#32041=CARTESIAN_POINT('Ctrl Pts',(-2.62956556622883,-0.794772684001521,
11.3377753181702));
#32042=CARTESIAN_POINT('Ctrl Pts',(-2.58641489207281,-0.636309800095733,
11.2852984453538));
#32043=CARTESIAN_POINT('Ctrl Pts',(-2.52564057129996,-0.319434907277429,
11.2424387508086));
#32044=CARTESIAN_POINT('Ctrl Pts',(-2.49916618353628,-0.158333333333466,
11.209851762818));
#32045=CARTESIAN_POINT('Ctrl Pts',(-2.47217564283986,0.158333333333468,
11.2265207446432));
#32046=CARTESIAN_POINT('Ctrl Pts',(-2.47081397410684,0.319434907277437,
11.2762737167092));
#32047=CARTESIAN_POINT('Ctrl Pts',(-2.47833276167054,0.636309800095743,
11.3520745692275));
#32048=CARTESIAN_POINT('Ctrl Pts',(-2.49205103357898,0.794772684001511,
11.4220216158322));
#32049=CARTESIAN_POINT('Ctrl Pts',(-2.52352329202462,1.0684760419467,11.465743363105));
#32050=CARTESIAN_POINT('Ctrl Pts',(-2.54067128140231,1.18514270861413,11.4732235296063));
#32051=CARTESIAN_POINT('Ctrl Pts',(-2.56134408563865,1.3000000000031,11.4692583382648));
#32052=CARTESIAN_POINT('Ctrl Pts',(-2.7641459971008,-1.30000000000134,11.3399386075426));
#32053=CARTESIAN_POINT('Ctrl Pts',(-2.73146844378851,-1.18514270861294,
11.3527617637104));
#32054=CARTESIAN_POINT('Ctrl Pts',(-2.69989867568352,-1.0684760419461,11.3552040201509));
#32055=CARTESIAN_POINT('Ctrl Pts',(-2.62952540129104,-0.794772684001521,
11.3368641660385));
#32056=CARTESIAN_POINT('Ctrl Pts',(-2.58635315650737,-0.636309800095733,
11.2844185273025));
#32057=CARTESIAN_POINT('Ctrl Pts',(-2.5255644397242,-0.319434907277429,
11.2415613108777));
#32058=CARTESIAN_POINT('Ctrl Pts',(-2.49907605021946,-0.158333333333466,
11.2090177185494));
#32059=CARTESIAN_POINT('Ctrl Pts',(-2.47209984924853,0.158333333333468,
11.2256815971009));
#32060=CARTESIAN_POINT('Ctrl Pts',(-2.47077678021634,0.319434907277437,
11.2753818890525));
#32061=CARTESIAN_POINT('Ctrl Pts',(-2.47831827749408,0.636309800095743,
11.3511783852092));
#32062=CARTESIAN_POINT('Ctrl Pts',(-2.49203108365346,0.794772684001511,
11.4211065984287));
#32063=CARTESIAN_POINT('Ctrl Pts',(-2.52350924912019,1.0684760419467,11.4649503359398));
#32064=CARTESIAN_POINT('Ctrl Pts',(-2.5406599129494,1.18514270861413,11.4725142638776));
#32065=CARTESIAN_POINT('Ctrl Pts',(-2.5613355091582,1.3000000000031,11.4686637903551));
#32066=CARTESIAN_POINT('Ctrl Pts',(-2.76402931431754,-1.30000000000134,
11.338682172166));
#32067=CARTESIAN_POINT('Ctrl Pts',(-2.73137172231167,-1.18514270861294,
11.3512448816346));
#32068=CARTESIAN_POINT('Ctrl Pts',(-2.69981107687792,-1.0684760419461,11.3534990541753));
#32069=CARTESIAN_POINT('Ctrl Pts',(-2.62943383826546,-0.794772684001521,
11.3348918611708));
#32070=CARTESIAN_POINT('Ctrl Pts',(-2.58621659385465,-0.636309800095733,
11.2825131577169));
#32071=CARTESIAN_POINT('Ctrl Pts',(-2.52539779351564,-0.319434907277428,
11.2396608293271));
#32072=CARTESIAN_POINT('Ctrl Pts',(-2.49887984433881,-0.158333333333466,
11.2072109433244));
#32073=CARTESIAN_POINT('Ctrl Pts',(-2.47193459901702,0.158333333333468,
11.2238637817233));
#32074=CARTESIAN_POINT('Ctrl Pts',(-2.47069320506725,0.319434907277437,
11.2734506758837));
#32075=CARTESIAN_POINT('Ctrl Pts',(-2.47828473941927,0.636309800095743,
11.3492374181108));
#32076=CARTESIAN_POINT('Ctrl Pts',(-2.49198924223239,0.794772684001511,
11.4191234920776));
#32077=CARTESIAN_POINT('Ctrl Pts',(-2.52348083005594,1.0684760419467,11.4632313171438));
#32078=CARTESIAN_POINT('Ctrl Pts',(-2.5406369264164,1.18514270861413,11.4709768715931));
#32079=CARTESIAN_POINT('Ctrl Pts',(-2.5613175776468,1.3000000000031,11.4673753373765));
#32080=CARTESIAN_POINT('Ctrl Pts',(-2.76384106606497,-1.30000000000133,
11.3367528528731));
#32081=CARTESIAN_POINT('Ctrl Pts',(-2.73120756008998,-1.18514270861294,
11.3489175947374));
#32082=CARTESIAN_POINT('Ctrl Pts',(-2.69965713366755,-1.0684760419461,11.3508839572717));
#32083=CARTESIAN_POINT('Ctrl Pts',(-2.62927146742631,-0.794772684001519,
11.3318663516645));
#32084=CARTESIAN_POINT('Ctrl Pts',(-2.58599385923292,-0.636309800095732,
11.2795868603255));
#32085=CARTESIAN_POINT('Ctrl Pts',(-2.52513457515162,-0.319434907277428,
11.2367395707489));
#32086=CARTESIAN_POINT('Ctrl Pts',(-2.49857540848214,-0.158333333333466,
11.2044321215613));
#32087=CARTESIAN_POINT('Ctrl Pts',(-2.47167760241594,0.158333333333468,
11.2210679345774));
#32088=CARTESIAN_POINT('Ctrl Pts',(-2.47055269207584,0.319434907277436,
11.2704838638599));
#32089=CARTESIAN_POINT('Ctrl Pts',(-2.47822465920485,0.636309800095742,
11.3462543179259));
#32090=CARTESIAN_POINT('Ctrl Pts',(-2.49193191562207,0.79477268400151,11.416069748549));
#32091=CARTESIAN_POINT('Ctrl Pts',(-2.52344696005734,1.0684760419467,11.4605828404811));
#32092=CARTESIAN_POINT('Ctrl Pts',(-2.54060989083201,1.18514270861413,11.4686084087007));
#32093=CARTESIAN_POINT('Ctrl Pts',(-2.56129405739276,1.3000000000031,11.465391477015));
#32094=CARTESIAN_POINT('Ctrl Pts',(-2.76360061952686,-1.30000000000133,
11.3344435152267));
#32095=CARTESIAN_POINT('Ctrl Pts',(-2.73097799067002,-1.18514270861294,
11.3461382704645));
#32096=CARTESIAN_POINT('Ctrl Pts',(-2.69942932223466,-1.06847604194609,
11.3477636570441));
#32097=CARTESIAN_POINT('Ctrl Pts',(-2.62902665027813,-0.794772684001518,
11.32825636923));
#32098=CARTESIAN_POINT('Ctrl Pts',(-2.58569889268955,-0.636309800095731,
11.2760863776604));
#32099=CARTESIAN_POINT('Ctrl Pts',(-2.5248079778311,-0.319434907277428,
11.2332380172859));
#32100=CARTESIAN_POINT('Ctrl Pts',(-2.49821542392339,-0.158333333333465,
11.2010950925747));
#32101=CARTESIAN_POINT('Ctrl Pts',(-2.47137359693892,0.158333333333467,
11.2177106241918));
#32102=CARTESIAN_POINT('Ctrl Pts',(-2.47035915085401,0.319434907277435,
11.2669326531755));
#32103=CARTESIAN_POINT('Ctrl Pts',(-2.47813379914407,0.636309800095741,
11.3426813909753));
#32104=CARTESIAN_POINT('Ctrl Pts',(-2.49188611954923,0.794772684001508,
11.4123964622437));
#32105=CARTESIAN_POINT('Ctrl Pts',(-2.52343468975773,1.06847604194669,11.4573939376935));
#32106=CARTESIAN_POINT('Ctrl Pts',(-2.54060061621157,1.18514270861413,11.4657574988284));
#32107=CARTESIAN_POINT('Ctrl Pts',(-2.56127626206568,1.30000000000309,11.4630068812969));
#32108=CARTESIAN_POINT('Ctrl Pts',(-2.76309350386812,-1.30000000000133,
11.3298351473961));
#32109=CARTESIAN_POINT('Ctrl Pts',(-2.73045517154361,-1.18514270861294,
11.3406057267502));
#32110=CARTESIAN_POINT('Ctrl Pts',(-2.69888781493744,-1.06847604194609,
11.3415585026455));
#32111=CARTESIAN_POINT('Ctrl Pts',(-2.62843507430646,-0.794772684001515,
11.3210785155308));
#32112=CARTESIAN_POINT('Ctrl Pts',(-2.58504928387606,-0.636309800095729,
11.2691093968105));
#32113=CARTESIAN_POINT('Ctrl Pts',(-2.52413061301386,-0.319434907277426,
11.2262440409975));
#32114=CARTESIAN_POINT('Ctrl Pts',(-2.49750907749174,-0.158333333333465,
11.1944150527455));
#32115=CARTESIAN_POINT('Ctrl Pts',(-2.47077890822903,0.158333333333467,
11.2109896331354));
#32116=CARTESIAN_POINT('Ctrl Pts',(-2.46992453282581,0.319434907277434,
11.2598472153409));
#32117=CARTESIAN_POINT('Ctrl Pts',(-2.47791479560751,0.636309800095739,
11.3355490050596));
#32118=CARTESIAN_POINT('Ctrl Pts',(-2.49183703931886,0.794772684001506,
11.4050337736974));
#32119=CARTESIAN_POINT('Ctrl Pts',(-2.52346511529109,1.06847604194669,11.4509954167954));
#32120=CARTESIAN_POINT('Ctrl Pts',(-2.5406286591004,1.18514270861412,11.4600380519337));
#32121=CARTESIAN_POINT('Ctrl Pts',(-2.56126512456632,1.30000000000309,11.4582282299596));
#32122=CARTESIAN_POINT('Ctrl Pts',(-2.76222770959521,-1.30000000000129,
11.3229634616086));
#32123=CARTESIAN_POINT('Ctrl Pts',(-2.7293887323951,-1.1851427086129,11.3324232623684));
#32124=CARTESIAN_POINT('Ctrl Pts',(-2.69768919111629,-1.06847604194606,
11.332411528792));
#32125=CARTESIAN_POINT('Ctrl Pts',(-2.62708923421229,-0.794772684001494,
11.3105032827926));
#32126=CARTESIAN_POINT('Ctrl Pts',(-2.58382313700693,-0.636309800095712,
11.2587466220022));
#32127=CARTESIAN_POINT('Ctrl Pts',(-2.52303388877888,-0.319434907277418,
11.2157845139037));
#32128=CARTESIAN_POINT('Ctrl Pts',(-2.49654983034628,-0.158333333333461,
11.1843543637192));
#32129=CARTESIAN_POINT('Ctrl Pts',(-2.46997662326551,0.158333333333463,
11.2008695548721));
#32130=CARTESIAN_POINT('Ctrl Pts',(-2.46905368135563,0.319434907277427,
11.2492992472544));
#32131=CARTESIAN_POINT('Ctrl Pts',(-2.47741359693355,0.636309800095722,
11.324915022394));
#32132=CARTESIAN_POINT('Ctrl Pts',(-2.49199886919655,0.794772684001485,
11.39390247055));
#32133=CARTESIAN_POINT('Ctrl Pts',(-2.52379078168629,1.06847604194666,11.4412940015727));
#32134=CARTESIAN_POINT('Ctrl Pts',(-2.5408960429585,1.18514270861409,11.4513755911155));
#32135=CARTESIAN_POINT('Ctrl Pts',(-2.56134502459252,1.30000000000306,11.4510247324508));
#32136=CARTESIAN_POINT('Ctrl Pts',(-2.76108397909559,-1.30000000000128,
11.3137922130238));
#32137=CARTESIAN_POINT('Ctrl Pts',(-2.72796787036885,-1.1851427086129,11.3215064835911));
#32138=CARTESIAN_POINT('Ctrl Pts',(-2.696073175759,-1.06847604194605,11.3202154940208));
#32139=CARTESIAN_POINT('Ctrl Pts',(-2.62521176165157,-0.794772684001488,
11.2964290974375));
#32140=CARTESIAN_POINT('Ctrl Pts',(-2.58200923659833,-0.636309800095708,
11.2449978338617));
#32141=CARTESIAN_POINT('Ctrl Pts',(-2.52134186084768,-0.319434907277416,
11.2019287017981));
#32142=CARTESIAN_POINT('Ctrl Pts',(-2.4950486259072,-0.15833333333346,11.1710284212635));
#32143=CARTESIAN_POINT('Ctrl Pts',(-2.46872146847482,0.158333333333462,
11.1874470610037));
#32144=CARTESIAN_POINT('Ctrl Pts',(-2.46780018656564,0.319434907277424,
11.2352637031698));
#32145=CARTESIAN_POINT('Ctrl Pts',(-2.47664852548579,0.636309800095717,
11.3107625985471));
#32146=CARTESIAN_POINT('Ctrl Pts',(-2.49195811589145,0.79477268400148,11.3791486794266));
#32147=CARTESIAN_POINT('Ctrl Pts',(-2.52402251623276,1.06847604194666,11.4284269609544));
#32148=CARTESIAN_POINT('Ctrl Pts',(-2.54111681522227,1.18514270861408,11.4398691438539));
#32149=CARTESIAN_POINT('Ctrl Pts',(-2.56142592239663,1.30000000000305,11.4414227675198));
#32150=CARTESIAN_POINT('Ctrl Pts',(-2.75980118259079,-1.30000000000125,
11.3014623485093));
#32151=CARTESIAN_POINT('Ctrl Pts',(-2.72668885406917,-1.18514270861286,
11.3066879411516));
#32152=CARTESIAN_POINT('Ctrl Pts',(-2.69474188830154,-1.06847604194603,
11.3036011429695));
#32153=CARTESIAN_POINT('Ctrl Pts',(-2.62363022750143,-0.794772684001467,
11.2772667359641));
#32154=CARTESIAN_POINT('Ctrl Pts',(-2.58003207349033,-0.63630980009569,
11.2264773244685));
#32155=CARTESIAN_POINT('Ctrl Pts',(-2.51901724331341,-0.319434907277407,
11.1834792920214));
#32156=CARTESIAN_POINT('Ctrl Pts',(-2.49240144992841,-0.158333333333455,
11.1535220447443));
#32157=CARTESIAN_POINT('Ctrl Pts',(-2.46637898161969,0.158333333333457,
11.1698229438921));
#32158=CARTESIAN_POINT('Ctrl Pts',(-2.46624982092312,0.319434907277415,
11.2165057451712));
#32159=CARTESIAN_POINT('Ctrl Pts',(-2.47573040833367,0.6363098000957,11.2918425441167));
#32160=CARTESIAN_POINT('Ctrl Pts',(-2.49117635189392,0.794772684001457,
11.3597287085015));
#32161=CARTESIAN_POINT('Ctrl Pts',(-2.52352169135959,1.06847604194663,11.4115569527867));
#32162=CARTESIAN_POINT('Ctrl Pts',(-2.54071050140298,1.18514270861405,11.4247776534393));
#32163=CARTESIAN_POINT('Ctrl Pts',(-2.56108702254797,1.30000000000301,11.4287845282192));
#32164=CARTESIAN_POINT('Ctrl Pts',(-2.75825795813088,-1.30000000000116,
11.2860117341614));
#32165=CARTESIAN_POINT('Ctrl Pts',(-2.72513502484691,-1.18514270861278,
11.2881298178769));
#32166=CARTESIAN_POINT('Ctrl Pts',(-2.69312058453786,-1.06847604194595,
11.2827970892231));
#32167=CARTESIAN_POINT('Ctrl Pts',(-2.62172166348246,-0.794772684001413,
11.2532645521214));
#32168=CARTESIAN_POINT('Ctrl Pts',(-2.57769388327834,-0.636309800095648,
11.2032509010327));
#32169=CARTESIAN_POINT('Ctrl Pts',(-2.51630763113037,-0.319434907277386,
11.1603190736043));
#32170=CARTESIAN_POINT('Ctrl Pts',(-2.48938193806615,-0.158333333333445,
11.1315094292022));
#32171=CARTESIAN_POINT('Ctrl Pts',(-2.46364866959619,0.158333333333447,
11.1477013127868));
#32172=CARTESIAN_POINT('Ctrl Pts',(-2.46417035515022,0.319434907277394,
11.1930962285957));
#32173=CARTESIAN_POINT('Ctrl Pts',(-2.47450603941183,0.636309800095658,
11.268208454363));
#32174=CARTESIAN_POINT('Ctrl Pts',(-2.49057818975681,0.794772684001404,
11.3353018937305));
#32175=CARTESIAN_POINT('Ctrl Pts',(-2.52343815187733,1.06847604194656,11.3902517119039));
#32176=CARTESIAN_POINT('Ctrl Pts',(-2.54075694726679,1.18514270861397,11.4056872918243));
#32177=CARTESIAN_POINT('Ctrl Pts',(-2.5611706780253,1.30000000000293,11.412772711469));
#32178=CARTESIAN_POINT('Ctrl Pts',(-2.75493542354467,-1.30000000000102,
11.2616597751113));
#32179=CARTESIAN_POINT('Ctrl Pts',(-2.72115084070019,-1.18514270861265,
11.2590784416815));
#32180=CARTESIAN_POINT('Ctrl Pts',(-2.68860134985113,-1.06847604194584,
11.2503326796887));
#32181=CARTESIAN_POINT('Ctrl Pts',(-2.61625882407524,-0.794772684001327,
11.2158871567315));
#32182=CARTESIAN_POINT('Ctrl Pts',(-2.57180751599066,-0.636309800095576,
11.1670064104961));
#32183=CARTESIAN_POINT('Ctrl Pts',(-2.5104314595887,-0.319434907277349,
11.1239157330979));
#32184=CARTESIAN_POINT('Ctrl Pts',(-2.48391525623262,-0.158333333333427,
11.0965453605644));
#32185=CARTESIAN_POINT('Ctrl Pts',(-2.45918556724436,0.158333333333429,
11.1123214520548));
#32186=CARTESIAN_POINT('Ctrl Pts',(-2.46083663420726,0.319434907277358,
11.1556249158299));
#32187=CARTESIAN_POINT('Ctrl Pts',(-2.47211599134814,0.636309800095586,
11.2305305584888));
#32188=CARTESIAN_POINT('Ctrl Pts',(-2.48811501046006,0.794772684001314,
11.2967506895527));
#32189=CARTESIAN_POINT('Ctrl Pts',(-2.52146216625009,1.06847604194643,11.356844218504));
#32190=CARTESIAN_POINT('Ctrl Pts',(-2.53902007409783,1.18514270861384,11.3758292365511));
#32191=CARTESIAN_POINT('Ctrl Pts',(-2.55970114168565,1.30000000000278,11.3877870106468));
#32192=CARTESIAN_POINT('Ctrl Pts',(-2.7518637748275,-1.30000000000087,11.2371614514306));
#32193=CARTESIAN_POINT('Ctrl Pts',(-2.71741456579904,-1.18514270861252,
11.2298815778422));
#32194=CARTESIAN_POINT('Ctrl Pts',(-2.6843818772594,-1.06847604194571,11.2176986913577));
#32195=CARTESIAN_POINT('Ctrl Pts',(-2.6113422042693,-0.794772684001233,
11.1782268457664));
#32196=CARTESIAN_POINT('Ctrl Pts',(-2.56707069312648,-0.636309800095504,
11.1302032988742));
#32197=CARTESIAN_POINT('Ctrl Pts',(-2.50562348786956,-0.319434907277313,
11.0869902458595));
#32198=CARTESIAN_POINT('Ctrl Pts',(-2.47909119587275,-0.158333333333409,
11.0612684020365));
#32199=CARTESIAN_POINT('Ctrl Pts',(-2.45452022313769,0.15833333333341,11.0769832866117));
#32200=CARTESIAN_POINT('Ctrl Pts',(-2.45612570166382,0.31943490727732,11.1186569966856));
#32201=CARTESIAN_POINT('Ctrl Pts',(-2.46824842658526,0.636309800095512,
11.1933974234602));
#32202=CARTESIAN_POINT('Ctrl Pts',(-2.48526252158171,0.794772684001224,
11.2583122288779));
#32203=CARTESIAN_POINT('Ctrl Pts',(-2.51983978146043,1.06847604194631,11.3232510423267));
#32204=CARTESIAN_POINT('Ctrl Pts',(-2.53792061586775,1.1851427086137,11.3456703913735));
#32205=CARTESIAN_POINT('Ctrl Pts',(-2.55911507009457,1.30000000000263,11.3623994833453));
#32206=CARTESIAN_POINT('Ctrl Pts',(-2.74834939782952,-1.30000000000082,
11.2128663351783));
#32207=CARTESIAN_POINT('Ctrl Pts',(-2.71340728818996,-1.18514270861247,
11.2007884395455));
#32208=CARTESIAN_POINT('Ctrl Pts',(-2.67981955403308,-1.06847604194567,
11.185186462444));
#32209=CARTESIAN_POINT('Ctrl Pts',(-2.60535404723434,-0.794772684001202,
11.1410014409916));
#32210=CARTESIAN_POINT('Ctrl Pts',(-2.55935977635548,-0.636309800095478,
11.0947175057529));
#32211=CARTESIAN_POINT('Ctrl Pts',(-2.49749108140857,-0.3194349072773,11.0515352465719));
#32212=CARTESIAN_POINT('Ctrl Pts',(-2.47195891583274,-0.158333333333402,
11.0269832733524));
#32213=CARTESIAN_POINT('Ctrl Pts',(-2.44847039799177,0.158333333333404,
11.0422134181132));
#32214=CARTESIAN_POINT('Ctrl Pts',(-2.45064429522044,0.319434907277308,
11.0819845588382));
#32215=CARTESIAN_POINT('Ctrl Pts',(-2.46440326171409,0.636309800095487,
11.1562118861686));
#32216=CARTESIAN_POINT('Ctrl Pts',(-2.48309797691221,0.794772684001192,
11.219540481514));
#32217=CARTESIAN_POINT('Ctrl Pts',(-2.51859141008612,1.06847604194627,11.2894664432714));
#32218=CARTESIAN_POINT('Ctrl Pts',(-2.53678252725346,1.18514270861366,11.3155017071016));
#32219=CARTESIAN_POINT('Ctrl Pts',(-2.55780096952842,1.30000000000258,11.3373038769293));
#32220=CARTESIAN_POINT('Ctrl Pts',(-2.74573850760591,-1.30000000000075,
11.194591028711));
#32221=CARTESIAN_POINT('Ctrl Pts',(-2.70959292316076,-1.18514270861241,
11.1793106824202));
#32222=CARTESIAN_POINT('Ctrl Pts',(-2.67524735232435,-1.06847604194562,
11.1613097598791));
#32223=CARTESIAN_POINT('Ctrl Pts',(-2.60006060441201,-0.794772684001161,
11.1134389523493));
#32224=CARTESIAN_POINT('Ctrl Pts',(-2.5555787040635,-0.636309800095446,
11.0671560420463));
#32225=CARTESIAN_POINT('Ctrl Pts',(-2.49364032028975,-0.319434907277284,
11.0238878071138));
#32226=CARTESIAN_POINT('Ctrl Pts',(-2.46702495262325,-0.158333333333394,
11.0010760834182));
#32227=CARTESIAN_POINT('Ctrl Pts',(-2.44338172711316,0.158333333333396,
11.0163803880387));
#32228=CARTESIAN_POINT('Ctrl Pts',(-2.44615547867357,0.319434907277292,
11.0546354570378));
#32229=CARTESIAN_POINT('Ctrl Pts',(-2.46033842181148,0.636309800095455,
11.1287942426758));
#32230=CARTESIAN_POINT('Ctrl Pts',(-2.47871468054937,0.794772684001151,
11.1915537053767));
#32231=CARTESIAN_POINT('Ctrl Pts',(-2.51532939498739,1.06847604194622,11.2650365289296));
#32232=CARTESIAN_POINT('Ctrl Pts',(-2.53427276633016,1.1851427086136,11.2935121246627));
#32233=CARTESIAN_POINT('Ctrl Pts',(-2.55631035584431,1.30000000000251,11.3186553246197));
#32234=CARTESIAN_POINT('Ctrl Pts',(-2.74194313468282,-1.30000000000071,
11.1769309522021));
#32235=CARTESIAN_POINT('Ctrl Pts',(-2.70552266600435,-1.18514270861237,
11.1579854994345));
#32236=CARTESIAN_POINT('Ctrl Pts',(-2.67079715330622,-1.06847604194558,
11.1373887609292));
#32237=CARTESIAN_POINT('Ctrl Pts',(-2.59448995954793,-0.794772684001138,
11.0859913742256));
#32238=CARTESIAN_POINT('Ctrl Pts',(-2.54840340341899,-0.636309800095426,
11.0411814441527));
#32239=CARTESIAN_POINT('Ctrl Pts',(-2.48605786049262,-0.319434907277274,
10.9979792561164));
#32240=CARTESIAN_POINT('Ctrl Pts',(-2.46005105058619,-0.15833333333339,
10.9761034409434));
#32241=CARTESIAN_POINT('Ctrl Pts',(-2.43778685380937,0.158333333333391,
10.9907711091253));
#32242=CARTESIAN_POINT('Ctrl Pts',(-2.44206476862543,0.319434907277283,
11.0270908601629));
#32243=CARTESIAN_POINT('Ctrl Pts',(-2.45796937480046,0.636309800095436,
11.1006257587997));
#32244=CARTESIAN_POINT('Ctrl Pts',(-2.47728146775959,0.794772684001127,
11.1623393375586));
#32245=CARTESIAN_POINT('Ctrl Pts',(-2.51438276944182,1.06847604194618,11.2396575410887));
#32246=CARTESIAN_POINT('Ctrl Pts',(-2.53329203241781,1.18514270861356,11.2709028445636));
#32247=CARTESIAN_POINT('Ctrl Pts',(-2.55505077961023,1.30000000000247,11.2999252661269));
#32248=CARTESIAN_POINT('Ctrl Pts',(-2.73966116432271,-1.30000000000066,
11.158478942661));
#32249=CARTESIAN_POINT('Ctrl Pts',(-2.70242984548913,-1.18514270861233,
11.1361367519602));
#32250=CARTESIAN_POINT('Ctrl Pts',(-2.66706342795359,-1.06847604194554,
11.1130797469362));
#32251=CARTESIAN_POINT('Ctrl Pts',(-2.58966822348966,-0.794772684001105,
11.058162088708));
#32252=CARTESIAN_POINT('Ctrl Pts',(-2.54340702433661,-0.636309800095402,
11.0141542266524));
#32253=CARTESIAN_POINT('Ctrl Pts',(-2.48069951827734,-0.319434907277262,
10.9710064276511));
#32254=CARTESIAN_POINT('Ctrl Pts',(-2.45480737171722,-0.158333333333383,
10.9503166592489));
#32255=CARTESIAN_POINT('Ctrl Pts',(-2.43239017645839,0.158333333333385,
10.9650437434));
#32256=CARTESIAN_POINT('Ctrl Pts',(-2.43611575138395,0.319434907277269,
11.0003481142894));
#32257=CARTESIAN_POINT('Ctrl Pts',(-2.45265054251548,0.63630980009541,11.0737230403714));
#32258=CARTESIAN_POINT('Ctrl Pts',(-2.47305803943563,0.794772684001096,
11.1342548378043));
#32259=CARTESIAN_POINT('Ctrl Pts',(-2.51172448148075,1.06847604194614,11.2149405437268));
#32260=CARTESIAN_POINT('Ctrl Pts',(-2.53138096354022,1.18514270861351,11.2486305072769));
#32261=CARTESIAN_POINT('Ctrl Pts',(-2.55395665763067,1.30000000000242,11.2810845819833));
#32262=CARTESIAN_POINT('Ctrl Pts',(-2.73574909450234,-1.30000000000064,
11.144116794413));
#32263=CARTESIAN_POINT('Ctrl Pts',(-2.69776719162632,-1.18514270861231,
11.1189659997614));
#32264=CARTESIAN_POINT('Ctrl Pts',(-2.66186056462313,-1.06847604194552,
11.0938501329944));
#32265=CARTESIAN_POINT('Ctrl Pts',(-2.58370337557335,-0.79477268400109,
11.0359081467518));
#32266=CARTESIAN_POINT('Ctrl Pts',(-2.53770217468129,-0.63630980009539,
10.9923659965246));
#32267=CARTESIAN_POINT('Ctrl Pts',(-2.47491433420959,-0.319434907277257,
10.9491493418208));
#32268=CARTESIAN_POINT('Ctrl Pts',(-2.44882343493709,-0.158333333333381,
10.9295894777583));
#32269=CARTESIAN_POINT('Ctrl Pts',(-2.42681406751302,0.158333333333383,
10.9441153090178));
#32270=CARTESIAN_POINT('Ctrl Pts',(-2.43113598017231,0.319434907277265,
10.9780824257723));
#32271=CARTESIAN_POINT('Ctrl Pts',(-2.44860268552448,0.6363098000954,11.0511286888608));
#32272=CARTESIAN_POINT('Ctrl Pts',(-2.46954364071995,0.794772684001082,
11.1108472790484));
#32273=CARTESIAN_POINT('Ctrl Pts',(-2.50916003180598,1.06847604194612,11.1944910794941));
#32274=CARTESIAN_POINT('Ctrl Pts',(-2.52924123422387,1.18514270861349,11.2303034178588));
#32275=CARTESIAN_POINT('Ctrl Pts',(-2.55225517129041,1.3000000000024,11.2657217926835));
#32276=CARTESIAN_POINT('Ctrl Pts',(-2.73421733091288,-1.30000000000063,
11.1318054961784));
#32277=CARTESIAN_POINT('Ctrl Pts',(-2.69568219536503,-1.1851427086123,11.1043904407161));
#32278=CARTESIAN_POINT('Ctrl Pts',(-2.65928523630985,-1.06847604194552,
11.0776608026002));
#32279=CARTESIAN_POINT('Ctrl Pts',(-2.58014059514451,-0.794772684001087,
11.0174934424942));
#32280=CARTESIAN_POINT('Ctrl Pts',(-2.53361645527697,-0.636309800095386,
10.9746833759411));
#32281=CARTESIAN_POINT('Ctrl Pts',(-2.47029199881909,-0.319434907277254,
10.9316507257101));
#32282=CARTESIAN_POINT('Ctrl Pts',(-2.44402307019611,-0.15833333333338,
10.9130133743054));
#32283=CARTESIAN_POINT('Ctrl Pts',(-2.42231413633528,0.158333333333381,
10.92738984692));
#32284=CARTESIAN_POINT('Ctrl Pts',(-2.42722284933438,0.319434907277263,
10.9602169003356));
#32285=CARTESIAN_POINT('Ctrl Pts',(-2.4456174566727,0.636309800095396,11.032913828414));
#32286=CARTESIAN_POINT('Ctrl Pts',(-2.4673458530226,0.794772684001076,11.0918301551621));
#32287=CARTESIAN_POINT('Ctrl Pts',(-2.50756957285321,1.06847604194612,11.1779141208763));
#32288=CARTESIAN_POINT('Ctrl Pts',(-2.52780280322549,1.18514270861349,11.2155104846413));
#32289=CARTESIAN_POINT('Ctrl Pts',(-2.55085790609104,1.30000000000239,11.2534406531388));
#32290=CARTESIAN_POINT('Ctrl Pts',(-2.73052114637815,-1.3000000000006,11.1140598974807));
#32291=CARTESIAN_POINT('Ctrl Pts',(-2.69121203817809,-1.18514270861227,
11.0832189188306));
#32292=CARTESIAN_POINT('Ctrl Pts',(-2.65417480751361,-1.06847604194549,
11.0540196347119));
#32293=CARTESIAN_POINT('Ctrl Pts',(-2.57385988700081,-0.794772684001062,
10.9903560898885));
#32294=CARTESIAN_POINT('Ctrl Pts',(-2.52683960535164,-0.636309800095369,
10.9485012201944));
#32295=CARTESIAN_POINT('Ctrl Pts',(-2.46323476709751,-0.319434907277246,
10.905476185748));
#32296=CARTESIAN_POINT('Ctrl Pts',(-2.43733245527519,-0.158333333333376,
10.8878982928609));
#32297=CARTESIAN_POINT('Ctrl Pts',(-2.41596612209797,0.158333333333377,
10.9020966854773));
#32298=CARTESIAN_POINT('Ctrl Pts',(-2.42094900457107,0.319434907277255,
10.9336232753893));
#32299=CARTESIAN_POINT('Ctrl Pts',(-2.44012184965078,0.63630980009538,11.0060780252185));
#32300=CARTESIAN_POINT('Ctrl Pts',(-2.46228533804278,0.794772684001055,
11.0640914506206));
#32301=CARTESIAN_POINT('Ctrl Pts',(-2.50412229577207,1.06847604194609,11.1535161961697));
#32302=CARTESIAN_POINT('Ctrl Pts',(-2.52524774255897,1.18514270861345,11.1934937403211));
#32303=CARTESIAN_POINT('Ctrl Pts',(-2.54938896734375,1.30000000000236,11.234740169789));
#32304=CARTESIAN_POINT('Ctrl Pts',(-2.72618669292035,-1.30000000000054,
11.090057041695));
#32305=CARTESIAN_POINT('Ctrl Pts',(-2.6852794327094,-1.18514270861222,11.0549236063513));
#32306=CARTESIAN_POINT('Ctrl Pts',(-2.64695621782421,-1.06847604194544,
11.0226451010771));
#32307=CARTESIAN_POINT('Ctrl Pts',(-2.56439158654555,-0.794772684001033,
10.954670756188));
#32308=CARTESIAN_POINT('Ctrl Pts',(-2.51675264711951,-0.636309800095345,
10.9140945200914));
#32309=CARTESIAN_POINT('Ctrl Pts',(-2.45250838794689,-0.319434907277234,
10.8712261373627));
#32310=CARTESIAN_POINT('Ctrl Pts',(-2.42678965977914,-0.15833333333337,
10.8552187665213));
#32311=CARTESIAN_POINT('Ctrl Pts',(-2.40611359010731,0.158333333333371,
10.8690496021633));
#32312=CARTESIAN_POINT('Ctrl Pts',(-2.41159051383702,0.319434907277242,
10.8985976683053));
#32313=CARTESIAN_POINT('Ctrl Pts',(-2.43283454080145,0.636309800095355,
10.9702294623685));
#32314=CARTESIAN_POINT('Ctrl Pts',(-2.45740069161927,0.794772684001025,
11.0262315201112));
#32315=CARTESIAN_POINT('Ctrl Pts',(-2.50098392074559,1.06847604194605,11.120292932966));
#32316=CARTESIAN_POINT('Ctrl Pts',(-2.52257860080518,1.18514270861341,11.1637706734171));
#32317=CARTESIAN_POINT('Ctrl Pts',(-2.54690239595331,1.30000000000231,11.2100104540132));
#32318=CARTESIAN_POINT('Ctrl Pts',(-2.72020047827003,-1.30000000000049,
11.0669081106694));
#32319=CARTESIAN_POINT('Ctrl Pts',(-2.67790604734494,-1.18514270861218,
11.0273779174215));
#32320=CARTESIAN_POINT('Ctrl Pts',(-2.63846510872675,-1.06847604194541,
10.9919366357417));
#32321=CARTESIAN_POINT('Ctrl Pts',(-2.55394078845416,-0.794772684001004,
10.9195063887635));
#32322=CARTESIAN_POINT('Ctrl Pts',(-2.50570797655504,-0.636309800095321,
10.8801953547377));
#32323=CARTESIAN_POINT('Ctrl Pts',(-2.44098964317585,-0.319434907277222,
10.8373965721291));
#32324=CARTESIAN_POINT('Ctrl Pts',(-2.41563858417114,-0.158333333333364,
10.8228649247209));
#32325=CARTESIAN_POINT('Ctrl Pts',(-2.39557038649268,0.158333333333365,
10.8363600501206));
#32326=CARTESIAN_POINT('Ctrl Pts',(-2.40157548437834,0.31943490727723,10.8639311832623));
#32327=CARTESIAN_POINT('Ctrl Pts',(-2.42394520017597,0.636309800095331,
10.9351466698216));
#32328=CARTESIAN_POINT('Ctrl Pts',(-2.44870206327488,0.794772684000997,
10.9900901533294));
#32329=CARTESIAN_POINT('Ctrl Pts',(-2.49448776363949,1.06847604194601,11.0885620182733));
#32330=CARTESIAN_POINT('Ctrl Pts',(-2.51737260574984,1.18514270861336,11.1351670001206));
#32331=CARTESIAN_POINT('Ctrl Pts',(-2.54332335681004,1.30000000000226,11.1857521422231));
#32332=CARTESIAN_POINT('Ctrl Pts',(-2.71488010558268,-1.30000000000047,
11.0433879560159));
#32333=CARTESIAN_POINT('Ctrl Pts',(-2.67119661166076,-1.18514270861215,
10.9994440491979));
#32334=CARTESIAN_POINT('Ctrl Pts',(-2.63052212327521,-1.06847604194538,
10.9608907478844));
#32335=CARTESIAN_POINT('Ctrl Pts',(-2.54350732293959,-0.794772684000988,
10.884278286391));
#32336=CARTESIAN_POINT('Ctrl Pts',(-2.49386695147061,-0.636309800095306,
10.8466866414759));
#32337=CARTESIAN_POINT('Ctrl Pts',(-2.42793766345227,-0.319434907277213,
10.8043600799878));
#32338=CARTESIAN_POINT('Ctrl Pts',(-2.40244873322788,-0.15833333333336,
10.7915861754419));
#32339=CARTESIAN_POINT('Ctrl Pts',(-2.38323040728465,0.158333333333362,
10.8046011359007));
#32340=CARTESIAN_POINT('Ctrl Pts',(-2.39059918924259,0.319434907277223,
10.829691026249));
#32341=CARTESIAN_POINT('Ctrl Pts',(-2.41514522222375,0.636309800095316,
10.8999518861306));
#32342=CARTESIAN_POINT('Ctrl Pts',(-2.44122298675669,0.794772684000977,
10.9533434101576));
#32343=CARTESIAN_POINT('Ctrl Pts',(-2.48924678398141,1.06847604194598,11.0562202485803));
#32344=CARTESIAN_POINT('Ctrl Pts',(-2.51312174160371,1.18514270861333,11.1060979118114));
#32345=CARTESIAN_POINT('Ctrl Pts',(-2.54008393448674,1.30000000000222,11.1613216668828));
#32346=CARTESIAN_POINT('Ctrl Pts',(-2.70911402584229,-1.30000000000036,
11.0234204248473));
#32347=CARTESIAN_POINT('Ctrl Pts',(-2.66373005632073,-1.18514270861205,
10.9759171644225));
#32348=CARTESIAN_POINT('Ctrl Pts',(-2.62175498217934,-1.06847604194529,
10.9347927600077));
#32349=CARTESIAN_POINT('Ctrl Pts',(-2.53265939410329,-0.794772684000918,
10.8545235923695));
#32350=CARTESIAN_POINT('Ctrl Pts',(-2.48305062346186,-0.636309800095253,
10.8177669943221));
#32351=CARTESIAN_POINT('Ctrl Pts',(-2.41646836772196,-0.319434907277188,
10.7756498564267));
#32352=CARTESIAN_POINT('Ctrl Pts',(-2.3906874974646,-0.158333333333347,
10.7645045281972));
#32353=CARTESIAN_POINT('Ctrl Pts',(-2.37167048785909,0.158333333333348,
10.7773744834247));
#32354=CARTESIAN_POINT('Ctrl Pts',(-2.37915028861769,0.319434907277195,
10.8008558590621));
#32355=CARTESIAN_POINT('Ctrl Pts',(-2.40553794661324,0.636309800095263,
10.8702757008739));
#32356=CARTESIAN_POINT('Ctrl Pts',(-2.43364132787521,0.794772684000912,
10.9218037896078));
#32357=CARTESIAN_POINT('Ctrl Pts',(-2.48442644900942,1.06847604194589,11.0280779511531));
#32358=CARTESIAN_POINT('Ctrl Pts',(-2.50952949299033,1.18514270861324,11.0806194354338));
#32359=CARTESIAN_POINT('Ctrl Pts',(-2.5377525837873,1.30000000000212,11.1397002573077));
#32360=CARTESIAN_POINT('Ctrl Pts',(-2.70353383063933,-1.30000000000036,
10.9999887293473));
#32361=CARTESIAN_POINT('Ctrl Pts',(-2.65640171232275,-1.18514270861205,
10.9482279231614));
#32362=CARTESIAN_POINT('Ctrl Pts',(-2.61284843769618,-1.06847604194529,
10.9041562286735));
#32363=CARTESIAN_POINT('Ctrl Pts',(-2.52049950537525,-0.79477268400092,
10.8201051841181));
#32364=CARTESIAN_POINT('Ctrl Pts',(-2.46859493916104,-0.636309800095253,
10.7856129456557));
#32365=CARTESIAN_POINT('Ctrl Pts',(-2.40099281991649,-0.319434907277187,
10.7438761231169));
#32366=CARTESIAN_POINT('Ctrl Pts',(-2.37662940595917,-0.158333333333347,
10.7336352602338));
#32367=CARTESIAN_POINT('Ctrl Pts',(-2.35854571391392,0.158333333333349,
10.7459410578073));
#32368=CARTESIAN_POINT('Ctrl Pts',(-2.36620623217419,0.319434907277197,
10.7675442578828));
#32369=CARTESIAN_POINT('Ctrl Pts',(-2.39416059005098,0.636309800095264,
10.8362688648969));
#32370=CARTESIAN_POINT('Ctrl Pts',(-2.42346068791063,0.794772684000911,
10.8862207282079));
#32371=CARTESIAN_POINT('Ctrl Pts',(-2.47663733261307,1.06847604194589,10.9968274519963));
#32372=CARTESIAN_POINT('Ctrl Pts',(-2.50291507230902,1.18514270861324,11.0525733958149));
#32373=CARTESIAN_POINT('Ctrl Pts',(-2.53245235259803,1.30000000000212,11.116187731107));
#32374=CARTESIAN_POINT('Ctrl Pts',(-2.69833596654814,-1.30000000000032,
10.9830060396341));
#32375=CARTESIAN_POINT('Ctrl Pts',(-2.64958615648012,-1.18514270861202,
10.9282953727471));
#32376=CARTESIAN_POINT('Ctrl Pts',(-2.6047560693387,-1.06847604194526,10.8821229387945));
#32377=CARTESIAN_POINT('Ctrl Pts',(-2.51024494391219,-0.794772684000899,
10.7951804057463));
#32378=CARTESIAN_POINT('Ctrl Pts',(-2.45809203088939,-0.636309800095237,
10.761587928484));
#32379=CARTESIAN_POINT('Ctrl Pts',(-2.38960851425324,-0.31943490727718,
10.7202309484447));
#32380=CARTESIAN_POINT('Ctrl Pts',(-2.36479931898168,-0.158333333333342,
10.7114988387911));
#32381=CARTESIAN_POINT('Ctrl Pts',(-2.34695005012083,0.158333333333344,
10.7236290565346));
#32382=CARTESIAN_POINT('Ctrl Pts',(-2.35510759647371,0.319434907277187,
10.7436092936404));
#32383=CARTESIAN_POINT('Ctrl Pts',(-2.38479397203959,0.636309800095246,
10.8114714082294));
#32384=CARTESIAN_POINT('Ctrl Pts',(-2.41546462185311,0.794772684000892,
10.8599534127673));
#32385=CARTESIAN_POINT('Ctrl Pts',(-2.471393618411,1.06847604194587,10.9732413382738));
#32386=CARTESIAN_POINT('Ctrl Pts',(-2.49903161954639,1.18514270861321,11.0311090911607));
#32387=CARTESIAN_POINT('Ctrl Pts',(-2.53009803158076,1.30000000000209,11.097806451714));
#32388=CARTESIAN_POINT('Ctrl Pts',(-2.69311023072135,-1.3000000000003,10.9659408795865));
#32389=CARTESIAN_POINT('Ctrl Pts',(-2.64291410704766,-1.185142708612,10.9080071562898));
#32390=CARTESIAN_POINT('Ctrl Pts',(-2.59675403835677,-1.06847604194525,
10.859633017996));
#32391=CARTESIAN_POINT('Ctrl Pts',(-2.49943913981101,-0.794772684000888,
10.7699636350696));
#32392=CARTESIAN_POINT('Ctrl Pts',(-2.44466296249883,-0.636309800095227,
10.738646337535));
#32393=CARTESIAN_POINT('Ctrl Pts',(-2.37626217071313,-0.319434907277174,
10.6970765318667));
#32394=CARTESIAN_POINT('Ctrl Pts',(-2.35501508934159,-0.15833333333334,
10.6875776769682));
#32395=CARTESIAN_POINT('Ctrl Pts',(-2.33819796752328,0.158333333333342,
10.6990649893284));
#32396=CARTESIAN_POINT('Ctrl Pts',(-2.34447911271732,0.319434907277183,
10.7187462166911));
#32397=CARTESIAN_POINT('Ctrl Pts',(-2.37485390637155,0.636309800095237,
10.7863729191327));
#32398=CARTESIAN_POINT('Ctrl Pts',(-2.40711206569752,0.79477268400088,10.8332727810217));
#32399=CARTESIAN_POINT('Ctrl Pts',(-2.46533825214189,1.06847604194585,10.9496658909979));
#32400=CARTESIAN_POINT('Ctrl Pts',(-2.49410027228615,1.18514270861319,11.0098921791677));
#32401=CARTESIAN_POINT('Ctrl Pts',(-2.52642035395566,1.30000000000207,11.0799624909882));
#32402=CARTESIAN_POINT('Ctrl Pts',(-2.68879778714322,-1.30000000000028,
10.9518289492139));
#32403=CARTESIAN_POINT('Ctrl Pts',(-2.63666143001629,-1.18514270861199,
10.8918972781788));
#32404=CARTESIAN_POINT('Ctrl Pts',(-2.58926308493424,-1.06847604194523,
10.8419658485832));
#32405=CARTESIAN_POINT('Ctrl Pts',(-2.49070918144798,-0.794772684000878,
10.7497168157353));
#32406=CARTESIAN_POINT('Ctrl Pts',(-2.43777016675234,-0.636309800095217,
10.7179763783682));
#32407=CARTESIAN_POINT('Ctrl Pts',(-2.37010102182277,-0.319434907277169,
10.675947759028));
#32408=CARTESIAN_POINT('Ctrl Pts',(-2.34949050527065,-0.158333333333338,
10.6671666584067));
#32409=CARTESIAN_POINT('Ctrl Pts',(-2.33211239333941,0.158333333333339,
10.6789569746833));
#32410=CARTESIAN_POINT('Ctrl Pts',(-2.33637043201771,0.319434907277178,
10.6986904147996));
#32411=CARTESIAN_POINT('Ctrl Pts',(-2.36655247148205,0.636309800095226,
10.7664419578325));
#32412=CARTESIAN_POINT('Ctrl Pts',(-2.39991574346204,0.794772684000865,
10.8120484177623));
#32413=CARTESIAN_POINT('Ctrl Pts',(-2.45985583774373,1.06847604194583,10.930792397416));
#32414=CARTESIAN_POINT('Ctrl Pts',(-2.48954170162142,1.18514270861317,10.9927928874551));
#32415=CARTESIAN_POINT('Ctrl Pts',(-2.52296758356156,1.30000000000205,11.065393998639));
#32416=CARTESIAN_POINT('Ctrl Pts',(-2.6829189620322,-1.30000000000027,10.9351338813409));
#32417=CARTESIAN_POINT('Ctrl Pts',(-2.6282936778402,-1.18514270861197,10.8724521279875));
#32418=CARTESIAN_POINT('Ctrl Pts',(-2.57942287118579,-1.06847604194522,
10.8202878113131));
#32419=CARTESIAN_POINT('Ctrl Pts',(-2.4798155255339,-0.79477268400087,10.7240751870941));
#32420=CARTESIAN_POINT('Ctrl Pts',(-2.43000817475013,-0.636309800095212,
10.6911348221682));
#32421=CARTESIAN_POINT('Ctrl Pts',(-2.36412291257034,-0.319434907277166,
10.6478639598545));
#32422=CARTESIAN_POINT('Ctrl Pts',(-2.34455008781469,-0.158333333333336,
10.6399331146946));
#32423=CARTESIAN_POINT('Ctrl Pts',(-2.3272641458419,0.158333333333338,10.6516441590843));
#32424=CARTESIAN_POINT('Ctrl Pts',(-2.33029888248175,0.319434907277175,
10.6705886890844));
#32425=CARTESIAN_POINT('Ctrl Pts',(-2.35945060103271,0.636309800095221,
10.7391345767872));
#32426=CARTESIAN_POINT('Ctrl Pts',(-2.39125326023901,0.794772684000859,
10.7850495283766));
#32427=CARTESIAN_POINT('Ctrl Pts',(-2.45240936131587,1.06847604194582,10.907725068849));
#32428=CARTESIAN_POINT('Ctrl Pts',(-2.48329430471972,1.18514270861316,10.9721548996655));
#32429=CARTESIAN_POINT('Ctrl Pts',(-2.51859198142806,1.30000000000203,11.0479128654045));
#32430=CARTESIAN_POINT('Ctrl Pts',(-2.67899628993017,-1.30000000000024,
10.9237203428818));
#32431=CARTESIAN_POINT('Ctrl Pts',(-2.62148033775193,-1.18514270861195,
10.8598450798923));
#32432=CARTESIAN_POINT('Ctrl Pts',(-2.57119727859248,-1.0684760419452,10.8064956917622));
#32433=CARTESIAN_POINT('Ctrl Pts',(-2.47174278265131,-0.794772684000851,
10.7075648092919));
#32434=CARTESIAN_POINT('Ctrl Pts',(-2.42808446301742,-0.636309800095197,
10.6722759426476));
#32435=CARTESIAN_POINT('Ctrl Pts',(-2.3654168542827,-0.319434907277159,
10.6276471138997));
#32436=CARTESIAN_POINT('Ctrl Pts',(-2.34617121474401,-0.158333333333332,
10.6207395121414));
#32437=CARTESIAN_POINT('Ctrl Pts',(-2.32904419103437,0.158333333333334,
10.632401614771));
#32438=CARTESIAN_POINT('Ctrl Pts',(-2.3318239996864,0.319434907277167,10.6503972077161));
#32439=CARTESIAN_POINT('Ctrl Pts',(-2.35825829213826,0.636309800095206,
10.7199503234929));
#32440=CARTESIAN_POINT('Ctrl Pts',(-2.38472809612601,0.79477268400084,10.7674363574646));
#32441=CARTESIAN_POINT('Ctrl Pts',(-2.44568313888404,1.0684760419458,10.8928702981304));
#32442=CARTESIAN_POINT('Ctrl Pts',(-2.47774091685543,1.18514270861313,10.958697047156));
#32443=CARTESIAN_POINT('Ctrl Pts',(-2.5154712933951,1.300000000002,11.0360548400783));
#32444=CARTESIAN_POINT('Ctrl Pts',(-2.67879510330303,-1.30000000000024,
10.9151206262377));
#32445=CARTESIAN_POINT('Ctrl Pts',(-2.62131393065162,-1.18514270861195,
10.8514942540814));
#32446=CARTESIAN_POINT('Ctrl Pts',(-2.5713673254344,-1.0684760419452,10.7982205274448));
#32447=CARTESIAN_POINT('Ctrl Pts',(-2.4733870336565,-0.794772684000851,
10.699064243732));
#32448=CARTESIAN_POINT('Ctrl Pts',(-2.43213760273471,-0.636309800095197,
10.6628920207773));
#32449=CARTESIAN_POINT('Ctrl Pts',(-2.37107459905216,-0.319434907277159,
10.6177437697791));
#32450=CARTESIAN_POINT('Ctrl Pts',(-2.35179040064045,-0.158333333333332,
10.6108007652544));
#32451=CARTESIAN_POINT('Ctrl Pts',(-2.33489442655109,0.158333333333334,
10.6224108757364));
#32452=CARTESIAN_POINT('Ctrl Pts',(-2.33820931733128,0.319434907277167,
10.6403006616186));
#32453=CARTESIAN_POINT('Ctrl Pts',(-2.36296888549193,0.636309800095206,
10.7104490253785));
#32454=CARTESIAN_POINT('Ctrl Pts',(-2.38602389855414,0.79477268400084,10.7592218256451));
#32455=CARTESIAN_POINT('Ctrl Pts',(-2.4456425950795,1.0684760419458,10.8848134171439));
#32456=CARTESIAN_POINT('Ctrl Pts',(-2.47765621323778,1.18514270861313,10.9504344264684));
#32457=CARTESIAN_POINT('Ctrl Pts',(-2.51587672491887,1.300000000002,11.0273124987845));
#32458=CARTESIAN_POINT('Ctrl Pts',(-2.67879510330291,-1.3,10.9151206262376));
#32459=CARTESIAN_POINT('Ctrl Pts',(-2.62131393065155,-1.18514270861178,
10.8514942540813));
#32460=CARTESIAN_POINT('Ctrl Pts',(-2.57136732543437,-1.06847604194512,
10.7982205274447));
#32461=CARTESIAN_POINT('Ctrl Pts',(-2.4733870336565,-0.794772684000851,
10.699064243732));
#32462=CARTESIAN_POINT('Ctrl Pts',(-2.43213760273471,-0.636309800095197,
10.6628920207773));
#32463=CARTESIAN_POINT('Ctrl Pts',(-2.37107459905216,-0.319434907277159,
10.6177437697791));
#32464=CARTESIAN_POINT('Ctrl Pts',(-2.35179040064045,-0.158333333333332,
10.6108007652544));
#32465=CARTESIAN_POINT('Ctrl Pts',(-2.33489442655109,0.158333333333334,
10.6224108757364));
#32466=CARTESIAN_POINT('Ctrl Pts',(-2.33820931733128,0.319434907277167,
10.6403006616186));
#32467=CARTESIAN_POINT('Ctrl Pts',(-2.36296888549193,0.636309800095206,
10.7104490253786));
#32468=CARTESIAN_POINT('Ctrl Pts',(-2.38602389855414,0.79477268400084,10.7592218256451));
#32469=CARTESIAN_POINT('Ctrl Pts',(-2.44564259507935,1.06847604194511,10.8848134171436));
#32470=CARTESIAN_POINT('Ctrl Pts',(-2.47765621323741,1.18514270861178,10.9504344264676));
#32471=CARTESIAN_POINT('Ctrl Pts',(-2.5158767249182,1.3,11.0273124987831));
#32472=CARTESIAN_POINT('',(-2.73377200308821,-1.2,11.3266197589711));
#32473=CARTESIAN_POINT('Ctrl Pts',(-2.73377200308821,-1.2,11.3266197589711));
#32474=CARTESIAN_POINT('Ctrl Pts',(-2.73576236750696,-1.21682511930476,
11.305118979092));
#32475=CARTESIAN_POINT('Ctrl Pts',(-2.73869233675414,-1.23325164823463,
11.2834011551542));
#32476=CARTESIAN_POINT('Ctrl Pts',(-2.7416170980304,-1.25864690463805,11.2507925097067));
#32477=CARTESIAN_POINT('Ctrl Pts',(-2.74261046385924,-1.26676740637328,
11.2403081349856));
#32478=CARTESIAN_POINT('Ctrl Pts',(-2.74424726899164,-1.28141903494891,
11.2214696307683));
#32479=CARTESIAN_POINT('Ctrl Pts',(-2.74534902187955,-1.29187033557532,
11.2080548826955));
#32480=CARTESIAN_POINT('Ctrl Pts',(-2.74593499828894,-1.29845679859462,
11.1996640849239));
#32481=CARTESIAN_POINT('Ctrl Pts',(-2.74600037704013,-1.29922898799516,
11.1986824960205));
#32482=CARTESIAN_POINT('Ctrl Pts',(-2.74606098174262,-1.30000000000076,
11.1977054774637));
#32483=CARTESIAN_POINT('',(-2.60194863161808,-0.653834841327687,11.4109812773269));
#32484=CARTESIAN_POINT('Ctrl Pts',(-2.60194863169232,-0.653834841312246,
11.4109812773313));
#32485=CARTESIAN_POINT('Ctrl Pts',(-2.61437551623445,-0.711429103212125,
11.4033027546542));
#32486=CARTESIAN_POINT('Ctrl Pts',(-2.62750506939667,-0.767209465733077,
11.3951126019967));
#32487=CARTESIAN_POINT('Ctrl Pts',(-2.65474262170037,-0.881586813988967,
11.3779310203753));
#32488=CARTESIAN_POINT('Ctrl Pts',(-2.66777274013477,-0.939011938483551,
11.3696339333288));
#32489=CARTESIAN_POINT('Ctrl Pts',(-2.69210580986878,-1.03699387118054,
11.353933891983));
#32490=CARTESIAN_POINT('Ctrl Pts',(-2.69333142495775,-1.0411369329597,11.3531667563918));
#32491=CARTESIAN_POINT('Ctrl Pts',(-2.71810657748227,-1.13882989710818,
11.3369709263887));
#32492=CARTESIAN_POINT('Ctrl Pts',(-2.72488491396426,-1.16582599832885,
11.3325072108943));
#32493=CARTESIAN_POINT('Ctrl Pts',(-2.73377200308821,-1.2,11.3266197589711));
#32494=CARTESIAN_POINT('',(-2.48224831221869,0.653834841531101,11.4826327552672));
#32495=CARTESIAN_POINT('Ctrl Pts',(-2.48224831221869,0.653834841531094,
11.4826327552672));
#32496=CARTESIAN_POINT('Ctrl Pts',(-2.47847611081766,0.575733241027942,
11.4410983042038));
#32497=CARTESIAN_POINT('Ctrl Pts',(-2.47624165072888,0.493688711564448,
11.4060553104082));
#32498=CARTESIAN_POINT('Ctrl Pts',(-2.47524533739703,0.338070081393044,
11.3554031699183));
#32499=CARTESIAN_POINT('Ctrl Pts',(-2.47618347792561,0.265612270873024,
11.3374916856793));
#32500=CARTESIAN_POINT('Ctrl Pts',(-2.48168727921389,0.129685337361217,
11.3136922909595));
#32501=CARTESIAN_POINT('Ctrl Pts',(-2.48565124756031,0.0666366523113049,
11.3064612606332));
#32502=CARTESIAN_POINT('Ctrl Pts',(-2.49684990484168,-0.0594732938431921,
11.2993200133022));
#32503=CARTESIAN_POINT('Ctrl Pts',(-2.50414835339649,-0.122670367054008,
11.2993485456319));
#32504=CARTESIAN_POINT('Ctrl Pts',(-2.5229219596009,-0.260039449736775,
11.307924387759));
#32505=CARTESIAN_POINT('Ctrl Pts',(-2.53495623693555,-0.333904359140863,
11.318007596868));
#32506=CARTESIAN_POINT('Ctrl Pts',(-2.56422571957007,-0.49149423887964,
11.352069384849));
#32507=CARTESIAN_POINT('Ctrl Pts',(-2.58242227177419,-0.574906056387881,
11.3781108287718));
#32508=CARTESIAN_POINT('Ctrl Pts',(-2.60194863169483,-0.653834841350394,
11.4109812772268));
#32509=CARTESIAN_POINT('',(-2.54449248972722,1.2,11.4459460629784));
#32510=CARTESIAN_POINT('Ctrl Pts',(-2.54449248972723,1.2,11.4459460629784));
#32511=CARTESIAN_POINT('Ctrl Pts',(-2.53481538344241,1.14033138422225,11.4517453180558));
#32512=CARTESIAN_POINT('Ctrl Pts',(-2.52020515509785,1.04182072801943,11.4604498142848));
#32513=CARTESIAN_POINT('Ctrl Pts',(-2.4925470916887,0.79704371814103,11.4766664306308));
#32514=CARTESIAN_POINT('Ctrl Pts',(-2.48792048827851,0.741502902961087,
11.4793451165048));
#32515=CARTESIAN_POINT('Ctrl Pts',(-2.48224831221869,0.653834841531102,
11.4826327552672));
#32516=CARTESIAN_POINT('Ctrl Pts',(-2.55655914734356,1.30000000000015,11.321468831149));
#32517=CARTESIAN_POINT('Ctrl Pts',(-2.55519028108804,1.28313676905805,11.3421620017419));
#32518=CARTESIAN_POINT('Ctrl Pts',(-2.55296550889272,1.2665451586595,11.3630099517663));
#32519=CARTESIAN_POINT('Ctrl Pts',(-2.54981239277721,1.23818291853827,11.3981516985073));
#32520=CARTESIAN_POINT('Ctrl Pts',(-2.54809619279288,1.21981197361561,11.420689297303));
#32521=CARTESIAN_POINT('Ctrl Pts',(-2.54449248972723,1.2,11.4459460629784));
#32522=CARTESIAN_POINT('Ctrl Pts',(-2.67879510330291,-1.3,10.9151206262376));
#32523=CARTESIAN_POINT('Ctrl Pts',(-2.62131393065155,-1.18514270861178,
10.8514942540813));
#32524=CARTESIAN_POINT('Ctrl Pts',(-2.57136732543437,-1.06847604194512,
10.7982205274447));
#32525=CARTESIAN_POINT('Ctrl Pts',(-2.4733870336565,-0.794772684000851,
10.699064243732));
#32526=CARTESIAN_POINT('Ctrl Pts',(-2.4321376027347,-0.636309800095197,
10.6628920207773));
#32527=CARTESIAN_POINT('Ctrl Pts',(-2.37107459905216,-0.319434907277159,
10.6177437697791));
#32528=CARTESIAN_POINT('Ctrl Pts',(-2.35179040064045,-0.158333333333332,
10.6108007652544));
#32529=CARTESIAN_POINT('Ctrl Pts',(-2.33489442655109,0.158333333333334,
10.6224108757364));
#32530=CARTESIAN_POINT('Ctrl Pts',(-2.33820931733128,0.319434907277167,
10.6403006616186));
#32531=CARTESIAN_POINT('Ctrl Pts',(-2.36296888549193,0.636309800095206,
10.7104490253785));
#32532=CARTESIAN_POINT('Ctrl Pts',(-2.38602389855414,0.79477268400084,10.7592218256451));
#32533=CARTESIAN_POINT('Ctrl Pts',(-2.44564259507935,1.06847604194511,10.8848134171436));
#32534=CARTESIAN_POINT('Ctrl Pts',(-2.47765621323741,1.18514270861178,10.9504344264676));
#32535=CARTESIAN_POINT('Ctrl Pts',(-2.5158767249182,1.3,11.0273124987831));
#32536=CARTESIAN_POINT('Ctrl Pts',(-2.74004401157309,-1.3,10.8685622702705));
#32537=CARTESIAN_POINT('Ctrl Pts',(-2.68128836180793,-1.18514270861178,
10.8061091896562));
#32538=CARTESIAN_POINT('Ctrl Pts',(-2.63048511284273,-1.06847604194512,
10.7536851161556));
#32539=CARTESIAN_POINT('Ctrl Pts',(-2.53149108129824,-0.794772684000851,
10.6557440316982));
#32540=CARTESIAN_POINT('Ctrl Pts',(-2.49090436112714,-0.636309800095197,
10.6192964682111));
#32541=CARTESIAN_POINT('Ctrl Pts',(-2.43050771496334,-0.319434907277159,
10.5741227058226));
#32542=CARTESIAN_POINT('Ctrl Pts',(-2.41232163607126,-0.158333333333332,
10.5666004040259));
#32543=CARTESIAN_POINT('Ctrl Pts',(-2.39563664855869,0.158333333333334,
10.5785009126177));
#32544=CARTESIAN_POINT('Ctrl Pts',(-2.39806125730008,0.319434907277167,
10.5972560595228));
#32545=CARTESIAN_POINT('Ctrl Pts',(-2.42259064688909,0.636309800095206,
10.66803028349));
#32546=CARTESIAN_POINT('Ctrl Pts',(-2.4451790066595,0.79477268400084,10.7173482742307));
#32547=CARTESIAN_POINT('Ctrl Pts',(-2.50626668917077,1.06847604194511,10.8423512591397));
#32548=CARTESIAN_POINT('Ctrl Pts',(-2.53935309295667,1.18514270861178,10.9074201091034));
#32549=CARTESIAN_POINT('Ctrl Pts',(-2.57908330629107,1.3,10.9834486486808));
#32550=CARTESIAN_POINT('Ctrl Pts',(-2.80129291984328,-1.3,10.8220039143035));
#32551=CARTESIAN_POINT('Ctrl Pts',(-2.7412627929643,-1.18514270861178,10.7607241252311));
#32552=CARTESIAN_POINT('Ctrl Pts',(-2.68960290025109,-1.06847604194512,
10.7091497048665));
#32553=CARTESIAN_POINT('Ctrl Pts',(-2.58959512893997,-0.794772684000851,
10.6124238196643));
#32554=CARTESIAN_POINT('Ctrl Pts',(-2.54967111951957,-0.636309800095197,
10.5757009156449));
#32555=CARTESIAN_POINT('Ctrl Pts',(-2.48994083087453,-0.319434907277159,
10.530501641866));
#32556=CARTESIAN_POINT('Ctrl Pts',(-2.47285287150207,-0.158333333333332,
10.5224000427974));
#32557=CARTESIAN_POINT('Ctrl Pts',(-2.4563788705663,0.158333333333334,10.5345909494989));
#32558=CARTESIAN_POINT('Ctrl Pts',(-2.45791319726889,0.319434907277167,
10.5542114574271));
#32559=CARTESIAN_POINT('Ctrl Pts',(-2.48221240828625,0.636309800095206,
10.6256115416015));
#32560=CARTESIAN_POINT('Ctrl Pts',(-2.50433411476485,0.79477268400084,10.6754747228163));
#32561=CARTESIAN_POINT('Ctrl Pts',(-2.5668907832622,1.06847604194511,10.7998891011359));
#32562=CARTESIAN_POINT('Ctrl Pts',(-2.60104997267594,1.18514270861178,10.8644057917392));
#32563=CARTESIAN_POINT('Ctrl Pts',(-2.64228988766393,1.3,10.9395847985784));
#32564=CARTESIAN_POINT('Ctrl Pts',(-2.86254182811346,-1.3,10.7754455583364));
#32565=CARTESIAN_POINT('Ctrl Pts',(-2.80123722412068,-1.18514270861178,
10.715339060806));
#32566=CARTESIAN_POINT('Ctrl Pts',(-2.74872068765946,-1.06847604194512,
10.6646142935774));
#32567=CARTESIAN_POINT('Ctrl Pts',(-2.6476991765817,-0.794772684000851,
10.5691036076304));
#32568=CARTESIAN_POINT('Ctrl Pts',(-2.60843787791201,-0.636309800095197,
10.5321053630787));
#32569=CARTESIAN_POINT('Ctrl Pts',(-2.54937394678571,-0.319434907277159,
10.4868805779095));
#32570=CARTESIAN_POINT('Ctrl Pts',(-2.53338410693288,-0.158333333333332,
10.4781996815688));
#32571=CARTESIAN_POINT('Ctrl Pts',(-2.5171210925739,0.158333333333334,10.4906809863802));
#32572=CARTESIAN_POINT('Ctrl Pts',(-2.5177651372377,0.319434907277167,10.5111668553313));
#32573=CARTESIAN_POINT('Ctrl Pts',(-2.54183416968341,0.636309800095206,
10.5831927997129));
#32574=CARTESIAN_POINT('Ctrl Pts',(-2.5634892228702,0.79477268400084,10.6336011714019));
#32575=CARTESIAN_POINT('Ctrl Pts',(-2.62751487735363,1.06847604194511,10.757426943132));
#32576=CARTESIAN_POINT('Ctrl Pts',(-2.6627468523952,1.18514270861178,10.821391474375));
#32577=CARTESIAN_POINT('Ctrl Pts',(-2.70549646903679,1.3,10.8957209484761));
#32578=CARTESIAN_POINT('Ctrl Pts',(-2.86254182811346,-1.3,10.7754455583364));
#32579=CARTESIAN_POINT('Ctrl Pts',(-2.80123722412068,-1.18514270861178,
10.715339060806));
#32580=CARTESIAN_POINT('Ctrl Pts',(-2.74872068765946,-1.06847604194512,
10.6646142935774));
#32581=CARTESIAN_POINT('Ctrl Pts',(-2.6476991765817,-0.794772684000851,
10.5691036076304));
#32582=CARTESIAN_POINT('Ctrl Pts',(-2.60843787791201,-0.636309800095197,
10.5321053630787));
#32583=CARTESIAN_POINT('Ctrl Pts',(-2.54937394678571,-0.319434907277159,
10.4868805779095));
#32584=CARTESIAN_POINT('Ctrl Pts',(-2.53338410693288,-0.158333333333332,
10.4781996815689));
#32585=CARTESIAN_POINT('Ctrl Pts',(-2.5171210925739,0.158333333333334,10.4906809863802));
#32586=CARTESIAN_POINT('Ctrl Pts',(-2.5177651372377,0.319434907277167,10.5111668553313));
#32587=CARTESIAN_POINT('Ctrl Pts',(-2.54183416968341,0.636309800095206,
10.5831927997129));
#32588=CARTESIAN_POINT('Ctrl Pts',(-2.56348922287021,0.79477268400084,10.6336011714019));
#32589=CARTESIAN_POINT('Ctrl Pts',(-2.62751487735363,1.06847604194511,10.757426943132));
#32590=CARTESIAN_POINT('Ctrl Pts',(-2.6627468523952,1.18514270861178,10.821391474375));
#32591=CARTESIAN_POINT('Ctrl Pts',(-2.70549646903679,1.3,10.8957209484761));
#32592=CARTESIAN_POINT('Ctrl Pts',(-2.86254182811353,-1.30000000000013,
10.7754455583365));
#32593=CARTESIAN_POINT('Ctrl Pts',(-2.80123722412072,-1.18514270861187,
10.715339060806));
#32594=CARTESIAN_POINT('Ctrl Pts',(-2.74872068765947,-1.06847604194516,
10.6646142935774));
#32595=CARTESIAN_POINT('Ctrl Pts',(-2.6476991765817,-0.794772684000851,
10.5691036076304));
#32596=CARTESIAN_POINT('Ctrl Pts',(-2.60843787791201,-0.636309800095197,
10.5321053630787));
#32597=CARTESIAN_POINT('Ctrl Pts',(-2.54937394678571,-0.319434907277159,
10.4868805779095));
#32598=CARTESIAN_POINT('Ctrl Pts',(-2.53338410693289,-0.158333333333332,
10.4781996815689));
#32599=CARTESIAN_POINT('Ctrl Pts',(-2.5171210925739,0.158333333333334,10.4906809863802));
#32600=CARTESIAN_POINT('Ctrl Pts',(-2.5177651372377,0.319434907277167,10.5111668553313));
#32601=CARTESIAN_POINT('Ctrl Pts',(-2.54183416968341,0.636309800095206,
10.5831927997129));
#32602=CARTESIAN_POINT('Ctrl Pts',(-2.56348922287021,0.79477268400084,10.6336011714019));
#32603=CARTESIAN_POINT('Ctrl Pts',(-2.62751487735368,1.06847604194532,10.7574269431321));
#32604=CARTESIAN_POINT('Ctrl Pts',(-2.66274685239533,1.18514270861219,10.8213914743752));
#32605=CARTESIAN_POINT('Ctrl Pts',(-2.70549646903702,1.30000000000061,10.8957209484765));
#32606=CARTESIAN_POINT('Ctrl Pts',(-2.87098157396354,-1.30000000000013,
10.7777615020269));
#32607=CARTESIAN_POINT('Ctrl Pts',(-2.80906926847882,-1.18514270861187,
10.7179729089025));
#32608=CARTESIAN_POINT('Ctrl Pts',(-2.75637070807042,-1.06847604194516,
10.6671425661359));
#32609=CARTESIAN_POINT('Ctrl Pts',(-2.65591208554583,-0.794772684000851,
10.5704096561886));
#32610=CARTESIAN_POINT('Ctrl Pts',(-2.61892980277956,-0.636309800095197,
10.5305613851358));
#32611=CARTESIAN_POINT('Ctrl Pts',(-2.56094950437881,-0.319434907277159,
10.4839277842398));
#32612=CARTESIAN_POINT('Ctrl Pts',(-2.54469368652178,-0.158333333333332,
10.4757230850146));
#32613=CARTESIAN_POINT('Ctrl Pts',(-2.52830982643484,0.158333333333334,
10.4884080646188));
#32614=CARTESIAN_POINT('Ctrl Pts',(-2.52893211645303,0.319434907277167,
10.5088463218988));
#32615=CARTESIAN_POINT('Ctrl Pts',(-2.55201129877011,0.636309800095206,
10.5822378260926));
#32616=CARTESIAN_POINT('Ctrl Pts',(-2.57208184262635,0.79477268400084,10.6346642149685));
#32617=CARTESIAN_POINT('Ctrl Pts',(-2.6354375736483,1.06847604194532,10.7598223853577));
#32618=CARTESIAN_POINT('Ctrl Pts',(-2.67063753705888,1.18514270861219,10.8241302839999));
#32619=CARTESIAN_POINT('Ctrl Pts',(-2.71361311548183,1.30000000000061,10.8985697468901));
#32620=CARTESIAN_POINT('Ctrl Pts',(-2.88130799910642,-1.30000000000008,
10.7843752712055));
#32621=CARTESIAN_POINT('Ctrl Pts',(-2.8201751994264,-1.18514270861182,10.7273767909063));
#32622=CARTESIAN_POINT('Ctrl Pts',(-2.76844666246347,-1.06847604194512,
10.6780839335672));
#32623=CARTESIAN_POINT('Ctrl Pts',(-2.67066912201355,-0.79477268400082,
10.582009102654));
#32624=CARTESIAN_POINT('Ctrl Pts',(-2.63680377542968,-0.636309800095171,
10.5376034533262));
#32625=CARTESIAN_POINT('Ctrl Pts',(-2.58060181184424,-0.319434907277146,
10.4887166000006));
#32626=CARTESIAN_POINT('Ctrl Pts',(-2.56351360569678,-0.158333333333326,
10.4799872004688));
#32627=CARTESIAN_POINT('Ctrl Pts',(-2.54702843312608,0.158333333333328,
10.4928124384856));
#32628=CARTESIAN_POINT('Ctrl Pts',(-2.54851681421681,0.319434907277155,
10.5138783362634));
#32629=CARTESIAN_POINT('Ctrl Pts',(-2.56933627910873,0.636309800095181,
10.589884803704));
#32630=CARTESIAN_POINT('Ctrl Pts',(-2.58533128900916,0.794772684000808,
10.6473785638044));
#32631=CARTESIAN_POINT('Ctrl Pts',(-2.64606408059228,1.06847604194528,10.7718410121851));
#32632=CARTESIAN_POINT('Ctrl Pts',(-2.68056571917546,1.18514270861214,10.8344520548743));
#32633=CARTESIAN_POINT('Ctrl Pts',(-2.72328002123719,1.30000000000056,10.905798958137));
#32634=CARTESIAN_POINT('Ctrl Pts',(-2.89657675896679,-1.30000000000006,
10.7939475114029));
#32635=CARTESIAN_POINT('Ctrl Pts',(-2.83786245193787,-1.18514270861181,
10.739717112883));
#32636=CARTESIAN_POINT('Ctrl Pts',(-2.78807069208927,-1.06847604194511,
10.6923235368659));
#32637=CARTESIAN_POINT('Ctrl Pts',(-2.69365463496759,-0.794772684000811,
10.5986293228974));
#32638=CARTESIAN_POINT('Ctrl Pts',(-2.66056908699804,-0.636309800095165,
10.5528292186773));
#32639=CARTESIAN_POINT('Ctrl Pts',(-2.60545199801408,-0.319434907277143,
10.5031969108166));
#32640=CARTESIAN_POINT('Ctrl Pts',(-2.58799440475969,-0.158333333333324,
10.4930527565231));
#32641=CARTESIAN_POINT('Ctrl Pts',(-2.57143636450316,0.158333333333326,
10.505914313829));
#32642=CARTESIAN_POINT('Ctrl Pts',(-2.57346983404538,0.319434907277151,
10.5281859967145));
#32643=CARTESIAN_POINT('Ctrl Pts',(-2.59254968088905,0.636309800095174,
10.6055115343826));
#32644=CARTESIAN_POINT('Ctrl Pts',(-2.60634895807667,0.794772684000802,
10.6656876864475));
#32645=CARTESIAN_POINT('Ctrl Pts',(-2.66362773438282,1.06847604194526,10.787923442475));
#32646=CARTESIAN_POINT('Ctrl Pts',(-2.69647182859621,1.18514270861213,10.8484289414837));
#32647=CARTESIAN_POINT('Ctrl Pts',(-2.73736615714789,1.30000000000054,10.9165286099978));
#32648=CARTESIAN_POINT('Ctrl Pts',(-2.90939733936904,-1.30000000000003,
10.8016830781138));
#32649=CARTESIAN_POINT('Ctrl Pts',(-2.85277794295122,-1.18514270861178,
10.7492279012714));
#32650=CARTESIAN_POINT('Ctrl Pts',(-2.80440263622773,-1.06847604194508,
10.7032260336092));
#32651=CARTESIAN_POINT('Ctrl Pts',(-2.71169149666796,-0.794772684000791,
10.6118609518534));
#32652=CARTESIAN_POINT('Ctrl Pts',(-2.67698456243157,-0.636309800095147,
10.5667713648255));
#32653=CARTESIAN_POINT('Ctrl Pts',(-2.62198781289779,-0.319434907277134,
10.5170532377087));
#32654=CARTESIAN_POINT('Ctrl Pts',(-2.60518369447283,-0.15833333333332,
10.5050370914482));
#32655=CARTESIAN_POINT('Ctrl Pts',(-2.58900027913727,0.158333333333322,
10.5175329029115));
#32656=CARTESIAN_POINT('Ctrl Pts',(-2.59136705757064,0.319434907277142,
10.5407427661508));
#32657=CARTESIAN_POINT('Ctrl Pts',(-2.6098427255564,0.636309800095157,10.618566234201));
#32658=CARTESIAN_POINT('Ctrl Pts',(-2.6229812366886,0.794772684000779,10.6800848080548));
#32659=CARTESIAN_POINT('Ctrl Pts',(-2.67822876463443,1.06847604194523,10.800342369775));
#32660=CARTESIAN_POINT('Ctrl Pts',(-2.70993424876684,1.18514270861209,10.8592459875587));
#32661=CARTESIAN_POINT('Ctrl Pts',(-2.74943060930655,1.3000000000005,10.9249981806394));
#32662=CARTESIAN_POINT('Ctrl Pts',(-2.92255067730094,-1.3,10.8092626647235));
#32663=CARTESIAN_POINT('Ctrl Pts',(-2.86823924221959,-1.18514270861175,
10.7587576758521));
#32664=CARTESIAN_POINT('Ctrl Pts',(-2.82142143722469,-1.06847604194506,
10.7143091764557));
#32665=CARTESIAN_POINT('Ctrl Pts',(-2.73057472641195,-0.794772684000774,
10.6256159532415));
#32666=CARTESIAN_POINT('Ctrl Pts',(-2.69426049879219,-0.636309800095134,
10.5813094568819));
#32667=CARTESIAN_POINT('Ctrl Pts',(-2.63898342204987,-0.319434907277128,
10.5319919830244));
#32668=CARTESIAN_POINT('Ctrl Pts',(-2.62245246795658,-0.158333333333317,
10.5183581005772));
#32669=CARTESIAN_POINT('Ctrl Pts',(-2.60566422148455,0.158333333333319,
10.531359703171));
#32670=CARTESIAN_POINT('Ctrl Pts',(-2.60681389033176,0.319434907277137,
10.5569638279893));
#32671=CARTESIAN_POINT('Ctrl Pts',(-2.62502863909171,0.636309800095145,
10.634865436697));
#32672=CARTESIAN_POINT('Ctrl Pts',(-2.64011247630467,0.794772684000763,
10.6953567565866));
#32673=CARTESIAN_POINT('Ctrl Pts',(-2.69385664340059,1.06847604194521,10.8126926805983));
#32674=CARTESIAN_POINT('Ctrl Pts',(-2.72422830809232,1.18514270861207,10.8698798781649));
#32675=CARTESIAN_POINT('Ctrl Pts',(-2.76170777895762,1.30000000000048,10.9334638995178));
#32676=CARTESIAN_POINT('Ctrl Pts',(-2.93364134797168,-1.29999999999998,
10.8146096561709));
#32677=CARTESIAN_POINT('Ctrl Pts',(-2.88110586058543,-1.18514270861173,
10.765538855818));
#32678=CARTESIAN_POINT('Ctrl Pts',(-2.83544209508976,-1.06847604194504,
10.722278164585));
#32679=CARTESIAN_POINT('Ctrl Pts',(-2.74582471404032,-0.79477268400076,
10.6357598279408));
#32680=CARTESIAN_POINT('Ctrl Pts',(-2.70815544963049,-0.636309800095123,
10.5921789864677));
#32681=CARTESIAN_POINT('Ctrl Pts',(-2.65198788829456,-0.319434907277122,
10.5437895582696));
#32682=CARTESIAN_POINT('Ctrl Pts',(-2.63461414097152,-0.158333333333314,
10.5299086096514));
#32683=CARTESIAN_POINT('Ctrl Pts',(-2.61730002870664,0.158333333333316,
10.5433402077525));
#32684=CARTESIAN_POINT('Ctrl Pts',(-2.61847805619027,0.31943490727713,10.5698315744701));
#32685=CARTESIAN_POINT('Ctrl Pts',(-2.63709993265635,0.636309800095133,
10.6472528854295));
#32686=CARTESIAN_POINT('Ctrl Pts',(-2.65397682566829,0.794772684000749,
10.7067377621516));
#32687=CARTESIAN_POINT('Ctrl Pts',(-2.70649287215143,1.06847604194519,10.8220022733572));
#32688=CARTESIAN_POINT('Ctrl Pts',(-2.73567401252214,1.18514270861205,10.8780795065985));
#32689=CARTESIAN_POINT('Ctrl Pts',(-2.7713040426523,1.30000000000045,10.9403402371513));
#32690=CARTESIAN_POINT('Ctrl Pts',(-2.94454127932457,-1.29999999999996,
10.8202105050095));
#32691=CARTESIAN_POINT('Ctrl Pts',(-2.89370153575553,-1.18514270861172,
10.7727504801566));
#32692=CARTESIAN_POINT('Ctrl Pts',(-2.84916686915389,-1.06847604194502,
10.7307723697174));
#32693=CARTESIAN_POINT('Ctrl Pts',(-2.76084886929562,-0.794772684000748,
10.6464588558599));
#32694=CARTESIAN_POINT('Ctrl Pts',(-2.72210825231037,-0.636309800095113,
10.6033006630912));
#32695=CARTESIAN_POINT('Ctrl Pts',(-2.66520808832749,-0.319434907277117,
10.5556735424191));
#32696=CARTESIAN_POINT('Ctrl Pts',(-2.64676320471826,-0.158333333333312,
10.5416884442415));
#32697=CARTESIAN_POINT('Ctrl Pts',(-2.62938737440501,0.158333333333314,
10.5551568985966));
#32698=CARTESIAN_POINT('Ctrl Pts',(-2.63171112765893,0.319434907277125,
10.5816477591922));
#32699=CARTESIAN_POINT('Ctrl Pts',(-2.65066224292211,0.636309800095123,
10.6586700857846));
#32700=CARTESIAN_POINT('Ctrl Pts',(-2.66783258409506,0.794772684000737,
10.7184529688622));
#32701=CARTESIAN_POINT('Ctrl Pts',(-2.71892149588491,1.06847604194518,10.8316990745312));
#32702=CARTESIAN_POINT('Ctrl Pts',(-2.74708102516698,1.18514270861203,10.8864396280687));
#32703=CARTESIAN_POINT('Ctrl Pts',(-2.78128558684804,1.30000000000044,10.9469006921814));
#32704=CARTESIAN_POINT('Ctrl Pts',(-2.96280984633306,-1.29999999999991,
10.8308072518359));
#32705=CARTESIAN_POINT('Ctrl Pts',(-2.91532013949125,-1.18514270861167,
10.7856898450932));
#32706=CARTESIAN_POINT('Ctrl Pts',(-2.87307106373488,-1.06847604194498,
10.7455850031852));
#32707=CARTESIAN_POINT('Ctrl Pts',(-2.78757415303104,-0.794772684000721,
10.6645148229603));
#32708=CARTESIAN_POINT('Ctrl Pts',(-2.74709018776719,-0.636309800095094,
10.6220267483154));
#32709=CARTESIAN_POINT('Ctrl Pts',(-2.68913215432975,-0.319434907277108,
10.57556179981));
#32710=CARTESIAN_POINT('Ctrl Pts',(-2.66916152367942,-0.158333333333307,
10.5611593392128));
#32711=CARTESIAN_POINT('Ctrl Pts',(-2.65102314855752,0.158333333333309,
10.5752777094955));
#32712=CARTESIAN_POINT('Ctrl Pts',(-2.65356013672887,0.319434907277116,
10.6032946602505));
#32713=CARTESIAN_POINT('Ctrl Pts',(-2.67313611639813,0.636309800095105,
10.6795440799993));
#32714=CARTESIAN_POINT('Ctrl Pts',(-2.69305833511178,0.794772684000714,
10.737821432715));
#32715=CARTESIAN_POINT('Ctrl Pts',(-2.74189854612259,1.06847604194515,10.8473865048979));
#32716=CARTESIAN_POINT('Ctrl Pts',(-2.76799328720399,1.18514270861199,10.9000916623425));
#32717=CARTESIAN_POINT('Ctrl Pts',(-2.79904165172837,1.30000000000039,10.9580753172698));
#32718=CARTESIAN_POINT('Ctrl Pts',(-2.99104878850529,-1.2999999999998,10.843667343189));
#32719=CARTESIAN_POINT('Ctrl Pts',(-2.94861710368942,-1.18514270861157,
10.8016268124618));
#32720=CARTESIAN_POINT('Ctrl Pts',(-2.90970236271676,-1.06847604194489,
10.7641432672306));
#32721=CARTESIAN_POINT('Ctrl Pts',(-2.82792637004268,-0.794772684000651,
10.6880763273062));
#32722=CARTESIAN_POINT('Ctrl Pts',(-2.78389301348772,-0.636309800095033,
10.6477071761781));
#32723=CARTESIAN_POINT('Ctrl Pts',(-2.72376072317303,-0.319434907277076,
10.603619031765));
#32724=CARTESIAN_POINT('Ctrl Pts',(-2.70111831575195,-0.158333333333292,
10.5890402621661));
#32725=CARTESIAN_POINT('Ctrl Pts',(-2.68261307994366,0.158333333333294,
10.6034604755936));
#32726=CARTESIAN_POINT('Ctrl Pts',(-2.68774540138619,0.319434907277086,
10.6316097871425));
#32727=CARTESIAN_POINT('Ctrl Pts',(-2.70815681023057,0.636309800095044,
10.7068015876387));
#32728=CARTESIAN_POINT('Ctrl Pts',(-2.72946345267766,0.794772684000635,
10.7652017115724));
#32729=CARTESIAN_POINT('Ctrl Pts',(-2.77434485092659,1.06847604194504,10.8701458336658));
#32730=CARTESIAN_POINT('Ctrl Pts',(-2.79750261992242,1.18514270861188,10.9199136815502));
#32731=CARTESIAN_POINT('Ctrl Pts',(-2.82439066363181,1.30000000000028,10.9740229554276));
#32732=CARTESIAN_POINT('Ctrl Pts',(-3.01834269857635,-1.29999999999968,
10.8574591123472));
#32733=CARTESIAN_POINT('Ctrl Pts',(-2.98046491035473,-1.18514270861146,
10.8190105036788));
#32734=CARTESIAN_POINT('Ctrl Pts',(-2.9447942397598,-1.06847604194479,10.7842434833884));
#32735=CARTESIAN_POINT('Ctrl Pts',(-2.86748673804234,-0.794772684000576,
10.7124299170517));
#32736=CARTESIAN_POINT('Ctrl Pts',(-2.82234682309723,-0.636309800094976,
10.6716853336954));
#32737=CARTESIAN_POINT('Ctrl Pts',(-2.76109407379248,-0.319434907277048,
10.6289560348325));
#32738=CARTESIAN_POINT('Ctrl Pts',(-2.73541472162827,-0.158333333333277,
10.6146850901235));
#32739=CARTESIAN_POINT('Ctrl Pts',(-2.71600552864647,0.158333333333279,
10.6299428199933));
#32740=CARTESIAN_POINT('Ctrl Pts',(-2.72268668763626,0.319434907277056,
10.6591473057952));
#32741=CARTESIAN_POINT('Ctrl Pts',(-2.74356713133065,0.636309800094986,
10.7336158510058));
#32742=CARTESIAN_POINT('Ctrl Pts',(-2.76711068084563,0.794772684000565,
10.7913518889265));
#32743=CARTESIAN_POINT('Ctrl Pts',(-2.80768348975369,1.06847604194495,10.8920278319734));
#32744=CARTESIAN_POINT('Ctrl Pts',(-2.82754652527184,1.18514270861178,10.9392085103723));
#32745=CARTESIAN_POINT('Ctrl Pts',(-2.84971013070257,1.30000000000016,10.9899909818365));
#32746=CARTESIAN_POINT('Ctrl Pts',(-3.04099809512413,-1.2999999999996,10.8675872666515));
#32747=CARTESIAN_POINT('Ctrl Pts',(-3.00762724759638,-1.18514270861139,
10.831064390507));
#32748=CARTESIAN_POINT('Ctrl Pts',(-2.97504038096538,-1.06847604194473,
10.7979362546403));
#32749=CARTESIAN_POINT('Ctrl Pts',(-2.9015693527738,-0.794772684000529,
10.7292461626843));
#32750=CARTESIAN_POINT('Ctrl Pts',(-2.85408545169189,-0.636309800094938,
10.6897924612697));
#32751=CARTESIAN_POINT('Ctrl Pts',(-2.79158851066336,-0.319434907277029,
10.6485850969138));
#32752=CARTESIAN_POINT('Ctrl Pts',(-2.76395740512797,-0.158333333333268,
10.6341165951374));
#32753=CARTESIAN_POINT('Ctrl Pts',(-2.74396501783023,0.15833333333327,10.6499441997137));
#32754=CARTESIAN_POINT('Ctrl Pts',(-2.75189768034267,0.319434907277039,
10.6799927615318));
#32755=CARTESIAN_POINT('Ctrl Pts',(-2.77307282462227,0.63630980009495,10.7539440471771));
#32756=CARTESIAN_POINT('Ctrl Pts',(-2.79821037766364,0.794772684000518,
10.8112808656079));
#32757=CARTESIAN_POINT('Ctrl Pts',(-2.83523034666321,1.06847604194488,10.9086287951997));
#32758=CARTESIAN_POINT('Ctrl Pts',(-2.85243431226021,1.18514270861171,10.9537645467817));
#32759=CARTESIAN_POINT('Ctrl Pts',(-2.87081767059933,1.30000000000008,11.0018977383219));
#32760=CARTESIAN_POINT('Ctrl Pts',(-3.05375053744494,-1.29999999999949,
10.8732488581604));
#32761=CARTESIAN_POINT('Ctrl Pts',(-3.02253872191128,-1.18514270861129,
10.8382134400058));
#32762=CARTESIAN_POINT('Ctrl Pts',(-2.9914515894023,-1.06847604194464,10.8062588675511));
#32763=CARTESIAN_POINT('Ctrl Pts',(-2.91992213707681,-0.794772684000461,
10.7395547825784));
#32764=CARTESIAN_POINT('Ctrl Pts',(-2.87147188423377,-0.636309800094884,
10.7004414750604));
#32765=CARTESIAN_POINT('Ctrl Pts',(-2.80852967755736,-0.319434907277002,
10.6598151083373));
#32766=CARTESIAN_POINT('Ctrl Pts',(-2.77999655012691,-0.158333333333255,
10.6450279038195));
#32767=CARTESIAN_POINT('Ctrl Pts',(-2.75983985593594,0.158333333333257,
10.6610058941037));
#32768=CARTESIAN_POINT('Ctrl Pts',(-2.76857308529266,0.319434907277011,
10.6914381411507));
#32769=CARTESIAN_POINT('Ctrl Pts',(-2.78973078923156,0.636309800094895,
10.7652887142333));
#32770=CARTESIAN_POINT('Ctrl Pts',(-2.81520148560987,0.794772684000449,
10.8229710284112));
#32771=CARTESIAN_POINT('Ctrl Pts',(-2.85020824756776,1.06847604194479,10.9184715141894));
#32772=CARTESIAN_POINT('Ctrl Pts',(-2.86603439018921,1.18514270861161,10.9623435382482));
#32773=CARTESIAN_POINT('Ctrl Pts',(-2.88253354530889,1.29999999999997,11.0087489647142));
#32774=CARTESIAN_POINT('Ctrl Pts',(-3.06242055860223,-1.29999999999949,
10.8768361729215));
#32775=CARTESIAN_POINT('Ctrl Pts',(-3.03267278550666,-1.18514270861128,
10.8427724582233));
#32776=CARTESIAN_POINT('Ctrl Pts',(-3.00261276335823,-1.06847604194463,
10.8115765723584));
#32777=CARTESIAN_POINT('Ctrl Pts',(-2.93244674093124,-0.794772684000459,
10.7461330936069));
#32778=CARTESIAN_POINT('Ctrl Pts',(-2.88343100137299,-0.636309800094882,
10.7071638759166));
#32779=CARTESIAN_POINT('Ctrl Pts',(-2.82021740568332,-0.319434907277,10.666908333352));
#32780=CARTESIAN_POINT('Ctrl Pts',(-2.79105344249383,-0.158333333333254,
10.6519528326215));
#32781=CARTESIAN_POINT('Ctrl Pts',(-2.77072506317317,0.158333333333256,
10.668100025496));
#32782=CARTESIAN_POINT('Ctrl Pts',(-2.7798575468528,0.31943490727701,10.6989198683978));
#32783=CARTESIAN_POINT('Ctrl Pts',(-2.80105893402106,0.636309800094892,
10.7726422267279));
#32784=CARTESIAN_POINT('Ctrl Pts',(-2.82711707716874,0.794772684000446,
10.830181207447));
#32785=CARTESIAN_POINT('Ctrl Pts',(-2.86065357629568,1.06847604194479,10.9245703549084));
#32786=CARTESIAN_POINT('Ctrl Pts',(-2.87540107879178,1.1851427086116,10.9677570528055));
#32787=CARTESIAN_POINT('Ctrl Pts',(-2.89037937596168,1.29999999999997,11.0132728841261));
#32788=CARTESIAN_POINT('Ctrl Pts',(-3.06815466520313,-1.29999999999948,
10.879276631911));
#32789=CARTESIAN_POINT('Ctrl Pts',(-3.03946963545971,-1.18514270861128,
10.8457621660883));
#32790=CARTESIAN_POINT('Ctrl Pts',(-3.01015132615301,-1.06847604194463,
10.8150076866289));
#32791=CARTESIAN_POINT('Ctrl Pts',(-2.94095716406855,-0.794772684000456,
10.7503348072978));
#32792=CARTESIAN_POINT('Ctrl Pts',(-2.89151463437421,-0.636309800094879,
10.7115234919949));
#32793=CARTESIAN_POINT('Ctrl Pts',(-2.82805721887487,-0.319434907276999,
10.6715838103291));
#32794=CARTESIAN_POINT('Ctrl Pts',(-2.79835809901693,-0.158333333333254,
10.656633107884));
#32795=CARTESIAN_POINT('Ctrl Pts',(-2.77792811427938,0.158333333333256,
10.6728825178909));
#32796=CARTESIAN_POINT('Ctrl Pts',(-2.78745064686552,0.319434907277009,
10.7038364701324));
#32797=CARTESIAN_POINT('Ctrl Pts',(-2.80877750206969,0.63630980009489,10.7773764406106));
#32798=CARTESIAN_POINT('Ctrl Pts',(-2.83527090747759,0.794772684000444,
10.8347736190766));
#32799=CARTESIAN_POINT('Ctrl Pts',(-2.86785556647318,1.06847604194479,10.9283947091163));
#32800=CARTESIAN_POINT('Ctrl Pts',(-2.88188448559708,1.1851427086116,10.9711253407065));
#32801=CARTESIAN_POINT('Ctrl Pts',(-2.89583763234629,1.29999999999996,11.0160615030121));
#32802=CARTESIAN_POINT('Ctrl Pts',(-3.07523784637402,-1.29999999999946,
10.8824189159388));
#32803=CARTESIAN_POINT('Ctrl Pts',(-3.04796476281486,-1.18514270861126,
10.849495529204));
#32804=CARTESIAN_POINT('Ctrl Pts',(-3.01962948296483,-1.06847604194461,
10.8192292580368));
#32805=CARTESIAN_POINT('Ctrl Pts',(-2.95171543213439,-0.794772684000441,
10.7554465854091));
#32806=CARTESIAN_POINT('Ctrl Pts',(-2.90168998820482,-0.636309800094867,
10.7168934624449));
#32807=CARTESIAN_POINT('Ctrl Pts',(-2.8378908573945,-0.319434907276993,
10.6773894319303));
#32808=CARTESIAN_POINT('Ctrl Pts',(-2.80745761776207,-0.158333333333251,
10.6625105926622));
#32809=CARTESIAN_POINT('Ctrl Pts',(-2.7869115402588,0.158333333333253,10.6788774623961));
#32810=CARTESIAN_POINT('Ctrl Pts',(-2.79701271806406,0.319434907277003,
10.7099064844615));
#32811=CARTESIAN_POINT('Ctrl Pts',(-2.81852503384429,0.636309800094878,
10.7831900258582));
#32812=CARTESIAN_POINT('Ctrl Pts',(-2.84549847764126,0.794772684000428,
10.8404745189034));
#32813=CARTESIAN_POINT('Ctrl Pts',(-2.87692789917283,1.06847604194477,10.9331029465521));
#32814=CARTESIAN_POINT('Ctrl Pts',(-2.89009076804454,1.18514270861158,10.9752324838597));
#32815=CARTESIAN_POINT('Ctrl Pts',(-2.90281187378179,1.29999999999994,11.0193961443673));
#32816=CARTESIAN_POINT('Ctrl Pts',(-3.08358965610494,-1.29999999999945,
10.8863527724723));
#32817=CARTESIAN_POINT('Ctrl Pts',(-3.05804567124122,-1.18514270861125,
10.8540971838029));
#32818=CARTESIAN_POINT('Ctrl Pts',(-3.03092169320698,-1.0684760419446,10.8243795583149));
#32819=CARTESIAN_POINT('Ctrl Pts',(-2.96460977751422,-0.794772684000435,
10.7615891011136));
#32820=CARTESIAN_POINT('Ctrl Pts',(-2.91395450626128,-0.636309800094863,
10.723269875));
#32821=CARTESIAN_POINT('Ctrl Pts',(-2.84972419210867,-0.319434907276991,
10.6843118023107));
#32822=CARTESIAN_POINT('Ctrl Pts',(-2.81832933467205,-0.158333333333249,
10.6696114794886));
#32823=CARTESIAN_POINT('Ctrl Pts',(-2.79752458508349,0.158333333333252,
10.686245596063));
#32824=CARTESIAN_POINT('Ctrl Pts',(-2.8082605562833,0.319434907277001,10.7174240573484));
#32825=CARTESIAN_POINT('Ctrl Pts',(-2.8298159803707,0.636309800094874,10.7905823439847));
#32826=CARTESIAN_POINT('Ctrl Pts',(-2.85717913317588,0.794772684000423,
10.847923536905));
#32827=CARTESIAN_POINT('Ctrl Pts',(-2.88712075511869,1.06847604194476,10.9394573178082));
#32828=CARTESIAN_POINT('Ctrl Pts',(-2.89923198379483,1.18514270861157,10.9808732955023));
#32829=CARTESIAN_POINT('Ctrl Pts',(-2.91049382245449,1.29999999999993,11.0240836687982));
#32830=CARTESIAN_POINT('Ctrl Pts',(-3.10080971693876,-1.29999999999934,
10.8936341625109));
#32831=CARTESIAN_POINT('Ctrl Pts',(-3.07833566280431,-1.18514270861116,
10.8631519636631));
#32832=CARTESIAN_POINT('Ctrl Pts',(-3.05335226645189,-1.06847604194452,
10.8348485035415));
#32833=CARTESIAN_POINT('Ctrl Pts',(-2.98983854045078,-0.794772684000373,
10.7744951708851));
#32834=CARTESIAN_POINT('Ctrl Pts',(-2.93783081929769,-0.636309800094812,
10.7367262126155));
#32835=CARTESIAN_POINT('Ctrl Pts',(-2.87309042237872,-0.319434907276965,
10.6984834504311));
#32836=CARTESIAN_POINT('Ctrl Pts',(-2.84049848157009,-0.158333333333237,
10.6833694821667));
#32837=CARTESIAN_POINT('Ctrl Pts',(-2.81968402648701,0.158333333333239,
10.6999957105264));
#32838=CARTESIAN_POINT('Ctrl Pts',(-2.83180795271723,0.319434907276975,
10.7313425331747));
#32839=CARTESIAN_POINT('Ctrl Pts',(-2.85344512895899,0.636309800094823,
10.8042529998644));
#32840=CARTESIAN_POINT('Ctrl Pts',(-2.881281674652,0.794772684000359,10.8620313005373));
#32841=CARTESIAN_POINT('Ctrl Pts',(-2.90806534832747,1.06847604194467,10.9515764346143));
#32842=CARTESIAN_POINT('Ctrl Pts',(-2.91801406667886,1.18514270861147,10.9916332152446));
#32843=CARTESIAN_POINT('Ctrl Pts',(-2.92631784348045,1.29999999999982,11.0329860059375));
#32844=CARTESIAN_POINT('Ctrl Pts',(-3.12726630276597,-1.29999999999915,
10.9037860597292));
#32845=CARTESIAN_POINT('Ctrl Pts',(-3.10990415514615,-1.18514270861097,
10.8753577686408));
#32846=CARTESIAN_POINT('Ctrl Pts',(-3.08851564146291,-1.06847604194435,
10.8487258397618));
#32847=CARTESIAN_POINT('Ctrl Pts',(-3.02980218501885,-0.794772684000252,
10.7913507124168));
#32848=CARTESIAN_POINT('Ctrl Pts',(-2.97608038840538,-0.636309800094717,
10.7541285055702));
#32849=CARTESIAN_POINT('Ctrl Pts',(-2.91005610250744,-0.319434907276919,
10.7175793582741));
#32850=CARTESIAN_POINT('Ctrl Pts',(-2.87460681156947,-0.158333333333213,
10.7030529564397));
#32851=CARTESIAN_POINT('Ctrl Pts',(-2.85267880346062,0.158333333333215,
10.7208784716313));
#32852=CARTESIAN_POINT('Ctrl Pts',(-2.86590325595896,0.319434907276927,
10.7534915361801));
#32853=CARTESIAN_POINT('Ctrl Pts',(-2.88786639021945,0.636309800094727,
10.8258180357411));
#32854=CARTESIAN_POINT('Ctrl Pts',(-2.91829508521574,0.794772684000243,
10.8822638836117));
#32855=CARTESIAN_POINT('Ctrl Pts',(-2.94066922555273,1.06847604194451,10.9684855749424));
#32856=CARTESIAN_POINT('Ctrl Pts',(-2.9472024446617,1.18514270861129,11.0066882228352));
#32857=CARTESIAN_POINT('Ctrl Pts',(-2.95058394657136,1.29999999999963,11.0457713432723));
#32858=CARTESIAN_POINT('Ctrl Pts',(-3.15602901483229,-1.29999999999882,
10.9157337896772));
#32859=CARTESIAN_POINT('Ctrl Pts',(-3.14419872081014,-1.18514270861068,
10.8897313639778));
#32860=CARTESIAN_POINT('Ctrl Pts',(-3.12675169145005,-1.06847604194409,
10.8650010651328));
#32861=CARTESIAN_POINT('Ctrl Pts',(-3.07346978110733,-0.794772684000054,
10.8108079950433));
#32862=CARTESIAN_POINT('Ctrl Pts',(-3.01816370804572,-0.63630980009456,
10.7738376644295));
#32863=CARTESIAN_POINT('Ctrl Pts',(-2.95126515113379,-0.31943490727684,
10.7385805017639));
#32864=CARTESIAN_POINT('Ctrl Pts',(-2.9128355854657,-0.158333333333174,
10.7245215983797));
#32865=CARTESIAN_POINT('Ctrl Pts',(-2.8907126092539,0.158333333333176,10.7425706729707));
#32866=CARTESIAN_POINT('Ctrl Pts',(-2.90693752767169,0.319434907276845,
10.7746836223076));
#32867=CARTESIAN_POINT('Ctrl Pts',(-2.92893953297227,0.636309800094568,
10.8466953240328));
#32868=CARTESIAN_POINT('Ctrl Pts',(-2.95940461178367,0.794772684000046,
10.9046636756723));
#32869=CARTESIAN_POINT('Ctrl Pts',(-2.97635305463127,1.06847604194425,10.9877859342387));
#32870=CARTESIAN_POINT('Ctrl Pts',(-2.97933175759914,1.185142708611,11.0236997722584));
#32871=CARTESIAN_POINT('Ctrl Pts',(-2.97795281062785,1.29999999999931,11.0595469025476));
#32872=CARTESIAN_POINT('Ctrl Pts',(-3.18010320518106,-1.29999999999858,
10.924026731429));
#32873=CARTESIAN_POINT('Ctrl Pts',(-3.17259939940327,-1.18514270861046,
10.9000631165806));
#32874=CARTESIAN_POINT('Ctrl Pts',(-3.15823173270695,-1.06847604194388,
10.8769284554676));
#32875=CARTESIAN_POINT('Ctrl Pts',(-3.1091826565641,-0.794772683999902,
10.8253978091835));
#32876=CARTESIAN_POINT('Ctrl Pts',(-3.05254831786319,-0.636309800094438,
10.7886958826654));
#32877=CARTESIAN_POINT('Ctrl Pts',(-2.98507404256285,-0.319434907276779,
10.7543604678475));
#32878=CARTESIAN_POINT('Ctrl Pts',(-2.94492658220406,-0.158333333333144,
10.7399863901776));
#32879=CARTESIAN_POINT('Ctrl Pts',(-2.92202390607915,0.158333333333146,
10.7589135934266));
#32880=CARTESIAN_POINT('Ctrl Pts',(-2.93866798081304,0.319434907276787,
10.7927720313494));
#32881=CARTESIAN_POINT('Ctrl Pts',(-2.96071475589337,0.636309800094449,
10.8645259076817));
#32882=CARTESIAN_POINT('Ctrl Pts',(-2.99356858890591,0.794772683999894,
10.9211606009691));
#32883=CARTESIAN_POINT('Ctrl Pts',(-3.00641322847654,1.06847604194404,11.0015499951531));
#32884=CARTESIAN_POINT('Ctrl Pts',(-3.00624339995034,1.18514270861077,11.0359634114943));
#32885=CARTESIAN_POINT('Ctrl Pts',(-3.00034377436861,1.29999999999906,11.0699926541552));
#32886=CARTESIAN_POINT('Ctrl Pts',(-3.19317119394676,-1.29999999999844,
10.9292052586356));
#32887=CARTESIAN_POINT('Ctrl Pts',(-3.18851667721922,-1.18514270861033,
10.905888404442));
#32888=CARTESIAN_POINT('Ctrl Pts',(-3.17612823403504,-1.06847604194377,
10.8833559052778));
#32889=CARTESIAN_POINT('Ctrl Pts',(-3.12964153469845,-0.794772683999815,
10.8331133416253));
#32890=CARTESIAN_POINT('Ctrl Pts',(-3.07159540712198,-0.636309800094369,
10.7973727984909));
#32891=CARTESIAN_POINT('Ctrl Pts',(-3.00380191880827,-0.319434907276744,
10.7635677244755));
#32892=CARTESIAN_POINT('Ctrl Pts',(-2.96290447793494,-0.158333333333126,
10.7487469719282));
#32893=CARTESIAN_POINT('Ctrl Pts',(-2.94019331992949,0.158333333333128,
10.7674662572841));
#32894=CARTESIAN_POINT('Ctrl Pts',(-2.95817659293092,0.319434907276751,
10.8010990163192));
#32895=CARTESIAN_POINT('Ctrl Pts',(-2.98012260412593,0.636309800094378,
10.8728450605019));
#32896=CARTESIAN_POINT('Ctrl Pts',(-3.01278690563514,0.794772683999808,
10.930407928881));
#32897=CARTESIAN_POINT('Ctrl Pts',(-3.02287677434149,1.06847604194393,11.0097570370282));
#32898=CARTESIAN_POINT('Ctrl Pts',(-3.02095452509254,1.18514270861064,11.0433115676966));
#32899=CARTESIAN_POINT('Ctrl Pts',(-3.01274249629816,1.29999999999891,11.0760733402908));
#32900=CARTESIAN_POINT('Ctrl Pts',(-3.20195356844581,-1.2999999999984,10.9325805430825));
#32901=CARTESIAN_POINT('Ctrl Pts',(-3.19905069408776,-1.18514270861029,
10.9098723006726));
#32902=CARTESIAN_POINT('Ctrl Pts',(-3.18791928835714,-1.06847604194373,
10.8878155849971));
#32903=CARTESIAN_POINT('Ctrl Pts',(-3.14319396070667,-0.794772683999789,
10.8383653164499));
#32904=CARTESIAN_POINT('Ctrl Pts',(-3.08471467087231,-0.636309800094348,
10.8026538736212));
#32905=CARTESIAN_POINT('Ctrl Pts',(-3.01669309422378,-0.319434907276734,
10.7692132537858));
#32906=CARTESIAN_POINT('Ctrl Pts',(-2.97494273212308,-0.158333333333121,
10.7545182980031));
#32907=CARTESIAN_POINT('Ctrl Pts',(-2.95200516165176,0.158333333333123,
10.7735019500123));
#32908=CARTESIAN_POINT('Ctrl Pts',(-2.97050921264184,0.319434907276741,
10.8073876617833));
#32909=CARTESIAN_POINT('Ctrl Pts',(-2.99243749225236,0.636309800094358,
10.8790747579997));
#32910=CARTESIAN_POINT('Ctrl Pts',(-3.02556140260726,0.794772683999782,
10.9366122936397));
#32911=CARTESIAN_POINT('Ctrl Pts',(-3.03400332614396,1.06847604194389,11.0150603449401));
#32912=CARTESIAN_POINT('Ctrl Pts',(-3.03091728399067,1.18514270861061,11.0480371272504));
#32913=CARTESIAN_POINT('Ctrl Pts',(-3.02109100378915,1.29999999999887,11.0800334372497));
#32914=CARTESIAN_POINT('Ctrl Pts',(-3.2078239063885,-1.29999999999838,10.9348154145648));
#32915=CARTESIAN_POINT('Ctrl Pts',(-3.20598833312576,-1.18514270861027,
10.9126326507061));
#32916=CARTESIAN_POINT('Ctrl Pts',(-3.19564031801075,-1.06847604194372,
10.8909578856118));
#32917=CARTESIAN_POINT('Ctrl Pts',(-3.15206888939482,-0.79477268399978,
10.8420584209926));
#32918=CARTESIAN_POINT('Ctrl Pts',(-3.09348408409014,-0.63630980009434,
10.8061442607962));
#32919=CARTESIAN_POINT('Ctrl Pts',(-3.02536870892628,-0.319434907276729,
10.7728771538103));
#32920=CARTESIAN_POINT('Ctrl Pts',(-2.98301636382883,-0.158333333333119,
10.7583098517379));
#32921=CARTESIAN_POINT('Ctrl Pts',(-2.95989991999098,0.158333333333121,
10.7775035462831));
#32922=CARTESIAN_POINT('Ctrl Pts',(-2.97870729740525,0.319434907276737,
10.8116079787124));
#32923=CARTESIAN_POINT('Ctrl Pts',(-3.00060901312884,0.63630980009435,10.8832717054751));
#32924=CARTESIAN_POINT('Ctrl Pts',(-3.03406590116684,0.794772683999772,
10.9407593352451));
#32925=CARTESIAN_POINT('Ctrl Pts',(-3.04141806022352,1.06847604194388,11.0185961538684));
#32926=CARTESIAN_POINT('Ctrl Pts',(-3.03755824404923,1.18514270861059,11.0511857312301));
#32927=CARTESIAN_POINT('Ctrl Pts',(-3.02665613446937,1.29999999999886,11.0826722113098));
#32928=CARTESIAN_POINT('Ctrl Pts',(-3.21827822516881,-1.29999999999833,
10.9385053407892));
#32929=CARTESIAN_POINT('Ctrl Pts',(-3.21831827069289,-1.18514270861023,
10.9172239362435));
#32930=CARTESIAN_POINT('Ctrl Pts',(-3.20933793812708,-1.06847604194368,
10.8962162353064));
#32931=CARTESIAN_POINT('Ctrl Pts',(-3.16775269548259,-0.794772683999748,
10.8483165536558));
#32932=CARTESIAN_POINT('Ctrl Pts',(-3.10890351858294,-0.636309800094315,
10.812154606619));
#32933=CARTESIAN_POINT('Ctrl Pts',(-3.04059454137874,-0.319434907276717,
10.7792317085672));
#32934=CARTESIAN_POINT('Ctrl Pts',(-2.99722861267192,-0.158333333333113,
10.7648411723961));
#32935=CARTESIAN_POINT('Ctrl Pts',(-2.97378898691106,0.158333333333115,
10.7844153481876));
#32936=CARTESIAN_POINT('Ctrl Pts',(-2.99308256531735,0.319434907276725,
10.8189529229403));
#32937=CARTESIAN_POINT('Ctrl Pts',(-3.01493552688533,0.636309800094325,
10.8905801274358));
#32938=CARTESIAN_POINT('Ctrl Pts',(-3.04902721113827,0.79477268399974,10.9479236125522));
#32939=CARTESIAN_POINT('Ctrl Pts',(-3.05446637157062,1.06847604194384,11.0246991870321));
#32940=CARTESIAN_POINT('Ctrl Pts',(-3.04923870066583,1.18514270861055,11.0566272492481));
#32941=CARTESIAN_POINT('Ctrl Pts',(-3.03642894784585,1.29999999999881,11.0872500723032));
#32942=CARTESIAN_POINT('Ctrl Pts',(-3.2303394252439,-1.29999999999813,10.9425619026323));
#32943=CARTESIAN_POINT('Ctrl Pts',(-3.23284776163168,-1.18514270861005,
10.9219129013773));
#32944=CARTESIAN_POINT('Ctrl Pts',(-3.22560190703575,-1.06847604194352,
10.9014572922326));
#32945=CARTESIAN_POINT('Ctrl Pts',(-3.18632840089931,-0.794772683999627,
10.8546475174401));
#32946=CARTESIAN_POINT('Ctrl Pts',(-3.12654679146467,-0.636309800094216,
10.8189703475746));
#32947=CARTESIAN_POINT('Ctrl Pts',(-3.05779687329653,-0.319434907276667,
10.7867111805289));
#32948=CARTESIAN_POINT('Ctrl Pts',(-3.01327450874528,-0.158333333333088,
10.7725141623555));
#32949=CARTESIAN_POINT('Ctrl Pts',(-2.98974250299873,0.15833333333309,10.7922101819601));
#32950=CARTESIAN_POINT('Ctrl Pts',(-3.0101308637112,0.319434907276676,10.8266298115445));
#32951=CARTESIAN_POINT('Ctrl Pts',(-3.03217400730282,0.636309800094226,
10.8979357227703));
#32952=CARTESIAN_POINT('Ctrl Pts',(-3.06689565791068,0.794772683999616,
10.9552203236505));
#32953=CARTESIAN_POINT('Ctrl Pts',(-3.06993147809271,1.06847604194367,11.0310329576894));
#32954=CARTESIAN_POINT('Ctrl Pts',(-3.06299302162609,1.18514270861036,11.0623753022289));
#32955=CARTESIAN_POINT('Ctrl Pts',(-3.04780201462427,1.2999999999986,11.0922435111674));
#32956=CARTESIAN_POINT('Ctrl Pts',(-3.24079513531022,-1.29999999999806,
10.9462274915081));
#32957=CARTESIAN_POINT('Ctrl Pts',(-3.24529551818108,-1.18514270860998,
10.9263349979427));
#32958=CARTESIAN_POINT('Ctrl Pts',(-3.23948544522855,-1.06847604194346,
10.9064610579923));
#32959=CARTESIAN_POINT('Ctrl Pts',(-3.20224379885544,-0.794772683999584,
10.860591143501));
#32960=CARTESIAN_POINT('Ctrl Pts',(-3.14205158607251,-0.636309800094183,
10.8248416467196));
#32961=CARTESIAN_POINT('Ctrl Pts',(-3.07300818112779,-0.31943490727665,
10.7930499844777));
#32962=CARTESIAN_POINT('Ctrl Pts',(-3.02732746867617,-0.15833333333308,
10.7792067503446));
#32963=CARTESIAN_POINT('Ctrl Pts',(-3.00360032053142,0.158333333333082,
10.7991416781415));
#32964=CARTESIAN_POINT('Ctrl Pts',(-3.02482853615089,0.319434907276658,
10.8335848462574));
#32965=CARTESIAN_POINT('Ctrl Pts',(-3.0470189317855,0.636309800094193,10.90462795134));
#32966=CARTESIAN_POINT('Ctrl Pts',(-3.08240549912536,0.794772683999574,
10.9617301143442));
#32967=CARTESIAN_POINT('Ctrl Pts',(-3.08340009269825,1.06847604194362,11.0366323287546));
#32968=CARTESIAN_POINT('Ctrl Pts',(-3.07498480978701,1.1851427086103,11.0674414679324));
#32969=CARTESIAN_POINT('Ctrl Pts',(-3.05772372126014,1.29999999999854,11.0966373530704));
#32970=CARTESIAN_POINT('Ctrl Pts',(-3.2461042721859,-1.29999999999804,10.9479547779649));
#32971=CARTESIAN_POINT('Ctrl Pts',(-3.25166886294995,-1.18514270860997,
10.9283516942736));
#32972=CARTESIAN_POINT('Ctrl Pts',(-3.24660822507569,-1.06847604194344,
10.9087271456776));
#32973=CARTESIAN_POINT('Ctrl Pts',(-3.2103707354848,-0.794772683999574,
10.86334092432));
#32974=CARTESIAN_POINT('Ctrl Pts',(-3.14977467070274,-0.636309800094174,
10.8278074737177));
#32975=CARTESIAN_POINT('Ctrl Pts',(-3.08057765298618,-0.319434907276646,
10.7962643145884));
#32976=CARTESIAN_POINT('Ctrl Pts',(-3.03449437995621,-0.158333333333078,
10.782386020323));
#32977=CARTESIAN_POINT('Ctrl Pts',(-3.01067167508799,0.15833333333308,10.8024375578468));
#32978=CARTESIAN_POINT('Ctrl Pts',(-3.03220630719915,0.319434907276654,
10.8370269173354));
#32979=CARTESIAN_POINT('Ctrl Pts',(-3.05435686985674,0.636309800094185,
10.9080702042062));
#32980=CARTESIAN_POINT('Ctrl Pts',(-3.08995186955548,0.794772683999564,
10.9652217061407));
#32981=CARTESIAN_POINT('Ctrl Pts',(-3.08994294375201,1.0684760419436,11.0396498899755));
#32982=CARTESIAN_POINT('Ctrl Pts',(-3.08083571066518,1.18514270861028,11.0701398337137));
#32983=CARTESIAN_POINT('Ctrl Pts',(-3.0626251081411,1.29999999999852,11.0989025182441));
#32984=CARTESIAN_POINT('Ctrl Pts',(-3.24914998256638,-1.29999999999804,
10.9489257242858));
#32985=CARTESIAN_POINT('Ctrl Pts',(-3.25533657941007,-1.18514270860996,
10.929470106966));
#32986=CARTESIAN_POINT('Ctrl Pts',(-3.25071124430535,-1.06847604194344,
10.9099789462566));
#32987=CARTESIAN_POINT('Ctrl Pts',(-3.21504806919795,-0.794772683999571,
10.8648683534842));
#32988=CARTESIAN_POINT('Ctrl Pts',(-3.15418675220007,-0.636309800094172,
10.8295019440878));
#32989=CARTESIAN_POINT('Ctrl Pts',(-3.08490169855022,-0.319434907276645,
10.7981023713605));
#32990=CARTESIAN_POINT('Ctrl Pts',(-3.03861899866046,-0.158333333333077,
10.7841677328696));
#32991=CARTESIAN_POINT('Ctrl Pts',(-3.0147430786694,0.158333333333079,10.8042843725331));
#32992=CARTESIAN_POINT('Ctrl Pts',(-3.0364346996967,0.319434907276653,10.8389786262426));
#32993=CARTESIAN_POINT('Ctrl Pts',(-3.05854295057592,0.636309800094182,
10.9100446506083));
#32994=CARTESIAN_POINT('Ctrl Pts',(-3.09423482136392,0.794772683999561,
10.9672494803309));
#32995=CARTESIAN_POINT('Ctrl Pts',(-3.0936531799886,1.0684760419436,11.0414062000157));
#32996=CARTESIAN_POINT('Ctrl Pts',(-3.08415726944502,1.18514270861028,11.0717062434621));
#32997=CARTESIAN_POINT('Ctrl Pts',(-3.06541721935728,1.29999999999851,11.1002066341807));
#32998=CARTESIAN_POINT('Ctrl Pts',(-3.2522037750961,-1.29999999999803,10.9498858595903));
#32999=CARTESIAN_POINT('Ctrl Pts',(-3.25902095733855,-1.18514270860995,
10.9305666068651));
#33000=CARTESIAN_POINT('Ctrl Pts',(-3.25483534210919,-1.06847604194343,
10.9112030885064));
#33001=CARTESIAN_POINT('Ctrl Pts',(-3.21974707033794,-0.794772683999564,
10.8663672249707));
#33002=CARTESIAN_POINT('Ctrl Pts',(-3.15859991758064,-0.636309800094167,
10.8311937863848));
#33003=CARTESIAN_POINT('Ctrl Pts',(-3.089226467721,-0.319434907276642,10.799939045965));
#33004=CARTESIAN_POINT('Ctrl Pts',(-3.04276163465701,-0.158333333333076,
10.7859277402349));
#33005=CARTESIAN_POINT('Ctrl Pts',(-3.01883418833475,0.158333333333078,
10.8061076516815));
#33006=CARTESIAN_POINT('Ctrl Pts',(-3.04067416343987,0.319434907276651,
10.8409169435151));
#33007=CARTESIAN_POINT('Ctrl Pts',(-3.06272970526287,0.636309800094177,
10.9120177369764));
#33008=CARTESIAN_POINT('Ctrl Pts',(-3.09850592289566,0.794772683999555,
10.969290063757));
#33009=CARTESIAN_POINT('Ctrl Pts',(-3.09735039907804,1.06847604194359,11.0431768350281));
#33010=CARTESIAN_POINT('Ctrl Pts',(-3.08746850869887,1.18514270861027,11.0732840274282));
#33011=CARTESIAN_POINT('Ctrl Pts',(-3.06820491138482,1.2999999999985,11.1015155667196));
#33012=CARTESIAN_POINT('Ctrl Pts',(-3.25602504189697,-1.29999999999801,
10.9510798888505));
#33013=CARTESIAN_POINT('Ctrl Pts',(-3.26363685807521,-1.18514270860993,
10.9319227517664));
#33014=CARTESIAN_POINT('Ctrl Pts',(-3.2600049829205,-1.06847604194341,10.9127134541495));
#33015=CARTESIAN_POINT('Ctrl Pts',(-3.22563944848708,-0.794772683999553,
10.8682156325821));
#33016=CARTESIAN_POINT('Ctrl Pts',(-3.16412692814332,-0.636309800094157,
10.8332933902027));
#33017=CARTESIAN_POINT('Ctrl Pts',(-3.09464460637555,-0.319434907276637,
10.8022185450546));
#33018=CARTESIAN_POINT('Ctrl Pts',(-3.0479593676407,-0.158333333333074,
10.788103923345));
#33019=CARTESIAN_POINT('Ctrl Pts',(-3.02396993643298,0.158333333333076,
10.8083605668864));
#33020=CARTESIAN_POINT('Ctrl Pts',(-3.04599441333248,0.319434907276646,
10.8433144176721));
#33021=CARTESIAN_POINT('Ctrl Pts',(-3.06797944317755,0.636309800094167,
10.9144639024002));
#33022=CARTESIAN_POINT('Ctrl Pts',(-3.10385470629991,0.794772683999542,
10.9718277275117));
#33023=CARTESIAN_POINT('Ctrl Pts',(-3.10197566521276,1.06847604194357,11.0453844124093));
#33024=CARTESIAN_POINT('Ctrl Pts',(-3.09160897176982,1.18514270861025,11.0752534399488));
#33025=CARTESIAN_POINT('Ctrl Pts',(-3.07168895214525,1.29999999999848,11.1031515316794));
#33026=CARTESIAN_POINT('Ctrl Pts',(-3.25983121780103,-1.29999999999798,
10.9522921169358));
#33027=CARTESIAN_POINT('Ctrl Pts',(-3.2682232328086,-1.18514270860991,10.9333152942735));
#33028=CARTESIAN_POINT('Ctrl Pts',(-3.26514019968536,-1.0684760419434,10.914266350886));
#33029=CARTESIAN_POINT('Ctrl Pts',(-3.23150811965428,-0.79477268399954,
10.87009286763));
#33030=CARTESIAN_POINT('Ctrl Pts',(-3.16968791589892,-0.636309800094147,
10.8353486978133));
#33031=CARTESIAN_POINT('Ctrl Pts',(-3.10010376764258,-0.319434907276632,
10.8044448005871));
#33032=CARTESIAN_POINT('Ctrl Pts',(-3.05315163017489,-0.158333333333071,
10.7902851974788));
#33033=CARTESIAN_POINT('Ctrl Pts',(-3.02910177510456,0.158333333333073,
10.8106178616161));
#33034=CARTESIAN_POINT('Ctrl Pts',(-3.05134352126923,0.319434907276641,
10.8456766004499));
#33035=CARTESIAN_POINT('Ctrl Pts',(-3.0732853111402,0.636309800094157,10.9168428086852));
#33036=CARTESIAN_POINT('Ctrl Pts',(-3.10929020858042,0.794772683999529,
10.9742631704055));
#33037=CARTESIAN_POINT('Ctrl Pts',(-3.1066698378272,1.06847604194355,11.0475104035141));
#33038=CARTESIAN_POINT('Ctrl Pts',(-3.09579807220139,1.18514270861023,11.0771646918295));
#33039=CARTESIAN_POINT('Ctrl Pts',(-3.07518880235454,1.29999999999846,11.1047672553249));
#33040=CARTESIAN_POINT('Ctrl Pts',(-3.26285879810893,-1.29999999999797,
10.9532835226745));
#33041=CARTESIAN_POINT('Ctrl Pts',(-3.27185662151802,-1.1851427086099,10.9344741764721));
#33042=CARTESIAN_POINT('Ctrl Pts',(-3.26920527733258,-1.06847604194339,
10.9155628521418));
#33043=CARTESIAN_POINT('Ctrl Pts',(-3.23616823431326,-0.794772683999533,
10.8716383198648));
#33044=CARTESIAN_POINT('Ctrl Pts',(-3.17416424763992,-0.636309800094141,
10.8369578318921));
#33045=CARTESIAN_POINT('Ctrl Pts',(-3.10450550169272,-0.319434907276629,
10.8061814921185));
#33046=CARTESIAN_POINT('Ctrl Pts',(-3.05729089109247,-0.15833333333307,
10.7920463667222));
#33047=CARTESIAN_POINT('Ctrl Pts',(-3.03319235162169,0.158333333333072,
10.8124410566994));
#33048=CARTESIAN_POINT('Ctrl Pts',(-3.05563863850475,0.319434907276638,
10.8475467077765));
#33049=CARTESIAN_POINT('Ctrl Pts',(-3.07757469698629,0.636309800094151,
10.9186926267006));
#33050=CARTESIAN_POINT('Ctrl Pts',(-3.1137177384153,0.794772683999522,10.9761189313738));
#33051=CARTESIAN_POINT('Ctrl Pts',(-3.1104911948604,1.06847604194355,11.0491337572892));
#33052=CARTESIAN_POINT('Ctrl Pts',(-3.09919727000925,1.18514270861022,11.0786371083924));
#33053=CARTESIAN_POINT('Ctrl Pts',(-3.07800607145667,1.29999999999845,11.106038397926));
#33054=CARTESIAN_POINT('Ctrl Pts',(-3.26512130110185,-1.29999999999797,
10.9540372474851));
#33055=CARTESIAN_POINT('Ctrl Pts',(-3.27456462137896,-1.1851427086099,10.9353646813646));
#33056=CARTESIAN_POINT('Ctrl Pts',(-3.27223346753816,-1.06847604194338,
10.9165610678225));
#33057=CARTESIAN_POINT('Ctrl Pts',(-3.23964664513232,-0.794772683999528,
10.8728182131305));
#33058=CARTESIAN_POINT('Ctrl Pts',(-3.17753465024573,-0.636309800094137,
10.838147852488));
#33059=CARTESIAN_POINT('Ctrl Pts',(-3.10782359105474,-0.319434907276627,
10.8074623493028));
#33060=CARTESIAN_POINT('Ctrl Pts',(-3.06038943072611,-0.158333333333069,
10.7933735951485));
#33061=CARTESIAN_POINT('Ctrl Pts',(-3.03625414615705,0.158333333333071,
10.8138154556009));
#33062=CARTESIAN_POINT('Ctrl Pts',(-3.0588676056342,0.319434907276636,10.8489397238093));
#33063=CARTESIAN_POINT('Ctrl Pts',(-3.08081297157187,0.636309800094147,
10.920054595231));
#33064=CARTESIAN_POINT('Ctrl Pts',(-3.1170765070553,0.794772683999518,10.9774660881753));
#33065=CARTESIAN_POINT('Ctrl Pts',(-3.11338943202109,1.06847604194354,11.0503134887088));
#33066=CARTESIAN_POINT('Ctrl Pts',(-3.10177040926063,1.18514270861021,11.0797134368291));
#33067=CARTESIAN_POINT('Ctrl Pts',(-3.08012836190243,1.29999999999844,11.106980392641));
#33068=CARTESIAN_POINT('Ctrl Pts',(-3.26700083590201,-1.29999999999796,
10.9546726147595));
#33069=CARTESIAN_POINT('Ctrl Pts',(-3.27680898774437,-1.18514270860989,
10.9361220819641));
#33070=CARTESIAN_POINT('Ctrl Pts',(-3.27474209984817,-1.06847604194337,
10.9174114201572));
#33071=CARTESIAN_POINT('Ctrl Pts',(-3.24253345793881,-0.794772683999523,
10.8738161182781));
#33072=CARTESIAN_POINT('Ctrl Pts',(-3.18035310750234,-0.636309800094134,
10.8391269232331));
#33073=CARTESIAN_POINT('Ctrl Pts',(-3.1106016129151,-0.319434907276625,
10.8085129890696));
#33074=CARTESIAN_POINT('Ctrl Pts',(-3.06296897051024,-0.158333333333068,
10.7944820510319));
#33075=CARTESIAN_POINT('Ctrl Pts',(-3.0388028643722,0.15833333333307,10.814963736934));
#33076=CARTESIAN_POINT('Ctrl Pts',(-3.06156451504281,0.319434907276634,
10.8500928419119));
#33077=CARTESIAN_POINT('Ctrl Pts',(-3.08352719265029,0.636309800094144,
10.9211707680412));
#33078=CARTESIAN_POINT('Ctrl Pts',(-3.11990372997025,0.794772683999513,
10.9785555320188));
#33079=CARTESIAN_POINT('Ctrl Pts',(-3.11582897433454,1.06847604194353,11.051268042067));
#33080=CARTESIAN_POINT('Ctrl Pts',(-3.10393309734347,1.18514270861021,11.0805887333396));
#33081=CARTESIAN_POINT('Ctrl Pts',(-3.08190515409146,1.29999999999843,11.1077555645489));
#33082=CARTESIAN_POINT('Ctrl Pts',(-3.26822071808255,-1.29999999999796,
10.9550877927237));
#33083=CARTESIAN_POINT('Ctrl Pts',(-3.27826398910814,-1.18514270860989,
10.936619089118));
#33084=CARTESIAN_POINT('Ctrl Pts',(-3.27636811928977,-1.06847604194337,
10.9179697712191));
#33085=CARTESIAN_POINT('Ctrl Pts',(-3.24440647697536,-0.794772683999522,
10.8744688609399));
#33086=CARTESIAN_POINT('Ctrl Pts',(-3.18218878382604,-0.636309800094133,
10.8397585327295));
#33087=CARTESIAN_POINT('Ctrl Pts',(-3.11241252899853,-0.319434907276625,
10.8091891951106));
#33088=CARTESIAN_POINT('Ctrl Pts',(-3.06464662184015,-0.158333333333068,
10.7952011106947));
#33089=CARTESIAN_POINT('Ctrl Pts',(-3.0404604264161,0.15833333333307,10.8157088562877));
#33090=CARTESIAN_POINT('Ctrl Pts',(-3.06332043523314,0.319434907276634,
10.8508386805889));
#33091=CARTESIAN_POINT('Ctrl Pts',(-3.08529713446789,0.636309800094143,
10.9218894186497));
#33092=CARTESIAN_POINT('Ctrl Pts',(-3.1217513001438,0.794772683999512,10.9792520038199));
#33093=CARTESIAN_POINT('Ctrl Pts',(-3.11742350878161,1.06847604194353,11.0518781349094));
#33094=CARTESIAN_POINT('Ctrl Pts',(-3.10534591028257,1.18514270861021,11.0811494049298));
#33095=CARTESIAN_POINT('Ctrl Pts',(-3.08306405380469,1.29999999999843,11.1082547838853));
#33096=CARTESIAN_POINT('Ctrl Pts',(-3.26878350127814,-1.29999999999796,
10.9552796922352));
#33097=CARTESIAN_POINT('Ctrl Pts',(-3.27893502398191,-1.18514270860989,
10.9368490790607));
#33098=CARTESIAN_POINT('Ctrl Pts',(-3.2771179959373,-1.06847604194337,10.9182281800829));
#33099=CARTESIAN_POINT('Ctrl Pts',(-3.24527055112992,-0.794772683999522,
10.8747705800738));
#33100=CARTESIAN_POINT('Ctrl Pts',(-3.18303660409327,-0.636309800094133,
10.8400492724346));
#33101=CARTESIAN_POINT('Ctrl Pts',(-3.11324920707446,-0.319434907276625,
10.8095001642765));
#33102=CARTESIAN_POINT('Ctrl Pts',(-3.06542132947862,-0.158333333333068,
10.7955324393821));
#33103=CARTESIAN_POINT('Ctrl Pts',(-3.04122585740674,0.15833333333307,10.8160522357225));
#33104=CARTESIAN_POINT('Ctrl Pts',(-3.06413141273467,0.319434907276633,
10.851182215591));
#33105=CARTESIAN_POINT('Ctrl Pts',(-3.08611491678922,0.636309800094143,
10.9222200294419));
#33106=CARTESIAN_POINT('Ctrl Pts',(-3.12260550379441,0.794772683999512,
10.9795716923723));
#33107=CARTESIAN_POINT('Ctrl Pts',(-3.11816081934627,1.06847604194353,11.0521581036447));
#33108=CARTESIAN_POINT('Ctrl Pts',(-3.10599913119212,1.1851427086102,11.0814068304583));
#33109=CARTESIAN_POINT('Ctrl Pts',(-3.08359969408964,1.29999999999843,11.1084843162373));
#33110=CARTESIAN_POINT('Ctrl Pts',(-3.26906484675215,-1.29999999999796,
10.9553756952532));
#33111=CARTESIAN_POINT('Ctrl Pts',(-3.27927044399567,-1.18514270860989,
10.9369641894471));
#33112=CARTESIAN_POINT('Ctrl Pts',(-3.27749281955508,-1.06847604194337,
10.9183575200967));
#33113=CARTESIAN_POINT('Ctrl Pts',(-3.24570251215918,-0.794772683999522,
10.8749215248163));
#33114=CARTESIAN_POINT('Ctrl Pts',(-3.18346062881311,-0.636309800094133,
10.8401944891827));
#33115=CARTESIAN_POINT('Ctrl Pts',(-3.11366771647733,-0.319434907276625,
10.8096554267729));
#33116=CARTESIAN_POINT('Ctrl Pts',(-3.06580876385529,-0.158333333333068,
10.7956979946858));
#33117=CARTESIAN_POINT('Ctrl Pts',(-3.04160865286627,0.15833333333307,10.8162238206007));
#33118=CARTESIAN_POINT('Ctrl Pts',(-3.06453701000585,0.319434907276633,
10.8513538442853));
#33119=CARTESIAN_POINT('Ctrl Pts',(-3.08652398303935,0.636309800094143,
10.9223851210484));
#33120=CARTESIAN_POINT('Ctrl Pts',(-3.12303290043782,0.794772683999512,
10.9797311847854));
#33121=CARTESIAN_POINT('Ctrl Pts',(-3.1185297481833,1.06847604194353,11.0522977658325));
#33122=CARTESIAN_POINT('Ctrl Pts',(-3.10632597148495,1.18514270861021,11.0815352746523));
#33123=CARTESIAN_POINT('Ctrl Pts',(-3.08386766584099,1.29999999999843,11.1085989082136));
#33124=CARTESIAN_POINT('Ctrl Pts',(-3.26929927812004,-1.29999999999795,
10.9554557230908));
#33125=CARTESIAN_POINT('Ctrl Pts',(-3.27954991189458,-1.18514270860989,
10.9370601705783));
#33126=CARTESIAN_POINT('Ctrl Pts',(-3.27780511729567,-1.06847604194337,
10.9184653664804));
#33127=CARTESIAN_POINT('Ctrl Pts',(-3.24606245350732,-0.794772683999522,
10.875047338114));
#33128=CARTESIAN_POINT('Ctrl Pts',(-3.18381406354817,-0.636309800094132,
10.8403153969248));
#33129=CARTESIAN_POINT('Ctrl Pts',(-3.11401660292878,-0.319434907276625,
10.8097846479383));
#33130=CARTESIAN_POINT('Ctrl Pts',(-3.06613173190375,-0.158333333333067,
10.7958358224271));
#33131=CARTESIAN_POINT('Ctrl Pts',(-3.04192775500594,0.15833333333307,10.8163666756604));
#33132=CARTESIAN_POINT('Ctrl Pts',(-3.06487510153954,0.319434907276633,
10.8514967520241));
#33133=CARTESIAN_POINT('Ctrl Pts',(-3.08686498759334,0.636309800094142,
10.922522557656));
#33134=CARTESIAN_POINT('Ctrl Pts',(-3.1233892413128,0.794772683999511,10.9798638833143));
#33135=CARTESIAN_POINT('Ctrl Pts',(-3.11883736264261,1.06847604194353,11.0524139469481));
#33136=CARTESIAN_POINT('Ctrl Pts',(-3.10659849600036,1.1851427086102,11.0816421288434));
#33137=CARTESIAN_POINT('Ctrl Pts',(-3.08409110232845,1.29999999999843,11.1086942583318));
#33138=CARTESIAN_POINT('Ctrl Pts',(-3.26946335327275,-1.29999999999796,
10.9555117735233));
#33139=CARTESIAN_POINT('Ctrl Pts',(-3.27974548388032,-1.18514270860989,
10.9371274226514));
#33140=CARTESIAN_POINT('Ctrl Pts',(-3.27802365958171,-1.06847604194337,
10.9185409361608));
#33141=CARTESIAN_POINT('Ctrl Pts',(-3.24631436378593,-0.794772683999522,
10.8751354604371));
#33142=CARTESIAN_POINT('Ctrl Pts',(-3.18406152138737,-0.636309800094133,
10.8403999564982));
#33143=CARTESIAN_POINT('Ctrl Pts',(-3.11426089875868,-0.319434907276625,
10.8098749994742));
#33144=CARTESIAN_POINT('Ctrl Pts',(-3.06635782253387,-0.158333333333068,
10.7959322775262));
#33145=CARTESIAN_POINT('Ctrl Pts',(-3.04215113968003,0.15833333333307,10.8164666513532));
#33146=CARTESIAN_POINT('Ctrl Pts',(-3.06511180759166,0.319434907276633,
10.8515967284603));
#33147=CARTESIAN_POINT('Ctrl Pts',(-3.08710377997276,0.636309800094143,
10.9226186504884));
#33148=CARTESIAN_POINT('Ctrl Pts',(-3.12363884507739,0.794772683999512,
10.9799565735776));
#33149=CARTESIAN_POINT('Ctrl Pts',(-3.11905284184813,1.06847604194353,11.052495096842));
#33150=CARTESIAN_POINT('Ctrl Pts',(-3.10678938233382,1.1851427086102,11.0817167861432));
#33151=CARTESIAN_POINT('Ctrl Pts',(-3.08424757417498,1.29999999999843,11.1087609258417));
#33152=CARTESIAN_POINT('Ctrl Pts',(-3.26955712717019,-1.29999999999795,
10.9555437816027));
#33153=CARTESIAN_POINT('Ctrl Pts',(-3.27985727277926,-1.18514270860989,
10.9371658112677));
#33154=CARTESIAN_POINT('Ctrl Pts',(-3.2781485829776,-1.06847604194337,10.9185840677267));
#33155=CARTESIAN_POINT('Ctrl Pts',(-3.24645835555544,-0.794772683999521,
10.875185766011));
#33156=CARTESIAN_POINT('Ctrl Pts',(-3.18420292236256,-0.636309800094132,
10.8404482870144));
#33157=CARTESIAN_POINT('Ctrl Pts',(-3.11440050346004,-0.319434907276625,
10.8099266281638));
#33158=CARTESIAN_POINT('Ctrl Pts',(-3.0664870875896,-0.158333333333067,
10.7959873145624));
#33159=CARTESIAN_POINT('Ctrl Pts',(-3.04227885824284,0.15833333333307,10.8165237003086));
#33160=CARTESIAN_POINT('Ctrl Pts',(-3.06524709039278,0.319434907276633,
10.8516538385203));
#33161=CARTESIAN_POINT('Ctrl Pts',(-3.08724021216317,0.636309800094142,
10.922673591622));
#33162=CARTESIAN_POINT('Ctrl Pts',(-3.12378140786306,0.794772683999511,
10.980009621591));
#33163=CARTESIAN_POINT('Ctrl Pts',(-3.11917592303689,1.06847604194353,11.052541528731));
#33164=CARTESIAN_POINT('Ctrl Pts',(-3.10689843573048,1.1851427086102,11.0817594789404));
#33165=CARTESIAN_POINT('Ctrl Pts',(-3.08433700484887,1.29999999999843,11.1087990043302));
#33166=CARTESIAN_POINT('Ctrl Pts',(-3.27860149639123,-1.29999999999811,
10.9586383734117));
#33167=CARTESIAN_POINT('Ctrl Pts',(-3.29063514544287,-1.18514270861003,
10.9408820776598));
#33168=CARTESIAN_POINT('Ctrl Pts',(-3.29019168489462,-1.0684760419435,10.9227606023519));
#33169=CARTESIAN_POINT('Ctrl Pts',(-3.26034258310117,-0.794772683999615,
10.8800527313739));
#33170=CARTESIAN_POINT('Ctrl Pts',(-3.19785238484134,-0.636309800094207,
10.8451050522886));
#33171=CARTESIAN_POINT('Ctrl Pts',(-3.12787622340848,-0.319434907276662,
10.8149018513781));
#33172=CARTESIAN_POINT('Ctrl Pts',(-3.07894950238631,-0.158333333333086,
10.8013109843307));
#33173=CARTESIAN_POINT('Ctrl Pts',(-3.0545921000759,0.158333333333088,10.8220415825818));
#33174=CARTESIAN_POINT('Ctrl Pts',(-3.07830078447487,0.319434907276671,
10.8571643390185));
#33175=CARTESIAN_POINT('Ctrl Pts',(-3.10041572132,0.636309800094218,10.9279621035605));
#33176=CARTESIAN_POINT('Ctrl Pts',(-3.1375622532135,0.794772683999603,10.9851003389286));
#33177=CARTESIAN_POINT('Ctrl Pts',(-3.13107245976098,1.06847604194366,11.0569991517836));
#33178=CARTESIAN_POINT('Ctrl Pts',(-3.11743471538953,1.18514270861034,11.0858639693406));
#33179=CARTESIAN_POINT('Ctrl Pts',(-3.0929684177617,1.29999999999859,11.1124712724833));
#33180=CARTESIAN_POINT('Ctrl Pts',(-3.29087914694721,-1.29999999999912,
10.9624030458906));
#33181=CARTESIAN_POINT('Ctrl Pts',(-3.30552730370085,-1.18514270861095,
10.945066268376));
#33182=CARTESIAN_POINT('Ctrl Pts',(-3.3069203004573,-1.06847604194433,10.9273522227033));
#33183=CARTESIAN_POINT('Ctrl Pts',(-3.27951633035355,-0.794772684000236,
10.8855576685992));
#33184=CARTESIAN_POINT('Ctrl Pts',(-3.21585242742383,-0.636309800094705,
10.8514266221781));
#33185=CARTESIAN_POINT('Ctrl Pts',(-3.14575898006573,-0.319434907276912,
10.8215319562725));
#33186=CARTESIAN_POINT('Ctrl Pts',(-3.09649779902851,-0.15833333333321,
10.8071774067706));
#33187=CARTESIAN_POINT('Ctrl Pts',(-3.07196064508898,0.158333333333212,
10.8281430733825));
#33188=CARTESIAN_POINT('Ctrl Pts',(-3.09589251350698,0.319434907276919,
10.8641713452021));
#33189=CARTESIAN_POINT('Ctrl Pts',(-3.11761911521719,0.636309800094713,
10.935329305927));
#33190=CARTESIAN_POINT('Ctrl Pts',(-3.15506335099256,0.794772684000226,
10.9927733519278));
#33191=CARTESIAN_POINT('Ctrl Pts',(-3.14637586894705,1.06847604194449,11.0635105079469));
#33192=CARTESIAN_POINT('Ctrl Pts',(-3.1312833583335,1.18514270861127,11.0915216415227));
#33193=CARTESIAN_POINT('Ctrl Pts',(-3.10485882618096,1.2999999999996,11.1169244149035));
#33194=CARTESIAN_POINT('Ctrl Pts',(-3.30924538286601,-1.2999999999992,10.9680453426394));
#33195=CARTESIAN_POINT('Ctrl Pts',(-3.32757099145425,-1.18514270861102,
10.9516278490388));
#33196=CARTESIAN_POINT('Ctrl Pts',(-3.33159804337833,-1.06847604194439,
10.9346635406921));
#33197=CARTESIAN_POINT('Ctrl Pts',(-3.30786881262129,-0.794772684000279,
10.8942093432592));
#33198=CARTESIAN_POINT('Ctrl Pts',(-3.24331509553749,-0.63630980009474,
10.8602193379614));
#33199=CARTESIAN_POINT('Ctrl Pts',(-3.17260211198495,-0.31943490727693,
10.8313189415465));
#33200=CARTESIAN_POINT('Ctrl Pts',(-3.1212001718748,-0.158333333333219,
10.8178261868591));
#33201=CARTESIAN_POINT('Ctrl Pts',(-3.09633320761107,0.158333333333221,
10.8392273848434));
#33202=CARTESIAN_POINT('Ctrl Pts',(-3.1220499431571,0.319434907276938,10.8748551818682));
#33203=CARTESIAN_POINT('Ctrl Pts',(-3.14377740756195,0.63630980009475,10.9458534895315));
#33204=CARTESIAN_POINT('Ctrl Pts',(-3.18158047197996,0.79477268400027,11.0038982027768));
#33205=CARTESIAN_POINT('Ctrl Pts',(-3.16919220103572,1.06847604194455,11.0733388251436));
#33206=CARTESIAN_POINT('Ctrl Pts',(-3.15161288425918,1.18514270861134,11.100402316501));
#33207=CARTESIAN_POINT('Ctrl Pts',(-3.12181667416719,1.29999999999968,11.1244710268218));
#33208=CARTESIAN_POINT('Ctrl Pts',(-3.3243274772242,-1.29999999999955,10.9730006918154));
#33209=CARTESIAN_POINT('Ctrl Pts',(-3.34588851006542,-1.18514270861134,
10.9571288525117));
#33210=CARTESIAN_POINT('Ctrl Pts',(-3.35220225995525,-1.06847604194468,
10.9406718024574));
#33211=CARTESIAN_POINT('Ctrl Pts',(-3.33156401143583,-0.794772684000493,
10.9013007707052));
#33212=CARTESIAN_POINT('Ctrl Pts',(-3.26575478710962,-0.636309800094912,
10.868086218826));
#33213=CARTESIAN_POINT('Ctrl Pts',(-3.19479764779382,-0.319434907277016,
10.8396875638873));
#33214=CARTESIAN_POINT('Ctrl Pts',(-3.14252835935329,-0.158333333333261,
10.825779426311));
#33215=CARTESIAN_POINT('Ctrl Pts',(-3.11752885059753,0.158333333333263,
10.8473618163122));
#33216=CARTESIAN_POINT('Ctrl Pts',(-3.14392467480981,0.319434907277023,
10.8836346317217));
#33217=CARTESIAN_POINT('Ctrl Pts',(-3.16573979918509,0.636309800094921,
10.9544015971221));
#33218=CARTESIAN_POINT('Ctrl Pts',(-3.20491078620108,0.794772684000484,
11.0116782649417));
#33219=CARTESIAN_POINT('Ctrl Pts',(-3.18926926156555,1.06847604194484,11.0802325544955));
#33220=CARTESIAN_POINT('Ctrl Pts',(-3.16929090560949,1.18514270861166,11.106889174787));
#33221=CARTESIAN_POINT('Ctrl Pts',(-3.13610483013649,1.30000000000003,11.1305278036089));
#33222=CARTESIAN_POINT('Ctrl Pts',(-3.33687491329961,-1.30000000000013,
10.9763612687376));
#33223=CARTESIAN_POINT('Ctrl Pts',(-3.36075240801907,-1.18514270861187,
10.9612527084206));
#33224=CARTESIAN_POINT('Ctrl Pts',(-3.36875682745956,-1.06847604194516,
10.9453628297242));
#33225=CARTESIAN_POINT('Ctrl Pts',(-3.35057865835347,-0.794772684000851,
10.9068490294177));
#33226=CARTESIAN_POINT('Ctrl Pts',(-3.28443962791702,-0.636309800095197,
10.873385773417));
#33227=CARTESIAN_POINT('Ctrl Pts',(-3.21328105992889,-0.319434907277159,
10.8454018207699));
#33228=CARTESIAN_POINT('Ctrl Pts',(-3.15982488509512,-0.158333333333332,
10.8318180571383));
#33229=CARTESIAN_POINT('Ctrl Pts',(-3.13444040097792,0.158333333333334,
10.8539097309621));
#33230=CARTESIAN_POINT('Ctrl Pts',(-3.16145464955745,0.319434907277167,
10.8905991594872));
#33231=CARTESIAN_POINT('Ctrl Pts',(-3.18306078463709,0.636309800095206,
10.9615168342609));
#33232=CARTESIAN_POINT('Ctrl Pts',(-3.22263648930952,0.79477268400084,11.0189791881958));
#33233=CARTESIAN_POINT('Ctrl Pts',(-3.20470961432298,1.06847604194532,11.0864845545939));
#33234=CARTESIAN_POINT('Ctrl Pts',(-3.18318073063071,1.18514270861219,11.1124051525384));
#33235=CARTESIAN_POINT('Ctrl Pts',(-3.14788284317166,1.30000000000061,11.1350257766339));
#33236=CARTESIAN_POINT('Ctrl Pts',(-3.34312043552664,-1.30000000000013,
10.9780717341714));
#33237=CARTESIAN_POINT('Ctrl Pts',(-3.36817625250943,-1.18514270861187,
10.9633184123726));
#33238=CARTESIAN_POINT('Ctrl Pts',(-3.3770361693725,-1.06847604194516,10.9476988830842));
#33239=CARTESIAN_POINT('Ctrl Pts',(-3.36008858049118,-0.794772684000851,
10.9096135331669));
#33240=CARTESIAN_POINT('Ctrl Pts',(-3.29374448453208,-0.636309800095197,
10.876080714948));
#33241=CARTESIAN_POINT('Ctrl Pts',(-3.22246485929502,-0.319434907277159,
10.8483292952626));
#33242=CARTESIAN_POINT('Ctrl Pts',(-3.16838675811195,-0.158333333333332,
10.8349383562734));
#33243=CARTESIAN_POINT('Ctrl Pts',(-3.14286241424647,0.158333333333334,
10.8572187973924));
#33244=CARTESIAN_POINT('Ctrl Pts',(-3.17031238807969,0.319434907277167,
10.8939627249896));
#33245=CARTESIAN_POINT('Ctrl Pts',(-3.19184909015918,0.636309800095206,
10.9649130969802));
#33246=CARTESIAN_POINT('Ctrl Pts',(-3.23156943363573,0.79477268400084,11.0225410569458));
#33247=CARTESIAN_POINT('Ctrl Pts',(-3.21244012754108,1.06847604194532,11.0895917213652));
#33248=CARTESIAN_POINT('Ctrl Pts',(-3.19010469464416,1.18514270861219,11.1151799568387));
#33249=CARTESIAN_POINT('Ctrl Pts',(-3.15371419664804,1.30000000000061,11.1373326796307));
#33250=CARTESIAN_POINT('',(-3.07975929592511,1.2,11.0752525955301));
#33251=CARTESIAN_POINT('Ctrl Pts',(-3.07975929592511,1.2,11.0752525955301));
#33252=CARTESIAN_POINT('Ctrl Pts',(-3.05872636744548,1.21680769549872,11.0704989090906));
#33253=CARTESIAN_POINT('Ctrl Pts',(-3.03710141769083,1.23314403937139,11.0667390106653));
#33254=CARTESIAN_POINT('Ctrl Pts',(-2.99520540299999,1.26665353031124,11.0569415951956));
#33255=CARTESIAN_POINT('Ctrl Pts',(-2.97413477718184,1.28321842329864,11.0523060114257));
#33256=CARTESIAN_POINT('Ctrl Pts',(-2.95338171769412,1.29999999999958,11.0470815470424));
#33257=CARTESIAN_POINT('',(-3.2008348383287,0.653834841336403,10.9758649786952));
#33258=CARTESIAN_POINT('Ctrl Pts',(-3.20083483831068,0.653834841321624,
10.975864978764));
#33259=CARTESIAN_POINT('Ctrl Pts',(-3.18812833935079,0.719511596407524,
10.9866363926712));
#33260=CARTESIAN_POINT('Ctrl Pts',(-3.17771111571533,0.767412490766721,
10.9953791471888));
#33261=CARTESIAN_POINT('Ctrl Pts',(-3.13847134847367,0.94981031949708,11.0280199746604));
#33262=CARTESIAN_POINT('Ctrl Pts',(-3.11682163850512,1.04818118464467,11.0457982331948));
#33263=CARTESIAN_POINT('Ctrl Pts',(-3.07975929592511,1.2,11.0752525955301));
#33264=CARTESIAN_POINT('',(-3.3059688760626,-0.653834841531101,10.8841647344419));
#33265=CARTESIAN_POINT('Ctrl Pts',(-3.30596887606259,-0.653834841531102,
10.8841647344419));
#33266=CARTESIAN_POINT('Ctrl Pts',(-3.26765010478892,-0.575768210610585,
10.8677496595377));
#33267=CARTESIAN_POINT('Ctrl Pts',(-3.23494824939066,-0.493706163102552,
10.8548265221935));
#33268=CARTESIAN_POINT('Ctrl Pts',(-3.18709017845533,-0.337903894569622,
10.8381694530451));
#33269=CARTESIAN_POINT('Ctrl Pts',(-3.16979179495297,-0.2654146213422,10.8335054310253));
#33270=CARTESIAN_POINT('Ctrl Pts',(-3.14556133124211,-0.129502257227768,
10.831330995582));
#33271=CARTESIAN_POINT('Ctrl Pts',(-3.13750239985805,-0.0665294992617646,
10.8328438160244));
#33272=CARTESIAN_POINT('Ctrl Pts',(-3.12727067311581,0.0594283132875214,
10.8412732840013));
#33273=CARTESIAN_POINT('Ctrl Pts',(-3.1250264806205,0.122541336619068,10.8482282183473));
#33274=CARTESIAN_POINT('Ctrl Pts',(-3.12729278947957,0.25988248099301,10.8687757330099));
#33275=CARTESIAN_POINT('Ctrl Pts',(-3.13313315594363,0.333772875107173,
10.8833608794714));
#33276=CARTESIAN_POINT('Ctrl Pts',(-3.15645864391337,0.491496380642283,
10.9217822007945));
#33277=CARTESIAN_POINT('Ctrl Pts',(-3.17560601109368,0.57490233849731,10.9471353939645));
#33278=CARTESIAN_POINT('Ctrl Pts',(-3.20083483821487,0.653834841358134,
10.9758649787354));
#33279=CARTESIAN_POINT('',(-3.25181112747254,-1.2,10.9320536426002));
#33280=CARTESIAN_POINT('Ctrl Pts',(-3.25181112747254,-1.2,10.9320536426002));
#33281=CARTESIAN_POINT('Ctrl Pts',(-3.26281768457294,-1.12280248951958,
10.9224634147306));
#33282=CARTESIAN_POINT('Ctrl Pts',(-3.27215610527124,-1.0521071107758,10.9142855469299));
#33283=CARTESIAN_POINT('Ctrl Pts',(-3.30019612230759,-0.767168051992084,
10.8893756587268));
#33284=CARTESIAN_POINT('Ctrl Pts',(-3.30337667056459,-0.700407703040203,
10.8864908385427));
#33285=CARTESIAN_POINT('Ctrl Pts',(-3.30596887606259,-0.6538348415311,10.8841647344419));
#33286=CARTESIAN_POINT('Ctrl Pts',(-3.12979327626223,-1.2999999999991,10.904982327606));
#33287=CARTESIAN_POINT('Ctrl Pts',(-3.15020519847771,-1.28299035195331,
10.9100057513286));
#33288=CARTESIAN_POINT('Ctrl Pts',(-3.15975174726777,-1.27543828608662,
10.9118308894838));
#33289=CARTESIAN_POINT('Ctrl Pts',(-3.20107070619102,-1.24116690344093,
10.9215350399886));
#33290=CARTESIAN_POINT('Ctrl Pts',(-3.21071565722415,-1.23311873582876,
10.9238506811936));
#33291=CARTESIAN_POINT('Ctrl Pts',(-3.22591635566606,-1.22085268075416,
10.9269247721703));
#33292=CARTESIAN_POINT('Ctrl Pts',(-3.22669721991101,-1.22026908223654,
10.9270235897164));
#33293=CARTESIAN_POINT('Ctrl Pts',(-3.23909005932958,-1.210183748322,10.929622486052));
#33294=CARTESIAN_POINT('Ctrl Pts',(-3.24523385162528,-1.205183253303,10.9309097562926));
#33295=CARTESIAN_POINT('Ctrl Pts',(-3.25181112747254,-1.2,10.9320536426002));
#33296=CARTESIAN_POINT('Origin',(0.,1.25,7.2));
#33297=CARTESIAN_POINT('Origin',(0.,1.2,7.2));
#33298=CARTESIAN_POINT('Origin',(0.,0.92691742076555,7.2));
#33299=CARTESIAN_POINT('Origin',(0.,0.653834841531101,7.2));
#33300=CARTESIAN_POINT('Origin',(0.,0.,7.2));
#33301=CARTESIAN_POINT('Origin',(0.,-0.653834841531101,7.2));
#33302=CARTESIAN_POINT('Origin',(0.,-0.926917420765551,7.2));
#33303=CARTESIAN_POINT('Origin',(0.,-1.2,7.2));
#33304=CARTESIAN_POINT('Origin',(0.,-1.25,7.2));
#33305=CARTESIAN_POINT('Ctrl Pts',(-3.58611066068418,-1.30000000000019,
10.7480011546782));
#33306=CARTESIAN_POINT('Ctrl Pts',(-3.56027544999381,-1.18514270861191,
10.781876711649));
#33307=CARTESIAN_POINT('Ctrl Pts',(-3.53249270107504,-1.06847604194518,
10.8014150897762));
#33308=CARTESIAN_POINT('Ctrl Pts',(-3.46380979024152,-0.794772684000851,
10.8134309006175));
#33309=CARTESIAN_POINT('Ctrl Pts',(-3.41064942873151,-0.636309800095197,
10.7679043872394));
#33310=CARTESIAN_POINT('Ctrl Pts',(-3.34233892867367,-0.319434907277159,
10.7390693321139));
#33311=CARTESIAN_POINT('Ctrl Pts',(-3.30866559173879,-0.158333333333333,
10.7079289458242));
#33312=CARTESIAN_POINT('Ctrl Pts',(-3.2838391847674,0.158333333333334,10.7309845243923));
#33313=CARTESIAN_POINT('Ctrl Pts',(-3.29150406597897,0.319434907277167,
10.7861661143534));
#33314=CARTESIAN_POINT('Ctrl Pts',(-3.31165271079404,0.636309800095206,
10.8599560755972));
#33315=CARTESIAN_POINT('Ctrl Pts',(-3.33806698632524,0.79477268400084,10.929441865611));
#33316=CARTESIAN_POINT('Ctrl Pts',(-3.37417219528941,1.06847604194587,10.9502776169276));
#33317=CARTESIAN_POINT('Ctrl Pts',(-3.39063227265752,1.18514270861327,10.9430989210106));
#33318=CARTESIAN_POINT('Ctrl Pts',(-3.40792382026295,1.30000000000221,10.9197225044723));
#33319=CARTESIAN_POINT('Ctrl Pts',(-3.58274121447438,-1.30000000000018,
10.7359200632382));
#33320=CARTESIAN_POINT('Ctrl Pts',(-3.55620374541987,-1.18514270861191,
10.767524552013));
#33321=CARTESIAN_POINT('Ctrl Pts',(-3.52792852769938,-1.06847604194518,
10.7853891857851));
#33322=CARTESIAN_POINT('Ctrl Pts',(-3.45859257127325,-0.794772684000847,
10.7949182499019));
#33323=CARTESIAN_POINT('Ctrl Pts',(-3.40573136963309,-0.636309800095194,
10.7497140504956));
#33324=CARTESIAN_POINT('Ctrl Pts',(-3.3375004212098,-0.319434907277158,
10.7207477256613));
#33325=CARTESIAN_POINT('Ctrl Pts',(-3.30384439394133,-0.158333333333332,
10.690485409397));
#33326=CARTESIAN_POINT('Ctrl Pts',(-3.27942269203529,0.158333333333333,
10.7133022639117));
#33327=CARTESIAN_POINT('Ctrl Pts',(-3.28760112792004,0.319434907277165,
10.7672871264616));
#33328=CARTESIAN_POINT('Ctrl Pts',(-3.30823759882109,0.636309800095203,
10.840884912149));
#33329=CARTESIAN_POINT('Ctrl Pts',(-3.33455638238823,0.794772684000836,
10.9099482753614));
#33330=CARTESIAN_POINT('Ctrl Pts',(-3.37125653661945,1.06847604194586,10.9333212751551));
#33331=CARTESIAN_POINT('Ctrl Pts',(-3.38807550314534,1.18514270861327,10.9279007194989));
#33332=CARTESIAN_POINT('Ctrl Pts',(-3.40582729930512,1.3000000000022,10.9069423026308));
#33333=CARTESIAN_POINT('Ctrl Pts',(-3.57558296861516,-1.30000000000236,
10.7121202278766));
#33334=CARTESIAN_POINT('Ctrl Pts',(-3.54899722098252,-1.18514270861389,
10.7382144502947));
#33335=CARTESIAN_POINT('Ctrl Pts',(-3.52050276185225,-1.06847604194697,
10.7521771288085));
#33336=CARTESIAN_POINT('Ctrl Pts',(-3.45026535556835,-0.794772684002182,
10.7564074160735));
#33337=CARTESIAN_POINT('Ctrl Pts',(-3.39573104119172,-0.636309800096262,
10.7133992517982));
#33338=CARTESIAN_POINT('Ctrl Pts',(-3.3270486465882,-0.319434907277695,
10.6845828030105));
#33339=CARTESIAN_POINT('Ctrl Pts',(-3.29427438855773,-0.158333333333598,
10.6555281147055));
#33340=CARTESIAN_POINT('Ctrl Pts',(-3.27041076489765,0.1583333333336,10.6780128576633));
#33341=CARTESIAN_POINT('Ctrl Pts',(-3.27864253380086,0.319434907277705,
10.7301959709333));
#33342=CARTESIAN_POINT('Ctrl Pts',(-3.30009924532343,0.636309800096275,
10.8035010882691));
#33343=CARTESIAN_POINT('Ctrl Pts',(-3.32709168674241,0.794772684002175,
10.8711791666546));
#33344=CARTESIAN_POINT('Ctrl Pts',(-3.36497326618527,1.06847604194766,10.8996552636671));
#33345=CARTESIAN_POINT('Ctrl Pts',(-3.38235194885042,1.18514270861525,10.8978655456807));
#33346=CARTESIAN_POINT('Ctrl Pts',(-3.40071178209068,1.30000000000438,10.8819598624545));
#33347=CARTESIAN_POINT('Ctrl Pts',(-3.56846700829314,-1.30000000000448,
10.6880753023113));
#33348=CARTESIAN_POINT('Ctrl Pts',(-3.5396465007391,-1.18514270861582,10.7101749123656));
#33349=CARTESIAN_POINT('Ctrl Pts',(-3.50966832071176,-1.06847604194871,
10.7211153748007));
#33350=CARTESIAN_POINT('Ctrl Pts',(-3.43773827272932,-0.794772684003476,
10.7206101682778));
#33351=CARTESIAN_POINT('Ctrl Pts',(-3.38488511663496,-0.636309800097297,
10.6775025502549));
#33352=CARTESIAN_POINT('Ctrl Pts',(-3.31672657946322,-0.319434907278215,
10.6481671548942));
#33353=CARTESIAN_POINT('Ctrl Pts',(-3.28399515052784,-0.158333333333855,
10.6208824265012));
#33354=CARTESIAN_POINT('Ctrl Pts',(-3.26072518366511,0.158333333333857,
10.6430059624589));
#33355=CARTESIAN_POINT('Ctrl Pts',(-3.26924648437681,0.319434907278222,
10.6932227713766));
#33356=CARTESIAN_POINT('Ctrl Pts',(-3.29192081554073,0.636309800097307,
10.7659752694701));
#33357=CARTESIAN_POINT('Ctrl Pts',(-3.32006229542947,0.794772684003464,
10.8319547752052));
#33358=CARTESIAN_POINT('Ctrl Pts',(-3.35925865987659,1.06847604194939,10.8654753627169));
#33359=CARTESIAN_POINT('Ctrl Pts',(-3.37715256797164,1.18514270861719,10.8673647356509));
#33360=CARTESIAN_POINT('Ctrl Pts',(-3.39597373036095,1.3000000000065,10.8566336612452));
#33361=CARTESIAN_POINT('Ctrl Pts',(-3.56482293374636,-1.30000000000484,
10.6760625013374));
#33362=CARTESIAN_POINT('Ctrl Pts',(-3.53566894486391,-1.18514270861616,
10.6955880507016));
#33363=CARTESIAN_POINT('Ctrl Pts',(-3.5053946453138,-1.06847604194901,10.7046832736887));
#33364=CARTESIAN_POINT('Ctrl Pts',(-3.43286681524052,-0.794772684003699,
10.7015989177713));
#33365=CARTESIAN_POINT('Ctrl Pts',(-3.3796708582827,-0.636309800097476,
10.6592633358045));
#33366=CARTESIAN_POINT('Ctrl Pts',(-3.31123172933568,-0.319434907278304,
10.6300376279778));
#33367=CARTESIAN_POINT('Ctrl Pts',(-3.27845132813535,-0.1583333333339,10.6036939265839));
#33368=CARTESIAN_POINT('Ctrl Pts',(-3.25546516233841,0.158333333333902,
10.6256432851867));
#33369=CARTESIAN_POINT('Ctrl Pts',(-3.26453005067804,0.319434907278311,
10.6746022809027));
#33370=CARTESIAN_POINT('Ctrl Pts',(-3.28763364240969,0.636309800097486,
10.7471807886859));
#33371=CARTESIAN_POINT('Ctrl Pts',(-3.31555303628374,0.794772684003689,
10.8128030858203));
#33372=CARTESIAN_POINT('Ctrl Pts',(-3.35541107546838,1.0684760419497,10.8488670492249));
#33373=CARTESIAN_POINT('Ctrl Pts',(-3.37373782596862,1.18514270861752,10.8525041026793));
#33374=CARTESIAN_POINT('Ctrl Pts',(-3.39313825869191,1.30000000000687,10.8441674561317));
#33375=CARTESIAN_POINT('Ctrl Pts',(-3.5647656098383,-1.30000000000484,10.6758768710106));
#33376=CARTESIAN_POINT('Ctrl Pts',(-3.53560670555812,-1.18514270861615,
10.6953623028687));
#33377=CARTESIAN_POINT('Ctrl Pts',(-3.50532801058858,-1.06847604194901,
10.704428759195));
#33378=CARTESIAN_POINT('Ctrl Pts',(-3.43279122747106,-0.794772684003698,
10.7013041692597));
#33379=CARTESIAN_POINT('Ctrl Pts',(-3.37959022019577,-0.636309800097475,
10.658980400634));
#33380=CARTESIAN_POINT('Ctrl Pts',(-3.31114632355007,-0.319434907278303,
10.6297566683138));
#33381=CARTESIAN_POINT('Ctrl Pts',(-3.27836400035346,-0.158333333333899,
10.6034283295616));
#33382=CARTESIAN_POINT('Ctrl Pts',(-3.25538212571374,0.158333333333901,
10.6253750534706));
#33383=CARTESIAN_POINT('Ctrl Pts',(-3.26445637979772,0.319434907278311,
10.6743139130905));
#33384=CARTESIAN_POINT('Ctrl Pts',(-3.28756705840575,0.636309800097484,
10.7468894351868));
#33385=CARTESIAN_POINT('Ctrl Pts',(-3.315482936733,0.794772684003688,10.8125062482728));
#33386=CARTESIAN_POINT('Ctrl Pts',(-3.35535126532992,1.06847604194969,10.8486096365886));
#33387=CARTESIAN_POINT('Ctrl Pts',(-3.37368471811786,1.18514270861751,10.8522737991005));
#33388=CARTESIAN_POINT('Ctrl Pts',(-3.39309410151123,1.30000000000686,10.8439743050846));
#33389=CARTESIAN_POINT('Ctrl Pts',(-3.56466570358193,-1.30000000000484,
10.6755517052646));
#33390=CARTESIAN_POINT('Ctrl Pts',(-3.53549792772271,-1.18514270861615,
10.6949671392659));
#33391=CARTESIAN_POINT('Ctrl Pts',(-3.50521135057255,-1.06847604194901,
10.7039833998441));
#33392=CARTESIAN_POINT('Ctrl Pts',(-3.43265864374919,-0.794772684003698,
10.7007885945215));
#33393=CARTESIAN_POINT('Ctrl Pts',(-3.37944873025216,-0.636309800097476,
10.6584855261697));
#33394=CARTESIAN_POINT('Ctrl Pts',(-3.31099685750756,-0.319434907278303,
10.6292650047689));
#33395=CARTESIAN_POINT('Ctrl Pts',(-3.27821203825765,-0.1583333333339,10.6029629733926));
#33396=CARTESIAN_POINT('Ctrl Pts',(-3.25523775215173,0.158333333333901,
10.624905036394));
#33397=CARTESIAN_POINT('Ctrl Pts',(-3.26432762546627,0.319434907278311,
10.6738091758094));
#33398=CARTESIAN_POINT('Ctrl Pts',(-3.28745046379999,0.636309800097485,
10.746379635446));
#33399=CARTESIAN_POINT('Ctrl Pts',(-3.31536045548722,0.794772684003688,
10.8119866746284));
#33400=CARTESIAN_POINT('Ctrl Pts',(-3.35524682273211,1.06847604194969,10.8481590280866));
#33401=CARTESIAN_POINT('Ctrl Pts',(-3.37359199792297,1.18514270861752,10.8518706311386));
#33402=CARTESIAN_POINT('Ctrl Pts',(-3.39301701785986,1.30000000000686,10.8436361657485));
#33403=CARTESIAN_POINT('Ctrl Pts',(-3.56452220822542,-1.30000000000484,
10.6750877402548));
#33404=CARTESIAN_POINT('Ctrl Pts',(-3.53534166513088,-1.18514270861615,
10.6944032219802));
#33405=CARTESIAN_POINT('Ctrl Pts',(-3.50504379632556,-1.06847604194901,
10.7033477814798));
#33406=CARTESIAN_POINT('Ctrl Pts',(-3.43246841240526,-0.794772684003697,
10.7000525982394));
#33407=CARTESIAN_POINT('Ctrl Pts',(-3.3792461880662,-0.636309800097475,
10.6577788260496));
#33408=CARTESIAN_POINT('Ctrl Pts',(-3.31078289800484,-0.319434907278303,
10.6285628970504));
#33409=CARTESIAN_POINT('Ctrl Pts',(-3.27799407242096,-0.158333333333899,
10.6022987392734));
#33410=CARTESIAN_POINT('Ctrl Pts',(-3.2550305779373,0.158333333333901,10.6242341681237));
#33411=CARTESIAN_POINT('Ctrl Pts',(-3.26414294810058,0.319434907278311,
10.673088573858));
#33412=CARTESIAN_POINT('Ctrl Pts',(-3.28728350341888,0.636309800097484,
10.7456515726491));
#33413=CARTESIAN_POINT('Ctrl Pts',(-3.31518555604749,0.794772684003687,
10.811244349333));
#33414=CARTESIAN_POINT('Ctrl Pts',(-3.35509782672543,1.06847604194969,10.8475151463616));
#33415=CARTESIAN_POINT('Ctrl Pts',(-3.37345971013758,1.18514270861751,10.8512945514547));
#33416=CARTESIAN_POINT('Ctrl Pts',(-3.3929069338807,1.30000000000686,10.8431530775728));
#33417=CARTESIAN_POINT('Ctrl Pts',(-3.564349417289,-1.30000000000484,10.674531392229));
#33418=CARTESIAN_POINT('Ctrl Pts',(-3.53515306526229,-1.18514270861615,
10.6937272657619));
#33419=CARTESIAN_POINT('Ctrl Pts',(-3.50484135793382,-1.06847604194901,
10.7025859799768));
#33420=CARTESIAN_POINT('Ctrl Pts',(-3.43223855629568,-0.794772684003697,
10.6991704760268));
#33421=CARTESIAN_POINT('Ctrl Pts',(-3.37900212853287,-0.636309800097474,
10.656931455314));
#33422=CARTESIAN_POINT('Ctrl Pts',(-3.31052558194566,-0.319434907278303,
10.6277207251215));
#33423=CARTESIAN_POINT('Ctrl Pts',(-3.27773238178739,-0.158333333333899,
10.6015017257394));
#33424=CARTESIAN_POINT('Ctrl Pts',(-3.2547818419222,0.158333333333901,10.6234291808475));
#33425=CARTESIAN_POINT('Ctrl Pts',(-3.26392046214312,0.31943490727831,10.6722243902951));
#33426=CARTESIAN_POINT('Ctrl Pts',(-3.28708249045311,0.636309800097484,
10.7447783005775));
#33427=CARTESIAN_POINT('Ctrl Pts',(-3.31497613290306,0.794772684003687,
10.8103532451295));
#33428=CARTESIAN_POINT('Ctrl Pts',(-3.35491970635418,1.06847604194969,10.8467420377067));
#33429=CARTESIAN_POINT('Ctrl Pts',(-3.37330154458274,1.18514270861751,10.8506028685909));
#33430=CARTESIAN_POINT('Ctrl Pts',(-3.39277512814806,1.30000000000686,10.8425731703904));
#33431=CARTESIAN_POINT('Ctrl Pts',(-3.5640021797759,-1.30000000000484,10.6734198538772));
#33432=CARTESIAN_POINT('Ctrl Pts',(-3.53477320726961,-1.18514270861615,
10.6923771850188));
#33433=CARTESIAN_POINT('Ctrl Pts',(-3.50443325568522,-1.068476041949,10.7010645848694));
#33434=CARTESIAN_POINT('Ctrl Pts',(-3.43177531411776,-0.794772684003695,
10.6974086206578));
#33435=CARTESIAN_POINT('Ctrl Pts',(-3.37851196008848,-0.636309800097473,
10.6552380707824));
#33436=CARTESIAN_POINT('Ctrl Pts',(-3.31000971826934,-0.319434907278302,
10.6260371567929));
#33437=CARTESIAN_POINT('Ctrl Pts',(-3.27720815839903,-0.158333333333899,
10.599908210249));
#33438=CARTESIAN_POINT('Ctrl Pts',(-3.25428347088739,0.158333333333901,
10.6218197316737));
#33439=CARTESIAN_POINT('Ctrl Pts',(-3.26347335217478,0.31943490727831,10.6704973405271));
#33440=CARTESIAN_POINT('Ctrl Pts',(-3.28667900751217,0.636309800097482,
10.7430326358703));
#33441=CARTESIAN_POINT('Ctrl Pts',(-3.31455833413199,0.794772684003684,
10.8085703159024));
#33442=CARTESIAN_POINT('Ctrl Pts',(-3.35456499042273,1.06847604194969,10.8451948052891));
#33443=CARTESIAN_POINT('Ctrl Pts',(-3.37298649636271,1.18514270861751,10.8492186495772));
#33444=CARTESIAN_POINT('Ctrl Pts',(-3.39251210912706,1.30000000000686,10.841412953769));
#33445=CARTESIAN_POINT('Ctrl Pts',(-3.56347571232416,-1.30000000000483,
10.6717564062968));
#33446=CARTESIAN_POINT('Ctrl Pts',(-3.53419300891418,-1.18514270861614,
10.6903592176008));
#33447=CARTESIAN_POINT('Ctrl Pts',(-3.50380790798684,-1.06847604194899,
10.6987915422063));
#33448=CARTESIAN_POINT('Ctrl Pts',(-3.43106548752715,-0.794772684003688,
10.6947760400535));
#33449=CARTESIAN_POINT('Ctrl Pts',(-3.37776796299676,-0.636309800097467,
10.652703824103));
#33450=CARTESIAN_POINT('Ctrl Pts',(-3.30923142734901,-0.319434907278299,
10.6235146541448));
#33451=CARTESIAN_POINT('Ctrl Pts',(-3.2764207460507,-0.158333333333898,
10.5975184936668));
#33452=CARTESIAN_POINT('Ctrl Pts',(-3.25353469006426,0.158333333333899,
10.6194061215614));
#33453=CARTESIAN_POINT('Ctrl Pts',(-3.26279455275997,0.319434907278307,
10.6679118021839));
#33454=CARTESIAN_POINT('Ctrl Pts',(-3.28606791379863,0.636309800097477,
10.7404177444664));
#33455=CARTESIAN_POINT('Ctrl Pts',(-3.31393689224648,0.794772684003677,
10.805892423076));
#33456=CARTESIAN_POINT('Ctrl Pts',(-3.35404007894592,1.06847604194968,10.8428692671772));
#33457=CARTESIAN_POINT('Ctrl Pts',(-3.37251994711931,1.1851427086175,10.8471383750334));
#33458=CARTESIAN_POINT('Ctrl Pts',(-3.39212049991335,1.30000000000685,10.8396706850613));
#33459=CARTESIAN_POINT('Ctrl Pts',(-3.56288008463113,-1.30000000000482,
10.6699153100721));
#33460=CARTESIAN_POINT('Ctrl Pts',(-3.53352504187793,-1.18514270861613,
10.688132976957));
#33461=CARTESIAN_POINT('Ctrl Pts',(-3.50308238913506,-1.06847604194898,
10.6962869902133));
#33462=CARTESIAN_POINT('Ctrl Pts',(-3.43024117461551,-0.794772684003681,
10.6918753389307));
#33463=CARTESIAN_POINT('Ctrl Pts',(-3.37692113363069,-0.636309800097462,
10.6499014916574));
#33464=CARTESIAN_POINT('Ctrl Pts',(-3.30835829639661,-0.319434907278296,
10.6207171664895));
#33465=CARTESIAN_POINT('Ctrl Pts',(-3.27554874317051,-0.158333333333896,
10.5948610178512));
#33466=CARTESIAN_POINT('Ctrl Pts',(-3.25270507405461,0.158333333333898,
10.6167222438594));
#33467=CARTESIAN_POINT('Ctrl Pts',(-3.26202237611515,0.319434907278304,
10.66505008052));
#33468=CARTESIAN_POINT('Ctrl Pts',(-3.28537541909464,0.636309800097471,
10.7375206818382));
#33469=CARTESIAN_POINT('Ctrl Pts',(-3.31326193793976,0.794772684003671,
10.8029068995155));
#33470=CARTESIAN_POINT('Ctrl Pts',(-3.35347649267537,1.06847604194967,10.8402726868186));
#33471=CARTESIAN_POINT('Ctrl Pts',(-3.37201781453021,1.18514270861749,10.8448164903824));
#33472=CARTESIAN_POINT('Ctrl Pts',(-3.39169306759087,1.30000000000684,10.8377298327253));
#33473=CARTESIAN_POINT('Ctrl Pts',(-3.56239728410032,-1.30000000000481,
10.6684465924844));
#33474=CARTESIAN_POINT('Ctrl Pts',(-3.53297521638305,-1.18514270861612,
10.6863625247026));
#33475=CARTESIAN_POINT('Ctrl Pts',(-3.50248113498807,-1.06847604194898,
10.6942976370287));
#33476=CARTESIAN_POINT('Ctrl Pts',(-3.42955714059451,-0.794772684003679,
10.6895716433085));
#33477=CARTESIAN_POINT('Ctrl Pts',(-3.37622978260571,-0.63630980009746,
10.647668936555));
#33478=CARTESIAN_POINT('Ctrl Pts',(-3.30765465018317,-0.319434907278295,
10.6184824351893));
#33479=CARTESIAN_POINT('Ctrl Pts',(-3.27485508668908,-0.158333333333896,
10.5927322349785));
#33480=CARTESIAN_POINT('Ctrl Pts',(-3.25204494547751,0.158333333333897,
10.6145724490381));
#33481=CARTESIAN_POINT('Ctrl Pts',(-3.26139275085378,0.319434907278303,
10.662768043132));
#33482=CARTESIAN_POINT('Ctrl Pts',(-3.28481219545305,0.636309800097469,
10.7352087802632));
#33483=CARTESIAN_POINT('Ctrl Pts',(-3.31273351341567,0.794772684003668,
10.8005110532342));
#33484=CARTESIAN_POINT('Ctrl Pts',(-3.35303990765138,1.06847604194967,10.8381862837691));
#33485=CARTESIAN_POINT('Ctrl Pts',(-3.3716278902605,1.18514270861749,10.842951442016));
#33486=CARTESIAN_POINT('Ctrl Pts',(-3.39135671091313,1.30000000000683,10.8361735472162));
#33487=CARTESIAN_POINT('Ctrl Pts',(-3.56166717131598,-1.3000000000048,10.6662473927834));
#33488=CARTESIAN_POINT('Ctrl Pts',(-3.53213539832158,-1.18514270861612,
10.6837171284086));
#33489=CARTESIAN_POINT('Ctrl Pts',(-3.5015587453786,-1.06847604194897,10.6913276776729));
#33490=CARTESIAN_POINT('Ctrl Pts',(-3.4285066785331,-0.794772684003673,
10.6861328761411));
#33491=CARTESIAN_POINT('Ctrl Pts',(-3.37517873510585,-0.636309800097455,
10.644329539887));
#33492=CARTESIAN_POINT('Ctrl Pts',(-3.30659388175246,-0.319434907278293,
10.6151337471993));
#33493=CARTESIAN_POINT('Ctrl Pts',(-3.27381864911049,-0.158333333333895,
10.5895362325923));
#33494=CARTESIAN_POINT('Ctrl Pts',(-3.25105854279058,0.158333333333896,
10.6113449523485));
#33495=CARTESIAN_POINT('Ctrl Pts',(-3.26043674820715,0.319434907278301,
10.6593521508946));
#33496=CARTESIAN_POINT('Ctrl Pts',(-3.28395826579358,0.636309800097465,
10.7317466146758));
#33497=CARTESIAN_POINT('Ctrl Pts',(-3.31195199728272,0.794772684003663,
10.7969101537614));
#33498=CARTESIAN_POINT('Ctrl Pts',(-3.35239889578995,1.06847604194966,10.8350478260744));
#33499=CARTESIAN_POINT('Ctrl Pts',(-3.37105449282202,1.18514270861748,10.8401465257561));
#33500=CARTESIAN_POINT('Ctrl Pts',(-3.3908577232276,1.30000000000682,10.8338355399152));
#33501=CARTESIAN_POINT('Ctrl Pts',(-3.5605509826163,-1.30000000000476,10.6629622113181));
#33502=CARTESIAN_POINT('Ctrl Pts',(-3.53081837342967,-1.18514270861608,
10.6797880844511));
#33503=CARTESIAN_POINT('Ctrl Pts',(-3.50009634366811,-1.06847604194894,
10.6869268691001));
#33504=CARTESIAN_POINT('Ctrl Pts',(-3.42683654953696,-0.794772684003649,
10.6810397774547));
#33505=CARTESIAN_POINT('Ctrl Pts',(-3.37354839289819,-0.636309800097436,
10.6393567271974));
#33506=CARTESIAN_POINT('Ctrl Pts',(-3.30498358068139,-0.319434907278283,
10.610123118836));
#33507=CARTESIAN_POINT('Ctrl Pts',(-3.27228264912268,-0.15833333333389,
10.5847294420948));
#33508=CARTESIAN_POINT('Ctrl Pts',(-3.24959637980222,0.158333333333892,
10.6064911810025));
#33509=CARTESIAN_POINT('Ctrl Pts',(-3.2589585365903,0.319434907278291,10.6542558381739));
#33510=CARTESIAN_POINT('Ctrl Pts',(-3.28264215828697,0.636309800097445,
10.7265755606784));
#33511=CARTESIAN_POINT('Ctrl Pts',(-3.31082405553576,0.794772684003639,
10.7914805646343));
#33512=CARTESIAN_POINT('Ctrl Pts',(-3.3514923734059,1.06847604194963,10.8303051522282));
#33513=CARTESIAN_POINT('Ctrl Pts',(-3.37024002099385,1.18514270861744,10.8359100775422));
#33514=CARTESIAN_POINT('Ctrl Pts',(-3.39013150827335,1.30000000000678,10.8303142027936));
#33515=CARTESIAN_POINT('Ctrl Pts',(-3.55903559501172,-1.30000000000473,
10.6585990137924));
#33516=CARTESIAN_POINT('Ctrl Pts',(-3.52898566602019,-1.18514270861605,
10.6746008966558));
#33517=CARTESIAN_POINT('Ctrl Pts',(-3.49803917570353,-1.06847604194892,
10.6811319700951));
#33518=CARTESIAN_POINT('Ctrl Pts',(-3.42447535623036,-0.79477268400363,
10.6743405918781));
#33519=CARTESIAN_POINT('Ctrl Pts',(-3.37128560137921,-0.636309800097421,
10.6327859803119));
#33520=CARTESIAN_POINT('Ctrl Pts',(-3.30278947088664,-0.319434907278276,
10.6034731326008));
#33521=CARTESIAN_POINT('Ctrl Pts',(-3.27023986261253,-0.158333333333886,
10.5783165335595));
#33522=CARTESIAN_POINT('Ctrl Pts',(-3.24765357747863,0.158333333333888,
10.6000134933769));
#33523=CARTESIAN_POINT('Ctrl Pts',(-3.25691882719003,0.319434907278284,
10.6475029434009));
#33524=CARTESIAN_POINT('Ctrl Pts',(-3.28083024644292,0.63630980009743,10.7197156715094));
#33525=CARTESIAN_POINT('Ctrl Pts',(-3.30935748754829,0.79477268400362,10.7842163758251));
#33526=CARTESIAN_POINT('Ctrl Pts',(-3.35033881509226,1.0684760419496,10.8239457582688));
#33527=CARTESIAN_POINT('Ctrl Pts',(-3.36920131774698,1.18514270861741,10.8302307025121));
#33528=CARTESIAN_POINT('Ctrl Pts',(-3.3891870248704,1.30000000000675,10.8256032134573));
#33529=CARTESIAN_POINT('Ctrl Pts',(-3.55752159162629,-1.30000000000469,
10.6542337760585));
#33530=CARTESIAN_POINT('Ctrl Pts',(-3.52715172501055,-1.18514270861602,
10.6694131300325));
#33531=CARTESIAN_POINT('Ctrl Pts',(-3.49597694911425,-1.06847604194888,
10.6753389254243));
#33532=CARTESIAN_POINT('Ctrl Pts',(-3.42209747884168,-0.794772684003606,
10.6676511267378));
#33533=CARTESIAN_POINT('Ctrl Pts',(-3.368992580335,-0.636309800097402,10.626234723924));
#33534=CARTESIAN_POINT('Ctrl Pts',(-3.30055362425563,-0.319434907278266,
10.5968508024426));
#33535=CARTESIAN_POINT('Ctrl Pts',(-3.26815037522595,-0.158333333333881,
10.5719351062856));
#33536=CARTESIAN_POINT('Ctrl Pts',(-3.24566707198885,0.158333333333883,
10.5935646644834));
#33537=CARTESIAN_POINT('Ctrl Pts',(-3.2548509611682,0.319434907278274,10.6407670490172));
#33538=CARTESIAN_POINT('Ctrl Pts',(-3.27899234172843,0.636309800097411,
10.7128702963079));
#33539=CARTESIAN_POINT('Ctrl Pts',(-3.30784607106761,0.794772684003596,
10.7769787929198));
#33540=CARTESIAN_POINT('Ctrl Pts',(-3.34914925161841,1.06847604194957,10.8176075249763));
#33541=CARTESIAN_POINT('Ctrl Pts',(-3.36813583255034,1.18514270861738,10.8245668295542));
#33542=CARTESIAN_POINT('Ctrl Pts',(-3.38823037798735,1.30000000000671,10.8208987660454));
#33543=CARTESIAN_POINT('Ctrl Pts',(-3.55627990365541,-1.30000000000468,
10.650581842169));
#33544=CARTESIAN_POINT('Ctrl Pts',(-3.52567472551719,-1.185142708616,10.6650532747694));
#33545=CARTESIAN_POINT('Ctrl Pts',(-3.49432538040437,-1.06847604194887,
10.6704633371688));
#33546=CARTESIAN_POINT('Ctrl Pts',(-3.42018294719733,-0.794772684003595,
10.6620280857059));
#33547=CARTESIAN_POINT('Ctrl Pts',(-3.36709213569808,-0.636309800097393,
10.6207672424199));
#33548=CARTESIAN_POINT('Ctrl Pts',(-3.29865407552894,-0.319434907278262,
10.5913565459549));
#33549=CARTESIAN_POINT('Ctrl Pts',(-3.26633175109663,-0.158333333333879,
10.5666693570679));
#33550=CARTESIAN_POINT('Ctrl Pts',(-3.24394125733372,0.158333333333881,
10.5882377662089));
#33551=CARTESIAN_POINT('Ctrl Pts',(-3.2531381412007,0.31943490727827,10.635146342547));
#33552=CARTESIAN_POINT('Ctrl Pts',(-3.27746541146243,0.636309800097403,
10.7071602656532));
#33553=CARTESIAN_POINT('Ctrl Pts',(-3.30648891039559,0.794772684003586,
10.7710069393103));
#33554=CARTESIAN_POINT('Ctrl Pts',(-3.34805987709607,1.06847604194956,10.8123856843356));
#33555=CARTESIAN_POINT('Ctrl Pts',(-3.3671700124198,1.18514270861736,10.8198945045906));
#33556=CARTESIAN_POINT('Ctrl Pts',(-3.38739575193867,1.3000000000067,10.8170008196127));
#33557=CARTESIAN_POINT('Ctrl Pts',(-3.55530544718959,-1.30000000000466,
10.6476469380569));
#33558=CARTESIAN_POINT('Ctrl Pts',(-3.52453845358926,-1.18514270861599,
10.6615332127035));
#33559=CARTESIAN_POINT('Ctrl Pts',(-3.49306443829092,-1.06847604194886,
10.6665199771758));
#33560=CARTESIAN_POINT('Ctrl Pts',(-3.41871980503502,-0.794772684003589,
10.657480751862));
#33561=CARTESIAN_POINT('Ctrl Pts',(-3.36560903961373,-0.636309800097388,
10.6163664598669));
#33562=CARTESIAN_POINT('Ctrl Pts',(-3.29713541830363,-0.319434907278259,
10.5869595650996));
#33563=CARTESIAN_POINT('Ctrl Pts',(-3.26483504926751,-0.158333333333878,
10.5624846541022));
#33564=CARTESIAN_POINT('Ctrl Pts',(-3.24251388738839,0.15833333333388,10.5840077208246));
#33565=CARTESIAN_POINT('Ctrl Pts',(-3.25177237466923,0.319434907278268,
10.6306468149272));
#33566=CARTESIAN_POINT('Ctrl Pts',(-3.27624745090271,0.636309800097398,
10.7025887389857));
#33567=CARTESIAN_POINT('Ctrl Pts',(-3.30535393223191,0.794772684003579,
10.7662588842987));
#33568=CARTESIAN_POINT('Ctrl Pts',(-3.34713655006451,1.06847604194955,10.8082394976319));
#33569=CARTESIAN_POINT('Ctrl Pts',(-3.36635419398821,1.18514270861735,10.8161828028864));
#33570=CARTESIAN_POINT('Ctrl Pts',(-3.38670333477437,1.30000000000668,10.8138975614185));
#33571=CARTESIAN_POINT('Ctrl Pts',(-3.55433797136118,-1.30000000000466,
10.6447070646829));
#33572=CARTESIAN_POINT('Ctrl Pts',(-3.52342067206276,-1.18514270861598,
10.6579998855295));
#33573=CARTESIAN_POINT('Ctrl Pts',(-3.49182717097928,-1.06847604194885,
10.6625595905517));
#33574=CARTESIAN_POINT('Ctrl Pts',(-3.41727770182104,-0.794772684003584,
10.6529181767109));
#33575=CARTESIAN_POINT('Ctrl Pts',(-3.36411925843592,-0.636309800097384,
10.6119703680613));
#33576=CARTESIAN_POINT('Ctrl Pts',(-3.29559467409961,-0.319434907278257,
10.5825779694666));
#33577=CARTESIAN_POINT('Ctrl Pts',(-3.26330933623401,-0.158333333333877,
10.5583195887821));
#33578=CARTESIAN_POINT('Ctrl Pts',(-3.24106629086893,0.158333333333879,
10.579791104));
#33579=CARTESIAN_POINT('Ctrl Pts',(-3.25042046142221,0.319434907278266,
10.626137820413));
#33580=CARTESIAN_POINT('Ctrl Pts',(-3.27503921876234,0.636309800097394,
10.6980097305382));
#33581=CARTESIAN_POINT('Ctrl Pts',(-3.30417980955526,0.794772684003574,
10.7615346745576));
#33582=CARTESIAN_POINT('Ctrl Pts',(-3.34617223155567,1.06847604194954,10.8041184706937));
#33583=CARTESIAN_POINT('Ctrl Pts',(-3.36550607566519,1.18514270861734,10.8124908401636));
#33584=CARTESIAN_POINT('Ctrl Pts',(-3.38599680037276,1.30000000000668,10.8108026316413));
#33585=CARTESIAN_POINT('Ctrl Pts',(-3.54984970514755,-1.30000000000455,
10.6306658122771));
#33586=CARTESIAN_POINT('Ctrl Pts',(-3.51834143663056,-1.18514270861589,
10.6410528143556));
#33587=CARTESIAN_POINT('Ctrl Pts',(-3.48626566849313,-1.06847604194877,
10.6435233970436));
#33588=CARTESIAN_POINT('Ctrl Pts',(-3.41085318970915,-0.794772684003521,
10.6309424248252));
#33589=CARTESIAN_POINT('Ctrl Pts',(-3.35748539912993,-0.636309800097333,
10.5907706537778));
#33590=CARTESIAN_POINT('Ctrl Pts',(-3.28854880426052,-0.319434907278232,
10.5615660112157));
#33591=CARTESIAN_POINT('Ctrl Pts',(-3.25600785230901,-0.158333333333864,
10.5385678190991));
#33592=CARTESIAN_POINT('Ctrl Pts',(-3.23398649691687,0.158333333333866,
10.5599007473991));
#33593=CARTESIAN_POINT('Ctrl Pts',(-3.24388113552723,0.31943490727824,10.6047995313936));
#33594=CARTESIAN_POINT('Ctrl Pts',(-3.26923480939674,0.636309800097343,
10.6763015230462));
#33595=CARTESIAN_POINT('Ctrl Pts',(-3.29863995344783,0.79477268400351,10.7390613151974));
#33596=CARTESIAN_POINT('Ctrl Pts',(-3.34161847429591,1.06847604194946,10.7845180418296));
#33597=CARTESIAN_POINT('Ctrl Pts',(-3.36147233784438,1.18514270861725,10.7949519108724));
#33598=CARTESIAN_POINT('Ctrl Pts',(-3.38257625577727,1.30000000000657,10.7961431163365));
#33599=CARTESIAN_POINT('Ctrl Pts',(-3.54346327544845,-1.30000000000345,
10.6116084872656));
#33600=CARTESIAN_POINT('Ctrl Pts',(-3.51087038822887,-1.18514270861488,
10.6182069030137));
#33601=CARTESIAN_POINT('Ctrl Pts',(-3.47788547855602,-1.06847604194786,
10.6179921149657));
#33602=CARTESIAN_POINT('Ctrl Pts',(-3.40077808831231,-0.794772684002841,
10.6017560478612));
#33603=CARTESIAN_POINT('Ctrl Pts',(-3.34648395165712,-0.636309800096792,
10.5631227662308));
#33604=CARTESIAN_POINT('Ctrl Pts',(-3.27736572352823,-0.319434907277961,
10.5339123302075));
#33605=CARTESIAN_POINT('Ctrl Pts',(-3.24570255877244,-0.15833333333373,
10.5117636373826));
#33606=CARTESIAN_POINT('Ctrl Pts',(-3.22473605365345,0.158333333333732,
10.5323693415874));
#33607=CARTESIAN_POINT('Ctrl Pts',(-3.23555825476826,0.31943490727797,10.5751540299561));
#33608=CARTESIAN_POINT('Ctrl Pts',(-3.26171350265685,0.636309800096803,
10.6462751005081));
#33609=CARTESIAN_POINT('Ctrl Pts',(-3.29042133095542,0.794772684002834,
10.7086999413166));
#33610=CARTESIAN_POINT('Ctrl Pts',(-3.33480204109443,1.06847604194855,10.7580517685289));
#33611=CARTESIAN_POINT('Ctrl Pts',(-3.35562786553996,1.18514270861624,10.7711322840336));
#33612=CARTESIAN_POINT('Ctrl Pts',(-3.37806874947915,1.30000000000547,10.7759307377082));
#33613=CARTESIAN_POINT('Ctrl Pts',(-3.53506496247113,-1.30000000000306,
10.5885155682011));
#33614=CARTESIAN_POINT('Ctrl Pts',(-3.50062776708192,-1.18514270861453,
10.5908138492831));
#33615=CARTESIAN_POINT('Ctrl Pts',(-3.46639685555495,-1.06847604194754,
10.5873798227));
#33616=CARTESIAN_POINT('Ctrl Pts',(-3.38779315904599,-0.79477268400261,
10.5662037568673));
#33617=CARTESIAN_POINT('Ctrl Pts',(-3.33486996497483,-0.636309800096606,
10.5276326062933));
#33618=CARTESIAN_POINT('Ctrl Pts',(-3.26577734696951,-0.319434907277867,
10.4982277618773));
#33619=CARTESIAN_POINT('Ctrl Pts',(-3.23377655240389,-0.158333333333683,
10.4781750219806));
#33620=CARTESIAN_POINT('Ctrl Pts',(-3.21261251753656,0.158333333333685,
10.4989346304306));
#33621=CARTESIAN_POINT('Ctrl Pts',(-3.22291473938703,0.319434907277874,
10.5402309269832));
#33622=CARTESIAN_POINT('Ctrl Pts',(-3.24998655733667,0.636309800096615,
10.6109358314202));
#33623=CARTESIAN_POINT('Ctrl Pts',(-3.28026677895592,0.794772684002601,
10.671291429696));
#33624=CARTESIAN_POINT('Ctrl Pts',(-3.3263996702633,1.06847604194823,10.7254459437499));
#33625=CARTESIAN_POINT('Ctrl Pts',(-3.34797394235853,1.18514270861589,10.7421061125178));
#33626=CARTESIAN_POINT('Ctrl Pts',(-3.37115326729403,1.30000000000509,10.7519849675422));
#33627=CARTESIAN_POINT('Ctrl Pts',(-3.52689650086691,-1.30000000000268,
10.5652540209631));
#33628=CARTESIAN_POINT('Ctrl Pts',(-3.49113723742897,-1.18514270861418,
10.562853485114));
#33629=CARTESIAN_POINT('Ctrl Pts',(-3.45576242609193,-1.06847604194723,
10.5561146433435));
#33630=CARTESIAN_POINT('Ctrl Pts',(-3.3749276964591,-0.794772684002374,
10.5305242161996));
#33631=CARTESIAN_POINT('Ctrl Pts',(-3.32053529474771,-0.636309800096415,
10.4941077758252));
#33632=CARTESIAN_POINT('Ctrl Pts',(-3.25116009621693,-0.31943490727777,
10.4647365721695));
#33633=CARTESIAN_POINT('Ctrl Pts',(-3.22065187264131,-0.158333333333636,
10.4454354717321));
#33634=CARTESIAN_POINT('Ctrl Pts',(-3.20049904729554,0.158333333333637,
10.465470439846));
#33635=CARTESIAN_POINT('Ctrl Pts',(-3.21091965362889,0.319434907277778,
10.5048325382507));
#33636=CARTESIAN_POINT('Ctrl Pts',(-3.2391121737702,0.636309800096424,10.5749605084516));
#33637=CARTESIAN_POINT('Ctrl Pts',(-3.26980391173995,0.794772684002361,
10.6340355202244));
#33638=CARTESIAN_POINT('Ctrl Pts',(-3.31812627927797,1.06847604194791,10.6926922434587));
#33639=CARTESIAN_POINT('Ctrl Pts',(-3.34093984347042,1.18514270861554,10.7125985698184));
#33640=CARTESIAN_POINT('Ctrl Pts',(-3.36565000946822,1.3000000000047,10.7270209004954));
#33641=CARTESIAN_POINT('Ctrl Pts',(-3.51848982050878,-1.30000000000228,
10.5421141081693));
#33642=CARTESIAN_POINT('Ctrl Pts',(-3.4805863296336,-1.18514270861381,10.5356318371647));
#33643=CARTESIAN_POINT('Ctrl Pts',(-3.44368553106901,-1.0684760419469,10.5258764582561));
#33644=CARTESIAN_POINT('Ctrl Pts',(-3.36075372423075,-0.794772684002127,
10.4957780473791));
#33645=CARTESIAN_POINT('Ctrl Pts',(-3.30728683871919,-0.636309800096218,
10.4597379308942));
#33646=CARTESIAN_POINT('Ctrl Pts',(-3.23767528843882,-0.319434907277672,
10.4303589106883));
#33647=CARTESIAN_POINT('Ctrl Pts',(-3.20694464491671,-0.158333333333587,
10.4130789334689));
#33648=CARTESIAN_POINT('Ctrl Pts',(-3.1868156375817,0.158333333333589,10.4330970843297));
#33649=CARTESIAN_POINT('Ctrl Pts',(-3.19711015924159,0.31943490727768,10.4706721108572));
#33650=CARTESIAN_POINT('Ctrl Pts',(-3.22634594109612,0.636309800096228,
10.5402626408123));
#33651=CARTESIAN_POINT('Ctrl Pts',(-3.25813763743538,0.794772684002116,
10.5975581252224));
#33652=CARTESIAN_POINT('Ctrl Pts',(-3.30855188048357,1.06847604194758,10.6607913253926));
#33653=CARTESIAN_POINT('Ctrl Pts',(-3.33241496581671,1.18514270861517,10.6840852949285));
#33654=CARTESIAN_POINT('Ctrl Pts',(-3.35831867869917,1.3000000000043,10.7033019246676));
#33655=CARTESIAN_POINT('Ctrl Pts',(-3.51014479419037,-1.30000000000198,
10.5226552577285));
#33656=CARTESIAN_POINT('Ctrl Pts',(-3.47081330763693,-1.18514270861354,
10.5122336534893));
#33657=CARTESIAN_POINT('Ctrl Pts',(-3.43276073750195,-1.06847604194665,
10.4996794489523));
#33658=CARTESIAN_POINT('Ctrl Pts',(-3.34780624087258,-0.794772684001944,
10.4657499916987));
#33659=CARTESIAN_POINT('Ctrl Pts',(-3.29367302138748,-0.636309800096072,
10.4311638915496));
#33660=CARTESIAN_POINT('Ctrl Pts',(-3.2236579236351,-0.319434907277599,
10.4019302275856));
#33661=CARTESIAN_POINT('Ctrl Pts',(-3.193285751204,-0.15833333333355,10.3860071381036));
#33662=CARTESIAN_POINT('Ctrl Pts',(-3.17425631785229,0.158333333333552,
10.405209097692));
#33663=CARTESIAN_POINT('Ctrl Pts',(-3.18586725480623,0.319434907277607,
10.4401640643241));
#33664=CARTESIAN_POINT('Ctrl Pts',(-3.21657446722625,0.636309800096082,
10.5088571830631));
#33665=CARTESIAN_POINT('Ctrl Pts',(-3.24843254019359,0.794772684001934,
10.5652288826434));
#33666=CARTESIAN_POINT('Ctrl Pts',(-3.30057225868985,1.06847604194734,10.6325503637368));
#33667=CARTESIAN_POINT('Ctrl Pts',(-3.32540393947806,1.1851427086149,10.6587825433198));
#33668=CARTESIAN_POINT('Ctrl Pts',(-3.35249794888434,1.300000000004,10.682105927827));
#33669=CARTESIAN_POINT('Ctrl Pts',(-3.50627111332775,-1.30000000000195,
10.5126758013699));
#33670=CARTESIAN_POINT('Ctrl Pts',(-3.46614340916371,-1.18514270861352,
10.5003491529217));
#33671=CARTESIAN_POINT('Ctrl Pts',(-3.42745785791775,-1.06847604194663,
10.4864410559917));
#33672=CARTESIAN_POINT('Ctrl Pts',(-3.34141815726407,-0.794772684001931,
10.4506571074177));
#33673=CARTESIAN_POINT('Ctrl Pts',(-3.28697220080956,-0.636309800096061,
10.4167873260709));
#33674=CARTESIAN_POINT('Ctrl Pts',(-3.21680479490168,-0.319434907277593,
10.3875900843894));
#33675=CARTESIAN_POINT('Ctrl Pts',(-3.18691486237597,-0.158333333333548,
10.3721194208555));
#33676=CARTESIAN_POINT('Ctrl Pts',(-3.16805993730455,0.158333333333549,
10.3911809611948));
#33677=CARTESIAN_POINT('Ctrl Pts',(-3.17936658980045,0.319434907277601,
10.4255224204891));
#33678=CARTESIAN_POINT('Ctrl Pts',(-3.21057454954685,0.636309800096071,
10.4939351803383));
#33679=CARTESIAN_POINT('Ctrl Pts',(-3.24308445280218,0.79477268400192,10.5493933453868));
#33680=CARTESIAN_POINT('Ctrl Pts',(-3.29631738645729,1.06847604194732,10.618596658197));
#33681=CARTESIAN_POINT('Ctrl Pts',(-3.32168699236818,1.18514270861488,10.6462629950032));
#33682=CARTESIAN_POINT('Ctrl Pts',(-3.34938363968517,1.30000000000397,10.6716401187353));
#33683=CARTESIAN_POINT('Ctrl Pts',(-3.50442220663023,-1.30000000000194,
10.5076132694343));
#33684=CARTESIAN_POINT('Ctrl Pts',(-3.46384552380066,-1.18514270861351,
10.4943747916605));
#33685=CARTESIAN_POINT('Ctrl Pts',(-3.4248217357718,-1.06847604194662,10.4798074269121));
#33686=CARTESIAN_POINT('Ctrl Pts',(-3.33825647638829,-0.794772684001924,
10.4430839053978));
#33687=CARTESIAN_POINT('Ctrl Pts',(-3.28384015432874,-0.636309800096055,
10.4094268857005));
#33688=CARTESIAN_POINT('Ctrl Pts',(-3.21356381239586,-0.319434907277589,
10.3802731839803));
#33689=CARTESIAN_POINT('Ctrl Pts',(-3.1837029538244,-0.158333333333546,
10.3651927772445));
#33690=CARTESIAN_POINT('Ctrl Pts',(-3.16486895641784,0.158333333333548,
10.384237183974));
#33691=CARTESIAN_POINT('Ctrl Pts',(-3.17613062389401,0.319434907277598,
10.4181942985397));
#33692=CARTESIAN_POINT('Ctrl Pts',(-3.20756518565311,0.636309800096065,
10.4864816761086));
#33693=CARTESIAN_POINT('Ctrl Pts',(-3.24022250464605,0.794772684001912,
10.541604280706));
#33694=CARTESIAN_POINT('Ctrl Pts',(-3.29408957437523,1.06847604194731,10.6116856914377));
#33695=CARTESIAN_POINT('Ctrl Pts',(-3.31982231985351,1.18514270861487,10.640003080883));
#33696=CARTESIAN_POINT('Ctrl Pts',(-3.34797075229587,1.30000000000396,10.6663022138399));
#33697=CARTESIAN_POINT('Ctrl Pts',(-3.50332286786843,-1.30000000000194,
10.5047548383451));
#33698=CARTESIAN_POINT('Ctrl Pts',(-3.46249907684773,-1.18514270861351,
10.4909872449872));
#33699=CARTESIAN_POINT('Ctrl Pts',(-3.42328867404982,-1.06847604194662,
10.4760374556843));
#33700=CARTESIAN_POINT('Ctrl Pts',(-3.33643204912433,-0.794772684001923,
10.4387693425693));
#33701=CARTESIAN_POINT('Ctrl Pts',(-3.28202668760804,-0.636309800096055,
10.4052388113571));
#33702=CARTESIAN_POINT('Ctrl Pts',(-3.21169158000919,-0.31943490727759,
10.3761071804382));
#33703=CARTESIAN_POINT('Ctrl Pts',(-3.18185600383943,-0.158333333333546,
10.3612432547402));
#33704=CARTESIAN_POINT('Ctrl Pts',(-3.16303173093386,0.158333333333548,
10.3802790615228));
#33705=CARTESIAN_POINT('Ctrl Pts',(-3.17425209796324,0.319434907277598,
10.4140275193072));
#33706=CARTESIAN_POINT('Ctrl Pts',(-3.20581766920952,0.636309800096064,
10.4822418536827));
#33707=CARTESIAN_POINT('Ctrl Pts',(-3.23858232090324,0.794772684001912,
10.5371560079436));
#33708=CARTESIAN_POINT('Ctrl Pts',(-3.29280828302676,1.06847604194731,10.6077416082037));
#33709=CARTESIAN_POINT('Ctrl Pts',(-3.31874163469961,1.18514270861487,10.6364359889067));
#33710=CARTESIAN_POINT('Ctrl Pts',(-3.34713592831186,1.30000000000396,10.6632708594143));
#33711=CARTESIAN_POINT('Ctrl Pts',(-3.49802816243002,-1.3000000000019,10.4921711193909));
#33712=CARTESIAN_POINT('Ctrl Pts',(-3.45607526139304,-1.18514270861347,
10.4760324866026));
#33713=CARTESIAN_POINT('Ctrl Pts',(-3.41602730485291,-1.06847604194659,
10.4593577238278));
#33714=CARTESIAN_POINT('Ctrl Pts',(-3.32790931654956,-0.7947726840019,10.4195971185223));
#33715=CARTESIAN_POINT('Ctrl Pts',(-3.27368731733683,-0.636309800096035,
10.3865334216883));
#33716=CARTESIAN_POINT('Ctrl Pts',(-3.20313098737036,-0.31943490727758,
10.3574669172447));
#33717=CARTESIAN_POINT('Ctrl Pts',(-3.17331373829767,-0.158333333333541,
10.3436502842482));
#33718=CARTESIAN_POINT('Ctrl Pts',(-3.15458900713016,0.158333333333543,
10.3626037702061));
#33719=CARTESIAN_POINT('Ctrl Pts',(-3.16579131284204,0.319434907277589,
10.3952847176026));
#33720=CARTESIAN_POINT('Ctrl Pts',(-3.19798308378842,0.636309800096045,
10.4631397442888));
#33721=CARTESIAN_POINT('Ctrl Pts',(-3.23113884245982,0.794772684001888,
10.517183788305));
#33722=CARTESIAN_POINT('Ctrl Pts',(-3.28690490196432,1.06847604194728,10.5900916182367));
#33723=CARTESIAN_POINT('Ctrl Pts',(-3.3137062707773,1.18514270861483,10.6205071590004));
#33724=CARTESIAN_POINT('Ctrl Pts',(-3.34316994757983,1.30000000000392,10.6497791424516));
#33725=CARTESIAN_POINT('Ctrl Pts',(-3.48397706310386,-1.30000000000141,
10.4576138699549));
#33726=CARTESIAN_POINT('Ctrl Pts',(-3.43892185456666,-1.18514270861303,
10.4350647117943));
#33727=CARTESIAN_POINT('Ctrl Pts',(-3.39646067472579,-1.06847604194619,
10.4138137881798));
#33728=CARTESIAN_POINT('Ctrl Pts',(-3.30435958018563,-0.7947726840016,10.3677190849106));
#33729=CARTESIAN_POINT('Ctrl Pts',(-3.24962674772453,-0.636309800095795,
10.3367046172998));
#33730=CARTESIAN_POINT('Ctrl Pts',(-3.1781699323947,-0.319434907277458,
10.3080563523622));
#33731=CARTESIAN_POINT('Ctrl Pts',(-3.14881299455345,-0.158333333333481,
10.2967802534541));
#33732=CARTESIAN_POINT('Ctrl Pts',(-3.13084603918494,0.158333333333483,
10.3151362963075));
#33733=CARTESIAN_POINT('Ctrl Pts',(-3.1424211459828,0.319434907277467,10.3445817757753));
#33734=CARTESIAN_POINT('Ctrl Pts',(-3.17690348196985,0.636309800095804,
10.4110001959783));
#33735=CARTESIAN_POINT('Ctrl Pts',(-3.21181232388892,0.794772684001585,
10.4621613398969));
#33736=CARTESIAN_POINT('Ctrl Pts',(-3.27143809948091,1.06847604194687,10.5415995405055));
#33737=CARTESIAN_POINT('Ctrl Pts',(-3.30019347467114,1.18514270861439,10.5769819782888));
#33738=CARTESIAN_POINT('Ctrl Pts',(-3.33189443615046,1.30000000000344,10.6133610002872));
#33739=CARTESIAN_POINT('Ctrl Pts',(-3.46377916361696,-1.30000000000082,
10.4138557361379));
#33740=CARTESIAN_POINT('Ctrl Pts',(-3.41402371948706,-1.18514270861249,
10.3833809953346));
#33741=CARTESIAN_POINT('Ctrl Pts',(-3.36792730141995,-1.0684760419457,10.356495138021));
#33742=CARTESIAN_POINT('Ctrl Pts',(-3.2698884363188,-0.794772684001241,
10.3026744679445));
#33743=CARTESIAN_POINT('Ctrl Pts',(-3.2142860913702,-0.636309800095512,
10.2745877798555));
#33744=CARTESIAN_POINT('Ctrl Pts',(-3.14208095012235,-0.319434907277318,
10.2461465738796));
#33745=CARTESIAN_POINT('Ctrl Pts',(-3.11455340661153,-0.158333333333411,
10.2371914073107));
#33746=CARTESIAN_POINT('Ctrl Pts',(-3.09792221777229,0.158333333333413,
10.2544087077735));
#33747=CARTESIAN_POINT('Ctrl Pts',(-3.10963346579246,0.319434907277324,
10.2798132868226));
#33748=CARTESIAN_POINT('Ctrl Pts',(-3.14630219378336,0.63630980009552,10.3448890266851));
#33749=CARTESIAN_POINT('Ctrl Pts',(-3.18162015994576,0.794772684001235,
10.3936449172902));
#33750=CARTESIAN_POINT('Ctrl Pts',(-3.24699522480645,1.0684760419464,10.4811548570736));
#33751=CARTESIAN_POINT('Ctrl Pts',(-3.27920998334397,1.18514270861386,10.5224088501547));
#33752=CARTESIAN_POINT('Ctrl Pts',(-3.31534105722563,1.30000000000285,10.5670370259473));
#33753=CARTESIAN_POINT('Ctrl Pts',(-3.44488287358291,-1.30000000000062,
10.3765723257512));
#33754=CARTESIAN_POINT('Ctrl Pts',(-3.39066496137285,-1.1851427086123,10.3394879857485));
#33755=CARTESIAN_POINT('Ctrl Pts',(-3.34107969198908,-1.06847604194554,
10.3079609144036));
#33756=CARTESIAN_POINT('Ctrl Pts',(-3.23723013189924,-0.794772684001115,
10.2479654749552));
#33757=CARTESIAN_POINT('Ctrl Pts',(-3.18090985311315,-0.636309800095411,
10.2224572148459));
#33758=CARTESIAN_POINT('Ctrl Pts',(-3.10701733313301,-0.319434907277268,
10.1951055044507));
#33759=CARTESIAN_POINT('Ctrl Pts',(-3.07956989313146,-0.158333333333386,
10.189486269028));
#33760=CARTESIAN_POINT('Ctrl Pts',(-3.06373460659005,0.158333333333388,
10.2059523010134));
#33761=CARTESIAN_POINT('Ctrl Pts',(-3.07606165687102,0.319434907277274,
10.227261115237));
#33762=CARTESIAN_POINT('Ctrl Pts',(-3.116242644995,0.63630980009542,10.2897345264231));
#33763=CARTESIAN_POINT('Ctrl Pts',(-3.15420785454821,0.79477268400111,10.3344921720662));
#33764=CARTESIAN_POINT('Ctrl Pts',(-3.22583655900311,1.06847604194623,10.428013227239));
#33765=CARTESIAN_POINT('Ctrl Pts',(-3.26127444105666,1.18514270861367,10.4742267922661));
#33766=CARTESIAN_POINT('Ctrl Pts',(-3.30114479311019,1.30000000000264,10.5261721228327));
#33767=CARTESIAN_POINT('Ctrl Pts',(-3.43444272475388,-1.30000000000054,
10.3549066020539));
#33768=CARTESIAN_POINT('Ctrl Pts',(-3.37747777932839,-1.18514270861223,
10.3141508035821));
#33769=CARTESIAN_POINT('Ctrl Pts',(-3.32566871721267,-1.06847604194547,
10.2801253752984));
#33770=CARTESIAN_POINT('Ctrl Pts',(-3.21789054123447,-0.794772684001071,
10.2170683307399));
#33771=CARTESIAN_POINT('Ctrl Pts',(-3.16022877986869,-0.636309800095372,
10.19386882768));
#33772=CARTESIAN_POINT('Ctrl Pts',(-3.08551117227782,-0.319434907277247,
10.1670275964095));
#33773=CARTESIAN_POINT('Ctrl Pts',(-3.05948635543789,-0.158333333333376,
10.1621534237937));
#33774=CARTESIAN_POINT('Ctrl Pts',(-3.04426266656423,0.158333333333378,
10.1780338017966));
#33775=CARTESIAN_POINT('Ctrl Pts',(-3.05611868438866,0.319434907277256,
10.1976691980544));
#33776=CARTESIAN_POINT('Ctrl Pts',(-3.09767799919942,0.636309800095382,
10.2591372527431));
#33777=CARTESIAN_POINT('Ctrl Pts',(-3.13673010463398,0.79477268400106,10.3018913725775));
#33778=CARTESIAN_POINT('Ctrl Pts',(-3.2117957519062,1.06847604194616,10.3989965816232));
#33779=CARTESIAN_POINT('Ctrl Pts',(-3.24913105512162,1.18514270861359,10.4480394373749));
#33780=CARTESIAN_POINT('Ctrl Pts',(-3.29130852430455,1.30000000000256,10.5040919019848));
#33781=CARTESIAN_POINT('Ctrl Pts',(-3.4258722715173,-1.30000000000042,10.3393534519172));
#33782=CARTESIAN_POINT('Ctrl Pts',(-3.3668675213799,-1.18514270861212,10.2959381003515));
#33783=CARTESIAN_POINT('Ctrl Pts',(-3.31344654722717,-1.06847604194537,
10.2600789851213));
#33784=CARTESIAN_POINT('Ctrl Pts',(-3.20293304966028,-0.794772684000992,
10.1946936729031));
#33785=CARTESIAN_POINT('Ctrl Pts',(-3.14481525590605,-0.636309800095313,
10.172787671385));
#33786=CARTESIAN_POINT('Ctrl Pts',(-3.06922746540355,-0.319434907277219,
10.1465725101371));
#33787=CARTESIAN_POINT('Ctrl Pts',(-3.04322309875081,-0.158333333333361,
10.1431059236598));
#33788=CARTESIAN_POINT('Ctrl Pts',(-3.02833554978959,0.158333333333363,
10.1586363454208));
#33789=CARTESIAN_POINT('Ctrl Pts',(-3.04050029213829,0.319434907277224,
10.1764674528015));
#33790=CARTESIAN_POINT('Ctrl Pts',(-3.08362867027232,0.636309800095321,
10.2366918210486));
#33791=CARTESIAN_POINT('Ctrl Pts',(-3.12363637801034,0.794772684000988,
10.2778011992827));
#33792=CARTESIAN_POINT('Ctrl Pts',(-3.20185073556315,1.06847604194606,10.377011123269));
#33793=CARTESIAN_POINT('Ctrl Pts',(-3.24090185094023,1.18514270861348,10.427870915147));
#33794=CARTESIAN_POINT('Ctrl Pts',(-3.28514798443724,1.30000000000244,10.4866461988992));
#33795=CARTESIAN_POINT('Ctrl Pts',(-3.41721009436127,-1.30000000000036,
10.3237432942192));
#33796=CARTESIAN_POINT('Ctrl Pts',(-3.35605655066583,-1.18514270861207,
10.2775200347506));
#33797=CARTESIAN_POINT('Ctrl Pts',(-3.30084535509438,-1.06847604194533,
10.2398021730802));
#33798=CARTESIAN_POINT('Ctrl Pts',(-3.18702446129158,-0.794772684000962,
10.1723155376019));
#33799=CARTESIAN_POINT('Ctrl Pts',(-3.12697012194977,-0.636309800095285,
10.15303905683));
#33800=CARTESIAN_POINT('Ctrl Pts',(-3.05144450916497,-0.319434907277203,
10.1265784713633));
#33801=CARTESIAN_POINT('Ctrl Pts',(-3.02869685173172,-0.158333333333355,
10.1216965641621));
#33802=CARTESIAN_POINT('Ctrl Pts',(-3.01462692612418,0.158333333333357,
10.1364364939386));
#33803=CARTESIAN_POINT('Ctrl Pts',(-3.02483723154194,0.319434907277213,
10.1544033900266));
#33804=CARTESIAN_POINT('Ctrl Pts',(-3.06858167687439,0.636309800095296,
10.2142591465703));
#33805=CARTESIAN_POINT('Ctrl Pts',(-3.10986244179941,0.794772684000952,
10.2534454206316));
#33806=CARTESIAN_POINT('Ctrl Pts',(-3.19101517929812,1.06847604194602,10.3551902348169));
#33807=CARTESIAN_POINT('Ctrl Pts',(-3.23167729713891,1.18514270861343,10.4081154683092));
#33808=CARTESIAN_POINT('Ctrl Pts',(-3.27787351976245,1.30000000000239,10.4699243752498));
#33809=CARTESIAN_POINT('Ctrl Pts',(-3.41007224859412,-1.3000000000003,10.3108264414936));
#33810=CARTESIAN_POINT('Ctrl Pts',(-3.34662820042611,-1.18514270861202,
10.2630357435561));
#33811=CARTESIAN_POINT('Ctrl Pts',(-3.28989222434501,-1.06847604194528,
10.2240457564814));
#33812=CARTESIAN_POINT('Ctrl Pts',(-3.17431775807052,-0.794772684000926,
10.1543024890875));
#33813=CARTESIAN_POINT('Ctrl Pts',(-3.11591086660822,-0.636309800095255,
10.1342856641298));
#33814=CARTESIAN_POINT('Ctrl Pts',(-3.04098812630273,-0.319434907277188,
10.1072387673856));
#33815=CARTESIAN_POINT('Ctrl Pts',(-3.01902837233301,-0.158333333333347,
10.1029077311548));
#33816=CARTESIAN_POINT('Ctrl Pts',(-3.00449374065794,0.158333333333349,
10.1180418711654));
#33817=CARTESIAN_POINT('Ctrl Pts',(-3.0127637651021,0.319434907277197,10.1364598249738));
#33818=CARTESIAN_POINT('Ctrl Pts',(-3.05635950237011,0.636309800095265,
10.1964669919186));
#33819=CARTESIAN_POINT('Ctrl Pts',(-3.09844750254128,0.794772684000913,
10.2341642937794));
#33820=CARTESIAN_POINT('Ctrl Pts',(-3.18175214399387,1.06847604194597,10.3378593563706));
#33821=CARTESIAN_POINT('Ctrl Pts',(-3.22367765549952,1.18514270861338,10.3923324889705));
#33822=CARTESIAN_POINT('Ctrl Pts',(-3.27146918596705,1.30000000000232,10.4563930038551));
#33823=CARTESIAN_POINT('Ctrl Pts',(-3.40085406844961,-1.30000000000027,
10.2957145443334));
#33824=CARTESIAN_POINT('Ctrl Pts',(-3.33439270608681,-1.18514270861199,
10.245758638802));
#33825=CARTESIAN_POINT('Ctrl Pts',(-3.2757464998873,-1.06847604194525,10.2048938980597));
#33826=CARTESIAN_POINT('Ctrl Pts',(-3.15831660558689,-0.794772684000905,
10.1314905813258));
#33827=CARTESIAN_POINT('Ctrl Pts',(-3.10274865638003,-0.63630980009524,
10.1096261219701));
#33828=CARTESIAN_POINT('Ctrl Pts',(-3.02931459861233,-0.31943490727718,
10.0809918745011));
#33829=CARTESIAN_POINT('Ctrl Pts',(-3.00853263993761,-0.158333333333343,
10.0772919082541));
#33830=CARTESIAN_POINT('Ctrl Pts',(-2.99406174270539,0.158333333333345,
10.0923384537343));
#33831=CARTESIAN_POINT('Ctrl Pts',(-3.00096348447118,0.319434907277189,
10.1102436642837));
#33832=CARTESIAN_POINT('Ctrl Pts',(-3.04371819322789,0.636309800095249,
10.1712403114327));
#33833=CARTESIAN_POINT('Ctrl Pts',(-3.08435585321636,0.794772684000894,
10.2095531317405));
#33834=CARTESIAN_POINT('Ctrl Pts',(-3.16967607158215,1.06847604194594,10.316836258828));
#33835=CARTESIAN_POINT('Ctrl Pts',(-3.21328275026215,1.18514270861335,10.3734354818652));
#33836=CARTESIAN_POINT('Ctrl Pts',(-3.26356414651715,1.30000000000229,10.440195037455));
#33837=CARTESIAN_POINT('Ctrl Pts',(-3.39465878599097,-1.30000000000019,
10.2853534708596));
#33838=CARTESIAN_POINT('Ctrl Pts',(-3.32511928143436,-1.18514270861191,
10.2348322744866));
#33839=CARTESIAN_POINT('Ctrl Pts',(-3.26484306626976,-1.06847604194518,
10.1931031343358));
#33840=CARTESIAN_POINT('Ctrl Pts',(-3.14699300263423,-0.794772684000851,
10.1170118814196));
#33841=CARTESIAN_POINT('Ctrl Pts',(-3.09695175410121,-0.636309800095197,
10.0915712362322));
#33842=CARTESIAN_POINT('Ctrl Pts',(-3.02637472772942,-0.319434907277159,
10.0609469829604));
#33843=CARTESIAN_POINT('Ctrl Pts',(-3.00611348042902,-0.158333333333332,
10.058191722331));
#33844=CARTESIAN_POINT('Ctrl Pts',(-2.99178541075593,0.158333333333334,
10.0731598884958));
#33845=CARTESIAN_POINT('Ctrl Pts',(-2.99824596807587,0.319434907277167,
10.0901842798419));
#33846=CARTESIAN_POINT('Ctrl Pts',(-3.03856351371756,0.636309800095206,
10.1527214947233));
#33847=CARTESIAN_POINT('Ctrl Pts',(-3.07432779059338,0.79477268400084,10.1936664632184));
#33848=CARTESIAN_POINT('Ctrl Pts',(-3.16003000210956,1.06847604194587,10.3036861053275));
#33849=CARTESIAN_POINT('Ctrl Pts',(-3.2050733914081,1.18514270861327,10.3614091951292));
#33850=CARTESIAN_POINT('Ctrl Pts',(-3.25806285821962,1.30000000000221,10.4292319482927));
#33851=CARTESIAN_POINT('Ctrl Pts',(-3.39267401414631,-1.30000000000019,
10.276983507709));
#33852=CARTESIAN_POINT('Ctrl Pts',(-3.32322027641436,-1.18514270861191,
10.226698532237));
#33853=CARTESIAN_POINT('Ctrl Pts',(-3.26328889377517,-1.06847604194518,
10.1849734474866));
#33854=CARTESIAN_POINT('Ctrl Pts',(-3.1468339558515,-0.794772684000851,
10.1083552146057));
#33855=CARTESIAN_POINT('Ctrl Pts',(-3.09896529592857,-0.636309800095197,
10.0815496804376));
#33856=CARTESIAN_POINT('Ctrl Pts',(-3.02984981618038,-0.319434907277159,
10.0500837393884));
#33857=CARTESIAN_POINT('Ctrl Pts',(-3.00954349196179,-0.158333333333332,
10.0473018664685));
#33858=CARTESIAN_POINT('Ctrl Pts',(-2.99543061314513,0.158333333333334,
10.0621711387216));
#33859=CARTESIAN_POINT('Ctrl Pts',(-3.0023925612396,0.319434907277167,10.078980785313));
#33860=CARTESIAN_POINT('Ctrl Pts',(-3.04119573834857,0.636309800095206,
10.14244843534));
#33861=CARTESIAN_POINT('Ctrl Pts',(-3.0738873794296,0.79477268400084,10.1853620261542));
#33862=CARTESIAN_POINT('Ctrl Pts',(-3.15831522453578,1.06847604194587,10.2958137160522));
#33863=CARTESIAN_POINT('Ctrl Pts',(-3.20327264332997,1.18514270861327,10.3533447434002));
#33864=CARTESIAN_POINT('Ctrl Pts',(-3.25664179513173,1.30000000000221,10.4205963541777));
#33865=CARTESIAN_POINT('Ctrl Pts',(-3.39267401414619,-1.3,10.2769835077089));
#33866=CARTESIAN_POINT('Ctrl Pts',(-3.3232202764143,-1.18514270861178,10.226698532237));
#33867=CARTESIAN_POINT('Ctrl Pts',(-3.26328889377514,-1.06847604194512,
10.1849734474866));
#33868=CARTESIAN_POINT('Ctrl Pts',(-3.1468339558515,-0.794772684000851,
10.1083552146057));
#33869=CARTESIAN_POINT('Ctrl Pts',(-3.09896529592857,-0.636309800095197,
10.0815496804376));
#33870=CARTESIAN_POINT('Ctrl Pts',(-3.02984981618038,-0.319434907277159,
10.0500837393884));
#33871=CARTESIAN_POINT('Ctrl Pts',(-3.00954349196179,-0.158333333333332,
10.0473018664685));
#33872=CARTESIAN_POINT('Ctrl Pts',(-2.99543061314513,0.158333333333334,
10.0621711387217));
#33873=CARTESIAN_POINT('Ctrl Pts',(-3.0023925612396,0.319434907277167,10.078980785313));
#33874=CARTESIAN_POINT('Ctrl Pts',(-3.04119573834858,0.636309800095206,
10.14244843534));
#33875=CARTESIAN_POINT('Ctrl Pts',(-3.0738873794296,0.79477268400084,10.1853620261542));
#33876=CARTESIAN_POINT('Ctrl Pts',(-3.15831522453555,1.06847604194511,10.2958137160519));
#33877=CARTESIAN_POINT('Ctrl Pts',(-3.2032726433294,1.18514270861178,10.3533447433995));
#33878=CARTESIAN_POINT('Ctrl Pts',(-3.25664179513071,1.3,10.4205963541764));
#33879=CARTESIAN_POINT('',(-3.53203864909401,-1.2,10.6680258045906));
#33880=CARTESIAN_POINT('Ctrl Pts',(-3.53203864909401,-1.2,10.6680258045906));
#33881=CARTESIAN_POINT('Ctrl Pts',(-3.52949649314404,-1.21682298576918,
10.6466030151777));
#33882=CARTESIAN_POINT('Ctrl Pts',(-3.52798214088104,-1.23318431453843,
10.624704621099));
#33883=CARTESIAN_POINT('Ctrl Pts',(-3.52274184472548,-1.26590569890439,
10.5830210172903));
#33884=CARTESIAN_POINT('Ctrl Pts',(-3.5205885687882,-1.28162309756721,10.5625446886959));
#33885=CARTESIAN_POINT('Ctrl Pts',(-3.51745747224793,-1.2984297825913,10.5414408389829));
#33886=CARTESIAN_POINT('Ctrl Pts',(-3.51730897053275,-1.29921484486248,
10.5404572435777));
#33887=CARTESIAN_POINT('Ctrl Pts',(-3.51715788243336,-1.30000000000224,
10.5394760711847));
#33888=CARTESIAN_POINT('',(-3.42060206480302,-0.653834841417127,10.7779856782843));
#33889=CARTESIAN_POINT('Ctrl Pts',(-3.42060206482294,-0.653834841416443,
10.7779856783013));
#33890=CARTESIAN_POINT('Ctrl Pts',(-3.43236036060181,-0.717945624492541,
10.7667445905954));
#33891=CARTESIAN_POINT('Ctrl Pts',(-3.44189203683076,-0.763782257331169,
10.757549404514));
#33892=CARTESIAN_POINT('Ctrl Pts',(-3.4790210626449,-0.949542760432358,
10.7213842943359));
#33893=CARTESIAN_POINT('Ctrl Pts',(-3.49909315631117,-1.04876680996024,
10.7015794055091));
#33894=CARTESIAN_POINT('Ctrl Pts',(-3.53203864909401,-1.2,10.6680258045906));
#33895=CARTESIAN_POINT('',(-3.31841464832137,0.653834841531101,10.8729585107657));
#33896=CARTESIAN_POINT('Ctrl Pts',(-3.31841464832137,0.653834841531102,
10.8729585107657));
#33897=CARTESIAN_POINT('Ctrl Pts',(-3.30609938026503,0.575796605817473,
10.8331482966237));
#33898=CARTESIAN_POINT('Ctrl Pts',(-3.29643526076467,0.493919104637004,
10.799577764871));
#33899=CARTESIAN_POINT('Ctrl Pts',(-3.28487506509149,0.338196295579431,
10.7502176157553));
#33900=CARTESIAN_POINT('Ctrl Pts',(-3.28202732600753,0.265710097563185,
10.7325309479634));
#33901=CARTESIAN_POINT('Ctrl Pts',(-3.28242869861854,0.129740215298289,
10.70812432938));
#33902=CARTESIAN_POINT('Ctrl Pts',(-3.28482835999103,0.066640938344181,
10.7001962776734));
#33903=CARTESIAN_POINT('Ctrl Pts',(-3.29434436054939,-0.0595500090171539,
10.6908442069019));
#33904=CARTESIAN_POINT('Ctrl Pts',(-3.30152115228924,-0.122795915650191,
10.6893370787071));
#33905=CARTESIAN_POINT('Ctrl Pts',(-3.32179927220444,-0.260148629827643,
10.6937120240392));
#33906=CARTESIAN_POINT('Ctrl Pts',(-3.33574425320147,-0.333949114798701,
10.7009893453216));
#33907=CARTESIAN_POINT('Ctrl Pts',(-3.37150302708504,-0.491142723769832,
10.728020880275));
#33908=CARTESIAN_POINT('Ctrl Pts',(-3.39445736914294,-0.574254147968246,
10.7496580885196));
#33909=CARTESIAN_POINT('Ctrl Pts',(-3.42060206481036,-0.653834841428803,
10.7779856782448));
#33910=CARTESIAN_POINT('',(-3.37162231815327,1.2,10.8241775541122));
#33911=CARTESIAN_POINT('Ctrl Pts',(-3.37162231815327,1.2,10.8241775541122));
#33912=CARTESIAN_POINT('Ctrl Pts',(-3.36246959501592,1.13404402018397,10.8326924585674));
#33913=CARTESIAN_POINT('Ctrl Pts',(-3.35047549472867,1.03816619550936,10.8437839273622));
#33914=CARTESIAN_POINT('Ctrl Pts',(-3.32701157089733,0.79525632445983,10.8651966335573));
#33915=CARTESIAN_POINT('Ctrl Pts',(-3.32327568128371,0.741437054735132,
10.8685667042857));
#33916=CARTESIAN_POINT('Ctrl Pts',(-3.31841464832137,0.653834841531101,
10.8729585107657));
#33917=CARTESIAN_POINT('Ctrl Pts',(-3.35750281628589,1.30000000000061,10.699953548067));
#33918=CARTESIAN_POINT('Ctrl Pts',(-3.36044168963578,1.28316801238108,10.7204589243298));
#33919=CARTESIAN_POINT('Ctrl Pts',(-3.36254952465714,1.26661750999833,10.7413041016838));
#33920=CARTESIAN_POINT('Ctrl Pts',(-3.36761026216994,1.23437943378003,10.7808733082656));
#33921=CARTESIAN_POINT('Ctrl Pts',(-3.37028225138757,1.21555984826321,10.8041721739107));
#33922=CARTESIAN_POINT('Ctrl Pts',(-3.37162231815327,1.2,10.8241775541122));
#33923=CARTESIAN_POINT('Ctrl Pts',(-3.39267401414619,-1.3,10.2769835077089));
#33924=CARTESIAN_POINT('Ctrl Pts',(-3.32322027641429,-1.18514270861178,
10.226698532237));
#33925=CARTESIAN_POINT('Ctrl Pts',(-3.26328889377514,-1.06847604194512,
10.1849734474866));
#33926=CARTESIAN_POINT('Ctrl Pts',(-3.14683395585151,-0.794772684000851,
10.1083552146057));
#33927=CARTESIAN_POINT('Ctrl Pts',(-3.09896529592857,-0.636309800095197,
10.0815496804376));
#33928=CARTESIAN_POINT('Ctrl Pts',(-3.02984981618038,-0.319434907277159,
10.0500837393884));
#33929=CARTESIAN_POINT('Ctrl Pts',(-3.00954349196179,-0.158333333333332,
10.0473018664685));
#33930=CARTESIAN_POINT('Ctrl Pts',(-2.99543061314513,0.158333333333334,
10.0621711387216));
#33931=CARTESIAN_POINT('Ctrl Pts',(-3.0023925612396,0.319434907277167,10.078980785313));
#33932=CARTESIAN_POINT('Ctrl Pts',(-3.04119573834858,0.636309800095206,
10.14244843534));
#33933=CARTESIAN_POINT('Ctrl Pts',(-3.0738873794296,0.79477268400084,10.1853620261542));
#33934=CARTESIAN_POINT('Ctrl Pts',(-3.15831522453555,1.06847604194511,10.2958137160519));
#33935=CARTESIAN_POINT('Ctrl Pts',(-3.2032726433294,1.18514270861178,10.3533447433995));
#33936=CARTESIAN_POINT('Ctrl Pts',(-3.25664179513071,1.3,10.4205963541764));
#33937=CARTESIAN_POINT('Ctrl Pts',(-3.44290446030743,-1.3,10.2187081994464));
#33938=CARTESIAN_POINT('Ctrl Pts',(-3.37244803687278,-1.18514270861178,
10.1698358549729));
#33939=CARTESIAN_POINT('Ctrl Pts',(-3.31185538302694,-1.06847604194512,
10.129119962649));
#33940=CARTESIAN_POINT('Ctrl Pts',(-3.19466151211464,-0.794772684000851,
10.0539011423529));
#33941=CARTESIAN_POINT('Ctrl Pts',(-3.14738383460686,-0.636309800095197,
10.026688499191));
#33942=CARTESIAN_POINT('Ctrl Pts',(-3.07891484675056,-0.319434907277159,
9.99505906071815));
#33943=CARTESIAN_POINT('Ctrl Pts',(-3.05956220283012,-0.158333333333332,
9.99148223767552));
#33944=CARTESIAN_POINT('Ctrl Pts',(-3.04571607718934,0.158333333333334,
10.0065916955671));
#33945=CARTESIAN_POINT('Ctrl Pts',(-3.05198711671705,0.319434907277167,
10.0244328930108));
#33946=CARTESIAN_POINT('Ctrl Pts',(-3.09069526886232,0.636309800095206,
10.0885605835139));
#33947=CARTESIAN_POINT('Ctrl Pts',(-3.12304380561888,0.79477268400084,10.1321044737573));
#33948=CARTESIAN_POINT('Ctrl Pts',(-3.20878615765139,1.06847604194511,10.2416750001716));
#33949=CARTESIAN_POINT('Ctrl Pts',(-3.25467811874699,1.18514270861178,10.2984428894918));
#33950=CARTESIAN_POINT('Ctrl Pts',(-3.30934735381061,1.3,10.3645496472358));
#33951=CARTESIAN_POINT('Ctrl Pts',(-3.49313490646867,-1.3,10.1604328911839));
#33952=CARTESIAN_POINT('Ctrl Pts',(-3.42167579733126,-1.18514270861178,
10.1129731777087));
#33953=CARTESIAN_POINT('Ctrl Pts',(-3.36042187227873,-1.06847604194512,
10.0732664778114));
#33954=CARTESIAN_POINT('Ctrl Pts',(-3.24248906837778,-0.794772684000851,
9.99944707010019));
#33955=CARTESIAN_POINT('Ctrl Pts',(-3.19580237328515,-0.636309800095197,
9.97182731794448));
#33956=CARTESIAN_POINT('Ctrl Pts',(-3.12797987732075,-0.319434907277159,
9.94003438204794));
#33957=CARTESIAN_POINT('Ctrl Pts',(-3.10958091369845,-0.158333333333332,
9.93566260888258));
#33958=CARTESIAN_POINT('Ctrl Pts',(-3.09600154123355,0.158333333333334,
9.95101225241256));
#33959=CARTESIAN_POINT('Ctrl Pts',(-3.10158167219449,0.319434907277167,
9.96988500070868));
#33960=CARTESIAN_POINT('Ctrl Pts',(-3.14019479937607,0.636309800095206,
10.0346727316879));
#33961=CARTESIAN_POINT('Ctrl Pts',(-3.17220023180817,0.79477268400084,10.0788469213604));
#33962=CARTESIAN_POINT('Ctrl Pts',(-3.25925709076722,1.06847604194511,10.1875362842913));
#33963=CARTESIAN_POINT('Ctrl Pts',(-3.30608359416459,1.18514270861178,10.2435410355842));
#33964=CARTESIAN_POINT('Ctrl Pts',(-3.3620529124905,1.3,10.3085029402952));
#33965=CARTESIAN_POINT('Ctrl Pts',(-3.54336535262991,-1.3,10.1021575829215));
#33966=CARTESIAN_POINT('Ctrl Pts',(-3.47090355778975,-1.18514270861178,
10.0561105004446));
#33967=CARTESIAN_POINT('Ctrl Pts',(-3.40898836153053,-1.06847604194512,
10.0174129929737));
#33968=CARTESIAN_POINT('Ctrl Pts',(-3.29031662464092,-0.794772684000851,
9.94499299784744));
#33969=CARTESIAN_POINT('Ctrl Pts',(-3.24422091196344,-0.636309800095197,
9.91696613669794));
#33970=CARTESIAN_POINT('Ctrl Pts',(-3.17704490789093,-0.319434907277159,
9.88500970337774));
#33971=CARTESIAN_POINT('Ctrl Pts',(-3.15959962456678,-0.158333333333332,
9.87984298008964));
#33972=CARTESIAN_POINT('Ctrl Pts',(-3.14628700527777,0.158333333333334,
9.89543280925802));
#33973=CARTESIAN_POINT('Ctrl Pts',(-3.15117622767193,0.319434907277167,
9.91533710840653));
#33974=CARTESIAN_POINT('Ctrl Pts',(-3.18969432988981,0.636309800095206,
9.98078487986183));
#33975=CARTESIAN_POINT('Ctrl Pts',(-3.22135665799746,0.79477268400084,10.0255893689635));
#33976=CARTESIAN_POINT('Ctrl Pts',(-3.30972802388306,1.06847604194511,10.133397568411));
#33977=CARTESIAN_POINT('Ctrl Pts',(-3.35748906958219,1.18514270861178,10.1886391816766));
#33978=CARTESIAN_POINT('Ctrl Pts',(-3.4147584711704,1.3,10.2524562333546));
#33979=CARTESIAN_POINT('Ctrl Pts',(-3.54336535262991,-1.3,10.1021575829215));
#33980=CARTESIAN_POINT('Ctrl Pts',(-3.47090355778975,-1.18514270861178,
10.0561105004446));
#33981=CARTESIAN_POINT('Ctrl Pts',(-3.40898836153053,-1.06847604194512,
10.0174129929737));
#33982=CARTESIAN_POINT('Ctrl Pts',(-3.29031662464092,-0.794772684000851,
9.94499299784744));
#33983=CARTESIAN_POINT('Ctrl Pts',(-3.24422091196343,-0.636309800095197,
9.91696613669794));
#33984=CARTESIAN_POINT('Ctrl Pts',(-3.17704490789093,-0.319434907277159,
9.88500970337774));
#33985=CARTESIAN_POINT('Ctrl Pts',(-3.15959962456678,-0.158333333333332,
9.87984298008964));
#33986=CARTESIAN_POINT('Ctrl Pts',(-3.14628700527777,0.158333333333334,
9.89543280925802));
#33987=CARTESIAN_POINT('Ctrl Pts',(-3.15117622767194,0.319434907277167,
9.91533710840653));
#33988=CARTESIAN_POINT('Ctrl Pts',(-3.18969432988982,0.636309800095206,
9.98078487986184));
#33989=CARTESIAN_POINT('Ctrl Pts',(-3.22135665799746,0.79477268400084,10.0255893689635));
#33990=CARTESIAN_POINT('Ctrl Pts',(-3.30972802388306,1.06847604194511,10.133397568411));
#33991=CARTESIAN_POINT('Ctrl Pts',(-3.35748906958219,1.18514270861178,10.1886391816766));
#33992=CARTESIAN_POINT('Ctrl Pts',(-3.4147584711704,1.3,10.2524562333546));
#33993=CARTESIAN_POINT('Ctrl Pts',(-3.54336535262998,-1.30000000000011,
10.1021575829215));
#33994=CARTESIAN_POINT('Ctrl Pts',(-3.47090355778979,-1.18514270861186,
10.0561105004446));
#33995=CARTESIAN_POINT('Ctrl Pts',(-3.40898836153054,-1.06847604194515,
10.0174129929738));
#33996=CARTESIAN_POINT('Ctrl Pts',(-3.29031662464092,-0.794772684000851,
9.94499299784743));
#33997=CARTESIAN_POINT('Ctrl Pts',(-3.24422091196343,-0.636309800095196,
9.91696613669794));
#33998=CARTESIAN_POINT('Ctrl Pts',(-3.17704490789093,-0.319434907277159,
9.88500970337773));
#33999=CARTESIAN_POINT('Ctrl Pts',(-3.15959962456677,-0.158333333333332,
9.87984298008964));
#34000=CARTESIAN_POINT('Ctrl Pts',(-3.14628700527777,0.158333333333334,
9.89543280925802));
#34001=CARTESIAN_POINT('Ctrl Pts',(-3.15117622767193,0.319434907277167,
9.91533710840652));
#34002=CARTESIAN_POINT('Ctrl Pts',(-3.18969432988981,0.636309800095206,
9.98078487986183));
#34003=CARTESIAN_POINT('Ctrl Pts',(-3.22135665799746,0.79477268400084,10.0255893689635));
#34004=CARTESIAN_POINT('Ctrl Pts',(-3.30972802388312,1.06847604194529,10.133397568411));
#34005=CARTESIAN_POINT('Ctrl Pts',(-3.35748906958234,1.18514270861213,10.1886391816768));
#34006=CARTESIAN_POINT('Ctrl Pts',(-3.41475847117067,1.30000000000053,10.2524562333549));
#34007=CARTESIAN_POINT('Ctrl Pts',(-3.55210218155249,-1.30000000000011,
10.102668195856));
#34008=CARTESIAN_POINT('Ctrl Pts',(-3.4791120609986,-1.18514270861186,10.0570584190558));
#34009=CARTESIAN_POINT('Ctrl Pts',(-3.41699686806357,-1.06847604194515,
10.0182954880324));
#34010=CARTESIAN_POINT('Ctrl Pts',(-3.29862160460325,-0.794772684000851,
9.94456294632176));
#34011=CARTESIAN_POINT('Ctrl Pts',(-3.25416255203501,-0.636309800095196,
9.91327450453827));
#34012=CARTESIAN_POINT('Ctrl Pts',(-3.18775359145326,-0.319434907277159,
9.87971474158285));
#34013=CARTESIAN_POINT('Ctrl Pts',(-3.17014714932986,-0.158333333333332,
9.8750691092973));
#34014=CARTESIAN_POINT('Ctrl Pts',(-3.15675867145257,0.158333333333334,
9.89088328771536));
#34015=CARTESIAN_POINT('Ctrl Pts',(-3.16161671556929,0.319434907277167,
9.91074553866713));
#34016=CARTESIAN_POINT('Ctrl Pts',(-3.19945051410825,0.636309800095206,
9.97773483059028));
#34017=CARTESIAN_POINT('Ctrl Pts',(-3.22998252758134,0.79477268400084,10.0248426763756));
#34018=CARTESIAN_POINT('Ctrl Pts',(-3.31797563069844,1.06847604194529,10.1340934432942));
#34019=CARTESIAN_POINT('Ctrl Pts',(-3.36577675439403,1.18514270861213,10.1896775761499));
#34020=CARTESIAN_POINT('Ctrl Pts',(-3.42329004791162,1.30000000000053,10.2535552330021));
#34021=CARTESIAN_POINT('Ctrl Pts',(-3.5635999009408,-1.30000000000012,10.1069613837584));
#34022=CARTESIAN_POINT('Ctrl Pts',(-3.49195235234982,-1.18514270861186,
10.0639305254688));
#34023=CARTESIAN_POINT('Ctrl Pts',(-3.4311052249638,-1.06847604194516,10.0264789131465));
#34024=CARTESIAN_POINT('Ctrl Pts',(-3.31548732187626,-0.794772684000854,
9.95284737082135));
#34025=CARTESIAN_POINT('Ctrl Pts',(-3.27312737539359,-0.636309800095199,
9.91645281846877));
#34026=CARTESIAN_POINT('Ctrl Pts',(-3.20798504741422,-0.319434907277159,
9.88032500074145));
#34027=CARTESIAN_POINT('Ctrl Pts',(-3.18944580480551,-0.158333333333333,
9.87534702119606));
#34028=CARTESIAN_POINT('Ctrl Pts',(-3.17599570552034,0.158333333333335,
9.89131075156943));
#34029=CARTESIAN_POINT('Ctrl Pts',(-3.18186432348549,0.319434907277169,
9.91157121719164));
#34030=CARTESIAN_POINT('Ctrl Pts',(-3.21802203393935,0.636309800095209,
9.98160364984369));
#34031=CARTESIAN_POINT('Ctrl Pts',(-3.24556763131071,0.794772684000842,
10.0345895015107));
#34032=CARTESIAN_POINT('Ctrl Pts',(-3.33084003434444,1.06847604194529,10.1437070747227));
#34033=CARTESIAN_POINT('Ctrl Pts',(-3.37760980803081,1.18514270861214,10.1977620137398));
#34034=CARTESIAN_POINT('Ctrl Pts',(-3.43423809178417,1.30000000000053,10.2586389375353));
#34035=CARTESIAN_POINT('Ctrl Pts',(-3.58052453593308,-1.30000000000012,
10.1131512829018));
#34036=CARTESIAN_POINT('Ctrl Pts',(-3.51182111180035,-1.18514270861186,
10.0723212585934));
#34037=CARTESIAN_POINT('Ctrl Pts',(-3.45326554656784,-1.06847604194516,
10.03632181748));
#34038=CARTESIAN_POINT('Ctrl Pts',(-3.34143406101177,-0.794772684000854,
9.96431552037965));
#34039=CARTESIAN_POINT('Ctrl Pts',(-3.29954742189089,-0.6363098000952,9.92639412658323));
#34040=CARTESIAN_POINT('Ctrl Pts',(-3.23531051004868,-0.319434907277161,
9.88931318271086));
#34041=CARTESIAN_POINT('Ctrl Pts',(-3.21611582752958,-0.158333333333333,
9.88302883410783));
#34042=CARTESIAN_POINT('Ctrl Pts',(-3.20259452330713,0.158333333333335,
9.89905411840604));
#34043=CARTESIAN_POINT('Ctrl Pts',(-3.20923276053098,0.319434907277168,
9.92040043925532));
#34044=CARTESIAN_POINT('Ctrl Pts',(-3.2439624010757,0.636309800095209,9.99208593067343));
#34045=CARTESIAN_POINT('Ctrl Pts',(-3.26993455454521,0.794772684000845,
10.0481295568208));
#34046=CARTESIAN_POINT('Ctrl Pts',(-3.35136767971977,1.0684760419453,10.1557832977204));
#34047=CARTESIAN_POINT('Ctrl Pts',(-3.39607665566982,1.18514270861214,10.2081250226386));
#34048=CARTESIAN_POINT('Ctrl Pts',(-3.4502452250765,1.30000000000053,10.2662091570036));
#34049=CARTESIAN_POINT('Ctrl Pts',(-3.59470999228296,-1.30000000000012,
10.1179996604394));
#34050=CARTESIAN_POINT('Ctrl Pts',(-3.52841604334897,-1.18514270861187,
10.0784975008717));
#34051=CARTESIAN_POINT('Ctrl Pts',(-3.47152795348144,-1.06847604194516,
10.0435856794783));
#34052=CARTESIAN_POINT('Ctrl Pts',(-3.36183450154324,-0.794772684000855,
9.97353698745057));
#34053=CARTESIAN_POINT('Ctrl Pts',(-3.31850387428926,-0.636309800095199,
9.93665114702491));
#34054=CARTESIAN_POINT('Ctrl Pts',(-3.25436105612193,-0.31943490727716,
9.89946741885329));
#34055=CARTESIAN_POINT('Ctrl Pts',(-3.23540186323813,-0.158333333333333,
9.89122756687286));
#34056=CARTESIAN_POINT('Ctrl Pts',(-3.22220303021708,0.158333333333335,
9.90677602232352));
#34057=CARTESIAN_POINT('Ctrl Pts',(-3.22944979183797,0.31943490727717,9.92886386820246));
#34058=CARTESIAN_POINT('Ctrl Pts',(-3.26367984413207,0.63630980009521,10.0011823983456));
#34059=CARTESIAN_POINT('Ctrl Pts',(-3.28915985991411,0.794772684000842,
10.0588476958572));
#34060=CARTESIAN_POINT('Ctrl Pts',(-3.36817452647295,1.06847604194529,10.1650030429831));
#34061=CARTESIAN_POINT('Ctrl Pts',(-3.41144891624779,1.18514270861214,10.2159886719713));
#34062=CARTESIAN_POINT('Ctrl Pts',(-3.46379517442606,1.30000000000054,10.2720092136201));
#34063=CARTESIAN_POINT('Ctrl Pts',(-3.60911751064946,-1.30000000000012,
10.1227295726391));
#34064=CARTESIAN_POINT('Ctrl Pts',(-3.54550367467917,-1.18514270861187,
10.0846191774548));
#34065=CARTESIAN_POINT('Ctrl Pts',(-3.49047558704248,-1.06847604194516,
10.0508755280719));
#34066=CARTESIAN_POINT('Ctrl Pts',(-3.38318449249417,-0.794772684000856,
9.98300900396935));
#34067=CARTESIAN_POINT('Ctrl Pts',(-3.33845114784564,-0.636309800095201,
9.94721788326197));
#34068=CARTESIAN_POINT('Ctrl Pts',(-3.2741201089056,-0.319434907277161,
9.91048396957203));
#34069=CARTESIAN_POINT('Ctrl Pts',(-3.25510443899921,-0.158333333333333,
9.9005970671488));
#34070=CARTESIAN_POINT('Ctrl Pts',(-3.2413673604884,0.158333333333335,9.91683651347412));
#34071=CARTESIAN_POINT('Ctrl Pts',(-3.24779972547716,0.319434907277169,
9.94167544852661));
#34072=CARTESIAN_POINT('Ctrl Pts',(-3.28179917085832,0.636309800095211,
10.0141103141042));
#34073=CARTESIAN_POINT('Ctrl Pts',(-3.30913046338384,0.794772684000846,
10.070145021745));
#34074=CARTESIAN_POINT('Ctrl Pts',(-3.38609183274489,1.0684760419453,10.1737301684728));
#34075=CARTESIAN_POINT('Ctrl Pts',(-3.42768849705096,1.18514270861214,10.2233422864552));
#34076=CARTESIAN_POINT('Ctrl Pts',(-3.47756810056647,1.30000000000053,10.2777283506095));
#34077=CARTESIAN_POINT('Ctrl Pts',(-3.62418184228244,-1.30000000000013,
10.1262166523165));
#34078=CARTESIAN_POINT('Ctrl Pts',(-3.56307216446774,-1.18514270861187,
10.0894944243691));
#34079=CARTESIAN_POINT('Ctrl Pts',(-3.50973124244813,-1.06847604194516,
10.0569771634264));
#34080=CARTESIAN_POINT('Ctrl Pts',(-3.40445042178884,-0.794772684000856,
9.99157010057452));
#34081=CARTESIAN_POINT('Ctrl Pts',(-3.35822909918292,-0.636309800095201,
9.95703313191003));
#34082=CARTESIAN_POINT('Ctrl Pts',(-3.29303524674374,-0.319434907277161,
9.92167902532558));
#34083=CARTESIAN_POINT('Ctrl Pts',(-3.27288063940016,-0.158333333333333,
9.91174316405932));
#34084=CARTESIAN_POINT('Ctrl Pts',(-3.25874017194707,0.158333333333336,
9.92847582885122));
#34085=CARTESIAN_POINT('Ctrl Pts',(-3.26576122781523,0.319434907277169,
9.9539858175574));
#34086=CARTESIAN_POINT('Ctrl Pts',(-3.30010095085377,0.636309800095211,
10.0257830146997));
#34087=CARTESIAN_POINT('Ctrl Pts',(-3.32891779836226,0.794772684000847,
10.0807296485886));
#34088=CARTESIAN_POINT('Ctrl Pts',(-3.40377037538339,1.0684760419453,10.1821617920228));
#34089=CARTESIAN_POINT('Ctrl Pts',(-3.44366765324861,1.18514270861214,10.230642064719));
#34090=CARTESIAN_POINT('Ctrl Pts',(-3.49106130194792,1.30000000000053,10.2836963936501));
#34091=CARTESIAN_POINT('Ctrl Pts',(-3.64724297519888,-1.30000000000012,
10.1335969392188));
#34092=CARTESIAN_POINT('Ctrl Pts',(-3.59027824508293,-1.18514270861187,
10.0990538498164));
#34093=CARTESIAN_POINT('Ctrl Pts',(-3.53982856865866,-1.06847604194516,
10.0683339334076));
#34094=CARTESIAN_POINT('Ctrl Pts',(-3.4383308010552,-0.794772684000858,
10.0061970754434));
#34095=CARTESIAN_POINT('Ctrl Pts',(-3.39043018200663,-0.636309800095201,
9.97259895733519));
#34096=CARTESIAN_POINT('Ctrl Pts',(-3.32428145980048,-0.319434907277161,
9.93882474384284));
#34097=CARTESIAN_POINT('Ctrl Pts',(-3.30202986962655,-0.158333333333333,
9.92911371588886));
#34098=CARTESIAN_POINT('Ctrl Pts',(-3.28753271539489,0.158333333333336,
9.94629507157737));
#34099=CARTESIAN_POINT('Ctrl Pts',(-3.29613726709655,0.31943490727717,9.97221235514739));
#34100=CARTESIAN_POINT('Ctrl Pts',(-3.33102470537107,0.636309800095211,
10.0429699617166));
#34101=CARTESIAN_POINT('Ctrl Pts',(-3.36144877189567,0.794772684000847,
10.0970951480506));
#34102=CARTESIAN_POINT('Ctrl Pts',(-3.43280627831961,1.0684760419453,10.1949767111377));
#34103=CARTESIAN_POINT('Ctrl Pts',(-3.47005463965042,1.18514270861214,10.2414003155185));
#34104=CARTESIAN_POINT('Ctrl Pts',(-3.51366334183729,1.30000000000053,10.291878222489));
#34105=CARTESIAN_POINT('Ctrl Pts',(-3.67397691592538,-1.30000000000014,
10.1404382070295));
#34106=CARTESIAN_POINT('Ctrl Pts',(-3.62202609023204,-1.18514270861188,
10.1075758257365));
#34107=CARTESIAN_POINT('Ctrl Pts',(-3.5750265102802,-1.06847604194518,10.0784238599931));
#34108=CARTESIAN_POINT('Ctrl Pts',(-3.47788644651384,-0.794772684000867,
10.0196487894806));
#34109=CARTESIAN_POINT('Ctrl Pts',(-3.42747667068375,-0.63630980009521,
9.98822773199515));
#34110=CARTESIAN_POINT('Ctrl Pts',(-3.36014651860966,-0.319434907277166,
9.95652681394419));
#34111=CARTESIAN_POINT('Ctrl Pts',(-3.33602530341171,-0.158333333333335,
9.94652219551044));
#34112=CARTESIAN_POINT('Ctrl Pts',(-3.32078017859728,0.158333333333338,
9.96469262459665));
#34113=CARTESIAN_POINT('Ctrl Pts',(-3.33018258285647,0.319434907277173,
9.99224309046664));
#34114=CARTESIAN_POINT('Ctrl Pts',(-3.3653874499001,0.636309800095219,10.0622280921016));
#34115=CARTESIAN_POINT('Ctrl Pts',(-3.3983426815493,0.794772684000859,10.1144671820177));
#34116=CARTESIAN_POINT('Ctrl Pts',(-3.46559427745884,1.06847604194531,10.208815312985));
#34117=CARTESIAN_POINT('Ctrl Pts',(-3.4996381254075,1.18514270861215,10.2533737903643));
#34118=CARTESIAN_POINT('Ctrl Pts',(-3.53861509735278,1.30000000000055,10.3016509351699));
#34119=CARTESIAN_POINT('Ctrl Pts',(-3.70101609997424,-1.30000000000014,
10.1467971727461));
#34120=CARTESIAN_POINT('Ctrl Pts',(-3.65404756630734,-1.18514270861189,
10.1157658379245));
#34121=CARTESIAN_POINT('Ctrl Pts',(-3.61053545627869,-1.06847604194518,
10.0882065343632));
#34122=CARTESIAN_POINT('Ctrl Pts',(-3.51799880760425,-0.794772684000871,
10.0325601167053));
#34123=CARTESIAN_POINT('Ctrl Pts',(-3.46577617204281,-0.636309800095214,
10.0022958257452));
#34124=CARTESIAN_POINT('Ctrl Pts',(-3.39714216002861,-0.319434907277169,
9.97288211177708));
#34125=CARTESIAN_POINT('Ctrl Pts',(-3.36997360449769,-0.158333333333336,
9.96426715395719));
#34126=CARTESIAN_POINT('Ctrl Pts',(-3.35430928158604,0.158333333333338,
9.98302909004582));
#34127=CARTESIAN_POINT('Ctrl Pts',(-3.36619456824415,0.319434907277173,
10.0099446275918));
#34128=CARTESIAN_POINT('Ctrl Pts',(-3.40214530271569,0.636309800095221,
10.0785148041599));
#34129=CARTESIAN_POINT('Ctrl Pts',(-3.43676382154103,0.794772684000866,
10.1299492333641));
#34130=CARTESIAN_POINT('Ctrl Pts',(-3.49950020459075,1.06847604194532,10.2211856027531));
#34131=CARTESIAN_POINT('Ctrl Pts',(-3.53019839035192,1.18514270861216,10.2640078435357));
#34132=CARTESIAN_POINT('Ctrl Pts',(-3.56443850626412,1.30000000000055,10.3101594814332));
#34133=CARTESIAN_POINT('Ctrl Pts',(-3.71878759513281,-1.30000000000015,
10.1514335393157));
#34134=CARTESIAN_POINT('Ctrl Pts',(-3.67489198161409,-1.18514270861189,
10.1220295507434));
#34135=CARTESIAN_POINT('Ctrl Pts',(-3.63358998434732,-1.06847604194518,
10.0957168890385));
#34136=CARTESIAN_POINT('Ctrl Pts',(-3.54416588061798,-0.794772684000874,
10.0420709601515));
#34137=CARTESIAN_POINT('Ctrl Pts',(-3.49117463237641,-0.636309800095215,
10.0117948092667));
#34138=CARTESIAN_POINT('Ctrl Pts',(-3.42225724530448,-0.319434907277169,
9.98301045242503));
#34139=CARTESIAN_POINT('Ctrl Pts',(-3.3937754601307,-0.158333333333337,
9.97433581792676));
#34140=CARTESIAN_POINT('Ctrl Pts',(-3.37779065274495,0.158333333333339,
9.99355658156853));
#34141=CARTESIAN_POINT('Ctrl Pts',(-3.3905367988662,0.319434907277174,10.0211696006522));
#34142=CARTESIAN_POINT('Ctrl Pts',(-3.42638674628363,0.636309800095223,
10.0896804548971));
#34143=CARTESIAN_POINT('Ctrl Pts',(-3.46182891275466,0.794772684000866,
10.1410408923148));
#34144=CARTESIAN_POINT('Ctrl Pts',(-3.52141617533198,1.06847604194532,10.23043352704));
#34145=CARTESIAN_POINT('Ctrl Pts',(-3.54990764801574,1.18514270861216,10.2720718272872));
#34146=CARTESIAN_POINT('Ctrl Pts',(-3.58109747533919,1.30000000000056,10.3166536685326));
#34147=CARTESIAN_POINT('Ctrl Pts',(-3.73401038434222,-1.30000000000015,
10.1545818971217));
#34148=CARTESIAN_POINT('Ctrl Pts',(-3.69324257501991,-1.18514270861189,
10.1255598410473));
#34149=CARTESIAN_POINT('Ctrl Pts',(-3.65411138747389,-1.06847604194518,
10.0997261594864));
#34150=CARTESIAN_POINT('Ctrl Pts',(-3.56749143978366,-0.794772684000874,
10.0474109700294));
#34151=CARTESIAN_POINT('Ctrl Pts',(-3.51312199982019,-0.636309800095216,
10.0184536727513));
#34152=CARTESIAN_POINT('Ctrl Pts',(-3.44347872018291,-0.319434907277169,
9.99102543581514));
#34153=CARTESIAN_POINT('Ctrl Pts',(-3.41355347653865,-0.158333333333337,
9.98280749464256));
#34154=CARTESIAN_POINT('Ctrl Pts',(-3.39726080503651,0.158333333333339,
10.0024891622436));
#34155=CARTESIAN_POINT('Ctrl Pts',(-3.41104041731569,0.319434907277174,
10.0302188284627));
#34156=CARTESIAN_POINT('Ctrl Pts',(-3.44719718804243,0.636309800095223,
10.0980833659227));
#34157=CARTESIAN_POINT('Ctrl Pts',(-3.48378843925299,0.794772684000865,
10.1486515677517));
#34158=CARTESIAN_POINT('Ctrl Pts',(-3.54080406639039,1.06847604194532,10.2364196566261));
#34159=CARTESIAN_POINT('Ctrl Pts',(-3.56736250509839,1.18514270861217,10.2772146646551));
#34160=CARTESIAN_POINT('Ctrl Pts',(-3.5957994301638,1.30000000000056,10.3208131271675));
#34161=CARTESIAN_POINT('Ctrl Pts',(-3.74458338262462,-1.30000000000015,
10.1569162443583));
#34162=CARTESIAN_POINT('Ctrl Pts',(-3.70576961061605,-1.18514270861189,
10.1285656394162));
#34163=CARTESIAN_POINT('Ctrl Pts',(-3.6680144134445,-1.06847604194519,10.1033120089907));
#34164=CARTESIAN_POINT('Ctrl Pts',(-3.58323787471761,-0.794772684000877,
10.0521257014175));
#34165=CARTESIAN_POINT('Ctrl Pts',(-3.52812698520538,-0.636309800095216,
10.0236832244191));
#34166=CARTESIAN_POINT('Ctrl Pts',(-3.45819987631133,-0.319434907277169,
9.99683436947552));
#34167=CARTESIAN_POINT('Ctrl Pts',(-3.42748734455854,-0.158333333333337,
9.98859811477711));
#34168=CARTESIAN_POINT('Ctrl Pts',(-3.4111088685937,0.158333333333339,10.0084029104395));
#34169=CARTESIAN_POINT('Ctrl Pts',(-3.42563400563729,0.319434907277174,
10.0361870918687));
#34170=CARTESIAN_POINT('Ctrl Pts',(-3.46181011952091,0.636309800095224,
10.1039001131025));
#34171=CARTESIAN_POINT('Ctrl Pts',(-3.49871339236154,0.794772684000867,
10.1546653062899));
#34172=CARTESIAN_POINT('Ctrl Pts',(-3.55391749921246,1.06847604194532,10.2413119292474));
#34173=CARTESIAN_POINT('Ctrl Pts',(-3.57923030510806,1.18514270861217,10.2813512158437));
#34174=CARTESIAN_POINT('Ctrl Pts',(-3.60596010455725,1.30000000000056,10.3239236765318));
#34175=CARTESIAN_POINT('Ctrl Pts',(-3.75070071224822,-1.30000000000015,
10.158117784076));
#34176=CARTESIAN_POINT('Ctrl Pts',(-3.71293555971019,-1.18514270861189,
10.1302712463608));
#34177=CARTESIAN_POINT('Ctrl Pts',(-3.67592652198007,-1.06847604194519,
10.1054206976937));
#34178=CARTESIAN_POINT('Ctrl Pts',(-3.59217501765742,-0.794772684000877,
10.0549322929838));
#34179=CARTESIAN_POINT('Ctrl Pts',(-3.53672118512614,-0.636309800095217,
10.0266422905552));
#34180=CARTESIAN_POINT('Ctrl Pts',(-3.46669189355701,-0.319434907277169,
10.0000273475389));
#34181=CARTESIAN_POINT('Ctrl Pts',(-3.43560761307563,-0.158333333333337,
9.99166315756603));
#34182=CARTESIAN_POINT('Ctrl Pts',(-3.41913503061073,0.158333333333339,
10.0116063008335));
#34183=CARTESIAN_POINT('Ctrl Pts',(-3.43393288855804,0.319434907277175,
10.0396543473314));
#34184=CARTESIAN_POINT('Ctrl Pts',(-3.47002952133634,0.636309800095224,
10.1074201856546));
#34185=CARTESIAN_POINT('Ctrl Pts',(-3.50714515538911,0.794772684000867,
10.1582504041928));
#34186=CARTESIAN_POINT('Ctrl Pts',(-3.56125634144506,1.06847604194532,10.2443441091965));
#34187=CARTESIAN_POINT('Ctrl Pts',(-3.5858219639986,1.18514270861217,10.2840044287812));
#34188=CARTESIAN_POINT('Ctrl Pts',(-3.61153048167909,1.30000000000056,10.3260582931406));
#34189=CARTESIAN_POINT('Ctrl Pts',(-3.76607211082024,-1.30000000000015,
10.1609742455453));
#34190=CARTESIAN_POINT('Ctrl Pts',(-3.73099751271949,-1.18514270861189,
10.1342611827223));
#34191=CARTESIAN_POINT('Ctrl Pts',(-3.69590262596997,-1.06847604194519,
10.1103306661676));
#34192=CARTESIAN_POINT('Ctrl Pts',(-3.61477954603314,-0.794772684000878,
10.0614746241691));
#34193=CARTESIAN_POINT('Ctrl Pts',(-3.55846721318748,-0.636309800095217,
10.0335856640069));
#34194=CARTESIAN_POINT('Ctrl Pts',(-3.48812651758648,-0.319434907277169,
10.0076608129102));
#34195=CARTESIAN_POINT('Ctrl Pts',(-3.45597529768671,-0.158333333333337,
9.99920817797782));
#34196=CARTESIAN_POINT('Ctrl Pts',(-3.43925943579227,0.158333333333339,
10.0195222842871));
#34197=CARTESIAN_POINT('Ctrl Pts',(-3.45479591099045,0.319434907277175,
10.0481423271903));
#34198=CARTESIAN_POINT('Ctrl Pts',(-3.49088163105331,0.636309800095224,
10.1157443641273));
#34199=CARTESIAN_POINT('Ctrl Pts',(-3.52886328959088,0.794772684000867,
10.1661993892385));
#34200=CARTESIAN_POINT('Ctrl Pts',(-3.58023784918361,1.06847604194532,10.250919595152));
#34201=CARTESIAN_POINT('Ctrl Pts',(-3.60284905222399,1.18514270861217,10.2897719074366));
#34202=CARTESIAN_POINT('Ctrl Pts',(-3.62583331507207,1.30000000000056,10.3308042940587));
#34203=CARTESIAN_POINT('Ctrl Pts',(-3.7915912137151,-1.30000000000016,10.166868855423));
#34204=CARTESIAN_POINT('Ctrl Pts',(-3.76166361794079,-1.1851427086119,10.1410540242383));
#34205=CARTESIAN_POINT('Ctrl Pts',(-3.73019934521846,-1.0684760419452,10.1180149543402));
#34206=CARTESIAN_POINT('Ctrl Pts',(-3.65396054966258,-0.794772684000883,
10.0712026577869));
#34207=CARTESIAN_POINT('Ctrl Pts',(-3.59579091152071,-0.636309800095222,
10.0447592722612));
#34208=CARTESIAN_POINT('Ctrl Pts',(-3.52464131310718,-0.319434907277172,
10.0204798922187));
#34209=CARTESIAN_POINT('Ctrl Pts',(-3.49014293988893,-0.158333333333338,
10.0126931881361));
#34210=CARTESIAN_POINT('Ctrl Pts',(-3.47330320399168,0.15833333333334,10.0331780310056));
#34211=CARTESIAN_POINT('Ctrl Pts',(-3.49118822947503,0.319434907277177,
10.0610441144754));
#34212=CARTESIAN_POINT('Ctrl Pts',(-3.52757536198082,0.636309800095229,
10.1278755444044));
#34213=CARTESIAN_POINT('Ctrl Pts',(-3.56642191385663,0.794772684000873,
10.1786655205029));
#34214=CARTESIAN_POINT('Ctrl Pts',(-3.61303850726719,1.06847604194533,10.2612448037204));
#34215=CARTESIAN_POINT('Ctrl Pts',(-3.63234446820997,1.18514270861218,10.2987099793951));
#34216=CARTESIAN_POINT('Ctrl Pts',(-3.6507777941231,1.30000000000058,10.3378948189035));
#34217=CARTESIAN_POINT('Ctrl Pts',(-3.82904434197742,-1.30000000000017,
10.1725573801911));
#34218=CARTESIAN_POINT('Ctrl Pts',(-3.80603578149659,-1.18514270861191,
10.1485789281661));
#34219=CARTESIAN_POINT('Ctrl Pts',(-3.7794981298758,-1.0684760419452,10.1271271007892));
#34220=CARTESIAN_POINT('Ctrl Pts',(-3.71003793926713,-0.794772684000884,
10.0834060965121));
#34221=CARTESIAN_POINT('Ctrl Pts',(-3.64975703515377,-0.636309800095225,
10.0581463894763));
#34222=CARTESIAN_POINT('Ctrl Pts',(-3.57770260659287,-0.319434907277174,
10.0359093284447));
#34223=CARTESIAN_POINT('Ctrl Pts',(-3.54024857503223,-0.158333333333339,
10.02866262349));
#34224=CARTESIAN_POINT('Ctrl Pts',(-3.52260595669352,0.158333333333341,
10.0504829942974));
#34225=CARTESIAN_POINT('Ctrl Pts',(-3.54225771277102,0.319434907277179,
10.0797339881208));
#34226=CARTESIAN_POINT('Ctrl Pts',(-3.57870060819418,0.636309800095233,
10.1460429455198));
#34227=CARTESIAN_POINT('Ctrl Pts',(-3.62006023327149,0.794772684000877,
10.195179164837));
#34228=CARTESIAN_POINT('Ctrl Pts',(-3.65986116385648,1.06847604194534,10.2748722818108));
#34229=CARTESIAN_POINT('Ctrl Pts',(-3.67422220811065,1.18514270861218,10.3108252288688));
#34230=CARTESIAN_POINT('Ctrl Pts',(-3.68571594853856,1.30000000000058,10.3482349255678));
#34231=CARTESIAN_POINT('Ctrl Pts',(-3.85796273426452,-1.30000000000018,
10.178266574707));
#34232=CARTESIAN_POINT('Ctrl Pts',(-3.84081716435615,-1.18514270861192,
10.1550010588959));
#34233=CARTESIAN_POINT('Ctrl Pts',(-3.81847119538827,-1.06847604194521,
10.134256092061));
#34234=CARTESIAN_POINT('Ctrl Pts',(-3.75483357461295,-0.794772684000895,
10.0921540410251));
#34235=CARTESIAN_POINT('Ctrl Pts',(-3.69289320873997,-0.636309800095232,
10.0678948309938));
#34236=CARTESIAN_POINT('Ctrl Pts',(-3.62016465998514,-0.319434907277177,
10.0472382191901));
#34237=CARTESIAN_POINT('Ctrl Pts',(-3.57998281606451,-0.158333333333341,
10.0410808411431));
#34238=CARTESIAN_POINT('Ctrl Pts',(-3.56213974746018,0.158333333333343,
10.0632503369065));
#34239=CARTESIAN_POINT('Ctrl Pts',(-3.58443579868164,0.319434907277182,
10.0915216009712));
#34240=CARTESIAN_POINT('Ctrl Pts',(-3.62090632733795,0.636309800095239,
10.1574491524359));
#34241=CARTESIAN_POINT('Ctrl Pts',(-3.66277298302753,0.794772684000885,
10.2077161021715));
#34242=CARTESIAN_POINT('Ctrl Pts',(-3.69695770961202,1.06847604194535,10.2855472711458));
#34243=CARTESIAN_POINT('Ctrl Pts',(-3.70754953577959,1.1851427086122,10.3201022877664));
#34244=CARTESIAN_POINT('Ctrl Pts',(-3.71393588664526,1.3000000000006,10.3555220918877));
#34245=CARTESIAN_POINT('Ctrl Pts',(-3.88331383738313,-1.30000000000019,
10.1812451374793));
#34246=CARTESIAN_POINT('Ctrl Pts',(-3.87071504559958,-1.18514270861193,
10.1592808151736));
#34247=CARTESIAN_POINT('Ctrl Pts',(-3.85164934528007,-1.06847604194522,
10.1395770461112));
#34248=CARTESIAN_POINT('Ctrl Pts',(-3.792663911043,-0.794772684000897,10.0992797280657));
#34249=CARTESIAN_POINT('Ctrl Pts',(-3.72966428221427,-0.636309800095233,
10.0752174409862));
#34250=CARTESIAN_POINT('Ctrl Pts',(-3.65656987687846,-0.319434907277177,
10.055565012233));
#34251=CARTESIAN_POINT('Ctrl Pts',(-3.6145153650832,-0.158333333333341,
10.0496759387229));
#34252=CARTESIAN_POINT('Ctrl Pts',(-3.59606894268156,0.158333333333343,
10.0729123621764));
#34253=CARTESIAN_POINT('Ctrl Pts',(-3.61922110816113,0.319434907277183,
10.1026755664624));
#34254=CARTESIAN_POINT('Ctrl Pts',(-3.65567016343661,0.636309800095241,
10.1683599528127));
#34255=CARTESIAN_POINT('Ctrl Pts',(-3.69948766699002,0.794772684000886,
10.2169949438957));
#34256=CARTESIAN_POINT('Ctrl Pts',(-3.72910291164311,1.06847604194535,10.2929745585285));
#34257=CARTESIAN_POINT('Ctrl Pts',(-3.73633364482524,1.1851427086122,10.3266612256361));
#34258=CARTESIAN_POINT('Ctrl Pts',(-3.73797576913212,1.3000000000006,10.3611457999992));
#34259=CARTESIAN_POINT('Ctrl Pts',(-3.90174032585728,-1.3000000000002,10.1844798363048));
#34260=CARTESIAN_POINT('Ctrl Pts',(-3.89300705345891,-1.18514270861193,
10.1626302526796));
#34261=CARTESIAN_POINT('Ctrl Pts',(-3.87667429073231,-1.06847604194522,
10.1431943317848));
#34262=CARTESIAN_POINT('Ctrl Pts',(-3.82138599854488,-0.794772684000903,
10.1038695101342));
#34263=CARTESIAN_POINT('Ctrl Pts',(-3.75686382275297,-0.636309800095237,
10.0813423020077));
#34264=CARTESIAN_POINT('Ctrl Pts',(-3.6835405027242,-0.319434907277179,
10.0623901632465));
#34265=CARTESIAN_POINT('Ctrl Pts',(-3.64041659361247,-0.158333333333342,
10.0560697623108));
#34266=CARTESIAN_POINT('Ctrl Pts',(-3.62215778243213,0.158333333333344,
10.0789889568926));
#34267=CARTESIAN_POINT('Ctrl Pts',(-3.64693561561035,0.319434907277186,
10.1081907696719));
#34268=CARTESIAN_POINT('Ctrl Pts',(-3.68324480396177,0.636309800095246,
10.1739046182766));
#34269=CARTESIAN_POINT('Ctrl Pts',(-3.72711751271952,0.794772684000892,
10.2237230640728));
#34270=CARTESIAN_POINT('Ctrl Pts',(-3.75286406183021,1.06847604194536,10.299088735948));
#34271=CARTESIAN_POINT('Ctrl Pts',(-3.7575711949502,1.1851427086122,10.3321417122785));
#34272=CARTESIAN_POINT('Ctrl Pts',(-3.75584073408384,1.3000000000006,10.3656246581581));
#34273=CARTESIAN_POINT('Ctrl Pts',(-3.92200665684785,-1.3000000000002,10.187442466889));
#34274=CARTESIAN_POINT('Ctrl Pts',(-3.91700851637555,-1.18514270861194,
10.1665604654));
#34275=CARTESIAN_POINT('Ctrl Pts',(-3.9034222469725,-1.06847604194523,10.1478092117938));
#34276=CARTESIAN_POINT('Ctrl Pts',(-3.8521949508482,-0.794772684000906,
10.1094125186521));
#34277=CARTESIAN_POINT('Ctrl Pts',(-3.78730781975507,-0.636309800095239,
10.0861175764946));
#34278=CARTESIAN_POINT('Ctrl Pts',(-3.71374852816862,-0.31943490727718,
10.0678795136089));
#34279=CARTESIAN_POINT('Ctrl Pts',(-3.6686668503439,-0.158333333333343,
10.0626129675919));
#34280=CARTESIAN_POINT('Ctrl Pts',(-3.64980811405989,0.158333333333344,
10.0866279809606));
#34281=CARTESIAN_POINT('Ctrl Pts',(-3.67550669183711,0.319434907277187,
10.1166464057035));
#34282=CARTESIAN_POINT('Ctrl Pts',(-3.71172018671788,0.636309800095247,
10.1823003800064));
#34283=CARTESIAN_POINT('Ctrl Pts',(-3.75686878802455,0.794772684000892,
10.2313091805914));
#34284=CARTESIAN_POINT('Ctrl Pts',(-3.77883878245198,1.06847604194536,10.3052965512782));
#34285=CARTESIAN_POINT('Ctrl Pts',(-3.78084109508027,1.18514270861221,10.3376124724536));
#34286=CARTESIAN_POINT('Ctrl Pts',(-3.77533572381774,1.30000000000061,10.3702179235365));
#34287=CARTESIAN_POINT('Ctrl Pts',(-3.93787421728648,-1.30000000000021,
10.1891442942232));
#34288=CARTESIAN_POINT('Ctrl Pts',(-3.93601570989885,-1.18514270861194,
10.168468189729));
#34289=CARTESIAN_POINT('Ctrl Pts',(-3.92466395193018,-1.06847604194523,
10.1499934640814));
#34290=CARTESIAN_POINT('Ctrl Pts',(-3.87650781215066,-0.794772684000909,
10.1123987774988));
#34291=CARTESIAN_POINT('Ctrl Pts',(-3.81060836194368,-0.636309800095243,
10.0899431628784));
#34292=CARTESIAN_POINT('Ctrl Pts',(-3.73672414330885,-0.319434907277183,
10.0725578565363));
#34293=CARTESIAN_POINT('Ctrl Pts',(-3.69036900847232,-0.158333333333344,
10.0676607019504));
#34294=CARTESIAN_POINT('Ctrl Pts',(-3.67144693011197,0.158333333333346,
10.0918192063));
#34295=CARTESIAN_POINT('Ctrl Pts',(-3.69840825330412,0.31943490727719,10.1215004566747));
#34296=CARTESIAN_POINT('Ctrl Pts',(-3.73471044748741,0.636309800095253,
10.1868206121894));
#34297=CARTESIAN_POINT('Ctrl Pts',(-3.78053057570353,0.794772684000899,
10.2357323241856));
#34298=CARTESIAN_POINT('Ctrl Pts',(-3.79930689286134,1.06847604194537,10.3091734262881));
#34299=CARTESIAN_POINT('Ctrl Pts',(-3.79908419968581,1.18514270861222,10.3411844214108));
#34300=CARTESIAN_POINT('Ctrl Pts',(-3.79051124136824,1.30000000000062,10.373416479817));
#34301=CARTESIAN_POINT('Ctrl Pts',(-3.95042528865478,-1.30000000000021,
10.1907726542255));
#34302=CARTESIAN_POINT('Ctrl Pts',(-3.95098551996914,-1.18514270861195,
10.1704463443776));
#34303=CARTESIAN_POINT('Ctrl Pts',(-3.94138516874209,-1.06847604194524,
10.1522652425601));
#34304=CARTESIAN_POINT('Ctrl Pts',(-3.8957334585757,-0.794772684000912,
10.1152191199419));
#34305=CARTESIAN_POINT('Ctrl Pts',(-3.82935596711379,-0.636309800095244,
10.0927819243377));
#34306=CARTESIAN_POINT('Ctrl Pts',(-3.75524010088347,-0.319434907277182,
10.0760144773478));
#34307=CARTESIAN_POINT('Ctrl Pts',(-3.70764638659068,-0.158333333333344,
10.0718387952671));
#34308=CARTESIAN_POINT('Ctrl Pts',(-3.68855509195389,0.158333333333346,
10.0963248232461));
#34309=CARTESIAN_POINT('Ctrl Pts',(-3.71647280399642,0.31943490727719,10.1258106403559));
#34310=CARTESIAN_POINT('Ctrl Pts',(-3.75289208497874,0.636309800095253,
10.190775716563));
#34311=CARTESIAN_POINT('Ctrl Pts',(-3.79943225862935,0.794772684000899,
10.2392902622796));
#34312=CARTESIAN_POINT('Ctrl Pts',(-3.81571432852043,1.06847604194537,10.3121932875574));
#34313=CARTESIAN_POINT('Ctrl Pts',(-3.8137112109172,1.18514270861222,10.3439650773515));
#34314=CARTESIAN_POINT('Ctrl Pts',(-3.80265707096503,1.30000000000062,10.3759516386202));
#34315=CARTESIAN_POINT('Ctrl Pts',(-3.95998493006225,-1.30000000000021,
10.1916909496914));
#34316=CARTESIAN_POINT('Ctrl Pts',(-3.96246157838396,-1.18514270861195,
10.1714087627593));
#34317=CARTESIAN_POINT('Ctrl Pts',(-3.95421929895579,-1.06847604194524,
10.1533510482225));
#34318=CARTESIAN_POINT('Ctrl Pts',(-3.91041511719802,-0.794772684000914,
10.1167730914459));
#34319=CARTESIAN_POINT('Ctrl Pts',(-3.84334389128597,-0.636309800095247,
10.0950320918671));
#34320=CARTESIAN_POINT('Ctrl Pts',(-3.76905895310044,-0.319434907277184,
10.0787420572256));
#34321=CARTESIAN_POINT('Ctrl Pts',(-3.7208679411399,-0.158333333333345,
10.0744802704328));
#34322=CARTESIAN_POINT('Ctrl Pts',(-3.70166044317268,0.158333333333347,
10.0991912863336));
#34323=CARTESIAN_POINT('Ctrl Pts',(-3.73008710276877,0.319434907277192,
10.1289200681933));
#34324=CARTESIAN_POINT('Ctrl Pts',(-3.7663820228931,0.636309800095256,10.1940047878435));
#34325=CARTESIAN_POINT('Ctrl Pts',(-3.81322425648508,0.794772684000904,
10.242642154839));
#34326=CARTESIAN_POINT('Ctrl Pts',(-3.82766422345967,1.06847604194537,10.3150922134062));
#34327=CARTESIAN_POINT('Ctrl Pts',(-3.824411638536,1.18514270861223,10.3465324873549));
#34328=CARTESIAN_POINT('Ctrl Pts',(-3.81165594203887,1.30000000000063,10.3780520894376));
#34329=CARTESIAN_POINT('Ctrl Pts',(-3.96796056930311,-1.30000000000022,
10.192428239807));
#34330=CARTESIAN_POINT('Ctrl Pts',(-3.97206870982618,-1.18514270861195,
10.1721128975678));
#34331=CARTESIAN_POINT('Ctrl Pts',(-3.96497989930268,-1.06847604194524,
10.1541138410264));
#34332=CARTESIAN_POINT('Ctrl Pts',(-3.92273613202175,-0.794772684000917,
10.1178835030499));
#34333=CARTESIAN_POINT('Ctrl Pts',(-3.85504424735611,-0.636309800095248,
10.0968054295953));
#34334=CARTESIAN_POINT('Ctrl Pts',(-3.78061951838933,-0.319434907277185,
10.0809165143215));
#34335=CARTESIAN_POINT('Ctrl Pts',(-3.7319573146038,-0.158333333333345,
10.0765407935441));
#34336=CARTESIAN_POINT('Ctrl Pts',(-3.71266131128897,0.158333333333347,
10.1014272047489));
#34337=CARTESIAN_POINT('Ctrl Pts',(-3.74150943516619,0.319434907277192,
10.1313609681455));
#34338=CARTESIAN_POINT('Ctrl Pts',(-3.77768487945715,0.636309800095257,
10.1965736463306));
#34339=CARTESIAN_POINT('Ctrl Pts',(-3.82475685902025,0.794772684000905,
10.2453518195525));
#34340=CARTESIAN_POINT('Ctrl Pts',(-3.83763969446987,1.06847604194538,10.3174666274569));
#34341=CARTESIAN_POINT('Ctrl Pts',(-3.83333732055447,1.18514270861223,10.348647953515));
#34342=CARTESIAN_POINT('Ctrl Pts',(-3.81915607061362,1.30000000000063,10.3797947774065));
#34343=CARTESIAN_POINT('Ctrl Pts',(-3.97349722602794,-1.30000000000022,
10.1930368892965));
#34344=CARTESIAN_POINT('Ctrl Pts',(-3.97869435191075,-1.18514270861196,
10.1728056047134));
#34345=CARTESIAN_POINT('Ctrl Pts',(-3.97239076473802,-1.06847604194524,
10.15489249281));
#34346=CARTESIAN_POINT('Ctrl Pts',(-3.93125926947268,-0.794772684000917,
10.1188650634462));
#34347=CARTESIAN_POINT('Ctrl Pts',(-3.86330482897738,-0.636309800095249,
10.0979046517948));
#34348=CARTESIAN_POINT('Ctrl Pts',(-3.78880121328532,-0.319434907277185,
10.0822558040718));
#34349=CARTESIAN_POINT('Ctrl Pts',(-3.73967479280392,-0.158333333333345,
10.0780642463435));
#34350=CARTESIAN_POINT('Ctrl Pts',(-3.72031792819803,0.158333333333347,
10.103075489714));
#34351=CARTESIAN_POINT('Ctrl Pts',(-3.74954897211557,0.319434907277193,
10.1329852943817));
#34352=CARTESIAN_POINT('Ctrl Pts',(-3.78572095843012,0.636309800095258,
10.1981401286174));
#34353=CARTESIAN_POINT('Ctrl Pts',(-3.83304673731638,0.794772684000906,
10.2468510356027));
#34354=CARTESIAN_POINT('Ctrl Pts',(-3.8448011432344,1.06847604194538,10.3188000213527));
#34355=CARTESIAN_POINT('Ctrl Pts',(-3.83971283334336,1.18514270861223,10.349891825942));
#34356=CARTESIAN_POINT('Ctrl Pts',(-3.82444816678303,1.30000000000063,10.3809313851622));
#34357=CARTESIAN_POINT('Ctrl Pts',(-3.97625624878831,-1.30000000000022,
10.1933594053906));
#34358=CARTESIAN_POINT('Ctrl Pts',(-3.98198868097057,-1.18514270861196,
10.1731886222752));
#34359=CARTESIAN_POINT('Ctrl Pts',(-3.97607415657479,-1.06847604194524,
10.1553255933479));
#34360=CARTESIAN_POINT('Ctrl Pts',(-3.93550362236307,-0.794772684000918,
10.1193897968784));
#34361=CARTESIAN_POINT('Ctrl Pts',(-3.86744965977133,-0.636309800095249,
10.0984242956282));
#34362=CARTESIAN_POINT('Ctrl Pts',(-3.79291200164116,-0.319434907277185,
10.0828842209601));
#34363=CARTESIAN_POINT('Ctrl Pts',(-3.74353202195387,-0.158333333333345,
10.0788268713356));
#34364=CARTESIAN_POINT('Ctrl Pts',(-3.72414430417208,0.158333333333347,
10.1039020972553));
#34365=CARTESIAN_POINT('Ctrl Pts',(-3.7535777313355,0.319434907277192,10.1337792027508));
#34366=CARTESIAN_POINT('Ctrl Pts',(-3.78976231043831,0.636309800095258,
10.1988791532386));
#34367=CARTESIAN_POINT('Ctrl Pts',(-3.83723623512286,0.794772684000907,
10.2475182334964));
#34368=CARTESIAN_POINT('Ctrl Pts',(-3.84842102626566,1.06847604194538,10.3193945152741));
#34369=CARTESIAN_POINT('Ctrl Pts',(-3.8429306802829,1.18514270861223,10.3504582082888));
#34370=CARTESIAN_POINT('Ctrl Pts',(-3.82710850666902,1.30000000000063,10.3814730152152));
#34371=CARTESIAN_POINT('Ctrl Pts',(-3.97783126988176,-1.30000000000022,
10.1935466720133));
#34372=CARTESIAN_POINT('Ctrl Pts',(-3.98386793609951,-1.18514270861196,
10.1734137657586));
#34373=CARTESIAN_POINT('Ctrl Pts',(-3.97817508118458,-1.06847604194524,
10.1555806625564));
#34374=CARTESIAN_POINT('Ctrl Pts',(-3.93792590718021,-0.794772684000918,
10.119695631785));
#34375=CARTESIAN_POINT('Ctrl Pts',(-3.8698211572568,-0.636309800095249,
10.0987151648293));
#34376=CARTESIAN_POINT('Ctrl Pts',(-3.79526405358766,-0.319434907277185,
10.083237165949));
#34377=CARTESIAN_POINT('Ctrl Pts',(-3.74573299628995,-0.158333333333345,
10.0792685590858));
#34378=CARTESIAN_POINT('Ctrl Pts',(-3.72632788005725,0.158333333333347,
10.1043800434176));
#34379=CARTESIAN_POINT('Ctrl Pts',(-3.75588220968736,0.319434907277192,
10.1342284153063));
#34380=CARTESIAN_POINT('Ctrl Pts',(-3.79207682014073,0.636309800095258,
10.1992917672285));
#34381=CARTESIAN_POINT('Ctrl Pts',(-3.83963639922207,0.794772684000907,
10.2478883083645));
#34382=CARTESIAN_POINT('Ctrl Pts',(-3.85049411959542,1.06847604194538,10.3197258711542));
#34383=CARTESIAN_POINT('Ctrl Pts',(-3.84477253459402,1.18514270861223,10.3507761541805));
#34384=CARTESIAN_POINT('Ctrl Pts',(-3.82862945975979,1.30000000000063,10.3817809011455));
#34385=CARTESIAN_POINT('Ctrl Pts',(-3.99120834453964,-1.30000000000021,
10.1951589192355));
#34386=CARTESIAN_POINT('Ctrl Pts',(-3.99981622143662,-1.18514270861195,
10.1753762694606));
#34387=CARTESIAN_POINT('Ctrl Pts',(-3.99600223628861,-1.06847604194524,
10.1578071058687));
#34388=CARTESIAN_POINT('Ctrl Pts',(-3.95849418130268,-0.794772684000911,
10.1223324191615));
#34389=CARTESIAN_POINT('Ctrl Pts',(-3.88999698655893,-0.636309800095245,
10.1011441035307));
#34390=CARTESIAN_POINT('Ctrl Pts',(-3.81531447193312,-0.319434907277184,
10.0861154983723));
#34391=CARTESIAN_POINT('Ctrl Pts',(-3.76453674642973,-0.158333333333344,
10.0828314136448));
#34392=CARTESIAN_POINT('Ctrl Pts',(-3.74497949862722,0.158333333333346,
10.108261146524));
#34393=CARTESIAN_POINT('Ctrl Pts',(-3.77549313140824,0.31943490727719,10.1379971254146));
#34394=CARTESIAN_POINT('Ctrl Pts',(-3.81177873263614,0.636309800095254,
10.2027421965092));
#34395=CARTESIAN_POINT('Ctrl Pts',(-3.86014910952305,0.794772684000902,
10.2508212795318));
#34396=CARTESIAN_POINT('Ctrl Pts',(-3.86823541825366,1.06847604194537,10.322318788935));
#34397=CARTESIAN_POINT('Ctrl Pts',(-3.86053734572664,1.18514270861222,10.3532789195567));
#34398=CARTESIAN_POINT('Ctrl Pts',(-3.84164093725037,1.30000000000063,10.3842505582232));
#34399=CARTESIAN_POINT('Ctrl Pts',(-4.01715141436988,-1.30000000000016,
10.1974276921261));
#34400=CARTESIAN_POINT('Ctrl Pts',(-4.03105905169031,-1.18514270861191,
10.1774944457447));
#34401=CARTESIAN_POINT('Ctrl Pts',(-4.03102853929687,-1.0684760419452,10.1600161809904));
#34402=CARTESIAN_POINT('Ctrl Pts',(-3.99875813540771,-0.79477268400089,
10.1253093915692));
#34403=CARTESIAN_POINT('Ctrl Pts',(-3.92860155491193,-0.636309800095222,
10.1056019296984));
#34404=CARTESIAN_POINT('Ctrl Pts',(-3.85350972014637,-0.31943490727717,
10.0918183982673));
#34405=CARTESIAN_POINT('Ctrl Pts',(-3.80085090679698,-0.158333333333339,
10.0888822558709));
#34406=CARTESIAN_POINT('Ctrl Pts',(-3.78103814166869,0.158333333333341,
10.1148544498269));
#34407=CARTESIAN_POINT('Ctrl Pts',(-3.81330939641933,0.319434907277181,
10.1445089974631));
#34408=CARTESIAN_POINT('Ctrl Pts',(-3.8492148680978,0.636309800095232,10.2096760392664));
#34409=CARTESIAN_POINT('Ctrl Pts',(-3.89789606902708,0.79477268400087,10.259034550803));
#34410=CARTESIAN_POINT('Ctrl Pts',(-3.90095428259184,1.06847604194533,10.3294593072443));
#34411=CARTESIAN_POINT('Ctrl Pts',(-3.88994950178544,1.18514270861218,10.3594286553047));
#34412=CARTESIAN_POINT('Ctrl Pts',(-3.86661615283843,1.30000000000058,10.3888830838563));
#34413=CARTESIAN_POINT('Ctrl Pts',(-4.04264117857264,-1.30000000000011,
10.1996888386742));
#34414=CARTESIAN_POINT('Ctrl Pts',(-4.06162921508693,-1.18514270861186,
10.1798435376198));
#34415=CARTESIAN_POINT('Ctrl Pts',(-4.06526201565739,-1.06847604194515,
10.1625501048079));
#34416=CARTESIAN_POINT('Ctrl Pts',(-4.03818084487975,-0.794772684000851,
10.1284941416128));
#34417=CARTESIAN_POINT('Ctrl Pts',(-3.96674475595548,-0.636309800095196,
10.1095386222874));
#34418=CARTESIAN_POINT('Ctrl Pts',(-3.891393048032,-0.319434907277159,10.0967082635573));
#34419=CARTESIAN_POINT('Ctrl Pts',(-3.83684904087863,-0.158333333333332,
10.0942175847262));
#34420=CARTESIAN_POINT('Ctrl Pts',(-3.81670994245091,0.158333333333334,
10.1208905127328));
#34421=CARTESIAN_POINT('Ctrl Pts',(-3.85032449139867,0.319434907277167,
10.1511988953562));
#34422=CARTESIAN_POINT('Ctrl Pts',(-3.88626421184787,0.636309800095206,
10.2160282620725));
#34423=CARTESIAN_POINT('Ctrl Pts',(-3.93674627805647,0.79477268400084,10.2638747589896));
#34424=CARTESIAN_POINT('Ctrl Pts',(-3.93451699612749,1.06847604194529,10.3338269442228));
#34425=CARTESIAN_POINT('Ctrl Pts',(-3.91970579175577,1.18514270861213,10.3638146300663));
#34426=CARTESIAN_POINT('Ctrl Pts',(-3.89104835655634,1.30000000000053,10.3935102927497));
#34427=CARTESIAN_POINT('Ctrl Pts',(-4.05557051525689,-1.30000000000011,
10.2004379798222));
#34428=CARTESIAN_POINT('Ctrl Pts',(-4.07701141444267,-1.18514270861186,
10.1807976562281));
#34429=CARTESIAN_POINT('Ctrl Pts',(-4.08243023812086,-1.06847604194515,
10.1636773708346));
#34430=CARTESIAN_POINT('Ctrl Pts',(-4.05793460522167,-0.794772684000851,
10.1299478790495));
#34431=CARTESIAN_POINT('Ctrl Pts',(-3.98606842200265,-0.636309800095196,
10.1109415465295));
#34432=CARTESIAN_POINT('Ctrl Pts',(-3.91057658300642,-0.319434907277159,
10.0986164293511));
#34433=CARTESIAN_POINT('Ctrl Pts',(-3.85489608531509,-0.158333333333332,
10.0967615839605));
#34434=CARTESIAN_POINT('Ctrl Pts',(-3.83456187378799,0.158333333333334,
10.1238619534744));
#34435=CARTESIAN_POINT('Ctrl Pts',(-3.86905149194718,0.319434907277167,
10.1540957676226));
#34436=CARTESIAN_POINT('Ctrl Pts',(-3.90486897721865,0.636309800095206,
10.2190179716123));
#34437=CARTESIAN_POINT('Ctrl Pts',(-3.95570286248539,0.79477268400084,10.2671282986158));
#34438=CARTESIAN_POINT('Ctrl Pts',(-3.95093219463511,1.06847604194529,10.3366909515195));
#34439=CARTESIAN_POINT('Ctrl Pts',(-3.93440493783799,1.18514270861213,10.3663638202738));
#34440=CARTESIAN_POINT('Ctrl Pts',(-3.90341546958548,1.30000000000053,10.3955984628905));
#34441=CARTESIAN_POINT('',(-3.81817959106573,1.2,10.3502388179897));
#34442=CARTESIAN_POINT('Ctrl Pts',(-3.81817959106573,1.2,10.3502388179897));
#34443=CARTESIAN_POINT('Ctrl Pts',(-3.79661778313311,1.21681395190025,10.3499524248101));
#34444=CARTESIAN_POINT('Ctrl Pts',(-3.7746889739999,1.23316487520676,10.3507417153752));
#34445=CARTESIAN_POINT('Ctrl Pts',(-3.74255521985325,1.25821638180379,10.3500589326249));
#34446=CARTESIAN_POINT('Ctrl Pts',(-3.73195596097856,1.26642443139157,10.3498984954673));
#34447=CARTESIAN_POINT('Ctrl Pts',(-3.71004144468884,1.28334474964523,10.3495995663522));
#34448=CARTESIAN_POINT('Ctrl Pts',(-3.69832282339783,1.29250139325086,10.3492436833369));
#34449=CARTESIAN_POINT('Ctrl Pts',(-3.68879127704346,1.30000000000059,10.3488599388354));
#34450=CARTESIAN_POINT('',(-3.91593537812686,0.653834841369882,10.2278623010254));
#34451=CARTESIAN_POINT('Ctrl Pts',(-3.91593537815288,0.653834841368625,
10.2278623010518));
#34452=CARTESIAN_POINT('Ctrl Pts',(-3.90605735116792,0.717483776812682,
10.2406375568233));
#34453=CARTESIAN_POINT('Ctrl Pts',(-3.89793780545931,0.764248674190916,
10.2510423166789));
#34454=CARTESIAN_POINT('Ctrl Pts',(-3.86587044819959,0.949850976170393,
10.291727520538));
#34455=CARTESIAN_POINT('Ctrl Pts',(-3.84608078280016,1.0589088106385,10.3164217752187));
#34456=CARTESIAN_POINT('Ctrl Pts',(-3.81817959106573,1.2,10.3502388179897));
#34457=CARTESIAN_POINT('',(-3.99970644341025,-0.653834841531101,10.1163073168894));
#34458=CARTESIAN_POINT('Ctrl Pts',(-3.99970644341023,-0.653834841531111,
10.1163073168894));
#34459=CARTESIAN_POINT('Ctrl Pts',(-3.95891593940165,-0.575966355975947,
10.1082384035645));
#34460=CARTESIAN_POINT('Ctrl Pts',(-3.92429340983449,-0.493639798317628,
10.1021623354875));
#34461=CARTESIAN_POINT('Ctrl Pts',(-3.87408237926539,-0.338140650733339,
10.0958281963273));
#34462=CARTESIAN_POINT('Ctrl Pts',(-3.85622336702604,-0.265666408457172,
10.0948144796845));
#34463=CARTESIAN_POINT('Ctrl Pts',(-3.83202394298176,-0.129722242244509,
10.0977329215106));
#34464=CARTESIAN_POINT('Ctrl Pts',(-3.82439528475797,-0.066627635979717,
10.1009429954397));
#34465=CARTESIAN_POINT('Ctrl Pts',(-3.81609773603222,0.0595477087246973,
10.1113738105213));
#34466=CARTESIAN_POINT('Ctrl Pts',(-3.8153544130588,0.122784223523335,10.1186606316291));
#34467=CARTESIAN_POINT('Ctrl Pts',(-3.82182947500263,0.26013995765241,10.1383623818109));
#34468=CARTESIAN_POINT('Ctrl Pts',(-3.83052491254541,0.333957153420333,
10.1514746983359));
#34469=CARTESIAN_POINT('Ctrl Pts',(-3.86115450447686,0.491217719043045,
10.1842373489534));
#34470=CARTESIAN_POINT('Ctrl Pts',(-3.88506933429854,0.574353853455511,
10.2048500775317));
#34471=CARTESIAN_POINT('Ctrl Pts',(-3.91593537807148,0.653834841386436,
10.2278623010425));
#34472=CARTESIAN_POINT('',(-3.95668316628078,-1.2,10.1744173079227));
#34473=CARTESIAN_POINT('Ctrl Pts',(-3.95668316628078,-1.2,10.1744173079227));
#34474=CARTESIAN_POINT('Ctrl Pts',(-3.96492264622143,-1.12750309682141,
10.1634568379533));
#34475=CARTESIAN_POINT('Ctrl Pts',(-3.97439867849545,-1.03220200323701,
10.1507580406354));
#34476=CARTESIAN_POINT('Ctrl Pts',(-3.99268946522797,-0.796459678297759,
10.1259357400627));
#34477=CARTESIAN_POINT('Ctrl Pts',(-3.99590797836092,-0.740048759787163,
10.1215168999278));
#34478=CARTESIAN_POINT('Ctrl Pts',(-3.99970644341023,-0.653834841531099,
10.1163073168894));
#34479=CARTESIAN_POINT('Ctrl Pts',(-3.83170332429324,-1.30000000000002,
10.1733061790875));
#34480=CARTESIAN_POINT('Ctrl Pts',(-3.84079303276221,-1.29262062153828,
10.1736293612034));
#34481=CARTESIAN_POINT('Ctrl Pts',(-3.85131337624757,-1.28398008608649,
10.1741514649677));
#34482=CARTESIAN_POINT('Ctrl Pts',(-3.87298321825068,-1.26674725507027,
10.1742566864986));
#34483=CARTESIAN_POINT('Ctrl Pts',(-3.88398522746645,-1.25800071781436,
10.1742825776218));
#34484=CARTESIAN_POINT('Ctrl Pts',(-3.90782377744779,-1.23869680098493,
10.174873105833));
#34485=CARTESIAN_POINT('Ctrl Pts',(-3.93037425193878,-1.22042603079793,
10.1754216007778));
#34486=CARTESIAN_POINT('Ctrl Pts',(-3.95668316628078,-1.2,10.1744173079227));
#34487=CARTESIAN_POINT('Origin',(0.,1.25,7.2));
#34488=CARTESIAN_POINT('Origin',(0.,1.2,7.2));
#34489=CARTESIAN_POINT('Origin',(0.,0.92691742076555,7.2));
#34490=CARTESIAN_POINT('Origin',(0.,0.653834841531101,7.2));
#34491=CARTESIAN_POINT('Origin',(0.,0.,7.2));
#34492=CARTESIAN_POINT('Origin',(0.,-0.653834841531101,7.2));
#34493=CARTESIAN_POINT('Origin',(0.,-0.926917420765551,7.2));
#34494=CARTESIAN_POINT('Origin',(0.,-1.2,7.2));
#34495=CARTESIAN_POINT('Origin',(0.,-1.25,7.2));
#34496=CARTESIAN_POINT('Ctrl Pts',(-4.24541645780663,-1.30000000000008,
9.92487448592682));
#34497=CARTESIAN_POINT('Ctrl Pts',(-4.2271889327826,-1.18514270861184,9.96338122303863));
#34498=CARTESIAN_POINT('Ctrl Pts',(-4.20407556081819,-1.06847604194514,
9.98826899902922));
#34499=CARTESIAN_POINT('Ctrl Pts',(-4.13939176392353,-0.794772684000851,
10.0143022156962));
#34500=CARTESIAN_POINT('Ctrl Pts',(-4.07792758948489,-0.636309800095197,
9.98082322651161));
#34501=CARTESIAN_POINT('Ctrl Pts',(-4.00511469268244,-0.319434907277159,
9.96682083809129));
#34502=CARTESIAN_POINT('Ctrl Pts',(-3.96570274858467,-0.158333333333333,
9.94336202437368));
#34503=CARTESIAN_POINT('Ctrl Pts',(-3.94621238249364,0.158333333333334,
9.97107548348392));
#34504=CARTESIAN_POINT('Ctrl Pts',(-3.96518266533145,0.319434907277167,
10.0234576048964));
#34505=CARTESIAN_POINT('Ctrl Pts',(-4.00023280952294,0.636309800095206,
10.0914459396341));
#34506=CARTESIAN_POINT('Ctrl Pts',(-4.04051677784849,0.79477268400084,10.1539214617338));
#34507=CARTESIAN_POINT('Ctrl Pts',(-4.08016499765647,1.06847604194587,10.1667952068506));
#34508=CARTESIAN_POINT('Ctrl Pts',(-4.09477284803601,1.18514270861327,10.1563511401463));
#34509=CARTESIAN_POINT('Ctrl Pts',(-4.10682630355149,1.30000000000221,10.1298904394961));
#34510=CARTESIAN_POINT('Ctrl Pts',(-4.24251264986958,-1.30000000000008,
9.91931621425302));
#34511=CARTESIAN_POINT('Ctrl Pts',(-4.22370557786425,-1.18514270861184,
9.95678523527321));
#34512=CARTESIAN_POINT('Ctrl Pts',(-4.20017735680198,-1.06847604194514,
9.98090562176186));
#34513=CARTESIAN_POINT('Ctrl Pts',(-4.13491566055947,-0.794772684000851,
10.0057905236644));
#34514=CARTESIAN_POINT('Ctrl Pts',(-4.07363130379674,-0.636309800095197,
9.97243807038172));
#34515=CARTESIAN_POINT('Ctrl Pts',(-4.00084366736096,-0.319434907277159,
9.95836321152855));
#34516=CARTESIAN_POINT('Ctrl Pts',(-3.96153146947934,-0.158333333333333,
9.93533203941429));
#34517=CARTESIAN_POINT('Ctrl Pts',(-3.94221421727185,0.158333333333334,
9.96288667338731));
#34518=CARTESIAN_POINT('Ctrl Pts',(-3.96131125943563,0.319434907277167,
10.0146301197666));
#34519=CARTESIAN_POINT('Ctrl Pts',(-3.99658000881247,0.636309800095206,
10.0824737541014));
#34520=CARTESIAN_POINT('Ctrl Pts',(-4.03677336078499,0.79477268400084,10.1447526052678));
#34521=CARTESIAN_POINT('Ctrl Pts',(-4.07697631454619,1.06847604194587,10.1588054041015));
#34522=CARTESIAN_POINT('Ctrl Pts',(-4.0919424571672,1.18514270861327,10.1491838891105));
#34523=CARTESIAN_POINT('Ctrl Pts',(-4.10447237339219,1.30000000000221,10.1238579232207));
#34524=CARTESIAN_POINT('Ctrl Pts',(-4.23681986628123,-1.3000000000001,9.9080585135877));
#34525=CARTESIAN_POINT('Ctrl Pts',(-4.21674166253644,-1.18514270861185,
9.94357552431802));
#34526=CARTESIAN_POINT('Ctrl Pts',(-4.19229548072165,-1.06847604194515,
9.96625706117423));
#34527=CARTESIAN_POINT('Ctrl Pts',(-4.1257290071349,-0.794772684000856,
9.98900343636103));
#34528=CARTESIAN_POINT('Ctrl Pts',(-4.06469021042839,-0.636309800095198,
9.95601141287329));
#34529=CARTESIAN_POINT('Ctrl Pts',(-3.99208575376412,-0.319434907277158,
9.94165487404065));
#34530=CARTESIAN_POINT('Ctrl Pts',(-3.95335341894101,-0.158333333333333,
9.91909219744007));
#34531=CARTESIAN_POINT('Ctrl Pts',(-3.93450274268745,0.158333333333335,
9.94620879746131));
#34532=CARTESIAN_POINT('Ctrl Pts',(-3.95367786492859,0.319434907277169,
9.99685790233624));
#34533=CARTESIAN_POINT('Ctrl Pts',(-3.98932401498674,0.636309800095209,
10.0644735326305));
#34534=CARTESIAN_POINT('Ctrl Pts',(-4.02933574586201,0.79477268400084,10.1263541693987));
#34535=CARTESIAN_POINT('Ctrl Pts',(-4.07064867242679,1.06847604194587,10.1427653324373));
#34536=CARTESIAN_POINT('Ctrl Pts',(-4.08633771688935,1.18514270861327,10.1347839656526));
#34537=CARTESIAN_POINT('Ctrl Pts',(-4.09983297069931,1.30000000000221,10.1117174476973));
#34538=CARTESIAN_POINT('Ctrl Pts',(-4.22773027115874,-1.3000000000001,9.89184542464046));
#34539=CARTESIAN_POINT('Ctrl Pts',(-4.20673506497644,-1.18514270861185,
9.92334340244841));
#34540=CARTESIAN_POINT('Ctrl Pts',(-4.18151913362969,-1.06847604194515,
9.94319197628689));
#34541=CARTESIAN_POINT('Ctrl Pts',(-4.11351456830585,-0.794772684000856,
9.96213369892261));
#34542=CARTESIAN_POINT('Ctrl Pts',(-4.05176903880094,-0.636309800095199,
9.93083420913925));
#34543=CARTESIAN_POINT('Ctrl Pts',(-3.97883825081608,-0.319434907277159,
9.91667421944362));
#34544=CARTESIAN_POINT('Ctrl Pts',(-3.94078375282828,-0.158333333333333,
9.89502227718623));
#34545=CARTESIAN_POINT('Ctrl Pts',(-3.92215022335235,0.158333333333335,
9.92194096575744));
#34546=CARTESIAN_POINT('Ctrl Pts',(-3.9409421645071,0.319434907277169,9.9713830921904));
#34547=CARTESIAN_POINT('Ctrl Pts',(-3.97719907804311,0.636309800095209,
10.0385993384994));
#34548=CARTESIAN_POINT('Ctrl Pts',(-4.01782137157219,0.794772684000842,
10.0990389685616));
#34549=CARTESIAN_POINT('Ctrl Pts',(-4.06081173472643,1.06847604194587,10.1190064288439));
#34550=CARTESIAN_POINT('Ctrl Pts',(-4.07741740679809,1.18514270861328,10.1136670291134));
#34551=CARTESIAN_POINT('Ctrl Pts',(-4.09201981568185,1.30000000000221,10.0943450559635));
#34552=CARTESIAN_POINT('Ctrl Pts',(-4.21852308140183,-1.3000000000001,9.8756612747752));
#34553=CARTESIAN_POINT('Ctrl Pts',(-4.19550261185785,-1.18514270861186,
9.90432169235314));
#34554=CARTESIAN_POINT('Ctrl Pts',(-4.16887662610448,-1.06847604194516,
9.9220231565384));
#34555=CARTESIAN_POINT('Ctrl Pts',(-4.09903580877927,-0.79477268400086,
9.93759970530387));
#34556=CARTESIAN_POINT('Ctrl Pts',(-4.03833506779414,-0.636309800095202,
9.9061569634847));
#34557=CARTESIAN_POINT('Ctrl Pts',(-3.96548412441517,-0.319434907277161,
9.89176508749895));
#34558=CARTESIAN_POINT('Ctrl Pts',(-3.927363106507,-0.158333333333334,9.87177971841636));
#34559=CARTESIAN_POINT('Ctrl Pts',(-3.90916433055663,0.158333333333335,
9.89828720877045));
#34560=CARTESIAN_POINT('Ctrl Pts',(-3.92839276445368,0.31943490727717,9.94571238450143));
#34561=CARTESIAN_POINT('Ctrl Pts',(-3.96558734864098,0.636309800095212,
10.0121990485734));
#34562=CARTESIAN_POINT('Ctrl Pts',(-4.00646810712007,0.794772684000845,
10.0715308840212));
#34563=CARTESIAN_POINT('Ctrl Pts',(-4.05119187067628,1.06847604194588,10.0949974551163));
#34564=CARTESIAN_POINT('Ctrl Pts',(-4.06878677662875,1.18514270861328,10.0922306101798));
#34565=CARTESIAN_POINT('Ctrl Pts',(-4.08461732846891,1.30000000000222,10.0765391112017));
#34566=CARTESIAN_POINT('Ctrl Pts',(-4.21277725489613,-1.30000000000011,
9.86437445357206));
#34567=CARTESIAN_POINT('Ctrl Pts',(-4.18871035144018,-1.18514270861186,
9.8908147696321));
#34568=CARTESIAN_POINT('Ctrl Pts',(-4.16129306149929,-1.06847604194516,
9.90692099325134));
#34569=CARTESIAN_POINT('Ctrl Pts',(-4.090213573903,-0.794772684000864,9.92025577098438));
#34570=CARTESIAN_POINT('Ctrl Pts',(-4.02940487828938,-0.636309800095204,
9.8895529233566));
#34571=CARTESIAN_POINT('Ctrl Pts',(-3.95658703201688,-0.319434907277162,
9.87503390675468));
#34572=CARTESIAN_POINT('Ctrl Pts',(-3.91917788307007,-0.158333333333335,
9.85539785270959));
#34573=CARTESIAN_POINT('Ctrl Pts',(-3.90119054960112,0.158333333333336,
9.88170489192799));
#34574=CARTESIAN_POINT('Ctrl Pts',(-3.91999084243052,0.319434907277171,
9.92849828883152));
#34575=CARTESIAN_POINT('Ctrl Pts',(-3.95743578244152,0.636309800095215,
9.99487084286091));
#34576=CARTESIAN_POINT('Ctrl Pts',(-3.99853228417306,0.794772684000848,
10.053411740087));
#34577=CARTESIAN_POINT('Ctrl Pts',(-4.04440238583212,1.06847604194588,10.0792434466343));
#34578=CARTESIAN_POINT('Ctrl Pts',(-4.06267934271888,1.18514270861329,10.0781861728379));
#34579=CARTESIAN_POINT('Ctrl Pts',(-4.07937778913892,1.30000000000222,10.0648900366399));
#34580=CARTESIAN_POINT('Ctrl Pts',(-4.20970628126203,-1.30000000000011,
9.85885446397306));
#34581=CARTESIAN_POINT('Ctrl Pts',(-4.18521300724093,-1.18514270861186,
9.88405188320314));
#34582=CARTESIAN_POINT('Ctrl Pts',(-4.15746191721057,-1.06847604194516,
9.89927317397398));
#34583=CARTESIAN_POINT('Ctrl Pts',(-4.08582514094864,-0.794772684000863,
9.91139054820488));
#34584=CARTESIAN_POINT('Ctrl Pts',(-4.02493162928629,-0.636309800095206,
9.88110165101293));
#34585=CARTESIAN_POINT('Ctrl Pts',(-3.95197514461098,-0.319434907277163,
9.86667820019585));
#34586=CARTESIAN_POINT('Ctrl Pts',(-3.91461123572,-0.158333333333335,9.84754083457005));
#34587=CARTESIAN_POINT('Ctrl Pts',(-3.89674427954975,0.158333333333336,
9.87373343071214));
#34588=CARTESIAN_POINT('Ctrl Pts',(-3.91570877873406,0.319434907277172,
9.91982112826059));
#34589=CARTESIAN_POINT('Ctrl Pts',(-3.95335612966987,0.636309800095216,
9.98605355826342));
#34590=CARTESIAN_POINT('Ctrl Pts',(-3.99429516133064,0.794772684000851,
10.0444522831198));
#34591=CARTESIAN_POINT('Ctrl Pts',(-4.04075765464447,1.06847604194588,10.0714686819131));
#34592=CARTESIAN_POINT('Ctrl Pts',(-4.0594320810401,1.18514270861329,10.0712266075604));
#34593=CARTESIAN_POINT('Ctrl Pts',(-4.07666904208079,1.30000000000222,10.0590480608735));
#34594=CARTESIAN_POINT('Ctrl Pts',(-4.20963545591083,-1.30000000000011,
9.85872702181624));
#34595=CARTESIAN_POINT('Ctrl Pts',(-4.18513223806645,-1.18514270861186,
9.88389587516515));
#34596=CARTESIAN_POINT('Ctrl Pts',(-4.15737337933957,-1.06847604194516,
9.89909681736857));
#34597=CARTESIAN_POINT('Ctrl Pts',(-4.08572368081249,-0.794772684000863,
9.91118616597669));
#34598=CARTESIAN_POINT('Ctrl Pts',(-4.02482827235545,-0.636309800095206,
9.88090674820191));
#34599=CARTESIAN_POINT('Ctrl Pts',(-3.95186872525836,-0.319434907277163,
9.86648535991826));
#34600=CARTESIAN_POINT('Ctrl Pts',(-3.91450611474061,-0.158333333333335,
9.84735924543995));
#34601=CARTESIAN_POINT('Ctrl Pts',(-3.89664190857931,0.158333333333336,
9.87354922796575));
#34602=CARTESIAN_POINT('Ctrl Pts',(-3.91560983625881,0.319434907277172,
9.91962100343749));
#34603=CARTESIAN_POINT('Ctrl Pts',(-3.95326182446619,0.636309800095215,
9.98585023775694));
#34604=CARTESIAN_POINT('Ctrl Pts',(-3.99419753968574,0.79477268400085,10.0442453697909));
#34605=CARTESIAN_POINT('Ctrl Pts',(-4.04067373102421,1.06847604194588,10.0712890816844));
#34606=CARTESIAN_POINT('Ctrl Pts',(-4.05935728940721,1.18514270861329,10.0710658594948));
#34607=CARTESIAN_POINT('Ctrl Pts',(-4.07660658505531,1.30000000000222,10.0589131943051));
#34608=CARTESIAN_POINT('Ctrl Pts',(-4.20956455372579,-1.30000000000011,
9.85859966803531));
#34609=CARTESIAN_POINT('Ctrl Pts',(-4.18505141943581,-1.18514270861186,
9.8837399224243));
#34610=CARTESIAN_POINT('Ctrl Pts',(-4.15728481071699,-1.06847604194516,
9.89892049350013));
#34611=CARTESIAN_POINT('Ctrl Pts',(-4.08562221309949,-0.794772684000863,
9.91098178866697));
#34612=CARTESIAN_POINT('Ctrl Pts',(-4.0247249144713,-0.636309800095206,
9.88071184746151));
#34613=CARTESIAN_POINT('Ctrl Pts',(-3.95176225583807,-0.319434907277163,
9.86629257173117));
#34614=CARTESIAN_POINT('Ctrl Pts',(-3.91440082462096,-0.158333333333335,
9.84717782853973));
#34615=CARTESIAN_POINT('Ctrl Pts',(-3.89653938038487,0.158333333333336,
9.87336518476813));
#34616=CARTESIAN_POINT('Ctrl Pts',(-3.91551088497831,0.319434907277172,
9.9194208877983));
#34617=CARTESIAN_POINT('Ctrl Pts',(-3.95316754834085,0.636309800095215,
9.98564688632071));
#34618=CARTESIAN_POINT('Ctrl Pts',(-3.9940998582532,0.794772684000851,10.0440385122106));
#34619=CARTESIAN_POINT('Ctrl Pts',(-4.04058975015895,1.06847604194588,10.0711095347789));
#34620=CARTESIAN_POINT('Ctrl Pts',(-4.0592824557011,1.18514270861329,10.0709051503023));
#34621=CARTESIAN_POINT('Ctrl Pts',(-4.07654411519959,1.30000000000222,10.0587783387596));
#34622=CARTESIAN_POINT('Ctrl Pts',(-4.20942270138084,-1.30000000000011,
9.85834500849095));
#34623=CARTESIAN_POINT('Ctrl Pts',(-4.18488967018863,-1.18514270861186,
9.88342813329698));
#34624=CARTESIAN_POINT('Ctrl Pts',(-4.15710752302828,-1.06847604194516,
9.89856800290258));
#34625=CARTESIAN_POINT('Ctrl Pts',(-4.08541909741854,-0.794772684000863,
9.91057322175767));
#34626=CARTESIAN_POINT('Ctrl Pts',(-4.02451808128831,-0.636309800095206,
9.88032216363038));
#34627=CARTESIAN_POINT('Ctrl Pts',(-3.95154926822279,-0.319434907277163,
9.86590704002388));
#34628=CARTESIAN_POINT('Ctrl Pts',(-3.91419029087762,-0.158333333333335,
9.84681494278848));
#34629=CARTESIAN_POINT('Ctrl Pts',(-3.89633435929325,0.158333333333336,
9.87299705619156));
#34630=CARTESIAN_POINT('Ctrl Pts',(-3.91531286007442,0.319434907277171,
9.91902077196273));
#34631=CARTESIAN_POINT('Ctrl Pts',(-3.95297888652735,0.636309800095215,
9.98524028740749));
#34632=CARTESIAN_POINT('Ctrl Pts',(-3.99390457240559,0.79477268400085,10.0436247170789));
#34633=CARTESIAN_POINT('Ctrl Pts',(-4.04042189267401,1.06847604194588,10.0707503352224));
#34634=CARTESIAN_POINT('Ctrl Pts',(-4.0591328728242,1.18514270861329,10.070583646189));
#34635=CARTESIAN_POINT('Ctrl Pts',(-4.0764192088169,1.30000000000222,10.058508593131));
#34636=CARTESIAN_POINT('Ctrl Pts',(-4.20911489946616,-1.30000000000011,
9.85779374196368));
#34637=CARTESIAN_POINT('Ctrl Pts',(-4.18453859769891,-1.18514270861186,
9.88275324427473));
#34638=CARTESIAN_POINT('Ctrl Pts',(-4.15672269581207,-1.06847604194516,
9.89780501156095));
#34639=CARTESIAN_POINT('Ctrl Pts',(-4.08497827354528,-0.794772684000863,
9.90968875514491));
#34640=CARTESIAN_POINT('Ctrl Pts',(-4.02406948399971,-0.636309800095206,
9.87947831400066));
#34641=CARTESIAN_POINT('Ctrl Pts',(-3.95108743737665,-0.319434907277163,
9.86507207165953));
#34642=CARTESIAN_POINT('Ctrl Pts',(-3.91373372858721,-0.158333333333335,
9.84602908681854));
#34643=CARTESIAN_POINT('Ctrl Pts',(-3.8958897421842,0.158333333333336,9.87219983137673));
#34644=CARTESIAN_POINT('Ctrl Pts',(-3.9148833111106,0.319434907277172,9.91815432514302));
#34645=CARTESIAN_POINT('Ctrl Pts',(-3.95256980967421,0.636309800095216,
9.98435960611405));
#34646=CARTESIAN_POINT('Ctrl Pts',(-3.99348156089107,0.794772684000851,
10.0427280298469));
#34647=CARTESIAN_POINT('Ctrl Pts',(-4.04005842136669,1.06847604194588,10.0699718320407));
#34648=CARTESIAN_POINT('Ctrl Pts',(-4.05880897032625,1.18514270861329,10.0698868459808));
#34649=CARTESIAN_POINT('Ctrl Pts',(-4.07614867118817,1.30000000000222,10.0579240413735));
#34650=CARTESIAN_POINT('Ctrl Pts',(-4.20863976745657,-1.30000000000011,
9.85694734936963));
#34651=CARTESIAN_POINT('Ctrl Pts',(-4.18399602124621,-1.18514270861186,
9.88171755971258));
#34652=CARTESIAN_POINT('Ctrl Pts',(-4.15612769058842,-1.06847604194516,
9.89663428854023));
#34653=CARTESIAN_POINT('Ctrl Pts',(-4.08429683657899,-0.794772684000863,
9.90833140273091));
#34654=CARTESIAN_POINT('Ctrl Pts',(-4.02337734430711,-0.636309800095206,
9.87818210770303));
#34655=CARTESIAN_POINT('Ctrl Pts',(-3.95037564248984,-0.319434907277163,
9.8637887589159));
#34656=CARTESIAN_POINT('Ctrl Pts',(-3.91303039482342,-0.158333333333335,
9.84482095921614));
#34657=CARTESIAN_POINT('Ctrl Pts',(-3.89520475213598,0.158333333333336,
9.87097421369106));
#34658=CARTESIAN_POINT('Ctrl Pts',(-3.91422042138237,0.319434907277172,
9.91682327553824));
#34659=CARTESIAN_POINT('Ctrl Pts',(-3.95193905333691,0.636309800095215,
9.98300602138339));
#34660=CARTESIAN_POINT('Ctrl Pts',(-3.99283160922943,0.79477268400085,10.0413476062463));
#34661=CARTESIAN_POINT('Ctrl Pts',(-4.03950053014917,1.06847604194588,10.0687727924243));
#34662=CARTESIAN_POINT('Ctrl Pts',(-4.05831175619488,1.18514270861329,10.0688137102661));
#34663=CARTESIAN_POINT('Ctrl Pts',(-4.07573296167402,1.30000000000222,10.0570241990566));
#34664=CARTESIAN_POINT('Ctrl Pts',(-4.20806696965542,-1.30000000000011,
9.85593446970752));
#34665=CARTESIAN_POINT('Ctrl Pts',(-4.18334015744563,-1.18514270861186,
9.88047976421315));
#34666=CARTESIAN_POINT('Ctrl Pts',(-4.15540768083246,-1.06847604194516,
9.89523572728958));
#34667=CARTESIAN_POINT('Ctrl Pts',(-4.08347234592043,-0.794772684000863,
9.90670963996597));
#34668=CARTESIAN_POINT('Ctrl Pts',(-4.02254283004788,-0.636309800095206,
9.87663069019566));
#34669=CARTESIAN_POINT('Ctrl Pts',(-3.94951942063887,-0.319434907277163,
9.86225079315611));
#34670=CARTESIAN_POINT('Ctrl Pts',(-3.91218578056065,-0.158333333333335,
9.84337171740359));
#34671=CARTESIAN_POINT('Ctrl Pts',(-3.89438204868042,0.158333333333336,
9.86950402703382));
#34672=CARTESIAN_POINT('Ctrl Pts',(-3.91342112525749,0.319434907277171,
9.91522966746529));
#34673=CARTESIAN_POINT('Ctrl Pts',(-3.9511794034085,0.636309800095215,9.98138431152671));
#34674=CARTESIAN_POINT('Ctrl Pts',(-3.99205408438125,0.79477268400085,10.0396886129266));
#34675=CARTESIAN_POINT('Ctrl Pts',(-4.03883435040479,1.06847604194588,10.0673306244702));
#34676=CARTESIAN_POINT('Ctrl Pts',(-4.05771784961653,1.18514270861329,10.0675231719302));
#34677=CARTESIAN_POINT('Ctrl Pts',(-4.07523540425804,1.30000000000222,10.0559430642906));
#34678=CARTESIAN_POINT('Ctrl Pts',(-4.20729978356503,-1.30000000000011,
9.85458758065339));
#34679=CARTESIAN_POINT('Ctrl Pts',(-4.18245885715696,-1.18514270861186,
9.87883653400406));
#34680=CARTESIAN_POINT('Ctrl Pts',(-4.15443889534823,-1.06847604194516,
9.89338019829312));
#34681=CARTESIAN_POINT('Ctrl Pts',(-4.08236297045647,-0.794772684000863,
9.90455781298223));
#34682=CARTESIAN_POINT('Ctrl Pts',(-4.02142431303854,-0.636309800095206,
9.87456810921836));
#34683=CARTESIAN_POINT('Ctrl Pts',(-3.9483749932468,-0.319434907277163,
9.8602029025274));
#34684=CARTESIAN_POINT('Ctrl Pts',(-3.9110595018654,-0.158333333333335,
9.84143937715152));
#34685=CARTESIAN_POINT('Ctrl Pts',(-3.89328483770833,0.158333333333336,
9.86754382120249));
#34686=CARTESIAN_POINT('Ctrl Pts',(-3.91234996015436,0.319434907277172,
9.91311004771467));
#34687=CARTESIAN_POINT('Ctrl Pts',(-3.95016254525791,0.636309800095215,
9.97922582794848));
#34688=CARTESIAN_POINT('Ctrl Pts',(-3.99102131770104,0.79477268400085,10.0374726331695));
#34689=CARTESIAN_POINT('Ctrl Pts',(-4.03795128511267,1.06847604194588,10.0654025539362));
#34690=CARTESIAN_POINT('Ctrl Pts',(-4.05693027753792,1.18514270861329,10.0657981457286));
#34691=CARTESIAN_POINT('Ctrl Pts',(-4.07457401842252,1.30000000000222,10.0544995015191));
#34692=CARTESIAN_POINT('Ctrl Pts',(-4.20633388256444,-1.30000000000011,
9.85291111779125));
#34693=CARTESIAN_POINT('Ctrl Pts',(-4.18134193001888,-1.18514270861186,
9.87679856646903));
#34694=CARTESIAN_POINT('Ctrl Pts',(-4.15320771225699,-1.06847604194516,
9.89108205667209));
#34695=CARTESIAN_POINT('Ctrl Pts',(-4.0809527797383,-0.794772684000862,
9.9018927111017));
#34696=CARTESIAN_POINT('Ctrl Pts',(-4.02001288636102,-0.636309800095206,
9.87200356719769));
#34697=CARTESIAN_POINT('Ctrl Pts',(-3.9469391178162,-0.319434907277163,
9.85764827324214));
#34698=CARTESIAN_POINT('Ctrl Pts',(-3.90965405515109,-0.158333333333335,
9.83902122733326));
#34699=CARTESIAN_POINT('Ctrl Pts',(-3.89191535958804,0.158333333333336,
9.86509101628633));
#34700=CARTESIAN_POINT('Ctrl Pts',(-3.91099923026029,0.319434907277171,
9.91047179106491));
#34701=CARTESIAN_POINT('Ctrl Pts',(-3.94888262509831,0.636309800095215,
9.97653623166595));
#34702=CARTESIAN_POINT('Ctrl Pts',(-3.98974110428675,0.79477268400085,10.0346919588768));
#34703=CARTESIAN_POINT('Ctrl Pts',(-4.03686087928501,1.06847604194588,10.062979181776));
#34704=CARTESIAN_POINT('Ctrl Pts',(-4.05595689544923,1.18514270861329,10.0636308936443));
#34705=CARTESIAN_POINT('Ctrl Pts',(-4.07375252314058,1.30000000000222,10.0526898267328));
#34706=CARTESIAN_POINT('Ctrl Pts',(-4.20399595551413,-1.3000000000001,9.8489076789416));
#34707=CARTESIAN_POINT('Ctrl Pts',(-4.17861348591113,-1.18514270861186,
9.87195746698897));
#34708=CARTESIAN_POINT('Ctrl Pts',(-4.15018848428161,-1.06847604194516,
9.88563419569662));
#34709=CARTESIAN_POINT('Ctrl Pts',(-4.07749218647761,-0.794772684000863,
9.89557653288265));
#34710=CARTESIAN_POINT('Ctrl Pts',(-4.01658172222461,-0.636309800095205,
9.86589371255771));
#34711=CARTESIAN_POINT('Ctrl Pts',(-3.94347564908434,-0.319434907277163,
9.85153423006119));
#34712=CARTESIAN_POINT('Ctrl Pts',(-3.90629110283546,-0.158333333333335,
9.83320656333423));
#34713=CARTESIAN_POINT('Ctrl Pts',(-3.88863762367487,0.158333333333336,
9.85919366497471));
#34714=CARTESIAN_POINT('Ctrl Pts',(-3.9077196744278,0.319434907277172,9.90417613627861));
#34715=CARTESIAN_POINT('Ctrl Pts',(-3.94578149555549,0.636309800095215,
9.97010941087807));
#34716=CARTESIAN_POINT('Ctrl Pts',(-3.98670278361234,0.79477268400085,10.02798434251));
#34717=CARTESIAN_POINT('Ctrl Pts',(-4.03428693524991,1.06847604194588,10.0571205549456));
#34718=CARTESIAN_POINT('Ctrl Pts',(-4.05365640950548,1.18514270861328,10.0583942458085));
#34719=CARTESIAN_POINT('Ctrl Pts',(-4.07179794193922,1.30000000000222,10.048329640774));
#34720=CARTESIAN_POINT('Ctrl Pts',(-4.20040784106706,-1.3000000000001,9.84298435754321));
#34721=CARTESIAN_POINT('Ctrl Pts',(-4.1743076309958,-1.18514270861185,9.86491912305311));
#34722=CARTESIAN_POINT('Ctrl Pts',(-4.14536838919967,-1.06847604194516,
9.87776936096711));
#34723=CARTESIAN_POINT('Ctrl Pts',(-4.07195422014435,-0.794772684000861,
9.88646890512968));
#34724=CARTESIAN_POINT('Ctrl Pts',(-4.0112364048357,-0.636309800095204,
9.85693508166246));
#34725=CARTESIAN_POINT('Ctrl Pts',(-3.93821104618483,-0.319434907277162,
9.84243266425045));
#34726=CARTESIAN_POINT('Ctrl Pts',(-3.90131968533194,-0.158333333333334,
9.82440782567619));
#34727=CARTESIAN_POINT('Ctrl Pts',(-3.88379015100995,0.158333333333336,
9.85027179693815));
#34728=CARTESIAN_POINT('Ctrl Pts',(-3.90263894184727,0.31943490727717,9.89488746204669));
#34729=CARTESIAN_POINT('Ctrl Pts',(-3.94100291802066,0.636309800095213,
9.96059237479716));
#34730=CARTESIAN_POINT('Ctrl Pts',(-3.98231865005701,0.794772684000848,
10.017752737638));
#34731=CARTESIAN_POINT('Ctrl Pts',(-4.03063693422305,1.06847604194588,10.0481259924018));
#34732=CARTESIAN_POINT('Ctrl Pts',(-4.05037942106035,1.18514270861328,10.050368943366));
#34733=CARTESIAN_POINT('Ctrl Pts',(-4.06894919988829,1.30000000000222,10.0417073887471));
#34734=CARTESIAN_POINT('Ctrl Pts',(-4.1968256822688,-1.3000000000001,9.83705064195634));
#34735=CARTESIAN_POINT('Ctrl Pts',(-4.1700044681053,-1.18514270861185,9.85787241418812));
#34736=CARTESIAN_POINT('Ctrl Pts',(-4.14054247363241,-1.06847604194516,
9.86990432345096));
#34737=CARTESIAN_POINT('Ctrl Pts',(-4.06637864174727,-0.79477268400086,
9.87739409895908));
#34738=CARTESIAN_POINT('Ctrl Pts',(-4.00580735908187,-0.636309800095204,
9.84805992860588));
#34739=CARTESIAN_POINT('Ctrl Pts',(-3.93282936913909,-0.319434907277162,
9.83345069349348));
#34740=CARTESIAN_POINT('Ctrl Pts',(-3.89622042641662,-0.158333333333334,
9.81574129977556));
#34741=CARTESIAN_POINT('Ctrl Pts',(-3.87882705640936,0.158333333333336,
9.84146716804513));
#34742=CARTESIAN_POINT('Ctrl Pts',(-3.8974936901642,0.319434907277171,9.88565824574615));
#34743=CARTESIAN_POINT('Ctrl Pts',(-3.93616078690375,0.636309800095214,
9.95112968001173));
#34744=CARTESIAN_POINT('Ctrl Pts',(-3.97779854689507,0.794772684000848,
10.0076472985041));
#34745=CARTESIAN_POINT('Ctrl Pts',(-4.02687371345706,1.06847604194588,10.0392359805595));
#34746=CARTESIAN_POINT('Ctrl Pts',(-4.04701803744443,1.18514270861328,10.0424206334433));
#34747=CARTESIAN_POINT('Ctrl Pts',(-4.06606386422855,1.30000000000222,10.035116369225));
#34748=CARTESIAN_POINT('Ctrl Pts',(-4.19448001643774,-1.3000000000001,9.83304924992269));
#34749=CARTESIAN_POINT('Ctrl Pts',(-4.16724072708871,-1.18514270861185,
9.85306085170418));
#34750=CARTESIAN_POINT('Ctrl Pts',(-4.13746434556555,-1.06847604194516,
9.86450992596167));
#34751=CARTESIAN_POINT('Ctrl Pts',(-4.06281375703653,-0.79477268400086,
9.87117842636774));
#34752=CARTESIAN_POINT('Ctrl Pts',(-4.00225118025671,-0.636309800095204,
9.84207406594856));
#34753=CARTESIAN_POINT('Ctrl Pts',(-3.92922046485511,-0.319434907277162,
9.82748327159995));
#34754=CARTESIAN_POINT('Ctrl Pts',(-3.89271235913522,-0.158333333333334,
9.81007549925909));
#34755=CARTESIAN_POINT('Ctrl Pts',(-3.87541122126775,0.158333333333336,
9.83570817700522));
#34756=CARTESIAN_POINT('Ctrl Pts',(-3.89409296887522,0.319434907277171,
9.87947571683529));
#34757=CARTESIAN_POINT('Ctrl Pts',(-3.93295234798587,0.636309800095213,
9.94479740068427));
#34758=CARTESIAN_POINT('Ctrl Pts',(-3.97464088946348,0.794772684000847,
10.001046114713));
#34759=CARTESIAN_POINT('Ctrl Pts',(-4.02421355278176,1.06847604194588,10.0334526591426));
#34760=CARTESIAN_POINT('Ctrl Pts',(-4.04465393193101,1.18514270861328,10.0372384894363));
#34761=CARTESIAN_POINT('Ctrl Pts',(-4.06407652112715,1.30000000000222,10.0307825577209));
#34762=CARTESIAN_POINT('Ctrl Pts',(-4.19292299273677,-1.3000000000001,9.83037415643151));
#34763=CARTESIAN_POINT('Ctrl Pts',(-4.1654137661498,-1.18514270861185,9.8498359998899));
#34764=CARTESIAN_POINT('Ctrl Pts',(-4.13543275923749,-1.06847604194516,
9.86089103928364));
#34765=CARTESIAN_POINT('Ctrl Pts',(-4.06046032856068,-0.79477268400086,
9.86700899267152));
#34766=CARTESIAN_POINT('Ctrl Pts',(-3.99989325823722,-0.636309800095204,
9.83806908637676));
#34767=CARTESIAN_POINT('Ctrl Pts',(-3.92681497328307,-0.319434907277162,
9.82350388919076));
#34768=CARTESIAN_POINT('Ctrl Pts',(-3.89035937021541,-0.158333333333334,
9.80631285247433));
#34769=CARTESIAN_POINT('Ctrl Pts',(-3.87311760228999,0.158333333333336,
9.83188568740066));
#34770=CARTESIAN_POINT('Ctrl Pts',(-3.89182538863478,0.319434907277171,
9.8753541709064));
#34771=CARTESIAN_POINT('Ctrl Pts',(-3.93081421873702,0.636309800095213,
9.94057414790096));
#34772=CARTESIAN_POINT('Ctrl Pts',(-3.97252364569437,0.794772684000847,
9.99665590741682));
#34773=CARTESIAN_POINT('Ctrl Pts',(-4.02242720258882,1.06847604194588,10.0296086204888));
#34774=CARTESIAN_POINT('Ctrl Pts',(-4.04306684180308,1.18514270861328,10.0337936350233));
#34775=CARTESIAN_POINT('Ctrl Pts',(-4.06274471956094,1.30000000000222,10.0278996556217));
#34776=CARTESIAN_POINT('Ctrl Pts',(-4.18867884642207,-1.3000000000001,9.82297686484869));
#34777=CARTESIAN_POINT('Ctrl Pts',(-4.16048043130391,-1.18514270861185,
9.84086892551032));
#34778=CARTESIAN_POINT('Ctrl Pts',(-4.12996650707679,-1.06847604194516,
9.85080774886732));
#34779=CARTESIAN_POINT('Ctrl Pts',(-4.05412394856475,-0.79477268400086,
9.85539484986342));
#34780=CARTESIAN_POINT('Ctrl Pts',(-3.99347745659756,-0.636309800095204,
9.82698000795613));
#34781=CARTESIAN_POINT('Ctrl Pts',(-3.92019730142325,-0.319434907277162,
9.81256084403552));
#34782=CARTESIAN_POINT('Ctrl Pts',(-3.88380645695757,-0.158333333333334,
9.79604955309708));
#34783=CARTESIAN_POINT('Ctrl Pts',(-3.86672209666436,0.158333333333336,
9.82146449407055));
#34784=CARTESIAN_POINT('Ctrl Pts',(-3.88560788011893,0.319434907277171,
9.86400104662747));
#34785=CARTESIAN_POINT('Ctrl Pts',(-3.92494536056161,0.636309800095213,
9.92894543616526));
#34786=CARTESIAN_POINT('Ctrl Pts',(-3.96659069941214,0.794772684000848,
9.98468540910302));
#34787=CARTESIAN_POINT('Ctrl Pts',(-4.0173955002244,1.06847604194588,10.0191495270543));
#34788=CARTESIAN_POINT('Ctrl Pts',(-4.03860173661218,1.18514270861328,10.0244152737678));
#34789=CARTESIAN_POINT('Ctrl Pts',(-4.05902269361942,1.30000000000222,10.0200285275551));
#34790=CARTESIAN_POINT('Ctrl Pts',(-4.18327543477343,-1.3000000000001,9.81355715492352));
#34791=CARTESIAN_POINT('Ctrl Pts',(-4.15419431067351,-1.18514270861185,
9.82945370324904));
#34792=CARTESIAN_POINT('Ctrl Pts',(-4.12300938712133,-1.06847604194515,
9.83796172973357));
#34793=CARTESIAN_POINT('Ctrl Pts',(-4.04610577759482,-0.794772684000857,
9.84054800941627));
#34794=CARTESIAN_POINT('Ctrl Pts',(-3.98547441096753,-0.636309800095203,
9.81267820358621));
#34795=CARTESIAN_POINT('Ctrl Pts',(-3.91194208684675,-0.319434907277162,
9.7984430963628));
#34796=CARTESIAN_POINT('Ctrl Pts',(-3.87555616930008,-0.158333333333334,
9.78288741997211));
#34797=CARTESIAN_POINT('Ctrl Pts',(-3.85858039408216,0.158333333333336,
9.8081980387313));
#34798=CARTESIAN_POINT('Ctrl Pts',(-3.87752872335823,0.319434907277171,
9.84970799273135));
#34799=CARTESIAN_POINT('Ctrl Pts',(-3.91742329559321,0.636309800095213,
9.9141879212094));
#34800=CARTESIAN_POINT('Ctrl Pts',(-3.95944359784781,0.794772684000847,
9.96903623482389));
#34801=CARTESIAN_POINT('Ctrl Pts',(-4.0114028600779,1.06847604194588,10.0054193555547));
#34802=CARTESIAN_POINT('Ctrl Pts',(-4.03323521473105,1.18514270861328,10.0121574872712));
#34803=CARTESIAN_POINT('Ctrl Pts',(-4.05440868469828,1.30000000000222,10.0098848458672));
#34804=CARTESIAN_POINT('Ctrl Pts',(-4.17689145237611,-1.3000000000001,9.80301252814214));
#34805=CARTESIAN_POINT('Ctrl Pts',(-4.1465997387043,-1.18514270861185,9.81684487549646));
#34806=CARTESIAN_POINT('Ctrl Pts',(-4.11450022071243,-1.06847604194516,
9.82387604727132));
#34807=CARTESIAN_POINT('Ctrl Pts',(-4.03616752303527,-0.794772684000861,
9.82440738449327));
#34808=CARTESIAN_POINT('Ctrl Pts',(-3.97545993580296,-0.636309800095203,
9.79726188892626));
#34809=CARTESIAN_POINT('Ctrl Pts',(-3.9018874991181,-0.319434907277162,
9.78296702519706));
#34810=CARTESIAN_POINT('Ctrl Pts',(-3.86605396024536,-0.158333333333334,
9.76791040528507));
#34811=CARTESIAN_POINT('Ctrl Pts',(-3.84946804647695,0.158333333333336,
9.79281292514629));
#34812=CARTESIAN_POINT('Ctrl Pts',(-3.86849596672761,0.31943490727717,9.83315145538546));
#34813=CARTESIAN_POINT('Ctrl Pts',(-3.90873161425928,0.636309800095212,
9.89739816796892));
#34814=CARTESIAN_POINT('Ctrl Pts',(-3.950382362248,0.794772684000848,9.95203175065576));
#34815=CARTESIAN_POINT('Ctrl Pts',(-4.00371999356563,1.06847604194588,9.99054841316902));
#34816=CARTESIAN_POINT('Ctrl Pts',(-4.02649062745679,1.18514270861328,9.99874474446717));
#34817=CARTESIAN_POINT('Ctrl Pts',(-4.04894401099567,1.30000000000222,9.99846497104443));
#34818=CARTESIAN_POINT('Ctrl Pts',(-4.17047928941036,-1.30000000000009,
9.79249304649564));
#34819=CARTESIAN_POINT('Ctrl Pts',(-4.13894720136848,-1.18514270861185,
9.80429279693164));
#34820=CARTESIAN_POINT('Ctrl Pts',(-4.10591112926829,-1.06847604194515,
9.80987067792703));
#34821=CARTESIAN_POINT('Ctrl Pts',(-4.02611668982759,-0.794772684000857,
9.80838293578912));
#34822=CARTESIAN_POINT('Ctrl Pts',(-3.96535321334187,-0.636309800095201,
9.78194278190101));
#34823=CARTESIAN_POINT('Ctrl Pts',(-3.89170712988408,-0.319434907277161,
9.76762399515949));
#34824=CARTESIAN_POINT('Ctrl Pts',(-3.85635262368045,-0.158333333333334,
9.75314386280003));
#34825=CARTESIAN_POINT('Ctrl Pts',(-3.84017053254468,0.158333333333335,
9.77761910141739));
#34826=CARTESIAN_POINT('Ctrl Pts',(-3.85937613224551,0.319434907277171,
9.81667709579077));
#34827=CARTESIAN_POINT('Ctrl Pts',(-3.899992866501,0.636309800095212,9.8806411448506));
#34828=CARTESIAN_POINT('Ctrl Pts',(-3.9412868762951,0.794772684000845,9.93503778605955));
#34829=CARTESIAN_POINT('Ctrl Pts',(-3.9959273914875,1.06847604194587,9.97577138358011));
#34830=CARTESIAN_POINT('Ctrl Pts',(-4.01958056028507,1.18514270861328,9.98548958062305));
#34831=CARTESIAN_POINT('Ctrl Pts',(-4.04323504348396,1.30000000000222,9.98729390967078));
#34832=CARTESIAN_POINT('Ctrl Pts',(-4.1623027602077,-1.30000000000009,9.77952294110834));
#34833=CARTESIAN_POINT('Ctrl Pts',(-4.12916991535113,-1.18514270861185,
9.78883210821292));
#34834=CARTESIAN_POINT('Ctrl Pts',(-4.09501090828536,-1.06847604194515,
9.79253669957329));
#34835=CARTESIAN_POINT('Ctrl Pts',(-4.01372612849118,-0.794772684000858,
9.78814735555604));
#34836=CARTESIAN_POINT('Ctrl Pts',(-3.95376169659582,-0.636309800095203,
9.76163075512583));
#34837=CARTESIAN_POINT('Ctrl Pts',(-3.88005908306621,-0.319434907277162,
9.74724167966076));
#34838=CARTESIAN_POINT('Ctrl Pts',(-3.84471622657658,-0.158333333333334,
9.73414067785112));
#34839=CARTESIAN_POINT('Ctrl Pts',(-3.82837867217028,0.158333333333335,
9.75878967722972));
#34840=CARTESIAN_POINT('Ctrl Pts',(-3.84695230195744,0.319434907277168,
9.79712332573153));
#34841=CARTESIAN_POINT('Ctrl Pts',(-3.88825577889028,0.636309800095211,
9.86053179059021));
#34842=CARTESIAN_POINT('Ctrl Pts',(-3.9307976075957,0.794772684000848,9.91290040708799));
#34843=CARTESIAN_POINT('Ctrl Pts',(-3.98709463873616,1.06847604194588,9.95638684629109));
#34844=CARTESIAN_POINT('Ctrl Pts',(-4.01151951885904,1.18514270861328,9.96835168815166));
#34845=CARTESIAN_POINT('Ctrl Pts',(-4.03600038033461,1.30000000000221,9.97345770367308));
#34846=CARTESIAN_POINT('Ctrl Pts',(-4.15271715219705,-1.30000000000009,
9.76367829885413));
#34847=CARTESIAN_POINT('Ctrl Pts',(-4.11773142355429,-1.18514270861185,
9.76992275657636));
#34848=CARTESIAN_POINT('Ctrl Pts',(-4.08214402329409,-1.06847604194515,
9.77146808850168));
#34849=CARTESIAN_POINT('Ctrl Pts',(-3.99854002765769,-0.794772684000857,
9.764182193744));
#34850=CARTESIAN_POINT('Ctrl Pts',(-3.93818305842922,-0.636309800095199,
9.7390655135235));
#34851=CARTESIAN_POINT('Ctrl Pts',(-3.86437826392957,-0.319434907277159,
9.72463233575177));
#34852=CARTESIAN_POINT('Ctrl Pts',(-3.83016010562027,-0.158333333333333,
9.71196014514568));
#34853=CARTESIAN_POINT('Ctrl Pts',(-3.81435573406753,0.158333333333335,
9.73603306311532));
#34854=CARTESIAN_POINT('Ctrl Pts',(-3.83272201883899,0.319434907277169,
9.77293474300738));
#34855=CARTESIAN_POINT('Ctrl Pts',(-3.87443120456167,0.636309800095209,
9.83608379687782));
#34856=CARTESIAN_POINT('Ctrl Pts',(-3.91637856299569,0.794772684000842,
9.88815189746707));
#34857=CARTESIAN_POINT('Ctrl Pts',(-3.97509502513964,1.06847604194587,9.93448054688383));
#34858=CARTESIAN_POINT('Ctrl Pts',(-4.00117540355945,1.18514270861327,9.94838567794813));
#34859=CARTESIAN_POINT('Ctrl Pts',(-4.02791997959621,1.30000000000221,9.95614198438979));
#34860=CARTESIAN_POINT('Ctrl Pts',(-4.14458288155458,-1.30000000000009,
9.75064115448924));
#34861=CARTESIAN_POINT('Ctrl Pts',(-4.10811453968855,-1.18514270861185,
9.75424928515064));
#34862=CARTESIAN_POINT('Ctrl Pts',(-4.07135896780956,-1.06847604194515,
9.75396300487519));
#34863=CARTESIAN_POINT('Ctrl Pts',(-3.98578268505204,-0.794772684000857,
9.74430477183034));
#34864=CARTESIAN_POINT('Ctrl Pts',(-3.92497542566649,-0.636309800095201,
9.72052245946643));
#34865=CARTESIAN_POINT('Ctrl Pts',(-3.85084161620007,-0.319434907277161,
9.70632290465302));
#34866=CARTESIAN_POINT('Ctrl Pts',(-3.81721658744817,-0.158333333333333,
9.69437078927507));
#34867=CARTESIAN_POINT('Ctrl Pts',(-3.80187495488852,0.158333333333335,
9.71792536556004));
#34868=CARTESIAN_POINT('Ctrl Pts',(-3.82021028003475,0.319434907277167,
9.75343912820627));
#34869=CARTESIAN_POINT('Ctrl Pts',(-3.86298851307109,0.636309800095209,
9.81560325584252));
#34870=CARTESIAN_POINT('Ctrl Pts',(-3.90596293721407,0.794772684000845,
9.86587151787597));
#34871=CARTESIAN_POINT('Ctrl Pts',(-3.96639767861555,1.06847604194587,9.91489479795498));
#34872=CARTESIAN_POINT('Ctrl Pts',(-3.99329518192105,1.18514270861328,9.93100668664934));
#34873=CARTESIAN_POINT('Ctrl Pts',(-4.02093022830713,1.30000000000221,9.94201010258334));
#34874=CARTESIAN_POINT('Ctrl Pts',(-4.13792080370513,-1.30000000000009,
9.7403656665557));
#34875=CARTESIAN_POINT('Ctrl Pts',(-4.09991568165613,-1.18514270861185,
9.7422691668776));
#34876=CARTESIAN_POINT('Ctrl Pts',(-4.06208162057071,-1.06847604194515,
9.74068441285067));
#34877=CARTESIAN_POINT('Ctrl Pts',(-3.97507255583187,-0.794772684000857,
9.72896474865087));
#34878=CARTESIAN_POINT('Ctrl Pts',(-3.91499224411171,-0.636309800095201,
9.70500070162394));
#34879=CARTESIAN_POINT('Ctrl Pts',(-3.84087419871896,-0.31943490727716,
9.69067377855575));
#34880=CARTESIAN_POINT('Ctrl Pts',(-3.80740469694953,-0.158333333333333,
9.67968200748737));
#34881=CARTESIAN_POINT('Ctrl Pts',(-3.79197211150342,0.158333333333335,
9.70333725927779));
#34882=CARTESIAN_POINT('Ctrl Pts',(-3.80990338042646,0.319434907277168,
9.73816695474585));
#34883=CARTESIAN_POINT('Ctrl Pts',(-3.85280155659604,0.636309800095209,
9.80030583152426));
#34884=CARTESIAN_POINT('Ctrl Pts',(-3.89559684856876,0.794772684000844,
9.85012092965609));
#34885=CARTESIAN_POINT('Ctrl Pts',(-3.9576382974083,1.06847604194587,9.90105238271874));
#34886=CARTESIAN_POINT('Ctrl Pts',(-3.98560809415924,1.18514270861328,9.91850102054971));
#34887=CARTESIAN_POINT('Ctrl Pts',(-4.01469224332062,1.30000000000221,9.93135195737708));
#34888=CARTESIAN_POINT('Ctrl Pts',(-4.1278777586158,-1.30000000000009,9.7250220110376));
#34889=CARTESIAN_POINT('Ctrl Pts',(-4.08773437020547,-1.18514270861184,
9.72417262169841));
#34890=CARTESIAN_POINT('Ctrl Pts',(-4.04832068672469,-1.06847604194515,
9.72059219835672));
#34891=CARTESIAN_POINT('Ctrl Pts',(-3.95895295756798,-0.794772684000853,
9.70601146928899));
#34892=CARTESIAN_POINT('Ctrl Pts',(-3.8992301361605,-0.636309800095199,
9.6826078545982));
#34893=CARTESIAN_POINT('Ctrl Pts',(-3.82480580924965,-0.31943490727716,
9.66846543483889));
#34894=CARTESIAN_POINT('Ctrl Pts',(-3.79137440572589,-0.158333333333333,
9.65913160969459));
#34895=CARTESIAN_POINT('Ctrl Pts',(-3.7765073752783,0.158333333333335,9.68215845182108));
#34896=CARTESIAN_POINT('Ctrl Pts',(-3.79520088663898,0.319434907277168,
9.71442671474825));
#34897=CARTESIAN_POINT('Ctrl Pts',(-3.83907909760253,0.636309800095208,
9.77566137492616));
#34898=CARTESIAN_POINT('Ctrl Pts',(-3.88150208085316,0.794772684000841,
9.82497614627297));
#34899=CARTESIAN_POINT('Ctrl Pts',(-3.94580247883527,1.06847604194587,9.87893518081619));
#34900=CARTESIAN_POINT('Ctrl Pts',(-3.97522304931586,1.18514270861327,9.89854771494412));
#34901=CARTESIAN_POINT('Ctrl Pts',(-4.00623093055504,1.30000000000221,9.91441591652541));
#34902=CARTESIAN_POINT('Ctrl Pts',(-4.11635470812674,-1.3000000000001,9.70687190739252));
#34903=CARTESIAN_POINT('Ctrl Pts',(-4.07409459096131,-1.18514270861185,
9.70235142307796));
#34904=CARTESIAN_POINT('Ctrl Pts',(-4.03300344320846,-1.06847604194515,
9.6962394264141));
#34905=CARTESIAN_POINT('Ctrl Pts',(-3.94077522483799,-0.794772684000855,
9.67844277951203));
#34906=CARTESIAN_POINT('Ctrl Pts',(-3.88026343239008,-0.636309800095201,
9.65713349321762));
#34907=CARTESIAN_POINT('Ctrl Pts',(-3.80545909140476,-0.319434907277161,
9.64323923547767));
#34908=CARTESIAN_POINT('Ctrl Pts',(-3.77335449162494,-0.158333333333333,
9.63435059380748));
#34909=CARTESIAN_POINT('Ctrl Pts',(-3.75885308043993,0.158333333333335,
9.65694128325831));
#34910=CARTESIAN_POINT('Ctrl Pts',(-3.77669857829229,0.319434907277168,
9.68815090112606));
#34911=CARTESIAN_POINT('Ctrl Pts',(-3.82147102231926,0.636309800095209,
9.74861015317067));
#34912=CARTESIAN_POINT('Ctrl Pts',(-3.86480586979095,0.794772684000845,
9.7958608588833));
#34913=CARTESIAN_POINT('Ctrl Pts',(-3.93202952355851,1.06847604194587,9.85304439935273));
#34914=CARTESIAN_POINT('Ctrl Pts',(-3.96309385828612,1.18514270861328,9.87524035766234));
#34915=CARTESIAN_POINT('Ctrl Pts',(-3.99612389890713,1.30000000000221,9.89487963847128));
#34916=CARTESIAN_POINT('Ctrl Pts',(-4.10202300360559,-1.30000000000009,
9.68751099507706));
#34917=CARTESIAN_POINT('Ctrl Pts',(-4.05666990056074,-1.18514270861184,
9.67958214782389));
#34918=CARTESIAN_POINT('Ctrl Pts',(-4.01334637963241,-1.06847604194515,
9.67094158349285));
#34919=CARTESIAN_POINT('Ctrl Pts',(-3.91794912015298,-0.794772684000855,
9.64933594252076));
#34920=CARTESIAN_POINT('Ctrl Pts',(-3.85840997143452,-0.636309800095199,
9.62819587095804));
#34921=CARTESIAN_POINT('Ctrl Pts',(-3.78334012526085,-0.31943490727716,
9.6143824976442));
#34922=CARTESIAN_POINT('Ctrl Pts',(-3.75139511139691,-0.158333333333333,
9.60762197008548));
#34923=CARTESIAN_POINT('Ctrl Pts',(-3.73708422400504,0.158333333333335,
9.62997188908506));
#34924=CARTESIAN_POINT('Ctrl Pts',(-3.75477217548896,0.319434907277168,
9.65900825018191));
#34925=CARTESIAN_POINT('Ctrl Pts',(-3.80058213678986,0.636309800095208,
9.71849770600095));
#34926=CARTESIAN_POINT('Ctrl Pts',(-3.84417322803187,0.794772684000842,
9.764189669864));
#34927=CARTESIAN_POINT('Ctrl Pts',(-3.9148570456614,1.06847604194587,9.824923839085));
#34928=CARTESIAN_POINT('Ctrl Pts',(-3.94802895223982,1.18514270861327,9.84983730924623));
#34929=CARTESIAN_POINT('Ctrl Pts',(-3.98377635983831,1.30000000000221,9.8733746781356));
#34930=CARTESIAN_POINT('Ctrl Pts',(-4.09223550484063,-1.30000000000009,
9.67180067703011));
#34931=CARTESIAN_POINT('Ctrl Pts',(-4.04492506092978,-1.18514270861184,
9.66088402866375));
#34932=CARTESIAN_POINT('Ctrl Pts',(-4.00004421825906,-1.06847604194515,
9.65020916578641));
#34933=CARTESIAN_POINT('Ctrl Pts',(-3.90197335821266,-0.794772684000854,
9.62610666988942));
#34934=CARTESIAN_POINT('Ctrl Pts',(-3.84178364041155,-0.636309800095198,
9.60674608144195));
#34935=CARTESIAN_POINT('Ctrl Pts',(-3.76608130219754,-0.319434907277159,
9.59351969773874));
#34936=CARTESIAN_POINT('Ctrl Pts',(-3.73471560689843,-0.158333333333333,
9.58781315447167));
#34937=CARTESIAN_POINT('Ctrl Pts',(-3.72083677057423,0.158333333333335,
9.60964344590414));
#34938=CARTESIAN_POINT('Ctrl Pts',(-3.73860850554392,0.319434907277169,
9.63679929512494));
#34939=CARTESIAN_POINT('Ctrl Pts',(-3.78546038158528,0.636309800095208,
9.69526845063128));
#34940=CARTESIAN_POINT('Ctrl Pts',(-3.82955687974671,0.794772684000841,
9.73947794767306));
#34941=CARTESIAN_POINT('Ctrl Pts',(-3.90259112333981,1.06847604194587,9.80315290720977));
#34942=CARTESIAN_POINT('Ctrl Pts',(-3.93709699733448,1.18514270861327,9.83037577538033));
#34943=CARTESIAN_POINT('Ctrl Pts',(-3.97449492745768,1.30000000000221,9.85725898112772));
#34944=CARTESIAN_POINT('Ctrl Pts',(-4.08088288391462,-1.30000000000009,
9.65800792817637));
#34945=CARTESIAN_POINT('Ctrl Pts',(-4.0310277457008,-1.18514270861184,9.6448068787467));
#34946=CARTESIAN_POINT('Ctrl Pts',(-3.98431745788211,-1.06847604194514,
9.63242188925164));
#34947=CARTESIAN_POINT('Ctrl Pts',(-3.88367258219778,-0.794772684000849,
9.60569534761062));
#34948=CARTESIAN_POINT('Ctrl Pts',(-3.82416264746573,-0.636309800095196,
9.58651222178451));
#34949=CARTESIAN_POINT('Ctrl Pts',(-3.74862535627239,-0.319434907277159,
9.57290001362148));
#34950=CARTESIAN_POINT('Ctrl Pts',(-3.71821062371238,-0.158333333333333,
9.5677937300466));
#34951=CARTESIAN_POINT('Ctrl Pts',(-3.70451747313622,0.158333333333334,
9.58937323654366));
#34952=CARTESIAN_POINT('Ctrl Pts',(-3.72141492809999,0.319434907277168,
9.61578986157383));
#34953=CARTESIAN_POINT('Ctrl Pts',(-3.76870201691248,0.636309800095208,
9.67390624050485));
#34954=CARTESIAN_POINT('Ctrl Pts',(-3.81278249322028,0.79477268400084,9.71712672772544));
#34955=CARTESIAN_POINT('Ctrl Pts',(-3.88891793965976,1.06847604194587,9.78289475248831));
#34956=CARTESIAN_POINT('Ctrl Pts',(-3.92540934858402,1.18514270861327,9.81171155206745));
#34957=CARTESIAN_POINT('Ctrl Pts',(-3.96543595276512,1.30000000000221,9.84087661025131));
#34958=CARTESIAN_POINT('Ctrl Pts',(-4.07272838886402,-1.30000000000009,
9.64488009164317));
#34959=CARTESIAN_POINT('Ctrl Pts',(-4.02104634242638,-1.18514270861184,
9.62941756709542));
#34960=CARTESIAN_POINT('Ctrl Pts',(-3.97289920341682,-1.06847604194515,
9.61550255020163));
#34961=CARTESIAN_POINT('Ctrl Pts',(-3.86983602381723,-0.794772684000853,
9.58693112974593));
#34962=CARTESIAN_POINT('Ctrl Pts',(-3.80992709147984,-0.636309800095198,
9.56908533013396));
#34963=CARTESIAN_POINT('Ctrl Pts',(-3.73373118466259,-0.31943490727716,
9.55613499866793));
#34964=CARTESIAN_POINT('Ctrl Pts',(-3.70354447410378,-0.158333333333333,
9.55222294139156));
#34965=CARTESIAN_POINT('Ctrl Pts',(-3.69014793205364,0.158333333333334,
9.5734258816163));
#34966=CARTESIAN_POINT('Ctrl Pts',(-3.70716886738543,0.319434907277167,
9.59816262664611));
#34967=CARTESIAN_POINT('Ctrl Pts',(-3.75560692722669,0.636309800095207,
9.65507229373653));
#34968=CARTESIAN_POINT('Ctrl Pts',(-3.80062603915456,0.794772684000841,
9.69646175637529));
#34969=CARTESIAN_POINT('Ctrl Pts',(-3.87879994236377,1.06847604194587,9.76458752472658));
#34970=CARTESIAN_POINT('Ctrl Pts',(-3.91632666232639,1.18514270861327,9.79541903485025));
#34971=CARTESIAN_POINT('Ctrl Pts',(-3.95754151618084,1.30000000000221,9.82759293428673));
#34972=CARTESIAN_POINT('Ctrl Pts',(-4.06138621253067,-1.30000000000009,
9.63106202969797));
#34973=CARTESIAN_POINT('Ctrl Pts',(-4.00730211428524,-1.18514270861184,
9.61313433541102));
#34974=CARTESIAN_POINT('Ctrl Pts',(-3.95736582749986,-1.06847604194515,
9.59745646095828));
#34975=CARTESIAN_POINT('Ctrl Pts',(-3.85158528954522,-0.794772684000852,
9.56643496851635));
#34976=CARTESIAN_POINT('Ctrl Pts',(-3.79178142684599,-0.636309800095198,
9.54948273309652));
#34977=CARTESIAN_POINT('Ctrl Pts',(-3.71552477875022,-0.31943490727716,
9.53642279036497));
#34978=CARTESIAN_POINT('Ctrl Pts',(-3.68634494508279,-0.158333333333333,
9.5330333244766));
#34979=CARTESIAN_POINT('Ctrl Pts',(-3.67337150255953,0.158333333333334,
9.55369078341368));
#34980=CARTESIAN_POINT('Ctrl Pts',(-3.68994656139196,0.319434907277167,
9.57716760640096));
#34981=CARTESIAN_POINT('Ctrl Pts',(-3.73902629165065,0.636309800095207,
9.6334665619966));
#34982=CARTESIAN_POINT('Ctrl Pts',(-3.78402389339273,0.794772684000841,
9.67387788185577));
#34983=CARTESIAN_POINT('Ctrl Pts',(-3.86502638086352,1.06847604194587,9.74440089113378));
#34984=CARTESIAN_POINT('Ctrl Pts',(-3.90434124164542,1.18514270861327,9.77704838131755));
#34985=CARTESIAN_POINT('Ctrl Pts',(-3.94790798782096,1.30000000000221,9.81181656410356));
#34986=CARTESIAN_POINT('Ctrl Pts',(-4.04716422159609,-1.30000000000008,
9.61149186781036));
#34987=CARTESIAN_POINT('Ctrl Pts',(-3.9900803286236,-1.18514270861184,9.59001943537044));
#34988=CARTESIAN_POINT('Ctrl Pts',(-3.9378059472672,-1.06847604194515,9.57193282854236));
#34989=CARTESIAN_POINT('Ctrl Pts',(-3.8281526028524,-0.794772684000852,
9.53797108305162));
#34990=CARTESIAN_POINT('Ctrl Pts',(-3.76783820314362,-0.636309800095198,
9.52306019173905));
#34991=CARTESIAN_POINT('Ctrl Pts',(-3.69064922620234,-0.31943490727716,
9.51093114831833));
#34992=CARTESIAN_POINT('Ctrl Pts',(-3.66194871726299,-0.158333333333333,
9.50931618908867));
#34993=CARTESIAN_POINT('Ctrl Pts',(-3.64945527695434,0.158333333333334,
9.52932029129036));
#34994=CARTESIAN_POINT('Ctrl Pts',(-3.66631284837025,0.319434907277167,
9.54995749515016));
#34995=CARTESIAN_POINT('Ctrl Pts',(-3.71672855962466,0.636309800095207,
9.60483342758972));
#34996=CARTESIAN_POINT('Ctrl Pts',(-3.7618242424883,0.794772684000842,9.64385514916113));
#34997=CARTESIAN_POINT('Ctrl Pts',(-3.8465484654073,1.06847604194587,9.71762767022338));
#34998=CARTESIAN_POINT('Ctrl Pts',(-3.88814294340621,1.18514270861327,9.75280796524565));
#34999=CARTESIAN_POINT('Ctrl Pts',(-3.93465792264413,1.30000000000221,9.79123516446356));
#35000=CARTESIAN_POINT('Ctrl Pts',(-4.02999794901952,-1.30000000000008,
9.59094278729835));
#35001=CARTESIAN_POINT('Ctrl Pts',(-3.96900965522733,-1.18514270861183,
9.5661695695801));
#35002=CARTESIAN_POINT('Ctrl Pts',(-3.91382227090955,-1.06847604194514,
9.54574039801195));
#35003=CARTESIAN_POINT('Ctrl Pts',(-3.79972963429092,-0.794772684000849,
9.508580540478));
#35004=CARTESIAN_POINT('Ctrl Pts',(-3.73982716968739,-0.636309800095198,
9.4946692715688));
#35005=CARTESIAN_POINT('Ctrl Pts',(-3.66196688951287,-0.319434907277161,
9.48314438624894));
#35006=CARTESIAN_POINT('Ctrl Pts',(-3.633791005323,-0.158333333333332,9.4836530037158));
#35007=CARTESIAN_POINT('Ctrl Pts',(-3.62157560849388,0.158333333333334,
9.50325490140512));
#35008=CARTESIAN_POINT('Ctrl Pts',(-3.63788921901196,0.319434907277164,
9.52169048774121));
#35009=CARTESIAN_POINT('Ctrl Pts',(-3.6901483289376,0.636309800095204,9.57448270236182));
#35010=CARTESIAN_POINT('Ctrl Pts',(-3.73668867689305,0.794772684000843,
9.61023444256769));
#35011=CARTESIAN_POINT('Ctrl Pts',(-3.82637409362723,1.06847604194587,9.68670843100664));
#35012=CARTESIAN_POINT('Ctrl Pts',(-3.87074606138443,1.18514270861327,9.72449403600665));
#35013=CARTESIAN_POINT('Ctrl Pts',(-3.92066850316669,1.3000000000022,9.76696249005188));
#35014=CARTESIAN_POINT('Ctrl Pts',(-4.01715577671309,-1.30000000000008,
9.57427610753466));
#35015=CARTESIAN_POINT('Ctrl Pts',(-3.95336640312922,-1.18514270861184,
9.54660857832973));
#35016=CARTESIAN_POINT('Ctrl Pts',(-3.89592815820484,-1.06847604194514,
9.52433493947444));
#35017=CARTESIAN_POINT('Ctrl Pts',(-3.77790669969032,-0.794772684000849,
9.48533934364431));
#35018=CARTESIAN_POINT('Ctrl Pts',(-3.71674723482175,-0.636309800095197,
9.47438761560753));
#35019=CARTESIAN_POINT('Ctrl Pts',(-3.63816837785436,-0.319434907277159,
9.46357932395661));
#35020=CARTESIAN_POINT('Ctrl Pts',(-3.61155232655921,-0.158333333333332,
9.46411500242012));
#35021=CARTESIAN_POINT('Ctrl Pts',(-3.59992805160763,0.158333333333334,
9.48285863809054));
#35022=CARTESIAN_POINT('Ctrl Pts',(-3.6157130109624,0.319434907277166,9.49975938519163));
#35023=CARTESIAN_POINT('Ctrl Pts',(-3.66899840014624,0.636309800095205,
9.55140980597997));
#35024=CARTESIAN_POINT('Ctrl Pts',(-3.71596769087412,0.79477268400084,9.58543622672668));
#35025=CARTESIAN_POINT('Ctrl Pts',(-3.80909149309595,1.06847604194587,9.66450059946136));
#35026=CARTESIAN_POINT('Ctrl Pts',(-3.85552438516391,1.18514270861327,9.70442591341075));
#35027=CARTESIAN_POINT('Ctrl Pts',(-3.9080803258948,1.3000000000022,9.75005250397632));
#35028=CARTESIAN_POINT('Ctrl Pts',(-4.01049046738461,-1.30000000000008,
9.56625472662844));
#35029=CARTESIAN_POINT('Ctrl Pts',(-3.94503884995572,-1.18514270861183,
9.53748069470923));
#35030=CARTESIAN_POINT('Ctrl Pts',(-3.88636334134026,-1.06847604194514,
9.514425957823));
#35031=CARTESIAN_POINT('Ctrl Pts',(-3.76646534535823,-0.79477268400085,
9.47437761919877));
#35032=CARTESIAN_POINT('Ctrl Pts',(-3.70553200215322,-0.636309800095198,
9.46373730882956));
#35033=CARTESIAN_POINT('Ctrl Pts',(-3.62662698637735,-0.319434907277161,
9.45326350530048));
#35034=CARTESIAN_POINT('Ctrl Pts',(-3.60013762995176,-0.158333333333332,
9.4547533903638));
#35035=CARTESIAN_POINT('Ctrl Pts',(-3.58856078912183,0.158333333333334,
9.47341021636554));
#35036=CARTESIAN_POINT('Ctrl Pts',(-3.60417149421509,0.319434907277165,
9.48937813042208));
#35037=CARTESIAN_POINT('Ctrl Pts',(-3.65807315704533,0.636309800095205,
9.54029687660626));
#35038=CARTESIAN_POINT('Ctrl Pts',(-3.70532264680744,0.794772684000842,
9.57334189081042));
#35039=CARTESIAN_POINT('Ctrl Pts',(-3.8004913239218,1.06847604194587,9.65331202159248));
#35040=CARTESIAN_POINT('Ctrl Pts',(-3.84814442854337,1.18514270861327,9.69409179552363));
#35041=CARTESIAN_POINT('Ctrl Pts',(-3.90225564381061,1.30000000000221,9.74103523695565));
#35042=CARTESIAN_POINT('Ctrl Pts',(-4.00659335599282,-1.30000000000008,
9.56178696274011));
#35043=CARTESIAN_POINT('Ctrl Pts',(-3.94028249235065,-1.18514270861184,
9.53226304267891));
#35044=CARTESIAN_POINT('Ctrl Pts',(-3.88093929508802,-1.06847604194514,
9.50871543648836));
#35045=CARTESIAN_POINT('Ctrl Pts',(-3.75994134105903,-0.794772684000851,
9.46812223610436));
#35046=CARTESIAN_POINT('Ctrl Pts',(-3.69883896773334,-0.636309800095198,
9.45809388202234));
#35047=CARTESIAN_POINT('Ctrl Pts',(-3.61975297932188,-0.31943490727716,
9.44780401461268));
#35048=CARTESIAN_POINT('Ctrl Pts',(-3.59359330179776,-0.158333333333333,
9.44945850523304));
#35049=CARTESIAN_POINT('Ctrl Pts',(-3.58213377403886,0.158333333333334,
9.46793215917097));
#35050=CARTESIAN_POINT('Ctrl Pts',(-3.59755411097818,0.319434907277166,
9.48349796950585));
#35051=CARTESIAN_POINT('Ctrl Pts',(-3.65183089703969,0.636309800095206,
9.53397032962117));
#35052=CARTESIAN_POINT('Ctrl Pts',(-3.69933866067861,0.794772684000842,
9.56633036465978));
#35053=CARTESIAN_POINT('Ctrl Pts',(-3.7956733638959,1.06847604194587,9.64681194796218));
#35054=CARTESIAN_POINT('Ctrl Pts',(-3.84400078616579,1.18514270861327,9.68810289381018));
#35055=CARTESIAN_POINT('Ctrl Pts',(-3.89895590723521,1.30000000000221,9.73584729023102));
#35056=CARTESIAN_POINT('Ctrl Pts',(-4.00072166766443,-1.30000000000008,
9.555143627305));
#35057=CARTESIAN_POINT('Ctrl Pts',(-3.93325540212071,-1.18514270861184,
9.52435152354733));
#35058=CARTESIAN_POINT('Ctrl Pts',(-3.87297212247522,-1.06847604194514,
9.50000972486456));
#35059=CARTESIAN_POINT('Ctrl Pts',(-3.75029982124167,-0.79477268400085,
9.4586767954494));
#35060=CARTESIAN_POINT('Ctrl Pts',(-3.68854925872017,-0.636309800095198,
9.450112526269));
#35061=CARTESIAN_POINT('Ctrl Pts',(-3.60918410847569,-0.319434907277161,
9.44009345725221));
#35062=CARTESIAN_POINT('Ctrl Pts',(-3.58382081815314,-0.158333333333333,
9.44152662577802));
#35063=CARTESIAN_POINT('Ctrl Pts',(-3.57266363030392,0.158333333333334,
9.45954457671088));
#35064=CARTESIAN_POINT('Ctrl Pts',(-3.58775278672523,0.319434907277166,
9.47460764988021));
#35065=CARTESIAN_POINT('Ctrl Pts',(-3.64259283135499,0.636309800095206,
9.52442759976224));
#35066=CARTESIAN_POINT('Ctrl Pts',(-3.69049519762091,0.794772684000843,
9.55577179754062));
#35067=CARTESIAN_POINT('Ctrl Pts',(-3.78853507143873,1.06847604194587,9.63704397580051));
#35068=CARTESIAN_POINT('Ctrl Pts',(-3.83784386572028,1.18514270861327,9.67911301725969));
#35069=CARTESIAN_POINT('Ctrl Pts',(-3.89402362564286,1.30000000000221,9.72807138564023));
#35070=CARTESIAN_POINT('Ctrl Pts',(-3.99198996060069,-1.30000000000008,
9.54496247330596));
#35071=CARTESIAN_POINT('Ctrl Pts',(-3.92239848053823,-1.18514270861184,
9.51258568427901));
#35072=CARTESIAN_POINT('Ctrl Pts',(-3.86045956466931,-1.06847604194514,
9.48722049547628));
#35073=CARTESIAN_POINT('Ctrl Pts',(-3.73504723235175,-0.794772684000852,
9.44482003423708));
#35074=CARTESIAN_POINT('Ctrl Pts',(-3.67258059959666,-0.636309800095198,
9.43806097931972));
#35075=CARTESIAN_POINT('Ctrl Pts',(-3.59326729399712,-0.31943490727716,
9.42779540032309));
#35076=CARTESIAN_POINT('Ctrl Pts',(-3.56992252153975,-0.158333333333333,
9.42792332139754));
#35077=CARTESIAN_POINT('Ctrl Pts',(-3.55915076488227,0.158333333333334,
9.4453691550592));
#35078=CARTESIAN_POINT('Ctrl Pts',(-3.57280337312768,0.319434907277167,
9.46085721877722));
#35079=CARTESIAN_POINT('Ctrl Pts',(-3.62797633392986,0.636309800095207,
9.51038597519395));
#35080=CARTESIAN_POINT('Ctrl Pts',(-3.67645485979168,0.794772684000843,
9.54018297807693));
#35081=CARTESIAN_POINT('Ctrl Pts',(-3.77705435099628,1.06847604194587,9.62285502829093));
#35082=CARTESIAN_POINT('Ctrl Pts',(-3.8278900846652,1.18514270861327,9.66616756632872));
#35083=CARTESIAN_POINT('Ctrl Pts',(-3.88601575983895,1.30000000000221,9.7170069751679));
#35084=CARTESIAN_POINT('Ctrl Pts',(-3.98223602054929,-1.30000000000008,
9.53389065551683));
#35085=CARTESIAN_POINT('Ctrl Pts',(-3.91009970729482,-1.18514270861184,
9.50037021018406));
#35086=CARTESIAN_POINT('Ctrl Pts',(-3.84640729865907,-1.06847604194515,
9.47403296621852));
#35087=CARTESIAN_POINT('Ctrl Pts',(-3.71877220195439,-0.794772684000855,
9.42978329606333));
#35088=CARTESIAN_POINT('Ctrl Pts',(-3.657624226043,-0.636309800095198,9.42216489294489));
#35089=CARTESIAN_POINT('Ctrl Pts',(-3.57877337913983,-0.31943490727716,
9.41120306132792));
#35090=CARTESIAN_POINT('Ctrl Pts',(-3.55642229010766,-0.158333333333333,
9.41156642016226));
#35091=CARTESIAN_POINT('Ctrl Pts',(-3.54533915517231,0.158333333333334,
9.42940478405905));
#35092=CARTESIAN_POINT('Ctrl Pts',(-3.55719468008065,0.319434907277166,
9.44570670973183));
#35093=CARTESIAN_POINT('Ctrl Pts',(-3.61227313969613,0.636309800095206,
9.49539348245401));
#35094=CARTESIAN_POINT('Ctrl Pts',(-3.66122310062954,0.794772684000842,
9.52357900580051));
#35095=CARTESIAN_POINT('Ctrl Pts',(-3.76434798221053,1.06847604194587,9.60775523228691));
#35096=CARTESIAN_POINT('Ctrl Pts',(-3.81675088661188,1.18514270861327,9.65234746810249));
#35097=CARTESIAN_POINT('Ctrl Pts',(-3.87691775533148,1.30000000000221,9.70509517032415));
#35098=CARTESIAN_POINT('Ctrl Pts',(-3.97422670435764,-1.30000000000008,
9.52527149172315));
#35099=CARTESIAN_POINT('Ctrl Pts',(-3.89993944215733,-1.18514270861184,
9.49074311189192));
#35100=CARTESIAN_POINT('Ctrl Pts',(-3.83481605433959,-1.06847604194514,
9.46345282333785));
#35101=CARTESIAN_POINT('Ctrl Pts',(-3.70553838364206,-0.794772684000852,
9.41712823619988));
#35102=CARTESIAN_POINT('Ctrl Pts',(-3.64587798071845,-0.636309800095197,
9.40803695520255));
#35103=CARTESIAN_POINT('Ctrl Pts',(-3.56772851893399,-0.319434907277159,
9.3959004776643));
#35104=CARTESIAN_POINT('Ctrl Pts',(-3.54619807190222,-0.158333333333333,
9.39649432519919));
#35105=CARTESIAN_POINT('Ctrl Pts',(-3.53514505713312,0.158333333333334,
9.41426901412984));
#35106=CARTESIAN_POINT('Ctrl Pts',(-3.54608006064357,0.319434907277166,
9.43043728191244));
#35107=CARTESIAN_POINT('Ctrl Pts',(-3.60078328750133,0.636309800095205,
9.48084206052464));
#35108=CARTESIAN_POINT('Ctrl Pts',(-3.64893849711766,0.794772684000841,
9.50956420724531));
#35109=CARTESIAN_POINT('Ctrl Pts',(-3.75380923964106,1.06847604194587,9.59573353455122));
#35110=CARTESIAN_POINT('Ctrl Pts',(-3.80754380960878,1.18514270861327,9.64145231986177));
#35111=CARTESIAN_POINT('Ctrl Pts',(-3.86961829094969,1.30000000000221,9.69559038158027));
#35112=CARTESIAN_POINT('Ctrl Pts',(-3.9658917442215,-1.30000000000008,9.51663189767499));
#35113=CARTESIAN_POINT('Ctrl Pts',(-3.88867313305062,-1.18514270861184,
9.4816967127887));
#35114=CARTESIAN_POINT('Ctrl Pts',(-3.82176442120232,-1.06847604194515,
9.45367222838924));
#35115=CARTESIAN_POINT('Ctrl Pts',(-3.69100984171424,-0.794772684000854,
9.40489516375309));
#35116=CARTESIAN_POINT('Ctrl Pts',(-3.63472860148631,-0.636309800095199,
9.39236816688827));
#35117=CARTESIAN_POINT('Ctrl Pts',(-3.55824395824535,-0.31943490727716,
9.37820427155903));
#35118=CARTESIAN_POINT('Ctrl Pts',(-3.53752962997678,-0.158333333333333,
9.3794112337313));
#35119=CARTESIAN_POINT('Ctrl Pts',(-3.52653899124765,0.158333333333334,
9.39711672986148));
#35120=CARTESIAN_POINT('Ctrl Pts',(-3.53661209047723,0.319434907277166,
9.41279812490356));
#35121=CARTESIAN_POINT('Ctrl Pts',(-3.58999787159868,0.636309800095206,
9.46469129414753));
#35122=CARTESIAN_POINT('Ctrl Pts',(-3.63546698501272,0.794772684000843,
9.49566253282961));
#35123=CARTESIAN_POINT('Ctrl Pts',(-3.74183138047937,1.06847604194587,9.58429741893322));
#35124=CARTESIAN_POINT('Ctrl Pts',(-3.79719329321463,1.18514270861327,9.63104264461239));
#35125=CARTESIAN_POINT('Ctrl Pts',(-3.86187591307676,1.30000000000221,9.68616633802254));
#35126=CARTESIAN_POINT('Ctrl Pts',(-3.9607311993876,-1.30000000000008,9.50955037962429));
#35127=CARTESIAN_POINT('Ctrl Pts',(-3.88225168772289,-1.18514270861184,
9.47466234423755));
#35128=CARTESIAN_POINT('Ctrl Pts',(-3.81472938981739,-1.06847604194514,
9.44635463975158));
#35129=CARTESIAN_POINT('Ctrl Pts',(-3.68405272963316,-0.794772684000851,
9.39616006022359));
#35130=CARTESIAN_POINT('Ctrl Pts',(-3.63042937353999,-0.636309800095197,
9.38108392494785));
#35131=CARTESIAN_POINT('Ctrl Pts',(-3.55544568811449,-0.319434907277159,
9.36542695146836));
#35132=CARTESIAN_POINT('Ctrl Pts',(-3.53503780515506,-0.158333333333333,
9.36693889716871));
#35133=CARTESIAN_POINT('Ctrl Pts',(-3.52419820399014,0.158333333333334,
9.38451178833638));
#35134=CARTESIAN_POINT('Ctrl Pts',(-3.53420574803466,0.319434907277167,
9.39971616479935));
#35135=CARTESIAN_POINT('Ctrl Pts',(-3.58621520078905,0.636309800095206,
9.45291262168402));
#35136=CARTESIAN_POINT('Ctrl Pts',(-3.62884548279216,0.79477268400084,9.48638184647067));
#35137=CARTESIAN_POINT('Ctrl Pts',(-3.73516370162499,1.06847604194587,9.57640799112453));
#35138=CARTESIAN_POINT('Ctrl Pts',(-3.79118274870548,1.18514270861327,9.62344798197328));
#35139=CARTESIAN_POINT('Ctrl Pts',(-3.85719962541184,1.30000000000221,9.67855898144743));
#35140=CARTESIAN_POINT('Ctrl Pts',(-3.95827679071521,-1.30000000000008,
9.50436744488838));
#35141=CARTESIAN_POINT('Ctrl Pts',(-3.87988594951763,-1.18514270861184,
9.46962156082299));
#35142=CARTESIAN_POINT('Ctrl Pts',(-3.8125890784605,-1.06847604194514,9.44126870438154));
#35143=CARTESIAN_POINT('Ctrl Pts',(-3.68274913399113,-0.794772684000851,
9.39053710676437));
#35144=CARTESIAN_POINT('Ctrl Pts',(-3.630353335205,-0.636309800095197,9.3742697918532));
#35145=CARTESIAN_POINT('Ctrl Pts',(-3.55620605750903,-0.319434907277159,
9.35786137336722));
#35146=CARTESIAN_POINT('Ctrl Pts',(-3.53576509129249,-0.158333333333333,
9.35936221324764));
#35147=CARTESIAN_POINT('Ctrl Pts',(-3.52505210827391,0.158333333333334,
9.37684078872384));
#35148=CARTESIAN_POINT('Ctrl Pts',(-3.53535684314381,0.319434907277167,
9.39183563380664));
#35149=CARTESIAN_POINT('Ctrl Pts',(-3.58650774416314,0.636309800095206,
9.44584872924291));
#35150=CARTESIAN_POINT('Ctrl Pts',(-3.62740723167583,0.79477268400084,9.48102758076392));
#35151=CARTESIAN_POINT('Ctrl Pts',(-3.73295432340194,1.06847604194587,9.57151210020652));
#35152=CARTESIAN_POINT('Ctrl Pts',(-3.78889068790107,1.18514270861327,9.61843876361845));
#35153=CARTESIAN_POINT('Ctrl Pts',(-3.85507599179614,1.30000000000221,9.67312469475735));
#35154=CARTESIAN_POINT('Ctrl Pts',(-3.95827679071515,-1.3,9.50436744488836));
#35155=CARTESIAN_POINT('Ctrl Pts',(-3.8798859495176,-1.18514270861178,9.46962156082298));
#35156=CARTESIAN_POINT('Ctrl Pts',(-3.81258907846048,-1.06847604194512,
9.44126870438153));
#35157=CARTESIAN_POINT('Ctrl Pts',(-3.68274913399113,-0.794772684000851,
9.39053710676437));
#35158=CARTESIAN_POINT('Ctrl Pts',(-3.630353335205,-0.636309800095197,9.3742697918532));
#35159=CARTESIAN_POINT('Ctrl Pts',(-3.55620605750903,-0.319434907277159,
9.35786137336722));
#35160=CARTESIAN_POINT('Ctrl Pts',(-3.53576509129249,-0.158333333333332,
9.35936221324765));
#35161=CARTESIAN_POINT('Ctrl Pts',(-3.52505210827392,0.158333333333334,
9.37684078872385));
#35162=CARTESIAN_POINT('Ctrl Pts',(-3.53535684314381,0.319434907277167,
9.39183563380664));
#35163=CARTESIAN_POINT('Ctrl Pts',(-3.58650774416314,0.636309800095206,
9.44584872924292));
#35164=CARTESIAN_POINT('Ctrl Pts',(-3.62740723167583,0.79477268400084,9.48102758076392));
#35165=CARTESIAN_POINT('Ctrl Pts',(-3.73295432340165,1.06847604194511,9.57151210020627));
#35166=CARTESIAN_POINT('Ctrl Pts',(-3.78889068790036,1.18514270861178,9.61843876361785));
#35167=CARTESIAN_POINT('Ctrl Pts',(-3.85507599179487,1.3,9.6731246947563));
#35168=CARTESIAN_POINT('',(-4.17593056680875,-1.2,9.85783820071734));
#35169=CARTESIAN_POINT('Ctrl Pts',(-4.17593056680875,-1.2,9.85783820071734));
#35170=CARTESIAN_POINT('Ctrl Pts',(-4.16900460433805,-1.21680656858669,
9.83741928428235));
#35171=CARTESIAN_POINT('Ctrl Pts',(-4.16296024818596,-1.23316317392224,
9.8163387999078));
#35172=CARTESIAN_POINT('Ctrl Pts',(-4.1488048506352,-1.2666702566154,9.77575381663696));
#35173=CARTESIAN_POINT('Ctrl Pts',(-4.14194603049473,-1.28324039240427,
9.75534893186735));
#35174=CARTESIAN_POINT('Ctrl Pts',(-4.13459357261703,-1.30000000000009,
9.73527828635697));
#35175=CARTESIAN_POINT('',(-4.08975874013753,-0.653834841453647,9.98861496935521));
#35176=CARTESIAN_POINT('Ctrl Pts',(-4.0897587401673,-0.653834841446134,
9.98861496933965));
#35177=CARTESIAN_POINT('Ctrl Pts',(-4.09775715954222,-0.709816513138484,
9.97688455624721));
#35178=CARTESIAN_POINT('Ctrl Pts',(-4.10667273452126,-0.767198090793461,
9.96369085870135));
#35179=CARTESIAN_POINT('Ctrl Pts',(-4.13494013389672,-0.949641514625852,
9.92139732810018));
#35180=CARTESIAN_POINT('Ctrl Pts',(-4.15505714074664,-1.07515677647218,
9.89063401872584));
#35181=CARTESIAN_POINT('Ctrl Pts',(-4.17593056680875,-1.2,9.85783820071734));
#35182=CARTESIAN_POINT('',(-4.00955034077224,0.653834841531101,10.1027583545334));
#35183=CARTESIAN_POINT('Ctrl Pts',(-4.00955034077224,0.653834841531109,
10.1027583545334));
#35184=CARTESIAN_POINT('Ctrl Pts',(-3.9892075661712,0.575721283879273,10.0663434637934));
#35185=CARTESIAN_POINT('Ctrl Pts',(-3.97294247893386,0.49370810326247,10.0352117278294));
#35186=CARTESIAN_POINT('Ctrl Pts',(-3.95139645767513,0.338002156994941,
9.98935818625072));
#35187=CARTESIAN_POINT('Ctrl Pts',(-3.94495289412142,0.265532347033553,
9.97263620467793));
#35188=CARTESIAN_POINT('Ctrl Pts',(-3.94026888251158,0.129607443941674,
9.94872120414658));
#35189=CARTESIAN_POINT('Ctrl Pts',(-3.94093793002591,0.0665876566835187,
9.94052695975531));
#35190=CARTESIAN_POINT('Ctrl Pts',(-3.94825596348623,-0.0594622425677186,
9.92946225854297));
#35191=CARTESIAN_POINT('Ctrl Pts',(-3.95493666965847,-0.12262589836043,
9.92651382436694));
#35192=CARTESIAN_POINT('Ctrl Pts',(-3.97559481777179,-0.259989755378361,
9.92666831668788));
#35193=CARTESIAN_POINT('Ctrl Pts',(-3.99070125145753,-0.333867720853484,
9.93096966087476));
#35194=CARTESIAN_POINT('Ctrl Pts',(-4.03134687200918,-0.491609040819702,
9.95017991763267));
#35195=CARTESIAN_POINT('Ctrl Pts',(-4.05860469882518,-0.575043211348306,
9.9665674288075));
#35196=CARTESIAN_POINT('Ctrl Pts',(-4.08975874015232,-0.653834841462508,
9.98861496930265));
#35197=CARTESIAN_POINT('',(-4.05146929769195,1.2,10.0439578987495));
#35198=CARTESIAN_POINT('Ctrl Pts',(-4.05146929769195,1.2,10.0439578987495));
#35199=CARTESIAN_POINT('Ctrl Pts',(-4.04424830449576,1.13358862703007,10.0542448415506));
#35200=CARTESIAN_POINT('Ctrl Pts',(-4.03476005464607,1.03679350577961,10.0676732148766));
#35201=CARTESIAN_POINT('Ctrl Pts',(-4.01423194498588,0.76628625112874,10.0963297482212));
#35202=CARTESIAN_POINT('Ctrl Pts',(-4.01217510060249,0.713687193651155,
10.0991328007027));
#35203=CARTESIAN_POINT('Ctrl Pts',(-4.00955034077224,0.6538348415311,10.1027583545334));
#35204=CARTESIAN_POINT('Ctrl Pts',(-4.01176133534861,1.30000000000221,9.92548545917613));
#35205=CARTESIAN_POINT('Ctrl Pts',(-4.01208413859466,1.29919712732527,9.92643902247361));
#35206=CARTESIAN_POINT('Ctrl Pts',(-4.01241001091402,1.29839310268918,9.92738991408859));
#35207=CARTESIAN_POINT('Ctrl Pts',(-4.01932105646512,1.28166623088641,9.9469745517571));
#35208=CARTESIAN_POINT('Ctrl Pts',(-4.02569239595674,1.26580539078481,9.96573574783945));
#35209=CARTESIAN_POINT('Ctrl Pts',(-4.03644635502667,1.2393255832925,9.99676311150203));
#35210=CARTESIAN_POINT('Ctrl Pts',(-4.04452227242327,1.21971041315455,10.0195479433281));
#35211=CARTESIAN_POINT('Ctrl Pts',(-4.05146929769195,1.2,10.0439578987495));
#35212=CARTESIAN_POINT('Ctrl Pts',(-3.95827679071515,-1.3,9.50436744488836));
#35213=CARTESIAN_POINT('Ctrl Pts',(-3.8798859495176,-1.18514270861178,9.46962156082298));
#35214=CARTESIAN_POINT('Ctrl Pts',(-3.81258907846048,-1.06847604194512,
9.44126870438153));
#35215=CARTESIAN_POINT('Ctrl Pts',(-3.68274913399113,-0.794772684000851,
9.39053710676437));
#35216=CARTESIAN_POINT('Ctrl Pts',(-3.630353335205,-0.636309800095197,9.3742697918532));
#35217=CARTESIAN_POINT('Ctrl Pts',(-3.55620605750903,-0.319434907277159,
9.35786137336722));
#35218=CARTESIAN_POINT('Ctrl Pts',(-3.53576509129249,-0.158333333333332,
9.35936221324765));
#35219=CARTESIAN_POINT('Ctrl Pts',(-3.52505210827391,0.158333333333334,
9.37684078872384));
#35220=CARTESIAN_POINT('Ctrl Pts',(-3.53535684314381,0.319434907277167,
9.39183563380664));
#35221=CARTESIAN_POINT('Ctrl Pts',(-3.58650774416314,0.636309800095206,
9.44584872924291));
#35222=CARTESIAN_POINT('Ctrl Pts',(-3.62740723167583,0.79477268400084,9.48102758076392));
#35223=CARTESIAN_POINT('Ctrl Pts',(-3.73295432340165,1.06847604194511,9.57151210020627));
#35224=CARTESIAN_POINT('Ctrl Pts',(-3.78889068790036,1.18514270861178,9.61843876361785));
#35225=CARTESIAN_POINT('Ctrl Pts',(-3.85507599179487,1.3,9.6731246947563));
#35226=CARTESIAN_POINT('Ctrl Pts',(-3.99529346323778,-1.3,9.43692209493747));
#35227=CARTESIAN_POINT('Ctrl Pts',(-3.91621554992515,-1.18514270861178,
9.40376644257368));
#35228=CARTESIAN_POINT('Ctrl Pts',(-3.84848168092754,-1.06847604194512,
9.37653821129757));
#35229=CARTESIAN_POINT('Ctrl Pts',(-3.7182099051649,-0.794772684000851,
9.32732907854981));
#35230=CARTESIAN_POINT('Ctrl Pts',(-3.66630753169098,-0.636309800095197,
9.31054067879995));
#35231=CARTESIAN_POINT('Ctrl Pts',(-3.59275862546216,-0.319434907277159,
9.29383792247894));
#35232=CARTESIAN_POINT('Ctrl Pts',(-3.57308521991698,-0.158333333333332,
9.29436290252082));
#35233=CARTESIAN_POINT('Ctrl Pts',(-3.56268309827957,0.158333333333334,
9.31202095389912));
#35234=CARTESIAN_POINT('Ctrl Pts',(-3.57252649407444,0.319434907277167,
9.32816845594153));
#35235=CARTESIAN_POINT('Ctrl Pts',(-3.62372167678492,0.636309800095206,
9.38284692518677));
#35236=CARTESIAN_POINT('Ctrl Pts',(-3.66441660424588,0.79477268400084,9.41871363798237));
#35237=CARTESIAN_POINT('Ctrl Pts',(-3.77106627357833,1.06847604194511,9.50806294811988));
#35238=CARTESIAN_POINT('Ctrl Pts',(-3.8277580930697,1.18514270861178,9.55404884763091));
#35239=CARTESIAN_POINT('Ctrl Pts',(-3.89497704195816,1.3,9.60734464101269));
#35240=CARTESIAN_POINT('Ctrl Pts',(-4.0323101357604,-1.3,9.36947674498658));
#35241=CARTESIAN_POINT('Ctrl Pts',(-3.95254515033271,-1.18514270861178,
9.33791132432438));
#35242=CARTESIAN_POINT('Ctrl Pts',(-3.88437428339459,-1.06847604194512,
9.3118077182136));
#35243=CARTESIAN_POINT('Ctrl Pts',(-3.75367067633867,-0.794772684000851,
9.26412105033525));
#35244=CARTESIAN_POINT('Ctrl Pts',(-3.70226172817696,-0.636309800095197,
9.24681156574669));
#35245=CARTESIAN_POINT('Ctrl Pts',(-3.62931119341529,-0.319434907277159,
9.22981447159065));
#35246=CARTESIAN_POINT('Ctrl Pts',(-3.61040534854147,-0.158333333333332,
9.229363591794));
#35247=CARTESIAN_POINT('Ctrl Pts',(-3.60031408828524,0.158333333333334,
9.24720111907439));
#35248=CARTESIAN_POINT('Ctrl Pts',(-3.60969614500508,0.319434907277167,
9.26450127807642));
#35249=CARTESIAN_POINT('Ctrl Pts',(-3.6609356094067,0.636309800095206,9.31984512113063));
#35250=CARTESIAN_POINT('Ctrl Pts',(-3.70142597681592,0.79477268400084,9.35639969520082));
#35251=CARTESIAN_POINT('Ctrl Pts',(-3.80917822375501,1.06847604194511,9.4446137960335));
#35252=CARTESIAN_POINT('Ctrl Pts',(-3.86662549823905,1.18514270861178,9.48965893164399));
#35253=CARTESIAN_POINT('Ctrl Pts',(-3.93487809212145,1.3,9.54156458726908));
#35254=CARTESIAN_POINT('Ctrl Pts',(-4.06932680828303,-1.3,9.30203139503569));
#35255=CARTESIAN_POINT('Ctrl Pts',(-3.98887475074027,-1.18514270861178,
9.27205620607508));
#35256=CARTESIAN_POINT('Ctrl Pts',(-3.92026688586165,-1.06847604194512,
9.24707722512964));
#35257=CARTESIAN_POINT('Ctrl Pts',(-3.78913144751244,-0.794772684000851,
9.20091302212069));
#35258=CARTESIAN_POINT('Ctrl Pts',(-3.73821592466294,-0.636309800095197,
9.18308245269344));
#35259=CARTESIAN_POINT('Ctrl Pts',(-3.66586376136842,-0.319434907277159,
9.16579102070237));
#35260=CARTESIAN_POINT('Ctrl Pts',(-3.64772547716596,-0.158333333333332,
9.16436428106718));
#35261=CARTESIAN_POINT('Ctrl Pts',(-3.6379450782909,0.158333333333334,9.18238128424967));
#35262=CARTESIAN_POINT('Ctrl Pts',(-3.64686579593571,0.319434907277167,
9.20083410021131));
#35263=CARTESIAN_POINT('Ctrl Pts',(-3.69814954202848,0.636309800095206,
9.25684331707449));
#35264=CARTESIAN_POINT('Ctrl Pts',(-3.73843534938597,0.79477268400084,9.29408575241927));
#35265=CARTESIAN_POINT('Ctrl Pts',(-3.84729017393168,1.06847604194511,9.38116464394711));
#35266=CARTESIAN_POINT('Ctrl Pts',(-3.90549290340839,1.18514270861178,9.42526901565705));
#35267=CARTESIAN_POINT('Ctrl Pts',(-3.97477914228474,1.3,9.47578453352548));
#35268=CARTESIAN_POINT('Ctrl Pts',(-4.06932680828303,-1.3,9.30203139503569));
#35269=CARTESIAN_POINT('Ctrl Pts',(-3.98887475074027,-1.18514270861178,
9.27205620607508));
#35270=CARTESIAN_POINT('Ctrl Pts',(-3.92026688586165,-1.06847604194512,
9.24707722512964));
#35271=CARTESIAN_POINT('Ctrl Pts',(-3.78913144751244,-0.794772684000851,
9.20091302212069));
#35272=CARTESIAN_POINT('Ctrl Pts',(-3.73821592466294,-0.636309800095197,
9.18308245269344));
#35273=CARTESIAN_POINT('Ctrl Pts',(-3.66586376136842,-0.319434907277159,
9.16579102070237));
#35274=CARTESIAN_POINT('Ctrl Pts',(-3.64772547716596,-0.158333333333332,
9.16436428106718));
#35275=CARTESIAN_POINT('Ctrl Pts',(-3.6379450782909,0.158333333333334,9.18238128424967));
#35276=CARTESIAN_POINT('Ctrl Pts',(-3.64686579593571,0.319434907277167,
9.20083410021132));
#35277=CARTESIAN_POINT('Ctrl Pts',(-3.69814954202848,0.636309800095206,
9.25684331707449));
#35278=CARTESIAN_POINT('Ctrl Pts',(-3.73843534938597,0.79477268400084,9.29408575241927));
#35279=CARTESIAN_POINT('Ctrl Pts',(-3.84729017393169,1.06847604194511,9.38116464394711));
#35280=CARTESIAN_POINT('Ctrl Pts',(-3.90549290340839,1.18514270861178,9.42526901565705));
#35281=CARTESIAN_POINT('Ctrl Pts',(-3.97477914228474,1.3,9.47578453352548));
#35282=CARTESIAN_POINT('Ctrl Pts',(-4.0693268082841,-1.30000000000154,9.30203139503609));
#35283=CARTESIAN_POINT('Ctrl Pts',(-3.98887475074088,-1.18514270861282,
9.2720562060753));
#35284=CARTESIAN_POINT('Ctrl Pts',(-3.9202668858619,-1.06847604194564,9.24707722512973));
#35285=CARTESIAN_POINT('Ctrl Pts',(-3.78913144751244,-0.794772684000851,
9.20091302212069));
#35286=CARTESIAN_POINT('Ctrl Pts',(-3.73821592466294,-0.636309800095197,
9.18308245269344));
#35287=CARTESIAN_POINT('Ctrl Pts',(-3.66586376136842,-0.319434907277159,
9.16579102070237));
#35288=CARTESIAN_POINT('Ctrl Pts',(-3.64772547716596,-0.158333333333332,
9.16436428106718));
#35289=CARTESIAN_POINT('Ctrl Pts',(-3.6379450782909,0.158333333333334,9.18238128424967));
#35290=CARTESIAN_POINT('Ctrl Pts',(-3.64686579593571,0.319434907277167,
9.20083410021132));
#35291=CARTESIAN_POINT('Ctrl Pts',(-3.69814954202848,0.636309800095206,
9.25684331707449));
#35292=CARTESIAN_POINT('Ctrl Pts',(-3.73843534938597,0.79477268400084,9.29408575241927));
#35293=CARTESIAN_POINT('Ctrl Pts',(-3.84729017393255,1.06847604194727,9.3811646439478));
#35294=CARTESIAN_POINT('Ctrl Pts',(-3.90549290341051,1.18514270861603,9.42526901565866));
#35295=CARTESIAN_POINT('Ctrl Pts',(-3.97477914228853,1.30000000000629,9.47578453352824));
#35296=CARTESIAN_POINT('Ctrl Pts',(-4.07797887893123,-1.30000000000154,
9.30071436097919));
#35297=CARTESIAN_POINT('Ctrl Pts',(-3.9971009618214,-1.18514270861282,9.27127676660931));
#35298=CARTESIAN_POINT('Ctrl Pts',(-3.92828386835242,-1.06847604194564,
9.24627537341984));
#35299=CARTESIAN_POINT('Ctrl Pts',(-3.79716553099689,-0.794772684000851,
9.19876566582649));
#35300=CARTESIAN_POINT('Ctrl Pts',(-3.74717278256212,-0.636309800095197,
9.1774045083569));
#35301=CARTESIAN_POINT('Ctrl Pts',(-3.67523755004237,-0.319434907277159,
9.15838530602086));
#35302=CARTESIAN_POINT('Ctrl Pts',(-3.65704996965851,-0.158333333333332,
9.15750177709801));
#35303=CARTESIAN_POINT('Ctrl Pts',(-3.64724201471915,0.158333333333334,
9.17575399884814));
#35304=CARTESIAN_POINT('Ctrl Pts',(-3.65612349309497,0.319434907277167,
9.1941721677954));
#35305=CARTESIAN_POINT('Ctrl Pts',(-3.70705838931291,0.636309800095206,
9.2518314939406));
#35306=CARTESIAN_POINT('Ctrl Pts',(-3.7467174769052,0.79477268400084,9.29156195772604));
#35307=CARTESIAN_POINT('Ctrl Pts',(-3.85550223127429,1.06847604194727,9.38013053841707));
#35308=CARTESIAN_POINT('Ctrl Pts',(-3.91381537677535,1.18514270861603,9.42456161215902));
#35309=CARTESIAN_POINT('Ctrl Pts',(-3.98335277848303,1.30000000000629,9.47508570285074));
#35310=CARTESIAN_POINT('Ctrl Pts',(-4.09011797873321,-1.30000000000154,
9.30252364569461));
#35311=CARTESIAN_POINT('Ctrl Pts',(-4.01108973039803,-1.18514270861282,
9.27532957844728));
#35312=CARTESIAN_POINT('Ctrl Pts',(-3.94378582323447,-1.06847604194564,
9.25134724675337));
#35313=CARTESIAN_POINT('Ctrl Pts',(-3.81538590713933,-0.794772684000851,
9.2033630145254));
#35314=CARTESIAN_POINT('Ctrl Pts',(-3.76638481191805,-0.636309800095196,
9.17657067845296));
#35315=CARTESIAN_POINT('Ctrl Pts',(-3.69515467615052,-0.319434907277158,
9.15477598516934));
#35316=CARTESIAN_POINT('Ctrl Pts',(-3.67598551438858,-0.158333333333332,
9.15376112563587));
#35317=CARTESIAN_POINT('Ctrl Pts',(-3.6661483823356,0.158333333333334,9.17217245872481));
#35318=CARTESIAN_POINT('Ctrl Pts',(-3.67610124044008,0.319434907277168,
9.19077019887138));
#35319=CARTESIAN_POINT('Ctrl Pts',(-3.72602926377211,0.636309800095206,
9.25175495003996));
#35320=CARTESIAN_POINT('Ctrl Pts',(-3.76398909419763,0.794772684000839,
9.29785643624438));
#35321=CARTESIAN_POINT('Ctrl Pts',(-3.87008466638102,1.06847604194727,9.38686020609118));
#35322=CARTESIAN_POINT('Ctrl Pts',(-3.9270709548608,1.18514270861603,9.43000966829725));
#35323=CARTESIAN_POINT('Ctrl Pts',(-3.99511868985009,1.30000000000629,9.47778215865702));
#35324=CARTESIAN_POINT('Ctrl Pts',(-4.10795972278025,-1.30000000000153,
9.30505955869257));
#35325=CARTESIAN_POINT('Ctrl Pts',(-4.03226889918297,-1.18514270861282,
9.27940612168916));
#35326=CARTESIAN_POINT('Ctrl Pts',(-3.96750844541615,-1.06847604194564,
9.25636778477935));
#35327=CARTESIAN_POINT('Ctrl Pts',(-3.84315018285207,-0.794772684000848,
9.20918602207947));
#35328=CARTESIAN_POINT('Ctrl Pts',(-3.79429460663926,-0.636309800095195,
9.18080176601074));
#35329=CARTESIAN_POINT('Ctrl Pts',(-3.72375195285354,-0.319434907277158,
9.15788647602099));
#35330=CARTESIAN_POINT('Ctrl Pts',(-3.70367005810356,-0.158333333333332,
9.15573000955476));
#35331=CARTESIAN_POINT('Ctrl Pts',(-3.69377607554661,0.158333333333334,
9.17421636327135));
#35332=CARTESIAN_POINT('Ctrl Pts',(-3.70470750896684,0.319434907277167,
9.1937162806825));
#35333=CARTESIAN_POINT('Ctrl Pts',(-3.75358233346997,0.636309800095204,
9.25661495278545));
#35334=CARTESIAN_POINT('Ctrl Pts',(-3.79063880992344,0.794772684000837,
9.30603464088148));
#35335=CARTESIAN_POINT('Ctrl Pts',(-3.89267460720987,1.06847604194727,9.39440474368925));
#35336=CARTESIAN_POINT('Ctrl Pts',(-3.94728891409695,1.18514270861603,9.43630682995842));
#35337=CARTESIAN_POINT('Ctrl Pts',(-4.01235001202426,1.30000000000629,9.48185885942593));
#35338=CARTESIAN_POINT('Ctrl Pts',(-4.12284323460048,-1.30000000000154,
9.30685293138367));
#35339=CARTESIAN_POINT('Ctrl Pts',(-4.049785457782,-1.18514270861282,9.28199742225637));
#35340=CARTESIAN_POINT('Ctrl Pts',(-3.98688228258699,-1.06847604194564,
9.25967626151977));
#35341=CARTESIAN_POINT('Ctrl Pts',(-3.86502252532105,-0.794772684000848,
9.21396476666262));
#35342=CARTESIAN_POINT('Ctrl Pts',(-3.81496983539429,-0.636309800095194,
9.18689354017524));
#35343=CARTESIAN_POINT('Ctrl Pts',(-3.74449789211767,-0.319434907277157,
9.1638580222074));
#35344=CARTESIAN_POINT('Ctrl Pts',(-3.72423974057687,-0.158333333333331,
9.15973969708325));
#35345=CARTESIAN_POINT('Ctrl Pts',(-3.71456204305582,0.158333333333333,
9.17769261665386));
#35346=CARTESIAN_POINT('Ctrl Pts',(-3.72624291205814,0.319434907277165,
9.19779147741451));
#35347=CARTESIAN_POINT('Ctrl Pts',(-3.77476061621474,0.636309800095203,
9.261413403952));
#35348=CARTESIAN_POINT('Ctrl Pts',(-3.81167277195878,0.794772684000836,
9.31252192677137));
#35349=CARTESIAN_POINT('Ctrl Pts',(-3.91103129697726,1.06847604194727,9.39992907820287));
#35350=CARTESIAN_POINT('Ctrl Pts',(-3.96396036050981,1.18514270861603,9.44080281486098));
#35351=CARTESIAN_POINT('Ctrl Pts',(-4.02680986369017,1.30000000000629,9.48471497107627));
#35352=CARTESIAN_POINT('Ctrl Pts',(-4.13791931153452,-1.30000000000153,
9.30848411321606));
#35353=CARTESIAN_POINT('Ctrl Pts',(-4.06777250467259,-1.18514270861282,
9.2844327204044));
#35354=CARTESIAN_POINT('Ctrl Pts',(-4.00693160854003,-1.06847604194564,
9.26286747711773));
#35355=CARTESIAN_POINT('Ctrl Pts',(-3.88787548272047,-0.794772684000849,
9.2187909537687));
#35356=CARTESIAN_POINT('Ctrl Pts',(-3.83667833394984,-0.636309800095196,
9.19308213945078));
#35357=CARTESIAN_POINT('Ctrl Pts',(-3.76611582358144,-0.319434907277159,
9.17052568769673));
#35358=CARTESIAN_POINT('Ctrl Pts',(-3.74545998680562,-0.158333333333332,
9.16480797938058));
#35359=CARTESIAN_POINT('Ctrl Pts',(-3.73539946788037,0.158333333333334,
9.18354871474106));
#35360=CARTESIAN_POINT('Ctrl Pts',(-3.74685571876856,0.319434907277166,
9.20650796240082));
#35361=CARTESIAN_POINT('Ctrl Pts',(-3.79517201785929,0.636309800095204,
9.27029169704709));
#35362=CARTESIAN_POINT('Ctrl Pts',(-3.83355595154219,0.794772684000839,
9.31942042979027));
#35363=CARTESIAN_POINT('Ctrl Pts',(-3.93037163322943,1.06847604194727,9.4047403873389));
#35364=CARTESIAN_POINT('Ctrl Pts',(-3.98137404529088,1.18514270861603,9.44461938474921));
#35365=CARTESIAN_POINT('Ctrl Pts',(-4.04147094818551,1.30000000000629,9.48744553136265));
#35366=CARTESIAN_POINT('Ctrl Pts',(-4.1533794268455,-1.30000000000153,9.30876317496566));
#35367=CARTESIAN_POINT('Ctrl Pts',(-4.085970772055,-1.18514270861282,9.28554892971681));
#35368=CARTESIAN_POINT('Ctrl Pts',(-4.02703523000209,-1.06847604194564,
9.26483245483457));
#35369=CARTESIAN_POINT('Ctrl Pts',(-3.91045692330953,-0.794772684000848,
9.2227436027642));
#35370=CARTESIAN_POINT('Ctrl Pts',(-3.85806507197327,-0.636309800095194,
9.19857085576219));
#35371=CARTESIAN_POINT('Ctrl Pts',(-3.78694551084616,-0.319434907277157,
9.17754337018662));
#35372=CARTESIAN_POINT('Ctrl Pts',(-3.76516544649804,-0.158333333333331,
9.17201447101112));
#35373=CARTESIAN_POINT('Ctrl Pts',(-3.75481287203959,0.158333333333333,
9.19132159300446));
#35374=CARTESIAN_POINT('Ctrl Pts',(-3.76698441355051,0.319434907277164,
9.21481508671862));
#35375=CARTESIAN_POINT('Ctrl Pts',(-3.81550094633685,0.636309800095202,
9.27790442139565));
#35376=CARTESIAN_POINT('Ctrl Pts',(-3.85511179032036,0.794772684000835,
9.32565992050354));
#35377=CARTESIAN_POINT('Ctrl Pts',(-3.94941707868567,1.06847604194727,9.40931224094343));
#35378=CARTESIAN_POINT('Ctrl Pts',(-3.99852187921034,1.18514270861603,9.44843737352206));
#35379=CARTESIAN_POINT('Ctrl Pts',(-4.05591021528127,1.30000000000628,9.49047764878448));
#35380=CARTESIAN_POINT('Ctrl Pts',(-4.17747110574483,-1.30000000000153,
9.31118743640778));
#35381=CARTESIAN_POINT('Ctrl Pts',(-4.11456988829079,-1.18514270861282,
9.28924299342072));
#35382=CARTESIAN_POINT('Ctrl Pts',(-4.05883609878957,-1.06847604194564,
9.26968351006847));
#35383=CARTESIAN_POINT('Ctrl Pts',(-3.94663808794569,-0.79477268400085,
9.23000692452956));
#35384=CARTESIAN_POINT('Ctrl Pts',(-3.89279883435421,-0.636309800095195,
9.20710163656167));
#35385=CARTESIAN_POINT('Ctrl Pts',(-3.82107374744563,-0.319434907277158,
9.18781803868467));
#35386=CARTESIAN_POINT('Ctrl Pts',(-3.79728925346981,-0.158333333333332,
9.18294505239384));
#35387=CARTESIAN_POINT('Ctrl Pts',(-3.78668110903818,0.158333333333334,
9.20276514259551));
#35388=CARTESIAN_POINT('Ctrl Pts',(-3.8004863198785,0.319434907277165,9.22632762165036));
#35389=CARTESIAN_POINT('Ctrl Pts',(-3.84932243521093,0.636309800095203,
9.2882862617491));
#35390=CARTESIAN_POINT('Ctrl Pts',(-3.89033444775097,0.794772684000838,
9.33490442857791));
#35391=CARTESIAN_POINT('Ctrl Pts',(-3.98048279233754,1.06847604194727,9.41581046998228));
#35392=CARTESIAN_POINT('Ctrl Pts',(-4.02656895818941,1.18514270861603,9.45347458012295));
#35393=CARTESIAN_POINT('Ctrl Pts',(-4.0797194118466,1.30000000000628,9.49378157294425));
#35394=CARTESIAN_POINT('Ctrl Pts',(-4.20504288008068,-1.30000000000152,
9.31232210003516));
#35395=CARTESIAN_POINT('Ctrl Pts',(-4.14739578132247,-1.18514270861281,
9.29097859693842));
#35396=CARTESIAN_POINT('Ctrl Pts',(-4.0953629535084,-1.06847604194563,9.27223503249788));
#35397=CARTESIAN_POINT('Ctrl Pts',(-3.98812680113864,-0.794772684000841,
9.23494002741484));
#35398=CARTESIAN_POINT('Ctrl Pts',(-3.93228588504089,-0.636309800095189,
9.21468589554296));
#35399=CARTESIAN_POINT('Ctrl Pts',(-3.8598363508624,-0.319434907277155,
9.19767572904004));
#35400=CARTESIAN_POINT('Ctrl Pts',(-3.83416215730614,-0.15833333333333,
9.19290392150196));
#35401=CARTESIAN_POINT('Ctrl Pts',(-3.8230277047217,0.158333333333332,9.21384776584676));
#35402=CARTESIAN_POINT('Ctrl Pts',(-3.83795207230725,0.319434907277163,
9.23884390516112));
#35403=CARTESIAN_POINT('Ctrl Pts',(-3.88693807156031,0.636309800095198,
9.29998076988301));
#35404=CARTESIAN_POINT('Ctrl Pts',(-3.93003483749848,0.794772684000829,
9.3442254552323));
#35405=CARTESIAN_POINT('Ctrl Pts',(-4.01543246685247,1.06847604194726,9.42252823998472));
#35406=CARTESIAN_POINT('Ctrl Pts',(-4.05799623300798,1.18514270861602,9.45903423613183));
#35407=CARTESIAN_POINT('Ctrl Pts',(-4.10615829586529,1.30000000000628,9.4981518543105));
#35408=CARTESIAN_POINT('Ctrl Pts',(-4.23281323594865,-1.30000000000152,
9.31292054619255));
#35409=CARTESIAN_POINT('Ctrl Pts',(-4.18042031073655,-1.18514270861281,
9.29233208269215));
#35410=CARTESIAN_POINT('Ctrl Pts',(-4.13212992153116,-1.06847604194563,
9.27442120575142));
#35411=CARTESIAN_POINT('Ctrl Pts',(-4.03004714089272,-0.794772684000843,
9.23922925756194));
#35412=CARTESIAN_POINT('Ctrl Pts',(-3.97267347876869,-0.636309800095191,
9.22048356055537));
#35413=CARTESIAN_POINT('Ctrl Pts',(-3.89942412464079,-0.319434907277156,
9.20598169033391));
#35414=CARTESIAN_POINT('Ctrl Pts',(-3.87105812842082,-0.15833333333333,
9.20320269393037));
#35415=CARTESIAN_POINT('Ctrl Pts',(-3.85963656380305,0.158333333333332,
9.22481241000328));
#35416=CARTESIAN_POINT('Ctrl Pts',(-3.87685740408209,0.31943490727716,9.24867162974645));
#35417=CARTESIAN_POINT('Ctrl Pts',(-3.92627882889088,0.636309800095195,
9.30826947423017));
#35418=CARTESIAN_POINT('Ctrl Pts',(-3.97083543862442,0.794772684000832,
9.35138080852935));
#35419=CARTESIAN_POINT('Ctrl Pts',(-4.05116957893062,1.06847604194726,9.42757846509117));
#35420=CARTESIAN_POINT('Ctrl Pts',(-4.09009978676833,1.18514270861602,9.46308177444326));
#35421=CARTESIAN_POINT('Ctrl Pts',(-4.13318652977812,1.30000000000628,9.50110525102292));
#35422=CARTESIAN_POINT('Ctrl Pts',(-4.25116029379157,-1.30000000000152,
9.31376081103458));
#35423=CARTESIAN_POINT('Ctrl Pts',(-4.20211149992213,-1.18514270861281,
9.29412518622882));
#35424=CARTESIAN_POINT('Ctrl Pts',(-4.15624213215879,-1.06847604194563,
9.27697416319944));
#35425=CARTESIAN_POINT('Ctrl Pts',(-4.05761982683721,-0.794772684000842,
9.2430917960976));
#35426=CARTESIAN_POINT('Ctrl Pts',(-3.99949188056049,-0.636309800095188,
9.22449431303707));
#35427=CARTESIAN_POINT('Ctrl Pts',(-3.92609620592482,-0.319434907277154,
9.21066694055706));
#35428=CARTESIAN_POINT('Ctrl Pts',(-3.89643329069856,-0.15833333333333,
9.20810256072842));
#35429=CARTESIAN_POINT('Ctrl Pts',(-3.8847936228239,0.158333333333332,9.23022775344872));
#35430=CARTESIAN_POINT('Ctrl Pts',(-3.90300145842652,0.319434907277162,
9.25459038551016));
#35431=CARTESIAN_POINT('Ctrl Pts',(-3.95231197470889,0.636309800095196,
9.31415113672722));
#35432=CARTESIAN_POINT('Ctrl Pts',(-3.99765893703627,0.794772684000827,
9.35701865505897));
#35433=CARTESIAN_POINT('Ctrl Pts',(-4.07452946440137,1.06847604194726,9.43206753415053));
#35434=CARTESIAN_POINT('Ctrl Pts',(-4.11105502488755,1.18514270861602,9.46687156953381));
#35435=CARTESIAN_POINT('Ctrl Pts',(-4.15083174289697,1.30000000000627,9.50399376137633));
#35436=CARTESIAN_POINT('Ctrl Pts',(-4.26670499109829,-1.30000000000152,
9.31367542306743));
#35437=CARTESIAN_POINT('Ctrl Pts',(-4.22079506822243,-1.18514270861281,
9.29376305362827));
#35438=CARTESIAN_POINT('Ctrl Pts',(-4.17714866477651,-1.06847604194563,
9.2766291896994));
#35439=CARTESIAN_POINT('Ctrl Pts',(-4.08154592408225,-0.794772684000842,
9.24346543997298));
#35440=CARTESIAN_POINT('Ctrl Pts',(-4.02234410608837,-0.636309800095189,
9.22644454060134));
#35441=CARTESIAN_POINT('Ctrl Pts',(-3.94852035825935,-0.319434907277154,
9.21409456825448));
#35442=CARTESIAN_POINT('Ctrl Pts',(-3.91754048734327,-0.15833333333333,
9.21227699640609));
#35443=CARTESIAN_POINT('Ctrl Pts',(-3.90569550186702,0.158333333333332,
9.23491704998506));
#35444=CARTESIAN_POINT('Ctrl Pts',(-3.92493844300946,0.319434907277162,
9.25917897805349));
#35445=CARTESIAN_POINT('Ctrl Pts',(-3.97441470660465,0.636309800095196,
9.31804373083212));
#35446=CARTESIAN_POINT('Ctrl Pts',(-4.02072096957854,0.794772684000828,
9.35989732509025));
#35447=CARTESIAN_POINT('Ctrl Pts',(-4.09473830712847,1.06847604194726,9.43389179977599));
#35448=CARTESIAN_POINT('Ctrl Pts',(-4.1291977435757,1.18514270861602,9.46827286972838));
#35449=CARTESIAN_POINT('Ctrl Pts',(-4.16607725365714,1.30000000000627,9.50500554330687));
#35450=CARTESIAN_POINT('Ctrl Pts',(-4.27753228080596,-1.30000000000152,
9.31376050379798));
#35451=CARTESIAN_POINT('Ctrl Pts',(-4.23367329127038,-1.18514270861281,
9.29409865065746));
#35452=CARTESIAN_POINT('Ctrl Pts',(-4.19149340446467,-1.06847604194563,
9.27724608128728));
#35453=CARTESIAN_POINT('Ctrl Pts',(-4.09792849109564,-0.79477268400084,
9.24480328220206));
#35454=CARTESIAN_POINT('Ctrl Pts',(-4.03810846364677,-0.636309800095188,
9.22844010672574));
#35455=CARTESIAN_POINT('Ctrl Pts',(-3.96412755056454,-0.319434907277154,
9.21671586212742));
#35456=CARTESIAN_POINT('Ctrl Pts',(-3.93237379326356,-0.15833333333333,
9.21504405513902));
#35457=CARTESIAN_POINT('Ctrl Pts',(-3.92047047892969,0.158333333333332,
9.23782238423847));
#35458=CARTESIAN_POINT('Ctrl Pts',(-3.94045398425137,0.319434907277162,
9.261982637299));
#35459=CARTESIAN_POINT('Ctrl Pts',(-3.98991766466715,0.636309800095196,
9.32069516903308));
#35460=CARTESIAN_POINT('Ctrl Pts',(-4.03657008444672,0.794772684000827,
9.36267658603357));
#35461=CARTESIAN_POINT('Ctrl Pts',(-4.10858232727238,1.06847604194726,9.43595073645765));
#35462=CARTESIAN_POINT('Ctrl Pts',(-4.14166623194688,1.18514270861602,9.46985157773273));
#35463=CARTESIAN_POINT('Ctrl Pts',(-4.17666260969292,1.30000000000627,9.50593559563883));
#35464=CARTESIAN_POINT('Ctrl Pts',(-4.28376574468374,-1.30000000000152,
9.31366392579355));
#35465=CARTESIAN_POINT('Ctrl Pts',(-4.24103726129138,-1.18514270861281,
9.29427710274561));
#35466=CARTESIAN_POINT('Ctrl Pts',(-4.19967103402951,-1.06847604194563,
9.2776636701469));
#35467=CARTESIAN_POINT('Ctrl Pts',(-4.10725385794923,-0.794772684000841,
9.24569040409073));
#35468=CARTESIAN_POINT('Ctrl Pts',(-4.04713008303279,-0.636309800095188,
9.22954767265744));
#35469=CARTESIAN_POINT('Ctrl Pts',(-3.97309785341113,-0.319434907277154,
9.21807347310103));
#35470=CARTESIAN_POINT('Ctrl Pts',(-3.94095387220251,-0.15833333333333,
9.21635381743337));
#35471=CARTESIAN_POINT('Ctrl Pts',(-3.92898727114034,0.158333333333332,
9.23928703884165));
#35472=CARTESIAN_POINT('Ctrl Pts',(-3.94929239596999,0.319434907277162,
9.26364869411582));
#35473=CARTESIAN_POINT('Ctrl Pts',(-3.99868931413014,0.636309800095197,
9.32242941227565));
#35474=CARTESIAN_POINT('Ctrl Pts',(-4.04556297752378,0.794772684000828,
9.36443027327445));
#35475=CARTESIAN_POINT('Ctrl Pts',(-4.11639122616648,1.06847604194726,9.43739081622));
#35476=CARTESIAN_POINT('Ctrl Pts',(-4.14866548399181,1.18514270861602,9.47107631964459));
#35477=CARTESIAN_POINT('Ctrl Pts',(-4.18255507525001,1.30000000000627,9.50686541090687));
#35478=CARTESIAN_POINT('Ctrl Pts',(-4.299395134043,-1.30000000000152,9.31326205030675));
#35479=CARTESIAN_POINT('Ctrl Pts',(-4.2595340555938,-1.18514270861281,9.29442455647643));
#35480=CARTESIAN_POINT('Ctrl Pts',(-4.22023142337693,-1.06847604194563,
9.27831309146941));
#35481=CARTESIAN_POINT('Ctrl Pts',(-4.13072460300502,-0.79477268400084,
9.24739005613777));
#35482=CARTESIAN_POINT('Ctrl Pts',(-4.06984446995732,-0.636309800095188,
9.23181809073007));
#35483=CARTESIAN_POINT('Ctrl Pts',(-3.99565112279439,-0.319434907277155,
9.22108363448806));
#35484=CARTESIAN_POINT('Ctrl Pts',(-3.96244514185411,-0.15833333333333,
9.21949927156026));
#35485=CARTESIAN_POINT('Ctrl Pts',(-3.95031771039047,0.158333333333332,
9.24284591715237));
#35486=CARTESIAN_POINT('Ctrl Pts',(-3.97146423549848,0.319434907277161,
9.26761349642659));
#35487=CARTESIAN_POINT('Ctrl Pts',(-4.02081641650737,0.636309800095196,
9.32623628233159));
#35488=CARTESIAN_POINT('Ctrl Pts',(-4.06845915214776,0.794772684000829,
9.36769014467127));
#35489=CARTESIAN_POINT('Ctrl Pts',(-4.13632501846853,1.06847604194726,9.43987618616326));
#35490=CARTESIAN_POINT('Ctrl Pts',(-4.16651958174986,1.18514270861602,9.4731776780092));
#35491=CARTESIAN_POINT('Ctrl Pts',(-4.19753208946014,1.30000000000627,9.50853399909531));
#35492=CARTESIAN_POINT('Ctrl Pts',(-4.32558216921391,-1.30000000000151,
9.31372186269296));
#35493=CARTESIAN_POINT('Ctrl Pts',(-4.29094222329233,-1.1851427086128,9.29469301243295));
#35494=CARTESIAN_POINT('Ctrl Pts',(-4.25537610244751,-1.06847604194562,
9.27869877259595));
#35495=CARTESIAN_POINT('Ctrl Pts',(-4.17107159896477,-0.794772684000835,
9.24875943608465));
#35496=CARTESIAN_POINT('Ctrl Pts',(-4.10867533471152,-0.636309800095184,
9.23498747374347));
#35497=CARTESIAN_POINT('Ctrl Pts',(-4.03403287930407,-0.319434907277152,
9.22603066394919));
#35498=CARTESIAN_POINT('Ctrl Pts',(-3.99866953595907,-0.158333333333329,
9.22558567956006));
#35499=CARTESIAN_POINT('Ctrl Pts',(-3.98645646098271,0.158333333333331,
9.24912504001713));
#35500=CARTESIAN_POINT('Ctrl Pts',(-4.00974347283856,0.319434907277159,
9.27266673277605));
#35501=CARTESIAN_POINT('Ctrl Pts',(-4.05923023725212,0.636309800095192,
9.33047317536098));
#35502=CARTESIAN_POINT('Ctrl Pts',(-4.10778847468005,0.794772684000823,
9.37207515896062));
#35503=CARTESIAN_POINT('Ctrl Pts',(-4.17055531628905,1.06847604194725,9.44315633901884));
#35504=CARTESIAN_POINT('Ctrl Pts',(-4.197228550674,1.18514270861601,9.47578816178047));
#35505=CARTESIAN_POINT('Ctrl Pts',(-4.22340557945179,1.30000000000627,9.51028339827349));
#35506=CARTESIAN_POINT('Ctrl Pts',(-4.36339961556755,-1.30000000000151,
9.31149883582506));
#35507=CARTESIAN_POINT('Ctrl Pts',(-4.33590918874599,-1.1851427086128,9.29282781111208));
#35508=CARTESIAN_POINT('Ctrl Pts',(-4.30549194641469,-1.06847604194562,
9.27736191017708));
#35509=CARTESIAN_POINT('Ctrl Pts',(-4.22846050234616,-0.794772684000833,
9.24903706218436));
#35510=CARTESIAN_POINT('Ctrl Pts',(-4.16424523170537,-0.636309800095181,
9.23686177834877));
#35511=CARTESIAN_POINT('Ctrl Pts',(-4.08914233458117,-0.31943490727715,
9.23009077363859));
#35512=CARTESIAN_POINT('Ctrl Pts',(-4.05100021784028,-0.158333333333329,
9.23078853853655));
#35513=CARTESIAN_POINT('Ctrl Pts',(-4.03827950130655,0.158333333333331,
9.25580113040377));
#35514=CARTESIAN_POINT('Ctrl Pts',(-4.06358260654506,0.319434907277162,
9.28033001254928));
#35515=CARTESIAN_POINT('Ctrl Pts',(-4.11301527834565,0.636309800095193,
9.33761385094508));
#35516=CARTESIAN_POINT('Ctrl Pts',(-4.16368772934163,0.794772684000819,
9.37707595318374));
#35517=CARTESIAN_POINT('Ctrl Pts',(-4.21918785472595,1.06847604194724,9.44675113514984));
#35518=CARTESIAN_POINT('Ctrl Pts',(-4.24070989192469,1.185142708616,9.47893185897244));
#35519=CARTESIAN_POINT('Ctrl Pts',(-4.25973001852536,1.30000000000626,9.51313350206414));
#35520=CARTESIAN_POINT('Ctrl Pts',(-4.39287315342704,-1.3000000000015,9.31107034343129));
#35521=CARTESIAN_POINT('Ctrl Pts',(-4.37126556181242,-1.18514270861279,
9.29187809878067));
#35522=CARTESIAN_POINT('Ctrl Pts',(-4.3450951857209,-1.06847604194561,9.27623236383228));
#35523=CARTESIAN_POINT('Ctrl Pts',(-4.27409543666033,-0.794772684000828,
9.24828073307203));
#35524=CARTESIAN_POINT('Ctrl Pts',(-4.20846511303003,-0.63630980009518,
9.23742862906884));
#35525=CARTESIAN_POINT('Ctrl Pts',(-4.13303144622131,-0.319434907277151,
9.23234354937861));
#35526=CARTESIAN_POINT('Ctrl Pts',(-4.09244763322764,-0.158333333333328,
9.23467408865915));
#35527=CARTESIAN_POINT('Ctrl Pts',(-4.07960349336706,0.15833333333333,9.26006972675397));
#35528=CARTESIAN_POINT('Ctrl Pts',(-4.1072895064877,0.319434907277159,9.2830901745054));
#35529=CARTESIAN_POINT('Ctrl Pts',(-4.15666988679089,0.636309800095189,
9.33999529144816));
#35530=CARTESIAN_POINT('Ctrl Pts',(-4.20807314245923,0.794772684000818,
9.38045854599755));
#35531=CARTESIAN_POINT('Ctrl Pts',(-4.25769277471803,1.06847604194724,9.44948027541786));
#35532=CARTESIAN_POINT('Ctrl Pts',(-4.27523743063318,1.18514270861601,9.48107725233575));
#35533=CARTESIAN_POINT('Ctrl Pts',(-4.288848242247,1.30000000000626,9.5143942570123));
#35534=CARTESIAN_POINT('Ctrl Pts',(-4.41828955691599,-1.3000000000015,9.30871299493204));
#35535=CARTESIAN_POINT('Ctrl Pts',(-4.40139988976438,-1.18514270861279,
9.28984824185018));
#35536=CARTESIAN_POINT('Ctrl Pts',(-4.37865455922241,-1.06847604194561,
9.27453897962996));
#35537=CARTESIAN_POINT('Ctrl Pts',(-4.31258054162962,-0.794772684000826,
9.24738541645785));
#35538=CARTESIAN_POINT('Ctrl Pts',(-4.24595507448116,-0.636309800095179,
9.23694606010339));
#35539=CARTESIAN_POINT('Ctrl Pts',(-4.17037233349577,-0.319434907277151,
9.23291925778407));
#35540=CARTESIAN_POINT('Ctrl Pts',(-4.12801255166076,-0.158333333333328,
9.23590162478777));
#35541=CARTESIAN_POINT('Ctrl Pts',(-4.11480007208656,0.15833333333333,9.26246631800015));
#35542=CARTESIAN_POINT('Ctrl Pts',(-4.14363369407532,0.31943490727716,9.28676807309881));
#35543=CARTESIAN_POINT('Ctrl Pts',(-4.1929425096266,0.63630980009519,9.34343981792205));
#35544=CARTESIAN_POINT('Ctrl Pts',(-4.24591465250796,0.794772684000817,
9.38190123681928));
#35545=CARTESIAN_POINT('Ctrl Pts',(-4.29067970726545,1.06847604194724,9.45006192760711));
#35546=CARTESIAN_POINT('Ctrl Pts',(-4.30475619025655,1.185142708616,9.48150833098788));
#35547=CARTESIAN_POINT('Ctrl Pts',(-4.3135320227428,1.30000000000626,9.51489690030957));
#35548=CARTESIAN_POINT('Ctrl Pts',(-4.43698594830172,-1.3000000000015,9.30804571980993));
#35549=CARTESIAN_POINT('Ctrl Pts',(-4.42390105088262,-1.18514270861279,
9.2884897363668));
#35550=CARTESIAN_POINT('Ctrl Pts',(-4.40388453279908,-1.06847604194561,
9.27287439871892));
#35551=CARTESIAN_POINT('Ctrl Pts',(-4.34162894133467,-0.794772684000827,
9.24590352502531));
#35552=CARTESIAN_POINT('Ctrl Pts',(-4.27383343181233,-0.636309800095178,
9.23728199950697));
#35553=CARTESIAN_POINT('Ctrl Pts',(-4.19817239325749,-0.31943490727715,
9.23398769339868));
#35554=CARTESIAN_POINT('Ctrl Pts',(-4.15467691343505,-0.158333333333328,
9.23677055247689));
#35555=CARTESIAN_POINT('Ctrl Pts',(-4.14158202539205,0.15833333333333,9.26298585791562));
#35556=CARTESIAN_POINT('Ctrl Pts',(-4.17188912877299,0.319434907277159,
9.28640029692033));
#35557=CARTESIAN_POINT('Ctrl Pts',(-4.22106725238384,0.636309800095188,
9.34312997232989));
#35558=CARTESIAN_POINT('Ctrl Pts',(-4.27433933090947,0.794772684000817,
9.38273777429863));
#35559=CARTESIAN_POINT('Ctrl Pts',(-4.31519262141616,1.06847604194724,9.45110238518818));
#35560=CARTESIAN_POINT('Ctrl Pts',(-4.32666894689436,1.185142708616,9.48245364140811));
#35561=CARTESIAN_POINT('Ctrl Pts',(-4.33193772215384,1.30000000000625,9.51556364695209));
#35562=CARTESIAN_POINT('Ctrl Pts',(-4.45742539215227,-1.30000000000149,
9.30672991413338));
#35563=CARTESIAN_POINT('Ctrl Pts',(-4.44819512374719,-1.18514270861278,
9.2873438766223));
#35564=CARTESIAN_POINT('Ctrl Pts',(-4.4310073952158,-1.06847604194561,9.27182726939889));
#35565=CARTESIAN_POINT('Ctrl Pts',(-4.37291697913885,-0.794772684000826,
9.24491996066763));
#35566=CARTESIAN_POINT('Ctrl Pts',(-4.30460489739991,-0.636309800095177,
9.23562325498352));
#35567=CARTESIAN_POINT('Ctrl Pts',(-4.22886151246214,-0.319434907277149,
9.2330764560671));
#35568=CARTESIAN_POINT('Ctrl Pts',(-4.18367015350271,-0.158333333333327,
9.23729721921038));
#35569=CARTESIAN_POINT('Ctrl Pts',(-4.1702162969332,0.158333333333329,9.26470909809492));
#35570=CARTESIAN_POINT('Ctrl Pts',(-4.20159383392492,0.319434907277157,
9.28873078254841));
#35571=CARTESIAN_POINT('Ctrl Pts',(-4.2506659053382,0.636309800095186,9.34542179636802));
#35572=CARTESIAN_POINT('Ctrl Pts',(-4.30501761360352,0.794772684000815,
9.38397247896077));
#35573=CARTESIAN_POINT('Ctrl Pts',(-4.34189032661779,1.06847604194724,9.45177413756467));
#35574=CARTESIAN_POINT('Ctrl Pts',(-4.35056771527077,1.185142708616,9.4829668134292));
#35575=CARTESIAN_POINT('Ctrl Pts',(-4.35196166138135,1.30000000000625,9.51600333944736));
#35576=CARTESIAN_POINT('Ctrl Pts',(-4.47330007032464,-1.30000000000149,
9.30509533005243));
#35577=CARTESIAN_POINT('Ctrl Pts',(-4.46718357161219,-1.18514270861278,
9.28525798096092));
#35578=CARTESIAN_POINT('Ctrl Pts',(-4.45223897087315,-1.06847604194561,
9.26954732156572));
#35579=CARTESIAN_POINT('Ctrl Pts',(-4.39731927177176,-0.794772684000823,
9.24278603419616));
#35580=CARTESIAN_POINT('Ctrl Pts',(-4.32819150206691,-0.636309800095176,
9.23452078395232));
#35581=CARTESIAN_POINT('Ctrl Pts',(-4.25230757573395,-0.319434907277149,
9.23287568972763));
#35582=CARTESIAN_POINT('Ctrl Pts',(-4.20594738799116,-0.158333333333327,
9.23772258646171));
#35583=CARTESIAN_POINT('Ctrl Pts',(-4.19246143001637,0.158333333333329,
9.26528793158875));
#35584=CARTESIAN_POINT('Ctrl Pts',(-4.22500406516011,0.319434907277157,
9.28871710104222));
#35585=CARTESIAN_POINT('Ctrl Pts',(-4.27409350049364,0.636309800095185,
9.34506313089331));
#35586=CARTESIAN_POINT('Ctrl Pts',(-4.32908181488484,0.794772684000814,
9.38337935851737));
#35587=CARTESIAN_POINT('Ctrl Pts',(-4.36271708420564,1.06847604194724,9.45131076833307));
#35588=CARTESIAN_POINT('Ctrl Pts',(-4.36915471491328,1.18514270861599,9.48266781477494));
#35589=CARTESIAN_POINT('Ctrl Pts',(-4.36747051454899,1.30000000000625,9.51597691745595));
#35590=CARTESIAN_POINT('Ctrl Pts',(-4.48591544608392,-1.30000000000149,
9.30407848436835));
#35591=CARTESIAN_POINT('Ctrl Pts',(-4.48223751921892,-1.18514270861278,
9.28408043200416));
#35592=CARTESIAN_POINT('Ctrl Pts',(-4.46906707167276,-1.0684760419456,9.26829286640692));
#35593=CARTESIAN_POINT('Ctrl Pts',(-4.4167110813565,-0.794772684000821,
9.24154749832233));
#35594=CARTESIAN_POINT('Ctrl Pts',(-4.34711954603316,-0.636309800095173,
9.23339966233023));
#35595=CARTESIAN_POINT('Ctrl Pts',(-4.27113748432086,-0.319434907277147,
9.2324071115974));
#35596=CARTESIAN_POINT('Ctrl Pts',(-4.22371578345613,-0.158333333333326,
9.23821726492005));
#35597=CARTESIAN_POINT('Ctrl Pts',(-4.2101324175127,0.158333333333328,9.2661381208997));
#35598=CARTESIAN_POINT('Ctrl Pts',(-4.24356994227013,0.319434907277155,
9.28917716981086));
#35599=CARTESIAN_POINT('Ctrl Pts',(-4.29270008703502,0.636309800095182,
9.34515151932937));
#35600=CARTESIAN_POINT('Ctrl Pts',(-4.34831010011928,0.794772684000811,
9.3829296317695));
#35601=CARTESIAN_POINT('Ctrl Pts',(-4.3793937664007,1.06847604194723,9.45085335887142));
#35602=CARTESIAN_POINT('Ctrl Pts',(-4.38404015954559,1.18514270861599,9.48234661916512));
#35603=CARTESIAN_POINT('Ctrl Pts',(-4.37987797846535,1.30000000000624,9.51593147511192));
#35604=CARTESIAN_POINT('Ctrl Pts',(-4.49545712166529,-1.30000000000149,
9.30298909365531));
#35605=CARTESIAN_POINT('Ctrl Pts',(-4.49366288936686,-1.18514270861278,
9.28263576101769));
#35606=CARTESIAN_POINT('Ctrl Pts',(-4.4818464760129,-1.0684760419456,9.26668653526624));
#35607=CARTESIAN_POINT('Ctrl Pts',(-4.43139495413128,-0.794772684000821,
9.2400150010944));
#35608=CARTESIAN_POINT('Ctrl Pts',(-4.36126958694013,-0.636309800095173,
9.23269240322661));
#35609=CARTESIAN_POINT('Ctrl Pts',(-4.28522139944164,-0.319434907277147,
9.23220200621834));
#35610=CARTESIAN_POINT('Ctrl Pts',(-4.23719754852272,-0.158333333333326,
9.2380521444923));
#35611=CARTESIAN_POINT('Ctrl Pts',(-4.22354730410942,0.158333333333328,
9.26621721072458));
#35612=CARTESIAN_POINT('Ctrl Pts',(-4.25753318963454,0.319434907277155,
9.28938803048818));
#35613=CARTESIAN_POINT('Ctrl Pts',(-4.30656657183381,0.636309800095182,
9.34550524947842));
#35614=CARTESIAN_POINT('Ctrl Pts',(-4.36249756287696,0.794772684000811,
9.38334073259891));
#35615=CARTESIAN_POINT('Ctrl Pts',(-4.39168520889225,1.06847604194723,9.45120441704213));
#35616=CARTESIAN_POINT('Ctrl Pts',(-4.39504051886166,1.18514270861599,9.48263319967326));
#35617=CARTESIAN_POINT('Ctrl Pts',(-4.38911688834923,1.30000000000624,9.5161150905371));
#35618=CARTESIAN_POINT('Ctrl Pts',(-4.50341177882622,-1.30000000000148,
9.30205197134735));
#35619=CARTESIAN_POINT('Ctrl Pts',(-4.50320647280269,-1.18514270861278,
9.28132700338567));
#35620=CARTESIAN_POINT('Ctrl Pts',(-4.49253050120596,-1.0684760419456,9.26519534066278));
#35621=CARTESIAN_POINT('Ctrl Pts',(-4.44367753897328,-0.79477268400082,
9.23853942663408));
#35622=CARTESIAN_POINT('Ctrl Pts',(-4.37308289742706,-0.636309800095173,
9.23199434726505));
#35623=CARTESIAN_POINT('Ctrl Pts',(-4.29698135930824,-0.319434907277147,
9.23192540247938));
#35624=CARTESIAN_POINT('Ctrl Pts',(-4.24847292057746,-0.158333333333326,
9.23776209480255));
#35625=CARTESIAN_POINT('Ctrl Pts',(-4.23477258182423,0.158333333333328,
9.26611709674983));
#35626=CARTESIAN_POINT('Ctrl Pts',(-4.26921336639415,0.319434907277154,
9.28940069847015));
#35627=CARTESIAN_POINT('Ctrl Pts',(-4.31815649596753,0.636309800095181,
9.34566789569745));
#35628=CARTESIAN_POINT('Ctrl Pts',(-4.37434146750644,0.794772684000811,
9.38359338165133));
#35629=CARTESIAN_POINT('Ctrl Pts',(-4.40193631222051,1.06847604194723,9.4514529290796));
#35630=CARTESIAN_POINT('Ctrl Pts',(-4.40421094214181,1.18514270861599,9.48284670770899));
#35631=CARTESIAN_POINT('Ctrl Pts',(-4.39681541619732,1.30000000000624,9.51626038132981));
#35632=CARTESIAN_POINT('Ctrl Pts',(-4.50895399487148,-1.30000000000149,
9.3014961675291));
#35633=CARTESIAN_POINT('Ctrl Pts',(-4.50983134943706,-1.18514270861278,
9.28062700615559));
#35634=CARTESIAN_POINT('Ctrl Pts',(-4.49994130733982,-1.0684760419456,9.26441615343415));
#35635=CARTESIAN_POINT('Ctrl Pts',(-4.45221849129775,-0.79477268400082,
9.23772746555552));
#35636=CARTESIAN_POINT('Ctrl Pts',(-4.38139149177153,-0.636309800095173,
9.23135207715777));
#35637=CARTESIAN_POINT('Ctrl Pts',(-4.3052627002583,-0.319434907277147,
9.23153436528605));
#35638=CARTESIAN_POINT('Ctrl Pts',(-4.25633847738863,-0.158333333333326,
9.23764772076595));
#35639=CARTESIAN_POINT('Ctrl Pts',(-4.24260456385794,0.158333333333328,
9.26613747379966));
#35640=CARTESIAN_POINT('Ctrl Pts',(-4.27741492625282,0.319434907277154,
9.28931800303927));
#35641=CARTESIAN_POINT('Ctrl Pts',(-4.32634264934668,0.636309800095181,
9.34552933216575));
#35642=CARTESIAN_POINT('Ctrl Pts',(-4.38276188423467,0.794772684000811,
9.38333626246547));
#35643=CARTESIAN_POINT('Ctrl Pts',(-4.40921848311906,1.06847604194723,9.45126823561079));
#35644=CARTESIAN_POINT('Ctrl Pts',(-4.41070574048119,1.18514270861599,9.48273786026433));
#35645=CARTESIAN_POINT('Ctrl Pts',(-4.40222817386188,1.30000000000624,9.51627187552419));
#35646=CARTESIAN_POINT('Ctrl Pts',(-4.51171978258121,-1.30000000000148,
9.30123799540998));
#35647=CARTESIAN_POINT('Ctrl Pts',(-4.51313332307936,-1.18514270861277,
9.28031671505525));
#35648=CARTESIAN_POINT('Ctrl Pts',(-4.50363425316894,-1.0684760419456,9.26407395976082));
#35649=CARTESIAN_POINT('Ctrl Pts',(-4.45647918828954,-0.794772684000819,
9.23735827450373));
#35650=CARTESIAN_POINT('Ctrl Pts',(-4.38555378140777,-0.636309800095172,
9.23099860708769));
#35651=CARTESIAN_POINT('Ctrl Pts',(-4.30941430465361,-0.319434907277147,
9.23129437494411));
#35652=CARTESIAN_POINT('Ctrl Pts',(-4.26026996600083,-0.158333333333326,
9.2375917282832));
#35653=CARTESIAN_POINT('Ctrl Pts',(-4.24651917741272,0.158333333333328,
9.2661504769457));
#35654=CARTESIAN_POINT('Ctrl Pts',(-4.2815207054548,0.319434907277154,9.28925693144228));
#35655=CARTESIAN_POINT('Ctrl Pts',(-4.33044933657815,0.636309800095181,
9.34541195362376));
#35656=CARTESIAN_POINT('Ctrl Pts',(-4.38699854464526,0.79477268400081,9.38311782851278));
#35657=CARTESIAN_POINT('Ctrl Pts',(-4.41288286047686,1.06847604194723,9.45109712145016));
#35658=CARTESIAN_POINT('Ctrl Pts',(-4.41397102284211,1.18514270861599,9.48262284024169));
#35659=CARTESIAN_POINT('Ctrl Pts',(-4.40494298635743,1.30000000000624,9.51624856079291));
#35660=CARTESIAN_POINT('Ctrl Pts',(-4.51329932039636,-1.30000000000148,
9.30109370574358));
#35661=CARTESIAN_POINT('Ctrl Pts',(-4.51501832187378,-1.18514270861278,
9.2801462216824));
#35662=CARTESIAN_POINT('Ctrl Pts',(-4.5057422995373,-1.0684760419456,9.26388665087337));
#35663=CARTESIAN_POINT('Ctrl Pts',(-4.45891212772117,-0.794772684000819,
9.23715380701488));
#35664=CARTESIAN_POINT('Ctrl Pts',(-4.38793393240501,-0.636309800095172,
9.2307900577638));
#35665=CARTESIAN_POINT('Ctrl Pts',(-4.31178834187582,-0.319434907277147,
9.23115058609829));
#35666=CARTESIAN_POINT('Ctrl Pts',(-4.26251467800089,-0.158333333333326,
9.23756615242111));
#35667=CARTESIAN_POINT('Ctrl Pts',(-4.24875440944061,0.158333333333328,
9.26616398536437));
#35668=CARTESIAN_POINT('Ctrl Pts',(-4.28386822297713,0.319434907277154,
9.28921720033903));
#35669=CARTESIAN_POINT('Ctrl Pts',(-4.33279905653247,0.636309800095181,
9.3453343395105));
#35670=CARTESIAN_POINT('Ctrl Pts',(-4.3894232030314,0.79477268400081,9.38298079613845));
#35671=CARTESIAN_POINT('Ctrl Pts',(-4.41497954531572,1.06847604194723,9.45099021661041));
#35672=CARTESIAN_POINT('Ctrl Pts',(-4.41583873375347,1.18514270861599,9.48255089471637));
#35673=CARTESIAN_POINT('Ctrl Pts',(-4.40649471700977,1.30000000000624,9.51623349280305));
#35674=CARTESIAN_POINT('Ctrl Pts',(-4.52671929080664,-1.30000000000149,
9.29988940418204));
#35675=CARTESIAN_POINT('Ctrl Pts',(-4.53102612742524,-1.18514270861278,
9.27874990296268));
#35676=CARTESIAN_POINT('Ctrl Pts',(-4.52364278147363,-1.0684760419456,9.26235785230968));
#35677=CARTESIAN_POINT('Ctrl Pts',(-4.47957911494204,-0.794772684000821,
9.23545649661536));
#35678=CARTESIAN_POINT('Ctrl Pts',(-4.4081738110316,-0.636309800095175,
9.22897113594562));
#35679=CARTESIAN_POINT('Ctrl Pts',(-4.33199896083579,-0.319434907277148,
9.22979738586081));
#35680=CARTESIAN_POINT('Ctrl Pts',(-4.28164817918848,-0.158333333333327,
9.23714176846705));
#35681=CARTESIAN_POINT('Ctrl Pts',(-4.26780528345959,0.158333333333329,
9.26608248702132));
#35682=CARTESIAN_POINT('Ctrl Pts',(-4.30383410908715,0.319434907277155,
9.28882617419779));
#35683=CARTESIAN_POINT('Ctrl Pts',(-4.35278778872378,0.636309800095183,
9.34461301233644));
#35684=CARTESIAN_POINT('Ctrl Pts',(-4.4100974176126,0.794772684000813,9.38158476192281));
#35685=CARTESIAN_POINT('Ctrl Pts',(-4.43287220873722,1.06847604194723,9.44983783067013));
#35686=CARTESIAN_POINT('Ctrl Pts',(-4.4317793571628,1.18514270861599,9.48172130387332));
#35687=CARTESIAN_POINT('Ctrl Pts',(-4.41973529082518,1.30000000000624,9.51594402584412));
#35688=CARTESIAN_POINT('Ctrl Pts',(-4.55256722381233,-1.30000000000151,
9.29671431789035));
#35689=CARTESIAN_POINT('Ctrl Pts',(-4.56202663520296,-1.1851427086128,9.27432544232462));
#35690=CARTESIAN_POINT('Ctrl Pts',(-4.55836291693832,-1.06847604194562,
9.25723560809462));
#35691=CARTESIAN_POINT('Ctrl Pts',(-4.51958194004603,-0.794772684000833,
9.2299965177689));
#35692=CARTESIAN_POINT('Ctrl Pts',(-4.44686126006357,-0.636309800095181,
9.22530520419382));
#35693=CARTESIAN_POINT('Ctrl Pts',(-4.37054477627713,-0.319434907277149,
9.22743480805897));
#35694=CARTESIAN_POINT('Ctrl Pts',(-4.31842629925649,-0.158333333333328,
9.23551089484534));
#35695=CARTESIAN_POINT('Ctrl Pts',(-4.30444631564053,0.15833333333333,9.26503516002087));
#35696=CARTESIAN_POINT('Ctrl Pts',(-4.3421776205791,0.319434907277159,9.28733307489918));
#35697=CARTESIAN_POINT('Ctrl Pts',(-4.39084729791894,0.63630980009519,9.34361142133363));
#35698=CARTESIAN_POINT('Ctrl Pts',(-4.44872689766476,0.794772684000818,
9.38177011967397));
#35699=CARTESIAN_POINT('Ctrl Pts',(-4.46636044443875,1.06847604194724,9.45001957626592));
#35700=CARTESIAN_POINT('Ctrl Pts',(-4.46182716187524,1.185142708616,9.48162162355187));
#35701=CARTESIAN_POINT('Ctrl Pts',(-4.445127687737,1.30000000000626,9.51528305725643));
#35702=CARTESIAN_POINT('Ctrl Pts',(-4.57797014782426,-1.30000000000154,
9.29362607769095));
#35703=CARTESIAN_POINT('Ctrl Pts',(-4.59241718008654,-1.18514270861282,
9.27026660930158));
#35704=CARTESIAN_POINT('Ctrl Pts',(-4.59237508839258,-1.06847604194564,
9.25259577777905));
#35705=CARTESIAN_POINT('Ctrl Pts',(-4.55880507328098,-0.794772684000851,
9.22491451109467));
#35706=CARTESIAN_POINT('Ctrl Pts',(-4.48498896022062,-0.636309800095197,
9.22122561337946));
#35707=CARTESIAN_POINT('Ctrl Pts',(-4.40861628632671,-0.319434907277159,
9.22434212977147));
#35708=CARTESIAN_POINT('Ctrl Pts',(-4.35474635534818,-0.158333333333332,
9.23324621499998));
#35709=CARTESIAN_POINT('Ctrl Pts',(-4.34059295810106,0.158333333333334,
9.26352342953991));
#35710=CARTESIAN_POINT('Ctrl Pts',(-4.37977441558119,0.319434907277167,
9.28618064357722));
#35711=CARTESIAN_POINT('Ctrl Pts',(-4.42840755015825,0.636309800095206,
9.34212104504176));
#35712=CARTESIAN_POINT('Ctrl Pts',(-4.48773430817405,0.79477268400084,9.37842616946321));
#35713=CARTESIAN_POINT('Ctrl Pts',(-4.50009761851219,1.06847604194727,9.44731322539085));
#35714=CARTESIAN_POINT('Ctrl Pts',(-4.49184486495908,1.18514270861603,9.47972503089479));
#35715=CARTESIAN_POINT('Ctrl Pts',(-4.46998773891322,1.30000000000629,9.51472998790827));
#35716=CARTESIAN_POINT('Ctrl Pts',(-4.59077270268374,-1.30000000000154,
9.29167068805624));
#35717=CARTESIAN_POINT('Ctrl Pts',(-4.60766161389343,-1.18514270861282,
9.26800173905256));
#35718=CARTESIAN_POINT('Ctrl Pts',(-4.60940251578967,-1.06847604194564,
9.25012893617775));
#35719=CARTESIAN_POINT('Ctrl Pts',(-4.57842941557334,-0.794772684000851,
9.22222944316779));
#35720=CARTESIAN_POINT('Ctrl Pts',(-4.50418204215329,-0.636309800095197,
9.2185802642803));
#35721=CARTESIAN_POINT('Ctrl Pts',(-4.42777734501206,-0.319434907277159,
9.22222011637217));
#35722=CARTESIAN_POINT('Ctrl Pts',(-4.37292795574625,-0.158333333333332,
9.23198243022416));
#35723=CARTESIAN_POINT('Ctrl Pts',(-4.35867257917563,0.158333333333334,
9.26271831194325));
#35724=CARTESIAN_POINT('Ctrl Pts',(-4.39869447984769,0.319434907277167,
9.28512064988622));
#35725=CARTESIAN_POINT('Ctrl Pts',(-4.44722735233343,0.636309800095206,
9.34117727402952));
#35726=CARTESIAN_POINT('Ctrl Pts',(-4.50695309467615,0.79477268400084,9.37766731592182));
#35727=CARTESIAN_POINT('Ctrl Pts',(-4.51674956614754,1.06847604194727,9.44670173557987));
#35728=CARTESIAN_POINT('Ctrl Pts',(-4.50675280587843,1.18514270861603,9.47916239086454));
#35729=CARTESIAN_POINT('Ctrl Pts',(-4.48251875583523,1.30000000000629,9.51420125914098));
#35730=CARTESIAN_POINT('',(-4.38971485813411,1.2,9.48755403526923));
#35731=CARTESIAN_POINT('Ctrl Pts',(-4.38971485813412,1.2,9.48755403526923));
#35732=CARTESIAN_POINT('Ctrl Pts',(-4.36856465842126,1.21681404005281,9.49175671093172));
#35733=CARTESIAN_POINT('Ctrl Pts',(-4.34727912103697,1.23316506853804,9.49708784014508));
#35734=CARTESIAN_POINT('Ctrl Pts',(-4.31570563125357,1.25821670499925,9.50310064771019));
#35735=CARTESIAN_POINT('Ctrl Pts',(-4.30530467128022,1.26642476319251,9.50514734277103));
#35736=CARTESIAN_POINT('Ctrl Pts',(-4.28380750759288,1.28334467201644,9.50941095015061));
#35737=CARTESIAN_POINT('Ctrl Pts',(-4.27227103446103,1.29250131658665,9.51149917491571));
#35738=CARTESIAN_POINT('Ctrl Pts',(-4.26286793819922,1.30000000000626,9.51310547563494));
#35739=CARTESIAN_POINT('',(-4.45989076530874,0.653834841369816,9.34752749950966));
#35740=CARTESIAN_POINT('Ctrl Pts',(-4.45989076533968,0.653834841368558,
9.34752749953006));
#35741=CARTESIAN_POINT('Ctrl Pts',(-4.4528848487179,0.717482614179447,9.36207707938459));
#35742=CARTESIAN_POINT('Ctrl Pts',(-4.44710663293816,0.764240546950704,
9.37394135883623));
#35743=CARTESIAN_POINT('Ctrl Pts',(-4.42419760792246,0.949850583838299,
9.42040738323249));
#35744=CARTESIAN_POINT('Ctrl Pts',(-4.40997428413873,1.05891269470216,9.44867709423153));
#35745=CARTESIAN_POINT('Ctrl Pts',(-4.38971485813412,1.2,9.48755403526923));
#35746=CARTESIAN_POINT('',(-4.51863764645995,-0.653834841531101,9.22099327559368));
#35747=CARTESIAN_POINT('Ctrl Pts',(-4.51863764645995,-0.6538348415311,9.22099327559368));
#35748=CARTESIAN_POINT('Ctrl Pts',(-4.47706062852027,-0.57596586359716,
9.22158151376161));
#35749=CARTESIAN_POINT('Ctrl Pts',(-4.44193143807525,-0.49363919130031,
9.22283656802191));
#35750=CARTESIAN_POINT('Ctrl Pts',(-4.39150077182074,-0.338139586062805,
9.22708011483244));
#35751=CARTESIAN_POINT('Ctrl Pts',(-4.37382131335729,-0.265665248839193,
9.22980161915001));
#35752=CARTESIAN_POINT('Ctrl Pts',(-4.35075762524346,-0.129721413745824,
9.23768769470636));
#35753=CARTESIAN_POINT('Ctrl Pts',(-4.34396312512813,-0.0666272124195298,
9.24241374472171));
#35754=CARTESIAN_POINT('Ctrl Pts',(-4.33801561083273,0.059547323378811,
9.25434173739283));
#35755=CARTESIAN_POINT('Ctrl Pts',(-4.33880352141602,0.12278345398452,9.26162381306405));
#35756=CARTESIAN_POINT('Ctrl Pts',(-4.34923310016955,0.260138689594822,
9.27954883606279));
#35757=CARTESIAN_POINT('Ctrl Pts',(-4.36046457083349,0.333955905815987,
9.29056690922749));
#35758=CARTESIAN_POINT('Ctrl Pts',(-4.39723646550573,0.491216885915717,
9.31624550765387));
#35759=CARTESIAN_POINT('Ctrl Pts',(-4.42491449632406,0.574353373727776,
9.33143546434627));
#35760=CARTESIAN_POINT('Ctrl Pts',(-4.4598907652581,0.653834841386376,9.34752749953792));
#35761=CARTESIAN_POINT('',(-4.48863561636269,-1.2,9.28677988861316));
#35762=CARTESIAN_POINT('Ctrl Pts',(-4.48863561636269,-1.2,9.28677988861316));
#35763=CARTESIAN_POINT('Ctrl Pts',(-4.4944288750257,-1.12734343599548,9.27431866675094));
#35764=CARTESIAN_POINT('Ctrl Pts',(-4.50105363556384,-1.03203660304106,
9.25993526667585));
#35765=CARTESIAN_POINT('Ctrl Pts',(-4.51377570799241,-0.796458044101793,
9.23187056708943));
#35766=CARTESIAN_POINT('Ctrl Pts',(-4.51600510749749,-0.740055726332444,
9.22687923761306));
#35767=CARTESIAN_POINT('Ctrl Pts',(-4.51863764645995,-0.653834841531101,
9.22099327559368));
#35768=CARTESIAN_POINT('Ctrl Pts',(-4.36615556544122,-1.29999999999999,
9.31167837948083));
#35769=CARTESIAN_POINT('Ctrl Pts',(-4.37511427302833,-1.29262032296144,
9.31010442892759));
#35770=CARTESIAN_POINT('Ctrl Pts',(-4.38551309604794,-1.28397999449773,
9.30842771658611));
#35771=CARTESIAN_POINT('Ctrl Pts',(-4.40673157410085,-1.26674695084208,
9.30402510739829));
#35772=CARTESIAN_POINT('Ctrl Pts',(-4.41749867593977,-1.25800032086002,
9.30176293427779));
#35773=CARTESIAN_POINT('Ctrl Pts',(-4.44091918379889,-1.2387128136161,9.29738790117898));
#35774=CARTESIAN_POINT('Ctrl Pts',(-4.46310927593388,-1.22042691903373,
9.29323250571027));
#35775=CARTESIAN_POINT('Ctrl Pts',(-4.48863561636269,-1.2,9.28677988861316));
#35776=CARTESIAN_POINT('Origin',(0.,1.25,7.2));
#35777=CARTESIAN_POINT('Origin',(0.,1.2,7.2));
#35778=CARTESIAN_POINT('Origin',(0.,0.92691742076555,7.2));
#35779=CARTESIAN_POINT('Origin',(0.,0.653834841531101,7.2));
#35780=CARTESIAN_POINT('Origin',(0.,0.,7.2));
#35781=CARTESIAN_POINT('Origin',(0.,-0.653834841531101,7.2));
#35782=CARTESIAN_POINT('Origin',(0.,-0.926917420765551,7.2));
#35783=CARTESIAN_POINT('Origin',(0.,-1.2,7.2));
#35784=CARTESIAN_POINT('Origin',(0.,-1.25,7.2));
#35785=CARTESIAN_POINT('Ctrl Pts',(-4.71917718395474,-1.30000000000184,
8.98265772674134));
#35786=CARTESIAN_POINT('Ctrl Pts',(-4.70935397490598,-1.18514270861303,
9.02411271480684));
#35787=CARTESIAN_POINT('Ctrl Pts',(-4.69192014516097,-1.06847604194575,
9.05326217342547));
#35788=CARTESIAN_POINT('Ctrl Pts',(-4.63406245451663,-0.794772684000851,
9.0921750194286));
#35789=CARTESIAN_POINT('Ctrl Pts',(-4.56698074651016,-0.636309800095196,
9.07220674691498));
#35790=CARTESIAN_POINT('Ctrl Pts',(-4.49284772594841,-0.319434907277159,
9.07364899676464));
#35791=CARTESIAN_POINT('Ctrl Pts',(-4.44941966576432,-0.158333333333332,
9.05889701834648));
#35792=CARTESIAN_POINT('Ctrl Pts',(-4.43611716307696,0.158333333333335,
9.09005714685184));
#35793=CARTESIAN_POINT('Ctrl Pts',(-4.46556375515151,0.319434907277167,
9.13735044965271));
#35794=CARTESIAN_POINT('Ctrl Pts',(-4.51398353922898,0.636309800095206,
9.19656574141201));
#35795=CARTESIAN_POINT('Ctrl Pts',(-4.56637659762912,0.794772684000841,
9.24930051549101));
#35796=CARTESIAN_POINT('Ctrl Pts',(-4.60783501082195,1.06847604194523,9.25364960997122));
#35797=CARTESIAN_POINT('Ctrl Pts',(-4.61995220105506,1.18514270861202,9.24039662831112));
#35798=CARTESIAN_POINT('Ctrl Pts',(-4.6262407706357,1.30000000000035,9.21200810314026));
#35799=CARTESIAN_POINT('Ctrl Pts',(-4.71118521909806,-1.30000000000184,
8.97299157777347));
#35800=CARTESIAN_POINT('Ctrl Pts',(-4.69979673845635,-1.18514270861303,
9.01265747601402));
#35801=CARTESIAN_POINT('Ctrl Pts',(-4.68123224291413,-1.06847604194575,
9.04047819818707));
#35802=CARTESIAN_POINT('Ctrl Pts',(-4.62176651442011,-0.794772684000851,
9.0773849055878));
#35803=CARTESIAN_POINT('Ctrl Pts',(-4.55508919945686,-0.636309800095196,
9.05758940225795));
#35804=CARTESIAN_POINT('Ctrl Pts',(-4.48097546072877,-0.319434907277159,
9.05887937469646));
#35805=CARTESIAN_POINT('Ctrl Pts',(-4.43792035696632,-0.158333333333332,
9.04492251268587));
#35806=CARTESIAN_POINT('Ctrl Pts',(-4.42489047293301,0.158333333333335,
9.07569994753693));
#35807=CARTESIAN_POINT('Ctrl Pts',(-4.45431946765658,0.319434907277167,
9.12169110394353));
#35808=CARTESIAN_POINT('Ctrl Pts',(-4.50310673819832,0.636309800095206,
9.18053241785163));
#35809=CARTESIAN_POINT('Ctrl Pts',(-4.5552407438893,0.794772684000839,9.2329201259259));
#35810=CARTESIAN_POINT('Ctrl Pts',(-4.59827465855662,1.06847604194523,9.23934512618654));
#35811=CARTESIAN_POINT('Ctrl Pts',(-4.61143481041735,1.18514270861202,9.22755231220432));
#35812=CARTESIAN_POINT('Ctrl Pts',(-4.619127327043,1.30000000000036,9.20118553969676));
#35813=CARTESIAN_POINT('Ctrl Pts',(-4.69495064211116,-1.30000000000059,
8.95419085396944));
#35814=CARTESIAN_POINT('Ctrl Pts',(-4.68128463589822,-1.18514270861189,
8.98882994277146));
#35815=CARTESIAN_POINT('Ctrl Pts',(-4.66093855700018,-1.06847604194472,
9.01316614706116));
#35816=CARTESIAN_POINT('Ctrl Pts',(-4.59850274028019,-0.794772684000084,
9.04558592310283));
#35817=CARTESIAN_POINT('Ctrl Pts',(-4.53119122967445,-0.636309800094586,
9.02847825346989));
#35818=CARTESIAN_POINT('Ctrl Pts',(-4.45672260605069,-0.319434907276853,
9.03009305916203));
#35819=CARTESIAN_POINT('Ctrl Pts',(-4.41495444464664,-0.15833333333318,
9.01689174836914));
#35820=CARTESIAN_POINT('Ctrl Pts',(-4.40229456280709,0.158333333333182,
9.04714490931517));
#35821=CARTESIAN_POINT('Ctrl Pts',(-4.43103772959592,0.319434907276858,
9.09147270934599));
#35822=CARTESIAN_POINT('Ctrl Pts',(-4.48046279388933,0.636309800094593,
9.14970250735217));
#35823=CARTESIAN_POINT('Ctrl Pts',(-4.5326729724665,0.794772684000079,9.20051480885182));
#35824=CARTESIAN_POINT('Ctrl Pts',(-4.57885430690899,1.06847604194421,9.21113198619779));
#35825=CARTESIAN_POINT('Ctrl Pts',(-4.59399225125184,1.18514270861088,9.20244350937703));
#35826=CARTESIAN_POINT('Ctrl Pts',(-4.60427795144447,1.29999999999911,9.18047077306761));
#35827=CARTESIAN_POINT('Ctrl Pts',(-4.67856627830505,-1.29999999999933,
8.93502616643288));
#35828=CARTESIAN_POINT('Ctrl Pts',(-4.66121991197996,-1.18514270861074,
8.96689761340208));
#35829=CARTESIAN_POINT('Ctrl Pts',(-4.63827918184726,-1.06847604194369,
8.98905607801689));
#35830=CARTESIAN_POINT('Ctrl Pts',(-4.57235740641933,-0.794772683999317,
9.01780763174861));
#35831=CARTESIAN_POINT('Ctrl Pts',(-4.50654676965981,-0.636309800093967,
8.99992851636126));
#35832=CARTESIAN_POINT('Ctrl Pts',(-4.43234600151776,-0.319434907276541,
9.00085303067297));
#35833=CARTESIAN_POINT('Ctrl Pts',(-4.39134027920529,-0.158333333333026,
8.98925773605429));
#35834=CARTESIAN_POINT('Ctrl Pts',(-4.37907445022117,0.158333333333029,
9.01894067946668));
#35835=CARTESIAN_POINT('Ctrl Pts',(-4.40727167410129,0.31943490727655,9.06135701309618));
#35836=CARTESIAN_POINT('Ctrl Pts',(-4.45759321036425,0.636309800093976,
9.11857629848427));
#35837=CARTESIAN_POINT('Ctrl Pts',(-4.51018664253024,0.794772683999303,
9.16732445132942));
#35838=CARTESIAN_POINT('Ctrl Pts',(-4.5596318477288,1.06847604194317,9.18205049763488));
#35839=CARTESIAN_POINT('Ctrl Pts',(-4.57673844140366,1.18514270860973,9.17654629265128));
#35840=CARTESIAN_POINT('Ctrl Pts',(-4.58954863154836,1.29999999999785,9.15916352289222));
#35841=CARTESIAN_POINT('Ctrl Pts',(-4.6701509419572,-1.29999999999917,8.92533046634025));
#35842=CARTESIAN_POINT('Ctrl Pts',(-4.65142766969827,-1.1851427086106,8.95492352907192));
#35843=CARTESIAN_POINT('Ctrl Pts',(-4.62744617719791,-1.06847604194356,
8.97547310910894));
#35844=CARTESIAN_POINT('Ctrl Pts',(-4.55989659138003,-0.794772683999221,
9.00205449575667));
#35845=CARTESIAN_POINT('Ctrl Pts',(-4.49408411031015,-0.63630980009389,
8.98504509224385));
#35846=CARTESIAN_POINT('Ctrl Pts',(-4.41966049746464,-0.319434907276502,
8.98619857882796));
#35847=CARTESIAN_POINT('Ctrl Pts',(-4.37898964047838,-0.158333333333007,
8.97552017176666));
#35848=CARTESIAN_POINT('Ctrl Pts',(-4.36691509201292,0.15833333333301,9.00492423313939));
#35849=CARTESIAN_POINT('Ctrl Pts',(-4.39510610028442,0.319434907276512,
9.0459240393071));
#35850=CARTESIAN_POINT('Ctrl Pts',(-4.44576029472738,0.6363098000939,9.10279595766359));
#35851=CARTESIAN_POINT('Ctrl Pts',(-4.49799652989938,0.794772683999208,
9.15130408714472));
#35852=CARTESIAN_POINT('Ctrl Pts',(-4.54911845680959,1.06847604194304,9.16813305033091));
#35853=CARTESIAN_POINT('Ctrl Pts',(-4.56735662103664,1.18514270860958,9.16408323843005));
#35854=CARTESIAN_POINT('Ctrl Pts',(-4.58170416158539,1.29999999999769,9.14869898003955));
#35855=CARTESIAN_POINT('Ctrl Pts',(-4.66976691393927,-1.29999999999918,
8.92489233702175));
#35856=CARTESIAN_POINT('Ctrl Pts',(-4.65098084725317,-1.1851427086106,8.95438205260471));
#35857=CARTESIAN_POINT('Ctrl Pts',(-4.62695198669783,-1.06847604194356,
8.97485851129906));
#35858=CARTESIAN_POINT('Ctrl Pts',(-4.55932860920279,-0.794772683999223,
9.00134080067594));
#35859=CARTESIAN_POINT('Ctrl Pts',(-4.49351714732034,-0.636309800093892,
8.98436918385726));
#35860=CARTESIAN_POINT('Ctrl Pts',(-4.41908317169223,-0.319434907276503,
8.98553341344849));
#35861=CARTESIAN_POINT('Ctrl Pts',(-4.37842602012149,-0.158333333333007,
8.9748991022583));
#35862=CARTESIAN_POINT('Ctrl Pts',(-4.36636003466096,0.15833333333301,9.00429066709948));
#35863=CARTESIAN_POINT('Ctrl Pts',(-4.39455172304245,0.319434907276513,
9.04522449790572));
#35864=CARTESIAN_POINT('Ctrl Pts',(-4.44522186243731,0.636309800093902,
9.10207933113157));
#35865=CARTESIAN_POINT('Ctrl Pts',(-4.49744245446759,0.79477268399921,9.1505756752673));
#35866=CARTESIAN_POINT('Ctrl Pts',(-4.54864086351237,1.06847604194304,9.16749987030133));
#35867=CARTESIAN_POINT('Ctrl Pts',(-4.56693044085057,1.18514270860959,9.16351623316231));
#35868=CARTESIAN_POINT('Ctrl Pts',(-4.58134770133951,1.29999999999769,9.14822310195727));
#35869=CARTESIAN_POINT('Ctrl Pts',(-4.66938288464626,-1.29999999999917,
8.92445418124858));
#35870=CARTESIAN_POINT('Ctrl Pts',(-4.65053373614899,-1.1851427086106,8.95384105559867));
#35871=CARTESIAN_POINT('Ctrl Pts',(-4.62645731659445,-1.06847604194356,
8.97424472842433));
#35872=CARTESIAN_POINT('Ctrl Pts',(-4.55875992909808,-0.794772683999222,
9.00062830178755));
#35873=CARTESIAN_POINT('Ctrl Pts',(-4.49294953019207,-0.636309800093891,
8.98369436139404));
#35874=CARTESIAN_POINT('Ctrl Pts',(-4.41850559492078,-0.319434907276503,
8.98486867585451));
#35875=CARTESIAN_POINT('Ctrl Pts',(-4.37786298007624,-0.158333333333007,
8.97427713099188));
#35876=CARTESIAN_POINT('Ctrl Pts',(-4.3658055989932,0.15833333333301,9.00365612250243));
#35877=CARTESIAN_POINT('Ctrl Pts',(-4.39399706732632,0.319434907276513,
9.04452539926505));
#35878=CARTESIAN_POINT('Ctrl Pts',(-4.44468305731729,0.636309800093901,
9.10136330569213));
#35879=CARTESIAN_POINT('Ctrl Pts',(-4.49688870555336,0.794772683999209,
9.14984678924392));
#35880=CARTESIAN_POINT('Ctrl Pts',(-4.5481636859491,1.06847604194304,9.16686606916854));
#35881=CARTESIAN_POINT('Ctrl Pts',(-4.56650460819516,1.18514270860959,9.16294870394952));
#35882=CARTESIAN_POINT('Ctrl Pts',(-4.58099141359925,1.29999999999769,9.14774695785857));
#35883=CARTESIAN_POINT('Ctrl Pts',(-4.66861347039935,-1.29999999999918,
8.92358013837401));
#35884=CARTESIAN_POINT('Ctrl Pts',(-4.64963749040481,-1.1851427086106,8.95276236609815));
#35885=CARTESIAN_POINT('Ctrl Pts',(-4.6254655903302,-1.06847604194356,8.97302101570254));
#35886=CARTESIAN_POINT('Ctrl Pts',(-4.55762005076071,-0.794772683999223,
8.99920729840525));
#35887=CARTESIAN_POINT('Ctrl Pts',(-4.49181298717508,-0.636309800093892,
8.98234672987362));
#35888=CARTESIAN_POINT('Ctrl Pts',(-4.4173495517368,-0.319434907276503,
8.9835404905542));
#35889=CARTESIAN_POINT('Ctrl Pts',(-4.37673580888741,-0.158333333333008,
8.97303479950824));
#35890=CARTESIAN_POINT('Ctrl Pts',(-4.36469554604491,0.15833333333301,9.00238874670316));
#35891=CARTESIAN_POINT('Ctrl Pts',(-4.39288607310709,0.319434907276513,
9.04312964025067));
#35892=CARTESIAN_POINT('Ctrl Pts',(-4.44360440763777,0.636309800093902,
9.09993270284471));
#35893=CARTESIAN_POINT('Ctrl Pts',(-4.49578189097155,0.79477268399921,9.14838786158691));
#35894=CARTESIAN_POINT('Ctrl Pts',(-4.54721036505604,1.06847604194304,9.16559680985666));
#35895=CARTESIAN_POINT('Ctrl Pts',(-4.56565380824756,1.18514270860959,9.16181226444056));
#35896=CARTESIAN_POINT('Ctrl Pts',(-4.5802792138122,1.29999999999769,9.14679405755677));
#35897=CARTESIAN_POINT('Ctrl Pts',(-4.66694146222015,-1.29999999999918,
8.92169446539642));
#35898=CARTESIAN_POINT('Ctrl Pts',(-4.64768643612071,-1.18514270861061,
8.95044021925838));
#35899=CARTESIAN_POINT('Ctrl Pts',(-4.62330517815074,-1.06847604194356,
8.97038867822463));
#35900=CARTESIAN_POINT('Ctrl Pts',(-4.55513697366628,-0.794772683999226,
8.99615009801027));
#35901=CARTESIAN_POINT('Ctrl Pts',(-4.4893423677817,-0.636309800093895,
8.97943975591989));
#35902=CARTESIAN_POINT('Ctrl Pts',(-4.41484050350011,-0.319434907276505,
8.98066927837885));
#35903=CARTESIAN_POINT('Ctrl Pts',(-4.3742927596087,-0.158333333333008,
8.9703440922254));
#35904=CARTESIAN_POINT('Ctrl Pts',(-4.36228947202549,0.158333333333011,
8.99964374619661));
#35905=CARTESIAN_POINT('Ctrl Pts',(-4.39047144214751,0.319434907276514,
9.04011650144985));
#35906=CARTESIAN_POINT('Ctrl Pts',(-4.44126183214889,0.636309800093905,
9.09684112242019));
#35907=CARTESIAN_POINT('Ctrl Pts',(-4.4933884427905,0.794772683999213,9.14521954990681));
#35908=CARTESIAN_POINT('Ctrl Pts',(-4.5451512764238,1.06847604194305,9.16283677826069));
#35909=CARTESIAN_POINT('Ctrl Pts',(-4.56381585087666,1.18514270860959,9.1593415406099));
#35910=CARTESIAN_POINT('Ctrl Pts',(-4.57873878710452,1.2999999999977,9.14472521993657));
#35911=CARTESIAN_POINT('Ctrl Pts',(-4.66383012966025,-1.29999999999921,
8.9182524003141));
#35912=CARTESIAN_POINT('Ctrl Pts',(-4.64403034108178,-1.18514270861063,
8.94624124721707));
#35913=CARTESIAN_POINT('Ctrl Pts',(-4.61924529166989,-1.06847604194358,
8.96564550953633));
#35914=CARTESIAN_POINT('Ctrl Pts',(-4.55046991947324,-0.794772683999241,
8.99064112957451));
#35915=CARTESIAN_POINT('Ctrl Pts',(-4.48473463973545,-0.636309800093906,
8.97414722434077));
#35916=CARTESIAN_POINT('Ctrl Pts',(-4.41018948450046,-0.31943490727651,
8.97539711220255));
#35917=CARTESIAN_POINT('Ctrl Pts',(-4.36979011905288,-0.158333333333011,
8.96536307830696));
#35918=CARTESIAN_POINT('Ctrl Pts',(-4.35785324122113,0.158333333333013,
8.9945642572073));
#35919=CARTESIAN_POINT('Ctrl Pts',(-4.385970225677,0.31943490727652,9.03461780582221));
#35920=CARTESIAN_POINT('Ctrl Pts',(-4.43690458531225,0.636309800093916,
9.0911817256847));
#35921=CARTESIAN_POINT('Ctrl Pts',(-4.48900848213158,0.794772683999227,
9.13931103832431));
#35922=CARTESIAN_POINT('Ctrl Pts',(-4.54139807333501,1.06847604194306,9.15766798960639));
#35923=CARTESIAN_POINT('Ctrl Pts',(-4.56046217222793,1.18514270860961,9.15472013499506));
#35924=CARTESIAN_POINT('Ctrl Pts',(-4.57591285720746,1.29999999999772,9.14087838175445));
#35925=CARTESIAN_POINT('Ctrl Pts',(-4.66068107962505,-1.29999999999924,
8.91486837523097));
#35926=CARTESIAN_POINT('Ctrl Pts',(-4.64027435180129,-1.18514270861066,
8.94220381448194));
#35927=CARTESIAN_POINT('Ctrl Pts',(-4.6150485220739,-1.06847604194361,8.961125420333));
#35928=CARTESIAN_POINT('Ctrl Pts',(-4.54563871953845,-0.794772683999263,
8.98540047676775));
#35929=CARTESIAN_POINT('Ctrl Pts',(-4.48003079702452,-0.636309800093924,
8.96900863205523));
#35930=CARTESIAN_POINT('Ctrl Pts',(-4.40550277551653,-0.319434907276519,
8.97017988484825));
#35931=CARTESIAN_POINT('Ctrl Pts',(-4.36532033989244,-0.158333333333015,
8.9603283847655));
#35932=CARTESIAN_POINT('Ctrl Pts',(-4.35344807657413,0.158333333333018,
8.98943145542105));
#35933=CARTESIAN_POINT('Ctrl Pts',(-4.38139047634244,0.319434907276529,
9.02923464366669));
#35934=CARTESIAN_POINT('Ctrl Pts',(-4.4324846784807,0.636309800093934,9.08561567754849));
#35935=CARTESIAN_POINT('Ctrl Pts',(-4.48470648986488,0.79477268399925,9.13328477364608));
#35936=CARTESIAN_POINT('Ctrl Pts',(-4.53774240678189,1.06847604194309,9.15235208885783));
#35937=CARTESIAN_POINT('Ctrl Pts',(-4.55718993418727,1.18514270860965,9.14997562706888));
#35938=CARTESIAN_POINT('Ctrl Pts',(-4.57312770573906,1.29999999999776,9.13696916924947));
#35939=CARTESIAN_POINT('Ctrl Pts',(-4.65646846761001,-1.29999999999927,
8.91037603753981));
#35940=CARTESIAN_POINT('Ctrl Pts',(-4.6352269128868,-1.18514270861068,8.93688219706871));
#35941=CARTESIAN_POINT('Ctrl Pts',(-4.60939692572218,-1.06847604194363,
8.95518720285638));
#35942=CARTESIAN_POINT('Ctrl Pts',(-4.53912429124843,-0.794772683999279,
8.9785291223523));
#35943=CARTESIAN_POINT('Ctrl Pts',(-4.47370568965768,-0.636309800093937,
8.96224085178219));
#35944=CARTESIAN_POINT('Ctrl Pts',(-4.39921677806005,-0.319434907276526,
8.96328101300153));
#35945=CARTESIAN_POINT('Ctrl Pts',(-4.35934575137206,-0.158333333333019,
8.95363882849874));
#35946=CARTESIAN_POINT('Ctrl Pts',(-4.34755960691698,0.158333333333021,
8.98260930693076));
#35947=CARTESIAN_POINT('Ctrl Pts',(-4.37523520704753,0.319434907276536,
9.02212829560295));
#35948=CARTESIAN_POINT('Ctrl Pts',(-4.42655026919399,0.636309800093947,
9.07825279273653));
#35949=CARTESIAN_POINT('Ctrl Pts',(-4.478975712082,0.794772683999266,9.1252385327736));
#35950=CARTESIAN_POINT('Ctrl Pts',(-4.53288438138959,1.06847604194312,9.14523718484589));
#35951=CARTESIAN_POINT('Ctrl Pts',(-4.55284054409227,1.18514270860967,9.14362704630053));
#35952=CARTESIAN_POINT('Ctrl Pts',(-4.56941780406742,1.29999999999779,9.1317500937508));
#35953=CARTESIAN_POINT('Ctrl Pts',(-4.65173281621968,-1.29999999999929,
8.90531318004771));
#35954=CARTESIAN_POINT('Ctrl Pts',(-4.62955463356647,-1.18514270861071,
8.93088072622139));
#35955=CARTESIAN_POINT('Ctrl Pts',(-4.60304276398764,-1.06847604194366,
8.94849480373194));
#35956=CARTESIAN_POINT('Ctrl Pts',(-4.53178335783007,-0.794772683999295,
8.97081274276759));
#35957=CARTESIAN_POINT('Ctrl Pts',(-4.46654428001928,-0.636309800093951,
8.95469810355981));
#35958=CARTESIAN_POINT('Ctrl Pts',(-4.39208112856424,-0.319434907276533,
8.95562126723687));
#35959=CARTESIAN_POINT('Ctrl Pts',(-4.35255944184997,-0.158333333333022,
8.94621635495254));
#35960=CARTESIAN_POINT('Ctrl Pts',(-4.34088102723102,0.158333333333025,
8.97501821684063));
#35961=CARTESIAN_POINT('Ctrl Pts',(-4.36829040143653,0.319434907276542,
9.01415991626995));
#35962=CARTESIAN_POINT('Ctrl Pts',(-4.41984928194637,0.63630980009396,9.06999969602464));
#35963=CARTESIAN_POINT('Ctrl Pts',(-4.47244306656148,0.794772683999283,
9.11631047386423));
#35964=CARTESIAN_POINT('Ctrl Pts',(-4.52734909122831,1.06847604194314,9.13733324890494));
#35965=CARTESIAN_POINT('Ctrl Pts',(-4.54789985251689,1.1851427086097,9.1365511894133));
#35966=CARTESIAN_POINT('Ctrl Pts',(-4.56523459148449,1.29999999999781,9.12588709008547));
#35967=CARTESIAN_POINT('Ctrl Pts',(-4.64344920784895,-1.29999999999938,
8.89608889763532));
#35968=CARTESIAN_POINT('Ctrl Pts',(-4.61980770460998,-1.18514270861078,
8.91964675638172));
#35969=CARTESIAN_POINT('Ctrl Pts',(-4.59219580800188,-1.06847604194373,
8.93584234783779));
#35970=CARTESIAN_POINT('Ctrl Pts',(-4.51923440013915,-0.794772683999346,
8.95624909376107));
#35971=CARTESIAN_POINT('Ctrl Pts',(-4.45405596235386,-0.636309800093991,
8.94088045270961));
#35972=CARTESIAN_POINT('Ctrl Pts',(-4.37935657175661,-0.319434907276553,
8.94206055169668));
#35973=CARTESIAN_POINT('Ctrl Pts',(-4.34013166891365,-0.158333333333032,
8.93360300549307));
#35974=CARTESIAN_POINT('Ctrl Pts',(-4.32863106798455,0.158333333333035,
8.96212981746688));
#35975=CARTESIAN_POINT('Ctrl Pts',(-4.35601081266152,0.319434907276562,
8.99989490221463));
#35976=CARTESIAN_POINT('Ctrl Pts',(-4.40798614551958,0.636309800094001,
9.05523158141004));
#35977=CARTESIAN_POINT('Ctrl Pts',(-4.46040103921712,0.794772683999334,
9.10105041962622));
#35978=CARTESIAN_POINT('Ctrl Pts',(-4.51703295531289,1.06847604194321,9.12397152635148));
#35979=CARTESIAN_POINT('Ctrl Pts',(-4.5387044942274,1.18514270860977,9.12457455335947));
#35980=CARTESIAN_POINT('Ctrl Pts',(-4.55753371399785,1.29999999999789,9.11585890958479));
#35981=CARTESIAN_POINT('Ctrl Pts',(-4.63312481503961,-1.2999999999996,8.8844851501262));
#35982=CARTESIAN_POINT('Ctrl Pts',(-4.60764312208804,-1.18514270861098,
8.90554365189251));
#35983=CARTESIAN_POINT('Ctrl Pts',(-4.57865309865353,-1.06847604194391,
8.91996761939151));
#35984=CARTESIAN_POINT('Ctrl Pts',(-4.50357539983094,-0.79477268399948,
8.93796276842742));
#35985=CARTESIAN_POINT('Ctrl Pts',(-4.43850715508563,-0.6363098000941,8.92347121376613));
#35986=CARTESIAN_POINT('Ctrl Pts',(-4.36355026845127,-0.319434907276608,
8.92491696466319));
#35987=CARTESIAN_POINT('Ctrl Pts',(-4.32475600711511,-0.158333333333059,
8.9175594843186));
#35988=CARTESIAN_POINT('Ctrl Pts',(-4.31342837560234,0.158333333333061,
8.94582352378791));
#35989=CARTESIAN_POINT('Ctrl Pts',(-4.34057580169344,0.319434907276616,
8.98216733508143));
#35990=CARTESIAN_POINT('Ctrl Pts',(-4.39310931357207,0.636309800094108,
9.03682214176766));
#35991=CARTESIAN_POINT('Ctrl Pts',(-4.44556179129244,0.79477268399947,9.08163575589306));
#35992=CARTESIAN_POINT('Ctrl Pts',(-4.50444501918549,1.06847604194339,9.10677955103585));
#35993=CARTESIAN_POINT('Ctrl Pts',(-4.52752445138544,1.18514270860997,9.10909684800232));
#35994=CARTESIAN_POINT('Ctrl Pts',(-4.54819494826906,1.29999999999812,9.10284762468738));
#35995=CARTESIAN_POINT('Ctrl Pts',(-4.6161315750982,-1.29999999999994,8.866720229488));
#35996=CARTESIAN_POINT('Ctrl Pts',(-4.58734282213314,-1.1851427086113,8.8843813116644));
#35997=CARTESIAN_POINT('Ctrl Pts',(-4.55590757304771,-1.06847604194419,
8.89636879561943));
#35998=CARTESIAN_POINT('Ctrl Pts',(-4.47717192359272,-0.794772683999692,
8.91095513475269));
#35999=CARTESIAN_POINT('Ctrl Pts',(-4.41243224464801,-0.636309800094267,
8.89762029551915));
#36000=CARTESIAN_POINT('Ctrl Pts',(-4.33739806449051,-0.319434907276691,
8.8989196168512));
#36001=CARTESIAN_POINT('Ctrl Pts',(-4.29979269678325,-0.158333333333101,
8.89246819235823));
#36002=CARTESIAN_POINT('Ctrl Pts',(-4.2890368109278,0.158333333333103,8.91979970437644));
#36003=CARTESIAN_POINT('Ctrl Pts',(-4.31586211496023,0.319434907276701,
8.95379793509703));
#36004=CARTESIAN_POINT('Ctrl Pts',(-4.36903657855686,0.636309800094277,
9.00773239700906));
#36005=CARTESIAN_POINT('Ctrl Pts',(-4.42091912841294,0.794772683999679,
9.05187752173051));
#36006=CARTESIAN_POINT('Ctrl Pts',(-4.48321977595797,1.06847604194367,9.08089683226442));
#36007=CARTESIAN_POINT('Ctrl Pts',(-4.5085784892226,1.18514270861028,9.08594630258439));
#36008=CARTESIAN_POINT('Ctrl Pts',(-4.5323282738961,1.29999999999846,9.08348385896562));
#36009=CARTESIAN_POINT('Ctrl Pts',(-4.59925616540522,-1.30000000000032,
8.84868787826823));
#36010=CARTESIAN_POINT('Ctrl Pts',(-4.56715847804536,-1.18514270861164,
8.86295398912095));
#36011=CARTESIAN_POINT('Ctrl Pts',(-4.53330573141733,-1.0684760419445,8.87245513260324));
#36012=CARTESIAN_POINT('Ctrl Pts',(-4.45104457648016,-0.79477268399992,
8.88339664689042));
#36013=CARTESIAN_POINT('Ctrl Pts',(-4.38695875673159,-0.636309800094451,
8.87064203255691));
#36014=CARTESIAN_POINT('Ctrl Pts',(-4.31180285795805,-0.319434907276784,
8.87187236007619));
#36015=CARTESIAN_POINT('Ctrl Pts',(-4.27516556234439,-0.158333333333146,
8.86674567150868));
#36016=CARTESIAN_POINT('Ctrl Pts',(-4.26450690044457,0.158333333333149,
8.8939273071107));
#36017=CARTESIAN_POINT('Ctrl Pts',(-4.29033189167834,0.319434907276792,
8.92664269784874));
#36018=CARTESIAN_POINT('Ctrl Pts',(-4.34408982228034,0.636309800094459,
8.97995023961783));
#36019=CARTESIAN_POINT('Ctrl Pts',(-4.39602601489726,0.794772683999908,
9.02244203897655));
#36020=CARTESIAN_POINT('Ctrl Pts',(-4.46216995079192,1.06847604194398,9.05465827179795));
#36021=CARTESIAN_POINT('Ctrl Pts',(-4.48997068438421,1.18514270861063,9.06217871559226));
#36022=CARTESIAN_POINT('Ctrl Pts',(-4.51694089259435,1.29999999999883,9.06327438972156));
#36023=CARTESIAN_POINT('Ctrl Pts',(-4.58213601648041,-1.30000000000044,
8.83109175807416));
#36024=CARTESIAN_POINT('Ctrl Pts',(-4.54681642970871,-1.18514270861175,
8.84177044112995));
#36025=CARTESIAN_POINT('Ctrl Pts',(-4.5105029459682,-1.0684760419446,8.84883487206191));
#36026=CARTESIAN_POINT('Ctrl Pts',(-4.42431543321399,-0.794772683999997,
8.85680547531458));
#36027=CARTESIAN_POINT('Ctrl Pts',(-4.35985910129541,-0.63630980009451,
8.84647000817917));
#36028=CARTESIAN_POINT('Ctrl Pts',(-4.28438268322261,-0.319434907276813,
8.84796957882561));
#36029=CARTESIAN_POINT('Ctrl Pts',(-4.24924643579066,-0.158333333333161,
8.84319498291508));
#36030=CARTESIAN_POINT('Ctrl Pts',(-4.23918044863051,0.158333333333164,
8.86934531494356));
#36031=CARTESIAN_POINT('Ctrl Pts',(-4.26434527221524,0.319434907276823,
8.90018990350982));
#36032=CARTESIAN_POINT('Ctrl Pts',(-4.31912538055828,0.636309800094519,
8.95212032183667));
#36033=CARTESIAN_POINT('Ctrl Pts',(-4.37148981486424,0.794772683999981,
8.99233910505878));
#36034=CARTESIAN_POINT('Ctrl Pts',(-4.44130624086955,1.06847604194408,9.02805188718885));
#36035=CARTESIAN_POINT('Ctrl Pts',(-4.47132133777115,1.18514270861074,9.03843348444035));
#36036=CARTESIAN_POINT('Ctrl Pts',(-4.50113058771019,1.29999999999895,9.04373793884824));
#36037=CARTESIAN_POINT('Ctrl Pts',(-4.56928530707914,-1.30000000000059,
8.8178345395562));
#36038=CARTESIAN_POINT('Ctrl Pts',(-4.53110597748958,-1.18514270861189,
8.82663583470339));
#36039=CARTESIAN_POINT('Ctrl Pts',(-4.49276685699007,-1.06847604194472,
8.83220890665423));
#36040=CARTESIAN_POINT('Ctrl Pts',(-4.40382666995363,-0.794772684000086,
8.83762597636249));
#36041=CARTESIAN_POINT('Ctrl Pts',(-4.34059639319766,-0.636309800094585,
8.82639912022816));
#36042=CARTESIAN_POINT('Ctrl Pts',(-4.26501625064136,-0.319434907276852,
8.8278652604988));
#36043=CARTESIAN_POINT('Ctrl Pts',(-4.23003147946568,-0.15833333333318,
8.82512789904));
#36044=CARTESIAN_POINT('Ctrl Pts',(-4.21988571051916,0.158333333333182,
8.85142664380134));
#36045=CARTESIAN_POINT('Ctrl Pts',(-4.24464215762767,0.319434907276859,
8.88069629902359));
#36046=CARTESIAN_POINT('Ctrl Pts',(-4.29972425819613,0.636309800094593,
8.93232308575814));
#36047=CARTESIAN_POINT('Ctrl Pts',(-4.35149662840352,0.794772684000076,
8.97226784151546));
#36048=CARTESIAN_POINT('Ctrl Pts',(-4.42431116283579,1.0684760419442,9.01019869496993));
#36049=CARTESIAN_POINT('Ctrl Pts',(-4.45636948654916,1.18514270861088,9.02211217414616));
#36050=CARTESIAN_POINT('Ctrl Pts',(-4.48896742006456,1.2999999999991,9.0295202715148));
#36051=CARTESIAN_POINT('Ctrl Pts',(-4.55583799175337,-1.30000000000069,
8.80577096598503));
#36052=CARTESIAN_POINT('Ctrl Pts',(-4.51528035914532,-1.18514270861198,
8.81177075214429));
#36053=CARTESIAN_POINT('Ctrl Pts',(-4.47510676734569,-1.0684760419448,8.81546891809767));
#36054=CARTESIAN_POINT('Ctrl Pts',(-4.38318494468386,-0.794772684000149,
8.81869521815243));
#36055=CARTESIAN_POINT('Ctrl Pts',(-4.31952068576917,-0.636309800094635,
8.80960689064762));
#36056=CARTESIAN_POINT('Ctrl Pts',(-4.24365109879925,-0.319434907276876,
8.81136459575073));
#36057=CARTESIAN_POINT('Ctrl Pts',(-4.2097125059512,-0.158333333333192,
8.80902096173901));
#36058=CARTESIAN_POINT('Ctrl Pts',(-4.20031047460861,0.158333333333195,
8.83399022560956));
#36059=CARTESIAN_POINT('Ctrl Pts',(-4.22514604427133,0.319434907276886,
8.86080966478229));
#36060=CARTESIAN_POINT('Ctrl Pts',(-4.28125531227806,0.636309800094644,
8.91091769219793));
#36061=CARTESIAN_POINT('Ctrl Pts',(-4.33317146618663,0.794772684000139,
8.94946370267855));
#36062=CARTESIAN_POINT('Ctrl Pts',(-4.40863350682741,1.06847604194429,8.99021278084444));
#36063=CARTESIAN_POINT('Ctrl Pts',(-4.44229150336739,1.18514270861097,9.00438862413133));
#36064=CARTESIAN_POINT('Ctrl Pts',(-4.47694277519813,1.29999999999921,9.01510154466924));
#36065=CARTESIAN_POINT('Ctrl Pts',(-4.54314694081231,-1.30000000000081,
8.79218277495134));
#36066=CARTESIAN_POINT('Ctrl Pts',(-4.49993318296694,-1.18514270861209,
8.79591737570066));
#36067=CARTESIAN_POINT('Ctrl Pts',(-4.45779290816555,-1.0684760419449,8.79800537855424));
#36068=CARTESIAN_POINT('Ctrl Pts',(-4.36292040382263,-0.79477268400022,
8.79902511230956));
#36069=CARTESIAN_POINT('Ctrl Pts',(-4.29959080148349,-0.636309800094691,
8.79067950908064));
#36070=CARTESIAN_POINT('Ctrl Pts',(-4.22346388217673,-0.319434907276905,
8.79268807838411));
#36071=CARTESIAN_POINT('Ctrl Pts',(-4.19031851099241,-0.158333333333206,
8.79123196627607));
#36072=CARTESIAN_POINT('Ctrl Pts',(-4.18082761705046,0.158333333333209,
8.81634013469114));
#36073=CARTESIAN_POINT('Ctrl Pts',(-4.2046155438811,0.319434907276914,8.84267021748946));
#36074=CARTESIAN_POINT('Ctrl Pts',(-4.26113836839254,0.636309800094701,
8.89228222330199));
#36075=CARTESIAN_POINT('Ctrl Pts',(-4.3132448740173,0.794772684000209,8.92922932179509));
#36076=CARTESIAN_POINT('Ctrl Pts',(-4.39195396843211,1.06847604194438,8.97177994644193));
#36077=CARTESIAN_POINT('Ctrl Pts',(-4.42765482463769,1.18514270861108,8.9874919159399));
#36078=CARTESIAN_POINT('Ctrl Pts',(-4.46498628653604,1.29999999999932,9.00049726618224));
#36079=CARTESIAN_POINT('Ctrl Pts',(-4.53154583913819,-1.30000000000086,
8.78285112053937));
#36080=CARTESIAN_POINT('Ctrl Pts',(-4.48607560509566,-1.18514270861213,
8.78475025417892));
#36081=CARTESIAN_POINT('Ctrl Pts',(-4.44228833053133,-1.06847604194494,
8.7854889063467));
#36082=CARTESIAN_POINT('Ctrl Pts',(-4.34501893974323,-0.794772684000252,
8.78451439626788));
#36083=CARTESIAN_POINT('Ctrl Pts',(-4.2821642101198,-0.636309800094717,
8.77641182159235));
#36084=CARTESIAN_POINT('Ctrl Pts',(-4.20592949896746,-0.319434907276918,
8.77841722805452));
#36085=CARTESIAN_POINT('Ctrl Pts',(-4.17329074901145,-0.158333333333213,
8.77798649026425));
#36086=CARTESIAN_POINT('Ctrl Pts',(-4.16401602768526,0.158333333333215,
8.80268342941709));
#36087=CARTESIAN_POINT('Ctrl Pts',(-4.18750489629661,0.319434907276928,
8.82757110874094));
#36088=CARTESIAN_POINT('Ctrl Pts',(-4.24459337785601,0.636309800094728,
8.87636044696449));
#36089=CARTESIAN_POINT('Ctrl Pts',(-4.29665787175149,0.794772684000242,
8.91232952829772));
#36090=CARTESIAN_POINT('Ctrl Pts',(-4.37787154550263,1.06847604194443,8.95672080950009));
#36091=CARTESIAN_POINT('Ctrl Pts',(-4.41516042469046,1.18514270861112,8.97390617246834));
#36092=CARTESIAN_POINT('Ctrl Pts',(-4.45458379296244,1.29999999999938,8.98906155763138));
#36093=CARTESIAN_POINT('Ctrl Pts',(-4.52306413166245,-1.30000000000088,
8.77380443519589));
#36094=CARTESIAN_POINT('Ctrl Pts',(-4.4758111708909,-1.18514270861215,8.77420613643231));
#36095=CARTESIAN_POINT('Ctrl Pts',(-4.43067705000433,-1.06847604194496,
8.77393111173708));
#36096=CARTESIAN_POINT('Ctrl Pts',(-4.33130314571344,-0.794772684000266,
8.77173237739195));
#36097=CARTESIAN_POINT('Ctrl Pts',(-4.26846935116606,-0.636309800094728,
8.76450136718779));
#36098=CARTESIAN_POINT('Ctrl Pts',(-4.19191385220492,-0.319434907276924,
8.76696076118828));
#36099=CARTESIAN_POINT('Ctrl Pts',(-4.15967196114376,-0.158333333333216,
8.76738409871529));
#36100=CARTESIAN_POINT('Ctrl Pts',(-4.15054722647059,0.158333333333218,
8.79179444465084));
#36101=CARTESIAN_POINT('Ctrl Pts',(-4.17383252913904,0.319434907276932,
8.81543206158095));
#36102=CARTESIAN_POINT('Ctrl Pts',(-4.23145909870731,0.636309800094738,
8.86340646993248));
#36103=CARTESIAN_POINT('Ctrl Pts',(-4.28368320628294,0.794772684000255,
8.89827172268338));
#36104=CARTESIAN_POINT('Ctrl Pts',(-4.36682683181974,1.06847604194444,8.94427098979597));
#36105=CARTESIAN_POINT('Ctrl Pts',(-4.40529200932223,1.18514270861114,8.9628014504945));
#36106=CARTESIAN_POINT('Ctrl Pts',(-4.44623256960727,1.2999999999994,8.97995099359933));
#36107=CARTESIAN_POINT('Ctrl Pts',(-4.50966808728432,-1.30000000000095,
8.76156795041173));
#36108=CARTESIAN_POINT('Ctrl Pts',(-4.45978821012882,-1.18514270861221,
8.75962299771254));
#36109=CARTESIAN_POINT('Ctrl Pts',(-4.41268861520961,-1.06847604194501,
8.75771534776358));
#36110=CARTESIAN_POINT('Ctrl Pts',(-4.31030213686421,-0.794772684000305,
8.75339447157283));
#36111=CARTESIAN_POINT('Ctrl Pts',(-4.2475790859924,-0.63630980009476,8.74732930188912));
#36112=CARTESIAN_POINT('Ctrl Pts',(-4.17078494416672,-0.31943490727694,
8.74999343533582));
#36113=CARTESIAN_POINT('Ctrl Pts',(-4.13947211741483,-0.158333333333223,
8.75104020535033));
#36114=CARTESIAN_POINT('Ctrl Pts',(-4.13054071912278,0.158333333333226,
8.77506361269285));
#36115=CARTESIAN_POINT('Ctrl Pts',(-4.15314876472547,0.319434907276948,
8.79754744461613));
#36116=CARTESIAN_POINT('Ctrl Pts',(-4.2112886885093,0.636309800094769,8.84482107130969));
#36117=CARTESIAN_POINT('Ctrl Pts',(-4.26335617522184,0.794772684000296,
8.87866853656956));
#36118=CARTESIAN_POINT('Ctrl Pts',(-4.34975387162024,1.0684760419445,8.92645407663372));
#36119=CARTESIAN_POINT('Ctrl Pts',(-4.39032400174482,1.1851427086112,8.94641808617921));
#36120=CARTESIAN_POINT('Ctrl Pts',(-4.43406590057326,1.29999999999946,8.9656615156052));
#36121=CARTESIAN_POINT('Ctrl Pts',(-4.48972114667131,-1.3000000000011,8.74286441635357));
#36122=CARTESIAN_POINT('Ctrl Pts',(-4.43547883514081,-1.18514270861236,
8.73822466035712));
#36123=CARTESIAN_POINT('Ctrl Pts',(-4.38514975315686,-1.06847604194515,
8.73442121547394));
#36124=CARTESIAN_POINT('Ctrl Pts',(-4.27791984856732,-0.794772684000405,
8.72756654289241));
#36125=CARTESIAN_POINT('Ctrl Pts',(-4.21573214866852,-0.636309800094839,
8.7225529096059));
#36126=CARTESIAN_POINT('Ctrl Pts',(-4.13855575725197,-0.319434907276979,
8.72558877417398));
#36127=CARTESIAN_POINT('Ctrl Pts',(-4.10842119208862,-0.158333333333243,
8.72800182405605));
#36128=CARTESIAN_POINT('Ctrl Pts',(-4.09977236837343,0.158333333333246,
8.75144365581481));
#36129=CARTESIAN_POINT('Ctrl Pts',(-4.12136531014535,0.319434907276988,
8.7721314354358));
#36130=CARTESIAN_POINT('Ctrl Pts',(-4.18070631104924,0.636309800094849,
8.81753949133427));
#36131=CARTESIAN_POINT('Ctrl Pts',(-4.23351725580547,0.794772684000396,
8.84812274771854));
#36132=CARTESIAN_POINT('Ctrl Pts',(-4.32465269180564,1.06847604194463,8.8987984096838));
#36133=CARTESIAN_POINT('Ctrl Pts',(-4.36805402374264,1.18514270861135,8.92146825773577));
#36134=CARTESIAN_POINT('Ctrl Pts',(-4.41540753427286,1.29999999999962,8.94487233749329));
#36135=CARTESIAN_POINT('Ctrl Pts',(-4.46225757065984,-1.30000000000127,
8.71958453597259));
#36136=CARTESIAN_POINT('Ctrl Pts',(-4.4025506934583,-1.18514270861251,8.71060091650708));
#36137=CARTESIAN_POINT('Ctrl Pts',(-4.34809231889145,-1.06847604194528,
8.70388865690302));
#36138=CARTESIAN_POINT('Ctrl Pts',(-4.23440767032736,-0.794772684000507,
8.69362929009866));
#36139=CARTESIAN_POINT('Ctrl Pts',(-4.17214331313643,-0.63630980009492,
8.69166805282642));
#36140=CARTESIAN_POINT('Ctrl Pts',(-4.09424342713997,-0.31943490727702,
8.69563909448733));
#36141=CARTESIAN_POINT('Ctrl Pts',(-4.06586783821613,-0.158333333333263,
8.69949510324146));
#36142=CARTESIAN_POINT('Ctrl Pts',(-4.05786199444834,0.158333333333265,
8.72157248282735));
#36143=CARTESIAN_POINT('Ctrl Pts',(-4.07874176403268,0.319434907277027,
8.73856548687397));
#36144=CARTESIAN_POINT('Ctrl Pts',(-4.13929543967664,0.636309800094928,
8.78206657250136));
#36145=CARTESIAN_POINT('Ctrl Pts',(-4.19139502078103,0.794772684000495,
8.81130446539696));
#36146=CARTESIAN_POINT('Ctrl Pts',(-4.28896174323994,1.06847604194477,8.86567732901192));
#36147=CARTESIAN_POINT('Ctrl Pts',(-4.3365817094158,1.1851427086115,8.89121162387947));
#36148=CARTESIAN_POINT('Ctrl Pts',(-4.38958862281842,1.29999999999979,8.91874421566881));
#36149=CARTESIAN_POINT('Ctrl Pts',(-4.43911310247445,-1.30000000000157,
8.70074230118706));
#36150=CARTESIAN_POINT('Ctrl Pts',(-4.37448267385302,-1.18514270861279,
8.6889702543753));
#36151=CARTESIAN_POINT('Ctrl Pts',(-4.31635227442594,-1.06847604194553,
8.6803703284716));
#36152=CARTESIAN_POINT('Ctrl Pts',(-4.19707579056849,-0.794772684000693,
8.66783101310304));
#36153=CARTESIAN_POINT('Ctrl Pts',(-4.13529783701336,-0.636309800095066,
8.66733511322863));
#36154=CARTESIAN_POINT('Ctrl Pts',(-4.05664387112888,-0.319434907277092,
8.67245999763365));
#36155=CARTESIAN_POINT('Ctrl Pts',(-4.02921254050706,-0.158333333333299,
8.67863830460936));
#36156=CARTESIAN_POINT('Ctrl Pts',(-4.02140348472796,0.158333333333302,
8.70020161040361));
#36157=CARTESIAN_POINT('Ctrl Pts',(-4.04130261769599,0.319434907277102,
8.7147047681238));
#36158=CARTESIAN_POINT('Ctrl Pts',(-4.10348615916234,0.636309800095076,
8.7552990318348));
#36159=CARTESIAN_POINT('Ctrl Pts',(-4.15653007774043,0.794772684000676,
8.7804454628435));
#36160=CARTESIAN_POINT('Ctrl Pts',(-4.26006427161474,1.06847604194501,8.83661089969961));
#36161=CARTESIAN_POINT('Ctrl Pts',(-4.31123720445708,1.18514270861177,8.86439776995298));
#36162=CARTESIAN_POINT('Ctrl Pts',(-4.36876695393351,1.30000000000009,8.89565957397926));
#36163=CARTESIAN_POINT('Ctrl Pts',(-4.42075431675889,-1.30000000000158,
8.68521657502598));
#36164=CARTESIAN_POINT('Ctrl Pts',(-4.35219808770137,-1.18514270861279,
8.6710538738467));
#36165=CARTESIAN_POINT('Ctrl Pts',(-4.29106007738977,-1.06847604194554,
8.66099953632976));
#36166=CARTESIAN_POINT('Ctrl Pts',(-4.16695661226589,-0.794772684000697,
8.64726314723766));
#36167=CARTESIAN_POINT('Ctrl Pts',(-4.10471537309693,-0.636309800095071,
8.64981620211422));
#36168=CARTESIAN_POINT('Ctrl Pts',(-4.02550494520748,-0.319434907277095,
8.65575584817436));
#36169=CARTESIAN_POINT('Ctrl Pts',(-3.99977596517424,-0.158333333333301,
8.6617818347337));
#36170=CARTESIAN_POINT('Ctrl Pts',(-3.99236947390528,0.158333333333303,
8.68238426965024));
#36171=CARTESIAN_POINT('Ctrl Pts',(-4.01124821738469,0.319434907277104,
8.69539919887263));
#36172=CARTESIAN_POINT('Ctrl Pts',(-4.07423910504128,0.63630980009508,8.73460593135742));
#36173=CARTESIAN_POINT('Ctrl Pts',(-4.12728445891231,0.794772684000685,
8.75782848948147));
#36174=CARTESIAN_POINT('Ctrl Pts',(-4.23532127633879,1.06847604194502,8.81604471656162));
#36175=CARTESIAN_POINT('Ctrl Pts',(-4.28935485892354,1.18514270861178,8.84568172449774));
#36176=CARTESIAN_POINT('Ctrl Pts',(-4.35065688898772,1.30000000000009,8.87975609279077));
#36177=CARTESIAN_POINT('Ctrl Pts',(-4.40659708526905,-1.30000000000166,
8.67446878376005));
#36178=CARTESIAN_POINT('Ctrl Pts',(-4.33500103708209,-1.18514270861287,
8.65885991086501));
#36179=CARTESIAN_POINT('Ctrl Pts',(-4.27159398066144,-1.0684760419456,8.64785577527442));
#36180=CARTESIAN_POINT('Ctrl Pts',(-4.1440292049743,-0.794772684000745,
8.6330718850382));
#36181=CARTESIAN_POINT('Ctrl Pts',(-4.0820895603583,-0.63630980009511,8.63655403448564));
#36182=CARTESIAN_POINT('Ctrl Pts',(-4.00237175737431,-0.319434907277115,
8.643356071981));
#36183=CARTESIAN_POINT('Ctrl Pts',(-3.97716150569709,-0.15833333333331,
8.65088312043462));
#36184=CARTESIAN_POINT('Ctrl Pts',(-3.96985075878325,0.158333333333313,
8.67118698661727));
#36185=CARTESIAN_POINT('Ctrl Pts',(-3.98820168570649,0.319434907277123,
8.68254269792091));
#36186=CARTESIAN_POINT('Ctrl Pts',(-4.05210850918212,0.636309800095118,
8.7199928653782));
#36187=CARTESIAN_POINT('Ctrl Pts',(-4.10541687631528,0.794772684000733,
8.74119421122248));
#36188=CARTESIAN_POINT('Ctrl Pts',(-4.21724916319844,1.06847604194508,8.79997976559179));
#36189=CARTESIAN_POINT('Ctrl Pts',(-4.2736200148387,1.18514270861185,8.83055472465665));
#36190=CARTESIAN_POINT('Ctrl Pts',(-4.33795366492212,1.30000000000017,8.86625855451932));
#36191=CARTESIAN_POINT('Ctrl Pts',(-4.39232901724014,-1.3000000000017,8.66375480980727));
#36192=CARTESIAN_POINT('Ctrl Pts',(-4.31766672800015,-1.1851427086129,8.64639229265701));
#36193=CARTESIAN_POINT('Ctrl Pts',(-4.25188946484526,-1.06847604194564,
8.63438908801193));
#36194=CARTESIAN_POINT('Ctrl Pts',(-4.12045701596139,-0.79477268400077,
8.61904036806275));
#36195=CARTESIAN_POINT('Ctrl Pts',(-4.05774099367921,-0.636309800095132,
8.62588706975922));
#36196=CARTESIAN_POINT('Ctrl Pts',(-3.97797184968243,-0.319434907277126,
8.63245483859954));
#36197=CARTESIAN_POINT('Ctrl Pts',(-3.95519739470823,-0.158333333333316,
8.63725925921173));
#36198=CARTESIAN_POINT('Ctrl Pts',(-3.94834123033963,0.158333333333319,
8.65644217709915));
#36199=CARTESIAN_POINT('Ctrl Pts',(-3.96498865647832,0.319434907277135,
8.66867953880038));
#36200=CARTESIAN_POINT('Ctrl Pts',(-4.02930709073509,0.636309800095142,
8.70554733147818));
#36201=CARTESIAN_POINT('Ctrl Pts',(-4.0829650466866,0.794772684000761,8.72454112670396));
#36202=CARTESIAN_POINT('Ctrl Pts',(-4.19848477060446,1.06847604194512,8.78448064229685));
#36203=CARTESIAN_POINT('Ctrl Pts',(-4.25715537491875,1.18514270861189,8.81629550060161));
#36204=CARTESIAN_POINT('Ctrl Pts',(-4.32449237549088,1.30000000000022,8.85397962188891));
#36205=CARTESIAN_POINT('Ctrl Pts',(-4.38055136998851,-1.30000000000175,
8.65486034483293));
#36206=CARTESIAN_POINT('Ctrl Pts',(-4.30314549901928,-1.18514270861294,
8.63701984983662));
#36207=CARTESIAN_POINT('Ctrl Pts',(-4.23545078584017,-1.06847604194568,
8.62448447136143));
#36208=CARTESIAN_POINT('Ctrl Pts',(-4.10149717332144,-0.794772684000798,
8.60778111983862));
#36209=CARTESIAN_POINT('Ctrl Pts',(-4.0400134261722,-0.636309800095152,
8.61321666597366));
#36210=CARTESIAN_POINT('Ctrl Pts',(-3.96056350920759,-0.319434907277135,
8.61898989843895));
#36211=CARTESIAN_POINT('Ctrl Pts',(-3.93872539640991,-0.158333333333321,
8.62400320920415));
#36212=CARTESIAN_POINT('Ctrl Pts',(-3.93159547877079,0.158333333333323,
8.64375728571561));
#36213=CARTESIAN_POINT('Ctrl Pts',(-3.94664076546426,0.319434907277145,
8.65721696059045));
#36214=CARTESIAN_POINT('Ctrl Pts',(-4.01088092238389,0.636309800095162,
8.6942908495018));
#36215=CARTESIAN_POINT('Ctrl Pts',(-4.06467681579459,0.794772684000785,
8.71158207420152));
#36216=CARTESIAN_POINT('Ctrl Pts',(-4.18296403816074,1.06847604194515,8.77241849605042));
#36217=CARTESIAN_POINT('Ctrl Pts',(-4.24342309250851,1.18514270861193,8.80512936980167));
#36218=CARTESIAN_POINT('Ctrl Pts',(-4.31313904561529,1.30000000000026,8.84421728449737));
#36219=CARTESIAN_POINT('Ctrl Pts',(-4.36598120515593,-1.30000000000177,
8.64481132314811));
#36220=CARTESIAN_POINT('Ctrl Pts',(-4.28494496219392,-1.18514270861297,
8.62620935511287));
#36221=CARTESIAN_POINT('Ctrl Pts',(-4.2147464284803,-1.06847604194569,8.61273308884697));
#36222=CARTESIAN_POINT('Ctrl Pts',(-4.07761104887375,-0.794772684000812,
8.59344161433524));
#36223=CARTESIAN_POINT('Ctrl Pts',(-4.01795641242019,-0.636309800095164,
8.5960638488432));
#36224=CARTESIAN_POINT('Ctrl Pts',(-3.93922052986902,-0.319434907277142,
8.59978175807134));
#36225=CARTESIAN_POINT('Ctrl Pts',(-3.91872281830903,-0.158333333333324,
8.60487133018024));
#36226=CARTESIAN_POINT('Ctrl Pts',(-3.91162073886137,0.158333333333326,
8.62450764463315));
#36227=CARTESIAN_POINT('Ctrl Pts',(-3.925211094291,0.319434907277151,8.63805118402258));
#36228=CARTESIAN_POINT('Ctrl Pts',(-3.98908391499714,0.636309800095174,
8.6763744856589));
#36229=CARTESIAN_POINT('Ctrl Pts',(-4.04179842596812,0.7947726840008,8.69483225573699));
#36230=CARTESIAN_POINT('Ctrl Pts',(-4.16338112100733,1.06847604194518,8.75813315058748));
#36231=CARTESIAN_POINT('Ctrl Pts',(-4.22623879415762,1.18514270861196,8.79210358693433));
#36232=CARTESIAN_POINT('Ctrl Pts',(-4.29932549685856,1.30000000000029,8.83264384777654));
#36233=CARTESIAN_POINT('Ctrl Pts',(-4.3561014276295,-1.30000000000184,8.63787852952414));
#36234=CARTESIAN_POINT('Ctrl Pts',(-4.27202510729764,-1.18514270861303,
8.62000938470732));
#36235=CARTESIAN_POINT('Ctrl Pts',(-4.19998727434634,-1.06847604194575,
8.60640446368449));
#36236=CARTESIAN_POINT('Ctrl Pts',(-4.06137678325034,-0.794772684000851,
8.58482558448585));
#36237=CARTESIAN_POINT('Ctrl Pts',(-4.00531418533707,-0.636309800095196,
8.58193800807906));
#36238=CARTESIAN_POINT('Ctrl Pts',(-3.92838285750872,-0.319434907277159,
8.58266762339361));
#36239=CARTESIAN_POINT('Ctrl Pts',(-3.90875262161207,-0.158333333333332,
8.58839155927254));
#36240=CARTESIAN_POINT('Ctrl Pts',(-3.90175138030431,0.158333333333335,
8.60789341044225));
#36241=CARTESIAN_POINT('Ctrl Pts',(-3.91457783688431,0.319434907277167,
8.62081822042886));
#36242=CARTESIAN_POINT('Ctrl Pts',(-3.97684592441674,0.636309800095206,
8.66155018584608));
#36243=CARTESIAN_POINT('Ctrl Pts',(-4.02617203613903,0.794772684000841,
8.68440863390959));
#36244=CARTESIAN_POINT('Ctrl Pts',(-4.14921392208312,1.06847604194523,8.75005834839344));
#36245=CARTESIAN_POINT('Ctrl Pts',(-4.2138412015471,1.18514270861202,8.78447021792653));
#36246=CARTESIAN_POINT('Ctrl Pts',(-4.28983548720103,1.30000000000035,8.82487662815433));
#36247=CARTESIAN_POINT('Ctrl Pts',(-4.35088387761181,-1.30000000000184,
8.63103946714464));
#36248=CARTESIAN_POINT('Ctrl Pts',(-4.26698198886935,-1.18514270861303,
8.61335123634859));
#36249=CARTESIAN_POINT('Ctrl Pts',(-4.19526082558524,-1.06847604194575,
8.59960976409458));
#36250=CARTESIAN_POINT('Ctrl Pts',(-4.05771050318435,-0.794772684000851,
8.5769820159942));
#36251=CARTESIAN_POINT('Ctrl Pts',(-4.00307751336492,-0.636309800095196,
8.57196388006084));
#36252=CARTESIAN_POINT('Ctrl Pts',(-3.9271390295546,-0.319434907277159,
8.57133011076225));
#36253=CARTESIAN_POINT('Ctrl Pts',(-3.90745678965039,-0.158333333333332,
8.5770480695384));
#36254=CARTESIAN_POINT('Ctrl Pts',(-3.90061191119441,0.158333333333335,
8.59637205061778));
#36255=CARTESIAN_POINT('Ctrl Pts',(-3.91380906647831,0.319434907277167,
8.60889674750867));
#36256=CARTESIAN_POINT('Ctrl Pts',(-3.9750721515842,0.636309800095206,8.65109465690008));
#36257=CARTESIAN_POINT('Ctrl Pts',(-4.02239198166674,0.794772684000841,
8.67700128450958));
#36258=CARTESIAN_POINT('Ctrl Pts',(-4.14444540563293,1.06847604194523,8.74356402580408));
#36259=CARTESIAN_POINT('Ctrl Pts',(-4.20891602829553,1.18514270861202,8.77783540490947));
#36260=CARTESIAN_POINT('Ctrl Pts',(-4.28502486891082,1.30000000000035,8.8175656188065));
#36261=CARTESIAN_POINT('Ctrl Pts',(-4.35088387761047,-1.3,8.63103946714436));
#36262=CARTESIAN_POINT('Ctrl Pts',(-4.26698198886859,-1.18514270861178,
8.61335123634844));
#36263=CARTESIAN_POINT('Ctrl Pts',(-4.19526082558493,-1.06847604194512,
8.59960976409452));
#36264=CARTESIAN_POINT('Ctrl Pts',(-4.05771050318435,-0.794772684000851,
8.5769820159942));
#36265=CARTESIAN_POINT('Ctrl Pts',(-4.00307751336492,-0.636309800095197,
8.57196388006084));
#36266=CARTESIAN_POINT('Ctrl Pts',(-3.9271390295546,-0.319434907277159,
8.57133011076224));
#36267=CARTESIAN_POINT('Ctrl Pts',(-3.90745678965039,-0.158333333333332,
8.5770480695384));
#36268=CARTESIAN_POINT('Ctrl Pts',(-3.90061191119441,0.158333333333334,
8.59637205061778));
#36269=CARTESIAN_POINT('Ctrl Pts',(-3.91380906647831,0.319434907277167,
8.60889674750867));
#36270=CARTESIAN_POINT('Ctrl Pts',(-3.9750721515842,0.636309800095206,8.65109465690008));
#36271=CARTESIAN_POINT('Ctrl Pts',(-4.02239198166674,0.79477268400084,8.67700128450958));
#36272=CARTESIAN_POINT('Ctrl Pts',(-4.14444540563287,1.06847604194511,8.74356402580405));
#36273=CARTESIAN_POINT('Ctrl Pts',(-4.20891602829539,1.18514270861178,8.7778354049094));
#36274=CARTESIAN_POINT('Ctrl Pts',(-4.28502486891058,1.3,8.81756561880638));
#36275=CARTESIAN_POINT('',(-4.63723388560792,-1.2,8.93163561125591));
#36276=CARTESIAN_POINT('Ctrl Pts',(-4.63723388560792,-1.2,8.93163561125591));
#36277=CARTESIAN_POINT('Ctrl Pts',(-4.62753389439639,-1.21478802097806,
8.91533912501957));
#36278=CARTESIAN_POINT('Ctrl Pts',(-4.62697861968183,-1.21593888768291,
8.91350422791788));
#36279=CARTESIAN_POINT('Ctrl Pts',(-4.61456982759609,-1.23519182817029,
8.89149335283502));
#36280=CARTESIAN_POINT('Ctrl Pts',(-4.61325995412872,-1.23709049084105,
8.88956307144032));
#36281=CARTESIAN_POINT('Ctrl Pts',(-4.59898272268779,-1.25866691551418,
8.86569698934375));
#36282=CARTESIAN_POINT('Ctrl Pts',(-4.59362321232696,-1.26678758340789,
8.85663230638542));
#36283=CARTESIAN_POINT('Ctrl Pts',(-4.58386363196318,-1.28145275507162,
8.84041978907459));
#36284=CARTESIAN_POINT('Ctrl Pts',(-4.57687058714458,-1.29190031914763,
8.82892890064751));
#36285=CARTESIAN_POINT('Ctrl Pts',(-4.5724258367586,-1.29846636104134,8.82182026882674));
#36286=CARTESIAN_POINT('Ctrl Pts',(-4.57190495076468,-1.29923376230637,
8.82099308234304));
#36287=CARTESIAN_POINT('Ctrl Pts',(-4.57138290900173,-1.30000000000056,
8.82017230542972));
#36288=CARTESIAN_POINT('',(-4.58017336249762,-0.653834841416747,9.07736836268454));
#36289=CARTESIAN_POINT('Ctrl Pts',(-4.5801733625228,-0.653834841416062,
9.07736836269194));
#36290=CARTESIAN_POINT('Ctrl Pts',(-4.58634132012241,-0.717928704880547,
9.06232053528613));
#36291=CARTESIAN_POINT('Ctrl Pts',(-4.59131394979481,-0.763797028297237,
9.05003100375446));
#36292=CARTESIAN_POINT('Ctrl Pts',(-4.61052464146469,-0.949538109615673,
9.00188729361407));
#36293=CARTESIAN_POINT('Ctrl Pts',(-4.62075787424104,-1.04843725126253,
8.97575754875452));
#36294=CARTESIAN_POINT('Ctrl Pts',(-4.63723388560792,-1.2,8.93163561125591));
#36295=CARTESIAN_POINT('',(-4.52544944337419,0.653834841531101,9.20569372922794));
#36296=CARTESIAN_POINT('Ctrl Pts',(-4.52544944337418,0.653834841531102,
9.20569372922795));
#36297=CARTESIAN_POINT('Ctrl Pts',(-4.49800477099097,0.575791366845458,
9.1743322544575));
#36298=CARTESIAN_POINT('Ctrl Pts',(-4.47552136690656,0.493917914177405,
9.14760173032986));
#36299=CARTESIAN_POINT('Ctrl Pts',(-4.44488215025619,0.338198323071554,
9.10721680052762));
#36300=CARTESIAN_POINT('Ctrl Pts',(-4.43508703909453,0.265710276728555,
9.0922158274664));
#36301=CARTESIAN_POINT('Ctrl Pts',(-4.42552808798967,0.129738884446912,
9.06975255594665));
#36302=CARTESIAN_POINT('Ctrl Pts',(-4.4244963582949,0.0666402419227446,
9.06153246854483));
#36303=CARTESIAN_POINT('Ctrl Pts',(-4.42938618481451,-0.0595493706457138,
9.04911769727901));
#36304=CARTESIAN_POINT('Ctrl Pts',(-4.43532950520763,-0.122795525062026,
9.04482175652539));
#36305=CARTESIAN_POINT('Ctrl Pts',(-4.45563401062421,-0.260143259403432,
9.04056858786434));
#36306=CARTESIAN_POINT('Ctrl Pts',(-4.47133340707415,-0.333940698349591,
9.04154200493254));
#36307=CARTESIAN_POINT('Ctrl Pts',(-4.51502088722612,-0.49122835763458,
9.05169607394797));
#36308=CARTESIAN_POINT('Ctrl Pts',(-4.54472679166538,-0.574163474744005,
9.06210644021376));
#36309=CARTESIAN_POINT('Ctrl Pts',(-4.5801733624882,-0.653834841428463,
9.07736836264527));
#36310=CARTESIAN_POINT('',(-4.55421084628694,1.2,9.1395008552621));
#36311=CARTESIAN_POINT('Ctrl Pts',(-4.55421084628694,1.2,9.1395008552621));
#36312=CARTESIAN_POINT('Ctrl Pts',(-4.54938195732035,1.13478776924219,9.15083974095914));
#36313=CARTESIAN_POINT('Ctrl Pts',(-4.54293098542071,1.03871837843732,9.16586603442479));
#36314=CARTESIAN_POINT('Ctrl Pts',(-4.5301428206211,0.795010067313144,9.19511397277935));
#36315=CARTESIAN_POINT('Ctrl Pts',(-4.52811399206583,0.741769803333558,
9.1996817044518));
#36316=CARTESIAN_POINT('Ctrl Pts',(-4.52544944337418,0.653834841531102,
9.20569372922794));
#36317=CARTESIAN_POINT('Ctrl Pts',(-4.49082727704437,1.29999999999907,9.03165781950759));
#36318=CARTESIAN_POINT('Ctrl Pts',(-4.50187711672958,1.28314156068347,9.04920504305177));
#36319=CARTESIAN_POINT('Ctrl Pts',(-4.51232625581989,1.26655442348624,9.06737950428502));
#36320=CARTESIAN_POINT('Ctrl Pts',(-4.53007724292771,1.23873360654381,9.09710440627825));
#36321=CARTESIAN_POINT('Ctrl Pts',(-4.54264069501209,1.21921921678529,9.1176177947092));
#36322=CARTESIAN_POINT('Ctrl Pts',(-4.55421084628694,1.2,9.1395008552621));
#36323=CARTESIAN_POINT('Ctrl Pts',(-4.35088387761047,-1.3,8.63103946714436));
#36324=CARTESIAN_POINT('Ctrl Pts',(-4.26698198886859,-1.18514270861178,
8.61335123634844));
#36325=CARTESIAN_POINT('Ctrl Pts',(-4.19526082558493,-1.06847604194512,
8.59960976409452));
#36326=CARTESIAN_POINT('Ctrl Pts',(-4.05771050318435,-0.794772684000851,
8.5769820159942));
#36327=CARTESIAN_POINT('Ctrl Pts',(-4.00307751336492,-0.636309800095196,
8.57196388006084));
#36328=CARTESIAN_POINT('Ctrl Pts',(-3.9271390295546,-0.319434907277158,
8.57133011076224));
#36329=CARTESIAN_POINT('Ctrl Pts',(-3.90745678965039,-0.158333333333332,
8.57704806953839));
#36330=CARTESIAN_POINT('Ctrl Pts',(-3.90061191119441,0.158333333333335,
8.59637205061778));
#36331=CARTESIAN_POINT('Ctrl Pts',(-3.91380906647831,0.319434907277167,
8.60889674750866));
#36332=CARTESIAN_POINT('Ctrl Pts',(-3.9750721515842,0.636309800095206,8.65109465690008));
#36333=CARTESIAN_POINT('Ctrl Pts',(-4.02239198166674,0.794772684000841,
8.67700128450958));
#36334=CARTESIAN_POINT('Ctrl Pts',(-4.14444540563287,1.06847604194511,8.74356402580405));
#36335=CARTESIAN_POINT('Ctrl Pts',(-4.20891602829539,1.18514270861178,8.7778354049094));
#36336=CARTESIAN_POINT('Ctrl Pts',(-4.28502486891058,1.3,8.81756561880638));
#36337=CARTESIAN_POINT('Ctrl Pts',(-4.37306897027954,-1.3,8.55737176093662));
#36338=CARTESIAN_POINT('Ctrl Pts',(-4.28882565135864,-1.18514270861178,
8.54138186178938));
#36339=CARTESIAN_POINT('Ctrl Pts',(-4.21691086230761,-1.06847604194512,
8.52883129592335));
#36340=CARTESIAN_POINT('Ctrl Pts',(-4.0792546834088,-0.794772684000851,
8.50778252595658));
#36341=CARTESIAN_POINT('Ctrl Pts',(-4.02499599674477,-0.636309800095196,
8.50215210324751));
#36342=CARTESIAN_POINT('Ctrl Pts',(-3.94958161227244,-0.319434907277158,
8.5011060196783));
#36343=CARTESIAN_POINT('Ctrl Pts',(-3.93044726732831,-0.158333333333332,
8.50570985865775));
#36344=CARTESIAN_POINT('Ctrl Pts',(-3.92394377232475,0.158333333333335,
8.52514476194479));
#36345=CARTESIAN_POINT('Ctrl Pts',(-3.93692932075669,0.319434907277167,
8.53889284526232));
#36346=CARTESIAN_POINT('Ctrl Pts',(-3.99837405888618,0.636309800095206,
8.58173238176729));
#36347=CARTESIAN_POINT('Ctrl Pts',(-4.04563681344556,0.794772684000841,
8.6083543696584));
#36348=CARTESIAN_POINT('Ctrl Pts',(-4.16853269776624,1.06847604194511,8.67357746992056));
#36349=CARTESIAN_POINT('Ctrl Pts',(-4.23354667110408,1.18514270861178,8.70677157514888));
#36350=CARTESIAN_POINT('Ctrl Pts',(-4.31037754319865,1.3,8.74492712225608));
#36351=CARTESIAN_POINT('Ctrl Pts',(-4.39525406294861,-1.3,8.48370405472888));
#36352=CARTESIAN_POINT('Ctrl Pts',(-4.3106693138487,-1.18514270861178,8.46941248723032));
#36353=CARTESIAN_POINT('Ctrl Pts',(-4.2385608990303,-1.06847604194512,8.45805282775218));
#36354=CARTESIAN_POINT('Ctrl Pts',(-4.10079886363325,-0.794772684000851,
8.43858303591895));
#36355=CARTESIAN_POINT('Ctrl Pts',(-4.04691448012462,-0.636309800095196,
8.43234032643418));
#36356=CARTESIAN_POINT('Ctrl Pts',(-3.97202419499028,-0.319434907277158,
8.43088192859436));
#36357=CARTESIAN_POINT('Ctrl Pts',(-3.95343774500623,-0.158333333333332,
8.4343716477771));
#36358=CARTESIAN_POINT('Ctrl Pts',(-3.94727563345509,0.158333333333335,
8.4539174732718));
#36359=CARTESIAN_POINT('Ctrl Pts',(-3.96004957503508,0.319434907277167,
8.46888894301597));
#36360=CARTESIAN_POINT('Ctrl Pts',(-4.02167596618816,0.636309800095206,
8.5123701066345));
#36361=CARTESIAN_POINT('Ctrl Pts',(-4.06888164522438,0.794772684000841,
8.53970745480722));
#36362=CARTESIAN_POINT('Ctrl Pts',(-4.19261998989962,1.06847604194511,8.60359091403707));
#36363=CARTESIAN_POINT('Ctrl Pts',(-4.25817731391276,1.18514270861178,8.63570774538835));
#36364=CARTESIAN_POINT('Ctrl Pts',(-4.33573021748671,1.3,8.67228862570577));
#36365=CARTESIAN_POINT('Ctrl Pts',(-4.41743915561768,-1.3,8.41003634852114));
#36366=CARTESIAN_POINT('Ctrl Pts',(-4.33251297633875,-1.18514270861178,
8.39744311267125));
#36367=CARTESIAN_POINT('Ctrl Pts',(-4.26021093575299,-1.06847604194512,
8.38727435958101));
#36368=CARTESIAN_POINT('Ctrl Pts',(-4.12234304385769,-0.794772684000851,
8.36938354588133));
#36369=CARTESIAN_POINT('Ctrl Pts',(-4.06883296350448,-0.636309800095196,
8.36252854962085));
#36370=CARTESIAN_POINT('Ctrl Pts',(-3.99446677770812,-0.319434907277158,
8.36065783751042));
#36371=CARTESIAN_POINT('Ctrl Pts',(-3.97642822268415,-0.158333333333332,
8.36303343689645));
#36372=CARTESIAN_POINT('Ctrl Pts',(-3.97060749458543,0.158333333333335,
8.38269018459881));
#36373=CARTESIAN_POINT('Ctrl Pts',(-3.98316982931346,0.319434907277167,
8.39888504076963));
#36374=CARTESIAN_POINT('Ctrl Pts',(-4.04497787349015,0.636309800095206,
8.44300783150171));
#36375=CARTESIAN_POINT('Ctrl Pts',(-4.0921264770032,0.794772684000841,8.47106053995604));
#36376=CARTESIAN_POINT('Ctrl Pts',(-4.21670728203299,1.06847604194511,8.53360435815359));
#36377=CARTESIAN_POINT('Ctrl Pts',(-4.28280795672145,1.18514270861178,8.56464391562783));
#36378=CARTESIAN_POINT('Ctrl Pts',(-4.36108289177478,1.3,8.59965012915547));
#36379=CARTESIAN_POINT('Ctrl Pts',(-4.41743915561768,-1.3,8.41003634852114));
#36380=CARTESIAN_POINT('Ctrl Pts',(-4.33251297633875,-1.18514270861178,
8.39744311267125));
#36381=CARTESIAN_POINT('Ctrl Pts',(-4.26021093575299,-1.06847604194512,
8.38727435958101));
#36382=CARTESIAN_POINT('Ctrl Pts',(-4.12234304385769,-0.794772684000851,
8.36938354588133));
#36383=CARTESIAN_POINT('Ctrl Pts',(-4.06883296350448,-0.636309800095197,
8.36252854962085));
#36384=CARTESIAN_POINT('Ctrl Pts',(-3.99446677770812,-0.319434907277159,
8.36065783751042));
#36385=CARTESIAN_POINT('Ctrl Pts',(-3.97642822268415,-0.158333333333332,
8.36303343689645));
#36386=CARTESIAN_POINT('Ctrl Pts',(-3.97060749458543,0.158333333333334,
8.38269018459881));
#36387=CARTESIAN_POINT('Ctrl Pts',(-3.98316982931346,0.319434907277167,
8.39888504076963));
#36388=CARTESIAN_POINT('Ctrl Pts',(-4.04497787349014,0.636309800095206,
8.44300783150171));
#36389=CARTESIAN_POINT('Ctrl Pts',(-4.0921264770032,0.79477268400084,8.47106053995604));
#36390=CARTESIAN_POINT('Ctrl Pts',(-4.21670728203298,1.06847604194511,8.53360435815359));
#36391=CARTESIAN_POINT('Ctrl Pts',(-4.28280795672145,1.18514270861178,8.56464391562783));
#36392=CARTESIAN_POINT('Ctrl Pts',(-4.36108289177478,1.3,8.59965012915547));
#36393=CARTESIAN_POINT('Ctrl Pts',(-4.41743915562091,-1.30000000000437,
8.41003634852161));
#36394=CARTESIAN_POINT('Ctrl Pts',(-4.33251297634058,-1.18514270861474,
8.39744311267151));
#36395=CARTESIAN_POINT('Ctrl Pts',(-4.26021093575375,-1.06847604194662,
8.38727435958111));
#36396=CARTESIAN_POINT('Ctrl Pts',(-4.12234304385769,-0.794772684000851,
8.36938354588133));
#36397=CARTESIAN_POINT('Ctrl Pts',(-4.06883296350448,-0.636309800095197,
8.36252854962085));
#36398=CARTESIAN_POINT('Ctrl Pts',(-3.99446677770812,-0.319434907277159,
8.36065783751042));
#36399=CARTESIAN_POINT('Ctrl Pts',(-3.97642822268415,-0.158333333333332,
8.36303343689645));
#36400=CARTESIAN_POINT('Ctrl Pts',(-3.97060749458543,0.158333333333334,
8.38269018459881));
#36401=CARTESIAN_POINT('Ctrl Pts',(-3.98316982931346,0.319434907277167,
8.39888504076963));
#36402=CARTESIAN_POINT('Ctrl Pts',(-4.04497787349015,0.636309800095206,
8.44300783150171));
#36403=CARTESIAN_POINT('Ctrl Pts',(-4.0921264770032,0.79477268400084,8.47106053995604));
#36404=CARTESIAN_POINT('Ctrl Pts',(-4.21670728203318,1.06847604194555,8.53360435815368));
#36405=CARTESIAN_POINT('Ctrl Pts',(-4.28280795672194,1.18514270861264,8.56464391562806));
#36406=CARTESIAN_POINT('Ctrl Pts',(-4.36108289177564,1.30000000000127,8.59965012915586));
#36407=CARTESIAN_POINT('Ctrl Pts',(-4.42289860586574,-1.30000000000437,
8.40797826829483));
#36408=CARTESIAN_POINT('Ctrl Pts',(-4.33776923904344,-1.18514270861474,
8.39579462447261));
#36409=CARTESIAN_POINT('Ctrl Pts',(-4.26532765431604,-1.06847604194662,
8.3856402571071));
#36410=CARTESIAN_POINT('Ctrl Pts',(-4.12728441652869,-0.794772684000851,
8.36686967168899));
#36411=CARTESIAN_POINT('Ctrl Pts',(-4.0738867088757,-0.636309800095197,
8.35758448088744));
#36412=CARTESIAN_POINT('Ctrl Pts',(-3.99955292053485,-0.319434907277159,
8.35452930264375));
#36413=CARTESIAN_POINT('Ctrl Pts',(-3.98155751278828,-0.158333333333332,
8.35726596170137));
#36414=CARTESIAN_POINT('Ctrl Pts',(-3.97575141855083,0.158333333333334,
8.37707991454073));
#36415=CARTESIAN_POINT('Ctrl Pts',(-3.98828336306808,0.319434907277167,
8.39325761631741));
#36416=CARTESIAN_POINT('Ctrl Pts',(-4.05009264080661,0.636309800095206,
8.43850479398448));
#36417=CARTESIAN_POINT('Ctrl Pts',(-4.0971774214965,0.79477268400084,8.46826681004936));
#36418=CARTESIAN_POINT('Ctrl Pts',(-4.2219190164042,1.06847604194555,8.53179176443982));
#36419=CARTESIAN_POINT('Ctrl Pts',(-4.28813697665279,1.18514270861264,8.56302905926473));
#36420=CARTESIAN_POINT('Ctrl Pts',(-4.36657688284595,1.30000000000127,8.59800604999041));
#36421=CARTESIAN_POINT('Ctrl Pts',(-4.43168171124751,-1.30000000000412,
8.40635777334216));
#36422=CARTESIAN_POINT('Ctrl Pts',(-4.34743550989965,-1.18514270861451,
8.39517850942592));
#36423=CARTESIAN_POINT('Ctrl Pts',(-4.27565255026722,-1.06847604194641,
8.38531825593481));
#36424=CARTESIAN_POINT('Ctrl Pts',(-4.13861213501102,-0.794772684000699,
8.36558627578272));
#36425=CARTESIAN_POINT('Ctrl Pts',(-4.08517130083353,-0.636309800095075,
8.35251835237303));
#36426=CARTESIAN_POINT('Ctrl Pts',(-4.01088514461499,-0.319434907277098,
8.34756649540242));
#36427=CARTESIAN_POINT('Ctrl Pts',(-3.99249114174688,-0.158333333333302,
8.35057250956555));
#36428=CARTESIAN_POINT('Ctrl Pts',(-3.98668829928627,0.158333333333304,
8.37058162387864));
#36429=CARTESIAN_POINT('Ctrl Pts',(-3.99965319507378,0.319434907277107,
8.38677599326486));
#36430=CARTESIAN_POINT('Ctrl Pts',(-4.06135810695932,0.636309800095085,
8.43413230172235));
#36431=CARTESIAN_POINT('Ctrl Pts',(-4.10832680843737,0.794772684000687,
8.46757637384159));
#36432=CARTESIAN_POINT('Ctrl Pts',(-4.23206754042395,1.06847604194534,8.53210485181926));
#36433=CARTESIAN_POINT('Ctrl Pts',(-4.29766467805669,1.18514270861241,8.56307409624329));
#36434=CARTESIAN_POINT('Ctrl Pts',(-4.37529617549109,1.30000000000103,8.59708059799053));
#36435=CARTESIAN_POINT('Ctrl Pts',(-4.44386598093114,-1.30000000000411,
8.40580624828163));
#36436=CARTESIAN_POINT('Ctrl Pts',(-4.36209777541527,-1.1851427086145,8.39590606023192));
#36437=CARTESIAN_POINT('Ctrl Pts',(-4.29216674290469,-1.0684760419464,8.38656864163037));
#36438=CARTESIAN_POINT('Ctrl Pts',(-4.15795830581166,-0.794772684000692,
8.36629744672359));
#36439=CARTESIAN_POINT('Ctrl Pts',(-4.1043911877798,-0.636309800095068,
8.34972927827051));
#36440=CARTESIAN_POINT('Ctrl Pts',(-4.0303296578903,-0.319434907277094,
8.34280141108802));
#36441=CARTESIAN_POINT('Ctrl Pts',(-4.01099725901343,-0.158333333333301,
8.34549045978168));
#36442=CARTESIAN_POINT('Ctrl Pts',(-4.00518509494333,0.158333333333303,
8.36559053335744));
#36443=CARTESIAN_POINT('Ctrl Pts',(-4.01915231905867,0.319434907277104,
8.38197995070172));
#36444=CARTESIAN_POINT('Ctrl Pts',(-4.08046440418983,0.636309800095079,
8.43193116150102));
#36445=CARTESIAN_POINT('Ctrl Pts',(-4.12714006947675,0.794772684000679,
8.470189810946));
#36446=CARTESIAN_POINT('Ctrl Pts',(-4.24806959090074,1.06847604194533,8.53526181972456));
#36447=CARTESIAN_POINT('Ctrl Pts',(-4.31192641504674,1.1851427086124,8.5653946542121));
#36448=CARTESIAN_POINT('Ctrl Pts',(-4.3872941543946,1.30000000000101,8.59749306174244));
#36449=CARTESIAN_POINT('Ctrl Pts',(-4.45581389180656,-1.30000000000389,
8.40486348086234));
#36450=CARTESIAN_POINT('Ctrl Pts',(-4.37635417638695,-1.1851427086143,8.39545398101981));
#36451=CARTESIAN_POINT('Ctrl Pts',(-4.30815058881763,-1.06847604194623,
8.386354586336));
#36452=CARTESIAN_POINT('Ctrl Pts',(-4.1765905645673,-0.794772684000559,
8.36604956924188));
#36453=CARTESIAN_POINT('Ctrl Pts',(-4.12289143621399,-0.636309800094961,
8.34852785954195));
#36454=CARTESIAN_POINT('Ctrl Pts',(-4.04911224368695,-0.319434907277039,
8.34084171680965));
#36455=CARTESIAN_POINT('Ctrl Pts',(-4.02906394959355,-0.158333333333274,
8.3429410583932));
#36456=CARTESIAN_POINT('Ctrl Pts',(-4.02322438445646,0.158333333333276,
8.36310480910221));
#36457=CARTESIAN_POINT('Ctrl Pts',(-4.03791161393723,0.319434907277051,
8.37994596770624));
#36458=CARTESIAN_POINT('Ctrl Pts',(-4.09882136162751,0.636309800094973,
8.43119589202976));
#36459=CARTESIAN_POINT('Ctrl Pts',(-4.14540012634608,0.794772684000544,
8.47153457102627));
#36460=CARTESIAN_POINT('Ctrl Pts',(-4.26369021134847,1.06847604194515,8.53677119739374));
#36461=CARTESIAN_POINT('Ctrl Pts',(-4.32588176501405,1.1851427086122,8.56647926923266));
#36462=CARTESIAN_POINT('Ctrl Pts',(-4.39906147762723,1.30000000000079,8.59765689461122));
#36463=CARTESIAN_POINT('Ctrl Pts',(-4.47075640156972,-1.3000000000037,8.40366332508016));
#36464=CARTESIAN_POINT('Ctrl Pts',(-4.39408547423049,-1.18514270861413,
8.39449920403769));
#36465=CARTESIAN_POINT('Ctrl Pts',(-4.32788474088457,-1.06847604194607,
8.38571258744119));
#36466=CARTESIAN_POINT('Ctrl Pts',(-4.19913604612478,-0.794772684000445,
8.36628585613646));
#36467=CARTESIAN_POINT('Ctrl Pts',(-4.14455012992047,-0.63630980009487,
8.35020437312365));
#36468=CARTESIAN_POINT('Ctrl Pts',(-4.07082622887265,-0.319434907276994,
8.34232785746959));
#36469=CARTESIAN_POINT('Ctrl Pts',(-4.05018226442897,-0.158333333333251,
8.34251620036384));
#36470=CARTESIAN_POINT('Ctrl Pts',(-4.04443109382666,0.158333333333253,
8.36216210760339));
#36471=CARTESIAN_POINT('Ctrl Pts',(-4.05996668533522,0.319434907277002,
8.3795672648057));
#36472=CARTESIAN_POINT('Ctrl Pts',(-4.12066653339907,0.636309800094878,
8.43164168452648));
#36473=CARTESIAN_POINT('Ctrl Pts',(-4.16747651626436,0.794772684000431,
8.47359690481767));
#36474=CARTESIAN_POINT('Ctrl Pts',(-4.28289918668377,1.068476041945,8.53841973135357));
#36475=CARTESIAN_POINT('Ctrl Pts',(-4.34319383731295,1.18514270861203,8.56746214337356));
#36476=CARTESIAN_POINT('Ctrl Pts',(-4.4138209413781,1.3000000000006,8.59748756772854));
#36477=CARTESIAN_POINT('Ctrl Pts',(-4.48584345896765,-1.30000000000344,
8.40202163820259));
#36478=CARTESIAN_POINT('Ctrl Pts',(-4.41216396723739,-1.1851427086139,8.39306715726315));
#36479=CARTESIAN_POINT('Ctrl Pts',(-4.34811956953621,-1.06847604194586,
8.3846166180924));
#36480=CARTESIAN_POINT('Ctrl Pts',(-4.22242319351063,-0.794772684000284,
8.36625838838242));
#36481=CARTESIAN_POINT('Ctrl Pts',(-4.16699602803123,-0.636309800094742,
8.35177995975142));
#36482=CARTESIAN_POINT('Ctrl Pts',(-4.09327754286868,-0.31943490727693,
8.34441429358004));
#36483=CARTESIAN_POINT('Ctrl Pts',(-4.07191265586848,-0.158333333333219,
8.34314884305873));
#36484=CARTESIAN_POINT('Ctrl Pts',(-4.06596905594175,0.158333333333221,
8.36356395927886));
#36485=CARTESIAN_POINT('Ctrl Pts',(-4.08191651241254,0.31943490727694,8.38361776836517));
#36486=CARTESIAN_POINT('Ctrl Pts',(-4.14245654330086,0.636309800094752,
8.43588114455287));
#36487=CARTESIAN_POINT('Ctrl Pts',(-4.19024487723722,0.794772684000271,
8.47580430836259));
#36488=CARTESIAN_POINT('Ctrl Pts',(-4.3027596398058,1.06847604194478,8.53915043374496));
#36489=CARTESIAN_POINT('Ctrl Pts',(-4.36098091201217,1.18514270861179,8.56760429441749));
#36490=CARTESIAN_POINT('Ctrl Pts',(-4.42871998479172,1.30000000000034,8.59709182528973));
#36491=CARTESIAN_POINT('Ctrl Pts',(-4.49796178306258,-1.30000000000328,
8.39985529775308));
#36492=CARTESIAN_POINT('Ctrl Pts',(-4.4265716679256,-1.18514270861375,8.39102831551921));
#36493=CARTESIAN_POINT('Ctrl Pts',(-4.3641669090176,-1.06847604194573,8.38286387332469));
#36494=CARTESIAN_POINT('Ctrl Pts',(-4.24075740231498,-0.794772684000189,
8.36553297859603));
#36495=CARTESIAN_POINT('Ctrl Pts',(-4.18466518323386,-0.636309800094665,
8.35239895718667));
#36496=CARTESIAN_POINT('Ctrl Pts',(-4.11077564597456,-0.319434907276892,
8.34628584930232));
#36497=CARTESIAN_POINT('Ctrl Pts',(-4.08858028343262,-0.1583333333332,8.34531114978367));
#36498=CARTESIAN_POINT('Ctrl Pts',(-4.08246237772048,0.158333333333202,
8.36639209712338));
#36499=CARTESIAN_POINT('Ctrl Pts',(-4.09895492167411,0.319434907276901,
8.38716863132232));
#36500=CARTESIAN_POINT('Ctrl Pts',(-4.15953722291765,0.636309800094675,
8.43882757144716));
#36501=CARTESIAN_POINT('Ctrl Pts',(-4.20818172714539,0.794772684000175,
8.4769038044228));
#36502=CARTESIAN_POINT('Ctrl Pts',(-4.31847323885501,1.06847604194465,8.53929490820517));
#36503=CARTESIAN_POINT('Ctrl Pts',(-4.37507204160506,1.18514270861165,8.56754341388116));
#36504=CARTESIAN_POINT('Ctrl Pts',(-4.44052853838925,1.30000000000019,8.59703362822392));
#36505=CARTESIAN_POINT('Ctrl Pts',(-4.51007860939701,-1.30000000000315,
8.3979383522798));
#36506=CARTESIAN_POINT('Ctrl Pts',(-4.44100930532193,-1.18514270861363,
8.38941168788246));
#36507=CARTESIAN_POINT('Ctrl Pts',(-4.38027215191213,-1.06847604194562,
8.38162370178122));
#36508=CARTESIAN_POINT('Ctrl Pts',(-4.25920611198825,-0.794772684000105,
8.36533839054226));
#36509=CARTESIAN_POINT('Ctrl Pts',(-4.20248488562437,-0.636309800094599,
8.35323389895756));
#36510=CARTESIAN_POINT('Ctrl Pts',(-4.12844451407313,-0.319434907276858,
8.34819835713744));
#36511=CARTESIAN_POINT('Ctrl Pts',(-4.10532022283471,-0.158333333333184,
8.34776543894798));
#36512=CARTESIAN_POINT('Ctrl Pts',(-4.0991761536252,0.158333333333186,8.36890156372869));
#36513=CARTESIAN_POINT('Ctrl Pts',(-4.11660188214324,0.319434907276868,
8.3889786766779));
#36514=CARTESIAN_POINT('Ctrl Pts',(-4.17721976246158,0.636309800094609,
8.440105936855));
#36515=CARTESIAN_POINT('Ctrl Pts',(-4.22627658771814,0.794772684000092,
8.47825264716756));
#36516=CARTESIAN_POINT('Ctrl Pts',(-4.33422678212072,1.06847604194454,8.53984899167736));
#36517=CARTESIAN_POINT('Ctrl Pts',(-4.38921285224113,1.18514270861152,8.56761729879319));
#36518=CARTESIAN_POINT('Ctrl Pts',(-4.45245735327389,1.30000000000005,8.596491137856));
#36519=CARTESIAN_POINT('Ctrl Pts',(-4.53106911977121,-1.30000000000305,
8.39593541505668));
#36520=CARTESIAN_POINT('Ctrl Pts',(-4.4660914337767,-1.18514270861354,8.38735736377513));
#36521=CARTESIAN_POINT('Ctrl Pts',(-4.40831205489554,-1.06847604194554,
8.37973152868131));
#36522=CARTESIAN_POINT('Ctrl Pts',(-4.29145966040395,-0.794772684000049,
8.36431413395546));
#36523=CARTESIAN_POINT('Ctrl Pts',(-4.23375442648326,-0.636309800094552,
8.35356438794742));
#36524=CARTESIAN_POINT('Ctrl Pts',(-4.15956532476393,-0.319434907276834,
8.34996167513517));
#36525=CARTESIAN_POINT('Ctrl Pts',(-4.13497148445359,-0.158333333333172,
8.35005035444579));
#36526=CARTESIAN_POINT('Ctrl Pts',(-4.12857804521935,0.158333333333174,
8.37223496440372));
#36527=CARTESIAN_POINT('Ctrl Pts',(-4.14703263166815,0.319434907276844,
8.39362037831457));
#36528=CARTESIAN_POINT('Ctrl Pts',(-4.207681000708,0.636309800094562,8.44385881569951));
#36529=CARTESIAN_POINT('Ctrl Pts',(-4.25809253894196,0.794772684000033,
8.47913032176147));
#36530=CARTESIAN_POINT('Ctrl Pts',(-4.36205133787161,1.06847604194446,8.53907191087305));
#36531=CARTESIAN_POINT('Ctrl Pts',(-4.41416449316683,1.18514270861144,8.56640563709156));
#36532=CARTESIAN_POINT('Ctrl Pts',(-4.47339089175368,1.29999999999995,8.59512659665689));
#36533=CARTESIAN_POINT('Ctrl Pts',(-4.56150565654056,-1.30000000000123,
8.38949940982674));
#36534=CARTESIAN_POINT('Ctrl Pts',(-4.50244338963643,-1.18514270861188,
8.38033582366812));
#36535=CARTESIAN_POINT('Ctrl Pts',(-4.44890849532253,-1.06847604194404,
8.37283373114573));
#36536=CARTESIAN_POINT('Ctrl Pts',(-4.33800151626977,-0.794772683998929,
8.35934077931099));
#36537=CARTESIAN_POINT('Ctrl Pts',(-4.27864161246945,-0.63630980009366,
8.35265240911047));
#36538=CARTESIAN_POINT('Ctrl Pts',(-4.2040464737142,-0.319434907276387,
8.35253483013444));
#36539=CARTESIAN_POINT('Ctrl Pts',(-4.17712750120142,-0.15833333333295,
8.35434255827378));
#36540=CARTESIAN_POINT('Ctrl Pts',(-4.17062388918443,0.158333333332952,
8.37694849962917));
#36541=CARTESIAN_POINT('Ctrl Pts',(-4.19133310937807,0.319434907276396,
8.39654062259916));
#36542=CARTESIAN_POINT('Ctrl Pts',(-4.25208228768441,0.636309800093669,
8.44516159542419));
#36543=CARTESIAN_POINT('Ctrl Pts',(-4.30369303470636,0.794772683998919,
8.47961188578339));
#36544=CARTESIAN_POINT('Ctrl Pts',(-4.4017359065261,1.06847604194297,8.53808733355857));
#36545=CARTESIAN_POINT('Ctrl Pts',(-4.44974244953311,1.18514270860978,8.56478284930283));
#36546=CARTESIAN_POINT('Ctrl Pts',(-4.50331640918273,1.29999999999814,8.59286202617833));
#36547=CARTESIAN_POINT('Ctrl Pts',(-4.59169939732753,-1.30000000000067,
8.3846346623458));
#36548=CARTESIAN_POINT('Ctrl Pts',(-4.53841605520976,-1.18514270861137,
8.37598483604062));
#36549=CARTESIAN_POINT('Ctrl Pts',(-4.48909322327351,-1.06847604194358,
8.36894569229234));
#36550=CARTESIAN_POINT('Ctrl Pts',(-4.38429718531943,-0.794772683998593,
8.35640486098037));
#36551=CARTESIAN_POINT('Ctrl Pts',(-4.32383495195998,-0.636309800093389,
8.34978771198848));
#36552=CARTESIAN_POINT('Ctrl Pts',(-4.24917041175543,-0.319434907276251,
8.35113767529032));
#36553=CARTESIAN_POINT('Ctrl Pts',(-4.2200309626269,-0.158333333332882,
8.35464748725542));
#36554=CARTESIAN_POINT('Ctrl Pts',(-4.21330443794114,0.158333333332884,
8.37837348494326));
#36555=CARTESIAN_POINT('Ctrl Pts',(-4.23586855189251,0.319434907276259,
8.39806561965051));
#36556=CARTESIAN_POINT('Ctrl Pts',(-4.29652368349501,0.636309800093397,
8.44611125949594));
#36557=CARTESIAN_POINT('Ctrl Pts',(-4.34948336474048,0.794772683998581,
8.47911759872889));
#36558=CARTESIAN_POINT('Ctrl Pts',(-4.44149850175252,1.06847604194251,8.53678390432497));
#36559=CARTESIAN_POINT('Ctrl Pts',(-4.48531559698022,1.18514270860927,8.56328821396476));
#36560=CARTESIAN_POINT('Ctrl Pts',(-4.53311984411989,1.29999999999758,8.59133522629897));
#36561=CARTESIAN_POINT('Ctrl Pts',(-4.61597083254814,-1.30000000000025,
8.37961235158112));
#36562=CARTESIAN_POINT('Ctrl Pts',(-4.56749114781657,-1.18514270861098,
8.36964515588487));
#36563=CARTESIAN_POINT('Ctrl Pts',(-4.52164350144129,-1.06847604194323,
8.36197774758551));
#36564=CARTESIAN_POINT('Ctrl Pts',(-4.42180680166536,-0.79477268399833,
8.349577469512));
#36565=CARTESIAN_POINT('Ctrl Pts',(-4.36020003889848,-0.636309800093179,
8.34555660847258));
#36566=CARTESIAN_POINT('Ctrl Pts',(-4.28539468703016,-0.319434907276146,
8.34909085241622));
#36567=CARTESIAN_POINT('Ctrl Pts',(-4.25450152199579,-0.15833333333283,
8.35391668965212));
#36568=CARTESIAN_POINT('Ctrl Pts',(-4.24763644272708,0.158333333332832,
8.37845901604611));
#36569=CARTESIAN_POINT('Ctrl Pts',(-4.27175720512554,0.319434907276154,
8.39781547154599));
#36570=CARTESIAN_POINT('Ctrl Pts',(-4.33239010919754,0.636309800093188,
8.44500554199925));
#36571=CARTESIAN_POINT('Ctrl Pts',(-4.38643587888284,0.794772683998319,
8.4765648173077));
#36572=CARTESIAN_POINT('Ctrl Pts',(-4.47363483284698,1.06847604194216,8.53351665496209));
#36573=CARTESIAN_POINT('Ctrl Pts',(-4.51409770384844,1.18514270860888,8.55991989753419));
#36574=CARTESIAN_POINT('Ctrl Pts',(-4.55727824971992,1.29999999999715,8.58807404243134));
#36575=CARTESIAN_POINT('Ctrl Pts',(-4.63419695389682,-1.29999999999978,
8.37547771778039));
#36576=CARTESIAN_POINT('Ctrl Pts',(-4.58919288393035,-1.18514270861056,
8.3657354368593));
#36577=CARTESIAN_POINT('Ctrl Pts',(-4.54587154765948,-1.06847604194285,
8.35835394360906));
#36578=CARTESIAN_POINT('Ctrl Pts',(-4.44967804593736,-0.794772683998049,
8.34675510933199));
#36579=CARTESIAN_POINT('Ctrl Pts',(-4.38731242984226,-0.636309800092953,
8.34358113784012));
#36580=CARTESIAN_POINT('Ctrl Pts',(-4.3125118722081,-0.319434907276032,
8.3478546023281));
#36581=CARTESIAN_POINT('Ctrl Pts',(-4.28044235230206,-0.158333333332774,
8.35274872547764));
#36582=CARTESIAN_POINT('Ctrl Pts',(-4.27351671455972,0.158333333332776,
8.3775853109577));
#36583=CARTESIAN_POINT('Ctrl Pts',(-4.2987586842706,0.319434907276041,8.39702114369619));
#36584=CARTESIAN_POINT('Ctrl Pts',(-4.35925241921496,0.636309800092963,
8.44436998353798));
#36585=CARTESIAN_POINT('Ctrl Pts',(-4.41391057284775,0.794772683998036,
8.47615970930566));
#36586=CARTESIAN_POINT('Ctrl Pts',(-4.49745258358852,1.06847604194178,8.53285635263349));
#36587=CARTESIAN_POINT('Ctrl Pts',(-4.53542189161,1.18514270860846,8.55903248064369));
#36588=CARTESIAN_POINT('Ctrl Pts',(-4.57519826673979,1.29999999999669,8.58684286058509));
#36589=CARTESIAN_POINT('Ctrl Pts',(-4.65239690742634,-1.29999999999925,
8.37146876966087));
#36590=CARTESIAN_POINT('Ctrl Pts',(-4.61097032453698,-1.18514270861007,
8.36085690229744));
#36591=CARTESIAN_POINT('Ctrl Pts',(-4.57024914788923,-1.06847604194241,
8.3530118089499));
#36592=CARTESIAN_POINT('Ctrl Pts',(-4.47780471312426,-0.794772683997723,
8.34127987537955));
#36593=CARTESIAN_POINT('Ctrl Pts',(-4.41468297213334,-0.63630980009269,
8.33935590736899));
#36594=CARTESIAN_POINT('Ctrl Pts',(-4.33983425300278,-0.319434907275899,
8.34498441267624));
#36595=CARTESIAN_POINT('Ctrl Pts',(-4.30644484530562,-0.158333333332708,
8.35107549269899));
#36596=CARTESIAN_POINT('Ctrl Pts',(-4.2994246769601,0.15833333333271,8.37656059683744));
#36597=CARTESIAN_POINT('Ctrl Pts',(-4.32582229625926,0.319434907275909,
8.39580990391751));
#36598=CARTESIAN_POINT('Ctrl Pts',(-4.38631363002924,0.636309800092699,
8.44238749893344));
#36599=CARTESIAN_POINT('Ctrl Pts',(-4.44184660082066,0.794772683997706,
8.47258005635774));
#36600=CARTESIAN_POINT('Ctrl Pts',(-4.52173596106959,1.06847604194134,8.52901154981768));
#36601=CARTESIAN_POINT('Ctrl Pts',(-4.55715003109018,1.18514270860797,8.55540087922434));
#36602=CARTESIAN_POINT('Ctrl Pts',(-4.59339702727207,1.29999999999615,8.58375243551171));
#36603=CARTESIAN_POINT('Ctrl Pts',(-4.67662765556481,-1.29999999999835,
8.36638064005668));
#36604=CARTESIAN_POINT('Ctrl Pts',(-4.6399265403655,-1.18514270860925,8.35506988887774));
#36605=CARTESIAN_POINT('Ctrl Pts',(-4.60264173680922,-1.06847604194167,
8.34690329443953));
#36606=CARTESIAN_POINT('Ctrl Pts',(-4.51515794492436,-0.794772683997172,
8.33530045862321));
#36607=CARTESIAN_POINT('Ctrl Pts',(-4.45104183914462,-0.63630980009225,
8.33471367558874));
#36608=CARTESIAN_POINT('Ctrl Pts',(-4.37615858752344,-0.319434907275679,
8.34182081472496));
#36609=CARTESIAN_POINT('Ctrl Pts',(-4.3410379233413,-0.158333333332599,
8.34929253009869));
#36610=CARTESIAN_POINT('Ctrl Pts',(-4.33396356331471,0.158333333332601,
8.37509679924112));
#36611=CARTESIAN_POINT('Ctrl Pts',(-4.36205431788642,0.31943490727569,8.39302674220606));
#36612=CARTESIAN_POINT('Ctrl Pts',(-4.42243706520714,0.636309800092261,
8.43930113056221));
#36613=CARTESIAN_POINT('Ctrl Pts',(-4.47875680438225,0.794772683997159,
8.47003111695546));
#36614=CARTESIAN_POINT('Ctrl Pts',(-4.55370323347117,1.0684760419406,8.52660505233009));
#36615=CARTESIAN_POINT('Ctrl Pts',(-4.58574695648383,1.18514270860715,8.55301302704109));
#36616=CARTESIAN_POINT('Ctrl Pts',(-4.61739287039539,1.29999999999525,8.58134021611028));
#36617=CARTESIAN_POINT('Ctrl Pts',(-4.69789919864171,-1.29999999999678,
8.36090082369946));
#36618=CARTESIAN_POINT('Ctrl Pts',(-4.66536018132445,-1.18514270860782,
8.34847304056692));
#36619=CARTESIAN_POINT('Ctrl Pts',(-4.63110015263561,-1.06847604194038,
8.33973082770565));
#36620=CARTESIAN_POINT('Ctrl Pts',(-4.54797675211423,-0.794772683996213,
8.32804897174489));
#36621=CARTESIAN_POINT('Ctrl Pts',(-4.48294097752206,-0.636309800091482,
8.3295239875756));
#36622=CARTESIAN_POINT('Ctrl Pts',(-4.4080743825454,-0.319434907275293,
8.33788201166714));
#36623=CARTESIAN_POINT('Ctrl Pts',(-4.37158871913637,-0.158333333332408,
8.34554546637412));
#36624=CARTESIAN_POINT('Ctrl Pts',(-4.36441939582717,0.15833333333241,8.37203984518833));
#36625=CARTESIAN_POINT('Ctrl Pts',(-4.39371384560967,0.319434907275301,
8.39075278554675));
#36626=CARTESIAN_POINT('Ctrl Pts',(-4.45402163421419,0.63630980009149,8.43660222784233));
#36627=CARTESIAN_POINT('Ctrl Pts',(-4.51138877020508,0.794772683996199,
8.46519550192625));
#36628=CARTESIAN_POINT('Ctrl Pts',(-4.58202224890887,1.06847604193931,8.52184443050647));
#36629=CARTESIAN_POINT('Ctrl Pts',(-4.61105314249528,1.18514270860572,8.54875829622621));
#36630=CARTESIAN_POINT('Ctrl Pts',(-4.63854031396548,1.29999999999368,8.57806480553295));
#36631=CARTESIAN_POINT('Ctrl Pts',(-4.7161409482319,-1.2999999999962,8.35590271413686));
#36632=CARTESIAN_POINT('Ctrl Pts',(-4.68713869592175,-1.1851427086073,8.34279578720867));
#36633=CARTESIAN_POINT('Ctrl Pts',(-4.65546276338965,-1.06847604193991,
8.33362197404163));
#36634=CARTESIAN_POINT('Ctrl Pts',(-4.57610828631184,-0.794772683995863,
8.32151491001579));
#36635=CARTESIAN_POINT('Ctrl Pts',(-4.51045420438319,-0.636309800091202,
8.3230585656632));
#36636=CARTESIAN_POINT('Ctrl Pts',(-4.43556241906787,-0.319434907275153,
8.33283856066987));
#36637=CARTESIAN_POINT('Ctrl Pts',(-4.39766426030354,-0.158333333332338,
8.34294220161402));
#36638=CARTESIAN_POINT('Ctrl Pts',(-4.39039693442986,0.15833333333234,8.37036241559784));
#36639=CARTESIAN_POINT('Ctrl Pts',(-4.42095202386697,0.319434907275162,
8.38797320825141));
#36640=CARTESIAN_POINT('Ctrl Pts',(-4.48119507360353,0.636309800091212,
8.4334469106398));
#36641=CARTESIAN_POINT('Ctrl Pts',(-4.53922661725484,0.79477268399585,8.4618577332553));
#36642=CARTESIAN_POINT('Ctrl Pts',(-4.60615474087746,1.06847604193884,8.51866629487098));
#36643=CARTESIAN_POINT('Ctrl Pts',(-4.6326429935655,1.1851427086052,8.5457569896651));
#36644=CARTESIAN_POINT('Ctrl Pts',(-4.65664879415669,1.29999999999311,8.57534805789455));
#36645=CARTESIAN_POINT('Ctrl Pts',(-4.72823715178914,-1.29999999999609,
8.35339014157118));
#36646=CARTESIAN_POINT('Ctrl Pts',(-4.70157648358082,-1.1851427086072,8.34013566417898));
#36647=CARTESIAN_POINT('Ctrl Pts',(-4.6716106932305,-1.06847604193982,8.33087284428749));
#36648=CARTESIAN_POINT('Ctrl Pts',(-4.59474822955049,-0.794772683995793,
8.31869540467249));
#36649=CARTESIAN_POINT('Ctrl Pts',(-4.52863710511104,-0.636309800091145,
8.32041158642372));
#36650=CARTESIAN_POINT('Ctrl Pts',(-4.45380783327018,-0.319434907275124,
8.33028811432542));
#36651=CARTESIAN_POINT('Ctrl Pts',(-4.41513333680483,-0.158333333332324,
8.34052686594499));
#36652=CARTESIAN_POINT('Ctrl Pts',(-4.40788109043004,0.158333333332326,
8.36780256651529));
#36653=CARTESIAN_POINT('Ctrl Pts',(-4.43925339017667,0.319434907275135,
8.38489298636552));
#36654=CARTESIAN_POINT('Ctrl Pts',(-4.49941210358521,0.636309800091156,
8.4304661802376));
#36655=CARTESIAN_POINT('Ctrl Pts',(-4.55779440082702,0.794772683995778,
8.45954256857753));
#36656=CARTESIAN_POINT('Ctrl Pts',(-4.62223204623287,1.06847604193874,8.51666493827882));
#36657=CARTESIAN_POINT('Ctrl Pts',(-4.64703395571431,1.18514270860509,8.54382151210089));
#36658=CARTESIAN_POINT('Ctrl Pts',(-4.66874510563104,1.29999999999299,8.57340850249371));
#36659=CARTESIAN_POINT('Ctrl Pts',(-4.74340335118311,-1.29999999999471,
8.34928292021594));
#36660=CARTESIAN_POINT('Ctrl Pts',(-4.71975192723288,-1.18514270860593,
8.33452631874549));
#36661=CARTESIAN_POINT('Ctrl Pts',(-4.69197337306874,-1.06847604193868,
8.32439339815895));
#36662=CARTESIAN_POINT('Ctrl Pts',(-4.61826485944567,-0.794772683994948,
8.3116659523263));
#36663=CARTESIAN_POINT('Ctrl Pts',(-4.55150389070566,-0.63630980009047,
8.31530639162805));
#36664=CARTESIAN_POINT('Ctrl Pts',(-4.47666293354192,-0.319434907274786,
8.32657119999817));
#36665=CARTESIAN_POINT('Ctrl Pts',(-4.43694261924442,-0.158333333332156,
8.337662514481));
#36666=CARTESIAN_POINT('Ctrl Pts',(-4.42961852259884,0.158333333332158,
8.3655893801562));
#36667=CARTESIAN_POINT('Ctrl Pts',(-4.46192298299084,0.319434907274794,
8.38263381659107));
#36668=CARTESIAN_POINT('Ctrl Pts',(-4.52203218557171,0.636309800090479,
8.4278285386015));
#36669=CARTESIAN_POINT('Ctrl Pts',(-4.58109824215759,0.794772683994937,
8.45573367388843));
#36670=CARTESIAN_POINT('Ctrl Pts',(-4.64245005899539,1.06847604193761,8.51300720003524));
#36671=CARTESIAN_POINT('Ctrl Pts',(-4.6651086871392,1.18514270860383,8.54052734185137));
#36672=CARTESIAN_POINT('Ctrl Pts',(-4.68386901522655,1.29999999999161,8.57077603820792));
#36673=CARTESIAN_POINT('Ctrl Pts',(-4.76167893245149,-1.29999999999383,
8.34369189625078));
#36674=CARTESIAN_POINT('Ctrl Pts',(-4.74150919494958,-1.18514270860513,
8.32887343937279));
#36675=CARTESIAN_POINT('Ctrl Pts',(-4.7162784389449,-1.06847604193795,8.31869365207076));
#36676=CARTESIAN_POINT('Ctrl Pts',(-4.64629837998445,-0.794772683994407,
8.30589256162683));
#36677=CARTESIAN_POINT('Ctrl Pts',(-4.57891469655928,-0.636309800090037,
8.30930913056515));
#36678=CARTESIAN_POINT('Ctrl Pts',(-4.50415702674796,-0.319434907274568,
8.32100124625156));
#36679=CARTESIAN_POINT('Ctrl Pts',(-4.46324312599945,-0.158333333332048,
8.33279575559108));
#36680=CARTESIAN_POINT('Ctrl Pts',(-4.45585255642742,0.15833333333205,8.36145869754515));
#36681=CARTESIAN_POINT('Ctrl Pts',(-4.48922780131988,0.319434907274574,
8.37907070770448));
#36682=CARTESIAN_POINT('Ctrl Pts',(-4.54923305414967,0.636309800090044,
8.42424832705878));
#36683=CARTESIAN_POINT('Ctrl Pts',(-4.6090698142711,0.794772683994395,8.45098139609059));
#36684=CARTESIAN_POINT('Ctrl Pts',(-4.66671552092437,1.06847604193688,8.50848521847131));
#36685=CARTESIAN_POINT('Ctrl Pts',(-4.68681425050692,1.18514270860302,8.53638505230757));
#36686=CARTESIAN_POINT('Ctrl Pts',(-4.70205901924573,1.29999999999073,8.56729344599807));
#36687=CARTESIAN_POINT('Ctrl Pts',(-4.77982710526041,-1.29999999999232,
8.33905011299784));
#36688=CARTESIAN_POINT('Ctrl Pts',(-4.76326639868391,-1.18514270860376,
8.32231210199745));
#36689=CARTESIAN_POINT('Ctrl Pts',(-4.74065971664241,-1.06847604193671,
8.3110086941711));
#36690=CARTESIAN_POINT('Ctrl Pts',(-4.67446634585838,-0.794772683993484,
8.29745058137394));
#36691=CARTESIAN_POINT('Ctrl Pts',(-4.60627902145023,-0.636309800089299,
8.30355111374383));
#36692=CARTESIAN_POINT('Ctrl Pts',(-4.53157317325735,-0.319434907274198,
8.31633606172721));
#36693=CARTESIAN_POINT('Ctrl Pts',(-4.48949570989188,-0.158333333331864,
8.32826416125297));
#36694=CARTESIAN_POINT('Ctrl Pts',(-4.48213234554617,0.158333333331866,
8.35668177661298));
#36695=CARTESIAN_POINT('Ctrl Pts',(-4.51675009789326,0.319434907274205,
8.37315955889524));
#36696=CARTESIAN_POINT('Ctrl Pts',(-4.57665355432879,0.636309800089306,
8.41828314766454));
#36697=CARTESIAN_POINT('Ctrl Pts',(-4.6370722671515,0.794772683993473,8.44570568631553));
#36698=CARTESIAN_POINT('Ctrl Pts',(-4.69093818547079,1.06847604193564,8.50417913824327));
#36699=CARTESIAN_POINT('Ctrl Pts',(-4.70846533482425,1.18514270860165,8.5325837124655));
#36700=CARTESIAN_POINT('Ctrl Pts',(-4.72020307341969,1.29999999998922,8.56408187022532));
#36701=CARTESIAN_POINT('Ctrl Pts',(-4.79803343217889,-1.29999999999099,
8.33394511610362));
#36702=CARTESIAN_POINT('Ctrl Pts',(-4.7849677374734,-1.18514270860254,8.31688391588858));
#36703=CARTESIAN_POINT('Ctrl Pts',(-4.76492392505446,-1.06847604193562,
8.30527350198988));
#36704=CARTESIAN_POINT('Ctrl Pts',(-4.70249786073047,-0.794772683992672,
8.29104353004542));
#36705=CARTESIAN_POINT('Ctrl Pts',(-4.63374160723767,-0.636309800088648,
8.29620513161596));
#36706=CARTESIAN_POINT('Ctrl Pts',(-4.55911762196679,-0.319434907273871,
8.30950121211404));
#36707=CARTESIAN_POINT('Ctrl Pts',(-4.51578716586765,-0.158333333331702,
8.32306342541251));
#36708=CARTESIAN_POINT('Ctrl Pts',(-4.50832961490194,0.158333333331705,
8.35263978253959));
#36709=CARTESIAN_POINT('Ctrl Pts',(-4.54402552275341,0.319434907273878,
8.36952925941727));
#36710=CARTESIAN_POINT('Ctrl Pts',(-4.60381954438777,0.636309800088656,
8.41469509842377));
#36711=CARTESIAN_POINT('Ctrl Pts',(-4.66500217002981,0.79477268399266,8.44099914592903));
#36712=CARTESIAN_POINT('Ctrl Pts',(-4.71516619093475,1.06847604193455,8.49972033154497));
#36713=CARTESIAN_POINT('Ctrl Pts',(-4.73013805396894,1.18514270860044,8.5284997162424));
#36714=CARTESIAN_POINT('Ctrl Pts',(-4.7383676341477,1.29999999998789,8.56064026021845));
#36715=CARTESIAN_POINT('Ctrl Pts',(-4.81094149750922,-1.29999999998978,
8.32978009402368));
#36716=CARTESIAN_POINT('Ctrl Pts',(-4.80039230401006,-1.18514270860144,
8.31169231381476));
#36717=CARTESIAN_POINT('Ctrl Pts',(-4.7821836182234,-1.06847604193462,8.29946834001264));
#36718=CARTESIAN_POINT('Ctrl Pts',(-4.72242295196123,-0.794772683991931,
8.28477508098243));
#36719=CARTESIAN_POINT('Ctrl Pts',(-4.65316124219068,-0.636309800088055,
8.29111147785697));
#36720=CARTESIAN_POINT('Ctrl Pts',(-4.57857606554552,-0.319434907273573,
8.30524578386532));
#36721=CARTESIAN_POINT('Ctrl Pts',(-4.53438456950182,-0.158333333331555,
8.31951483890184));
#36722=CARTESIAN_POINT('Ctrl Pts',(-4.52692720614846,0.158333333331557,
8.34921452120318));
#36723=CARTESIAN_POINT('Ctrl Pts',(-4.56348734251723,0.31943490727358,8.36538523893045));
#36724=CARTESIAN_POINT('Ctrl Pts',(-4.62323682493845,0.636309800088062,
8.4102395363381));
#36725=CARTESIAN_POINT('Ctrl Pts',(-4.68491217123887,0.794772683991919,
8.43621329058605));
#36726=CARTESIAN_POINT('Ctrl Pts',(-4.73240589414762,1.06847604193355,8.49562341725007));
#36727=CARTESIAN_POINT('Ctrl Pts',(-4.74554246979028,1.18514270859933,8.52494769230183));
#36728=CARTESIAN_POINT('Ctrl Pts',(-4.75125734824424,1.29999999998668,8.5578797999346));
#36729=CARTESIAN_POINT('Ctrl Pts',(-4.81852392502146,-1.29999999998959,
8.32749751318685));
#36730=CARTESIAN_POINT('Ctrl Pts',(-4.80944615872512,-1.18514270860127,
8.30897667740979));
#36731=CARTESIAN_POINT('Ctrl Pts',(-4.79231288165303,-1.06847604193448,
8.29646873585038));
#36732=CARTESIAN_POINT('Ctrl Pts',(-4.73412174272511,-0.79477268399182,
8.2814638771612));
#36733=CARTESIAN_POINT('Ctrl Pts',(-4.66458809103075,-0.636309800087967,
8.2880031704567));
#36734=CARTESIAN_POINT('Ctrl Pts',(-4.59002800238769,-0.319434907273529,
8.30255284095863));
#36735=CARTESIAN_POINT('Ctrl Pts',(-4.54531512979248,-0.158333333331533,
8.31750113977235));
#36736=CARTESIAN_POINT('Ctrl Pts',(-4.53784740212769,0.158333333331535,
8.34739593227855));
#36737=CARTESIAN_POINT('Ctrl Pts',(-4.5749074249398,0.319434907273536,8.36318641560727));
#36738=CARTESIAN_POINT('Ctrl Pts',(-4.63463337044967,0.636309800087975,
8.4078111388242));
#36739=CARTESIAN_POINT('Ctrl Pts',(-4.69661484844976,0.794772683991809,
8.43341649612987));
#36740=CARTESIAN_POINT('Ctrl Pts',(-4.74254482298291,1.0684760419334,8.49317263346162));
#36741=CARTESIAN_POINT('Ctrl Pts',(-4.75460297195919,1.18514270859917,8.52281712210147));
#36742=CARTESIAN_POINT('Ctrl Pts',(-4.75883788580962,1.2999999999865,8.55623988171332));
#36743=CARTESIAN_POINT('Ctrl Pts',(-4.82041977295653,-1.29999999998959,
8.32691849490388));
#36744=CARTESIAN_POINT('Ctrl Pts',(-4.81170975047181,-1.18514270860127,
8.30828675594369));
#36745=CARTESIAN_POINT('Ctrl Pts',(-4.79484522454245,-1.06847604193447,
8.29570698049037));
#36746=CARTESIAN_POINT('Ctrl Pts',(-4.73704626164923,-0.794772683991816,
8.28062642900982));
#36747=CARTESIAN_POINT('Ctrl Pts',(-4.66744427478885,-0.636309800087964,
8.28722884049732));
#36748=CARTESIAN_POINT('Ctrl Pts',(-4.59289080743435,-0.319434907273528,
8.3018811056208));
#36749=CARTESIAN_POINT('Ctrl Pts',(-4.54804875165676,-0.158333333331532,
8.31698349332809));
#36750=CARTESIAN_POINT('Ctrl Pts',(-4.54057832594463,0.158333333331534,
8.3469283166452));
#36751=CARTESIAN_POINT('Ctrl Pts',(-4.57776226683473,0.319434907273535,
8.36263692754277));
#36752=CARTESIAN_POINT('Ctrl Pts',(-4.6374813242383,0.636309800087972,8.40721577472294));
#36753=CARTESIAN_POINT('Ctrl Pts',(-4.69953831741039,0.794772683991806,
8.43273932158352));
#36754=CARTESIAN_POINT('Ctrl Pts',(-4.74507757726615,1.0684760419334,8.49257974884738));
#36755=CARTESIAN_POINT('Ctrl Pts',(-4.75686656169974,1.18514270859916,8.52229970933397));
#36756=CARTESIAN_POINT('Ctrl Pts',(-4.7607322723712,1.29999999998649,8.55583692665094));
#36757=CARTESIAN_POINT('Ctrl Pts',(-4.82269479895944,-1.29999999998956,
8.32621878032447));
#36758=CARTESIAN_POINT('Ctrl Pts',(-4.8144260230379,-1.18514270860124,8.30745082409725));
#36759=CARTESIAN_POINT('Ctrl Pts',(-4.79788395737724,-1.06847604193445,
8.29478338814642));
#36760=CARTESIAN_POINT('Ctrl Pts',(-4.74055552210931,-0.7947726839918,8.27961249923156));
#36761=CARTESIAN_POINT('Ctrl Pts',(-4.67087133177399,-0.636309800087951,
8.28630024690135));
#36762=CARTESIAN_POINT('Ctrl Pts',(-4.59632606869179,-0.319434907273521,
8.30107481000781));
#36763=CARTESIAN_POINT('Ctrl Pts',(-4.55132986051768,-0.158333333331529,
8.3163499578362));
#36764=CARTESIAN_POINT('Ctrl Pts',(-4.54385592295093,0.158333333331531,
8.34635759780241));
#36765=CARTESIAN_POINT('Ctrl Pts',(-4.58118745436961,0.319434907273528,
8.36198104652681));
#36766=CARTESIAN_POINT('Ctrl Pts',(-4.64089736676338,0.636309800087958,
8.40651507099385));
#36767=CARTESIAN_POINT('Ctrl Pts',(-4.70304427261792,0.794772683991789,
8.43194799941686));
#36768=CARTESIAN_POINT('Ctrl Pts',(-4.7481150701394,1.06847604193338,8.49188621570782));
#36769=CARTESIAN_POINT('Ctrl Pts',(-4.75958153919977,1.18514270859914,8.52169207072452));
#36770=CARTESIAN_POINT('Ctrl Pts',(-4.76300499911106,1.29999999998647,8.55535874785532));
#36771=CARTESIAN_POINT('Ctrl Pts',(-4.82724518123329,-1.29999999998947,
8.32480162162588));
#36772=CARTESIAN_POINT('Ctrl Pts',(-4.81985877333475,-1.18514270860116,
8.30575213666847));
#36773=CARTESIAN_POINT('Ctrl Pts',(-4.80396149243278,-1.06847604193437,
8.29290542346446));
#36774=CARTESIAN_POINT('Ctrl Pts',(-4.7475737740772,-0.794772683991742,
8.27755658959772));
#36775=CARTESIAN_POINT('Ctrl Pts',(-4.67772434607518,-0.636309800087904,
8.28444559580218));
#36776=CARTESIAN_POINT('Ctrl Pts',(-4.60319626152197,-0.319434907273498,
8.29946273161348));
#36777=CARTESIAN_POINT('Ctrl Pts',(-4.55789440269426,-0.158333333331517,
8.31504728914924));
#36778=CARTESIAN_POINT('Ctrl Pts',(-4.5504130055163,0.158333333331519,8.34518520592664));
#36779=CARTESIAN_POINT('Ctrl Pts',(-4.58803698786698,0.319434907273504,
8.36067115696744));
#36780=CARTESIAN_POINT('Ctrl Pts',(-4.64772621923239,0.636309800087912,
8.4051431652836));
#36781=CARTESIAN_POINT('Ctrl Pts',(-4.71005075988252,0.794772683991732,
8.43041777479225));
#36782=CARTESIAN_POINT('Ctrl Pts',(-4.75418534119007,1.0684760419333,8.49054555455211));
#36783=CARTESIAN_POINT('Ctrl Pts',(-4.76500790392179,1.18514270859905,8.52051208905625));
#36784=CARTESIAN_POINT('Ctrl Pts',(-4.76754880448457,1.29999999998637,8.55441807016026));
#36785=CARTESIAN_POINT('Ctrl Pts',(-4.83445330411152,-1.29999999998922,
8.3224116128313));
#36786=CARTESIAN_POINT('Ctrl Pts',(-4.82846766580034,-1.18514270860093,
8.30278026328514));
#36787=CARTESIAN_POINT('Ctrl Pts',(-4.8135928108613,-1.06847604193417,8.28958539587345));
#36788=CARTESIAN_POINT('Ctrl Pts',(-4.7586930515559,-0.794772683991593,
8.27397217387284));
#36789=CARTESIAN_POINT('Ctrl Pts',(-4.68856715970435,-0.636309800087784,
8.2815609625007));
#36790=CARTESIAN_POINT('Ctrl Pts',(-4.6140701043017,-0.319434907273438,
8.29697865182959));
#36791=CARTESIAN_POINT('Ctrl Pts',(-4.56830640821597,-0.158333333331488,
8.31272251695755));
#36792=CARTESIAN_POINT('Ctrl Pts',(-4.56081294584385,0.15833333333149,8.34306422751495));
#36793=CARTESIAN_POINT('Ctrl Pts',(-4.59888398565192,0.319434907273445,
8.35854789869529));
#36794=CARTESIAN_POINT('Ctrl Pts',(-4.65852314139286,0.636309800087793,
8.40312972582311));
#36795=CARTESIAN_POINT('Ctrl Pts',(-4.7211081020808,0.794772683991581,8.42837394721402));
#36796=CARTESIAN_POINT('Ctrl Pts',(-4.76376426071759,1.0684760419331,8.4887680229739));
#36797=CARTESIAN_POINT('Ctrl Pts',(-4.77357562396977,1.18514270859883,8.51890352477032));
#36798=CARTESIAN_POINT('Ctrl Pts',(-4.77473407996669,1.29999999998613,8.55303217078774));
#36799=CARTESIAN_POINT('Ctrl Pts',(-4.84090172139479,-1.29999999998864,
8.32022306470272));
#36800=CARTESIAN_POINT('Ctrl Pts',(-4.83617138484706,-1.1851427086004,8.30000540687456));
#36801=CARTESIAN_POINT('Ctrl Pts',(-4.82221247131159,-1.06847604193369,
8.28646006688069));
#36802=CARTESIAN_POINT('Ctrl Pts',(-4.76864472956175,-0.794772683991235,
8.27058201074876));
#36803=CARTESIAN_POINT('Ctrl Pts',(-4.69826634496861,-0.636309800087498,
8.27890451007233));
#36804=CARTESIAN_POINT('Ctrl Pts',(-4.62380013668611,-0.319434907273293,
8.29467661136089));
#36805=CARTESIAN_POINT('Ctrl Pts',(-4.57763211214118,-0.158333333331416,
8.31048006764925));
#36806=CARTESIAN_POINT('Ctrl Pts',(-4.57013078277785,0.158333333331418,
8.3409843725767));
#36807=CARTESIAN_POINT('Ctrl Pts',(-4.60859948159869,0.319434907273301,
8.35648703793527));
#36808=CARTESIAN_POINT('Ctrl Pts',(-4.66818932641239,0.636309800087505,
8.40121676647618));
#36809=CARTESIAN_POINT('Ctrl Pts',(-4.73100056677066,0.794772683991223,
8.42650073147393));
#36810=CARTESIAN_POINT('Ctrl Pts',(-4.7723309702851,1.06847604193262,8.4871754226118));
#36811=CARTESIAN_POINT('Ctrl Pts',(-4.78123739741691,1.1851427085983,8.5174718613016));
#36812=CARTESIAN_POINT('Ctrl Pts',(-4.7811598514415,1.29999999998554,8.55180091310643));
#36813=CARTESIAN_POINT('Ctrl Pts',(-4.84469211502532,-1.29999999998857,
8.31899636837851));
#36814=CARTESIAN_POINT('Ctrl Pts',(-4.84069767541249,-1.18514270860033,
8.29849818618627));
#36815=CARTESIAN_POINT('Ctrl Pts',(-4.82727652100109,-1.06847604193363,
8.28477299775572));
#36816=CARTESIAN_POINT('Ctrl Pts',(-4.77449337242585,-0.794772683991192,
8.26871203728901));
#36817=CARTESIAN_POINT('Ctrl Pts',(-4.70397525490767,-0.636309800087463,
8.27725099678412));
#36818=CARTESIAN_POINT('Ctrl Pts',(-4.62952730006986,-0.319434907273276,
8.29320881981134));
#36819=CARTESIAN_POINT('Ctrl Pts',(-4.58311248005771,-0.158333333331408,
8.3092164002926));
#36820=CARTESIAN_POINT('Ctrl Pts',(-4.57560738480491,0.15833333333141,8.33981920313398));
#36821=CARTESIAN_POINT('Ctrl Pts',(-4.61431686521015,0.319434907273283,
8.3552276973425));
#36822=CARTESIAN_POINT('Ctrl Pts',(-4.67388536473402,0.636309800087471,
8.39994900403055));
#36823=CARTESIAN_POINT('Ctrl Pts',(-4.73683980643477,0.79477268399118,8.42514666196667));
#36824=CARTESIAN_POINT('Ctrl Pts',(-4.77738673633568,1.06847604193256,8.48602790384311));
#36825=CARTESIAN_POINT('Ctrl Pts',(-4.78575576767938,1.18514270859823,8.51647683565076));
#36826=CARTESIAN_POINT('Ctrl Pts',(-4.78494256682449,1.29999999998547,8.55102146553006));
#36827=CARTESIAN_POINT('Ctrl Pts',(-4.84620807955783,-1.29999999998855,
8.31850938759095));
#36828=CARTESIAN_POINT('Ctrl Pts',(-4.84250783269422,-1.18514270860032,
8.29790295896496));
#36829=CARTESIAN_POINT('Ctrl Pts',(-4.82930171446687,-1.06847604193362,
8.28410738306688));
#36830=CARTESIAN_POINT('Ctrl Pts',(-4.77683247499386,-0.794772683991185,
8.26797127525481));
#36831=CARTESIAN_POINT('Ctrl Pts',(-4.70625903418148,-0.636309800087458,
8.27658305038065));
#36832=CARTESIAN_POINT('Ctrl Pts',(-4.63181841837675,-0.319434907273273,
8.29261338980029));
#36833=CARTESIAN_POINT('Ctrl Pts',(-4.58530434898141,-0.158333333331406,
8.30871300401627));
#36834=CARTESIAN_POINT('Ctrl Pts',(-4.57779781922702,0.158333333331408,
8.33935530629564));
#36835=CARTESIAN_POINT('Ctrl Pts',(-4.61660402946877,0.31943490727328,8.35471974975148));
#36836=CARTESIAN_POINT('Ctrl Pts',(-4.67616447814182,0.636309800087465,
8.39943171718987));
#36837=CARTESIAN_POINT('Ctrl Pts',(-4.73917685456128,0.794772683991173,
8.4245876721559));
#36838=CARTESIAN_POINT('Ctrl Pts',(-4.77941016424681,1.06847604193255,8.48555436720518));
#36839=CARTESIAN_POINT('Ctrl Pts',(-4.78756391136092,1.18514270859822,8.51606813087895));
#36840=CARTESIAN_POINT('Ctrl Pts',(-4.78645589661729,1.29999999998546,8.55070543497829));
#36841=CARTESIAN_POINT('Ctrl Pts',(-4.8481026095768,-1.29999999998851,8.31790944516153));
#36842=CARTESIAN_POINT('Ctrl Pts',(-4.84476969930837,-1.18514270860029,
8.29717727121702));
#36843=CARTESIAN_POINT('Ctrl Pts',(-4.83183220576747,-1.06847604193359,
8.28329759320041));
#36844=CARTESIAN_POINT('Ctrl Pts',(-4.77975549880186,-0.79477268399116,
8.26706339679263));
#36845=CARTESIAN_POINT('Ctrl Pts',(-4.70911424471676,-0.636309800087438,
8.27573422660257));
#36846=CARTESIAN_POINT('Ctrl Pts',(-4.63468285954174,-0.319434907273264,
8.29185128022252));
#36847=CARTESIAN_POINT('Ctrl Pts',(-4.58804345446328,-0.158333333331401,
8.30809002830088));
#36848=CARTESIAN_POINT('Ctrl Pts',(-4.58053525050573,0.158333333331403,
8.33878219628126));
#36849=CARTESIAN_POINT('Ctrl Pts',(-4.61946329649243,0.31943490727327,8.35407725721605));
#36850=CARTESIAN_POINT('Ctrl Pts',(-4.67901482319528,0.636309800087446,
8.39876357767907));
#36851=CARTESIAN_POINT('Ctrl Pts',(-4.74210119862822,0.794772683991148,
8.42385020461042));
#36852=CARTESIAN_POINT('Ctrl Pts',(-4.78194200703895,1.06847604193252,8.4849296291328));
#36853=CARTESIAN_POINT('Ctrl Pts',(-4.7898259182097,1.18514270859818,8.51553301549614));
#36854=CARTESIAN_POINT('Ctrl Pts',(-4.78834813083761,1.29999999998542,8.55030076856277));
#36855=CARTESIAN_POINT('Ctrl Pts',(-4.84980725425054,-1.29999999998848,
8.31737761465617));
#36856=CARTESIAN_POINT('Ctrl Pts',(-4.84680454639138,-1.18514270860025,
8.2965412065861));
#36857=CARTESIAN_POINT('Ctrl Pts',(-4.83410864630962,-1.06847604193356,
8.28258937106431));
#36858=CARTESIAN_POINT('Ctrl Pts',(-4.78238536416429,-0.794772683991136,
8.26626257979442));
#36859=CARTESIAN_POINT('Ctrl Pts',(-4.71168437486339,-0.636309800087419,
8.2749562061174));
#36860=CARTESIAN_POINT('Ctrl Pts',(-4.63726141895635,-0.319434907273254,
8.29114666110038));
#36861=CARTESIAN_POINT('Ctrl Pts',(-4.59050809948508,-0.158333333331397,
8.30753196390599));
#36862=CARTESIAN_POINT('Ctrl Pts',(-4.58299851718329,0.158333333331399,
8.33826944875672));
#36863=CARTESIAN_POINT('Ctrl Pts',(-4.62203700163914,0.319434907273261,
8.35349010881316));
#36864=CARTESIAN_POINT('Ctrl Pts',(-4.68158156410424,0.636309800087427,
8.39814067012216));
#36865=CARTESIAN_POINT('Ctrl Pts',(-4.74473605054966,0.794772683991125,
8.42314821811786));
#36866=CARTESIAN_POINT('Ctrl Pts',(-4.78422322584727,1.06847604193248,8.48433441417299));
#36867=CARTESIAN_POINT('Ctrl Pts',(-4.79186363629283,1.18514270859815,8.51502642501498));
#36868=CARTESIAN_POINT('Ctrl Pts',(-4.79005192214164,1.29999999998538,8.54992520959865));
#36869=CARTESIAN_POINT('Ctrl Pts',(-4.85094353887164,-1.29999999998846,
8.3170253307956));
#36870=CARTESIAN_POINT('Ctrl Pts',(-4.8481608384203,-1.18514270860024,8.29612198038685));
#36871=CARTESIAN_POINT('Ctrl Pts',(-4.83562594699106,-1.06847604193355,
8.28212298961925));
#36872=CARTESIAN_POINT('Ctrl Pts',(-4.7841383281153,-0.79477268399113,8.26573297244118));
#36873=CARTESIAN_POINT('Ctrl Pts',(-4.71339791183896,-0.636309800087413,
8.27443280912155));
#36874=CARTESIAN_POINT('Ctrl Pts',(-4.63898064804253,-0.319434907273251,
8.29067036055618));
#36875=CARTESIAN_POINT('Ctrl Pts',(-4.59215110952092,-0.158333333331395,
8.30715890120654));
#36876=CARTESIAN_POINT('Ctrl Pts',(-4.58464065380343,0.158333333331397,
8.33792673389281));
#36877=CARTESIAN_POINT('Ctrl Pts',(-4.62375294779913,0.319434907273258,
8.35309509327714));
#36878=CARTESIAN_POINT('Ctrl Pts',(-4.68329316798326,0.636309800087421,
8.39771843549319));
#36879=CARTESIAN_POINT('Ctrl Pts',(-4.74649349899409,0.794772683991118,
8.42266833267474));
#36880=CARTESIAN_POINT('Ctrl Pts',(-4.78574485520293,1.06847604193248,8.48392703633881));
#36881=CARTESIAN_POINT('Ctrl Pts',(-4.79322277563256,1.18514270859814,8.5146802882616));
#36882=CARTESIAN_POINT('Ctrl Pts',(-4.79118815879509,1.29999999998537,8.54967016914964));
#36883=CARTESIAN_POINT('Ctrl Pts',(-4.85151165403496,-1.29999999998846,
8.31684956349615));
#36884=CARTESIAN_POINT('Ctrl Pts',(-4.84883893538057,-1.18514270860024,
8.29591313944484));
#36885=CARTESIAN_POINT('Ctrl Pts',(-4.83638453913278,-1.06847604193355,
8.28189070955156));
#36886=CARTESIAN_POINT('Ctrl Pts',(-4.78501476024864,-0.794772683991129,
8.26546880096556));
#36887=CARTESIAN_POINT('Ctrl Pts',(-4.71425469626629,-0.636309800087412,
8.27417029196364));
#36888=CARTESIAN_POINT('Ctrl Pts',(-4.6398402970313,-0.319434907273251,
8.29043100080685));
#36889=CARTESIAN_POINT('Ctrl Pts',(-4.59297261469187,-0.158333333331395,
8.30697189695609));
#36890=CARTESIAN_POINT('Ctrl Pts',(-4.58546173106472,0.158333333331397,
8.33775491528288));
#36891=CARTESIAN_POINT('Ctrl Pts',(-4.62461094888219,0.319434907273258,
8.35289685748205));
#36892=CARTESIAN_POINT('Ctrl Pts',(-4.68414904630666,0.63630980008742,8.39750607192482));
#36893=CARTESIAN_POINT('Ctrl Pts',(-4.74737237762247,0.794772683991117,
8.42242623561674));
#36894=CARTESIAN_POINT('Ctrl Pts',(-4.78650581916945,1.06847604193247,8.48372139404888));
#36895=CARTESIAN_POINT('Ctrl Pts',(-4.79390247131605,1.18514270859814,8.51450562532234));
#36896=CARTESIAN_POINT('Ctrl Pts',(-4.79175635880045,1.29999999998537,8.54954168499341));
#36897=CARTESIAN_POINT('Ctrl Pts',(-4.85198506445694,-1.29999999998846,
8.31670332061117));
#36898=CARTESIAN_POINT('Ctrl Pts',(-4.84940397997935,-1.18514270860023,
8.29573963809466));
#36899=CARTESIAN_POINT('Ctrl Pts',(-4.83701665562309,-1.06847604193354,
8.28169778118904));
#36900=CARTESIAN_POINT('Ctrl Pts',(-4.78574508243343,-0.794772683991124,
8.26524908454092));
#36901=CARTESIAN_POINT('Ctrl Pts',(-4.71496869699086,-0.636309800087409,
8.2739508205106));
#36902=CARTESIAN_POINT('Ctrl Pts',(-4.64055669627058,-0.319434907273249,
8.29023058588678));
#36903=CARTESIAN_POINT('Ctrl Pts',(-4.59365719512019,-0.158333333331394,
8.3068157981148));
#36904=CARTESIAN_POINT('Ctrl Pts',(-4.58614596134621,0.158333333331396,
8.33761149946187));
#36905=CARTESIAN_POINT('Ctrl Pts',(-4.62532597163485,0.319434907273256,
8.35273109638902));
#36906=CARTESIAN_POINT('Ctrl Pts',(-4.68486233467704,0.636309800087417,
8.39732817014555));
#36907=CARTESIAN_POINT('Ctrl Pts',(-4.74810487786108,0.794772683991113,
8.42222305832064));
#36908=CARTESIAN_POINT('Ctrl Pts',(-4.78714005540755,1.06847604193247,8.4835487297326));
#36909=CARTESIAN_POINT('Ctrl Pts',(-4.79446897067439,1.18514270859813,8.51435899761028));
#36910=CARTESIAN_POINT('Ctrl Pts',(-4.79222991924408,1.29999999998536,8.54943392255144));
#36911=CARTESIAN_POINT('Ctrl Pts',(-4.85231643937463,-1.29999999998846,
8.31660108815661));
#36912=CARTESIAN_POINT('Ctrl Pts',(-4.84979949165294,-1.18514270860024,
8.29561841335129));
#36913=CARTESIAN_POINT('Ctrl Pts',(-4.83745911474827,-1.06847604193354,
8.28156297720895));
#36914=CARTESIAN_POINT('Ctrl Pts',(-4.78625628883194,-0.794772683991127,
8.26509541504073));
#36915=CARTESIAN_POINT('Ctrl Pts',(-4.71546849695651,-0.636309800087411,
8.27379696214256));
#36916=CARTESIAN_POINT('Ctrl Pts',(-4.64105818945796,-0.31943490727325,
8.29008982354754));
#36917=CARTESIAN_POINT('Ctrl Pts',(-4.59413642176686,-0.158333333331395,
8.30670599098071));
#36918=CARTESIAN_POINT('Ctrl Pts',(-4.58662494660489,0.158333333331397,
8.33751055346706));
#36919=CARTESIAN_POINT('Ctrl Pts',(-4.62582649875683,0.319434907273257,
8.35261471713071));
#36920=CARTESIAN_POINT('Ctrl Pts',(-4.68536166131313,0.636309800087419,
8.39720317678635));
#36921=CARTESIAN_POINT('Ctrl Pts',(-4.74861769015291,0.794772683991115,
8.42207989545944));
#36922=CARTESIAN_POINT('Ctrl Pts',(-4.78758408758185,1.06847604193247,8.48342696453893));
#36923=CARTESIAN_POINT('Ctrl Pts',(-4.79486558149654,1.18514270859813,8.51425558722074));
#36924=CARTESIAN_POINT('Ctrl Pts',(-4.79256145972622,1.29999999998536,8.54935795951273));
#36925=CARTESIAN_POINT('Ctrl Pts',(-4.85250579798908,-1.29999999998845,
8.31654263126025));
#36926=CARTESIAN_POINT('Ctrl Pts',(-4.85002549762174,-1.18514270860023,
8.29554916044781));
#36927=CARTESIAN_POINT('Ctrl Pts',(-4.83771194672594,-1.06847604193354,
8.28148599004196));
#36928=CARTESIAN_POINT('Ctrl Pts',(-4.7865484049838,-0.794772683991122,
8.265007633418));
#36929=CARTESIAN_POINT('Ctrl Pts',(-4.71575410397166,-0.636309800087407,
8.27370884675981));
#36930=CARTESIAN_POINT('Ctrl Pts',(-4.64134475800369,-0.319434907273248,
8.29000928574408));
#36931=CARTESIAN_POINT('Ctrl Pts',(-4.59441024648493,-0.158333333331394,
8.30664352448534));
#36932=CARTESIAN_POINT('Ctrl Pts',(-4.58689863389259,0.158333333331396,
8.33745318337796));
#36933=CARTESIAN_POINT('Ctrl Pts',(-4.62611251846933,0.319434907273255,
8.35254818476237));
#36934=CARTESIAN_POINT('Ctrl Pts',(-4.6856469976215,0.636309800087415,8.39713168181365));
#36935=CARTESIAN_POINT('Ctrl Pts',(-4.74891071436139,0.79477268399111,8.42199827809077));
#36936=CARTESIAN_POINT('Ctrl Pts',(-4.78783780671656,1.06847604193247,8.48335758804548));
#36937=CARTESIAN_POINT('Ctrl Pts',(-4.79509220458799,1.18514270859813,8.51419666155191));
#36938=CARTESIAN_POINT('Ctrl Pts',(-4.7927509044412,1.29999999998536,8.54931463687183));
#36939=CARTESIAN_POINT('Ctrl Pts',(-4.86471868730759,-1.29999999998952,
8.31278254654165));
#36940=CARTESIAN_POINT('Ctrl Pts',(-4.86460208837969,-1.1851427086012,8.29108942207398));
#36941=CARTESIAN_POINT('Ctrl Pts',(-4.85401881867296,-1.06847604193441,
8.27652499052704));
#36942=CARTESIAN_POINT('Ctrl Pts',(-4.80538924512544,-0.794772683991774,
8.25934694678619));
#36943=CARTESIAN_POINT('Ctrl Pts',(-4.7341748410259,-0.636309800087929,
8.2680389006263));
#36944=CARTESIAN_POINT('Ctrl Pts',(-4.65982891346145,-0.319434907273511,
8.28480552536));
#36945=CARTESIAN_POINT('Ctrl Pts',(-4.61207524473024,-0.158333333331524,
8.3025546175784));
#36946=CARTESIAN_POINT('Ctrl Pts',(-4.60455487191363,0.158333333331526,
8.33368824322348));
#36947=CARTESIAN_POINT('Ctrl Pts',(-4.64456077521837,0.319434907273517,
8.34824442195183));
#36948=CARTESIAN_POINT('Ctrl Pts',(-4.70405142721366,0.636309800087937,
8.39250819384349));
#36949=CARTESIAN_POINT('Ctrl Pts',(-4.76781486087401,0.794772683991763,
8.41666929233755));
#36950=CARTESIAN_POINT('Ctrl Pts',(-4.80420730546169,1.06847604193334,8.47881786275056));
#36951=CARTESIAN_POINT('Ctrl Pts',(-4.80971358233116,1.1851427085991,8.51034101279893));
#36952=CARTESIAN_POINT('Ctrl Pts',(-4.80497319528103,1.29999999998642,8.5464854995953));
#36953=CARTESIAN_POINT('Ctrl Pts',(-4.88296319426862,-1.29999999999803,
8.30623816835216));
#36954=CARTESIAN_POINT('Ctrl Pts',(-4.88638185991351,-1.18514270860896,
8.28290786847773));
#36955=CARTESIAN_POINT('Ctrl Pts',(-4.87838251735454,-1.06847604194141,
8.26729920094536));
#36956=CARTESIAN_POINT('Ctrl Pts',(-4.83352455266495,-0.794772683996978,
8.24907857185986));
#36957=CARTESIAN_POINT('Ctrl Pts',(-4.76163519605766,-0.636309800092096,
8.2591829394193));
#36958=CARTESIAN_POINT('Ctrl Pts',(-4.68739480387011,-0.319434907275602,
8.27685037539968));
#36959=CARTESIAN_POINT('Ctrl Pts',(-4.63849073644685,-0.158333333332561,
8.29527453260398));
#36960=CARTESIAN_POINT('Ctrl Pts',(-4.63095498045046,0.158333333332563,
8.32700558912046));
#36961=CARTESIAN_POINT('Ctrl Pts',(-4.67210354006842,0.319434907275611,
8.34128797459167));
#36962=CARTESIAN_POINT('Ctrl Pts',(-4.73144175849589,0.636309800092106,
8.3862674209549));
#36963=CARTESIAN_POINT('Ctrl Pts',(-4.79576457762992,0.794772683996967,
8.41158971382161));
#36964=CARTESIAN_POINT('Ctrl Pts',(-4.82846153604461,1.06847604194034,8.47426058233221));
#36965=CARTESIAN_POINT('Ctrl Pts',(-4.83146067933456,1.18514270860686,8.50582862891778));
#36966=CARTESIAN_POINT('Ctrl Pts',(-4.82330566415844,1.29999999999493,8.54183682529518));
#36967=CARTESIAN_POINT('Ctrl Pts',(-4.90715283621587,-1.3,8.29842404846038));
#36968=CARTESIAN_POINT('Ctrl Pts',(-4.9152638301882,-1.18514270861076,8.27298278446696));
#36969=CARTESIAN_POINT('Ctrl Pts',(-4.91069673261394,-1.06847604194303,
8.25599416747618));
#36970=CARTESIAN_POINT('Ctrl Pts',(-4.87085689585679,-0.794772683998181,
8.23627436918876));
#36971=CARTESIAN_POINT('Ctrl Pts',(-4.79810158493444,-0.636309800093057,
8.24784641680822));
#36972=CARTESIAN_POINT('Ctrl Pts',(-4.7239959857142,-0.319434907276084,
8.26668557716251));
#36973=CARTESIAN_POINT('Ctrl Pts',(-4.67351228603286,-0.1583333333328,8.28656988747768));
#36974=CARTESIAN_POINT('Ctrl Pts',(-4.66597277435144,0.158333333332802,
8.31875211991404));
#36975=CARTESIAN_POINT('Ctrl Pts',(-4.70866985933996,0.319434907276095,
8.33222208436452));
#36976=CARTESIAN_POINT('Ctrl Pts',(-4.76792134717021,0.636309800093068,
8.37654844845054));
#36977=CARTESIAN_POINT('Ctrl Pts',(-4.83327179504176,0.794772683998166,
8.39999714139346));
#36978=CARTESIAN_POINT('Ctrl Pts',(-4.86090739952758,1.06847604194195,8.46469604840318));
#36979=CARTESIAN_POINT('Ctrl Pts',(-4.86040992141996,1.18514270860865,8.49801701093837));
#36980=CARTESIAN_POINT('Ctrl Pts',(-4.84745253602286,1.2999999999969,8.53665317649499));
#36981=CARTESIAN_POINT('Ctrl Pts',(-4.91927797405485,-1.30000000000437,
8.29377458052673));
#36982=CARTESIAN_POINT('Ctrl Pts',(-4.92971468412874,-1.18514270861474,
8.26751665921141));
#36983=CARTESIAN_POINT('Ctrl Pts',(-4.92685055912788,-1.06847604194662,
8.24995659760688));
#36984=CARTESIAN_POINT('Ctrl Pts',(-4.8895062675643,-0.794772684000851,
8.22948313835506));
#36985=CARTESIAN_POINT('Ctrl Pts',(-4.81632945957884,-0.636309800095197,
8.24128634225486));
#36986=CARTESIAN_POINT('Ctrl Pts',(-4.74231241411425,-0.319434907277159,
8.26047280583125));
#36987=CARTESIAN_POINT('Ctrl Pts',(-4.69108112428619,-0.158333333333332,
8.28090406141698));
#36988=CARTESIAN_POINT('Ctrl Pts',(-4.683529805314,0.158333333333334,8.31369722637576));
#36989=CARTESIAN_POINT('Ctrl Pts',(-4.72695029650717,0.319434907277167,
8.32750102064963));
#36990=CARTESIAN_POINT('Ctrl Pts',(-4.78611439032821,0.636309800095206,
8.37217485718424));
#36991=CARTESIAN_POINT('Ctrl Pts',(-4.85190733217758,0.79477268400084,8.3954008624989));
#36992=CARTESIAN_POINT('Ctrl Pts',(-4.87708284447686,1.06847604194555,8.46055100386331));
#36993=CARTESIAN_POINT('Ctrl Pts',(-4.87490135690222,1.18514270861264,8.49417556843746));
#36994=CARTESIAN_POINT('Ctrl Pts',(-4.85964083532324,1.30000000000127,8.53322361543972));
#36995=CARTESIAN_POINT('Ctrl Pts',(-4.92533609403178,-1.30000000000437,
8.29148735027311));
#36996=CARTESIAN_POINT('Ctrl Pts',(-4.93693489080363,-1.18514270861474,
8.26482422250723));
#36997=CARTESIAN_POINT('Ctrl Pts',(-4.93492178515129,-1.06847604194662,
8.24698002939983));
#36998=CARTESIAN_POINT('Ctrl Pts',(-4.89882489072262,-0.794772684000851,
8.22612987688622));
#36999=CARTESIAN_POINT('Ctrl Pts',(-4.82544129359841,-0.636309800095197,
8.23799733825931));
#37000=CARTESIAN_POINT('Ctrl Pts',(-4.75146299020767,-0.319434907277159,
8.25744308061905));
#37001=CARTESIAN_POINT('Ctrl Pts',(-4.69984189087486,-0.158333333333332,
8.27839589375356));
#37002=CARTESIAN_POINT('Ctrl Pts',(-4.69228837762174,0.158333333333334,
8.31142398215957));
#37003=CARTESIAN_POINT('Ctrl Pts',(-4.73609341170092,0.319434907277167,
8.32501575423084));
#37004=CARTESIAN_POINT('Ctrl Pts',(-4.79522055198673,0.636309800095206,
8.36975685506309));
#37005=CARTESIAN_POINT('Ctrl Pts',(-4.86122784986915,0.79477268400084,8.39303182191491));
#37006=CARTESIAN_POINT('Ctrl Pts',(-4.88516330785013,1.06847604194555,8.4585208729234));
#37007=CARTESIAN_POINT('Ctrl Pts',(-4.88213395050331,1.18514270861264,8.49235062833803));
#37008=CARTESIAN_POINT('Ctrl Pts',(-4.86571446294582,1.30000000000127,8.53166235559416));
#37009=CARTESIAN_POINT('',(-4.76940701573779,1.2,8.5248610184586));
#37010=CARTESIAN_POINT('Ctrl Pts',(-4.76940701573779,1.2,8.5248610184586));
#37011=CARTESIAN_POINT('Ctrl Pts',(-4.74959775132473,1.21680199780992,8.53339667265294));
#37012=CARTESIAN_POINT('Ctrl Pts',(-4.72988508062029,1.23316175714919,8.54300746795801));
#37013=CARTESIAN_POINT('Ctrl Pts',(-4.70624255731438,1.25313382902886,8.552991453738));
#37014=CARTESIAN_POINT('Ctrl Pts',(-4.68241322188002,1.2731048455244,8.56362856372702));
#37015=CARTESIAN_POINT('Ctrl Pts',(-4.6525154957812,1.29841093120771,8.57550588696848));
#37016=CARTESIAN_POINT('Ctrl Pts',(-4.6515830528172,1.29920026509202,8.57587556280998));
#37017=CARTESIAN_POINT('Ctrl Pts',(-4.65063820841642,1.29999999999331,8.5762500697483));
#37018=CARTESIAN_POINT('',(-4.80892752946133,0.653834841327865,8.37333542346878));
#37019=CARTESIAN_POINT('Ctrl Pts',(-4.80892752948835,0.653834841312438,
8.37333542353798));
#37020=CARTESIAN_POINT('Ctrl Pts',(-4.80542009361191,0.712175033180002,
8.3877106862342));
#37021=CARTESIAN_POINT('Ctrl Pts',(-4.80171376700822,0.767439432116428,
8.40262161143459));
#37022=CARTESIAN_POINT('Ctrl Pts',(-4.79380687348683,0.881523157784702,
8.43376581863121));
#37023=CARTESIAN_POINT('Ctrl Pts',(-4.78991228436266,0.939238214520343,
8.44883908268581));
#37024=CARTESIAN_POINT('Ctrl Pts',(-4.78300534853591,1.03041410836302,8.47492136578765));
#37025=CARTESIAN_POINT('Ctrl Pts',(-4.7816957916988,1.04693620269592,8.47990356864517));
#37026=CARTESIAN_POINT('Ctrl Pts',(-4.77434691931254,1.13963387115676,8.50699986195079));
#37027=CARTESIAN_POINT('Ctrl Pts',(-4.77208504469432,1.16791763773685,8.51522030149607));
#37028=CARTESIAN_POINT('Ctrl Pts',(-4.76940701573779,1.2,8.5248610184586));
#37029=CARTESIAN_POINT('',(-4.84008270153025,-0.653834841531101,8.23735213035285));
#37030=CARTESIAN_POINT('Ctrl Pts',(-4.84008270153025,-0.653834841531099,
8.23735213035285));
#37031=CARTESIAN_POINT('Ctrl Pts',(-4.79943687647267,-0.575774454259114,
8.24659452518038));
#37032=CARTESIAN_POINT('Ctrl Pts',(-4.76540108947681,-0.493710702847288,
8.25532385189694));
#37033=CARTESIAN_POINT('Ctrl Pts',(-4.71692660388303,-0.338121740996384,
8.27001974097562));
#37034=CARTESIAN_POINT('Ctrl Pts',(-4.70018760001661,-0.265673667041442,
8.27641839251951));
#37035=CARTESIAN_POINT('Ctrl Pts',(-4.67924730487146,-0.129742825061959,
8.28899804955198));
#37036=CARTESIAN_POINT('Ctrl Pts',(-4.67358921948777,-0.066665686974624,
8.29501142948854));
#37037=CARTESIAN_POINT('Ctrl Pts',(-4.67025713110064,0.0595066342539753,
8.30787286844477));
#37038=CARTESIAN_POINT('Ctrl Pts',(-4.67254530496467,0.122729721736906,
8.31479683851603));
#37039=CARTESIAN_POINT('Ctrl Pts',(-4.68651536486654,0.260113581388072,
8.32999321016995));
#37040=CARTESIAN_POINT('Ctrl Pts',(-4.69982530968251,0.333986144077667,
8.33833894741233));
#37041=CARTESIAN_POINT('Ctrl Pts',(-4.74125637880943,0.491528819855043,
8.35566552490392));
#37042=CARTESIAN_POINT('Ctrl Pts',(-4.771640731347,0.574924749423742,8.364924270098));
#37043=CARTESIAN_POINT('Ctrl Pts',(-4.80892752938989,0.65383484135055,8.37333542357261));
#37044=CARTESIAN_POINT('',(-4.82442585316259,-1.2,8.3078877142276));
#37045=CARTESIAN_POINT('Ctrl Pts',(-4.82442585316259,-1.2,8.3078877142276));
#37046=CARTESIAN_POINT('Ctrl Pts',(-4.82689451181185,-1.14179354867607,
8.29713765313641));
#37047=CARTESIAN_POINT('Ctrl Pts',(-4.8307416685721,-1.0415419554568,8.28018439951763));
#37048=CARTESIAN_POINT('Ctrl Pts',(-4.83823646441324,-0.774556440178833,
8.24604982293182));
#37049=CARTESIAN_POINT('Ctrl Pts',(-4.83902226279081,-0.721499503691961,
8.24229993066929));
#37050=CARTESIAN_POINT('Ctrl Pts',(-4.84008270153025,-0.653834841531101,
8.23735213035285));
#37051=CARTESIAN_POINT('Ctrl Pts',(-4.70981757142094,-1.29999999999641,
8.35763484915121));
#37052=CARTESIAN_POINT('Ctrl Pts',(-4.71097463231061,-1.29899465260559,
8.35713934673585));
#37053=CARTESIAN_POINT('Ctrl Pts',(-4.71213258962288,-1.29798697378795,
8.35664921501205));
#37054=CARTESIAN_POINT('Ctrl Pts',(-4.73158341462519,-1.28099071752189,
8.34869701228178));
#37055=CARTESIAN_POINT('Ctrl Pts',(-4.74981785750062,-1.26509988311611,
8.34088437013692));
#37056=CARTESIAN_POINT('Ctrl Pts',(-4.77997485499785,-1.23871758437594,
8.3280932555352));
#37057=CARTESIAN_POINT('Ctrl Pts',(-4.80250841816378,-1.21895688910026,
8.31863107643311));
#37058=CARTESIAN_POINT('Ctrl Pts',(-4.82442585316259,-1.2,8.3078877142276));
#37059=CARTESIAN_POINT('Origin',(0.,1.25,7.2));
#37060=CARTESIAN_POINT('Origin',(0.,1.2,7.2));
#37061=CARTESIAN_POINT('Origin',(0.,0.92691742076555,7.2));
#37062=CARTESIAN_POINT('Origin',(0.,0.653834841531101,7.2));
#37063=CARTESIAN_POINT('Origin',(0.,0.,7.2));
#37064=CARTESIAN_POINT('Origin',(0.,-0.653834841531101,7.2));
#37065=CARTESIAN_POINT('Origin',(0.,-0.926917420765551,7.2));
#37066=CARTESIAN_POINT('Origin',(0.,-1.2,7.2));
#37067=CARTESIAN_POINT('Origin',(0.,-1.25,7.2));
#37068=CARTESIAN_POINT('Ctrl Pts',(-4.98668722203916,-1.30000000000015,
7.96253027075762));
#37069=CARTESIAN_POINT('Ctrl Pts',(-4.98569765033805,-1.18514270861188,
8.00512172787461));
#37070=CARTESIAN_POINT('Ctrl Pts',(-4.97470530482919,-1.06847604194517,
8.03725889790462));
#37071=CARTESIAN_POINT('Ctrl Pts',(-4.92620237914858,-0.794772684000851,
8.08735069514887));
#37072=CARTESIAN_POINT('Ctrl Pts',(-4.85643493010791,-0.636309800095197,
8.08176584863345));
#37073=CARTESIAN_POINT('Ctrl Pts',(-4.78422175451511,-0.319434907277159,
8.09858970351398));
#37074=CARTESIAN_POINT('Ctrl Pts',(-4.73867559286569,-0.158333333333332,
8.09318929263998));
#37075=CARTESIAN_POINT('Ctrl Pts',(-4.73214233678195,0.158333333333335,
8.1264342434019));
#37076=CARTESIAN_POINT('Ctrl Pts',(-4.77077828071914,0.319434907277167,
8.1665717833203));
#37077=CARTESIAN_POINT('Ctrl Pts',(-4.83045152777451,0.636309800095207,
8.21442603970484));
#37078=CARTESIAN_POINT('Ctrl Pts',(-4.89266384818737,0.794772684000841,
8.25511530308637));
#37079=CARTESIAN_POINT('Ctrl Pts',(-4.93412052316908,1.06847604194528,8.25074967063201));
#37080=CARTESIAN_POINT('Ctrl Pts',(-4.9432174738979,1.18514270861211,8.23526699290927));
#37081=CARTESIAN_POINT('Ctrl Pts',(-4.94346631687715,1.30000000000049,8.20619135799067));
#37082=CARTESIAN_POINT('Ctrl Pts',(-4.97686019541383,-1.30000000000015,
7.95473697326264));
#37083=CARTESIAN_POINT('Ctrl Pts',(-4.97396758436907,-1.18514270861188,
7.99590387472333));
#37084=CARTESIAN_POINT('Ctrl Pts',(-4.9615930209824,-1.06847604194517,8.02697642302472));
#37085=CARTESIAN_POINT('Ctrl Pts',(-4.9111000972684,-0.794772684000851,
8.07544025047651));
#37086=CARTESIAN_POINT('Ctrl Pts',(-4.84176412504578,-0.636309800095197,
8.06994031968232));
#37087=CARTESIAN_POINT('Ctrl Pts',(-4.76953814967826,-0.319434907277159,
8.08661121585988));
#37088=CARTESIAN_POINT('Ctrl Pts',(-4.72452210845454,-0.158333333333332,
8.08191100419208));
#37089=CARTESIAN_POINT('Ctrl Pts',(-4.71817594716844,0.158333333333335,
8.11472494346892));
#37090=CARTESIAN_POINT('Ctrl Pts',(-4.75652394684048,0.319434907277167,
8.15359245071089));
#37091=CARTESIAN_POINT('Ctrl Pts',(-4.81647889553182,0.636309800095207,
8.2010044968254));
#37092=CARTESIAN_POINT('Ctrl Pts',(-4.87836566507891,0.794772684000841,
8.2414081385139));
#37093=CARTESIAN_POINT('Ctrl Pts',(-4.92179501812863,1.06847604194528,8.23874548314256));
#37094=CARTESIAN_POINT('Ctrl Pts',(-4.93221572520194,1.18514270861211,8.22447422101514));
#37095=CARTESIAN_POINT('Ctrl Pts',(-4.93425818162945,1.30000000000049,8.19708426160946));
#37096=CARTESIAN_POINT('Ctrl Pts',(-4.95707257542365,-1.3000000000004,7.93971797339418));
#37097=CARTESIAN_POINT('Ctrl Pts',(-4.95090720637166,-1.18514270861211,
7.9764403553286));
#37098=CARTESIAN_POINT('Ctrl Pts',(-4.93606540805145,-1.06847604194537,
8.00447473012978));
#37099=CARTESIAN_POINT('Ctrl Pts',(-4.88173359751691,-0.794772684001005,
8.04916870967032));
#37100=CARTESIAN_POINT('Ctrl Pts',(-4.81233385660756,-0.636309800095321,
8.04643608415275));
#37101=CARTESIAN_POINT('Ctrl Pts',(-4.73982846661425,-0.319434907277221,
8.06349820095983));
#37102=CARTESIAN_POINT('Ctrl Pts',(-4.69623080845726,-0.158333333333363,
8.05926321453546));
#37103=CARTESIAN_POINT('Ctrl Pts',(-4.69013837127611,0.158333333333365,
8.09148533256226));
#37104=CARTESIAN_POINT('Ctrl Pts',(-4.72746932272836,0.319434907277228,
8.12886904361067));
#37105=CARTESIAN_POINT('Ctrl Pts',(-4.78791983132539,0.636309800095329,
8.17555363023394));
#37106=CARTESIAN_POINT('Ctrl Pts',(-4.84954939611665,0.794772684000997,
8.21441230389292));
#37107=CARTESIAN_POINT('Ctrl Pts',(-4.89693206221802,1.06847604194549,8.21518779027577));
#37108=CARTESIAN_POINT('Ctrl Pts',(-4.9099356983377,1.18514270861234,8.20353394339688));
#37109=CARTESIAN_POINT('Ctrl Pts',(-4.91543277012257,1.30000000000074,8.17989057031857));
#37110=CARTESIAN_POINT('Ctrl Pts',(-4.93706273410424,-1.30000000000065,
7.92437433149745));
#37111=CARTESIAN_POINT('Ctrl Pts',(-4.92672246011735,-1.18514270861234,
7.9591527062714));
#37112=CARTESIAN_POINT('Ctrl Pts',(-4.9088900170747,-1.06847604194558,7.98559559832303));
#37113=CARTESIAN_POINT('Ctrl Pts',(-4.85038509695605,-0.79477268400116,
8.0274273362486));
#37114=CARTESIAN_POINT('Ctrl Pts',(-4.78229038223289,-0.636309800095441,
8.02363556847094));
#37115=CARTESIAN_POINT('Ctrl Pts',(-4.70990346987882,-0.319434907277281,
8.03996699510912));
#37116=CARTESIAN_POINT('Ctrl Pts',(-4.66738796843898,-0.158333333333393,
8.03713816760568));
#37117=CARTESIAN_POINT('Ctrl Pts',(-4.66156310125004,0.158333333333395,
8.06871883459887));
#37118=CARTESIAN_POINT('Ctrl Pts',(-4.69796211219866,0.31943490727729,8.10434728984312));
#37119=CARTESIAN_POINT('Ctrl Pts',(-4.7590782051624,0.636309800095451,8.14986047271179));
#37120=CARTESIAN_POINT('Ctrl Pts',(-4.82064942303686,0.794772684001145,
8.18663205747421));
#37121=CARTESIAN_POINT('Ctrl Pts',(-4.87208201945832,1.06847604194569,8.19073989913263));
#37122=CARTESIAN_POINT('Ctrl Pts',(-4.88767626585109,1.18514270861257,8.18178352934301));
#37123=CARTESIAN_POINT('Ctrl Pts',(-4.89660149341129,1.30000000000099,8.16209265732034));
#37124=CARTESIAN_POINT('Ctrl Pts',(-4.92681556703292,-1.30000000000068,
7.91663963991158));
#37125=CARTESIAN_POINT('Ctrl Pts',(-4.91465480283025,-1.18514270861237,
7.94947552149818));
#37126=CARTESIAN_POINT('Ctrl Pts',(-4.89546982950633,-1.06847604194561,
7.97456102308863));
#37127=CARTESIAN_POINT('Ctrl Pts',(-4.83492137492904,-0.794772684001177,
8.01460862185063));
#37128=CARTESIAN_POINT('Ctrl Pts',(-4.76700538266001,-0.636309800095456,
8.01166877733264));
#37129=CARTESIAN_POINT('Ctrl Pts',(-4.69444812518406,-0.319434907277288,
8.02827046106348));
#37130=CARTESIAN_POINT('Ctrl Pts',(-4.65245112947184,-0.158333333333397,
8.02626803251437));
#37131=CARTESIAN_POINT('Ctrl Pts',(-4.64675546908366,0.158333333333399,
8.05753591142075));
#37132=CARTESIAN_POINT('Ctrl Pts',(-4.68285379896454,0.319434907277297,
8.09178027156682));
#37133=CARTESIAN_POINT('Ctrl Pts',(-4.74422291380177,0.636309800095465,
8.13688493060965));
#37134=CARTESIAN_POINT('Ctrl Pts',(-4.80539436748246,0.794772684001164,
8.17349735392384));
#37135=CARTESIAN_POINT('Ctrl Pts',(-4.85890464595191,1.06847604194571,8.17931255377106));
#37136=CARTESIAN_POINT('Ctrl Pts',(-4.87590847415212,1.18514270861259,8.17154257504764));
#37137=CARTESIAN_POINT('Ctrl Pts',(-4.88675351375432,1.30000000000102,8.15348543306134));
#37138=CARTESIAN_POINT('Ctrl Pts',(-4.92634883800722,-1.30000000000068,
7.91629093381771));
#37139=CARTESIAN_POINT('Ctrl Pts',(-4.91410516658122,-1.18514270861237,
7.94903877767638));
#37140=CARTESIAN_POINT('Ctrl Pts',(-4.89485865912818,-1.0684760419456,7.9740626005799));
#37141=CARTESIAN_POINT('Ctrl Pts',(-4.83421742452598,-0.794772684001177,
8.01402860389416));
#37142=CARTESIAN_POINT('Ctrl Pts',(-4.7663102877219,-0.636309800095456,
8.01112550257999));
#37143=CARTESIAN_POINT('Ctrl Pts',(-4.69374512410901,-0.319434907277288,
8.02773985836219));
#37144=CARTESIAN_POINT('Ctrl Pts',(-4.6517706931809,-0.158333333333396,
8.02577773664887));
#37145=CARTESIAN_POINT('Ctrl Pts',(-4.6460808087952,0.158333333333399,8.05703161637855));
#37146=CARTESIAN_POINT('Ctrl Pts',(-4.68216609320299,0.319434907277297,
8.09121128549913));
#37147=CARTESIAN_POINT('Ctrl Pts',(-4.74354725462836,0.636309800095465,
8.1362959106994));
#37148=CARTESIAN_POINT('Ctrl Pts',(-4.80470095934226,0.794772684001163,
8.1729000489884));
#37149=CARTESIAN_POINT('Ctrl Pts',(-4.85830584169813,1.06847604194571,8.17879251565979));
#37150=CARTESIAN_POINT('Ctrl Pts',(-4.87537371287317,1.18514270861259,8.17107659024682));
#37151=CARTESIAN_POINT('Ctrl Pts',(-4.88630588790803,1.30000000000102,8.15309410893623));
#37152=CARTESIAN_POINT('Ctrl Pts',(-4.92588209917281,-1.30000000000068,
7.91594220576637));
#37153=CARTESIAN_POINT('Ctrl Pts',(-4.91355533436984,-1.18514270861237,
7.94860259453505));
#37154=CARTESIAN_POINT('Ctrl Pts',(-4.89424716922786,-1.0684760419456,7.97356512423356));
#37155=CARTESIAN_POINT('Ctrl Pts',(-4.83351301375721,-0.794772684001177,
8.01344996717057));
#37156=CARTESIAN_POINT('Ctrl Pts',(-4.76561475713913,-0.636309800095456,
8.0105834766292));
#37157=CARTESIAN_POINT('Ctrl Pts',(-4.69304195822735,-0.319434907277288,
8.02720973951435));
#37158=CARTESIAN_POINT('Ctrl Pts',(-4.65109065207363,-0.158333333333397,
8.02528638895818));
#37159=CARTESIAN_POINT('Ctrl Pts',(-4.64540657107658,0.158333333333399,
8.05652617740995));
#37160=CARTESIAN_POINT('Ctrl Pts',(-4.68147820223513,0.319434907277297,
8.09064279235515));
#37161=CARTESIAN_POINT('Ctrl Pts',(-4.74287134831426,0.636309800095465,
8.13570756737513));
#37162=CARTESIAN_POINT('Ctrl Pts',(-4.80400777628441,0.794772684001164,
8.17230219840906));
#37163=CARTESIAN_POINT('Ctrl Pts',(-4.85770732971282,1.06847604194571,8.17827174263832));
#37164=CARTESIAN_POINT('Ctrl Pts',(-4.87483920216915,1.18514270861259,8.17060996610002));
#37165=CARTESIAN_POINT('Ctrl Pts',(-4.8858584001672,1.30000000000102,8.15270241851999));
#37166=CARTESIAN_POINT('Ctrl Pts',(-4.92494779478317,-1.30000000000068,
7.91524717629567));
#37167=CARTESIAN_POINT('Ctrl Pts',(-4.91245445453818,-1.18514270861237,
7.94773366183714));
#37168=CARTESIAN_POINT('Ctrl Pts',(-4.89302276215951,-1.0684760419456,7.97257413225111));
#37169=CARTESIAN_POINT('Ctrl Pts',(-4.83210268402666,-0.794772684001177,
8.01229676370186));
#37170=CARTESIAN_POINT('Ctrl Pts',(-4.76422290354184,-0.636309800095456,
8.00950146958473));
#37171=CARTESIAN_POINT('Ctrl Pts',(-4.69163503655158,-0.319434907277288,
8.02615091416697));
#37172=CARTESIAN_POINT('Ctrl Pts',(-4.64972978259324,-0.158333333333396,
8.02430564665363));
#37173=CARTESIAN_POINT('Ctrl Pts',(-4.6440572383016,0.158333333333399,8.05551738278739));
#37174=CARTESIAN_POINT('Ctrl Pts',(-4.68010131535152,0.319434907277297,
8.08950845780255));
#37175=CARTESIAN_POINT('Ctrl Pts',(-4.74151884911486,0.636309800095465,
8.13453243628381));
#37176=CARTESIAN_POINT('Ctrl Pts',(-4.80262176161668,0.794772684001163,
8.17110541371026));
#37177=CARTESIAN_POINT('Ctrl Pts',(-4.8565108926544,1.06847604194571,8.17722855690648));
#37178=CARTESIAN_POINT('Ctrl Pts',(-4.87377067854012,1.18514270861259,8.16967533570393));
#37179=CARTESIAN_POINT('Ctrl Pts',(-4.88496364227441,1.30000000000102,8.15191841149398));
#37180=CARTESIAN_POINT('Ctrl Pts',(-4.9229201203918,-1.30000000000068,7.91375075345988));
#37181=CARTESIAN_POINT('Ctrl Pts',(-4.91006283010197,-1.18514270861237,
7.94586907183033));
#37182=CARTESIAN_POINT('Ctrl Pts',(-4.89036171580574,-1.0684760419456,7.97045009443501));
#37183=CARTESIAN_POINT('Ctrl Pts',(-4.82903759802996,-0.794772684001176,
8.00982451301876));
#37184=CARTESIAN_POINT('Ctrl Pts',(-4.76120153532038,-0.636309800095455,
8.00717269005564));
#37185=CARTESIAN_POINT('Ctrl Pts',(-4.68858380635237,-0.319434907277288,
8.02386427242913));
#37186=CARTESIAN_POINT('Ctrl Pts',(-4.64678096711319,-0.158333333333396,
8.02218093374858));
#37187=CARTESIAN_POINT('Ctrl Pts',(-4.64113331134503,0.158333333333399,
8.05333183005413));
#37188=CARTESIAN_POINT('Ctrl Pts',(-4.67711279962206,0.319434907277297,
8.08706365877751));
#37189=CARTESIAN_POINT('Ctrl Pts',(-4.73858453889471,0.636309800095464,
8.13199587542556));
#37190=CARTESIAN_POINT('Ctrl Pts',(-4.79962230512729,0.794772684001163,
8.16850293988758));
#37191=CARTESIAN_POINT('Ctrl Pts',(-4.85392337802701,1.06847604194571,8.17495592741023));
#37192=CARTESIAN_POINT('Ctrl Pts',(-4.8714595015132,1.18514270861259,8.16764000235142));
#37193=CARTESIAN_POINT('Ctrl Pts',(-4.88302682608031,1.30000000000102,8.150214893042));
#37194=CARTESIAN_POINT('Ctrl Pts',(-4.91853551063343,-1.30000000000067,
7.91057496125883));
#37195=CARTESIAN_POINT('Ctrl Pts',(-4.90487437231569,-1.18514270861236,
7.94195741056749));
#37196=CARTESIAN_POINT('Ctrl Pts',(-4.88458126831889,-1.0684760419456,7.96601291574697));
#37197=CARTESIAN_POINT('Ctrl Pts',(-4.82237897102587,-0.794772684001172,
8.00465923831033));
#37198=CARTESIAN_POINT('Ctrl Pts',(-4.75466130079436,-0.636309800095453,
8.0022453434556));
#37199=CARTESIAN_POINT('Ctrl Pts',(-4.68199751600308,-0.319434907277287,
8.01897522261329));
#37200=CARTESIAN_POINT('Ctrl Pts',(-4.64043299418673,-0.158333333333396,
8.01759269083693));
#37201=CARTESIAN_POINT('Ctrl Pts',(-4.63483723281784,0.158333333333398,
8.04861522386223));
#37202=CARTESIAN_POINT('Ctrl Pts',(-4.67064341031251,0.319434907277295,
8.08187764026623));
#37203=CARTESIAN_POINT('Ctrl Pts',(-4.73224020187204,0.636309800095462,
8.12659206370196));
#37204=CARTESIAN_POINT('Ctrl Pts',(-4.79318824006026,0.794772684001161,
8.16282900060846));
#37205=CARTESIAN_POINT('Ctrl Pts',(-4.84838418783909,1.06847604194571,8.16997350796069));
#37206=CARTESIAN_POINT('Ctrl Pts',(-4.86650983018688,1.18514270861259,8.16318320752625));
#37207=CARTESIAN_POINT('Ctrl Pts',(-4.87886883430042,1.30000000000101,8.14651001415467));
#37208=CARTESIAN_POINT('Ctrl Pts',(-4.91221750856866,-1.30000000000066,
7.90618028712686));
#37209=CARTESIAN_POINT('Ctrl Pts',(-4.89732171538367,-1.18514270861235,
7.93676277428599));
#37210=CARTESIAN_POINT('Ctrl Pts',(-4.87613173456936,-1.06847604194559,
7.96021652033425));
#37211=CARTESIAN_POINT('Ctrl Pts',(-4.81263780727549,-0.794772684001163,
7.99793054754568));
#37212=CARTESIAN_POINT('Ctrl Pts',(-4.74518442134474,-0.636309800095445,
7.99557610459018));
#37213=CARTESIAN_POINT('Ctrl Pts',(-4.6725406087231,-0.319434907277283,
8.01211698986252));
#37214=CARTESIAN_POINT('Ctrl Pts',(-4.63141471593923,-0.158333333333394,
8.01089761866659));
#37215=CARTESIAN_POINT('Ctrl Pts',(-4.62588971921968,0.158333333333396,
8.04173769180815));
#37216=CARTESIAN_POINT('Ctrl Pts',(-4.66128991219664,0.319434907277292,
8.07474335059151));
#37217=CARTESIAN_POINT('Ctrl Pts',(-4.72308852205137,0.636309800095455,
8.11909410305302));
#37218=CARTESIAN_POINT('Ctrl Pts',(-4.78411408326621,0.79477268400115,8.15442691127934));
#37219=CARTESIAN_POINT('Ctrl Pts',(-4.84061394483196,1.06847604194569,8.16249551717092));
#37220=CARTESIAN_POINT('Ctrl Pts',(-4.85955619075815,1.18514270861257,8.15652027226193));
#37221=CARTESIAN_POINT('Ctrl Pts',(-4.87298398606488,1.300000000001,8.14107718192479));
#37222=CARTESIAN_POINT('Ctrl Pts',(-4.90590397924942,-1.30000000000065,
7.90176328971422));
#37223=CARTESIAN_POINT('Ctrl Pts',(-4.88977578450812,-1.18514270861234,
7.93153530673559));
#37224=CARTESIAN_POINT('Ctrl Pts',(-4.86768692716434,-1.06847604194558,
7.95439047087062));
#37225=CARTESIAN_POINT('Ctrl Pts',(-4.80288692480121,-0.794772684001158,
7.99121115830334));
#37226=CARTESIAN_POINT('Ctrl Pts',(-4.73567112619427,-0.636309800095442,
7.98899675141701));
#37227=CARTESIAN_POINT('Ctrl Pts',(-4.66302451807155,-0.319434907277281,
8.00541558753617));
#37228=CARTESIAN_POINT('Ctrl Pts',(-4.62232442101259,-0.158333333333393,
8.00439907906812));
#37229=CARTESIAN_POINT('Ctrl Pts',(-4.61687292524796,0.158333333333395,
8.03504454203713));
#37230=CARTESIAN_POINT('Ctrl Pts',(-4.65189635062452,0.31943490727729,8.06770186423874));
#37231=CARTESIAN_POINT('Ctrl Pts',(-4.71389732152674,0.636309800095451,
8.11167817180113));
#37232=CARTESIAN_POINT('Ctrl Pts',(-4.77496018471075,0.794772684001146,
8.14621029392679));
#37233=CARTESIAN_POINT('Ctrl Pts',(-4.83277887881808,1.06847604194569,8.15516634666519));
#37234=CARTESIAN_POINT('Ctrl Pts',(-4.85255522845339,1.18514270861256,8.14996319804911));
#37235=CARTESIAN_POINT('Ctrl Pts',(-4.86708035743869,1.30000000000099,8.13568015744095));
#37236=CARTESIAN_POINT('Ctrl Pts',(-4.90087799425075,-1.30000000000065,
7.89815843086838));
#37237=CARTESIAN_POINT('Ctrl Pts',(-4.88380456050229,-1.18514270861234,
7.9271602890803));
#37238=CARTESIAN_POINT('Ctrl Pts',(-4.86101812269967,-1.06847604194558,
7.94947168469374));
#37239=CARTESIAN_POINT('Ctrl Pts',(-4.79517871071664,-0.794772684001156,
7.98555916491523));
#37240=CARTESIAN_POINT('Ctrl Pts',(-4.72808987790012,-0.636309800095441,
7.98364475480844));
#37241=CARTESIAN_POINT('Ctrl Pts',(-4.65538329456378,-0.319434907277281,
8.00013082479717));
#37242=CARTESIAN_POINT('Ctrl Pts',(-4.61496515703839,-0.158333333333393,
7.99943824782273));
#37243=CARTESIAN_POINT('Ctrl Pts',(-4.60957871500424,0.158333333333395,
8.02991066345015));
#37244=CARTESIAN_POINT('Ctrl Pts',(-4.64440612757375,0.319434907277289,
8.06200266067117));
#37245=CARTESIAN_POINT('Ctrl Pts',(-4.70655702592597,0.63630980009545,8.10569846556605));
#37246=CARTESIAN_POINT('Ctrl Pts',(-4.76751286578663,0.794772684001145,
8.13993353417728));
#37247=CARTESIAN_POINT('Ctrl Pts',(-4.82637845774924,1.06847604194569,8.14962346925743));
#37248=CARTESIAN_POINT('Ctrl Pts',(-4.84684451433475,1.18514270861256,8.14498504018903));
#37249=CARTESIAN_POINT('Ctrl Pts',(-4.8622958939303,1.30000000000099,8.1315137682035));
#37250=CARTESIAN_POINT('Ctrl Pts',(-4.88837681016349,-1.30000000000063,
7.88895028194231));
#37251=CARTESIAN_POINT('Ctrl Pts',(-4.86900693933979,-1.18514270861232,
7.91582915034754));
#37252=CARTESIAN_POINT('Ctrl Pts',(-4.84451742320507,-1.06847604194556,
7.93665969675292));
#37253=CARTESIAN_POINT('Ctrl Pts',(-4.77611433697291,-0.794772684001145,
7.97080959230356));
#37254=CARTESIAN_POINT('Ctrl Pts',(-4.70929268250738,-0.636309800095433,
7.96979288413007));
#37255=CARTESIAN_POINT('Ctrl Pts',(-4.6363516185457,-0.319434907277277,
7.98669439873285));
#37256=CARTESIAN_POINT('Ctrl Pts',(-4.59652414874773,-0.158333333333391,
7.98714544677113));
#37257=CARTESIAN_POINT('Ctrl Pts',(-4.59125935571234,0.158333333333393,
8.01730741108527));
#37258=CARTESIAN_POINT('Ctrl Pts',(-4.62566171926125,0.319434907277285,
8.04780317230802));
#37259=CARTESIAN_POINT('Ctrl Pts',(-4.68820532536085,0.636309800095442,
8.09074073463353));
#37260=CARTESIAN_POINT('Ctrl Pts',(-4.74887696505617,0.794772684001136,
8.12426276571075));
#37261=CARTESIAN_POINT('Ctrl Pts',(-4.8103702126134,1.06847604194567,8.1357578335284));
#37262=CARTESIAN_POINT('Ctrl Pts',(-4.83256879930426,1.18514270861255,8.13251177472534));
#37263=CARTESIAN_POINT('Ctrl Pts',(-4.85034782436782,1.30000000000097,8.1210438681952));
#37264=CARTESIAN_POINT('Ctrl Pts',(-4.86688257452678,-1.30000000000049,
7.87399374566793));
#37265=CARTESIAN_POINT('Ctrl Pts',(-4.84340178599782,-1.18514270861219,
7.897854654973));
#37266=CARTESIAN_POINT('Ctrl Pts',(-4.81588313053963,-1.06847604194544,
7.91655196948616));
#37267=CARTESIAN_POINT('Ctrl Pts',(-4.742981250964,-0.794772684001054,7.94781756945355));
#37268=CARTESIAN_POINT('Ctrl Pts',(-4.67671488697888,-0.63630980009536,
7.94806267967043));
#37269=CARTESIAN_POINT('Ctrl Pts',(-4.60360265705701,-0.31943490727724,
7.96500904542826));
#37270=CARTESIAN_POINT('Ctrl Pts',(-4.56511770040999,-0.158333333333372,
7.96640620775939));
#37271=CARTESIAN_POINT('Ctrl Pts',(-4.56022059376211,0.158333333333375,
7.99554457965105));
#37272=CARTESIAN_POINT('Ctrl Pts',(-4.59380357309349,0.319434907277248,
8.02358096865707));
#37273=CARTESIAN_POINT('Ctrl Pts',(-4.65695067057653,0.636309800095368,
8.0653861091333));
#37274=CARTESIAN_POINT('Ctrl Pts',(-4.71707246892219,0.794772684001043,
8.0978669334104));
#37275=CARTESIAN_POINT('Ctrl Pts',(-4.78294691811059,1.06847604194555,8.11268991939168));
#37276=CARTESIAN_POINT('Ctrl Pts',(-4.80805404966436,1.18514270861242,8.1119314974408));
#37277=CARTESIAN_POINT('Ctrl Pts',(-4.82975370460714,1.30000000000083,8.1039983321535));
#37278=CARTESIAN_POINT('Ctrl Pts',(-4.84151828404587,-1.30000000000042,
7.85646916935349));
#37279=CARTESIAN_POINT('Ctrl Pts',(-4.81307876780055,-1.18514270861214,
7.87712509595763));
#37280=CARTESIAN_POINT('Ctrl Pts',(-4.78193549602595,-1.06847604194539,
7.89347420359149));
#37281=CARTESIAN_POINT('Ctrl Pts',(-4.70374209187939,-0.794772684001021,
7.92129429945595));
#37282=CARTESIAN_POINT('Ctrl Pts',(-4.63841532094869,-0.636309800095332,
7.92211268173844));
#37283=CARTESIAN_POINT('Ctrl Pts',(-4.56516336664136,-0.319434907277226,
7.93892324566879));
#37284=CARTESIAN_POINT('Ctrl Pts',(-4.52826122899799,-0.158333333333366,
7.94152088547465));
#37285=CARTESIAN_POINT('Ctrl Pts',(-4.52349391948293,0.158333333333368,
7.97030284749727));
#37286=CARTESIAN_POINT('Ctrl Pts',(-4.55556801363061,0.319434907277235,
7.99690404660842));
#37287=CARTESIAN_POINT('Ctrl Pts',(-4.61923301245898,0.636309800095341,
8.03787111873039));
#37288=CARTESIAN_POINT('Ctrl Pts',(-4.6788605164949,0.79477268400101,8.06865183019706));
#37289=CARTESIAN_POINT('Ctrl Pts',(-4.75023795639241,1.06847604194551,8.08646674481053));
#37290=CARTESIAN_POINT('Ctrl Pts',(-4.77898396544915,1.18514270861236,8.0880753688951));
#37291=CARTESIAN_POINT('Ctrl Pts',(-4.80557933462579,1.30000000000077,8.08358120063571));
#37292=CARTESIAN_POINT('Ctrl Pts',(-4.82112874987559,-1.30000000000039,
7.84277001524222));
#37293=CARTESIAN_POINT('Ctrl Pts',(-4.78880172461059,-1.1851427086121,7.8605584606925));
#37294=CARTESIAN_POINT('Ctrl Pts',(-4.7547519322164,-1.06847604194537,7.87501539674751));
#37295=CARTESIAN_POINT('Ctrl Pts',(-4.67211016344138,-0.794772684000998,
7.90071735796543));
#37296=CARTESIAN_POINT('Ctrl Pts',(-4.60692508051203,-0.636309800095313,
7.90397466208613));
#37297=CARTESIAN_POINT('Ctrl Pts',(-4.53340717249417,-0.319434907277217,
7.92114127676621));
#37298=CARTESIAN_POINT('Ctrl Pts',(-4.49803145325506,-0.158333333333361,
7.92381830623259));
#37299=CARTESIAN_POINT('Ctrl Pts',(-4.49361450863589,0.158333333333363,
7.95151283923301));
#37300=CARTESIAN_POINT('Ctrl Pts',(-4.52463871769815,0.319434907277226,
7.97646143477411));
#37301=CARTESIAN_POINT('Ctrl Pts',(-4.58902634230981,0.636309800095323,
8.01584695036339));
#37302=CARTESIAN_POINT('Ctrl Pts',(-4.64863712159789,0.794772684000986,
8.04422098867795));
#37303=CARTESIAN_POINT('Ctrl Pts',(-4.72434480941012,1.06847604194547,8.06466009624927));
#37304=CARTESIAN_POINT('Ctrl Pts',(-4.75585078787386,1.18514270861233,8.06860628573794));
#37305=CARTESIAN_POINT('Ctrl Pts',(-4.78609169199371,1.30000000000073,8.0676513323912));
#37306=CARTESIAN_POINT('Ctrl Pts',(-4.80579794746511,-1.30000000000037,
7.83248813918676));
#37307=CARTESIAN_POINT('Ctrl Pts',(-4.77028007162946,-1.18514270861208,
7.84904374373791));
#37308=CARTESIAN_POINT('Ctrl Pts',(-4.73393636878789,-1.06847604194535,
7.86246982037874));
#37309=CARTESIAN_POINT('Ctrl Pts',(-4.64806731910125,-0.794772684000984,
7.88625690776372));
#37310=CARTESIAN_POINT('Ctrl Pts',(-4.58389442940921,-0.636309800095303,
7.8883926499238));
#37311=CARTESIAN_POINT('Ctrl Pts',(-4.51027105908399,-0.319434907277212,
7.90553912776898));
#37312=CARTESIAN_POINT('Ctrl Pts',(-4.47547361646124,-0.158333333333358,
7.91015777895858));
#37313=CARTESIAN_POINT('Ctrl Pts',(-4.47101506047161,0.158333333333361,
7.93799763499912));
#37314=CARTESIAN_POINT('Ctrl Pts',(-4.50131739459165,0.31943490727722,7.96147710343081));
#37315=CARTESIAN_POINT('Ctrl Pts',(-4.56593346222998,0.636309800095312,
8.00051234348569));
#37316=CARTESIAN_POINT('Ctrl Pts',(-4.6248930339895,0.794772684000973,8.02878061626448));
#37317=CARTESIAN_POINT('Ctrl Pts',(-4.70399233636378,1.06847604194546,8.0507728789089));
#37318=CARTESIAN_POINT('Ctrl Pts',(-4.73781730149281,1.18514270861231,8.05578862073716));
#37319=CARTESIAN_POINT('Ctrl Pts',(-4.77122807467102,1.30000000000071,8.05630046878855));
#37320=CARTESIAN_POINT('Ctrl Pts',(-4.79013869260304,-1.30000000000035,
7.82347634664023));
#37321=CARTESIAN_POINT('Ctrl Pts',(-4.75171347795003,-1.18514270861206,
7.837781748419));
#37322=CARTESIAN_POINT('Ctrl Pts',(-4.7131865700244,-1.06847604194533,7.84975228894376));
#37323=CARTESIAN_POINT('Ctrl Pts',(-4.62394677363127,-0.794772684000971,
7.87201263567021));
#37324=CARTESIAN_POINT('Ctrl Pts',(-4.5597935968354,-0.636309800095291,
7.87633136950941));
#37325=CARTESIAN_POINT('Ctrl Pts',(-4.48594654724452,-0.319434907277205,
7.89382691479891));
#37326=CARTESIAN_POINT('Ctrl Pts',(-4.45225272357408,-0.158333333333356,
7.89861844168121));
#37327=CARTESIAN_POINT('Ctrl Pts',(-4.44824328709278,0.158333333333358,
7.92500913485026));
#37328=CARTESIAN_POINT('Ctrl Pts',(-4.47811132969497,0.319434907277216,
7.94608132457026));
#37329=CARTESIAN_POINT('Ctrl Pts',(-4.54341735300971,0.636309800095302,
7.98341513439605));
#37330=CARTESIAN_POINT('Ctrl Pts',(-4.6022310012356,0.794772684000958,8.01027478191746));
#37331=CARTESIAN_POINT('Ctrl Pts',(-4.68450819501405,1.06847604194544,8.03446676261853));
#37332=CARTESIAN_POINT('Ctrl Pts',(-4.72036882450999,1.18514270861228,8.04136088759017));
#37333=CARTESIAN_POINT('Ctrl Pts',(-4.75647533498565,1.30000000000068,8.04467732548917));
#37334=CARTESIAN_POINT('Ctrl Pts',(-4.77489914987303,-1.30000000000033,
7.81282546636895));
#37335=CARTESIAN_POINT('Ctrl Pts',(-4.73340430295669,-1.18514270861205,
7.82546882596531));
#37336=CARTESIAN_POINT('Ctrl Pts',(-4.69261841482826,-1.06847604194531,
7.83627450334434));
#37337=CARTESIAN_POINT('Ctrl Pts',(-4.6000326906894,-0.794772684000959,
7.85699236620913));
#37338=CARTESIAN_POINT('Ctrl Pts',(-4.53636034458574,-0.636309800095283,
7.86197068256707));
#37339=CARTESIAN_POINT('Ctrl Pts',(-4.46231435141602,-0.319434907277201,
7.87976329549689));
#37340=CARTESIAN_POINT('Ctrl Pts',(-4.4295828439994,-0.158333333333353,
7.8852526458423));
#37341=CARTESIAN_POINT('Ctrl Pts',(-4.42551665113566,0.158333333333356,
7.91179396725503));
#37342=CARTESIAN_POINT('Ctrl Pts',(-4.45425909385832,0.319434907277209,
7.93260279656291));
#37343=CARTESIAN_POINT('Ctrl Pts',(-4.51986544041176,0.636309800095291,
7.96936820656945));
#37344=CARTESIAN_POINT('Ctrl Pts',(-4.57852879619251,0.794772684000948,
7.99463506736218));
#37345=CARTESIAN_POINT('Ctrl Pts',(-4.66435698263534,1.06847604194542,8.01991355514737));
#37346=CARTESIAN_POINT('Ctrl Pts',(-4.7025363183252,1.18514270861227,8.02788276798637));
#37347=CARTESIAN_POINT('Ctrl Pts',(-4.74174314804155,1.30000000000067,8.03287907296246));
#37348=CARTESIAN_POINT('Ctrl Pts',(-4.76161182290268,-1.30000000000032,
7.80610825536315));
#37349=CARTESIAN_POINT('Ctrl Pts',(-4.71752842160646,-1.18514270861204,
7.81742462867045));
#37350=CARTESIAN_POINT('Ctrl Pts',(-4.67485111019541,-1.06847604194531,
7.82725239943781));
#37351=CARTESIAN_POINT('Ctrl Pts',(-4.57950633219105,-0.794772684000953,
7.84651754628806));
#37352=CARTESIAN_POINT('Ctrl Pts',(-4.51634868295189,-0.636309800095279,
7.85163572302273));
#37353=CARTESIAN_POINT('Ctrl Pts',(-4.44219644796232,-0.3194349072772,7.86944813166365));
#37354=CARTESIAN_POINT('Ctrl Pts',(-4.41017374720179,-0.158333333333352,
7.87583513286652));
#37355=CARTESIAN_POINT('Ctrl Pts',(-4.40623331788559,0.158333333333355,
7.90192986702047));
#37356=CARTESIAN_POINT('Ctrl Pts',(-4.43438298209535,0.319434907277207,
7.92139088711657));
#37357=CARTESIAN_POINT('Ctrl Pts',(-4.50037157207737,0.636309800095287,
7.95723410938572));
#37358=CARTESIAN_POINT('Ctrl Pts',(-4.5587905780062,0.794772684000944,7.9815530285965));
#37359=CARTESIAN_POINT('Ctrl Pts',(-4.64745198274385,1.06847604194542,8.00810940448882));
#37360=CARTESIAN_POINT('Ctrl Pts',(-4.68749140106699,1.18514270861226,8.01718845533252));
#37361=CARTESIAN_POINT('Ctrl Pts',(-4.72919200083113,1.30000000000066,8.02385128590684));
#37362=CARTESIAN_POINT('Ctrl Pts',(-4.751434470258,-1.30000000000032,7.79902289403952));
#37363=CARTESIAN_POINT('Ctrl Pts',(-4.70529589232437,-1.18514270861203,
7.80924536461335));
#37364=CARTESIAN_POINT('Ctrl Pts',(-4.66109034485469,-1.0684760419453,7.81836178493761));
#37365=CARTESIAN_POINT('Ctrl Pts',(-4.56343237398343,-0.794772684000951,
7.83686734227923));
#37366=CARTESIAN_POINT('Ctrl Pts',(-4.50047624693983,-0.636309800095276,
7.84283414873083));
#37367=CARTESIAN_POINT('Ctrl Pts',(-4.4261047074392,-0.319434907277198,
7.86115706837341));
#37368=CARTESIAN_POINT('Ctrl Pts',(-4.39464806145917,-0.158333333333352,
7.86829614150567));
#37369=CARTESIAN_POINT('Ctrl Pts',(-4.39079493705768,0.158333333333354,
7.894078837855));
#37370=CARTESIAN_POINT('Ctrl Pts',(-4.41848568860533,0.319434907277207,
7.91235912758977));
#37371=CARTESIAN_POINT('Ctrl Pts',(-4.48483100996797,0.636309800095286,
7.9472937881376));
#37372=CARTESIAN_POINT('Ctrl Pts',(-4.54317603144512,0.79477268400094,7.97050145391679));
#37373=CARTESIAN_POINT('Ctrl Pts',(-4.63405963255871,1.06847604194541,7.9982291981047));
#37374=CARTESIAN_POINT('Ctrl Pts',(-4.67552950583216,1.18514270861226,8.00837888207417));
#37375=CARTESIAN_POINT('Ctrl Pts',(-4.71912910902628,1.30000000000066,8.01667593696833));
#37376=CARTESIAN_POINT('Ctrl Pts',(-4.73578719298179,-1.3000000000003,7.78983839804538));
#37377=CARTESIAN_POINT('Ctrl Pts',(-4.68659125419676,-1.18514270861203,
7.7983113785018));
#37378=CARTESIAN_POINT('Ctrl Pts',(-4.64012373839081,-1.0684760419453,7.80623938864637));
#37379=CARTESIAN_POINT('Ctrl Pts',(-4.53907768398521,-0.794772684000947,
7.82329568763203));
#37380=CARTESIAN_POINT('Ctrl Pts',(-4.47647185678535,-0.636309800095271,
7.83038096282361));
#37381=CARTESIAN_POINT('Ctrl Pts',(-4.40190948645908,-0.319434907277195,
7.84895368410313));
#37382=CARTESIAN_POINT('Ctrl Pts',(-4.37149167166539,-0.15833333333335,
7.85650826084508));
#37383=CARTESIAN_POINT('Ctrl Pts',(-4.36774732594694,0.158333333333353,
7.88187198112008));
#37384=CARTESIAN_POINT('Ctrl Pts',(-4.39453562043689,0.319434907277204,
7.89916475334937));
#37385=CARTESIAN_POINT('Ctrl Pts',(-4.46123713703452,0.63630980009528,7.93330791518739));
#37386=CARTESIAN_POINT('Ctrl Pts',(-4.5192165770096,0.794772684000933,7.95555481439467));
#37387=CARTESIAN_POINT('Ctrl Pts',(-4.61365511815839,1.0684760419454,7.98435171132209));
#37388=CARTESIAN_POINT('Ctrl Pts',(-4.65748255750737,1.18514270861225,7.99546447667734));
#37389=CARTESIAN_POINT('Ctrl Pts',(-4.70425849103481,1.30000000000064,8.00522489773817));
#37390=CARTESIAN_POINT('Ctrl Pts',(-4.71238759485044,-1.30000000000028,
7.77568997553473));
#37391=CARTESIAN_POINT('Ctrl Pts',(-4.65836428021862,-1.185142708612,7.78243366970776));
#37392=CARTESIAN_POINT('Ctrl Pts',(-4.6083436035125,-1.06847604194527,7.78917874543528));
#37393=CARTESIAN_POINT('Ctrl Pts',(-4.50203272805262,-0.794772684000925,
7.80476441138087));
#37394=CARTESIAN_POINT('Ctrl Pts',(-4.4401680936263,-0.63630980009526,7.81276995314513));
#37395=CARTESIAN_POINT('Ctrl Pts',(-4.36530930032411,-0.319434907277191,
7.83178520154449));
#37396=CARTESIAN_POINT('Ctrl Pts',(-4.33632940633184,-0.158333333333348,
7.84042764005913));
#37397=CARTESIAN_POINT('Ctrl Pts',(-4.33274105297626,0.15833333333335,7.86516233735358));
#37398=CARTESIAN_POINT('Ctrl Pts',(-4.35816294414213,0.319434907277198,
7.88090940365321));
#37399=CARTESIAN_POINT('Ctrl Pts',(-4.42565069818634,0.636309800095269,
7.91298008491273));
#37400=CARTESIAN_POINT('Ctrl Pts',(-4.48367624716704,0.794772684000921,
7.93188635609983));
#37401=CARTESIAN_POINT('Ctrl Pts',(-4.58335118562598,1.06847604194539,7.96252186347471));
#37402=CARTESIAN_POINT('Ctrl Pts',(-4.63051192582729,1.18514270861223,7.97568900065146));
#37403=CARTESIAN_POINT('Ctrl Pts',(-4.68168781869149,1.30000000000062,7.98876229901981));
#37404=CARTESIAN_POINT('Ctrl Pts',(-4.68068425748576,-1.30000000000025,
7.75862761062044));
#37405=CARTESIAN_POINT('Ctrl Pts',(-4.62041273591367,-1.18514270861197,
7.76225791249285));
#37406=CARTESIAN_POINT('Ctrl Pts',(-4.56574818199531,-1.06847604194525,
7.76701611525181));
#37407=CARTESIAN_POINT('Ctrl Pts',(-4.45241534378754,-0.794772684000912,
7.78061419218393));
#37408=CARTESIAN_POINT('Ctrl Pts',(-4.39110918291877,-0.636309800095245,
7.7916246561428));
#37409=CARTESIAN_POINT('Ctrl Pts',(-4.31573727102646,-0.319434907277182,
7.81170467698355));
#37410=CARTESIAN_POINT('Ctrl Pts',(-4.2887792412685,-0.158333333333344,
7.82138929851315));
#37411=CARTESIAN_POINT('Ctrl Pts',(-4.28553660227673,0.158333333333346,
7.84465438395679));
#37412=CARTESIAN_POINT('Ctrl Pts',(-4.3094926211426,0.319434907277191,7.85693583601697));
#37413=CARTESIAN_POINT('Ctrl Pts',(-4.37776936877316,0.636309800095255,
7.88689111269756));
#37414=CARTESIAN_POINT('Ctrl Pts',(-4.43481700835146,0.794772684000901,
7.90463604211364));
#37415=CARTESIAN_POINT('Ctrl Pts',(-4.54155275115623,1.06847604194536,7.93754731631996));
#37416=CARTESIAN_POINT('Ctrl Pts',(-4.59343691227159,1.1851427086122,7.95263540923971));
#37417=CARTESIAN_POINT('Ctrl Pts',(-4.65100328639117,1.30000000000059,7.96856552395818));
#37418=CARTESIAN_POINT('Ctrl Pts',(-4.65412859982384,-1.3000000000002,7.74500676190758));
#37419=CARTESIAN_POINT('Ctrl Pts',(-4.58846168458542,-1.18514270861193,
7.74693192997448));
#37420=CARTESIAN_POINT('Ctrl Pts',(-4.52981289644311,-1.06847604194521,
7.75060684134227));
#37421=CARTESIAN_POINT('Ctrl Pts',(-4.41053574074808,-0.794772684000884,
7.76313887882534));
#37422=CARTESIAN_POINT('Ctrl Pts',(-4.35000766089167,-0.636309800095221,
7.77548844878813));
#37423=CARTESIAN_POINT('Ctrl Pts',(-4.27413821844525,-0.31943490727717,
7.79685341886066));
#37424=CARTESIAN_POINT('Ctrl Pts',(-4.24858903766098,-0.158333333333338,
7.80860652078929));
#37425=CARTESIAN_POINT('Ctrl Pts',(-4.2454329537061,0.158333333333341,7.83132513803103));
#37426=CARTESIAN_POINT('Ctrl Pts',(-4.26791211437986,0.319434907277179,
7.84137487601959));
#37427=CARTESIAN_POINT('Ctrl Pts',(-4.33717753520158,0.636309800095231,
7.86815146594569));
#37428=CARTESIAN_POINT('Ctrl Pts',(-4.39429388038338,0.794772684000871,
7.88171031687834));
#37429=CARTESIAN_POINT('Ctrl Pts',(-4.50724165666521,1.06847604194532,7.91512818724497));
#37430=CARTESIAN_POINT('Ctrl Pts',(-4.56307192346659,1.18514270861215,7.93167421003735));
#37431=CARTESIAN_POINT('Ctrl Pts',(-4.62584154984451,1.30000000000054,7.95030089779451));
#37432=CARTESIAN_POINT('Ctrl Pts',(-4.63294304514757,-1.3000000000002,7.73363723320236));
#37433=CARTESIAN_POINT('Ctrl Pts',(-4.56293910323236,-1.18514270861193,
7.73404012696683));
#37434=CARTESIAN_POINT('Ctrl Pts',(-4.50104605242609,-1.06847604194521,
7.73691769506999));
#37435=CARTESIAN_POINT('Ctrl Pts',(-4.37679850444107,-0.794772684000881,
7.74928244582305));
#37436=CARTESIAN_POINT('Ctrl Pts',(-4.31645108600974,-0.636309800095221,
7.76471095515052));
#37437=CARTESIAN_POINT('Ctrl Pts',(-4.24020673369042,-0.319434907277171,
7.78698860707724));
#37438=CARTESIAN_POINT('Ctrl Pts',(-4.21629109567086,-0.158333333333338,
7.7982385847441));
#37439=CARTESIAN_POINT('Ctrl Pts',(-4.21332902939037,0.15833333333334,7.81993355065792));
#37440=CARTESIAN_POINT('Ctrl Pts',(-4.23450068448092,0.319434907277178,
7.82873972143735));
#37441=CARTESIAN_POINT('Ctrl Pts',(-4.30426730097828,0.63630980009523,7.85399130617029));
#37442=CARTESIAN_POINT('Ctrl Pts',(-4.36098494754636,0.794772684000871,
7.86566832729003));
#37443=CARTESIAN_POINT('Ctrl Pts',(-4.47876340129364,1.06847604194532,7.90015581847597));
#37444=CARTESIAN_POINT('Ctrl Pts',(-4.53777653582107,1.18514270861215,7.91791658710113));
#37445=CARTESIAN_POINT('Ctrl Pts',(-4.60482087637055,1.30000000000054,7.93850976730455));
#37446=CARTESIAN_POINT('Ctrl Pts',(-4.6168608328518,-1.30000000000018,7.72606704168878));
#37447=CARTESIAN_POINT('Ctrl Pts',(-4.54358307191281,-1.18514270861192,
7.72568677646031));
#37448=CARTESIAN_POINT('Ctrl Pts',(-4.47927319496849,-1.0684760419452,7.72810685793159));
#37449=CARTESIAN_POINT('Ctrl Pts',(-4.35142212012702,-0.794772684000877,
7.7401670913497));
#37450=CARTESIAN_POINT('Ctrl Pts',(-4.29156209657586,-0.636309800095215,
7.75644417809687));
#37451=CARTESIAN_POINT('Ctrl Pts',(-4.21500073541837,-0.319434907277167,
7.77967099750095));
#37452=CARTESIAN_POINT('Ctrl Pts',(-4.19190516024014,-0.158333333333336,
7.79227950123383));
#37453=CARTESIAN_POINT('Ctrl Pts',(-4.18897493925662,0.158333333333339,
7.81366169079514));
#37454=CARTESIAN_POINT('Ctrl Pts',(-4.209285431662,0.319434907277175,7.82095446965029));
#37455=CARTESIAN_POINT('Ctrl Pts',(-4.27958250757412,0.636309800095223,
7.84429813168956));
#37456=CARTESIAN_POINT('Ctrl Pts',(-4.33613614571148,0.794772684000864,
7.85394641256676));
#37457=CARTESIAN_POINT('Ctrl Pts',(-4.45774599007139,1.06847604194531,7.88820003389546));
#37458=CARTESIAN_POINT('Ctrl Pts',(-4.51924087753763,1.18514270861214,7.90639059637782));
#37459=CARTESIAN_POINT('Ctrl Pts',(-4.58959025693552,1.30000000000053,7.92794459789109));
#37460=CARTESIAN_POINT('Ctrl Pts',(-4.60067713755899,-1.30000000000017,
7.71855328487674));
#37461=CARTESIAN_POINT('Ctrl Pts',(-4.52403569735226,-1.18514270861191,
7.71709481226507));
#37462=CARTESIAN_POINT('Ctrl Pts',(-4.45719976387259,-1.06847604194519,
7.71903031071803));
#37463=CARTESIAN_POINT('Ctrl Pts',(-4.32544806917629,-0.794772684000868,
7.73134245146043));
#37464=CARTESIAN_POINT('Ctrl Pts',(-4.26552769529275,-0.636309800095211,
7.75107352021072));
#37465=CARTESIAN_POINT('Ctrl Pts',(-4.18886738502932,-0.319434907277166,
7.77408197784996));
#37466=CARTESIAN_POINT('Ctrl Pts',(-4.16758864112992,-0.158333333333336,
7.78351981943754));
#37467=CARTESIAN_POINT('Ctrl Pts',(-4.16487016749168,0.158333333333338,
7.80371054916999));
#37468=CARTESIAN_POINT('Ctrl Pts',(-4.183697750681,0.319434907277175,7.81221977204047));
#37469=CARTESIAN_POINT('Ctrl Pts',(-4.25427622869244,0.636309800095221,
7.8349085617001));
#37470=CARTESIAN_POINT('Ctrl Pts',(-4.3107122638051,0.79477268400086,7.84232650600807));
#37471=CARTESIAN_POINT('Ctrl Pts',(-4.43616916091367,1.0684760419453,7.87694127733603));
#37472=CARTESIAN_POINT('Ctrl Pts',(-4.50017163882838,1.18514270861213,7.89586553247259));
#37473=CARTESIAN_POINT('Ctrl Pts',(-4.57387095253565,1.30000000000052,7.9187305908415));
#37474=CARTESIAN_POINT('Ctrl Pts',(-4.58730781279972,-1.30000000000017,
7.71230138859931));
#37475=CARTESIAN_POINT('Ctrl Pts',(-4.50788362503931,-1.1851427086119,7.71094533350715));
#37476=CARTESIAN_POINT('Ctrl Pts',(-4.4390616358845,-1.06847604194518,7.71275877394741));
#37477=CARTESIAN_POINT('Ctrl Pts',(-4.3045622728866,-0.794772684000865,
7.72427035287721));
#37478=CARTESIAN_POINT('Ctrl Pts',(-4.24555331669918,-0.636309800095205,
7.74236664972257));
#37479=CARTESIAN_POINT('Ctrl Pts',(-4.16904001114168,-0.319434907277162,
7.76453178614663));
#37480=CARTESIAN_POINT('Ctrl Pts',(-4.14872086860415,-0.158333333333334,
7.7739781792026));
#37481=CARTESIAN_POINT('Ctrl Pts',(-4.14585353447854,0.158333333333337,
7.79478399944369));
#37482=CARTESIAN_POINT('Ctrl Pts',(-4.16336823012039,0.319434907277172,
7.80482177380069));
#37483=CARTESIAN_POINT('Ctrl Pts',(-4.23391288575959,0.636309800095215,
7.82772870678767));
#37484=CARTESIAN_POINT('Ctrl Pts',(-4.29012932459028,0.794772684000851,
7.83345416959625));
#37485=CARTESIAN_POINT('Ctrl Pts',(-4.41847992247652,1.06847604194529,7.86836987702009));
#37486=CARTESIAN_POINT('Ctrl Pts',(-4.48441830653494,1.18514270861212,7.8877977601388));
#37487=CARTESIAN_POINT('Ctrl Pts',(-4.56073685668519,1.30000000000051,7.91153981038689));
#37488=CARTESIAN_POINT('Ctrl Pts',(-4.57096682812091,-1.30000000000016,
7.70550102152383));
#37489=CARTESIAN_POINT('Ctrl Pts',(-4.48783339483817,-1.1851427086119,7.7041546867954));
#37490=CARTESIAN_POINT('Ctrl Pts',(-4.41636673485974,-1.06847604194518,
7.7055682845817));
#37491=CARTESIAN_POINT('Ctrl Pts',(-4.27821703371616,-0.79477268400086,
7.71520997448892));
#37492=CARTESIAN_POINT('Ctrl Pts',(-4.22041201886117,-0.636309800095203,
7.73017506044892));
#37493=CARTESIAN_POINT('Ctrl Pts',(-4.1441697959739,-0.319434907277162,
7.75018142748202));
#37494=CARTESIAN_POINT('Ctrl Pts',(-4.12517779033268,-0.158333333333334,
7.75942312339014));
#37495=CARTESIAN_POINT('Ctrl Pts',(-4.12231328988027,0.158333333333336,
7.78010768802387));
#37496=CARTESIAN_POINT('Ctrl Pts',(-4.13842233140064,0.31943490727717,7.79052990985211));
#37497=CARTESIAN_POINT('Ctrl Pts',(-4.2088673822804,0.636309800095213,7.81473549588073));
#37498=CARTESIAN_POINT('Ctrl Pts',(-4.26426830305468,0.794772684000848,
7.82182773003922));
#37499=CARTESIAN_POINT('Ctrl Pts',(-4.39635488621716,1.06847604194529,7.85846836579053));
#37500=CARTESIAN_POINT('Ctrl Pts',(-4.46490150414816,1.18514270861212,7.8786290559999));
#37501=CARTESIAN_POINT('Ctrl Pts',(-4.54481935244935,1.30000000000051,7.90309006287123));
#37502=CARTESIAN_POINT('Ctrl Pts',(-4.55986191625154,-1.30000000000015,
7.70077302060858));
#37503=CARTESIAN_POINT('Ctrl Pts',(-4.47390766112863,-1.18514270861188,
7.70077480939679));
#37504=CARTESIAN_POINT('Ctrl Pts',(-4.40061540553237,-1.06847604194517,
7.70244469619189));
#37505=CARTESIAN_POINT('Ctrl Pts',(-4.26054738497045,-0.794772684000851,
7.71015610884605));
#37506=CARTESIAN_POINT('Ctrl Pts',(-4.20510952843759,-0.636309800095197,
7.7189877024356));
#37507=CARTESIAN_POINT('Ctrl Pts',(-4.13001103025471,-0.319434907277159,
7.73569629635065));
#37508=CARTESIAN_POINT('Ctrl Pts',(-4.11199983529727,-0.158333333333332,
7.74537650603382));
#37509=CARTESIAN_POINT('Ctrl Pts',(-4.1092062507607,0.158333333333335,7.76590783488345));
#37510=CARTESIAN_POINT('Ctrl Pts',(-4.12443963758816,0.319434907277167,
7.77588343648702));
#37511=CARTESIAN_POINT('Ctrl Pts',(-4.19381566981051,0.636309800095207,
7.80277904737017));
#37512=CARTESIAN_POINT('Ctrl Pts',(-4.24681642623153,0.794772684000841,
7.81488250821034));
#37513=CARTESIAN_POINT('Ctrl Pts',(-4.38081889489758,1.06847604194528,7.85351577237354));
#37514=CARTESIAN_POINT('Ctrl Pts',(-4.45118854322609,1.18514270861211,7.87373889304781));
#37515=CARTESIAN_POINT('Ctrl Pts',(-4.53392313647837,1.30000000000049,7.8974622258436));
#37516=CARTESIAN_POINT('Ctrl Pts',(-4.55333646119712,-1.30000000000015,
7.69516819779691));
#37517=CARTESIAN_POINT('Ctrl Pts',(-4.46759044005481,-1.18514270861188,
7.69531068083379));
#37518=CARTESIAN_POINT('Ctrl Pts',(-4.39457954353638,-1.06847604194517,
7.69678116104379));
#37519=CARTESIAN_POINT('Ctrl Pts',(-4.25533045233313,-0.794772684000851,
7.70324620363229));
#37520=CARTESIAN_POINT('Ctrl Pts',(-4.20084799529369,-0.636309800095197,
7.7096965632967));
#37521=CARTESIAN_POINT('Ctrl Pts',(-4.1264371815048,-0.319434907277159,
7.724865141945));
#37522=CARTESIAN_POINT('Ctrl Pts',(-4.1083738762426,-0.158333333333332,
7.73455031738056));
#37523=CARTESIAN_POINT('Ctrl Pts',(-4.10569625638313,0.158333333333335,
7.75487515336321));
#37524=CARTESIAN_POINT('Ctrl Pts',(-4.12120905306815,0.319434907277167,
7.76438231270788));
#37525=CARTESIAN_POINT('Ctrl Pts',(-4.18990683146856,0.636309800095207,
7.792920784926));
#37526=CARTESIAN_POINT('Ctrl Pts',(-4.24157890048061,0.794772684000841,
7.80842294468367));
#37527=CARTESIAN_POINT('Ctrl Pts',(-4.37480433638251,1.06847604194528,7.84815479663225));
#37528=CARTESIAN_POINT('Ctrl Pts',(-4.44499154163424,1.18514270861211,7.86827306771218));
#37529=CARTESIAN_POINT('Ctrl Pts',(-4.52769759742464,1.30000000000049,7.89131116337371));
#37530=CARTESIAN_POINT('Ctrl Pts',(-4.55333646119701,-1.3,7.69516819779691));
#37531=CARTESIAN_POINT('Ctrl Pts',(-4.46759044005475,-1.18514270861178,
7.69531068083379));
#37532=CARTESIAN_POINT('Ctrl Pts',(-4.39457954353636,-1.06847604194512,
7.69678116104379));
#37533=CARTESIAN_POINT('Ctrl Pts',(-4.25533045233314,-0.794772684000851,
7.70324620363229));
#37534=CARTESIAN_POINT('Ctrl Pts',(-4.20084799529369,-0.636309800095197,
7.7096965632967));
#37535=CARTESIAN_POINT('Ctrl Pts',(-4.1264371815048,-0.319434907277159,
7.724865141945));
#37536=CARTESIAN_POINT('Ctrl Pts',(-4.1083738762426,-0.158333333333332,
7.73455031738056));
#37537=CARTESIAN_POINT('Ctrl Pts',(-4.10569625638312,0.158333333333334,
7.7548751533632));
#37538=CARTESIAN_POINT('Ctrl Pts',(-4.12120905306815,0.319434907277167,
7.76438231270788));
#37539=CARTESIAN_POINT('Ctrl Pts',(-4.18990683146856,0.636309800095206,
7.792920784926));
#37540=CARTESIAN_POINT('Ctrl Pts',(-4.24157890048061,0.79477268400084,7.80842294468366));
#37541=CARTESIAN_POINT('Ctrl Pts',(-4.37480433638243,1.06847604194511,7.84815479663222));
#37542=CARTESIAN_POINT('Ctrl Pts',(-4.44499154163404,1.18514270861178,7.86827306771212));
#37543=CARTESIAN_POINT('Ctrl Pts',(-4.52769759742429,1.3,7.89131116337361));
#37544=CARTESIAN_POINT('',(-4.8959285873767,-1.2,7.92964598765946));
#37545=CARTESIAN_POINT('Ctrl Pts',(-4.8959285873767,-1.2,7.92964598765946));
#37546=CARTESIAN_POINT('Ctrl Pts',(-4.88128614180205,-1.21682133722576,
7.91377904453193));
#37547=CARTESIAN_POINT('Ctrl Pts',(-4.86705709202731,-1.23328464930557,
7.89716046450904));
#37548=CARTESIAN_POINT('Ctrl Pts',(-4.82891600865078,-1.27679348086419,
7.85588891014176));
#37549=CARTESIAN_POINT('Ctrl Pts',(-4.81667637007595,-1.29060520248064,
7.84294482434472));
#37550=CARTESIAN_POINT('Ctrl Pts',(-4.80971615050746,-1.29844967893122,
7.83574479480255));
#37551=CARTESIAN_POINT('Ctrl Pts',(-4.8090271842101,-1.29922545708331,7.83503667156741));
#37552=CARTESIAN_POINT('Ctrl Pts',(-4.80833847418889,-1.30000000000037,
7.83433517767123));
#37553=CARTESIAN_POINT('',(-4.8704124160437,-0.653834841416788,8.08407177162779));
#37554=CARTESIAN_POINT('Ctrl Pts',(-4.87041241606985,-0.653834841416102,
8.08407177162979));
#37555=CARTESIAN_POINT('Ctrl Pts',(-4.87331744329784,-0.717939165694387,
8.06806777610109));
#37556=CARTESIAN_POINT('Ctrl Pts',(-4.87562719338777,-0.763825235527143,
8.05500749471629));
#37557=CARTESIAN_POINT('Ctrl Pts',(-4.88440882003114,-0.949536215866272,
8.00391931523675));
#37558=CARTESIAN_POINT('Ctrl Pts',(-4.88885629259023,-1.04568967639883,
7.9771011245465));
#37559=CARTESIAN_POINT('Ctrl Pts',(-4.8959285873767,-1.2,7.92964598765946));
#37560=CARTESIAN_POINT('',(-4.84356468978495,0.653834841531101,8.22097066356893));
#37561=CARTESIAN_POINT('Ctrl Pts',(-4.84356468978495,0.653834841531099,
8.22097066356893));
#37562=CARTESIAN_POINT('Ctrl Pts',(-4.81020009414171,0.575793149317761,
8.19600115080956));
#37563=CARTESIAN_POINT('Ctrl Pts',(-4.78265018138025,0.493919053872489,
8.1745279229996));
#37564=CARTESIAN_POINT('Ctrl Pts',(-4.74428415111832,0.338198890099698,
8.14139392359785));
#37565=CARTESIAN_POINT('Ctrl Pts',(-4.731584258065,0.265711321162047,8.12875730458245));
#37566=CARTESIAN_POINT('Ctrl Pts',(-4.71756354556536,0.129739858083149,
8.10877297973432));
#37567=CARTESIAN_POINT('Ctrl Pts',(-4.71484516590534,0.0666407666263151,
8.10094744092773));
#37568=CARTESIAN_POINT('Ctrl Pts',(-4.71704691134613,-0.0595497741256923,
8.08778747206704));
#37569=CARTESIAN_POINT('Ctrl Pts',(-4.72196721471519,-0.12279612842464,
8.08234971685884));
#37570=CARTESIAN_POINT('Ctrl Pts',(-4.74094387627607,-0.260145569197153,
8.0739688976417));
#37571=CARTESIAN_POINT('Ctrl Pts',(-4.75650261542264,-0.333943518744006,
8.07165826059291));
#37572=CARTESIAN_POINT('Ctrl Pts',(-4.80134670116416,-0.491230496872132,
8.07250778651032));
#37573=CARTESIAN_POINT('Ctrl Pts',(-4.83256715599814,-0.574163160314909,
8.07651308744752));
#37574=CARTESIAN_POINT('Ctrl Pts',(-4.87041241602633,-0.653834841428499,
8.08407177159134));
#37575=CARTESIAN_POINT('',(-4.85793966858526,1.2,8.15022217211857));
#37576=CARTESIAN_POINT('Ctrl Pts',(-4.85793966858526,1.2,8.15022217211857));
#37577=CARTESIAN_POINT('Ctrl Pts',(-4.85558604305792,1.13519300442415,8.16225490630404));
#37578=CARTESIAN_POINT('Ctrl Pts',(-4.85238400598773,1.03885769118231,8.17837680110599));
#37579=CARTESIAN_POINT('Ctrl Pts',(-4.84595734033846,0.795132005601969,
8.20963889291911));
#37580=CARTESIAN_POINT('Ctrl Pts',(-4.84491963285573,0.74167848084335,8.21454270765557));
#37581=CARTESIAN_POINT('Ctrl Pts',(-4.84356468978495,0.653834841531102,
8.22097066356893));
#37582=CARTESIAN_POINT('Ctrl Pts',(-4.77350315750449,1.30000000000006,8.05800210098462));
#37583=CARTESIAN_POINT('Ctrl Pts',(-4.78796292235706,1.28314221689022,8.07284648759814));
#37584=CARTESIAN_POINT('Ctrl Pts',(-4.80201716658242,1.26652079478402,8.08834475124509));
#37585=CARTESIAN_POINT('Ctrl Pts',(-4.83622047073047,1.22603540792557,8.12558944398319));
#37586=CARTESIAN_POINT('Ctrl Pts',(-4.84546925287898,1.21510518302868,8.13528868680846));
#37587=CARTESIAN_POINT('Ctrl Pts',(-4.85793966858526,1.2,8.15022217211857));
#37588=CARTESIAN_POINT('Ctrl Pts',(-4.55333646119701,-1.3,7.69516819779691));
#37589=CARTESIAN_POINT('Ctrl Pts',(-4.46759044005475,-1.18514270861178,
7.69531068083379));
#37590=CARTESIAN_POINT('Ctrl Pts',(-4.39457954353636,-1.06847604194512,
7.69678116104379));
#37591=CARTESIAN_POINT('Ctrl Pts',(-4.25533045233313,-0.794772684000851,
7.70324620363229));
#37592=CARTESIAN_POINT('Ctrl Pts',(-4.20084799529369,-0.636309800095196,
7.7096965632967));
#37593=CARTESIAN_POINT('Ctrl Pts',(-4.1264371815048,-0.319434907277159,
7.724865141945));
#37594=CARTESIAN_POINT('Ctrl Pts',(-4.1083738762426,-0.158333333333332,
7.73455031738055));
#37595=CARTESIAN_POINT('Ctrl Pts',(-4.10569625638313,0.158333333333334,
7.7548751533632));
#37596=CARTESIAN_POINT('Ctrl Pts',(-4.12120905306814,0.319434907277167,
7.76438231270788));
#37597=CARTESIAN_POINT('Ctrl Pts',(-4.18990683146856,0.636309800095206,
7.792920784926));
#37598=CARTESIAN_POINT('Ctrl Pts',(-4.24157890048061,0.79477268400084,7.80842294468366));
#37599=CARTESIAN_POINT('Ctrl Pts',(-4.37480433638243,1.06847604194511,7.84815479663222));
#37600=CARTESIAN_POINT('Ctrl Pts',(-4.44499154163404,1.18514270861178,7.86827306771212));
#37601=CARTESIAN_POINT('Ctrl Pts',(-4.52769759742429,1.3,7.89131116337361));
#37602=CARTESIAN_POINT('Ctrl Pts',(-4.559720379007,-1.3,7.61849776759047));
#37603=CARTESIAN_POINT('Ctrl Pts',(-4.47399349175896,-1.18514270861178,
7.62037245698057));
#37604=CARTESIAN_POINT('Ctrl Pts',(-4.40104080402149,-1.06847604194512,
7.62304807647726));
#37605=CARTESIAN_POINT('Ctrl Pts',(-4.26201645755201,-0.794772684000851,
7.63107960154223));
#37606=CARTESIAN_POINT('Ctrl Pts',(-4.20777282266716,-0.636309800095196,
7.63685323236411));
#37607=CARTESIAN_POINT('Ctrl Pts',(-4.13378893043113,-0.319434907277159,
7.65150954041835));
#37608=CARTESIAN_POINT('Ctrl Pts',(-4.11602990877888,-0.158333333333332,
7.65999102848028));
#37609=CARTESIAN_POINT('Ctrl Pts',(-4.11370927434805,0.158333333333334,
7.68035338514341));
#37610=CARTESIAN_POINT('Ctrl Pts',(-4.12926944463902,0.319434907277167,
7.69110119252446));
#37611=CARTESIAN_POINT('Ctrl Pts',(-4.19827830828669,0.636309800095206,
7.72022950297699));
#37612=CARTESIAN_POINT('Ctrl Pts',(-4.25004328077839,0.79477268400084,7.73644325734629));
#37613=CARTESIAN_POINT('Ctrl Pts',(-4.38381424022261,1.06847604194511,7.77468958527649));
#37614=CARTESIAN_POINT('Ctrl Pts',(-4.45430894480039,1.18514270861178,7.79364115454063));
#37615=CARTESIAN_POINT('Ctrl Pts',(-4.53739386231511,1.3,7.81498887487403));
#37616=CARTESIAN_POINT('Ctrl Pts',(-4.56610429681699,-1.3,7.54182733738403));
#37617=CARTESIAN_POINT('Ctrl Pts',(-4.48039654346318,-1.18514270861178,
7.54543423312735));
#37618=CARTESIAN_POINT('Ctrl Pts',(-4.40750206450663,-1.06847604194512,
7.54931499191074));
#37619=CARTESIAN_POINT('Ctrl Pts',(-4.26870246277088,-0.794772684000851,
7.55891299945218));
#37620=CARTESIAN_POINT('Ctrl Pts',(-4.21469765004064,-0.636309800095196,
7.56400990143152));
#37621=CARTESIAN_POINT('Ctrl Pts',(-4.14114067935745,-0.319434907277159,
7.57815393889169));
#37622=CARTESIAN_POINT('Ctrl Pts',(-4.12368594131515,-0.158333333333332,
7.58543173958001));
#37623=CARTESIAN_POINT('Ctrl Pts',(-4.12172229231298,0.158333333333334,
7.60583161692362));
#37624=CARTESIAN_POINT('Ctrl Pts',(-4.1373298362099,0.319434907277167,7.61782007234104));
#37625=CARTESIAN_POINT('Ctrl Pts',(-4.20664978510482,0.636309800095206,
7.64753822102798));
#37626=CARTESIAN_POINT('Ctrl Pts',(-4.25850766107617,0.79477268400084,7.66446357000892));
#37627=CARTESIAN_POINT('Ctrl Pts',(-4.39282414406279,1.06847604194511,7.70122437392077));
#37628=CARTESIAN_POINT('Ctrl Pts',(-4.46362634796674,1.18514270861178,7.71900924136913));
#37629=CARTESIAN_POINT('Ctrl Pts',(-4.54709012720593,1.3,7.73866658637446));
#37630=CARTESIAN_POINT('Ctrl Pts',(-4.57248821462698,-1.3,7.46515690717759));
#37631=CARTESIAN_POINT('Ctrl Pts',(-4.48679959516739,-1.18514270861178,
7.47049600927413));
#37632=CARTESIAN_POINT('Ctrl Pts',(-4.41396332499176,-1.06847604194512,
7.47558190734421));
#37633=CARTESIAN_POINT('Ctrl Pts',(-4.27538846798975,-0.794772684000851,
7.48674639736213));
#37634=CARTESIAN_POINT('Ctrl Pts',(-4.22162247741411,-0.636309800095196,
7.49116657049893));
#37635=CARTESIAN_POINT('Ctrl Pts',(-4.14849242828377,-0.319434907277159,
7.50479833736504));
#37636=CARTESIAN_POINT('Ctrl Pts',(-4.13134197385143,-0.158333333333332,
7.51087245067974));
#37637=CARTESIAN_POINT('Ctrl Pts',(-4.12973531027791,0.158333333333334,
7.53130984870382));
#37638=CARTESIAN_POINT('Ctrl Pts',(-4.14539022778078,0.319434907277167,
7.54453895215762));
#37639=CARTESIAN_POINT('Ctrl Pts',(-4.21502126192296,0.636309800095206,
7.57484693907897));
#37640=CARTESIAN_POINT('Ctrl Pts',(-4.26697204137396,0.79477268400084,7.59248388267156));
#37641=CARTESIAN_POINT('Ctrl Pts',(-4.40183404790297,1.06847604194511,7.62775916256504));
#37642=CARTESIAN_POINT('Ctrl Pts',(-4.47294375113309,1.18514270861178,7.64437732819764));
#37643=CARTESIAN_POINT('Ctrl Pts',(-4.55678639209675,1.3,7.66234429787488));
#37644=CARTESIAN_POINT('Ctrl Pts',(-4.57248821462698,-1.3,7.4651569071776));
#37645=CARTESIAN_POINT('Ctrl Pts',(-4.48679959516739,-1.18514270861178,
7.47049600927413));
#37646=CARTESIAN_POINT('Ctrl Pts',(-4.41396332499177,-1.06847604194512,
7.47558190734422));
#37647=CARTESIAN_POINT('Ctrl Pts',(-4.27538846798975,-0.794772684000851,
7.48674639736213));
#37648=CARTESIAN_POINT('Ctrl Pts',(-4.22162247741411,-0.636309800095197,
7.49116657049893));
#37649=CARTESIAN_POINT('Ctrl Pts',(-4.14849242828377,-0.319434907277159,
7.50479833736504));
#37650=CARTESIAN_POINT('Ctrl Pts',(-4.13134197385143,-0.158333333333332,
7.51087245067974));
#37651=CARTESIAN_POINT('Ctrl Pts',(-4.12973531027791,0.158333333333334,
7.53130984870382));
#37652=CARTESIAN_POINT('Ctrl Pts',(-4.14539022778078,0.319434907277167,
7.54453895215762));
#37653=CARTESIAN_POINT('Ctrl Pts',(-4.21502126192295,0.636309800095206,
7.57484693907897));
#37654=CARTESIAN_POINT('Ctrl Pts',(-4.26697204137395,0.79477268400084,7.59248388267156));
#37655=CARTESIAN_POINT('Ctrl Pts',(-4.40183404790297,1.06847604194511,7.62775916256504));
#37656=CARTESIAN_POINT('Ctrl Pts',(-4.47294375113309,1.18514270861178,7.64437732819763));
#37657=CARTESIAN_POINT('Ctrl Pts',(-4.55678639209675,1.3,7.66234429787488));
#37658=CARTESIAN_POINT('Ctrl Pts',(-4.5724882146272,-1.3000000000003,7.46515690717758));
#37659=CARTESIAN_POINT('Ctrl Pts',(-4.48679959516751,-1.18514270861198,
7.47049600927413));
#37660=CARTESIAN_POINT('Ctrl Pts',(-4.41396332499182,-1.06847604194522,
7.47558190734421));
#37661=CARTESIAN_POINT('Ctrl Pts',(-4.27538846798975,-0.794772684000851,
7.48674639736213));
#37662=CARTESIAN_POINT('Ctrl Pts',(-4.22162247741412,-0.636309800095197,
7.49116657049894));
#37663=CARTESIAN_POINT('Ctrl Pts',(-4.14849242828378,-0.319434907277159,
7.50479833736504));
#37664=CARTESIAN_POINT('Ctrl Pts',(-4.13134197385143,-0.158333333333332,
7.51087245067974));
#37665=CARTESIAN_POINT('Ctrl Pts',(-4.12973531027791,0.158333333333334,
7.53130984870382));
#37666=CARTESIAN_POINT('Ctrl Pts',(-4.14539022778078,0.319434907277167,
7.54453895215762));
#37667=CARTESIAN_POINT('Ctrl Pts',(-4.21502126192296,0.636309800095206,
7.57484693907897));
#37668=CARTESIAN_POINT('Ctrl Pts',(-4.26697204137396,0.79477268400084,7.59248388267156));
#37669=CARTESIAN_POINT('Ctrl Pts',(-4.40183404790331,1.06847604194578,7.62775916256513));
#37670=CARTESIAN_POINT('Ctrl Pts',(-4.47294375113389,1.1851427086131,7.64437732819782));
#37671=CARTESIAN_POINT('Ctrl Pts',(-4.55678639209818,1.30000000000195,7.66234429787519));
#37672=CARTESIAN_POINT('Ctrl Pts',(-4.57985658845494,-1.3000000000003,7.46043462252666));
#37673=CARTESIAN_POINT('Ctrl Pts',(-4.49399758634183,-1.18514270861198,
7.46643805441031));
#37674=CARTESIAN_POINT('Ctrl Pts',(-4.42096106045728,-1.06847604194522,
7.47158857881112));
#37675=CARTESIAN_POINT('Ctrl Pts',(-4.28185455997266,-0.794772684000851,
7.48151693362695));
#37676=CARTESIAN_POINT('Ctrl Pts',(-4.22749554624361,-0.636309800095197,
7.48233642792713));
#37677=CARTESIAN_POINT('Ctrl Pts',(-4.1540436348186,-0.319434907277159,
7.49422021701903));
#37678=CARTESIAN_POINT('Ctrl Pts',(-4.13706908978531,-0.158333333333332,
7.50081062857585));
#37679=CARTESIAN_POINT('Ctrl Pts',(-4.13553292450502,0.158333333333334,
7.52147411751504));
#37680=CARTESIAN_POINT('Ctrl Pts',(-4.1511379029416,0.319434907277167,7.53468752939477));
#37681=CARTESIAN_POINT('Ctrl Pts',(-4.2211214067753,0.636309800095206,7.56664485618235));
#37682=CARTESIAN_POINT('Ctrl Pts',(-4.27351162156741,0.79477268400084,7.58680963674882));
#37683=CARTESIAN_POINT('Ctrl Pts',(-4.40891552697358,1.06847604194578,7.62347431551885));
#37684=CARTESIAN_POINT('Ctrl Pts',(-4.48025898194793,1.1851427086131,7.64034602806548));
#37685=CARTESIAN_POINT('Ctrl Pts',(-4.56433455845528,1.30000000000195,7.65821867227938));
#37686=CARTESIAN_POINT('Ctrl Pts',(-4.59168342474784,-1.3000000000003,7.45718163914688));
#37687=CARTESIAN_POINT('Ctrl Pts',(-4.50842397388543,-1.18514270861199,
7.46447754241301));
#37688=CARTESIAN_POINT('Ctrl Pts',(-4.43718225163949,-1.06847604194522,
7.46993969508268));
#37689=CARTESIAN_POINT('Ctrl Pts',(-4.30036297863612,-0.794772684000854,
7.47832202973116));
#37690=CARTESIAN_POINT('Ctrl Pts',(-4.24470116695618,-0.636309800095197,
7.47377977131766));
#37691=CARTESIAN_POINT('Ctrl Pts',(-4.17076364579087,-0.319434907277159,
7.48282880263746));
#37692=CARTESIAN_POINT('Ctrl Pts',(-4.15283946666577,-0.158333333333333,
7.48967182383003));
#37693=CARTESIAN_POINT('Ctrl Pts',(-4.15133977222458,0.158333333333335,
7.51049912633798));
#37694=CARTESIAN_POINT('Ctrl Pts',(-4.16799329782777,0.319434907277169,
7.52348646991815));
#37695=CARTESIAN_POINT('Ctrl Pts',(-4.23840950953686,0.636309800095208,
7.55889184457618));
#37696=CARTESIAN_POINT('Ctrl Pts',(-4.29184104268107,0.794772684000841,
7.58552360736601));
#37697=CARTESIAN_POINT('Ctrl Pts',(-4.42496865500282,1.06847604194578,7.62366725460812));
#37698=CARTESIAN_POINT('Ctrl Pts',(-4.49458045110704,1.1851427086131,7.63990830968531));
#37699=CARTESIAN_POINT('Ctrl Pts',(-4.57617803280542,1.30000000000195,7.65587944830994));
#37700=CARTESIAN_POINT('Ctrl Pts',(-4.60901429870398,-1.3000000000003,7.45223840664109));
#37701=CARTESIAN_POINT('Ctrl Pts',(-4.5294315556627,-1.18514270861199,7.45959212322105));
#37702=CARTESIAN_POINT('Ctrl Pts',(-4.46089813449078,-1.06847604194522,
7.46488779903224));
#37703=CARTESIAN_POINT('Ctrl Pts',(-4.32809836544721,-0.794772684000851,
7.4723673836669));
#37704=CARTESIAN_POINT('Ctrl Pts',(-4.27192130062999,-0.636309800095196,
7.46631175328514));
#37705=CARTESIAN_POINT('Ctrl Pts',(-4.19815527265973,-0.319434907277159,
7.47405317109067));
#37706=CARTESIAN_POINT('Ctrl Pts',(-4.17893181023939,-0.158333333333332,
7.48021929441616));
#37707=CARTESIAN_POINT('Ctrl Pts',(-4.17741037262064,0.158333333333334,
7.50112354255511));
#37708=CARTESIAN_POINT('Ctrl Pts',(-4.19532546267363,0.319434907277167,
7.51451242989938));
#37709=CARTESIAN_POINT('Ctrl Pts',(-4.26555843318573,0.636309800095207,
7.55209975997349));
#37710=CARTESIAN_POINT('Ctrl Pts',(-4.31951500434467,0.794772684000839,
7.58217353749801));
#37711=CARTESIAN_POINT('Ctrl Pts',(-4.44867563298358,1.06847604194578,7.62139264277946));
#37712=CARTESIAN_POINT('Ctrl Pts',(-4.51561269110254,1.1851427086131,7.63745204139131));
#37713=CARTESIAN_POINT('Ctrl Pts',(-4.59357795707547,1.30000000000195,7.65259434114969));
#37714=CARTESIAN_POINT('Ctrl Pts',(-4.62334264925501,-1.3000000000003,7.44788165467971));
#37715=CARTESIAN_POINT('Ctrl Pts',(-4.54648329086464,-1.18514270861199,
7.45486630178287));
#37716=CARTESIAN_POINT('Ctrl Pts',(-4.47993360321558,-1.06847604194522,
7.46004142012346));
#37717=CARTESIAN_POINT('Ctrl Pts',(-4.35000791338186,-0.794772684000852,
7.4678166053326));
#37718=CARTESIAN_POINT('Ctrl Pts',(-4.29327346583404,-0.636309800095197,
7.46345145619193));
#37719=CARTESIAN_POINT('Ctrl Pts',(-4.21952367814165,-0.319434907277158,
7.47104479061018));
#37720=CARTESIAN_POINT('Ctrl Pts',(-4.1993445185557,-0.158333333333332,
7.47546103682555));
#37721=CARTESIAN_POINT('Ctrl Pts',(-4.19780196954188,0.158333333333334,
7.4958375256331));
#37722=CARTESIAN_POINT('Ctrl Pts',(-4.21663888113668,0.319434907277167,
7.50960329513933));
#37723=CARTESIAN_POINT('Ctrl Pts',(-4.2868386087941,0.636309800095206,7.5479853849349));
#37724=CARTESIAN_POINT('Ctrl Pts',(-4.34135241776995,0.794772684000839,
7.57948276964698));
#37725=CARTESIAN_POINT('Ctrl Pts',(-4.46768129760591,1.06847604194578,7.61888367845877));
#37726=CARTESIAN_POINT('Ctrl Pts',(-4.53266397770261,1.1851427086131,7.63470681844777));
#37727=CARTESIAN_POINT('Ctrl Pts',(-4.60794624676118,1.30000000000195,7.64929790494865));
#37728=CARTESIAN_POINT('Ctrl Pts',(-4.63777744145311,-1.3000000000003,7.44317884815643));
#37729=CARTESIAN_POINT('Ctrl Pts',(-4.56391391198511,-1.18514270861199,
7.44976250583294));
#37730=CARTESIAN_POINT('Ctrl Pts',(-4.49956220640914,-1.06847604194522,
7.4548250227973));
#37731=CARTESIAN_POINT('Ctrl Pts',(-4.37287110903858,-0.794772684000854,
7.46300631038979));
#37732=CARTESIAN_POINT('Ctrl Pts',(-4.31564116562494,-0.6363098000952,7.46034801937047));
#37733=CARTESIAN_POINT('Ctrl Pts',(-4.24200059940824,-0.31943490727716,
7.46841071460317));
#37734=CARTESIAN_POINT('Ctrl Pts',(-4.22080120062564,-0.158333333333333,
7.47153692196261));
#37735=CARTESIAN_POINT('Ctrl Pts',(-4.21922987515411,0.158333333333335,
7.49270076255547));
#37736=CARTESIAN_POINT('Ctrl Pts',(-4.23903267766996,0.319434907277168,
7.50897530883289));
#37737=CARTESIAN_POINT('Ctrl Pts',(-4.30911665623112,0.636309800095208,
7.54761311422366));
#37738=CARTESIAN_POINT('Ctrl Pts',(-4.36416991095692,0.794772684000843,
7.57699568476728));
#37739=CARTESIAN_POINT('Ctrl Pts',(-4.48732042833463,1.06847604194579,7.6155579202634));
#37740=CARTESIAN_POINT('Ctrl Pts',(-4.55013396214836,1.1851427086131,7.63121868568088));
#37741=CARTESIAN_POINT('Ctrl Pts',(-4.62245373397926,1.30000000000196,7.64584805364117));
#37742=CARTESIAN_POINT('Ctrl Pts',(-4.64917211308598,-1.30000000000031,
7.43850439917717));
#37743=CARTESIAN_POINT('Ctrl Pts',(-4.57756288722408,-1.18514270861199,
7.4447173982654));
#37744=CARTESIAN_POINT('Ctrl Pts',(-4.51486638728743,-1.06847604194522,
7.44971239799422));
#37745=CARTESIAN_POINT('Ctrl Pts',(-4.39061510991401,-0.794772684000856,
7.45843802443385));
#37746=CARTESIAN_POINT('Ctrl Pts',(-4.33301937306072,-0.6363098000952,7.45730186698481));
#37747=CARTESIAN_POINT('Ctrl Pts',(-4.25947297944506,-0.31943490727716,
7.4666540550818));
#37748=CARTESIAN_POINT('Ctrl Pts',(-4.23752467864517,-0.158333333333333,
7.47022849234999));
#37749=CARTESIAN_POINT('Ctrl Pts',(-4.23592101691603,0.158333333333335,
7.49206462085004));
#37750=CARTESIAN_POINT('Ctrl Pts',(-4.25640297863503,0.319434907277167,
7.50890472369068));
#37751=CARTESIAN_POINT('Ctrl Pts',(-4.32640311242899,0.636309800095208,
7.54692683029001));
#37752=CARTESIAN_POINT('Ctrl Pts',(-4.38190950729608,0.794772684000843,
7.57433453652904));
#37753=CARTESIAN_POINT('Ctrl Pts',(-4.50269748611023,1.06847604194578,7.61241799452743));
#37754=CARTESIAN_POINT('Ctrl Pts',(-4.56388830615953,1.1851427086131,7.62821040288113));
#37755=CARTESIAN_POINT('Ctrl Pts',(-4.63398530586503,1.30000000000196,7.64331030175218));
#37756=CARTESIAN_POINT('Ctrl Pts',(-4.6606296739892,-1.30000000000031,7.43416986317279));
#37757=CARTESIAN_POINT('Ctrl Pts',(-4.5913570163761,-1.18514270861199,7.44023858076217));
#37758=CARTESIAN_POINT('Ctrl Pts',(-4.53037198922488,-1.06847604194522,
7.44527262176997));
#37759=CARTESIAN_POINT('Ctrl Pts',(-4.40863046079444,-0.794772684000856,
7.45451195366465));
#37760=CARTESIAN_POINT('Ctrl Pts',(-4.3506248344246,-0.636309800095199,
7.45437946766052));
#37761=CARTESIAN_POINT('Ctrl Pts',(-4.27715204799888,-0.319434907277159,
7.46475922721751));
#37762=CARTESIAN_POINT('Ctrl Pts',(-4.254410018565,-0.158333333333333,7.46907130623477));
#37763=CARTESIAN_POINT('Ctrl Pts',(-4.25279259453082,0.158333333333335,
7.49098722395584));
#37764=CARTESIAN_POINT('Ctrl Pts',(-4.27404173721797,0.319434907277167,
7.50699230592871));
#37765=CARTESIAN_POINT('Ctrl Pts',(-4.34396627385687,0.636309800095207,
7.54451024511768));
#37766=CARTESIAN_POINT('Ctrl Pts',(-4.39989096848589,0.794772684000842,
7.57188784901723));
#37767=CARTESIAN_POINT('Ctrl Pts',(-4.5182235149054,1.06847604194578,7.60968824867482));
#37768=CARTESIAN_POINT('Ctrl Pts',(-4.57773690077526,1.1851427086131,7.62535146933581));
#37769=CARTESIAN_POINT('Ctrl Pts',(-4.6455418978228,1.30000000000196,7.64031551828881));
#37770=CARTESIAN_POINT('Ctrl Pts',(-4.68072279072018,-1.30000000000031,
7.42759731688899));
#37771=CARTESIAN_POINT('Ctrl Pts',(-4.61541911481721,-1.18514270861199,
7.43260381853245));
#37772=CARTESIAN_POINT('Ctrl Pts',(-4.557348277575,-1.06847604194523,7.43712245705713));
#37773=CARTESIAN_POINT('Ctrl Pts',(-4.43990233074511,-0.794772684000857,
7.44643435459863));
#37774=CARTESIAN_POINT('Ctrl Pts',(-4.38125332982614,-0.636309800095201,
7.44835440903243));
#37775=CARTESIAN_POINT('Ctrl Pts',(-4.30794495913783,-0.319434907277161,
7.46039562465073));
#37776=CARTESIAN_POINT('Ctrl Pts',(-4.28386650027582,-0.158333333333333,
7.4654873767949));
#37777=CARTESIAN_POINT('Ctrl Pts',(-4.28222139972213,0.158333333333335,
7.48835864464172));
#37778=CARTESIAN_POINT('Ctrl Pts',(-4.30474728282048,0.319434907277169,
7.50515701844512));
#37779=CARTESIAN_POINT('Ctrl Pts',(-4.37451623579684,0.63630980009521,7.54170144404907));
#37780=CARTESIAN_POINT('Ctrl Pts',(-4.43116658239244,0.794772684000845,
7.56616428453284));
#37781=CARTESIAN_POINT('Ctrl Pts',(-4.54525640247321,1.06847604194579,7.60313466934228));
#37782=CARTESIAN_POINT('Ctrl Pts',(-4.60187326939733,1.1851427086131,7.61891801345069));
#37783=CARTESIAN_POINT('Ctrl Pts',(-4.66572174757695,1.30000000000196,7.63448159197121));
#37784=CARTESIAN_POINT('Ctrl Pts',(-4.72058200346455,-1.30000000000031,
7.41055955717715));
#37785=CARTESIAN_POINT('Ctrl Pts',(-4.66328542491091,-1.18514270861199,
7.41376769125186));
#37786=CARTESIAN_POINT('Ctrl Pts',(-4.61110369976158,-1.06847604194523,
7.41757424322289));
#37787=CARTESIAN_POINT('Ctrl Pts',(-4.50236981033514,-0.794772684000858,
7.42775060482769));
#37788=CARTESIAN_POINT('Ctrl Pts',(-4.44249347992462,-0.636309800095199,
7.43416823300931));
#37789=CARTESIAN_POINT('Ctrl Pts',(-4.36958159441681,-0.319434907277159,
7.4502898228441));
#37790=CARTESIAN_POINT('Ctrl Pts',(-4.3428278760223,-0.158333333333332,
7.4582033613571));
#37791=CARTESIAN_POINT('Ctrl Pts',(-4.34115514161927,0.158333333333334,
7.48189348506881));
#37792=CARTESIAN_POINT('Ctrl Pts',(-4.36625935696994,0.319434907277166,
7.49638018296511));
#37793=CARTESIAN_POINT('Ctrl Pts',(-4.43571668233373,0.636309800095206,
7.53114107694557));
#37794=CARTESIAN_POINT('Ctrl Pts',(-4.4937939437635,0.794772684000839,7.55400281128164));
#37795=CARTESIAN_POINT('Ctrl Pts',(-4.59936624074172,1.06847604194579,7.59088089537082));
#37796=CARTESIAN_POINT('Ctrl Pts',(-4.65017390543712,1.18514270861311,7.60709116052329));
#37797=CARTESIAN_POINT('Ctrl Pts',(-4.70609089930505,1.30000000000197,7.62354853469364));
#37798=CARTESIAN_POINT('Ctrl Pts',(-4.75619240536058,-1.30000000000032,
7.39667294505808));
#37799=CARTESIAN_POINT('Ctrl Pts',(-4.70590917649517,-1.18514270861201,
7.39755866929844));
#37800=CARTESIAN_POINT('Ctrl Pts',(-4.65888186664025,-1.06847604194524,
7.39990867579963));
#37801=CARTESIAN_POINT('Ctrl Pts',(-4.55776119735292,-0.79477268400087,
7.40872044588576));
#37802=CARTESIAN_POINT('Ctrl Pts',(-4.49674677444273,-0.636309800095208,
7.41685452571745));
#37803=CARTESIAN_POINT('Ctrl Pts',(-4.42422834751872,-0.319434907277163,
7.4353232018333));
#37804=CARTESIAN_POINT('Ctrl Pts',(-4.39525391132892,-0.158333333333335,
7.4460826510108));
#37805=CARTESIAN_POINT('Ctrl Pts',(-4.39362598481891,0.158333333333337,
7.47138174563145));
#37806=CARTESIAN_POINT('Ctrl Pts',(-4.4209867281482,0.319434907277172,7.48549553851834));
#37807=CARTESIAN_POINT('Ctrl Pts',(-4.49016019306676,0.636309800095216,
7.51942672754422));
#37808=CARTESIAN_POINT('Ctrl Pts',(-4.54948882348156,0.794772684000852,
7.53987197370938));
#37809=CARTESIAN_POINT('Ctrl Pts',(-4.64749609348585,1.0684760419458,7.57715869939665));
#37810=CARTESIAN_POINT('Ctrl Pts',(-4.69314798885547,1.18514270861312,7.59418710374468));
#37811=CARTESIAN_POINT('Ctrl Pts',(-4.742028063937,1.30000000000198,7.61210387050001));
#37812=CARTESIAN_POINT('Ctrl Pts',(-4.78159245634849,-1.30000000000032,
7.38452953948181));
#37813=CARTESIAN_POINT('Ctrl Pts',(-4.73640400144256,-1.18514270861201,
7.38403131096895));
#37814=CARTESIAN_POINT('Ctrl Pts',(-4.69312438118273,-1.06847604194524,
7.38559077565983));
#37815=CARTESIAN_POINT('Ctrl Pts',(-4.59754959021777,-0.794772684000866,
7.39394713400638));
#37816=CARTESIAN_POINT('Ctrl Pts',(-4.53574283459765,-0.636309800095209,
7.40389616287617));
#37817=CARTESIAN_POINT('Ctrl Pts',(-4.46351035596197,-0.319434907277165,
7.4237879980083));
#37818=CARTESIAN_POINT('Ctrl Pts',(-4.43288546941762,-0.158333333333335,
7.43553357003229));
#37819=CARTESIAN_POINT('Ctrl Pts',(-4.43128483385098,0.158333333333337,
7.46145478870264));
#37820=CARTESIAN_POINT('Ctrl Pts',(-4.46030592709637,0.319434907277171,
7.47529081311309));
#37821=CARTESIAN_POINT('Ctrl Pts',(-4.52928445840577,0.636309800095217,
7.5088904200637));
#37822=CARTESIAN_POINT('Ctrl Pts',(-4.58948824265808,0.794772684000855,
7.52806622772443));
#37823=CARTESIAN_POINT('Ctrl Pts',(-4.682065906496,1.0684760419458,7.56631566101118));
#37824=CARTESIAN_POINT('Ctrl Pts',(-4.72402097248571,1.18514270861312,7.58425210078832));
#37825=CARTESIAN_POINT('Ctrl Pts',(-4.76785766413012,1.30000000000198,7.6035682179539));
#37826=CARTESIAN_POINT('Ctrl Pts',(-4.78724263544867,-1.30000000000032,
7.38189848275631));
#37827=CARTESIAN_POINT('Ctrl Pts',(-4.74317456636349,-1.185142708612,7.38098582392651));
#37828=CARTESIAN_POINT('Ctrl Pts',(-4.70071991070143,-1.06847604194524,
7.38229294656453));
#37829=CARTESIAN_POINT('Ctrl Pts',(-4.60636847086696,-0.794772684000865,
7.39044080060378));
#37830=CARTESIAN_POINT('Ctrl Pts',(-4.54439171706508,-0.636309800095209,
7.40079181135806));
#37831=CARTESIAN_POINT('Ctrl Pts',(-4.4722304122187,-0.319434907277165,
7.42106915937384));
#37832=CARTESIAN_POINT('Ctrl Pts',(-4.44125148812159,-0.158333333333335,
7.43321918233995));
#37833=CARTESIAN_POINT('Ctrl Pts',(-4.43965915366256,0.158333333333337,
7.45929086929445));
#37834=CARTESIAN_POINT('Ctrl Pts',(-4.46904138652334,0.319434907277172,
7.47294053951429));
#37835=CARTESIAN_POINT('Ctrl Pts',(-4.53796809517026,0.636309800095217,
7.50632337232342));
#37836=CARTESIAN_POINT('Ctrl Pts',(-4.59835652138401,0.794772684000854,
7.52505510834564));
#37837=CARTESIAN_POINT('Ctrl Pts',(-4.68972657257818,1.0684760419458,7.56350553669529));
#37838=CARTESIAN_POINT('Ctrl Pts',(-4.73086219664383,1.18514270861312,7.58168090727336));
#37839=CARTESIAN_POINT('Ctrl Pts',(-4.77358273520712,1.30000000000198,7.60138788272565));
#37840=CARTESIAN_POINT('Ctrl Pts',(-4.79573463031585,-1.30000000000032,
7.37812243727755));
#37841=CARTESIAN_POINT('Ctrl Pts',(-4.75332696102845,-1.18514270861201,
7.3764183801566));
#37842=CARTESIAN_POINT('Ctrl Pts',(-4.71209659401335,-1.06847604194524,
7.37723615010075));
#37843=CARTESIAN_POINT('Ctrl Pts',(-4.61956600186943,-0.794772684000868,
7.38495128727626));
#37844=CARTESIAN_POINT('Ctrl Pts',(-4.55735067689832,-0.636309800095211,
7.39603127227243));
#37845=CARTESIAN_POINT('Ctrl Pts',(-4.48530329615657,-0.319434907277166,
7.41696807003476));
#37846=CARTESIAN_POINT('Ctrl Pts',(-4.45379954175104,-0.158333333333336,
7.42983981676956));
#37847=CARTESIAN_POINT('Ctrl Pts',(-4.45221924396623,0.158333333333337,
7.4561124445076));
#37848=CARTESIAN_POINT('Ctrl Pts',(-4.4821330754945,0.319434907277172,7.46929534312405));
#37849=CARTESIAN_POINT('Ctrl Pts',(-4.55098110905412,0.636309800095218,
7.50231801079879));
#37850=CARTESIAN_POINT('Ctrl Pts',(-4.61165683769535,0.794772684000857,
7.52057094572087));
#37851=CARTESIAN_POINT('Ctrl Pts',(-4.70121335968738,1.0684760419458,7.55924305725064));
#37852=CARTESIAN_POINT('Ctrl Pts',(-4.74111652794842,1.18514270861312,7.57769178830973));
#37853=CARTESIAN_POINT('Ctrl Pts',(-4.78215716449621,1.30000000000198,7.5978495262896));
#37854=CARTESIAN_POINT('Ctrl Pts',(-4.80424392564089,-1.30000000000032,
7.37453487689565));
#37855=CARTESIAN_POINT('Ctrl Pts',(-4.7634901105747,-1.18514270861201,7.37200723460166));
#37856=CARTESIAN_POINT('Ctrl Pts',(-4.72347848273184,-1.06847604194524,
7.37230262570058));
#37857=CARTESIAN_POINT('Ctrl Pts',(-4.6327582190761,-0.794772684000867,
7.3795068101154));
#37858=CARTESIAN_POINT('Ctrl Pts',(-4.57029597217174,-0.636309800095211,
7.39121525105204));
#37859=CARTESIAN_POINT('Ctrl Pts',(-4.49836555817877,-0.319434907277166,
7.41282614349591));
#37860=CARTESIAN_POINT('Ctrl Pts',(-4.46634941917561,-0.158333333333335,
7.42649666961214));
#37861=CARTESIAN_POINT('Ctrl Pts',(-4.4647946338716,0.158333333333337,7.45314212589848));
#37862=CARTESIAN_POINT('Ctrl Pts',(-4.49524481309089,0.319434907277172,
7.46597526879084));
#37863=CARTESIAN_POINT('Ctrl Pts',(-4.56403100297875,0.636309800095218,
7.49892806274145));
#37864=CARTESIAN_POINT('Ctrl Pts',(-4.62501250401097,0.794772684000857,
7.51697123685178));
#37865=CARTESIAN_POINT('Ctrl Pts',(-4.71276269964325,1.0684760419458,7.55606737412409));
#37866=CARTESIAN_POINT('Ctrl Pts',(-4.75143286611581,1.18514270861312,7.5748406813716));
#37867=CARTESIAN_POINT('Ctrl Pts',(-4.79078939083679,1.30000000000198,7.59546402669605));
#37868=CARTESIAN_POINT('Ctrl Pts',(-4.82116392366532,-1.30000000000033,
7.36648906419669));
#37869=CARTESIAN_POINT('Ctrl Pts',(-4.78379435131418,-1.18514270861201,
7.36295501392018));
#37870=CARTESIAN_POINT('Ctrl Pts',(-4.74627296491281,-1.06847604194524,
7.36265612615519));
#37871=CARTESIAN_POINT('Ctrl Pts',(-4.65924033537166,-0.794772684000869,
7.36943950821944));
#37872=CARTESIAN_POINT('Ctrl Pts',(-4.59626304788614,-0.636309800095212,
7.38238506314081));
#37873=CARTESIAN_POINT('Ctrl Pts',(-4.52451696391414,-0.319434907277167,
7.40479741221343));
#37874=CARTESIAN_POINT('Ctrl Pts',(-4.49139649387496,-0.158333333333336,
7.41909656029638));
#37875=CARTESIAN_POINT('Ctrl Pts',(-4.48982928135806,0.158333333333338,
7.44571920738321));
#37876=CARTESIAN_POINT('Ctrl Pts',(-4.52133173317534,0.319434907277174,
7.45760023335444));
#37877=CARTESIAN_POINT('Ctrl Pts',(-4.58998900565639,0.636309800095222,
7.49031758521192));
#37878=CARTESIAN_POINT('Ctrl Pts',(-4.65161473512541,0.79477268400086,7.50833480079011));
#37879=CARTESIAN_POINT('Ctrl Pts',(-4.73577439163365,1.06847604194581,7.54844247985107));
#37880=CARTESIAN_POINT('Ctrl Pts',(-4.77198716776143,1.18514270861313,7.56790475507659));
#37881=CARTESIAN_POINT('Ctrl Pts',(-4.80798312313707,1.30000000000198,7.58946817739808));
#37882=CARTESIAN_POINT('Ctrl Pts',(-4.84216943247133,-1.30000000000034,
7.35556326655833));
#37883=CARTESIAN_POINT('Ctrl Pts',(-4.8088626711365,-1.18514270861203,7.34958957289585));
#37884=CARTESIAN_POINT('Ctrl Pts',(-4.77434749389395,-1.06847604194526,
7.34775870979043));
#37885=CARTESIAN_POINT('Ctrl Pts',(-4.69181884723649,-0.794772684000882,
7.35309981711123));
#37886=CARTESIAN_POINT('Ctrl Pts',(-4.62831370858818,-0.63630980009522,
7.36800584919602));
#37887=CARTESIAN_POINT('Ctrl Pts',(-4.55695114658674,-0.31943490727717,
7.39253573421515));
#37888=CARTESIAN_POINT('Ctrl Pts',(-4.52260959946483,-0.158333333333338,
7.40901668765982));
#37889=CARTESIAN_POINT('Ctrl Pts',(-4.52119448799517,0.15833333333334,7.43731905635201));
#37890=CARTESIAN_POINT('Ctrl Pts',(-4.55412793237604,0.31943490727718,7.44965249956768));
#37891=CARTESIAN_POINT('Ctrl Pts',(-4.62259373792968,0.63630980009523,7.48172953763251));
#37892=CARTESIAN_POINT('Ctrl Pts',(-4.68477221076676,0.794772684000869,
7.49662215096969));
#37893=CARTESIAN_POINT('Ctrl Pts',(-4.76439994582661,1.06847604194582,7.53744782378967));
#37894=CARTESIAN_POINT('Ctrl Pts',(-4.79756444748894,1.18514270861314,7.55804906096945));
#37895=CARTESIAN_POINT('Ctrl Pts',(-4.82942555480448,1.300000000002,7.58157961430544));
#37896=CARTESIAN_POINT('Ctrl Pts',(-4.86471527153658,-1.30000000000035,
7.34509153261728));
#37897=CARTESIAN_POINT('Ctrl Pts',(-4.83589630809817,-1.18514270861203,
7.33769155048644));
#37898=CARTESIAN_POINT('Ctrl Pts',(-4.80466872282125,-1.06847604194526,
7.33485296909692));
#37899=CARTESIAN_POINT('Ctrl Pts',(-4.72696235548441,-0.794772684000882,
7.3388330264484));
#37900=CARTESIAN_POINT('Ctrl Pts',(-4.66262689024078,-0.636309800095225,
7.3539602446291));
#37901=CARTESIAN_POINT('Ctrl Pts',(-4.5914984942633,-0.319434907277175,
7.37925740599487));
#37902=CARTESIAN_POINT('Ctrl Pts',(-4.55583447616005,-0.158333333333339,
7.3977301527819));
#37903=CARTESIAN_POINT('Ctrl Pts',(-4.55442495747738,0.158333333333341,
7.42603311863638));
#37904=CARTESIAN_POINT('Ctrl Pts',(-4.5886487993213,0.31943490727718,7.4360003318052));
#37905=CARTESIAN_POINT('Ctrl Pts',(-4.6569685545072,0.636309800095233,7.46807522688327));
#37906=CARTESIAN_POINT('Ctrl Pts',(-4.72014068304638,0.794772684000876,
7.48454481489632));
#37907=CARTESIAN_POINT('Ctrl Pts',(-4.79503056754589,1.06847604194583,7.52706756803765));
#37908=CARTESIAN_POINT('Ctrl Pts',(-4.82492219359691,1.18514270861315,7.54847119076495));
#37909=CARTESIAN_POINT('Ctrl Pts',(-4.85228838964271,1.30000000000201,7.57287191200792));
#37910=CARTESIAN_POINT('Ctrl Pts',(-4.88704394490281,-1.30000000000036,
7.33321427224023));
#37911=CARTESIAN_POINT('Ctrl Pts',(-4.86253353208781,-1.18514270861205,
7.32318476000548));
#37912=CARTESIAN_POINT('Ctrl Pts',(-4.83449612414015,-1.06847604194527,
7.31868392688339));
#37913=CARTESIAN_POINT('Ctrl Pts',(-4.76157603858742,-0.794772684000892,
7.32105845674154));
#37914=CARTESIAN_POINT('Ctrl Pts',(-4.69671678765166,-0.636309800095229,
7.3384858027196));
#37915=CARTESIAN_POINT('Ctrl Pts',(-4.62596803169993,-0.319434907277175,
7.36547258104057));
#37916=CARTESIAN_POINT('Ctrl Pts',(-4.58893586763949,-0.158333333333341,
7.38531685764692));
#37917=CARTESIAN_POINT('Ctrl Pts',(-4.58765224720057,0.158333333333343,
7.41480981799401));
#37918=CARTESIAN_POINT('Ctrl Pts',(-4.62340111677445,0.319434907277185,
7.42516619984583));
#37919=CARTESIAN_POINT('Ctrl Pts',(-4.69153456637431,0.636309800095241,
7.45681292809196));
#37920=CARTESIAN_POINT('Ctrl Pts',(-4.75533149080953,0.794772684000879,
7.47071865145091));
#37921=CARTESIAN_POINT('Ctrl Pts',(-4.82542784121493,1.06847604194583,7.51433058353202));
#37922=CARTESIAN_POINT('Ctrl Pts',(-4.85208582812171,1.18514270861316,7.53698574062284));
#37923=CARTESIAN_POINT('Ctrl Pts',(-4.87505968917045,1.30000000000202,7.56341806538787));
#37924=CARTESIAN_POINT('Ctrl Pts',(-4.90657768141063,-1.30000000000039,
7.32290090103421));
#37925=CARTESIAN_POINT('Ctrl Pts',(-4.88587644251424,-1.18514270861207,
7.31093727223514));
#37926=CARTESIAN_POINT('Ctrl Pts',(-4.86065279659967,-1.06847604194529,
7.30519616613079));
#37927=CARTESIAN_POINT('Ctrl Pts',(-4.79193346364755,-0.794772684000907,
7.30630833476157));
#37928=CARTESIAN_POINT('Ctrl Pts',(-4.726589320251,-0.636309800095241,7.32552593661041));
#37929=CARTESIAN_POINT('Ctrl Pts',(-4.6560830739072,-0.319434907277181,
7.35320238465496));
#37930=CARTESIAN_POINT('Ctrl Pts',(-4.61775946080383,-0.158333333333344,
7.37345657161974));
#37931=CARTESIAN_POINT('Ctrl Pts',(-4.6164647011132,0.158333333333345,7.40279181157517));
#37932=CARTESIAN_POINT('Ctrl Pts',(-4.65342039867833,0.31943490727719,7.41204353265549));
#37933=CARTESIAN_POINT('Ctrl Pts',(-4.72143832595232,0.636309800095251,
7.44377321758268));
#37934=CARTESIAN_POINT('Ctrl Pts',(-4.78602682992026,0.794772684000895,
7.45807417436264));
#37935=CARTESIAN_POINT('Ctrl Pts',(-4.85202756920001,1.06847604194585,7.50353636787379));
#37936=CARTESIAN_POINT('Ctrl Pts',(-4.87586835858379,1.18514270861318,7.52731501341855));
#37937=CARTESIAN_POINT('Ctrl Pts',(-4.89498066288547,1.30000000000204,7.55519340547731));
#37938=CARTESIAN_POINT('Ctrl Pts',(-4.92893700457517,-1.3000000000004,7.31156188893225));
#37939=CARTESIAN_POINT('Ctrl Pts',(-4.91258729373097,-1.18514270861208,
7.29737510222025));
#37940=CARTESIAN_POINT('Ctrl Pts',(-4.89055620351791,-1.06847604194531,
7.2900570681081));
#37941=CARTESIAN_POINT('Ctrl Pts',(-4.82653485492317,-0.794772684000918,
7.28901913793627));
#37942=CARTESIAN_POINT('Ctrl Pts',(-4.76039738489715,-0.63630980009525,
7.30861852477781));
#37943=CARTESIAN_POINT('Ctrl Pts',(-4.69019280711872,-0.319434907277186,
7.33729173276116));
#37944=CARTESIAN_POINT('Ctrl Pts',(-4.6506343999844,-0.158333333333346,
7.35966435741067));
#37945=CARTESIAN_POINT('Ctrl Pts',(-4.64949257205487,0.158333333333348,
7.39016580818862));
#37946=CARTESIAN_POINT('Ctrl Pts',(-4.68790778944678,0.319434907277195,
7.39912505243672));
#37947=CARTESIAN_POINT('Ctrl Pts',(-4.75578931986187,0.636309800095261,
7.43088960159304));
#37948=CARTESIAN_POINT('Ctrl Pts',(-4.82112875195722,0.794772684000907,
7.44406967143752));
#37949=CARTESIAN_POINT('Ctrl Pts',(-4.88239462582399,1.06847604194587,7.49108475371676));
#37950=CARTESIAN_POINT('Ctrl Pts',(-4.90301066772921,1.1851427086132,7.51609182245864));
#37951=CARTESIAN_POINT('Ctrl Pts',(-4.91772302486701,1.30000000000206,7.54575487290414));
#37952=CARTESIAN_POINT('Ctrl Pts',(-4.94276812717222,-1.30000000000042,
7.30353165417581));
#37953=CARTESIAN_POINT('Ctrl Pts',(-4.92910617557147,-1.1851427086121,7.28785768897104));
#37954=CARTESIAN_POINT('Ctrl Pts',(-4.90905961567349,-1.06847604194532,
7.27955583815619));
#37955=CARTESIAN_POINT('Ctrl Pts',(-4.84799832960546,-0.79477268400093,
7.27740796102146));
#37956=CARTESIAN_POINT('Ctrl Pts',(-4.78148095270192,-0.636309800095261,
7.29792502713165));
#37957=CARTESIAN_POINT('Ctrl Pts',(-4.71150402741766,-0.319434907277192,
7.32741460625986));
#37958=CARTESIAN_POINT('Ctrl Pts',(-4.67115338279767,-0.158333333333349,
7.35096105844497));
#37959=CARTESIAN_POINT('Ctrl Pts',(-4.67005823101757,0.15833333333335,7.38172799267763));
#37960=CARTESIAN_POINT('Ctrl Pts',(-4.70930946320504,0.319434907277199,
7.38981036950598));
#37961=CARTESIAN_POINT('Ctrl Pts',(-4.77706432180903,0.636309800095271,
7.42123520250692));
#37962=CARTESIAN_POINT('Ctrl Pts',(-4.84286804636516,0.794772684000922,
7.43373837818253));
#37963=CARTESIAN_POINT('Ctrl Pts',(-4.90122283435496,1.06847604194589,7.48211551282895));
#37964=CARTESIAN_POINT('Ctrl Pts',(-4.91985996547775,1.18514270861322,7.50817717942918));
#37965=CARTESIAN_POINT('Ctrl Pts',(-4.93187460226044,1.30000000000208,7.53935984359063));
#37966=CARTESIAN_POINT('Ctrl Pts',(-4.9538826414882,-1.30000000000043,7.29750420865769));
#37967=CARTESIAN_POINT('Ctrl Pts',(-4.94237897545242,-1.1851427086121,7.28065982526099));
#37968=CARTESIAN_POINT('Ctrl Pts',(-4.9239198168277,-1.06847604194533,7.27154899581461));
#37969=CARTESIAN_POINT('Ctrl Pts',(-4.86520688834062,-0.794772684000932,
7.26836721389572));
#37970=CARTESIAN_POINT('Ctrl Pts',(-4.79832348941349,-0.636309800095262,
7.28924975962404));
#37971=CARTESIAN_POINT('Ctrl Pts',(-4.72852281268025,-0.319434907277192,
7.3193741434352));
#37972=CARTESIAN_POINT('Ctrl Pts',(-4.68758819801886,-0.158333333333349,
7.3441861406594));
#37973=CARTESIAN_POINT('Ctrl Pts',(-4.68654436898808,0.158333333333351,
7.37528164155598));
#37974=CARTESIAN_POINT('Ctrl Pts',(-4.72645104332334,0.3194349072772,7.38261274912261));
#37975=CARTESIAN_POINT('Ctrl Pts',(-4.79409315133171,0.636309800095272,
7.41369376798486));
#37976=CARTESIAN_POINT('Ctrl Pts',(-4.86025356328873,0.794772684000922,
7.42552056445429));
#37977=CARTESIAN_POINT('Ctrl Pts',(-4.91627584311807,1.06847604194589,7.47494594133525));
#37978=CARTESIAN_POINT('Ctrl Pts',(-4.93333146029785,1.18514270861322,7.50185755652872));
#37979=CARTESIAN_POINT('Ctrl Pts',(-4.94319272554928,1.30000000000208,7.53428637265453));
#37980=CARTESIAN_POINT('Ctrl Pts',(-4.96215724239579,-1.30000000000043,
7.29262963018817));
#37981=CARTESIAN_POINT('Ctrl Pts',(-4.95223365671038,-1.18514270861211,
7.2747178533983));
#37982=CARTESIAN_POINT('Ctrl Pts',(-4.93494771744396,-1.06847604194533,
7.26492096827301));
#37983=CARTESIAN_POINT('Ctrl Pts',(-4.87800523009233,-0.794772684000934,
7.26103522689715));
#37984=CARTESIAN_POINT('Ctrl Pts',(-4.81096227090518,-0.636309800095264,
7.28284066593449));
#37985=CARTESIAN_POINT('Ctrl Pts',(-4.74130390136971,-0.319434907277193,
7.31344134352605));
#37986=CARTESIAN_POINT('Ctrl Pts',(-4.69983863963916,-0.158333333333349,
7.33855502594921));
#37987=CARTESIAN_POINT('Ctrl Pts',(-4.69883417799421,0.158333333333351,
7.36991044588953));
#37988=CARTESIAN_POINT('Ctrl Pts',(-4.73929568703575,0.3194349072772,7.37714562001663));
#37989=CARTESIAN_POINT('Ctrl Pts',(-4.8069065964319,0.636309800095273,7.40839011633368));
#37990=CARTESIAN_POINT('Ctrl Pts',(-4.87338113727392,0.794772684000924,
7.42011569025137));
#37991=CARTESIAN_POINT('Ctrl Pts',(-4.92764623373385,1.06847604194589,7.47025282760673));
#37992=CARTESIAN_POINT('Ctrl Pts',(-4.94349629326561,1.18514270861322,7.49763280042375));
#37993=CARTESIAN_POINT('Ctrl Pts',(-4.95170706279155,1.30000000000209,7.53069023706064));
#37994=CARTESIAN_POINT('Ctrl Pts',(-4.96904374222928,-1.30000000000044,
7.28854505812584));
#37995=CARTESIAN_POINT('Ctrl Pts',(-4.96042052541168,-1.18514270861211,
7.26964689949081));
#37996=CARTESIAN_POINT('Ctrl Pts',(-4.94410226763909,-1.06847604194533,
7.2592195633072));
#37997=CARTESIAN_POINT('Ctrl Pts',(-4.88862674373442,-0.794772684000939,
7.2546996251866));
#37998=CARTESIAN_POINT('Ctrl Pts',(-4.82147221694671,-0.636309800095268,
7.27741426685326));
#37999=CARTESIAN_POINT('Ctrl Pts',(-4.75193604936788,-0.319434907277195,
7.30841654884995));
#38000=CARTESIAN_POINT('Ctrl Pts',(-4.71002121431227,-0.15833333333335,
7.3337009050263));
#38001=CARTESIAN_POINT('Ctrl Pts',(-4.70904729083083,0.158333333333352,
7.36524202054646));
#38002=CARTESIAN_POINT('Ctrl Pts',(-4.74996964632282,0.319434907277201,
7.37239217961628));
#38003=CARTESIAN_POINT('Ctrl Pts',(-4.81755979929811,0.636309800095276,
7.4038170879835));
#38004=CARTESIAN_POINT('Ctrl Pts',(-4.8843054138207,0.794772684000929,7.41554223504929));
#38005=CARTESIAN_POINT('Ctrl Pts',(-4.93711398704773,1.0684760419459,7.46632498981442));
#38006=CARTESIAN_POINT('Ctrl Pts',(-4.95196218304734,1.18514270861323,7.49410887472559));
#38007=CARTESIAN_POINT('Ctrl Pts',(-4.95879970044698,1.30000000000209,7.52769467169654));
#38008=CARTESIAN_POINT('Ctrl Pts',(-4.97388099006215,-1.30000000000044,
7.28578416877527));
#38009=CARTESIAN_POINT('Ctrl Pts',(-4.96618885844481,-1.18514270861211,
7.26631812393833));
#38010=CARTESIAN_POINT('Ctrl Pts',(-4.95055672722461,-1.06847604194533,
7.25550099325927));
#38011=CARTESIAN_POINT('Ctrl Pts',(-4.89610038943475,-0.79477268400094,
7.25049197934511));
#38012=CARTESIAN_POINT('Ctrl Pts',(-4.82880131880616,-0.636309800095269,
7.27344835749128));
#38013=CARTESIAN_POINT('Ctrl Pts',(-4.75934190858374,-0.319434907277196,
7.30468767637323));
#38014=CARTESIAN_POINT('Ctrl Pts',(-4.71715983708938,-0.15833333333335,
7.33039352380046));
#38015=CARTESIAN_POINT('Ctrl Pts',(-4.71621018252856,0.158333333333352,
7.36207232505676));
#38016=CARTESIAN_POINT('Ctrl Pts',(-4.75742869369747,0.319434907277202,
7.36898193694131));
#38017=CARTESIAN_POINT('Ctrl Pts',(-4.82498205099828,0.636309800095277,
7.40036215025163));
#38018=CARTESIAN_POINT('Ctrl Pts',(-4.89189296390852,0.794772684000931,
7.41187977881973));
#38019=CARTESIAN_POINT('Ctrl Pts',(-4.94369104604812,1.0684760419459,7.4631905316123));
#38020=CARTESIAN_POINT('Ctrl Pts',(-4.95785081403603,1.18514270861323,7.49136397433223));
#38021=CARTESIAN_POINT('Ctrl Pts',(-4.96374887956164,1.3000000000021,7.52550033613888));
#38022=CARTESIAN_POINT('Ctrl Pts',(-4.97630270097834,-1.30000000000044,
7.2844238033571));
#38023=CARTESIAN_POINT('Ctrl Pts',(-4.96907918430619,-1.18514270861211,
7.26469184565172));
#38024=CARTESIAN_POINT('Ctrl Pts',(-4.95379125816367,-1.06847604194533,
7.2536865197006));
#38025=CARTESIAN_POINT('Ctrl Pts',(-4.89984269127916,-0.794772684000939,
7.24842228025466));
#38026=CARTESIAN_POINT('Ctrl Pts',(-4.83246023827133,-0.636309800095268,
7.27143376544033));
#38027=CARTESIAN_POINT('Ctrl Pts',(-4.76303744189354,-0.319434907277195,
7.3027823689946));
#38028=CARTESIAN_POINT('Ctrl Pts',(-4.72072944001479,-0.15833333333335,
7.32874778853514));
#38029=CARTESIAN_POINT('Ctrl Pts',(-4.71979232494156,0.158333333333352,
7.3604957560239));
#38030=CARTESIAN_POINT('Ctrl Pts',(-4.76115473178469,0.319434907277202,
7.36725593780331));
#38031=CARTESIAN_POINT('Ctrl Pts',(-4.82868596530568,0.636309800095277,
7.39858428837193));
#38032=CARTESIAN_POINT('Ctrl Pts',(-4.89567510113326,0.79477268400093,7.40996091959273));
#38033=CARTESIAN_POINT('Ctrl Pts',(-4.94696966254457,1.0684760419459,7.46154837310563));
#38034=CARTESIAN_POINT('Ctrl Pts',(-4.96078757083251,1.18514270861323,7.48993503887023));
#38035=CARTESIAN_POINT('Ctrl Pts',(-4.96621987242418,1.3000000000021,7.52437807327715));
#38036=CARTESIAN_POINT('Ctrl Pts',(-4.97751398613919,-1.30000000000044,
7.28374645930059));
#38037=CARTESIAN_POINT('Ctrl Pts',(-4.97052541992915,-1.18514270861211,
7.26388559369294));
#38038=CARTESIAN_POINT('Ctrl Pts',(-4.95540983892336,-1.06847604194533,
7.25278776428831));
#38039=CARTESIAN_POINT('Ctrl Pts',(-4.90171479295647,-0.794772684000939,
7.24739392491884));
#38040=CARTESIAN_POINT('Ctrl Pts',(-4.83428843862465,-0.636309800095268,
7.27041965738315));
#38041=CARTESIAN_POINT('Ctrl Pts',(-4.76488342798957,-0.319434907277195,
7.30181978514875));
#38042=CARTESIAN_POINT('Ctrl Pts',(-4.72251363369622,-0.15833333333335,
7.32792219164892));
#38043=CARTESIAN_POINT('Ctrl Pts',(-4.72158292793032,0.158333333333352,
7.35970515916855));
#38044=CARTESIAN_POINT('Ctrl Pts',(-4.76301691052441,0.319434907277202,
7.36638801246319));
#38045=CARTESIAN_POINT('Ctrl Pts',(-4.83053654094601,0.636309800095277,
7.39768590388837));
#38046=CARTESIAN_POINT('Ctrl Pts',(-4.89756383643552,0.79477268400093,7.40898434675011));
#38047=CARTESIAN_POINT('Ctrl Pts',(-4.94860690981511,1.0684760419459,7.4607117121741));
#38048=CARTESIAN_POINT('Ctrl Pts',(-4.96225430443568,1.18514270861323,7.48920795008445));
#38049=CARTESIAN_POINT('Ctrl Pts',(-4.96745443854299,1.3000000000021,7.52380956610082));
#38050=CARTESIAN_POINT('Ctrl Pts',(-4.97820627814295,-1.30000000000044,
7.28336032475575));
#38051=CARTESIAN_POINT('Ctrl Pts',(-4.971352034479,-1.18514270861211,7.26342613826192));
#38052=CARTESIAN_POINT('Ctrl Pts',(-4.95633495359243,-1.06847604194533,
7.25227550350771));
#38053=CARTESIAN_POINT('Ctrl Pts',(-4.90278470563348,-0.794772684000939,
7.24680706821067));
#38054=CARTESIAN_POINT('Ctrl Pts',(-4.83533294408251,-0.636309800095269,
7.26983886751155));
#38055=CARTESIAN_POINT('Ctrl Pts',(-4.76593808327655,-0.319434907277196,
7.3012684086979));
#38056=CARTESIAN_POINT('Ctrl Pts',(-4.7235333012043,-0.15833333333335,7.32745135262338));
#38057=CARTESIAN_POINT('Ctrl Pts',(-4.72260623327306,0.158333333333352,
7.35925411712625));
#38058=CARTESIAN_POINT('Ctrl Pts',(-4.76408083964513,0.319434907277202,
7.36589081709313));
#38059=CARTESIAN_POINT('Ctrl Pts',(-4.83159366012784,0.636309800095277,
7.39716990722543));
#38060=CARTESIAN_POINT('Ctrl Pts',(-4.89864264437605,0.79477268400093,7.40842250430178));
#38061=CARTESIAN_POINT('Ctrl Pts',(-4.94954210729726,1.0684760419459,7.4602306906211));
#38062=CARTESIAN_POINT('Ctrl Pts',(-4.96309216930703,1.18514270861323,7.48879047475649));
#38063=CARTESIAN_POINT('Ctrl Pts',(-4.96815980183889,1.3000000000021,7.52348419885205));
#38064=CARTESIAN_POINT('Ctrl Pts',(-4.98962759657728,-1.30000000000043,
7.27698199631737));
#38065=CARTESIAN_POINT('Ctrl Pts',(-4.98499149296135,-1.18514270861211,
7.25585362164017));
#38066=CARTESIAN_POINT('Ctrl Pts',(-4.97160014405788,-1.06847604194533,
7.24383836076752));
#38067=CARTESIAN_POINT('Ctrl Pts',(-4.92043708106566,-0.794772684000933,
7.23713382046774));
#38068=CARTESIAN_POINT('Ctrl Pts',(-4.85255964742921,-0.636309800095263,
7.26023174618339));
#38069=CARTESIAN_POINT('Ctrl Pts',(-4.7833269824838,-0.319434907277192,
7.29211112083101));
#38070=CARTESIAN_POINT('Ctrl Pts',(-4.74034072307501,-0.158333333333349,
7.3195841684387));
#38071=CARTESIAN_POINT('Ctrl Pts',(-4.73947577782764,0.158333333333351,
7.35172297496417));
#38072=CARTESIAN_POINT('Ctrl Pts',(-4.78163015967787,0.319434907277199,
7.35766431892539));
#38073=CARTESIAN_POINT('Ctrl Pts',(-4.84903363693141,0.636309800095271,
7.38865110421101));
#38074=CARTESIAN_POINT('Ctrl Pts',(-4.91643593658566,0.794772684000923,
7.39912063634426));
#38075=CARTESIAN_POINT('Ctrl Pts',(-4.96496492619457,1.06847604194589,7.45224044167948));
#38076=CARTESIAN_POINT('Ctrl Pts',(-4.97690899657539,1.18514270861322,7.48183781444401));
#38077=CARTESIAN_POINT('Ctrl Pts',(-4.97979073591155,1.30000000000209,7.51803896452616));
#38078=CARTESIAN_POINT('Ctrl Pts',(-5.0117800089259,-1.30000000000032,7.26370701698165));
#38079=CARTESIAN_POINT('Ctrl Pts',(-5.01130040405251,-1.185142708612,7.2393276982123));
#38080=CARTESIAN_POINT('Ctrl Pts',(-5.0009945786159,-1.06847604194524,7.22516638093642));
#38081=CARTESIAN_POINT('Ctrl Pts',(-4.95448552495434,-0.794772684000867,
7.21605653262139));
#38082=CARTESIAN_POINT('Ctrl Pts',(-4.88617347564889,-0.636309800095205,
7.24152150033735));
#38083=CARTESIAN_POINT('Ctrl Pts',(-4.81733005758418,-0.319434907277162,
7.27456911590342));
#38084=CARTESIAN_POINT('Ctrl Pts',(-4.77299395413638,-0.158333333333335,
7.30310726673854));
#38085=CARTESIAN_POINT('Ctrl Pts',(-4.77222903565246,0.158333333333337,
7.33575692848211));
#38086=CARTESIAN_POINT('Ctrl Pts',(-4.81576663729055,0.319434907277174,
7.3407686493571));
#38087=CARTESIAN_POINT('Ctrl Pts',(-4.88312037829608,0.636309800095217,
7.3723923810245));
#38088=CARTESIAN_POINT('Ctrl Pts',(-4.95152038481361,0.79477268400085,7.38373983305775));
#38089=CARTESIAN_POINT('Ctrl Pts',(-4.99539107681839,1.06847604194579,7.43891897026865));
#38090=CARTESIAN_POINT('Ctrl Pts',(-5.00410392158195,1.18514270861311,7.46962788899476));
#38091=CARTESIAN_POINT('Ctrl Pts',(-5.0025396141095,1.30000000000196,7.50716072253685));
#38092=CARTESIAN_POINT('Ctrl Pts',(-5.03373827646427,-1.3000000000003,7.25059438324909));
#38093=CARTESIAN_POINT('Ctrl Pts',(-5.03743514540706,-1.18514270861198,
7.22337830960446));
#38094=CARTESIAN_POINT('Ctrl Pts',(-5.03020931803739,-1.06847604194522,
7.20725232196869));
#38095=CARTESIAN_POINT('Ctrl Pts',(-4.98828259773198,-0.794772684000851,
7.19561838178191));
#38096=CARTESIAN_POINT('Ctrl Pts',(-4.91934781307156,-0.636309800095197,
7.22227212406156));
#38097=CARTESIAN_POINT('Ctrl Pts',(-4.85084550516312,-0.319434907277159,
7.25618276845748));
#38098=CARTESIAN_POINT('Ctrl Pts',(-4.80525449214961,-0.158333333333332,
7.28622792996134));
#38099=CARTESIAN_POINT('Ctrl Pts',(-4.80463957298795,0.158333333333334,
7.31964424705875));
#38100=CARTESIAN_POINT('Ctrl Pts',(-4.84964913467177,0.319434907277167,
7.32440610753906));
#38101=CARTESIAN_POINT('Ctrl Pts',(-4.9168307249596,0.636309800095206,7.35572932929558));
#38102=CARTESIAN_POINT('Ctrl Pts',(-4.98579503969523,0.79477268400084,7.36476534440009));
#38103=CARTESIAN_POINT('Ctrl Pts',(-5.02510837557522,1.06847604194578,7.42266819008859));
#38104=CARTESIAN_POINT('Ctrl Pts',(-5.03075217902048,1.1851427086131,7.4556345450565));
#38105=CARTESIAN_POINT('Ctrl Pts',(-5.02502249951117,1.30000000000195,7.49650325860557));
#38106=CARTESIAN_POINT('Ctrl Pts',(-5.04463866368648,-1.3000000000003,7.24360077774404));
#38107=CARTESIAN_POINT('Ctrl Pts',(-5.05044042294363,-1.18514270861198,
7.21510877784411));
#38108=CARTESIAN_POINT('Ctrl Pts',(-5.04476129211947,-1.06847604194522,
7.19807307136938));
#38109=CARTESIAN_POINT('Ctrl Pts',(-5.00511821097741,-0.794772684000851,
7.18518351106726));
#38110=CARTESIAN_POINT('Ctrl Pts',(-4.93580560547694,-0.636309800095197,
7.21204894769254));
#38111=CARTESIAN_POINT('Ctrl Pts',(-4.86748690268216,-0.319434907277159,
7.246450708068));
#38112=CARTESIAN_POINT('Ctrl Pts',(-4.82135018302871,-0.158333333333332,
7.2776782820083));
#38113=CARTESIAN_POINT('Ctrl Pts',(-4.82082865786803,0.158333333333334,
7.31155509115153));
#38114=CARTESIAN_POINT('Ctrl Pts',(-4.86650233516519,0.319434907277167,
7.31574227169103));
#38115=CARTESIAN_POINT('Ctrl Pts',(-4.93363960349709,0.636309800095206,
7.34721244841426));
#38116=CARTESIAN_POINT('Ctrl Pts',(-5.00304362126359,0.79477268400084,7.35625511248847));
#38117=CARTESIAN_POINT('Ctrl Pts',(-5.0400719713854,1.06847604194578,7.41533660906748));
#38118=CARTESIAN_POINT('Ctrl Pts',(-5.04414241441304,1.1851427086131,7.44905694196787));
#38119=CARTESIAN_POINT('Ctrl Pts',(-5.03625509973612,1.30000000000195,7.49092341708471));
#38120=CARTESIAN_POINT('',(-4.94063702204203,1.2,7.50431203792771));
#38121=CARTESIAN_POINT('Ctrl Pts',(-4.94063702204203,1.2,7.50431203792771));
#38122=CARTESIAN_POINT('Ctrl Pts',(-4.91512883127448,1.22435101060601,7.52235013201384));
#38123=CARTESIAN_POINT('Ctrl Pts',(-4.89401189434821,1.24430028798091,7.53844339299767));
#38124=CARTESIAN_POINT('Ctrl Pts',(-4.87220163471289,1.26499468132268,7.55373639813777));
#38125=CARTESIAN_POINT('Ctrl Pts',(-4.85380470391158,1.28236518345201,7.56693408695334));
#38126=CARTESIAN_POINT('Ctrl Pts',(-4.83514000569712,1.30000000019026,7.57936937601991));
#38127=CARTESIAN_POINT('',(-4.94779107628249,0.653834841367462,7.34786299432383));
#38128=CARTESIAN_POINT('Ctrl Pts',(-4.94779107631959,0.653834841366186,
7.34786299432997));
#38129=CARTESIAN_POINT('Ctrl Pts',(-4.9473084793979,0.717511353896306,7.36401165108777));
#38130=CARTESIAN_POINT('Ctrl Pts',(-4.94685377491289,0.764335173772842,
7.37724395261881));
#38131=CARTESIAN_POINT('Ctrl Pts',(-4.94482488289273,0.949838615028042,
7.42900031049909));
#38132=CARTESIAN_POINT('Ctrl Pts',(-4.94338416731764,1.05638952303416,7.45971095101033));
#38133=CARTESIAN_POINT('Ctrl Pts',(-4.94063702204202,1.2,7.50431203792771));
#38134=CARTESIAN_POINT('',(-4.94999291725008,-0.653834841531101,7.20837371924779));
#38135=CARTESIAN_POINT('Ctrl Pts',(-4.94999291725008,-0.653834841531101,
7.20837371924779));
#38136=CARTESIAN_POINT('Ctrl Pts',(-4.91226480228564,-0.575997064012115,
7.22581500711208));
#38137=CARTESIAN_POINT('Ctrl Pts',(-4.88066561057669,-0.493634399437435,
7.2412633377142));
#38138=CARTESIAN_POINT('Ctrl Pts',(-4.83631871381536,-0.338121115118327,
7.26566636353398));
#38139=CARTESIAN_POINT('Ctrl Pts',(-4.8212754954691,-0.265647609368857,
7.27534782958795));
#38140=CARTESIAN_POINT('Ctrl Pts',(-4.8034158492223,-0.129707195798598,
7.291927539413));
#38141=CARTESIAN_POINT('Ctrl Pts',(-4.79913204414778,-0.0666204750968713,
7.29900275589153));
#38142=CARTESIAN_POINT('Ctrl Pts',(-4.79855019295222,0.0595404098440564,
7.31231675611242));
#38143=CARTESIAN_POINT('Ctrl Pts',(-4.80223085851993,0.122767112688131,
7.31865112195024));
#38144=CARTESIAN_POINT('Ctrl Pts',(-4.81904696654134,0.260121328322853,
7.33078741696058));
#38145=CARTESIAN_POINT('Ctrl Pts',(-4.83378857283769,0.333940747791096,
7.33628126340755));
#38146=CARTESIAN_POINT('Ctrl Pts',(-4.87782538116292,0.491202933844601,
7.3447735102832));
#38147=CARTESIAN_POINT('Ctrl Pts',(-4.90928838065488,0.57434292395841,7.34738832882229));
#38148=CARTESIAN_POINT('Ctrl Pts',(-4.94779107624722,0.653834841384265,
7.34786299437092));
#38149=CARTESIAN_POINT('',(-4.94934469642006,-1.2,7.28054238647221));
#38150=CARTESIAN_POINT('Ctrl Pts',(-4.94934469642006,-1.2,7.28054238647221));
#38151=CARTESIAN_POINT('Ctrl Pts',(-4.94953491045765,-1.13825277839996,
7.26885369832488));
#38152=CARTESIAN_POINT('Ctrl Pts',(-4.94976307128066,-1.0401741657608,7.25196470745215));
#38153=CARTESIAN_POINT('Ctrl Pts',(-4.94997841213571,-0.793744901850011,
7.21979027555859));
#38154=CARTESIAN_POINT('Ctrl Pts',(-4.9499822550052,-0.738116445717161,
7.21467653823378));
#38155=CARTESIAN_POINT('Ctrl Pts',(-4.94999291725008,-0.653834841531101,
7.20837371924779));
#38156=CARTESIAN_POINT('Ctrl Pts',(-4.84757993445122,-1.30000000000002,
7.35319523199426));
#38157=CARTESIAN_POINT('Ctrl Pts',(-4.86540775027189,-1.28255817374891,
7.34125683870561));
#38158=CARTESIAN_POINT('Ctrl Pts',(-4.88292260055616,-1.26540481326165,
7.32844907968304));
#38159=CARTESIAN_POINT('Ctrl Pts',(-4.90992288706715,-1.2388585038152,7.30960616899799));
#38160=CARTESIAN_POINT('Ctrl Pts',(-4.9301532007377,-1.21894383345738,7.29560714691683));
#38161=CARTESIAN_POINT('Ctrl Pts',(-4.94934469642006,-1.2,7.28054238647221));
#38162=CARTESIAN_POINT('Origin',(0.,1.25,7.2));
#38163=CARTESIAN_POINT('Origin',(0.,1.2,7.2));
#38164=CARTESIAN_POINT('Origin',(0.,0.92691742076555,7.2));
#38165=CARTESIAN_POINT('Origin',(0.,0.653834841531101,7.2));
#38166=CARTESIAN_POINT('Origin',(0.,0.,7.2));
#38167=CARTESIAN_POINT('Origin',(0.,-0.653834841531101,7.2));
#38168=CARTESIAN_POINT('Origin',(0.,-0.926917420765551,7.2));
#38169=CARTESIAN_POINT('Origin',(0.,-1.2,7.2));
#38170=CARTESIAN_POINT('Origin',(0.,-1.25,7.2));
#38171=CARTESIAN_POINT('Ctrl Pts',(-5.03625509974048,-1.30000000000007,
6.90907658291501));
#38172=CARTESIAN_POINT('Ctrl Pts',(-5.04414241441886,-1.18514270861183,
6.9509430580313));
#38173=CARTESIAN_POINT('Ctrl Pts',(-5.04007197139197,-1.06847604194514,
6.98466339093132));
#38174=CARTESIAN_POINT('Ctrl Pts',(-5.00304362127007,-0.794772684000851,
7.04374488751009));
#38175=CARTESIAN_POINT('Ctrl Pts',(-4.93363960349964,-0.636309800095197,
7.05278755158465));
#38176=CARTESIAN_POINT('Ctrl Pts',(-4.86650233516645,-0.319434907277159,
7.08425772830795));
#38177=CARTESIAN_POINT('Ctrl Pts',(-4.82082865787051,-0.158333333333332,
7.08844490884737));
#38178=CARTESIAN_POINT('Ctrl Pts',(-4.82135018303128,0.158333333333334,
7.12232171799055));
#38179=CARTESIAN_POINT('Ctrl Pts',(-4.86748690268523,0.319434907277167,
7.15354929193078));
#38180=CARTESIAN_POINT('Ctrl Pts',(-4.93580560547817,0.636309800095206,
7.18795105230634));
#38181=CARTESIAN_POINT('Ctrl Pts',(-5.00511821097388,0.79477268400084,7.21481648893188));
#38182=CARTESIAN_POINT('Ctrl Pts',(-5.04476129211656,1.06847604194523,7.20192692862984));
#38183=CARTESIAN_POINT('Ctrl Pts',(-5.05044042294223,1.18514270861202,7.18489122215511));
#38184=CARTESIAN_POINT('Ctrl Pts',(-5.04463866368783,1.30000000000036,7.15639922225512));
#38185=CARTESIAN_POINT('Ctrl Pts',(-5.02502249956532,-1.30000000000007,
6.90349674138989));
#38186=CARTESIAN_POINT('Ctrl Pts',(-5.03075217910045,-1.18514270861183,
6.9443654549365));
#38187=CARTESIAN_POINT('Ctrl Pts',(-5.02510837566902,-1.06847604194514,
6.97733180990305));
#38188=CARTESIAN_POINT('Ctrl Pts',(-4.98579503979314,-0.794772684000855,
7.0352346555911));
#38189=CARTESIAN_POINT('Ctrl Pts',(-4.91683072500823,-0.636309800095199,
7.04427067069983));
#38190=CARTESIAN_POINT('Ctrl Pts',(-4.84964913470357,-0.31943490727716,
7.07559389245761));
#38191=CARTESIAN_POINT('Ctrl Pts',(-4.80463957303102,-0.158333333333333,
7.08035575293656));
#38192=CARTESIAN_POINT('Ctrl Pts',(-4.80525449219259,0.158333333333334,
7.11377207003401));
#38193=CARTESIAN_POINT('Ctrl Pts',(-4.85084550521327,0.319434907277166,
7.14381723153794));
#38194=CARTESIAN_POINT('Ctrl Pts',(-4.91934781310062,0.636309800095206,
7.17772787593541));
#38195=CARTESIAN_POINT('Ctrl Pts',(-4.98828259770892,0.794772684000844,
7.20438161821817));
#38196=CARTESIAN_POINT('Ctrl Pts',(-5.0302093180156,1.06847604194524,7.19274767803144));
#38197=CARTESIAN_POINT('Ctrl Pts',(-5.03743514539829,1.18514270861202,7.17662169039496));
#38198=CARTESIAN_POINT('Ctrl Pts',(-5.033738276481,1.30000000000036,7.14940561674885));
#38199=CARTESIAN_POINT('Ctrl Pts',(-5.0025359559224,-1.30000000000008,6.89289909745494));
#38200=CARTESIAN_POINT('Ctrl Pts',(-5.00410024125434,-1.18514270861184,
6.93044802472378));
#38201=CARTESIAN_POINT('Ctrl Pts',(-4.99538814623125,-1.06847604194515,
6.96116325404221));
#38202=CARTESIAN_POINT('Ctrl Pts',(-4.95152096947629,-0.794772684000856,
7.0163343689863));
#38203=CARTESIAN_POINT('Ctrl Pts',(-4.88312761342581,-0.636309800095201,
7.02762863210533));
#38204=CARTESIAN_POINT('Ctrl Pts',(-4.81577644945599,-0.319434907277162,
7.05924000300318));
#38205=CARTESIAN_POINT('Ctrl Pts',(-4.77223713746572,-0.158333333333333,
7.0642756873531));
#38206=CARTESIAN_POINT('Ctrl Pts',(-4.77299933894179,0.158333333333335,
7.09693713865633));
#38207=CARTESIAN_POINT('Ctrl Pts',(-4.81732684919991,0.319434907277168,
7.12550935560819));
#38208=CARTESIAN_POINT('Ctrl Pts',(-4.88617760910314,0.636309800095209,
7.15849915881206));
#38209=CARTESIAN_POINT('Ctrl Pts',(-4.9545167272229,0.794772684000848,7.18380586237005));
#38210=CARTESIAN_POINT('Ctrl Pts',(-5.00102376613031,1.06847604194524,7.17468790825758));
#38211=CARTESIAN_POINT('Ctrl Pts',(-5.01132229374821,1.18514270861203,7.16055774337157));
#38212=CARTESIAN_POINT('Ctrl Pts',(-5.01178817509663,1.30000000000037,7.13624423808135));
#38213=CARTESIAN_POINT('Ctrl Pts',(-4.97960716003471,-1.30000000000009,
6.88198377980277));
#38214=CARTESIAN_POINT('Ctrl Pts',(-4.97669041571901,-1.18514270861184,
6.91815440719478));
#38215=CARTESIAN_POINT('Ctrl Pts',(-4.96472125689941,-1.06847604194515,
6.94772734858306));
#38216=CARTESIAN_POINT('Ctrl Pts',(-4.91615721717078,-0.794772684000857,
7.00080478470547));
#38217=CARTESIAN_POINT('Ctrl Pts',(-4.84876949114567,-0.636309800095199,
7.0112284788478));
#38218=CARTESIAN_POINT('Ctrl Pts',(-4.78135960772631,-0.319434907277159,
7.04227252440624));
#38219=CARTESIAN_POINT('Ctrl Pts',(-4.7391933891993,-0.158333333333333,
7.04842067117444));
#38220=CARTESIAN_POINT('Ctrl Pts',(-4.74006716269824,0.158333333333335,
7.08049671518586));
#38221=CARTESIAN_POINT('Ctrl Pts',(-4.78307750678514,0.319434907277169,
7.10767563488256));
#38222=CARTESIAN_POINT('Ctrl Pts',(-4.85232759462526,0.636309800095209,
7.1394199387625));
#38223=CARTESIAN_POINT('Ctrl Pts',(-4.920192231045,0.794772684000842,7.16256630016529));
#38224=CARTESIAN_POINT('Ctrl Pts',(-4.97138753900633,1.06847604194524,7.1558995652819));
#38225=CARTESIAN_POINT('Ctrl Pts',(-4.98480071031427,1.18514270861203,7.14391294224171));
#38226=CARTESIAN_POINT('Ctrl Pts',(-4.98946650108681,1.30000000000037,7.1228254786655));
#38227=CARTESIAN_POINT('Ctrl Pts',(-4.96762885674604,-1.30000000000009,
6.87633742376048));
#38228=CARTESIAN_POINT('Ctrl Pts',(-4.96246510401137,-1.18514270861184,
6.91091779260864));
#38229=CARTESIAN_POINT('Ctrl Pts',(-4.94884396706527,-1.06847604194515,
6.93940240086729));
#38230=CARTESIAN_POINT('Ctrl Pts',(-4.89783816639833,-0.794772684000859,
6.99112511785659));
#38231=CARTESIAN_POINT('Ctrl Pts',(-4.83080275526198,-0.636309800095201,
7.00243958032192));
#38232=CARTESIAN_POINT('Ctrl Pts',(-4.76327970162913,-0.31943490727716,
7.03379293971568));
#38233=CARTESIAN_POINT('Ctrl Pts',(-4.72182353139671,-0.158333333333333,
7.04059690457321));
#38234=CARTESIAN_POINT('Ctrl Pts',(-4.72276118318227,0.158333333333335,
7.07232672526039));
#38235=CARTESIAN_POINT('Ctrl Pts',(-4.76516503248846,0.319434907277169,
7.09821999675232));
#38236=CARTESIAN_POINT('Ctrl Pts',(-4.83457759043127,0.63630980009521,7.12952744142756));
#38237=CARTESIAN_POINT('Ctrl Pts',(-4.9020024724805,0.794772684000845,7.15261167039543));
#38238=CARTESIAN_POINT('Ctrl Pts',(-4.95565656440269,1.06847604194524,7.14722264546846));
#38239=CARTESIAN_POINT('Ctrl Pts',(-4.97074493751111,1.18514270861203,7.1361257633454));
#38240=CARTESIAN_POINT('Ctrl Pts',(-4.97769681541484,1.30000000000037,7.11626470830709));
#38241=CARTESIAN_POINT('Ctrl Pts',(-4.96621745329077,-1.30000000000009,
6.87569216528662));
#38242=CARTESIAN_POINT('Ctrl Pts',(-4.96078822827751,-1.18514270861184,
6.91009158941893));
#38243=CARTESIAN_POINT('Ctrl Pts',(-4.94697216315507,-1.06847604194515,
6.93845087341062));
#38244=CARTESIAN_POINT('Ctrl Pts',(-4.89567901039405,-0.794772684000858,
6.99001256063605));
#38245=CARTESIAN_POINT('Ctrl Pts',(-4.82868781665214,-0.636309800095201,
7.00141242393467));
#38246=CARTESIAN_POINT('Ctrl Pts',(-4.76115128673114,-0.31943490727716,
7.03280189955936));
#38247=CARTESIAN_POINT('Ctrl Pts',(-4.71977594578805,-0.158333333333333,
7.03970082655641));
#38248=CARTESIAN_POINT('Ctrl Pts',(-4.72072083981947,0.158333333333335,
7.07139106428865));
#38249=CARTESIAN_POINT('Ctrl Pts',(-4.76305477630722,0.319434907277169,
7.09712274218798));
#38250=CARTESIAN_POINT('Ctrl Pts',(-4.83248807833971,0.63630980009521,7.12836853884634));
#38251=CARTESIAN_POINT('Ctrl Pts',(-4.89986290428982,0.794772684000845,
7.15143598900548));
#38252=CARTESIAN_POINT('Ctrl Pts',(-4.95380679298674,1.06847604194524,7.1461950032419));
#38253=CARTESIAN_POINT('Ctrl Pts',(-4.96909210626636,1.18514270861203,7.13520415984025));
#38254=CARTESIAN_POINT('Ctrl Pts',(-4.97631242222678,1.30000000000037,7.11549110157635));
#38255=CARTESIAN_POINT('Ctrl Pts',(-4.96374656696363,-1.30000000000009,
6.87456873959149));
#38256=CARTESIAN_POINT('Ctrl Pts',(-4.95785143305027,-1.18514270861184,
6.90866323031204));
#38257=CARTESIAN_POINT('Ctrl Pts',(-4.94369341141674,-1.06847604194515,
6.93681044950405));
#38258=CARTESIAN_POINT('Ctrl Pts',(-4.89189662552214,-0.794772684000858,
6.98809676969094));
#38259=CARTESIAN_POINT('Ctrl Pts',(-4.82498350845845,-0.636309800095202,
6.99963802448331));
#38260=CARTESIAN_POINT('Ctrl Pts',(-4.7574253787244,-0.31943490727716,7.03107568321695));
#38261=CARTESIAN_POINT('Ctrl Pts',(-4.71619510299612,-0.158333333333333,
7.03811616881096));
#38262=CARTESIAN_POINT('Ctrl Pts',(-4.71715260925729,0.158333333333335,
7.06973664888779));
#38263=CARTESIAN_POINT('Ctrl Pts',(-4.75935940748507,0.319434907277169,
7.09521663791622));
#38264=CARTESIAN_POINT('Ctrl Pts',(-4.82882917382214,0.63630980009521,7.12635439626132));
#38265=CARTESIAN_POINT('Ctrl Pts',(-4.89612151873647,0.794772684000845,
7.14936169526838));
#38266=CARTESIAN_POINT('Ctrl Pts',(-4.95057326325068,1.06847604194524,7.14437500161006));
#38267=CARTESIAN_POINT('Ctrl Pts',(-4.96620267682485,1.18514270861203,7.13357260010592));
#38268=CARTESIAN_POINT('Ctrl Pts',(-4.97389136140897,1.30000000000037,7.11412635200712));
#38269=CARTESIAN_POINT('Ctrl Pts',(-4.95879846811985,-1.30000000000009,
6.87236883666737));
#38270=CARTESIAN_POINT('Ctrl Pts',(-4.95196564729062,-1.18514270861184,
6.90589852110311));
#38271=CARTESIAN_POINT('Ctrl Pts',(-4.93712024036981,-1.06847604194515,
6.93364785801924));
#38272=CARTESIAN_POINT('Ctrl Pts',(-4.88431370378531,-0.794772684000859,
6.98440061840653));
#38273=CARTESIAN_POINT('Ctrl Pts',(-4.81756427071818,-0.636309800095202,
6.99616354044533));
#38274=CARTESIAN_POINT('Ctrl Pts',(-4.74996685995357,-0.31943490727716,
7.02766556635525));
#38275=CARTESIAN_POINT('Ctrl Pts',(-4.70902907192969,-0.158333333333333,
7.03497395089354));
#38276=CARTESIAN_POINT('Ctrl Pts',(-4.71001081751719,0.158333333333335,
7.06645747723653));
#38277=CARTESIAN_POINT('Ctrl Pts',(-4.75195523949809,0.319434907277169,
7.09148194038527));
#38278=CARTESIAN_POINT('Ctrl Pts',(-4.82150169951971,0.636309800095211,
7.12237958432224));
#38279=CARTESIAN_POINT('Ctrl Pts',(-4.88864476872158,0.794772684000845,
7.14517114864296));
#38280=CARTESIAN_POINT('Ctrl Pts',(-4.94411462370513,1.06847604194524,7.14068026114152));
#38281=CARTESIAN_POINT('Ctrl Pts',(-4.96043038643738,1.18514270861203,7.13026730503555));
#38282=CARTESIAN_POINT('Ctrl Pts',(-4.96905106704017,1.30000000000037,7.1113853316192));
#38283=CARTESIAN_POINT('Ctrl Pts',(-4.94886166525784,-1.30000000000009,
6.86822927322511));
#38284=CARTESIAN_POINT('Ctrl Pts',(-4.94009736845648,-1.18514270861184,
6.9010906915426));
#38285=CARTESIAN_POINT('Ctrl Pts',(-4.92384423109776,-1.06847604194515,
6.92831526656563));
#38286=CARTESIAN_POINT('Ctrl Pts',(-4.86899551254524,-0.794772684000858,
6.97818724546956));
#38287=CARTESIAN_POINT('Ctrl Pts',(-4.80263500910927,-0.636309800095202,
6.98986967448523));
#38288=CARTESIAN_POINT('Ctrl Pts',(-4.73502168478157,-0.319434907277161,
7.0210190415513));
#38289=CARTESIAN_POINT('Ctrl Pts',(-4.69474707272955,-0.158333333333333,
7.02832071879295));
#38290=CARTESIAN_POINT('Ctrl Pts',(-4.6957719818575,0.158333333333335,7.05953614177902));
#38291=CARTESIAN_POINT('Ctrl Pts',(-4.737061776107,0.319434907277169,7.08448458166602));
#38292=CARTESIAN_POINT('Ctrl Pts',(-4.80678257958942,0.63630980009521,7.11481118616956));
#38293=CARTESIAN_POINT('Ctrl Pts',(-4.87380031009546,0.794772684000846,
7.13616060747813));
#38294=CARTESIAN_POINT('Ctrl Pts',(-4.93132886568866,1.06847604194524,7.13252271691075));
#38295=CARTESIAN_POINT('Ctrl Pts',(-4.94899630268446,1.18514270861203,7.12300334849857));
#38296=CARTESIAN_POINT('Ctrl Pts',(-4.95942919660282,1.30000000000037,7.10553931970368));
#38297=CARTESIAN_POINT('Ctrl Pts',(-4.93470246489923,-1.30000000000008,
6.86201249896371));
#38298=CARTESIAN_POINT('Ctrl Pts',(-4.92322980335383,-1.18514270861184,
6.89348640190275));
#38299=CARTESIAN_POINT('Ctrl Pts',(-4.9049905596083,-1.06847604194515,6.91974778539996));
#38300=CARTESIAN_POINT('Ctrl Pts',(-4.84722209927548,-0.79477268400086,
6.96837487217873));
#38301=CARTESIAN_POINT('Ctrl Pts',(-4.78132833125217,-0.636309800095202,
6.98071090897872));
#38302=CARTESIAN_POINT('Ctrl Pts',(-4.71359913861764,-0.31943490727716,
7.0120951323827));
#38303=CARTESIAN_POINT('Ctrl Pts',(-4.6741726937007,-0.158333333333333,
7.02012386392998));
#38304=CARTESIAN_POINT('Ctrl Pts',(-4.67526623655484,0.158333333333335,
7.0508886474674));
#38305=CARTESIAN_POINT('Ctrl Pts',(-4.71579254504536,0.319434907277169,
7.07448489895168));
#38306=CARTESIAN_POINT('Ctrl Pts',(-4.78573633088569,0.63630980009521,7.10401416004235));
#38307=CARTESIAN_POINT('Ctrl Pts',(-4.85233696677326,0.794772684000844,
7.12467923821773));
#38308=CARTESIAN_POINT('Ctrl Pts',(-4.9127987545522,1.06847604194524,7.12232311099618));
#38309=CARTESIAN_POINT('Ctrl Pts',(-4.93244088128556,1.18514270861203,7.11385258528136));
#38310=CARTESIAN_POINT('Ctrl Pts',(-4.9455534671528,1.30000000000038,7.0979314140228));
#38311=CARTESIAN_POINT('Ctrl Pts',(-4.91772347406777,-1.30000000000008,
6.85432821639611));
#38312=CARTESIAN_POINT('Ctrl Pts',(-4.90302035506022,-1.18514270861184,
6.88390141473553));
#38313=CARTESIAN_POINT('Ctrl Pts',(-4.88240980055113,-1.06847604194515,
6.9088562755197));
#38314=CARTESIAN_POINT('Ctrl Pts',(-4.82114793872087,-0.794772684000859,
6.95583771248602));
#38315=CARTESIAN_POINT('Ctrl Pts',(-4.75579823557382,-0.6363098000952,6.96911855277399));
#38316=CARTESIAN_POINT('Ctrl Pts',(-4.6879078771988,-0.319434907277159,
7.00099100397379));
#38317=CARTESIAN_POINT('Ctrl Pts',(-4.64947742668345,-0.158333333333333,
7.01012824404134));
#38318=CARTESIAN_POINT('Ctrl Pts',(-4.65063053921603,0.158333333333335,
7.04053799216907));
#38319=CARTESIAN_POINT('Ctrl Pts',(-4.69022144677078,0.319434907277169,
7.06258925454765));
#38320=CARTESIAN_POINT('Ctrl Pts',(-4.76044565211625,0.636309800095209,
7.09107300423509));
#38321=CARTESIAN_POINT('Ctrl Pts',(-4.82658895705298,0.794772684000842,
7.11064697678831));
#38322=CARTESIAN_POINT('Ctrl Pts',(-4.8905994758702,1.06847604194524,7.10965725427226));
#38323=CARTESIAN_POINT('Ctrl Pts',(-4.91262041978007,1.18514270861203,7.10239436821986));
#38324=CARTESIAN_POINT('Ctrl Pts',(-4.92895452582728,1.30000000000037,7.08829701031943));
#38325=CARTESIAN_POINT('Ctrl Pts',(-4.89497550322615,-1.30000000000008,
6.84496254364098));
#38326=CARTESIAN_POINT('Ctrl Pts',(-4.87586793808774,-1.18514270861184,
6.87279864480645));
#38327=CARTESIAN_POINT('Ctrl Pts',(-4.85203155425065,-1.06847604194515,
6.89653623853556));
#38328=CARTESIAN_POINT('Ctrl Pts',(-4.78604022194376,-0.79477268400086,
6.94190645665755));
#38329=CARTESIAN_POINT('Ctrl Pts',(-4.7214628557846,-0.636309800095199,
6.95607542401912));
#38330=CARTESIAN_POINT('Ctrl Pts',(-4.65344063474061,-0.319434907277158,
6.98787198691369));
#38331=CARTESIAN_POINT('Ctrl Pts',(-4.61646069367224,-0.158333333333333,
6.99742355686582));
#38332=CARTESIAN_POINT('Ctrl Pts',(-4.61775673603919,0.158333333333334,
7.02675962258274));
#38333=CARTESIAN_POINT('Ctrl Pts',(-4.65610228950268,0.319434907277168,
7.04675694704748));
#38334=CARTESIAN_POINT('Ctrl Pts',(-4.72662274639178,0.636309800095207,
7.07428232101385));
#38335=CARTESIAN_POINT('Ctrl Pts',(-4.79197838832543,0.794772684000841,
7.0934352899));
#38336=CARTESIAN_POINT('Ctrl Pts',(-4.86068659839513,1.06847604194524,7.09459518377703));
#38337=CARTESIAN_POINT('Ctrl Pts',(-4.88589934228688,1.18514270861202,7.08891273185031));
#38338=CARTESIAN_POINT('Ctrl Pts',(-4.90658359182129,1.30000000000037,7.07704575291581));
#38339=CARTESIAN_POINT('Ctrl Pts',(-4.87221950826238,-1.30000000000007,
6.8354655065749));
#38340=CARTESIAN_POINT('Ctrl Pts',(-4.84871244991834,-1.18514270861184,
6.86149155824746));
#38341=CARTESIAN_POINT('Ctrl Pts',(-4.821658861283,-1.06847604194515,6.88390778160632));
#38342=CARTESIAN_POINT('Ctrl Pts',(-4.75096646502965,-0.794772684000856,
6.9273543163671));
#38343=CARTESIAN_POINT('Ctrl Pts',(-4.68721690445203,-0.636309800095198,
6.94185272432912));
#38344=CARTESIAN_POINT('Ctrl Pts',(-4.61905429626832,-0.319434907277158,
6.9736595223705));
#38345=CARTESIAN_POINT('Ctrl Pts',(-4.58349758943882,-0.158333333333333,
6.98404901772125));
#38346=CARTESIAN_POINT('Ctrl Pts',(-4.58482508549164,0.158333333333334,
7.01316526577346));
#38347=CARTESIAN_POINT('Ctrl Pts',(-4.62173850853168,0.319434907277168,
7.03232083572209));
#38348=CARTESIAN_POINT('Ctrl Pts',(-4.69254561123477,0.636309800095207,
7.05894826866698));
#38349=CARTESIAN_POINT('Ctrl Pts',(-4.75729511476953,0.794772684000841,
7.07645282720016));
#38350=CARTESIAN_POINT('Ctrl Pts',(-4.83080559532184,1.06847604194524,7.07903999007789));
#38351=CARTESIAN_POINT('Ctrl Pts',(-4.85924414270016,1.18514270861202,7.07469855911161));
#38352=CARTESIAN_POINT('Ctrl Pts',(-4.88430127425747,1.30000000000037,7.06489581023311));
#38353=CARTESIAN_POINT('Ctrl Pts',(-4.84942653756722,-1.30000000000008,
6.82625073361417));
#38354=CARTESIAN_POINT('Ctrl Pts',(-4.82151151621238,-1.18514270861184,
6.85040399206725));
#38355=CARTESIAN_POINT('Ctrl Pts',(-4.79121791804108,-1.06847604194515,
6.87162818259571));
#38356=CARTESIAN_POINT('Ctrl Pts',(-4.71573865777315,-0.794772684000856,
6.91389357573726));
#38357=CARTESIAN_POINT('Ctrl Pts',(-4.65266532438613,-0.636309800095195,
6.9303891365972));
#38358=CARTESIAN_POINT('Ctrl Pts',(-4.58432389488618,-0.319434907277155,
6.96252779418703));
#38359=CARTESIAN_POINT('Ctrl Pts',(-4.55026914228413,-0.158333333333332,
6.97279224916784));
#38360=CARTESIAN_POINT('Ctrl Pts',(-4.55169485151761,0.158333333333334,
7.00096988169182));
#38361=CARTESIAN_POINT('Ctrl Pts',(-4.58721478137616,0.319434907277168,
7.01896552662565));
#38362=CARTESIAN_POINT('Ctrl Pts',(-4.65837988440915,0.636309800095205,
7.04405469749339));
#38363=CARTESIAN_POINT('Ctrl Pts',(-4.72260078732687,0.794772684000835,
7.05922726431916));
#38364=CARTESIAN_POINT('Ctrl Pts',(-4.80090120822937,1.06847604194523,7.06339013240831));
#38365=CARTESIAN_POINT('Ctrl Pts',(-4.8325353964471,1.18514270861202,7.06068270166945));
#38366=CARTESIAN_POINT('Ctrl Pts',(-4.8619104219904,1.30000000000036,7.05346588884542));
#38367=CARTESIAN_POINT('Ctrl Pts',(-4.82657019046039,-1.30000000000008,
6.81740338407784));
#38368=CARTESIAN_POINT('Ctrl Pts',(-4.79416905836716,-1.18514270861184,
6.84057624086466));
#38369=CARTESIAN_POINT('Ctrl Pts',(-4.76060377570003,-1.06847604194515,
6.86098284638132));
#38370=CARTESIAN_POINT('Ctrl Pts',(-4.68037183731389,-0.79477268400086,
6.90173559363148));
#38371=CARTESIAN_POINT('Ctrl Pts',(-4.61824100496772,-0.636309800095199,
6.91727506454465));
#38372=CARTESIAN_POINT('Ctrl Pts',(-4.54974399512114,-0.319434907277158,
6.94956855491332));
#38373=CARTESIAN_POINT('Ctrl Pts',(-4.51700107538385,-0.158333333333333,
6.96198316429634));
#38374=CARTESIAN_POINT('Ctrl Pts',(-4.51846353819816,0.158333333333335,
6.98983189669192));
#38375=CARTESIAN_POINT('Ctrl Pts',(-4.55269701870694,0.319434907277169,
7.00542864644343));
#38376=CARTESIAN_POINT('Ctrl Pts',(-4.6241157264898,0.636309800095208,7.02952975983155));
#38377=CARTESIAN_POINT('Ctrl Pts',(-4.68749595868162,0.794772684000841,
7.04459296382786));
#38378=CARTESIAN_POINT('Ctrl Pts',(-4.77061014902644,1.06847604194523,7.05019540129841));
#38379=CARTESIAN_POINT('Ctrl Pts',(-4.80552645837556,1.18514270861202,7.04854708152255));
#38380=CARTESIAN_POINT('Ctrl Pts',(-4.83938202375779,1.30000000000036,7.0428253543806));
#38381=CARTESIAN_POINT('Ctrl Pts',(-4.79795229094086,-1.30000000000008,
6.807426875264));
#38382=CARTESIAN_POINT('Ctrl Pts',(-4.76002338322289,-1.18514270861183,
6.82818459790646));
#38383=CARTESIAN_POINT('Ctrl Pts',(-4.7223931560717,-1.06847604194514,6.8470950796854));
#38384=CARTESIAN_POINT('Ctrl Pts',(-4.63614981531142,-0.79477268400085,
6.88651457968965));
#38385=CARTESIAN_POINT('Ctrl Pts',(-4.57484916985655,-0.636309800095196,
6.90505395334045));
#38386=CARTESIAN_POINT('Ctrl Pts',(-4.50612552655079,-0.319434907277158,
6.93778081866204));
#38387=CARTESIAN_POINT('Ctrl Pts',(-4.47528358705089,-0.158333333333332,
6.94965909012082));
#38388=CARTESIAN_POINT('Ctrl Pts',(-4.47686718908055,0.158333333333334,
6.97607866248283));
#38389=CARTESIAN_POINT('Ctrl Pts',(-4.50933783153711,0.319434907277168,
6.99019693242906));
#38390=CARTESIAN_POINT('Ctrl Pts',(-4.58119529081328,0.636309800095206,
7.01214651733671));
#38391=CARTESIAN_POINT('Ctrl Pts',(-4.64387276186949,0.794772684000838,
7.02437494544686));
#38392=CARTESIAN_POINT('Ctrl Pts',(-4.73305776181358,1.06847604194523,7.03126602506554));
#38393=CARTESIAN_POINT('Ctrl Pts',(-4.77203210410964,1.18514270861202,7.03122247186028));
#38394=CARTESIAN_POINT('Ctrl Pts',(-4.81137590685587,1.30000000000036,7.02815247242249));
#38395=CARTESIAN_POINT('Ctrl Pts',(-4.77218237162956,-1.30000000000007,
6.79773450848216));
#38396=CARTESIAN_POINT('Ctrl Pts',(-4.7292024132972,-1.18514270861183,6.81729430755761));
#38397=CARTESIAN_POINT('Ctrl Pts',(-4.68787751090051,-1.06847604194515,
6.83535570779021));
#38398=CARTESIAN_POINT('Ctrl Pts',(-4.59623222964992,-0.794772684000858,
6.8736195544176));
#38399=CARTESIAN_POINT('Ctrl Pts',(-4.5359023188134,-0.6363098000952,6.8921746025984));
#38400=CARTESIAN_POINT('Ctrl Pts',(-4.46695698337517,-0.31943490727716,
6.92582470962968));
#38401=CARTESIAN_POINT('Ctrl Pts',(-4.43763614628022,-0.158333333333333,
6.94014570092824));
#38402=CARTESIAN_POINT('Ctrl Pts',(-4.43921533843528,0.158333333333335,
6.96643125277066));
#38403=CARTESIAN_POINT('Ctrl Pts',(-4.47011307856436,0.319434907277169,
6.97826785795477));
#38404=CARTESIAN_POINT('Ctrl Pts',(-4.54227977749132,0.636309800095209,
6.99842016325866));
#38405=CARTESIAN_POINT('Ctrl Pts',(-4.60419731222694,0.794772684000845,
7.00872952970313));
#38406=CARTESIAN_POINT('Ctrl Pts',(-4.69883926674906,1.06847604194524,7.01688503767645));
#38407=CARTESIAN_POINT('Ctrl Pts',(-4.74149462807118,1.18514270861202,7.01821760615924));
#38408=CARTESIAN_POINT('Ctrl Pts',(-4.78583835543282,1.30000000000036,7.01735252591453));
#38409=CARTESIAN_POINT('Ctrl Pts',(-4.75492703857426,-1.30000000000007,
6.79270521874686));
#38410=CARTESIAN_POINT('Ctrl Pts',(-4.70857931792514,-1.18514270861183,
6.81137871632538));
#38411=CARTESIAN_POINT('Ctrl Pts',(-4.6647859738728,-1.06847604194514,6.82886797362648));
#38412=CARTESIAN_POINT('Ctrl Pts',(-4.56951570922326,-0.794772684000854,
6.86653582475861));
#38413=CARTESIAN_POINT('Ctrl Pts',(-4.50976391569166,-0.6363098000952,6.88605516832133));
#38414=CARTESIAN_POINT('Ctrl Pts',(-4.44070375128662,-0.319434907277161,
6.91966119238193));
#38415=CARTESIAN_POINT('Ctrl Pts',(-4.41252091761176,-0.158333333333333,
6.93363240105524));
#38416=CARTESIAN_POINT('Ctrl Pts',(-4.41412987613798,0.158333333333335,
6.95928252399892));
#38417=CARTESIAN_POINT('Ctrl Pts',(-4.44391739568318,0.319434907277169,
6.97063151666728));
#38418=CARTESIAN_POINT('Ctrl Pts',(-4.51626359584969,0.636309800095209,
6.98994497272097));
#38419=CARTESIAN_POINT('Ctrl Pts',(-4.57762680043773,0.794772684000846,
6.99927890139707));
#38420=CARTESIAN_POINT('Ctrl Pts',(-4.67597917764199,1.06847604194524,7.00761371103398));
#38421=CARTESIAN_POINT('Ctrl Pts',(-4.72114777053477,1.18514270861202,7.00933571455169));
#38422=CARTESIAN_POINT('Ctrl Pts',(-4.76891185654332,1.30000000000036,7.00917189133044));
#38423=CARTESIAN_POINT('Ctrl Pts',(-4.74343177047671,-1.30000000000007,
6.78894839353199));
#38424=CARTESIAN_POINT('Ctrl Pts',(-4.69481076451741,-1.18514270861183,
6.80749338476164));
#38425=CARTESIAN_POINT('Ctrl Pts',(-4.64935536677492,-1.06847604194514,
6.82487435084292));
#38426=CARTESIAN_POINT('Ctrl Pts',(-4.55165749292722,-0.794772684000855,
6.86233872858587));
#38427=CARTESIAN_POINT('Ctrl Pts',(-4.49233964697176,-0.636309800095201,
6.88170146657958));
#38428=CARTESIAN_POINT('Ctrl Pts',(-4.42320138459244,-0.319434907277162,
6.9153662578531));
#38429=CARTESIAN_POINT('Ctrl Pts',(-4.39574455555068,-0.158333333333333,
6.92977938387961));
#38430=CARTESIAN_POINT('Ctrl Pts',(-4.39735399981225,0.158333333333335,
6.9552783179463));
#38431=CARTESIAN_POINT('Ctrl Pts',(-4.42639564879919,0.319434907277168,
6.96618433558605));
#38432=CARTESIAN_POINT('Ctrl Pts',(-4.49886239121498,0.636309800095209,
6.9848252571226));
#38433=CARTESIAN_POINT('Ctrl Pts',(-4.55987835731215,0.794772684000848,
6.99323036807503));
#38434=CARTESIAN_POINT('Ctrl Pts',(-4.66069740339173,1.06847604194524,7.00172678604837));
#38435=CARTESIAN_POINT('Ctrl Pts',(-4.70753252772009,1.18514270861203,7.00380117594681));
#38436=CARTESIAN_POINT('Ctrl Pts',(-4.75756194704279,1.30000000000037,7.00427217122634));
#38437=CARTESIAN_POINT('Ctrl Pts',(-4.72910106576438,-1.30000000000007,
6.78356480038481));
#38438=CARTESIAN_POINT('Ctrl Pts',(-4.67768109823327,-1.18514270861183,
6.8012358307048));
#38439=CARTESIAN_POINT('Ctrl Pts',(-4.6301699403561,-1.06847604194514,6.81813955457351));
#38440=CARTESIAN_POINT('Ctrl Pts',(-4.52943979334055,-0.794772684000856,
6.85541790688697));
#38441=CARTESIAN_POINT('Ctrl Pts',(-4.47057871361804,-0.6363098000952,6.87621956871056));
#38442=CARTESIAN_POINT('Ctrl Pts',(-4.40130529644547,-0.319434907277161,
6.91065660584509));
#38443=CARTESIAN_POINT('Ctrl Pts',(-4.37475075817477,-0.158333333333333,
6.92560315869304));
#38444=CARTESIAN_POINT('Ctrl Pts',(-4.37638344582047,0.158333333333335,
6.95053393682423));
#38445=CARTESIAN_POINT('Ctrl Pts',(-4.40453061134416,0.319434907277167,
6.96016363706222));
#38446=CARTESIAN_POINT('Ctrl Pts',(-4.47721129582908,0.636309800095208,
6.97723094189587));
#38447=CARTESIAN_POINT('Ctrl Pts',(-4.53789275173436,0.794772684000846,
6.98372009914652));
#38448=CARTESIAN_POINT('Ctrl Pts',(-4.64175773806367,1.06847604194524,6.99279885795604));
#38449=CARTESIAN_POINT('Ctrl Pts',(-4.69062602097088,1.18514270861203,6.99578117483915));
#38450=CARTESIAN_POINT('Ctrl Pts',(-4.74340328278039,1.30000000000037,6.9978159503179));
#38451=CARTESIAN_POINT('Ctrl Pts',(-4.71179979755842,-1.30000000000008,
6.77906526523393));
#38452=CARTESIAN_POINT('Ctrl Pts',(-4.65698137257456,-1.18514270861184,
6.79625865703069));
#38453=CARTESIAN_POINT('Ctrl Pts',(-4.60698344750808,-1.06847604194515,
6.81284466530486));
#38454=CARTESIAN_POINT('Ctrl Pts',(-4.5026145577007,-0.794772684000858,
6.84975848499391));
#38455=CARTESIAN_POINT('Ctrl Pts',(-4.44437945897796,-0.636309800095201,
6.87100152702682));
#38456=CARTESIAN_POINT('Ctrl Pts',(-4.37499166711687,-0.319434907277161,
6.90537712317566));
#38457=CARTESIAN_POINT('Ctrl Pts',(-4.34954854042974,-0.158333333333333,
6.92025735903156));
#38458=CARTESIAN_POINT('Ctrl Pts',(-4.35119141508047,0.158333333333335,
6.9446473087528));
#38459=CARTESIAN_POINT('Ctrl Pts',(-4.37823623949102,0.319434907277168,
6.95359905506214));
#38460=CARTESIAN_POINT('Ctrl Pts',(-4.4510543231609,0.636309800095209,6.97004057009735));
#38461=CARTESIAN_POINT('Ctrl Pts',(-4.51110163934993,0.794772684000847,
6.9761295594491));
#38462=CARTESIAN_POINT('Ctrl Pts',(-4.6186674384589,1.06847604194524,6.98542356437354));
#38463=CARTESIAN_POINT('Ctrl Pts',(-4.67006233573082,1.18514270861203,6.98868602561221));
#38464=CARTESIAN_POINT('Ctrl Pts',(-4.72629088154604,1.30000000000037,6.99118791773457));
#38465=CARTESIAN_POINT('Ctrl Pts',(-4.68591920074664,-1.30000000000007,
6.77087890474239));
#38466=CARTESIAN_POINT('Ctrl Pts',(-4.62604476318184,-1.18514270861183,
6.78691107828377));
#38467=CARTESIAN_POINT('Ctrl Pts',(-4.57233919319432,-1.06847604194514,
6.80288228225904));
#38468=CARTESIAN_POINT('Ctrl Pts',(-4.46251990094192,-0.79477268400085,
6.83963810657568));
#38469=CARTESIAN_POINT('Ctrl Pts',(-4.40516259399858,-0.636309800095198,
6.86266250192134));
#38470=CARTESIAN_POINT('Ctrl Pts',(-4.33554669631685,-0.319434907277161,
6.89871450375448));
#38471=CARTESIAN_POINT('Ctrl Pts',(-4.31171910011351,-0.158333333333333,
6.91563912927993));
#38472=CARTESIAN_POINT('Ctrl Pts',(-4.31336797283825,0.158333333333335,
6.93926032019774));
#38473=CARTESIAN_POINT('Ctrl Pts',(-4.33877696382717,0.319434907277167,
6.94516708872193));
#38474=CARTESIAN_POINT('Ctrl Pts',(-4.41188894422988,0.636309800095207,
6.9588385113594));
#38475=CARTESIAN_POINT('Ctrl Pts',(-4.47115905367224,0.794772684000845,
6.96281269084457));
#38476=CARTESIAN_POINT('Ctrl Pts',(-4.58426559796726,1.06847604194524,6.9722078167419));
#38477=CARTESIAN_POINT('Ctrl Pts',(-4.63940110944556,1.18514270861202,6.97622079803382));
#38478=CARTESIAN_POINT('Ctrl Pts',(-4.70071250038734,1.30000000000036,6.98017995874043));
#38479=CARTESIAN_POINT('Ctrl Pts',(-4.65706796695331,-1.30000000000007,
6.76297007363097));
#38480=CARTESIAN_POINT('Ctrl Pts',(-4.59150651464294,-1.18514270861183,
6.77828368661244));
#38481=CARTESIAN_POINT('Ctrl Pts',(-4.53363602969887,-1.06847604194514,
6.79401380628528));
#38482=CARTESIAN_POINT('Ctrl Pts',(-4.41771130571616,-0.794772684000849,
6.83131574330816));
#38483=CARTESIAN_POINT('Ctrl Pts',(-4.36137897286265,-0.636309800095198,
6.8570983207674));
#38484=CARTESIAN_POINT('Ctrl Pts',(-4.29154387441274,-0.319434907277161,
6.89377932179117));
#38485=CARTESIAN_POINT('Ctrl Pts',(-4.26956906956148,-0.158333333333333,
6.90966130373019));
#38486=CARTESIAN_POINT('Ctrl Pts',(-4.27120100423192,0.158333333333335,
6.93208761653411));
#38487=CARTESIAN_POINT('Ctrl Pts',(-4.29469526007313,0.319434907277168,
6.93739989461276));
#38488=CARTESIAN_POINT('Ctrl Pts',(-4.36808361310165,0.636309800095208,
6.94890928083732));
#38489=CARTESIAN_POINT('Ctrl Pts',(-4.42648405296358,0.794772684000843,
6.9496565215753));
#38490=CARTESIAN_POINT('Ctrl Pts',(-4.54578080039787,1.06847604194524,6.95909532760112));
#38491=CARTESIAN_POINT('Ctrl Pts',(-4.60510078398202,1.18514270861202,6.96397715982235));
#38492=CARTESIAN_POINT('Ctrl Pts',(-4.67210160956614,1.30000000000037,6.96965511487846));
#38493=CARTESIAN_POINT('Ctrl Pts',(-4.62824128498163,-1.30000000000007,
6.75514249224118));
#38494=CARTESIAN_POINT('Ctrl Pts',(-4.55705822919735,-1.18514270861183,
6.76997343913831));
#38495=CARTESIAN_POINT('Ctrl Pts',(-4.4950748534049,-1.06847604194514,6.78568042640955));
#38496=CARTESIAN_POINT('Ctrl Pts',(-4.37313395676334,-0.794772684000853,
6.82399053769364));
#38497=CARTESIAN_POINT('Ctrl Pts',(-4.31785205317386,-0.636309800095198,
6.85232071213997));
#38498=CARTESIAN_POINT('Ctrl Pts',(-4.24781120390648,-0.31943490727716,
6.89089241386308));
#38499=CARTESIAN_POINT('Ctrl Pts',(-4.22765878228674,-0.158333333333333,
6.90794909635979));
#38500=CARTESIAN_POINT('Ctrl Pts',(-4.22924496873314,0.158333333333335,
6.92951718428705));
#38501=CARTESIAN_POINT('Ctrl Pts',(-4.25082855928738,0.319434907277167,
6.93243445575821));
#38502=CARTESIAN_POINT('Ctrl Pts',(-4.32441611564697,0.636309800095207,
6.94104253228292));
#38503=CARTESIAN_POINT('Ctrl Pts',(-4.38182613959396,0.794772684000843,
6.93932195929744));
#38504=CARTESIAN_POINT('Ctrl Pts',(-4.50726340370541,1.06847604194524,6.94785703943639));
#38505=CARTESIAN_POINT('Ctrl Pts',(-4.57076648303345,1.18514270861202,6.95291462731048));
#38506=CARTESIAN_POINT('Ctrl Pts',(-4.64347549796437,1.30000000000036,6.95933528312239));
#38507=CARTESIAN_POINT('Ctrl Pts',(-4.60795779379676,-1.30000000000007,
6.75077046400054));
#38508=CARTESIAN_POINT('Ctrl Pts',(-4.532697496001,-1.18514270861183,6.76528337471195));
#38509=CARTESIAN_POINT('Ctrl Pts',(-4.46773218910147,-1.06847604194514,
6.78106969840869));
#38510=CARTESIAN_POINT('Ctrl Pts',(-4.3414328223746,-0.79477268400085,6.82048110293289));
#38511=CARTESIAN_POINT('Ctrl Pts',(-4.28692863454769,-0.636309800095197,
6.85217463225275));
#38512=CARTESIAN_POINT('Ctrl Pts',(-4.2167292513552,-0.319434907277159,
6.89061321103449));
#38513=CARTESIAN_POINT('Ctrl Pts',(-4.19787125500864,-0.158333333333333,
6.90432318701196));
#38514=CARTESIAN_POINT('Ctrl Pts',(-4.19940827209993,0.158333333333334,
6.924653254063));
#38515=CARTESIAN_POINT('Ctrl Pts',(-4.21959643664148,0.319434907277168,
6.92904737099824));
#38516=CARTESIAN_POINT('Ctrl Pts',(-4.29334794928819,0.636309800095208,
6.93655382403039));
#38517=CARTESIAN_POINT('Ctrl Pts',(-4.35009169193594,0.794772684000841,
6.93208263408248));
#38518=CARTESIAN_POINT('Ctrl Pts',(-4.47999547157628,1.06847604194523,6.93981305401699));
#38519=CARTESIAN_POINT('Ctrl Pts',(-4.5465288739018,1.18514270861202,6.94498811462777));
#38520=CARTESIAN_POINT('Ctrl Pts',(-4.62336514575594,1.30000000000036,6.95199202349996));
#38521=CARTESIAN_POINT('Ctrl Pts',(-4.59357758309325,-1.30000000000007,
6.74732625969349));
#38522=CARTESIAN_POINT('Ctrl Pts',(-4.51560674585504,-1.18514270861183,
6.76249095077157));
#38523=CARTESIAN_POINT('Ctrl Pts',(-4.44866546053796,-1.06847604194514,
6.77856704318338));
#38524=CARTESIAN_POINT('Ctrl Pts',(-4.31949817128937,-0.794772684000852,
6.81781155207203));
#38525=CARTESIAN_POINT('Ctrl Pts',(-4.26554133800437,-0.636309800095197,
6.84789782529569));
#38526=CARTESIAN_POINT('Ctrl Pts',(-4.1953076385941,-0.319434907277159,
6.88545957404936));
#38527=CARTESIAN_POINT('Ctrl Pts',(-4.17739534454885,-0.158333333333333,
6.89877049130274));
#38528=CARTESIAN_POINT('Ctrl Pts',(-4.1789158924004,0.158333333333334,6.91968195652444));
#38529=CARTESIAN_POINT('Ctrl Pts',(-4.19813604853114,0.319434907277168,
6.9259209804531));
#38530=CARTESIAN_POINT('Ctrl Pts',(-4.27190022002353,0.636309800095207,
6.93372770711639));
#38531=CARTESIAN_POINT('Ctrl Pts',(-4.32807553656376,0.794772684000841,
6.92770471093727));
#38532=CARTESIAN_POINT('Ctrl Pts',(-4.46087871138807,1.06847604194523,6.93522051755055));
#38533=CARTESIAN_POINT('Ctrl Pts',(-4.52941487992161,1.18514270861202,6.94052705783577));
#38534=CARTESIAN_POINT('Ctrl Pts',(-4.60900164344984,1.30000000000036,6.94788682421141));
#38535=CARTESIAN_POINT('Ctrl Pts',(-4.57618074025569,-1.30000000000007,
6.74410801342415));
#38536=CARTESIAN_POINT('Ctrl Pts',(-4.4945865145068,-1.18514270861183,6.76006832332152));
#38537=CARTESIAN_POINT('Ctrl Pts',(-4.42497743498526,-1.06847604194514,
6.77630653423347));
#38538=CARTESIAN_POINT('Ctrl Pts',(-4.29185462144734,-0.794772684000851,
6.8144620568206));
#38539=CARTESIAN_POINT('Ctrl Pts',(-4.23842533221008,-0.636309800095197,
6.84114616167115));
#38540=CARTESIAN_POINT('Ctrl Pts',(-4.1680089369724,-0.319434907277159,
6.87655595092038));
#38541=CARTESIAN_POINT('Ctrl Pts',(-4.15135127738475,-0.158333333333332,
6.88950117056474));
#38542=CARTESIAN_POINT('Ctrl Pts',(-4.15284929561901,0.158333333333334,
6.91031986218473));
#38543=CARTESIAN_POINT('Ctrl Pts',(-4.17077447432536,0.319434907277167,
6.91718425800275));
#38544=CARTESIAN_POINT('Ctrl Pts',(-4.24471173494722,0.636309800095206,
6.92623606006507));
#38545=CARTESIAN_POINT('Ctrl Pts',(-4.30037517936425,0.79477268400084,6.92167986871433));
#38546=CARTESIAN_POINT('Ctrl Pts',(-4.43719031458343,1.06847604194523,6.93006454131363));
#38547=CARTESIAN_POINT('Ctrl Pts',(-4.50842904308767,1.18514270861202,6.93553065253984));
#38548=CARTESIAN_POINT('Ctrl Pts',(-4.59168429756014,1.30000000000036,6.94283346090678));
#38549=CARTESIAN_POINT('Ctrl Pts',(-4.5643345584895,-1.30000000000007,6.74178132771715));
#38550=CARTESIAN_POINT('Ctrl Pts',(-4.48025898197815,-1.18514270861183,
6.75965397193162));
#38551=CARTESIAN_POINT('Ctrl Pts',(-4.40891552700136,-1.06847604194514,
6.7765256844786));
#38552=CARTESIAN_POINT('Ctrl Pts',(-4.2735116215927,-0.794772684000851,
6.81319036324906));
#38553=CARTESIAN_POINT('Ctrl Pts',(-4.22112140679107,-0.636309800095197,
6.83335514381641));
#38554=CARTESIAN_POINT('Ctrl Pts',(-4.15113790298685,-0.319434907277159,
6.86531247060112));
#38555=CARTESIAN_POINT('Ctrl Pts',(-4.13553292461561,-0.158333333333332,
6.87852588247456));
#38556=CARTESIAN_POINT('Ctrl Pts',(-4.13706908989958,0.158333333333334,
6.89918937141314));
#38557=CARTESIAN_POINT('Ctrl Pts',(-4.15404363487221,0.319434907277167,
6.90577978297536));
#38558=CARTESIAN_POINT('Ctrl Pts',(-4.22749554627324,0.636309800095206,
6.91766357206941));
#38559=CARTESIAN_POINT('Ctrl Pts',(-4.2818545600116,0.79477268400084,6.91848306636869));
#38560=CARTESIAN_POINT('Ctrl Pts',(-4.42096106050366,1.06847604194523,6.92841142118433));
#38561=CARTESIAN_POINT('Ctrl Pts',(-4.49399758639363,1.18514270861202,6.93356194558498));
#38562=CARTESIAN_POINT('Ctrl Pts',(-4.57985658851437,1.30000000000036,6.9395653774684));
#38563=CARTESIAN_POINT('Ctrl Pts',(-4.5567863920968,-1.30000000000007,6.7376557021251));
#38564=CARTESIAN_POINT('Ctrl Pts',(-4.47294375113312,-1.18514270861183,
6.75562267180235));
#38565=CARTESIAN_POINT('Ctrl Pts',(-4.40183404790299,-1.06847604194514,
6.77224083743495));
#38566=CARTESIAN_POINT('Ctrl Pts',(-4.26697204137396,-0.794772684000851,
6.80751611732843));
#38567=CARTESIAN_POINT('Ctrl Pts',(-4.21502126192295,-0.636309800095197,
6.82515306092102));
#38568=CARTESIAN_POINT('Ctrl Pts',(-4.14539022778077,-0.319434907277159,
6.85546104784237));
#38569=CARTESIAN_POINT('Ctrl Pts',(-4.12973531027791,-0.158333333333332,
6.86869015129617));
#38570=CARTESIAN_POINT('Ctrl Pts',(-4.13134197385142,0.158333333333334,
6.88912754932025));
#38571=CARTESIAN_POINT('Ctrl Pts',(-4.14849242828377,0.319434907277167,
6.89520166263495));
#38572=CARTESIAN_POINT('Ctrl Pts',(-4.22162247741411,0.636309800095206,
6.90883342950105));
#38573=CARTESIAN_POINT('Ctrl Pts',(-4.27538846798974,0.79477268400084,6.91325360263786));
#38574=CARTESIAN_POINT('Ctrl Pts',(-4.41396332499183,1.06847604194523,6.92441809265578));
#38575=CARTESIAN_POINT('Ctrl Pts',(-4.48679959516754,1.18514270861202,6.92950399072587));
#38576=CARTESIAN_POINT('Ctrl Pts',(-4.57248821462725,1.30000000000036,6.93484309282242));
#38577=CARTESIAN_POINT('Ctrl Pts',(-4.55678639209675,-1.3,6.73765570212511));
#38578=CARTESIAN_POINT('Ctrl Pts',(-4.47294375113309,-1.18514270861178,
6.75562267180236));
#38579=CARTESIAN_POINT('Ctrl Pts',(-4.40183404790298,-1.06847604194512,
6.77224083743496));
#38580=CARTESIAN_POINT('Ctrl Pts',(-4.26697204137396,-0.794772684000851,
6.80751611732844));
#38581=CARTESIAN_POINT('Ctrl Pts',(-4.21502126192295,-0.636309800095197,
6.82515306092103));
#38582=CARTESIAN_POINT('Ctrl Pts',(-4.14539022778078,-0.319434907277159,
6.85546104784238));
#38583=CARTESIAN_POINT('Ctrl Pts',(-4.12973531027791,-0.158333333333332,
6.86869015129617));
#38584=CARTESIAN_POINT('Ctrl Pts',(-4.13134197385143,0.158333333333334,
6.88912754932026));
#38585=CARTESIAN_POINT('Ctrl Pts',(-4.14849242828378,0.319434907277167,
6.89520166263495));
#38586=CARTESIAN_POINT('Ctrl Pts',(-4.22162247741411,0.636309800095206,
6.90883342950106));
#38587=CARTESIAN_POINT('Ctrl Pts',(-4.27538846798974,0.79477268400084,6.91325360263787));
#38588=CARTESIAN_POINT('Ctrl Pts',(-4.41396332499177,1.06847604194511,6.92441809265578));
#38589=CARTESIAN_POINT('Ctrl Pts',(-4.48679959516739,1.18514270861178,6.92950399072586));
#38590=CARTESIAN_POINT('Ctrl Pts',(-4.57248821462698,1.3,6.9348430928224));
#38591=CARTESIAN_POINT('',(-4.94063975534853,-1.2,6.89573234172909));
#38592=CARTESIAN_POINT('Ctrl Pts',(-4.94063975534853,-1.2,6.89573234172909));
#38593=CARTESIAN_POINT('Ctrl Pts',(-4.92830831155243,-1.21176551971707,
6.88690492025552));
#38594=CARTESIAN_POINT('Ctrl Pts',(-4.90579448474807,-1.23313228472086,
6.86991968472727));
#38595=CARTESIAN_POINT('Ctrl Pts',(-4.8691048329432,-1.26793264545523,6.84416995488295));
#38596=CARTESIAN_POINT('Ctrl Pts',(-4.852984802018,-1.28315106047734,6.83266786163372));
#38597=CARTESIAN_POINT('Ctrl Pts',(-4.83515073493498,-1.29999999995714,
6.82076739212789));
#38598=CARTESIAN_POINT('',(-4.9477910762941,-0.653834841369964,7.0521370060455));
#38599=CARTESIAN_POINT('Ctrl Pts',(-4.94779107633063,-0.653834841368707,
7.05213700603945));
#38600=CARTESIAN_POINT('Ctrl Pts',(-4.94731006149294,-0.717303034099604,
7.03604128893171));
#38601=CARTESIAN_POINT('Ctrl Pts',(-4.94685048132318,-0.764700269087877,
7.0226840845037));
#38602=CARTESIAN_POINT('Ctrl Pts',(-4.94483149264608,-0.949624416438056,
6.97114271915527));
#38603=CARTESIAN_POINT('Ctrl Pts',(-4.94334706810035,-1.0588111413964,6.93969316585301));
#38604=CARTESIAN_POINT('Ctrl Pts',(-4.94063975534853,-1.2,6.89573234172909));
#38605=CARTESIAN_POINT('',(-4.94999291725008,0.653834841531101,7.19162628075116));
#38606=CARTESIAN_POINT('Ctrl Pts',(-4.94999291725008,0.6538348415311,7.19162628075116));
#38607=CARTESIAN_POINT('Ctrl Pts',(-4.912250011592,0.575966548977897,7.17417815530401));
#38608=CARTESIAN_POINT('Ctrl Pts',(-4.88066509636651,0.493631594836088,
7.15874248042179));
#38609=CARTESIAN_POINT('Ctrl Pts',(-4.83632007966695,0.338125780962295,
7.13435355557771));
#38610=CARTESIAN_POINT('Ctrl Pts',(-4.82127653986155,0.265650240170082,
7.12467671828353));
#38611=CARTESIAN_POINT('Ctrl Pts',(-4.80341641242718,0.129710677149378,
7.10809226524267));
#38612=CARTESIAN_POINT('Ctrl Pts',(-4.79913228443917,0.0666218126861097,
7.10101164196315));
#38613=CARTESIAN_POINT('Ctrl Pts',(-4.79855056169654,-0.0595420532764043,
7.08769654216656));
#38614=CARTESIAN_POINT('Ctrl Pts',(-4.80223161155448,-0.122773043896495,
7.0813645288135));
#38615=CARTESIAN_POINT('Ctrl Pts',(-4.81904790002624,-0.260121668515325,
7.06922912756428));
#38616=CARTESIAN_POINT('Ctrl Pts',(-4.83378878852566,-0.333938915625325,
7.06372946172096));
#38617=CARTESIAN_POINT('Ctrl Pts',(-4.87782632754073,-0.491207904091508,
7.05522789406418));
#38618=CARTESIAN_POINT('Ctrl Pts',(-4.90929274037476,-0.574351920194419,
7.05261169456229));
#38619=CARTESIAN_POINT('Ctrl Pts',(-4.94779107625937,-0.653834841386509,
7.05213700599913));
#38620=CARTESIAN_POINT('',(-4.94934251834154,1.2,7.11932388124965));
#38621=CARTESIAN_POINT('Ctrl Pts',(-4.94934251834154,1.2,7.11932388124965));
#38622=CARTESIAN_POINT('Ctrl Pts',(-4.94955640842995,1.13010588871483,7.13244567398384));
#38623=CARTESIAN_POINT('Ctrl Pts',(-4.94975019917868,1.05323215079269,7.14617609376067));
#38624=CARTESIAN_POINT('Ctrl Pts',(-4.94997545250846,0.796441226852581,
7.17972746337783));
#38625=CARTESIAN_POINT('Ctrl Pts',(-4.94998203701647,0.739839576001175,
7.18519460114659));
#38626=CARTESIAN_POINT('Ctrl Pts',(-4.94999291725008,0.653834841531101,
7.19162628075116));
#38627=CARTESIAN_POINT('Ctrl Pts',(-4.84757460734146,1.3,7.04663629419473));
#38628=CARTESIAN_POINT('Ctrl Pts',(-4.8653921765581,1.28256957351368,7.05859758341152));
#38629=CARTESIAN_POINT('Ctrl Pts',(-4.88292805709936,1.26539376702234,7.07133403262219));
#38630=CARTESIAN_POINT('Ctrl Pts',(-4.91697372090008,1.2319240199412,7.09520398665546));
#38631=CARTESIAN_POINT('Ctrl Pts',(-4.93329979248523,1.21583846690231,7.10692202008179));
#38632=CARTESIAN_POINT('Ctrl Pts',(-4.94934251834154,1.2,7.11932388124965));
#38633=CARTESIAN_POINT('Ctrl Pts',(-4.55678639209675,-1.3,6.73765570212511));
#38634=CARTESIAN_POINT('Ctrl Pts',(-4.47294375113309,-1.18514270861178,
6.75562267180236));
#38635=CARTESIAN_POINT('Ctrl Pts',(-4.40183404790297,-1.06847604194512,
6.77224083743496));
#38636=CARTESIAN_POINT('Ctrl Pts',(-4.26697204137396,-0.794772684000851,
6.80751611732844));
#38637=CARTESIAN_POINT('Ctrl Pts',(-4.21502126192295,-0.636309800095197,
6.82515306092102));
#38638=CARTESIAN_POINT('Ctrl Pts',(-4.14539022778077,-0.319434907277159,
6.85546104784237));
#38639=CARTESIAN_POINT('Ctrl Pts',(-4.12973531027791,-0.158333333333332,
6.86869015129617));
#38640=CARTESIAN_POINT('Ctrl Pts',(-4.13134197385143,0.158333333333334,
6.88912754932025));
#38641=CARTESIAN_POINT('Ctrl Pts',(-4.14849242828378,0.319434907277167,
6.89520166263495));
#38642=CARTESIAN_POINT('Ctrl Pts',(-4.22162247741411,0.636309800095206,
6.90883342950106));
#38643=CARTESIAN_POINT('Ctrl Pts',(-4.27538846798974,0.79477268400084,6.91325360263786));
#38644=CARTESIAN_POINT('Ctrl Pts',(-4.41396332499176,1.06847604194511,6.92441809265578));
#38645=CARTESIAN_POINT('Ctrl Pts',(-4.48679959516739,1.18514270861178,6.92950399072586));
#38646=CARTESIAN_POINT('Ctrl Pts',(-4.57248821462698,1.3,6.9348430928224));
#38647=CARTESIAN_POINT('Ctrl Pts',(-4.54709012720593,-1.3,6.66133341362554));
#38648=CARTESIAN_POINT('Ctrl Pts',(-4.46362634796674,-1.18514270861178,
6.68099075863086));
#38649=CARTESIAN_POINT('Ctrl Pts',(-4.39282414406279,-1.06847604194512,
6.69877562607923));
#38650=CARTESIAN_POINT('Ctrl Pts',(-4.25850766107618,-0.794772684000851,
6.73553642999107));
#38651=CARTESIAN_POINT('Ctrl Pts',(-4.20664978510482,-0.636309800095197,
6.75246177897201));
#38652=CARTESIAN_POINT('Ctrl Pts',(-4.1373298362099,-0.319434907277159,
6.78217992765895));
#38653=CARTESIAN_POINT('Ctrl Pts',(-4.12172229231298,-0.158333333333332,
6.79416838307638));
#38654=CARTESIAN_POINT('Ctrl Pts',(-4.12368594131515,0.158333333333334,
6.81456826041998));
#38655=CARTESIAN_POINT('Ctrl Pts',(-4.14114067935745,0.319434907277167,
6.8218460611083));
#38656=CARTESIAN_POINT('Ctrl Pts',(-4.21469765004064,0.636309800095206,
6.83599009856847));
#38657=CARTESIAN_POINT('Ctrl Pts',(-4.26870246277087,0.79477268400084,6.84108700054781));
#38658=CARTESIAN_POINT('Ctrl Pts',(-4.40750206450663,1.06847604194511,6.85068500808925));
#38659=CARTESIAN_POINT('Ctrl Pts',(-4.48039654346317,1.18514270861178,6.85456576687264));
#38660=CARTESIAN_POINT('Ctrl Pts',(-4.56610429681699,1.3,6.85817266261596));
#38661=CARTESIAN_POINT('Ctrl Pts',(-4.53739386231511,-1.3,6.58501112512596));
#38662=CARTESIAN_POINT('Ctrl Pts',(-4.45430894480039,-1.18514270861178,
6.60635884545937));
#38663=CARTESIAN_POINT('Ctrl Pts',(-4.38381424022261,-1.06847604194512,
6.6253104147235));
#38664=CARTESIAN_POINT('Ctrl Pts',(-4.2500432807784,-0.794772684000851,
6.6635567426537));
#38665=CARTESIAN_POINT('Ctrl Pts',(-4.19827830828669,-0.636309800095197,
6.67977049702301));
#38666=CARTESIAN_POINT('Ctrl Pts',(-4.12926944463902,-0.319434907277159,
6.70889880747553));
#38667=CARTESIAN_POINT('Ctrl Pts',(-4.11370927434805,-0.158333333333332,
6.71964661485658));
#38668=CARTESIAN_POINT('Ctrl Pts',(-4.11602990877888,0.158333333333334,
6.74000897151971));
#38669=CARTESIAN_POINT('Ctrl Pts',(-4.13378893043113,0.319434907277167,
6.74849045958165));
#38670=CARTESIAN_POINT('Ctrl Pts',(-4.20777282266716,0.636309800095206,
6.76314676763588));
#38671=CARTESIAN_POINT('Ctrl Pts',(-4.262016457552,0.79477268400084,6.76892039845776));
#38672=CARTESIAN_POINT('Ctrl Pts',(-4.40104080402149,1.06847604194511,6.77695192352273));
#38673=CARTESIAN_POINT('Ctrl Pts',(-4.47399349175896,1.18514270861178,6.77962754301942));
#38674=CARTESIAN_POINT('Ctrl Pts',(-4.559720379007,1.3,6.78150223240952));
#38675=CARTESIAN_POINT('Ctrl Pts',(-4.52769759742428,-1.3,6.50868883662639));
#38676=CARTESIAN_POINT('Ctrl Pts',(-4.44499154163403,-1.18514270861178,
6.53172693228787));
#38677=CARTESIAN_POINT('Ctrl Pts',(-4.37480433638243,-1.06847604194512,
6.55184520336777));
#38678=CARTESIAN_POINT('Ctrl Pts',(-4.24157890048062,-0.794772684000851,
6.59157705531633));
#38679=CARTESIAN_POINT('Ctrl Pts',(-4.18990683146856,-0.636309800095197,
6.607079215074));
#38680=CARTESIAN_POINT('Ctrl Pts',(-4.12120905306814,-0.319434907277159,
6.63561768729211));
#38681=CARTESIAN_POINT('Ctrl Pts',(-4.10569625638312,-0.158333333333332,
6.64512484663679));
#38682=CARTESIAN_POINT('Ctrl Pts',(-4.1083738762426,0.158333333333334,6.66544968261944));
#38683=CARTESIAN_POINT('Ctrl Pts',(-4.1264371815048,0.319434907277167,6.67513485805499));
#38684=CARTESIAN_POINT('Ctrl Pts',(-4.20084799529369,0.636309800095206,
6.6903034367033));
#38685=CARTESIAN_POINT('Ctrl Pts',(-4.25533045233312,0.79477268400084,6.6967537963677));
#38686=CARTESIAN_POINT('Ctrl Pts',(-4.39457954353636,1.06847604194511,6.70321883895621));
#38687=CARTESIAN_POINT('Ctrl Pts',(-4.46759044005475,1.18514270861178,6.7046893191662));
#38688=CARTESIAN_POINT('Ctrl Pts',(-4.55333646119701,1.3,6.70483180220308));
#38689=CARTESIAN_POINT('Ctrl Pts',(-4.52769759742429,-1.3,6.50868883662639));
#38690=CARTESIAN_POINT('Ctrl Pts',(-4.44499154163404,-1.18514270861178,
6.53172693228787));
#38691=CARTESIAN_POINT('Ctrl Pts',(-4.37480433638243,-1.06847604194512,
6.55184520336777));
#38692=CARTESIAN_POINT('Ctrl Pts',(-4.24157890048062,-0.794772684000851,
6.59157705531633));
#38693=CARTESIAN_POINT('Ctrl Pts',(-4.18990683146856,-0.636309800095197,
6.607079215074));
#38694=CARTESIAN_POINT('Ctrl Pts',(-4.12120905306814,-0.319434907277159,
6.63561768729212));
#38695=CARTESIAN_POINT('Ctrl Pts',(-4.10569625638312,-0.158333333333332,
6.64512484663679));
#38696=CARTESIAN_POINT('Ctrl Pts',(-4.1083738762426,0.158333333333334,6.66544968261944));
#38697=CARTESIAN_POINT('Ctrl Pts',(-4.1264371815048,0.319434907277167,6.675134858055));
#38698=CARTESIAN_POINT('Ctrl Pts',(-4.20084799529369,0.636309800095206,
6.6903034367033));
#38699=CARTESIAN_POINT('Ctrl Pts',(-4.25533045233312,0.79477268400084,6.69675379636771));
#38700=CARTESIAN_POINT('Ctrl Pts',(-4.39457954353635,1.06847604194511,6.70321883895621));
#38701=CARTESIAN_POINT('Ctrl Pts',(-4.46759044005475,1.18514270861178,6.7046893191662));
#38702=CARTESIAN_POINT('Ctrl Pts',(-4.55333646119701,1.3,6.70483180220308));
#38703=CARTESIAN_POINT('Ctrl Pts',(-4.52769759742576,-1.30000000000204,
6.50868883662598));
#38704=CARTESIAN_POINT('Ctrl Pts',(-4.44499154163487,-1.18514270861317,
6.53172693228763));
#38705=CARTESIAN_POINT('Ctrl Pts',(-4.37480433638277,-1.06847604194582,
6.55184520336767));
#38706=CARTESIAN_POINT('Ctrl Pts',(-4.24157890048062,-0.794772684000851,
6.59157705531633));
#38707=CARTESIAN_POINT('Ctrl Pts',(-4.18990683146856,-0.636309800095197,
6.607079215074));
#38708=CARTESIAN_POINT('Ctrl Pts',(-4.12120905306814,-0.319434907277159,
6.63561768729212));
#38709=CARTESIAN_POINT('Ctrl Pts',(-4.10569625638313,-0.158333333333332,
6.64512484663679));
#38710=CARTESIAN_POINT('Ctrl Pts',(-4.10837387624261,0.158333333333334,
6.66544968261944));
#38711=CARTESIAN_POINT('Ctrl Pts',(-4.1264371815048,0.319434907277167,6.675134858055));
#38712=CARTESIAN_POINT('Ctrl Pts',(-4.20084799529369,0.636309800095206,
6.6903034367033));
#38713=CARTESIAN_POINT('Ctrl Pts',(-4.25533045233312,0.79477268400084,6.69675379636771));
#38714=CARTESIAN_POINT('Ctrl Pts',(-4.39457954353638,1.06847604194515,6.70321883895621));
#38715=CARTESIAN_POINT('Ctrl Pts',(-4.4675904400548,1.18514270861186,6.70468931916621));
#38716=CARTESIAN_POINT('Ctrl Pts',(-4.55333646119711,1.30000000000013,6.70483180220308));
#38717=CARTESIAN_POINT('Ctrl Pts',(-4.5339231364204,-1.30000000000204,6.50253777416358));
#38718=CARTESIAN_POINT('Ctrl Pts',(-4.45118854317515,-1.18514270861317,
6.52626110695818));
#38719=CARTESIAN_POINT('Ctrl Pts',(-4.3808188948516,-1.06847604194582,6.54648422763159));
#38720=CARTESIAN_POINT('Ctrl Pts',(-4.24681642619259,-0.794772684000851,
6.58511749179351));
#38721=CARTESIAN_POINT('Ctrl Pts',(-4.19381566978082,-0.636309800095197,
6.59722095263262));
#38722=CARTESIAN_POINT('Ctrl Pts',(-4.12443963753454,-0.319434907277159,
6.62411656351865));
#38723=CARTESIAN_POINT('Ctrl Pts',(-4.10920625064663,-0.158333333333332,
6.63409216512955));
#38724=CARTESIAN_POINT('Ctrl Pts',(-4.11199983518693,0.158333333333334,
6.65462349397901));
#38725=CARTESIAN_POINT('Ctrl Pts',(-4.13001103020958,0.319434907277167,
6.66430370365475));
#38726=CARTESIAN_POINT('Ctrl Pts',(-4.20510952842189,0.636309800095206,
6.68101229756646));
#38727=CARTESIAN_POINT('Ctrl Pts',(-4.26054738494527,0.79477268400084,6.68984389115715));
#38728=CARTESIAN_POINT('Ctrl Pts',(-4.40061540550435,1.06847604194515,6.69755530381139));
#38729=CARTESIAN_POINT('Ctrl Pts',(-4.47390766109767,1.18514270861186,6.69922519060665));
#38730=CARTESIAN_POINT('Ctrl Pts',(-4.55986191621595,1.30000000000013,6.69922697939514));
#38731=CARTESIAN_POINT('Ctrl Pts',(-4.5448135895363,-1.30000000000205,6.49689772508368));
#38732=CARTESIAN_POINT('Ctrl Pts',(-4.46489006285245,-1.18514270861317,
6.52135155288484));
#38733=CARTESIAN_POINT('Ctrl Pts',(-4.39633993528005,-1.06847604194582,
6.54150917877332));
#38734=CARTESIAN_POINT('Ctrl Pts',(-4.2642502543703,-0.794772684000855,
6.57815224122436));
#38735=CARTESIAN_POINT('Ctrl Pts',(-4.20885493857128,-0.636309800095198,
6.5852607203308));
#38736=CARTESIAN_POINT('Ctrl Pts',(-4.13841391482442,-0.319434907277159,
6.60948142826875));
#38737=CARTESIAN_POINT('Ctrl Pts',(-4.12230889881553,-0.158333333333333,
6.61991362476384));
#38738=CARTESIAN_POINT('Ctrl Pts',(-4.12517372525979,0.158333333333335,
6.64060379659608));
#38739=CARTESIAN_POINT('Ctrl Pts',(-4.14416327229731,0.319434907277169,
6.64985058645173));
#38740=CARTESIAN_POINT('Ctrl Pts',(-4.22039960441716,0.636309800095208,
6.66983398081229));
#38741=CARTESIAN_POINT('Ctrl Pts',(-4.27819317135791,0.794772684000841,
6.68474632087806));
#38742=CARTESIAN_POINT('Ctrl Pts',(-4.41634586929662,1.06847604194516,6.69438203741767));
#38743=CARTESIAN_POINT('Ctrl Pts',(-4.48781729178234,1.18514270861187,6.69580424692545));
#38744=CARTESIAN_POINT('Ctrl Pts',(-4.57095895287809,1.30000000000013,6.69447772128951));
#38745=CARTESIAN_POINT('Ctrl Pts',(-4.56073742191317,-1.30000000000205,
6.48845909030144));
#38746=CARTESIAN_POINT('Ctrl Pts',(-4.48442192180763,-1.18514270861317,
6.51220615399741));
#38747=CARTESIAN_POINT('Ctrl Pts',(-4.41848591804469,-1.06847604194582,
6.53163817724403));
#38748=CARTESIAN_POINT('Ctrl Pts',(-4.29013927186283,-0.794772684000854,
6.56656143164765));
#38749=CARTESIAN_POINT('Ctrl Pts',(-4.23392409411188,-0.636309800095199,
6.57229155951987));
#38750=CARTESIAN_POINT('Ctrl Pts',(-4.16337899081417,-0.319434907277161,
6.59519730954064));
#38751=CARTESIAN_POINT('Ctrl Pts',(-4.14586384459553,-0.158333333333333,
6.60524152164129));
#38752=CARTESIAN_POINT('Ctrl Pts',(-4.14872383855016,0.158333333333335,
6.62601326414715));
#38753=CARTESIAN_POINT('Ctrl Pts',(-4.16903064643432,0.319434907277169,
6.63539167526));
#38754=CARTESIAN_POINT('Ctrl Pts',(-4.24554053944403,0.636309800095209,
6.65754452796728));
#38755=CARTESIAN_POINT('Ctrl Pts',(-4.30456094488862,0.794772684000844,
6.67570553640629));
#38756=CARTESIAN_POINT('Ctrl Pts',(-4.43905798432154,1.06847604194516,6.68721928376245));
#38757=CARTESIAN_POINT('Ctrl Pts',(-4.50787657003776,1.18514270861187,6.68902278901192));
#38758=CARTESIAN_POINT('Ctrl Pts',(-4.58729495670616,1.30000000000014,6.68764592490677));
#38759=CARTESIAN_POINT('Ctrl Pts',(-4.57384637688119,-1.30000000000206,
6.48122083117096));
#38760=CARTESIAN_POINT('Ctrl Pts',(-4.5001190698821,-1.18514270861318,6.50404878417318));
#38761=CARTESIAN_POINT('Ctrl Pts',(-4.43609853906568,-1.06847604194583,
6.52295418356865));
#38762=CARTESIAN_POINT('Ctrl Pts',(-4.31062290043274,-0.794772684000857,
6.55756755464857));
#38763=CARTESIAN_POINT('Ctrl Pts',(-4.25420802456576,-0.636309800095198,
6.56504532209082));
#38764=CARTESIAN_POINT('Ctrl Pts',(-4.18364678301027,-0.319434907277158,
6.58779809546497));
#38765=CARTESIAN_POINT('Ctrl Pts',(-4.16483643709211,-0.158333333333333,
6.59633856424103));
#38766=CARTESIAN_POINT('Ctrl Pts',(-4.16756733952373,0.158333333333335,
6.61660382348019));
#38767=CARTESIAN_POINT('Ctrl Pts',(-4.18885460237251,0.319434907277171,
6.6261653388731));
#38768=CARTESIAN_POINT('Ctrl Pts',(-4.26549584572766,0.636309800095211,
6.64909787497906));
#38769=CARTESIAN_POINT('Ctrl Pts',(-4.32535183742634,0.79477268400084,6.66851424753936));
#38770=CARTESIAN_POINT('Ctrl Pts',(-4.45711939879762,1.06847604194516,6.68079853180302));
#38771=CARTESIAN_POINT('Ctrl Pts',(-4.52398008152087,1.18514270861187,6.68278444915833));
#38772=CARTESIAN_POINT('Ctrl Pts',(-4.60066415211911,1.30000000000014,6.68143887238882));
#38773=CARTESIAN_POINT('Ctrl Pts',(-4.58698656110146,-1.30000000000206,
6.47361713730369));
#38774=CARTESIAN_POINT('Ctrl Pts',(-4.51610414428804,-1.18514270861318,
6.49542637411433));
#38775=CARTESIAN_POINT('Ctrl Pts',(-4.4542087767042,-1.06847604194583,6.51376238589569));
#38776=CARTESIAN_POINT('Ctrl Pts',(-4.33197997703341,-0.794772684000859,
6.54809839658323));
#38777=CARTESIAN_POINT('Ctrl Pts',(-4.27543672620479,-0.636309800095201,
6.55735169090154));
#38778=CARTESIAN_POINT('Ctrl Pts',(-4.20508111331027,-0.31943490727716,
6.58054420274352));
#38779=CARTESIAN_POINT('Ctrl Pts',(-4.18500629610171,-0.158333333333334,
6.58803931713282));
#38780=CARTESIAN_POINT('Ctrl Pts',(-4.18787298644458,0.158333333333336,
6.60908156055377));
#38781=CARTESIAN_POINT('Ctrl Pts',(-4.21062555247697,0.319434907277171,
6.62089441202161));
#38782=CARTESIAN_POINT('Ctrl Pts',(-4.2872052674614,0.636309800095212,6.64409603346161));
#38783=CARTESIAN_POINT('Ctrl Pts',(-4.34714661054135,0.794772684000845,
6.66132220693935));
#38784=CARTESIAN_POINT('Ctrl Pts',(-4.4756319386759,1.06847604194516,6.67344753163792));
#38785=CARTESIAN_POINT('Ctrl Pts',(-4.54033845160057,1.18514270861187,6.67572832282236));
#38786=CARTESIAN_POINT('Ctrl Pts',(-4.61413493975109,1.30000000000014,6.6750413014168));
#38787=CARTESIAN_POINT('Ctrl Pts',(-4.59716171915453,-1.30000000000206,
6.46668272213426));
#38788=CARTESIAN_POINT('Ctrl Pts',(-4.52841185704875,-1.18514270861318,
6.48767753331008));
#38789=CARTESIAN_POINT('Ctrl Pts',(-4.46812366280871,-1.06847604194583,
6.50561171696502));
#38790=CARTESIAN_POINT('Ctrl Pts',(-4.34839401902338,-0.79477268400086,
6.5399726070793));
#38791=CARTESIAN_POINT('Ctrl Pts',(-4.29179822741274,-0.636309800095201,
6.55075275265294));
#38792=CARTESIAN_POINT('Ctrl Pts',(-4.22179938955352,-0.31943490727716,
6.57517535074014));
#38793=CARTESIAN_POINT('Ctrl Pts',(-4.20108843781605,-0.158333333333334,
6.58327406446806));
#38794=CARTESIAN_POINT('Ctrl Pts',(-4.20406498716468,0.158333333333336,
6.60498790748946));
#38795=CARTESIAN_POINT('Ctrl Pts',(-4.22760153990135,0.319434907277171,
6.61722407555977));
#38796=CARTESIAN_POINT('Ctrl Pts',(-4.30397086538426,0.636309800095213,
6.63983985698167));
#38797=CARTESIAN_POINT('Ctrl Pts',(-4.36393959524977,0.794772684000845,
6.65501862934024));
#38798=CARTESIAN_POINT('Ctrl Pts',(-4.49001682200018,1.06847604194516,6.66717258273725));
#38799=CARTESIAN_POINT('Ctrl Pts',(-4.55316604490403,1.18514270861187,6.66992754548968));
#38800=CARTESIAN_POINT('Ctrl Pts',(-4.62489033087317,1.30000000000014,6.67017647491734));
#38801=CARTESIAN_POINT('Ctrl Pts',(-4.6074622528922,-1.30000000000206,6.4600435350283));
#38802=CARTESIAN_POINT('Ctrl Pts',(-4.54095552050019,-1.18514270861318,
6.48037531005611));
#38803=CARTESIAN_POINT('Ctrl Pts',(-4.48234277686481,-1.06847604194583,
6.49797291440743));
#38804=CARTESIAN_POINT('Ctrl Pts',(-4.36517230684305,-0.794772684000862,
6.53231041961595));
#38805=CARTESIAN_POINT('Ctrl Pts',(-4.3084061450825,-0.636309800095201,
6.54422769854724));
#38806=CARTESIAN_POINT('Ctrl Pts',(-4.23870137528444,-0.31943490727716,
6.56966697083763));
#38807=CARTESIAN_POINT('Ctrl Pts',(-4.21736580827584,-0.158333333333334,
6.5786460731632));
#38808=CARTESIAN_POINT('Ctrl Pts',(-4.22034314131664,0.158333333333336,
6.60043051355548));
#38809=CARTESIAN_POINT('Ctrl Pts',(-4.24445058191402,0.319434907277172,
6.61166749200678));
#38810=CARTESIAN_POINT('Ctrl Pts',(-4.32063847085125,0.636309800095213,
6.63379619187466));
#38811=CARTESIAN_POINT('Ctrl Pts',(-4.38101305593257,0.794772684000846,
6.64887344683999));
#38812=CARTESIAN_POINT('Ctrl Pts',(-4.50462812710003,1.06847604194516,6.66125269831112));
#38813=CARTESIAN_POINT('Ctrl Pts',(-4.56610840349878,1.18514270861187,6.66422266738462));
#38814=CARTESIAN_POINT('Ctrl Pts',(-4.6355605723777,1.30000000000014,6.66480408626625));
#38815=CARTESIAN_POINT('Ctrl Pts',(-4.62576982567855,-1.30000000000206,
6.44950879919769));
#38816=CARTESIAN_POINT('Ctrl Pts',(-4.56297469544779,-1.18514270861318,
6.46813363441796));
#38817=CARTESIAN_POINT('Ctrl Pts',(-4.50713158452972,-1.06847604194583,
6.48470193121604));
#38818=CARTESIAN_POINT('Ctrl Pts',(-4.39418338229227,-0.794772684000863,
6.51822699613158));
#38819=CARTESIAN_POINT('Ctrl Pts',(-4.33711557690431,-0.636309800095203,
6.53196081109196));
#38820=CARTESIAN_POINT('Ctrl Pts',(-4.26788192627813,-0.319434907277161,
6.55887662222457));
#38821=CARTESIAN_POINT('Ctrl Pts',(-4.24541656673626,-0.158333333333334,
6.56894597707075));
#38822=CARTESIAN_POINT('Ctrl Pts',(-4.24857776470334,0.158333333333336,
6.59172388317241));
#38823=CARTESIAN_POINT('Ctrl Pts',(-4.27412252605687,0.319434907277173,
6.6035729289362));
#38824=CARTESIAN_POINT('Ctrl Pts',(-4.34996192220723,0.636309800095215,
6.62480482326914));
#38825=CARTESIAN_POINT('Ctrl Pts',(-4.41041420828552,0.794772684000848,
6.63676577957294));
#38826=CARTESIAN_POINT('Ctrl Pts',(-4.52971866708554,1.06847604194516,6.64925831825317));
#38827=CARTESIAN_POINT('Ctrl Pts',(-4.58840297499466,1.18514270861187,6.65299604768975));
#38828=CARTESIAN_POINT('Ctrl Pts',(-4.65412911126427,1.30000000000014,6.65506394946243));
#38829=CARTESIAN_POINT('Ctrl Pts',(-4.65102959463181,-1.30000000000207,
6.43149214232983));
#38830=CARTESIAN_POINT('Ctrl Pts',(-4.59342345447021,-1.18514270861319,
6.44725725954069));
#38831=CARTESIAN_POINT('Ctrl Pts',(-4.54151473414863,-1.06847604194584,
6.46223724960806));
#38832=CARTESIAN_POINT('Ctrl Pts',(-4.43475738549757,-0.794772684000863,
6.49503022263472));
#38833=CARTESIAN_POINT('Ctrl Pts',(-4.37775267111089,-0.636309800095206,
6.5129043391861));
#38834=CARTESIAN_POINT('Ctrl Pts',(-4.30949729821618,-0.319434907277163,
6.54291781500037));
#38835=CARTESIAN_POINT('Ctrl Pts',(-4.28555768686207,-0.158333333333335,
6.55527121133622));
#38836=CARTESIAN_POINT('Ctrl Pts',(-4.28879291291088,0.158333333333337,
6.57850141380386));
#38837=CARTESIAN_POINT('Ctrl Pts',(-4.31572986483542,0.319434907277173,
6.58808755367647));
#38838=CARTESIAN_POINT('Ctrl Pts',(-4.39105971583867,0.636309800095217,
6.60802132189756));
#38839=CARTESIAN_POINT('Ctrl Pts',(-4.45231395200949,0.794772684000851,
6.61885578366433));
#38840=CARTESIAN_POINT('Ctrl Pts',(-4.56563152943194,1.06847604194517,6.63244916713826));
#38841=CARTESIAN_POINT('Ctrl Pts',(-4.62030035672222,1.18514270861188,6.63725293761837));
#38842=CARTESIAN_POINT('Ctrl Pts',(-4.68058703086667,1.30000000000015,6.64097640655724));
#38843=CARTESIAN_POINT('Ctrl Pts',(-4.67660141836003,-1.30000000000208,
6.41469238425056));
#38844=CARTESIAN_POINT('Ctrl Pts',(-4.6244180160509,-1.1851427086132,6.42841838267233));
#38845=CARTESIAN_POINT('Ctrl Pts',(-4.57650422860925,-1.06847604194585,
6.44201135867463));
#38846=CARTESIAN_POINT('Ctrl Pts',(-4.47567745897646,-0.794772684000876,
6.47310654410536));
#38847=CARTESIAN_POINT('Ctrl Pts',(-4.41774861709085,-0.636309800095216,
6.49162551861622));
#38848=CARTESIAN_POINT('Ctrl Pts',(-4.35007866327408,-0.319434907277168,
6.52318622767854));
#38849=CARTESIAN_POINT('Ctrl Pts',(-4.32485665302354,-0.158333333333337,
6.53819614711616));
#38850=CARTESIAN_POINT('Ctrl Pts',(-4.32837761003057,0.158333333333339,
6.56267337539902));
#38851=CARTESIAN_POINT('Ctrl Pts',(-4.35705261249353,0.319434907277178,
6.57163732124803));
#38852=CARTESIAN_POINT('Ctrl Pts',(-4.43203294160927,0.636309800095227,
6.59096027795895));
#38853=CARTESIAN_POINT('Ctrl Pts',(-4.49385171345939,0.794772684000865,
6.59960001635686));
#38854=CARTESIAN_POINT('Ctrl Pts',(-4.60132980001507,1.06847604194518,6.61482716747228));
#38855=CARTESIAN_POINT('Ctrl Pts',(-4.65210969249407,1.1851427086119,6.6211845265236));
#38856=CARTESIAN_POINT('Ctrl Pts',(-4.70714619623773,1.30000000000016,6.62730797512994));
#38857=CARTESIAN_POINT('Ctrl Pts',(-4.69671938666277,-1.30000000000209,
6.40019410542714));
#38858=CARTESIAN_POINT('Ctrl Pts',(-4.64842311742148,-1.1851427086132,6.41087046079619));
#38859=CARTESIAN_POINT('Ctrl Pts',(-4.6034504998882,-1.06847604194585,6.42254637528841));
#38860=CARTESIAN_POINT('Ctrl Pts',(-4.5072330569851,-0.794772684000877,
6.45182925505966));
#38861=CARTESIAN_POINT('Ctrl Pts',(-4.44928913645816,-0.636309800095218,
6.47312960657745));
#38862=CARTESIAN_POINT('Ctrl Pts',(-4.38234940217106,-0.31943490727717,
6.50664610297841));
#38863=CARTESIAN_POINT('Ctrl Pts',(-4.35602518955894,-0.158333333333338,
6.52343144267528));
#38864=CARTESIAN_POINT('Ctrl Pts',(-4.35973297066254,0.15833333333334,6.54864062035165));
#38865=CARTESIAN_POINT('Ctrl Pts',(-4.38969701810412,0.319434907277179,
6.55667724125419));
#38866=CARTESIAN_POINT('Ctrl Pts',(-4.46432763719829,0.636309800095229,
6.57529875796418));
#38867=CARTESIAN_POINT('Ctrl Pts',(-4.52658608900722,0.794772684000869,
6.58231619209787));
#38868=CARTESIAN_POINT('Ctrl Pts',(-4.62938916242825,1.06847604194519,6.59890314423408));
#38869=CARTESIAN_POINT('Ctrl Pts',(-4.67706492192611,1.1851427086119,6.60653296645766));
#38870=CARTESIAN_POINT('Ctrl Pts',(-4.72791679966716,1.30000000000016,6.61461273393221));
#38871=CARTESIAN_POINT('Ctrl Pts',(-4.70923780805004,-1.3000000000021,6.39102177259869));
#38872=CARTESIAN_POINT('Ctrl Pts',(-4.6635969880334,-1.18514270861322,6.40051570703614));
#38873=CARTESIAN_POINT('Ctrl Pts',(-4.62060190244937,-1.06847604194587,
6.41144232091127));
#38874=CARTESIAN_POINT('Ctrl Pts',(-4.52738682942984,-0.794772684000888,
6.43999476093189));
#38875=CARTESIAN_POINT('Ctrl Pts',(-4.46920699193414,-0.636309800095222,
6.46234118216104));
#38876=CARTESIAN_POINT('Ctrl Pts',(-4.4025623868709,-0.31943490727717,6.49655685460303));
#38877=CARTESIAN_POINT('Ctrl Pts',(-4.37541513495486,-0.158333333333339,
6.51397711161568));
#38878=CARTESIAN_POINT('Ctrl Pts',(-4.37917902611795,0.158333333333341,
6.53943833931756));
#38879=CARTESIAN_POINT('Ctrl Pts',(-4.40997661151049,0.319434907277181,
6.54698729143357));
#38880=CARTESIAN_POINT('Ctrl Pts',(-4.48451930069498,0.636309800095233,
6.56563651295819));
#38881=CARTESIAN_POINT('Ctrl Pts',(-4.5473088792165,0.794772684000871,6.57257058558995));
#38882=CARTESIAN_POINT('Ctrl Pts',(-4.6472204427376,1.0684760419452,6.59009146329908));
#38883=CARTESIAN_POINT('Ctrl Pts',(-4.69291326935205,1.18514270861191,6.59834469554946));
#38884=CARTESIAN_POINT('Ctrl Pts',(-4.74105090882094,1.30000000000018,6.60726702130246));
#38885=CARTESIAN_POINT('Ctrl Pts',(-4.71915423907025,-1.3000000000021,6.38338868641404));
#38886=CARTESIAN_POINT('Ctrl Pts',(-4.67558438284768,-1.18514270861322,
6.39176024939273));
#38887=CARTESIAN_POINT('Ctrl Pts',(-4.6341320352647,-1.06847604194586,6.4019526285067));
#38888=CARTESIAN_POINT('Ctrl Pts',(-4.54326068839814,-0.794772684000886,
6.4297055127638));
#38889=CARTESIAN_POINT('Ctrl Pts',(-4.48488407740131,-0.636309800095222,
6.45283233370657));
#38890=CARTESIAN_POINT('Ctrl Pts',(-4.4185044797531,-0.319434907277171,
6.48765999012121));
#38891=CARTESIAN_POINT('Ctrl Pts',(-4.39077257383743,-0.158333333333339,
6.50579668879949));
#38892=CARTESIAN_POINT('Ctrl Pts',(-4.39462161644564,0.158333333333341,
6.53157765106085));
#38893=CARTESIAN_POINT('Ctrl Pts',(-4.42611643536731,0.31943490727718,6.5388660264981));
#38894=CARTESIAN_POINT('Ctrl Pts',(-4.50051169546631,0.636309800095232,
6.55727725244718));
#38895=CARTESIAN_POINT('Ctrl Pts',(-4.56348191940118,0.794772684000872,
6.56327773993498));
#38896=CARTESIAN_POINT('Ctrl Pts',(-4.66113327163995,1.0684760419452,6.5817654056829));
#38897=CARTESIAN_POINT('Ctrl Pts',(-4.70532941426806,1.18514270861191,6.59085487148191));
#38898=CARTESIAN_POINT('Ctrl Pts',(-4.75145204747931,1.30000000000018,6.60103117761319));
#38899=CARTESIAN_POINT('Ctrl Pts',(-4.72667488592144,-1.3000000000021,6.37792955793686));
#38900=CARTESIAN_POINT('Ctrl Pts',(-4.68456043694553,-1.18514270861322,
6.38516989090598));
#38901=CARTESIAN_POINT('Ctrl Pts',(-4.64420101572682,-1.06847604194587,
6.39462061151743));
#38902=CARTESIAN_POINT('Ctrl Pts',(-4.55501714404858,-0.79477268400089,
6.42156010438024));
#38903=CARTESIAN_POINT('Ctrl Pts',(-4.49655799527695,-0.636309800095224,
6.44544341871139));
#38904=CARTESIAN_POINT('Ctrl Pts',(-4.43043350640925,-0.319434907277171,
6.48091370749242));
#38905=CARTESIAN_POINT('Ctrl Pts',(-4.40235455693084,-0.158333333333339,
6.4999227553353));
#38906=CARTESIAN_POINT('Ctrl Pts',(-4.40625515181025,0.158333333333341,
6.52588892814653));
#38907=CARTESIAN_POINT('Ctrl Pts',(-4.43815605035426,0.319434907277181,
6.53254907422115));
#38908=CARTESIAN_POINT('Ctrl Pts',(-4.51238596599926,0.636309800095234,
6.55057493445345));
#38909=CARTESIAN_POINT('Ctrl Pts',(-4.57552966840074,0.794772684000873,
6.55601893442645));
#38910=CARTESIAN_POINT('Ctrl Pts',(-4.67145177573476,1.0684760419452,6.57509412671058));
#38911=CARTESIAN_POINT('Ctrl Pts',(-4.71450117951397,1.18514270861191,6.58471346725663));
#38912=CARTESIAN_POINT('Ctrl Pts',(-4.75907886107186,1.30000000000018,6.59569520441448));
#38913=CARTESIAN_POINT('Ctrl Pts',(-4.734255397592,-1.3000000000021,6.37265708709577));
#38914=CARTESIAN_POINT('Ctrl Pts',(-4.69358239480132,-1.18514270861322,
6.37873089092264));
#38915=CARTESIAN_POINT('Ctrl Pts',(-4.65430406422572,-1.06847604194587,
6.38740850709591));
#38916=CARTESIAN_POINT('Ctrl Pts',(-4.56678523481327,-0.79477268400089,
6.41347086381832));
#38917=CARTESIAN_POINT('Ctrl Pts',(-4.50823028163824,-0.636309800095224,
6.43806485257171));
#38918=CARTESIAN_POINT('Ctrl Pts',(-4.44235847902296,-0.319434907277172,
6.47416472709407));
#38919=CARTESIAN_POINT('Ctrl Pts',(-4.41392972446464,-0.158333333333339,
6.49401963091343));
#38920=CARTESIAN_POINT('Ctrl Pts',(-4.41792639169605,0.158333333333341,
6.52032614564209));
#38921=CARTESIAN_POINT('Ctrl Pts',(-4.4502860278473,0.319434907277181,6.52655417793902));
#38922=CARTESIAN_POINT('Ctrl Pts',(-4.52443275445227,0.636309800095234,
6.54449419332223));
#38923=CARTESIAN_POINT('Ctrl Pts',(-4.58781814377579,0.794772684000874,
6.54962033414097));
#38924=CARTESIAN_POINT('Ctrl Pts',(-4.68204912169694,1.0684760419452,6.56943868959626));
#38925=CARTESIAN_POINT('Ctrl Pts',(-4.7239553147106,1.18514270861191,6.57961360926114));
#38926=CARTESIAN_POINT('Ctrl Pts',(-4.7669786019977,1.30000000000018,6.59138481685674));
#38927=CARTESIAN_POINT('Ctrl Pts',(-4.74915526276146,-1.30000000000211,
6.36133152319297));
#38928=CARTESIAN_POINT('Ctrl Pts',(-4.71159373872046,-1.18514270861323,
6.36574451713122));
#38929=CARTESIAN_POINT('Ctrl Pts',(-4.67463144480465,-1.06847604194587,
6.37333227298729));
#38930=CARTESIAN_POINT('Ctrl Pts',(-4.59062549304262,-0.794772684000893,
6.39819584207924));
#38931=CARTESIAN_POINT('Ctrl Pts',(-4.53177671566121,-0.636309800095225,
6.42396941101353));
#38932=CARTESIAN_POINT('Ctrl Pts',(-4.46626236278133,-0.319434907277171,
6.46085697245643));
#38933=CARTESIAN_POINT('Ctrl Pts',(-4.43694193193331,-0.158333333333339,
6.48174434943689));
#38934=CARTESIAN_POINT('Ctrl Pts',(-4.44094155352027,0.158333333333341,
6.50809496769723));
#38935=CARTESIAN_POINT('Ctrl Pts',(-4.47410752652201,0.319434907277183,
6.51308535134564));
#38936=CARTESIAN_POINT('Ctrl Pts',(-4.54808266930368,0.636309800095236,
6.53083527893999));
#38937=CARTESIAN_POINT('Ctrl Pts',(-4.61211578504224,0.794772684000874,
6.53588389196195));
#38938=CARTESIAN_POINT('Ctrl Pts',(-4.70304571945319,1.0684760419452,6.55744846867296));
#38939=CARTESIAN_POINT('Ctrl Pts',(-4.7426871346182,1.18514270861191,6.56879771750923));
#38940=CARTESIAN_POINT('Ctrl Pts',(-4.78260976562786,1.30000000000019,6.58216170896991));
#38941=CARTESIAN_POINT('Ctrl Pts',(-4.76634878519204,-1.30000000000213,
6.3476858866717));
#38942=CARTESIAN_POINT('Ctrl Pts',(-4.73196573478673,-1.18514270861324,
6.34892138513482));
#38943=CARTESIAN_POINT('Ctrl Pts',(-4.69742228238918,-1.06847604194589,
6.35444763451218));
#38944=CARTESIAN_POINT('Ctrl Pts',(-4.61724943626669,-0.794772684000906,
6.37712686906987));
#38945=CARTESIAN_POINT('Ctrl Pts',(-4.5584804369824,-0.636309800095237,
6.4053238999801));
#38946=CARTESIAN_POINT('Ctrl Pts',(-4.49366541735373,-0.319434907277178,
6.44387353912698));
#38947=CARTESIAN_POINT('Ctrl Pts',(-4.46342250085206,-0.158333333333343,
6.46628358235333));
#38948=CARTESIAN_POINT('Ctrl Pts',(-4.46777277979179,0.158333333333345,
6.49379687313776));
#38949=CARTESIAN_POINT('Ctrl Pts',(-4.50235376958148,0.31943490727719,6.49900342147022));
#38950=CARTESIAN_POINT('Ctrl Pts',(-4.57605485621362,0.636309800095249,
6.516285958389));
#38951=CARTESIAN_POINT('Ctrl Pts',(-4.64005443781643,0.79477268400089,6.51856964778118));
#38952=CARTESIAN_POINT('Ctrl Pts',(-4.72702626445182,1.06847604194522,6.54178838191889));
#38953=CARTESIAN_POINT('Ctrl Pts',(-4.76411617897703,1.18514270861194,6.55480108031344));
#38954=CARTESIAN_POINT('Ctrl Pts',(-4.80064912690079,1.30000000000021,6.57077594743321));
#38955=CARTESIAN_POINT('Ctrl Pts',(-4.78351752825162,-1.30000000000214,
6.33396408287167));
#38956=CARTESIAN_POINT('Ctrl Pts',(-4.75275769233394,-1.18514270861325,
6.333286827875));
#38957=CARTESIAN_POINT('Ctrl Pts',(-4.72086801148614,-1.0684760419459,6.33742145422915));
#38958=CARTESIAN_POINT('Ctrl Pts',(-4.64458630140589,-0.794772684000911,
6.35808967677029));
#38959=CARTESIAN_POINT('Ctrl Pts',(-4.58500979039674,-0.636309800095242,
6.38620665294528));
#38960=CARTESIAN_POINT('Ctrl Pts',(-4.52064386708827,-0.31943490727718,
6.42570464158484));
#38961=CARTESIAN_POINT('Ctrl Pts',(-4.48987871233452,-0.158333333333344,
6.45081921693384));
#38962=CARTESIAN_POINT('Ctrl Pts',(-4.49440306962352,0.158333333333346,
6.47885211931188));
#38963=CARTESIAN_POINT('Ctrl Pts',(-4.52972330413681,0.319434907277192,
6.48200646357875));
#38964=CARTESIAN_POINT('Ctrl Pts',(-4.60324243801808,0.636309800095253,
6.49912872852762));
#38965=CARTESIAN_POINT('Ctrl Pts',(-4.66814302376787,0.794772684000896,
6.50182552231488));
#38966=CARTESIAN_POINT('Ctrl Pts',(-4.75129428421296,1.06847604194523,6.52712794414452));
#38967=CARTESIAN_POINT('Ctrl Pts',(-4.78573195602785,1.18514270861195,6.54143715833394));
#38968=CARTESIAN_POINT('Ctrl Pts',(-4.81861420006882,1.30000000000022,6.55910310584988));
#38969=CARTESIAN_POINT('Ctrl Pts',(-4.79351020449058,-1.30000000000214,
6.32669361767881));
#38970=CARTESIAN_POINT('Ctrl Pts',(-4.76463717974963,-1.18514270861326,
6.32440463555332));
#38971=CARTESIAN_POINT('Ctrl Pts',(-4.73416404442742,-1.0684760419459,6.32746190834394));
#38972=CARTESIAN_POINT('Ctrl Pts',(-4.66006843015977,-0.794772684000913,
6.34687573846635));
#38973=CARTESIAN_POINT('Ctrl Pts',(-4.6004453570215,-0.636309800095244,
6.37614473661813));
#38974=CARTESIAN_POINT('Ctrl Pts',(-4.53628448794618,-0.319434907277182,
6.41599063572804));
#38975=CARTESIAN_POINT('Ctrl Pts',(-4.50480502257955,-0.158333333333344,
6.44136201860304));
#38976=CARTESIAN_POINT('Ctrl Pts',(-4.50932945420639,0.158333333333346,
6.46940381619497));
#38977=CARTESIAN_POINT('Ctrl Pts',(-4.54529505697776,0.319434907277193,
6.47212900611573));
#38978=CARTESIAN_POINT('Ctrl Pts',(-4.6187498700802,0.636309800095256,6.48929065647793));
#38979=CARTESIAN_POINT('Ctrl Pts',(-4.68404496334481,0.794772684000899,
6.49180109369998));
#38980=CARTESIAN_POINT('Ctrl Pts',(-4.7650418024707,1.06847604194523,6.51838131827057));
#38981=CARTESIAN_POINT('Ctrl Pts',(-4.798002140494,1.18514270861195,6.53355737900788));
#38982=CARTESIAN_POINT('Ctrl Pts',(-4.82886228611167,1.30000000000022,6.55240390616028));
#38983=CARTESIAN_POINT('Ctrl Pts',(-4.80309023084405,-1.30000000000215,
6.31826901427401));
#38984=CARTESIAN_POINT('Ctrl Pts',(-4.77600203615311,-1.18514270861327,
6.3141225697839));
#38985=CARTESIAN_POINT('Ctrl Pts',(-4.74688787067909,-1.06847604194591,
6.31596191332453));
#38986=CARTESIAN_POINT('Ctrl Pts',(-4.67494792636251,-0.794772684000919,
6.33403953266657));
#38987=CARTESIAN_POINT('Ctrl Pts',(-4.61534329009613,-0.636309800095249,
6.36454325354339));
#38988=CARTESIAN_POINT('Ctrl Pts',(-4.55164121933099,-0.319434907277184,
6.40545613306711));
#38989=CARTESIAN_POINT('Ctrl Pts',(-4.51977914903012,-0.158333333333345,
6.4320952154525));
#38990=CARTESIAN_POINT('Ctrl Pts',(-4.52453026698855,0.158333333333347,
6.46083045310235));
#38991=CARTESIAN_POINT('Ctrl Pts',(-4.56119231513724,0.319434907277194,
6.46330528331013));
#38992=CARTESIAN_POINT('Ctrl Pts',(-4.63447254701522,0.636309800095259,
6.48015268027933));
#38993=CARTESIAN_POINT('Ctrl Pts',(-4.69980372445602,0.794772684000905,
6.48133545414669));
#38994=CARTESIAN_POINT('Ctrl Pts',(-4.77856328943643,1.06847604194524,6.50892485024042));
#38995=CARTESIAN_POINT('Ctrl Pts',(-4.81007267890541,1.18514270861196,6.52504888586614));
#38996=CARTESIAN_POINT('Ctrl Pts',(-4.83899936049287,1.30000000000023,6.5453545298365));
#38997=CARTESIAN_POINT('Ctrl Pts',(-4.8151634792988,-1.30000000000216,6.30798701144558));
#38998=CARTESIAN_POINT('Ctrl Pts',(-4.79067658130991,-1.18514270861328,
6.30253576501484));
#38999=CARTESIAN_POINT('Ctrl Pts',(-4.76347243022552,-1.06847604194592,
6.30343865451421));
#39000=CARTESIAN_POINT('Ctrl Pts',(-4.6943480008138,-0.794772684000923,
6.32020383501925));
#39001=CARTESIAN_POINT('Ctrl Pts',(-4.63428503062086,-0.636309800095255,
6.35100853932324));
#39002=CARTESIAN_POINT('Ctrl Pts',(-4.5707634552206,-0.319434907277188,
6.39213218953601));
#39003=CARTESIAN_POINT('Ctrl Pts',(-4.53812729072339,-0.158333333333347,
6.41940644321399));
#39004=CARTESIAN_POINT('Ctrl Pts',(-4.54300525495016,0.158333333333349,
6.44850906375524));
#39005=CARTESIAN_POINT('Ctrl Pts',(-4.58063982343268,0.319434907277196,
6.45094237657877));
#39006=CARTESIAN_POINT('Ctrl Pts',(-4.65385213362159,0.636309800095264,
6.46786643758685));
#39007=CARTESIAN_POINT('Ctrl Pts',(-4.71946179757621,0.794772684000914,
6.46817393771025));
#39008=CARTESIAN_POINT('Ctrl Pts',(-4.79551793645857,1.06847604194525,6.49731744769436));
#39009=CARTESIAN_POINT('Ctrl Pts',(-4.82521431329873,1.18514270861197,6.51461888169237));
#39010=CARTESIAN_POINT('Ctrl Pts',(-4.85168518261458,1.30000000000024,6.53660660408975));
#39011=CARTESIAN_POINT('Ctrl Pts',(-4.83477143778585,-1.3000000000022,6.29251624496656));
#39012=CARTESIAN_POINT('Ctrl Pts',(-4.81377366445927,-1.18514270861331,
6.28313357612478));
#39013=CARTESIAN_POINT('Ctrl Pts',(-4.78922108492948,-1.06847604194595,
6.28142252691672));
#39014=CARTESIAN_POINT('Ctrl Pts',(-4.72428740102317,-0.794772684000946,
6.295192637008));
#39015=CARTESIAN_POINT('Ctrl Pts',(-4.66435349403994,-0.63630980009527,
6.32877289855501));
#39016=CARTESIAN_POINT('Ctrl Pts',(-4.60144303786872,-0.319434907277194,
6.37109892073663));
#39017=CARTESIAN_POINT('Ctrl Pts',(-4.56763172782983,-0.15833333333335,
6.39963149870782));
#39018=CARTESIAN_POINT('Ctrl Pts',(-4.5725564222523,0.158333333333352,6.42885247543347));
#39019=CARTESIAN_POINT('Ctrl Pts',(-4.61122651902749,0.319434907277203,
6.42965623035112));
#39020=CARTESIAN_POINT('Ctrl Pts',(-4.68430247235875,0.636309800095278,
6.44661626158103));
#39021=CARTESIAN_POINT('Ctrl Pts',(-4.75085363649386,0.794772684000929,
6.44701279901738));
#39022=CARTESIAN_POINT('Ctrl Pts',(-4.82274353785692,1.06847604194528,6.47910808759719));
#39023=CARTESIAN_POINT('Ctrl Pts',(-4.84954953792693,1.185142708612,6.49831652994811));
#39024=CARTESIAN_POINT('Ctrl Pts',(-4.87204306355026,1.30000000000028,6.52284055347141));
#39025=CARTESIAN_POINT('Ctrl Pts',(-4.85153310217081,-1.30000000000223,
6.27786966763461));
#39026=CARTESIAN_POINT('Ctrl Pts',(-4.83402424918511,-1.18514270861334,
6.26630098670574));
#39027=CARTESIAN_POINT('Ctrl Pts',(-4.81201988519055,-1.06847604194598,
6.26297025167625));
#39028=CARTESIAN_POINT('Ctrl Pts',(-4.75079987265101,-0.79477268400097,
6.27430689046979));
#39029=CARTESIAN_POINT('Ctrl Pts',(-4.69003131232683,-0.63630980009529,
6.30770515699895));
#39030=CARTESIAN_POINT('Ctrl Pts',(-4.62751857539782,-0.319434907277205,
6.35069569126754));
#39031=CARTESIAN_POINT('Ctrl Pts',(-4.59310018206488,-0.158333333333355,
6.38142770799137));
#39032=CARTESIAN_POINT('Ctrl Pts',(-4.59840815265766,0.158333333333357,
6.41171884616477));
#39033=CARTESIAN_POINT('Ctrl Pts',(-4.63832885544279,0.319434907277214,
6.41216717778079));
#39034=CARTESIAN_POINT('Ctrl Pts',(-4.711257692019,0.636309800095299,6.42906625385325));
#39035=CARTESIAN_POINT('Ctrl Pts',(-4.77808303811375,0.794772684000955,
6.42788358715442));
#39036=CARTESIAN_POINT('Ctrl Pts',(-4.84621721564676,1.06847604194531,6.46219989217757));
#39037=CARTESIAN_POINT('Ctrl Pts',(-4.87053159509923,1.18514270861204,6.48317159004119));
#39038=CARTESIAN_POINT('Ctrl Pts',(-4.88966759317023,1.30000000000032,6.51026072886833));
#39039=CARTESIAN_POINT('Ctrl Pts',(-4.86590096980636,-1.30000000000225,
6.26540695232221));
#39040=CARTESIAN_POINT('Ctrl Pts',(-4.85112756911822,-1.18514270861336,
6.25127678148908));
#39041=CARTESIAN_POINT('Ctrl Pts',(-4.83116921414428,-1.06847604194599,
6.24618503207826));
#39042=CARTESIAN_POINT('Ctrl Pts',(-4.77308313985265,-0.794772684000978,
6.2553026339538));
#39043=CARTESIAN_POINT('Ctrl Pts',(-4.7120659869826,-0.636309800095298,
6.28980887743881));
#39044=CARTESIAN_POINT('Ctrl Pts',(-4.65004983253428,-0.31943490727721,
6.33377644641802));
#39045=CARTESIAN_POINT('Ctrl Pts',(-4.61510964605151,-0.158333333333357,
6.36639155506332));
#39046=CARTESIAN_POINT('Ctrl Pts',(-4.62053313323579,0.158333333333359,
6.39696545018637));
#39047=CARTESIAN_POINT('Ctrl Pts',(-4.66110704130425,0.319434907277217,
6.39587846474762));
#39048=CARTESIAN_POINT('Ctrl Pts',(-4.7337422163046,0.636309800095307,6.41224402484117));
#39049=CARTESIAN_POINT('Ctrl Pts',(-4.80092708373685,0.794772684000967,
6.41010148174191));
#39050=CARTESIAN_POINT('Ctrl Pts',(-4.86600560625236,1.06847604194532,6.44680209804103));
#39051=CARTESIAN_POINT('Ctrl Pts',(-4.88828350587341,1.18514270861205,6.46957015367528));
#39052=CARTESIAN_POINT('Ctrl Pts',(-4.90466922411546,1.30000000000034,6.49921992803975));
#39053=CARTESIAN_POINT('Ctrl Pts',(-4.87299453743658,-1.30000000000226,
6.25895256639751));
#39054=CARTESIAN_POINT('Ctrl Pts',(-4.85955957430163,-1.18514270861336,
6.24348838571595));
#39055=CARTESIAN_POINT('Ctrl Pts',(-4.84061301095117,-1.06847604194599,
6.23749936438882));
#39056=CARTESIAN_POINT('Ctrl Pts',(-4.78410976027508,-0.794772684000981,
6.24555304063138));
#39057=CARTESIAN_POINT('Ctrl Pts',(-4.72308912485098,-0.636309800095299,
6.28089123849204));
#39058=CARTESIAN_POINT('Ctrl Pts',(-4.66130212304377,-0.31943490727721,
6.32527212826392));
#39059=CARTESIAN_POINT('Ctrl Pts',(-4.62591888048782,-0.158333333333358,
6.35832773529538));
#39060=CARTESIAN_POINT('Ctrl Pts',(-4.63144916783238,0.15833333333336,6.38918989253));
#39061=CARTESIAN_POINT('Ctrl Pts',(-4.67256321428421,0.319434907277219,
6.38794731218294));
#39062=CARTESIAN_POINT('Ctrl Pts',(-4.74520657544105,0.636309800095309,
6.40449356194456));
#39063=CARTESIAN_POINT('Ctrl Pts',(-4.81266614593729,0.794772684000968,
6.40215115436439));
#39064=CARTESIAN_POINT('Ctrl Pts',(-4.87616496143012,1.06847604194533,6.43988664395963));
#39065=CARTESIAN_POINT('Ctrl Pts',(-4.89735697851544,1.18514270861205,6.4633515401264));
#39066=CARTESIAN_POINT('Ctrl Pts',(-4.91225472832225,1.30000000000034,6.49394703725185));
#39067=CARTESIAN_POINT('Ctrl Pts',(-4.87887450905704,-1.30000000000227,
6.25350829485688));
#39068=CARTESIAN_POINT('Ctrl Pts',(-4.86649867966928,-1.18514270861337,
6.23678922594398));
#39069=CARTESIAN_POINT('Ctrl Pts',(-4.84836392564263,-1.068476041946,6.22997309568147));
#39070=CARTESIAN_POINT('Ctrl Pts',(-4.7931647480114,-0.794772684000989,
6.23710424057133));
#39071=CARTESIAN_POINT('Ctrl Pts',(-4.73224393961161,-0.636309800095306,
6.2734062904428));
#39072=CARTESIAN_POINT('Ctrl Pts',(-4.67066449497868,-0.319434907277213,
6.31816582250651));
#39073=CARTESIAN_POINT('Ctrl Pts',(-4.63487003306998,-0.158333333333359,
6.35146409740365));
#39074=CARTESIAN_POINT('Ctrl Pts',(-4.64046203740145,0.158333333333361,
6.38248190288132));
#39075=CARTESIAN_POINT('Ctrl Pts',(-4.6820015236105,0.319434907277222,6.38103682856874));
#39076=CARTESIAN_POINT('Ctrl Pts',(-4.75465978777017,0.636309800095315,
6.39775669322459));
#39077=CARTESIAN_POINT('Ctrl Pts',(-4.82238897181522,0.794772684000976,
6.39537091488647));
#39078=CARTESIAN_POINT('Ctrl Pts',(-4.88460180587223,1.06847604194534,6.43405409518991));
#39079=CARTESIAN_POINT('Ctrl Pts',(-4.90490010156291,1.18514270861207,6.45812920302176));
#39080=CARTESIAN_POINT('Ctrl Pts',(-4.91856706229369,1.30000000000035,6.4895349032852));
#39081=CARTESIAN_POINT('Ctrl Pts',(-4.88303349416408,-1.30000000000227,
6.24980581282697));
#39082=CARTESIAN_POINT('Ctrl Pts',(-4.87145190564438,-1.18514270861337,
6.23234183502179));
#39083=CARTESIAN_POINT('Ctrl Pts',(-4.8539079585843,-1.06847604194601,6.22500365239295));
#39084=CARTESIAN_POINT('Ctrl Pts',(-4.79960369022706,-0.794772684000991,
6.23144359503765));
#39085=CARTESIAN_POINT('Ctrl Pts',(-4.73858754855097,-0.636309800095307,
6.26800085290985));
#39086=CARTESIAN_POINT('Ctrl Pts',(-4.67713136339042,-0.319434907277214,
6.31297344610454));
#39087=CARTESIAN_POINT('Ctrl Pts',(-4.64116430483494,-0.15833333333336,
6.34674272239031));
#39088=CARTESIAN_POINT('Ctrl Pts',(-4.64681024934969,0.158333333333362,
6.3778948753898));
#39089=CARTESIAN_POINT('Ctrl Pts',(-4.68859166985004,0.319434907277222,
6.37615982618997));
#39090=CARTESIAN_POINT('Ctrl Pts',(-4.76120518328696,0.636309800095316,
6.3928452042231));
#39091=CARTESIAN_POINT('Ctrl Pts',(-4.82905128233515,0.794772684000978,
6.39021706347285));
#39092=CARTESIAN_POINT('Ctrl Pts',(-4.89038451800035,1.06847604194534,6.42962388239991));
#39093=CARTESIAN_POINT('Ctrl Pts',(-4.91009005518737,1.18514270861207,6.45422208087761));
#39094=CARTESIAN_POINT('Ctrl Pts',(-4.92295224446233,1.30000000000035,6.48636072608605));
#39095=CARTESIAN_POINT('Ctrl Pts',(-4.88511906029955,-1.30000000000227,
6.24797069807145));
#39096=CARTESIAN_POINT('Ctrl Pts',(-4.87394015206932,-1.18514270861337,
6.23014816124439));
#39097=CARTESIAN_POINT('Ctrl Pts',(-4.85669357019099,-1.06847604194601,
6.22255385660423));
#39098=CARTESIAN_POINT('Ctrl Pts',(-4.8028329759242,-0.794772684000991,
6.22863875615257));
#39099=CARTESIAN_POINT('Ctrl Pts',(-4.74174774993459,-0.636309800095307,
6.26526985332957));
#39100=CARTESIAN_POINT('Ctrl Pts',(-4.68035044328705,-0.319434907277214,
6.31034259500331));
#39101=CARTESIAN_POINT('Ctrl Pts',(-4.64431401494797,-0.15833333333336,
6.34439156977969));
#39102=CARTESIAN_POINT('Ctrl Pts',(-4.64998628638108,0.158333333333362,
6.37560784920097));
#39103=CARTESIAN_POINT('Ctrl Pts',(-4.69187679406689,0.319434907277223,
6.37369499021199));
#39104=CARTESIAN_POINT('Ctrl Pts',(-4.76445777957717,0.636309800095317,
6.39033392162532));
#39105=CARTESIAN_POINT('Ctrl Pts',(-4.83235154908065,0.794772684000978,
6.38755292826981));
#39106=CARTESIAN_POINT('Ctrl Pts',(-4.89325001331377,1.06847604194534,6.42733573848687));
#39107=CARTESIAN_POINT('Ctrl Pts',(-4.91266555316545,1.18514270861207,6.45221377491437));
#39108=CARTESIAN_POINT('Ctrl Pts',(-4.92513594421278,1.30000000000035,6.48474934332482));
#39109=CARTESIAN_POINT('Ctrl Pts',(-4.88616316227367,-1.30000000000227,
6.24705661024912));
#39110=CARTESIAN_POINT('Ctrl Pts',(-4.87518733634367,-1.18514270861337,
6.2290593099747));
#39111=CARTESIAN_POINT('Ctrl Pts',(-4.858090127115,-1.06847604194601,6.22133875711569));
#39112=CARTESIAN_POINT('Ctrl Pts',(-4.80445053351347,-0.794772684000991,
6.22724407790598));
#39113=CARTESIAN_POINT('Ctrl Pts',(-4.74332517984475,-0.636309800095307,
6.26389783228499));
#39114=CARTESIAN_POINT('Ctrl Pts',(-4.68195577762773,-0.319434907277214,
6.30901673411741));
#39115=CARTESIAN_POINT('Ctrl Pts',(-4.64588712997815,-0.15833333333336,
6.34321187867584));
#39116=CARTESIAN_POINT('Ctrl Pts',(-4.65157298490524,0.158333333333362,
6.37446118104646));
#39117=CARTESIAN_POINT('Ctrl Pts',(-4.69351785246644,0.319434907277223,
6.37245896529304));
#39118=CARTESIAN_POINT('Ctrl Pts',(-4.76608117200806,0.636309800095317,
6.38907054326162));
#39119=CARTESIAN_POINT('Ctrl Pts',(-4.83399558226774,0.794772684000978,
6.38620392993072));
#39120=CARTESIAN_POINT('Ctrl Pts',(-4.89467711682258,1.06847604194534,6.42617579067426));
#39121=CARTESIAN_POINT('Ctrl Pts',(-4.91394871474128,1.18514270861207,6.45119662852342));
#39122=CARTESIAN_POINT('Ctrl Pts',(-4.92622512274235,1.30000000000035,6.48393596680926));
#39123=CARTESIAN_POINT('Ctrl Pts',(-4.88675992689258,-1.30000000000227,
6.2465346801272));
#39124=CARTESIAN_POINT('Ctrl Pts',(-4.87590019523263,-1.18514270861337,
6.22843761554879));
#39125=CARTESIAN_POINT('Ctrl Pts',(-4.85888833846411,-1.06847604194601,
6.22064489604193));
#39126=CARTESIAN_POINT('Ctrl Pts',(-4.80537490638943,-0.794772684000991,
6.22644725354528));
#39127=CARTESIAN_POINT('Ctrl Pts',(-4.74422603700827,-0.636309800095308,
6.26311241974435));
#39128=CARTESIAN_POINT('Ctrl Pts',(-4.68287294129434,-0.319434907277214,
6.30825867370313));
#39129=CARTESIAN_POINT('Ctrl Pts',(-4.64678722961753,-0.15833333333336,
6.34254095850511));
#39130=CARTESIAN_POINT('Ctrl Pts',(-4.6524807662358,0.158333333333362,6.37380888393949));
#39131=CARTESIAN_POINT('Ctrl Pts',(-4.69445524493705,0.319434907277223,
6.37175166515498));
#39132=CARTESIAN_POINT('Ctrl Pts',(-4.76700799451387,0.636309800095317,
6.38834629748932));
#39133=CARTESIAN_POINT('Ctrl Pts',(-4.8349346515849,0.794772684000978,6.3854318888518));
#39134=CARTESIAN_POINT('Ctrl Pts',(-4.89549252003682,1.06847604194534,6.42551268428735));
#39135=CARTESIAN_POINT('Ctrl Pts',(-4.91468201642996,1.18514270861207,6.45061562505171));
#39136=CARTESIAN_POINT('Ctrl Pts',(-4.92684775185358,1.30000000000035,6.48347201537625));
#39137=CARTESIAN_POINT('Ctrl Pts',(-4.89661012634148,-1.30000000000225,
6.23793284476157));
#39138=CARTESIAN_POINT('Ctrl Pts',(-4.88767323528789,-1.18514270861336,
6.21821005201528));
#39139=CARTESIAN_POINT('Ctrl Pts',(-4.87207220842793,-1.06847604194599,
6.20923437608288));
#39140=CARTESIAN_POINT('Ctrl Pts',(-4.82063522853835,-0.794772684000981,
6.21332675889466));
#39141=CARTESIAN_POINT('Ctrl Pts',(-4.75908214733113,-0.636309800095299,
6.25014073779938));
#39142=CARTESIAN_POINT('Ctrl Pts',(-4.69797005826219,-0.31943490727721,
6.29566381090703));
#39143=CARTESIAN_POINT('Ctrl Pts',(-4.66156496293845,-0.158333333333358,
6.33127953794985));
#39144=CARTESIAN_POINT('Ctrl Pts',(-4.66738833257477,0.15833333333336,6.36286126460822));
#39145=CARTESIAN_POINT('Ctrl Pts',(-4.70990593945366,0.319434907277218,
6.36004321413319));
#39146=CARTESIAN_POINT('Ctrl Pts',(-4.7822908519055,0.636309800095308,6.37637304185465));
#39147=CARTESIAN_POINT('Ctrl Pts',(-4.85037588380938,0.794772684000967,
6.37255171433152));
#39148=CARTESIAN_POINT('Ctrl Pts',(-4.90888799196061,1.06847604194532,6.41440829010348));
#39149=CARTESIAN_POINT('Ctrl Pts',(-4.92672720751677,1.18514270861205,6.44087330209631));
#39150=CARTESIAN_POINT('Ctrl Pts',(-4.9370779150977,1.30000000000034,6.47568516536931));
#39151=CARTESIAN_POINT('Ctrl Pts',(-4.91551434023808,-1.30000000000215,
6.22032402652648));
#39152=CARTESIAN_POINT('Ctrl Pts',(-4.90999433762571,-1.18514270861327,
6.19661715740314));
#39153=CARTESIAN_POINT('Ctrl Pts',(-4.89697781727854,-1.06847604194591,
6.18492582636369));
#39154=CARTESIAN_POINT('Ctrl Pts',(-4.84958859569011,-0.79477268400092,
6.18567480949371));
#39155=CARTESIAN_POINT('Ctrl Pts',(-4.78801610962174,-0.636309800095251,
6.22466937483527));
#39156=CARTESIAN_POINT('Ctrl Pts',(-4.72754050454037,-0.319434907277186,
6.2712911094235));
#39157=CARTESIAN_POINT('Ctrl Pts',(-4.69013335396713,-0.158333333333346,
6.30849393952512));
#39158=CARTESIAN_POINT('Ctrl Pts',(-4.69618212274349,0.158333333333348,
6.34061055348662));
#39159=CARTESIAN_POINT('Ctrl Pts',(-4.73980871380282,0.319434907277193,
6.33645276090364));
#39160=CARTESIAN_POINT('Ctrl Pts',(-4.81225757937188,0.63630980009526,6.35335912454488));
#39161=CARTESIAN_POINT('Ctrl Pts',(-4.88150378801858,0.794772684000909,
6.35018783882674));
#39162=CARTESIAN_POINT('Ctrl Pts',(-4.9358861614365,1.06847604194524,6.39503939976606));
#39163=CARTESIAN_POINT('Ctrl Pts',(-4.95079638343893,1.18514270861196,6.42327726850731));
#39164=CARTESIAN_POINT('Ctrl Pts',(-4.9570767130567,1.30000000000024,6.4603384271733));
#39165=CARTESIAN_POINT('Ctrl Pts',(-4.93425818161267,-1.30000000000204,
6.20291573839235));
#39166=CARTESIAN_POINT('Ctrl Pts',(-4.93221572521049,-1.18514270861317,
6.17552577898254));
#39167=CARTESIAN_POINT('Ctrl Pts',(-4.92179501815007,-1.06847604194582,
6.161254516853));
#39168=CARTESIAN_POINT('Ctrl Pts',(-4.87836566510148,-0.794772684000851,
6.15859186148136));
#39169=CARTESIAN_POINT('Ctrl Pts',(-4.81647889550275,-0.636309800095197,
6.19899550317773));
#39170=CARTESIAN_POINT('Ctrl Pts',(-4.75652394679047,-0.319434907277159,
6.2464075492951));
#39171=CARTESIAN_POINT('Ctrl Pts',(-4.71817594712549,-0.158333333333332,
6.28527505653548));
#39172=CARTESIAN_POINT('Ctrl Pts',(-4.72452210841149,0.158333333333334,
6.31808899581228));
#39173=CARTESIAN_POINT('Ctrl Pts',(-4.76953814964646,0.319434907277167,
6.31338878414349));
#39174=CARTESIAN_POINT('Ctrl Pts',(-4.84176412499723,0.636309800095206,
6.33005968032332));
#39175=CARTESIAN_POINT('Ctrl Pts',(-4.91110009717082,0.79477268400084,6.32455974953522));
#39176=CARTESIAN_POINT('Ctrl Pts',(-4.96159302088883,1.06847604194515,6.37302357698648));
#39177=CARTESIAN_POINT('Ctrl Pts',(-4.97396758428929,1.18514270861186,6.40409612528611));
#39178=CARTESIAN_POINT('Ctrl Pts',(-4.9768601953599,1.30000000000013,6.44526302674352));
#39179=CARTESIAN_POINT('Ctrl Pts',(-4.94346631687566,-1.30000000000204,
6.19380864200921));
#39180=CARTESIAN_POINT('Ctrl Pts',(-4.94321747389919,-1.18514270861317,
6.16473300708982));
#39181=CARTESIAN_POINT('Ctrl Pts',(-4.93412052317185,-1.06847604194582,
6.14925032936665));
#39182=CARTESIAN_POINT('Ctrl Pts',(-4.89266384819064,-0.794772684000851,
6.14488469691208));
#39183=CARTESIAN_POINT('Ctrl Pts',(-4.83045152777307,-0.636309800095197,
6.18557396029434));
#39184=CARTESIAN_POINT('Ctrl Pts',(-4.77077828071587,-0.319434907277159,
6.23342821667916));
#39185=CARTESIAN_POINT('Ctrl Pts',(-4.73214233677919,-0.158333333333332,
6.27356575659754));
#39186=CARTESIAN_POINT('Ctrl Pts',(-4.73867559286303,0.158333333333334,
6.30681070735946));
#39187=CARTESIAN_POINT('Ctrl Pts',(-4.78422175451366,0.319434907277167,
6.3014102964853));
#39188=CARTESIAN_POINT('Ctrl Pts',(-4.85643493010519,0.636309800095206,
6.31823415136601));
#39189=CARTESIAN_POINT('Ctrl Pts',(-4.92620237914194,0.79477268400084,6.31264930485107));
#39190=CARTESIAN_POINT('Ctrl Pts',(-4.97470530482241,1.06847604194515,6.36274110209546));
#39191=CARTESIAN_POINT('Ctrl Pts',(-4.98569765033206,1.18514270861186,6.39487827212544));
#39192=CARTESIAN_POINT('Ctrl Pts',(-4.98668722203483,1.30000000000013,6.43746972924232));
#39193=CARTESIAN_POINT('',(-4.89594487155746,1.2,6.47046328764746));
#39194=CARTESIAN_POINT('Ctrl Pts',(-4.89594487155747,1.2,6.47046328764746));
#39195=CARTESIAN_POINT('Ctrl Pts',(-4.88130603224287,1.21680975658284,6.48627790618805));
#39196=CARTESIAN_POINT('Ctrl Pts',(-4.86723316699216,1.23314745186375,6.50310393971268));
#39197=CARTESIAN_POINT('Ctrl Pts',(-4.8493590579957,1.253505911239,6.52222463180939));
#39198=CARTESIAN_POINT('Ctrl Pts',(-4.84243698897397,1.26137686198304,6.52950748511096));
#39199=CARTESIAN_POINT('Ctrl Pts',(-4.82345328747211,1.28297787599002,6.55019123736902));
#39200=CARTESIAN_POINT('Ctrl Pts',(-4.81590450479927,1.29149306134563,6.55797296612504));
#39201=CARTESIAN_POINT('Ctrl Pts',(-4.80835019126374,1.30000000000021,6.56575364551941));
#39202=CARTESIAN_POINT('',(-4.87041241531834,0.65383484136893,6.3159282244369));
#39203=CARTESIAN_POINT('Ctrl Pts',(-4.87041241535557,0.653834841367665,
6.31592822443521));
#39204=CARTESIAN_POINT('Ctrl Pts',(-4.87329288427579,0.717401826164069,
6.33179692647823));
#39205=CARTESIAN_POINT('Ctrl Pts',(-4.87557695120327,0.763838048869181,
6.3447039736521));
#39206=CARTESIAN_POINT('Ctrl Pts',(-4.88436973136448,0.94985745749883,6.39584548840163));
#39207=CARTESIAN_POINT('Ctrl Pts',(-4.88949053569551,1.05909846488692,6.42714802739034));
#39208=CARTESIAN_POINT('Ctrl Pts',(-4.89594487155747,1.2,6.47046328764746));
#39209=CARTESIAN_POINT('',(-4.84356468978474,-0.653834841531101,6.17902933643005));
#39210=CARTESIAN_POINT('Ctrl Pts',(-4.84356468978474,-0.653834841531102,
6.17902933643005));
#39211=CARTESIAN_POINT('Ctrl Pts',(-4.81028140400316,-0.575983337726512,
6.2039379982198));
#39212=CARTESIAN_POINT('Ctrl Pts',(-4.78259022663897,-0.493640408079208,
6.22559809788892));
#39213=CARTESIAN_POINT('Ctrl Pts',(-4.74428627662278,-0.338139747975588,
6.25868215812499));
#39214=CARTESIAN_POINT('Ctrl Pts',(-4.73158448822581,-0.265664659145223,
6.27128401929845));
#39215=CARTESIAN_POINT('Ctrl Pts',(-4.71756195934014,-0.129719176923065,
6.29122561025372));
#39216=CARTESIAN_POINT('Ctrl Pts',(-4.71484294667695,-0.0666270999531989,
6.2990415867733));
#39217=CARTESIAN_POINT('Ctrl Pts',(-4.71704250209496,0.0595442011092,6.3121886496183));
#39218=CARTESIAN_POINT('Ctrl Pts',(-4.72196055121145,0.122778981188862,
6.31761996529194));
#39219=CARTESIAN_POINT('Ctrl Pts',(-4.74093392508663,0.260130875799006,
6.32599484684145));
#39220=CARTESIAN_POINT('Ctrl Pts',(-4.75649502802252,0.333944555596331,
6.32830536516641));
#39221=CARTESIAN_POINT('Ctrl Pts',(-4.80133474624554,0.491207260125491,
6.32745516422823));
#39222=CARTESIAN_POINT('Ctrl Pts',(-4.83265655726508,0.574351676991665,
6.32346821745691));
#39223=CARTESIAN_POINT('Ctrl Pts',(-4.87041241529386,0.653834841385582,
6.31592822448981));
#39224=CARTESIAN_POINT('',(-4.85793751499296,-1.2,6.24976681786834));
#39225=CARTESIAN_POINT('Ctrl Pts',(-4.85793751499296,-1.2,6.24976681786834));
#39226=CARTESIAN_POINT('Ctrl Pts',(-4.85542006159989,-1.13062235224762,
6.23689668082158));
#39227=CARTESIAN_POINT('Ctrl Pts',(-4.85227594825653,-1.03539419544579,
6.22109841849004));
#39228=CARTESIAN_POINT('Ctrl Pts',(-4.84600629457664,-0.796367988442622,
6.19059863057003));
#39229=CARTESIAN_POINT('Ctrl Pts',(-4.84488934637906,-0.739714948888321,
6.1853136109301));
#39230=CARTESIAN_POINT('Ctrl Pts',(-4.84356468978474,-0.653834841531101,
6.17902933643005));
#39231=CARTESIAN_POINT('Ctrl Pts',(-4.7734976991615,-1.30000000000002,6.34196753202476));
#39232=CARTESIAN_POINT('Ctrl Pts',(-4.78796623709172,-1.28305027811014,
6.32665270521319));
#39233=CARTESIAN_POINT('Ctrl Pts',(-4.80233849726868,-1.26612557264441,
6.31121947396146));
#39234=CARTESIAN_POINT('Ctrl Pts',(-4.82382646364986,-1.24074712529506,
6.28813340180523));
#39235=CARTESIAN_POINT('Ctrl Pts',(-4.83211932393341,-1.23088984123249,
6.27897567894286));
#39236=CARTESIAN_POINT('Ctrl Pts',(-4.84513604156342,-1.21538971859288,
6.26453695584227));
#39237=CARTESIAN_POINT('Ctrl Pts',(-4.8521670910965,-1.20698331563184,6.25664413364353));
#39238=CARTESIAN_POINT('Ctrl Pts',(-4.85793751499296,-1.2,6.24976681786834));
#39239=CARTESIAN_POINT('Origin',(0.,1.25,7.2));
#39240=CARTESIAN_POINT('Origin',(0.,1.2,7.2));
#39241=CARTESIAN_POINT('Origin',(0.,0.92691742076555,7.2));
#39242=CARTESIAN_POINT('Origin',(0.,0.653834841531101,7.2));
#39243=CARTESIAN_POINT('Origin',(0.,0.,7.2));
#39244=CARTESIAN_POINT('Origin',(0.,-0.653834841531101,7.2));
#39245=CARTESIAN_POINT('Origin',(0.,-0.926917420765551,7.2));
#39246=CARTESIAN_POINT('Origin',(0.,-1.2,7.2));
#39247=CARTESIAN_POINT('Origin',(0.,-1.25,7.2));
#39248=CARTESIAN_POINT('Ctrl Pts',(-4.86571446294974,-1.30000000000134,
5.868337644404));
#39249=CARTESIAN_POINT('Ctrl Pts',(-4.8821339505088,-1.18514270861269,5.90764937165957));
#39250=CARTESIAN_POINT('Ctrl Pts',(-4.88516330785636,-1.06847604194558,
5.94147912707392));
#39251=CARTESIAN_POINT('Ctrl Pts',(-4.86122784987519,-0.794772684000851,
6.00696817808235));
#39252=CARTESIAN_POINT('Ctrl Pts',(-4.795220551989,-0.636309800095197,6.03024314493531));
#39253=CARTESIAN_POINT('Ctrl Pts',(-4.73609341170194,-0.319434907277159,
6.07498424576792));
#39254=CARTESIAN_POINT('Ctrl Pts',(-4.69228837762394,-0.158333333333332,
6.08857601783884));
#39255=CARTESIAN_POINT('Ctrl Pts',(-4.69984189087714,0.158333333333334,
6.12160410624479));
#39256=CARTESIAN_POINT('Ctrl Pts',(-4.75146299021043,0.319434907277167,
6.14255691937913));
#39257=CARTESIAN_POINT('Ctrl Pts',(-4.82544129359938,0.636309800095206,
6.16200266173935));
#39258=CARTESIAN_POINT('Ctrl Pts',(-4.89882489071899,0.79477268400084,6.17387012311368));
#39259=CARTESIAN_POINT('Ctrl Pts',(-4.9349217851481,1.06847604194518,6.15301997060013));
#39260=CARTESIAN_POINT('Ctrl Pts',(-4.93693489080205,1.18514270861192,6.13517577749273));
#39261=CARTESIAN_POINT('Ctrl Pts',(-4.92533609403335,1.30000000000022,6.10851264972677));
#39262=CARTESIAN_POINT('Ctrl Pts',(-4.85356720775247,-1.30000000000134,
5.86521512469838));
#39263=CARTESIAN_POINT('Ctrl Pts',(-4.86766876337791,-1.18514270861269,
5.90399949143929));
#39264=CARTESIAN_POINT('Ctrl Pts',(-4.86900238119369,-1.06847604194558,
5.93741886516899));
#39265=CARTESIAN_POINT('Ctrl Pts',(-4.84258681457997,-0.794772684000851,
6.00223009688818));
#39266=CARTESIAN_POINT('Ctrl Pts',(-4.77700822871633,-0.636309800095197,
6.02540714067998));
#39267=CARTESIAN_POINT('Ctrl Pts',(-4.71780718134386,-0.319434907277159,
6.07001371292168));
#39268=CARTESIAN_POINT('Ctrl Pts',(-4.67477123304744,-0.158333333333332,
6.08402952939453));
#39269=CARTESIAN_POINT('Ctrl Pts',(-4.6823203577386,0.158333333333334,6.11658777090616));
#39270=CARTESIAN_POINT('Ctrl Pts',(-4.73316183806893,0.319434907277167,
6.13649746894165));
#39271=CARTESIAN_POINT('Ctrl Pts',(-4.80721762558705,0.636309800095206,
6.15542465374059));
#39272=CARTESIAN_POINT('Ctrl Pts',(-4.88018764438342,0.79477268400084,6.16716360018097));
#39273=CARTESIAN_POINT('Ctrl Pts',(-4.91877933308293,1.06847604194518,6.14706683419082));
#39274=CARTESIAN_POINT('Ctrl Pts',(-4.92249447744502,1.18514270861192,6.12979090408604));
#39275=CARTESIAN_POINT('Ctrl Pts',(-4.91321985409419,1.30000000000022,6.10393818921505));
#39276=CARTESIAN_POINT('Ctrl Pts',(-4.82938120791274,-1.30000000000253,
5.8595404167699));
#39277=CARTESIAN_POINT('Ctrl Pts',(-4.83868584525243,-1.18514270861378,
5.89560518362874));
#39278=CARTESIAN_POINT('Ctrl Pts',(-4.8365301203178,-1.06847604194656,5.92725947612256));
#39279=CARTESIAN_POINT('Ctrl Pts',(-4.80507423497627,-0.794772684001587,
5.99019814610711));
#39280=CARTESIAN_POINT('Ctrl Pts',(-4.74056097052128,-0.636309800095781,
6.01592842036806));
#39281=CARTESIAN_POINT('Ctrl Pts',(-4.68126449885463,-0.31943490727745,
6.06100334291516));
#39282=CARTESIAN_POINT('Ctrl Pts',(-4.63971683522099,-0.158333333333478,
6.07486407107751));
#39283=CARTESIAN_POINT('Ctrl Pts',(-4.64725684719242,0.15833333333348,6.10676535616951));
#39284=CARTESIAN_POINT('Ctrl Pts',(-4.69656249034137,0.319434907277462,
6.12571209947254));
#39285=CARTESIAN_POINT('Ctrl Pts',(-4.77077343930226,0.636309800095791,
6.14377196129411));
#39286=CARTESIAN_POINT('Ctrl Pts',(-4.84287989741261,0.794772684001569,
6.15422858003056));
#39287=CARTESIAN_POINT('Ctrl Pts',(-4.88648202335048,1.06847604194616,6.13566971188501));
#39288=CARTESIAN_POINT('Ctrl Pts',(-4.89362191156687,1.18514270861301,6.11973294382499));
#39289=CARTESIAN_POINT('Ctrl Pts',(-4.88902794329912,1.30000000000141,6.09589285405133));
#39290=CARTESIAN_POINT('Ctrl Pts',(-4.80495569332938,-1.30000000000374,
5.85368628458532));
#39291=CARTESIAN_POINT('Ctrl Pts',(-4.80967406261113,-1.18514270861488,
5.88968235144291));
#39292=CARTESIAN_POINT('Ctrl Pts',(-4.80415227688878,-1.06847604194755,
5.92110637924295));
#39293=CARTESIAN_POINT('Ctrl Pts',(-4.76773904064537,-0.794772684002323,
5.98313984495985));
#39294=CARTESIAN_POINT('Ctrl Pts',(-4.70398214416904,-0.636309800096376,
6.00737539224725));
#39295=CARTESIAN_POINT('Ctrl Pts',(-4.64449817003754,-0.31943490727775,
6.05173515931923));
#39296=CARTESIAN_POINT('Ctrl Pts',(-4.60450849084288,-0.158333333333626,
6.06643614477618));
#39297=CARTESIAN_POINT('Ctrl Pts',(-4.6120319495031,0.158333333333627,6.09763340854605));
#39298=CARTESIAN_POINT('Ctrl Pts',(-4.65977508101751,0.31943490727776,6.11534010784939));
#39299=CARTESIAN_POINT('Ctrl Pts',(-4.73411531820855,0.636309800096385,
6.1320613803948));
#39300=CARTESIAN_POINT('Ctrl Pts',(-4.80532269523504,0.794772684002312,
6.14066184138635));
#39301=CARTESIAN_POINT('Ctrl Pts',(-4.8539609032049,1.06847604194716,6.12349932855702));
#39302=CARTESIAN_POINT('Ctrl Pts',(-4.86455173919657,1.18514270861412,6.10896728959689));
#39303=CARTESIAN_POINT('Ctrl Pts',(-4.86467973317292,1.30000000000263,6.08733222754667));
#39304=CARTESIAN_POINT('Ctrl Pts',(-4.79263759311852,-1.3000000000039,5.85082946845672));
#39305=CARTESIAN_POINT('Ctrl Pts',(-4.79494039025008,-1.18514270861502,
5.88581163158155));
#39306=CARTESIAN_POINT('Ctrl Pts',(-4.78765825739138,-1.06847604194768,
5.91655896413454));
#39307=CARTESIAN_POINT('Ctrl Pts',(-4.74869196796596,-0.794772684002417,
5.97780814751876));
#39308=CARTESIAN_POINT('Ctrl Pts',(-4.68543647819062,-0.63630980009645,
6.00273352707067));
#39309=CARTESIAN_POINT('Ctrl Pts',(-4.62590743407482,-0.319434907277788,
6.04740201192308));
#39310=CARTESIAN_POINT('Ctrl Pts',(-4.58671565461658,-0.158333333333644,
6.06263789863126));
#39311=CARTESIAN_POINT('Ctrl Pts',(-4.59423006993087,0.158333333333646,
6.09350046461607));
#39312=CARTESIAN_POINT('Ctrl Pts',(-4.64114799628483,0.319434907277798,
6.11008166880538));
#39313=CARTESIAN_POINT('Ctrl Pts',(-4.7155520813538,0.636309800096461,6.12633371016645));
#39314=CARTESIAN_POINT('Ctrl Pts',(-4.78633595217113,0.794772684002406,
6.13495132958802));
#39315=CARTESIAN_POINT('Ctrl Pts',(-4.83752743384807,1.06847604194729,6.11849378740315));
#39316=CARTESIAN_POINT('Ctrl Pts',(-4.84986177812713,1.18514270861426,6.10446522757005));
#39317=CARTESIAN_POINT('Ctrl Pts',(-4.85237157109861,1.30000000000278,6.08353196810363));
#39318=CARTESIAN_POINT('Ctrl Pts',(-4.79235345691312,-1.3000000000039,5.85076475170828));
#39319=CARTESIAN_POINT('Ctrl Pts',(-4.79460046688034,-1.18514270861502,
5.88572335809722));
#39320=CARTESIAN_POINT('Ctrl Pts',(-4.78727767678747,-1.06847604194768,
5.91645491529231));
#39321=CARTESIAN_POINT('Ctrl Pts',(-4.7482524141831,-0.794772684002416,
5.97768563098373));
#39322=CARTESIAN_POINT('Ctrl Pts',(-4.68500846948588,-0.636309800096449,
6.00262629599803));
#39323=CARTESIAN_POINT('Ctrl Pts',(-4.62547840464194,-0.319434907277788,
6.04730232452214));
#39324=CARTESIAN_POINT('Ctrl Pts',(-4.58630512781722,-0.158333333333644,
6.06255206409805));
#39325=CARTESIAN_POINT('Ctrl Pts',(-4.59381933770018,0.158333333333646,
6.0934070741634));
#39326=CARTESIAN_POINT('Ctrl Pts',(-4.64071814564975,0.319434907277797,
6.1099612324191));
#39327=CARTESIAN_POINT('Ctrl Pts',(-4.7151236688301,0.63630980009646,6.1262018217059));
#39328=CARTESIAN_POINT('Ctrl Pts',(-4.78589776844809,0.794772684002405,
6.13481967784126));
#39329=CARTESIAN_POINT('Ctrl Pts',(-4.83714817867047,1.06847604194729,6.11837827953156));
#39330=CARTESIAN_POINT('Ctrl Pts',(-4.84952276532352,1.18514270861426,6.10436134959035));
#39331=CARTESIAN_POINT('Ctrl Pts',(-4.85208753505921,1.30000000000278,6.08344436182233));
#39332=CARTESIAN_POINT('Ctrl Pts',(-4.79206929192536,-1.3000000000039,5.85069980751958));
#39333=CARTESIAN_POINT('Ctrl Pts',(-4.79426054278171,-1.18514270861502,
5.88563507380463));
#39334=CARTESIAN_POINT('Ctrl Pts',(-4.78689711474143,-1.06847604194768,
5.91635100912804));
#39335=CARTESIAN_POINT('Ctrl Pts',(-4.74781290326158,-0.794772684002417,
5.97756346583113));
#39336=CARTESIAN_POINT('Ctrl Pts',(-4.68458049645332,-0.63630980009645,
6.00251948238273));
#39337=CARTESIAN_POINT('Ctrl Pts',(-4.62504939046843,-0.319434907277788,
6.04720275100294));
#39338=CARTESIAN_POINT('Ctrl Pts',(-4.58589457293348,-0.158333333333644,
6.06246562381856));
#39339=CARTESIAN_POINT('Ctrl Pts',(-4.5934085730634,0.158333333333646,6.09331300309073));
#39340=CARTESIAN_POINT('Ctrl Pts',(-4.64028830282297,0.319434907277797,
6.10984075513259));
#39341=CARTESIAN_POINT('Ctrl Pts',(-4.71469527329583,0.63630980009646,6.12607005366339));
#39342=CARTESIAN_POINT('Ctrl Pts',(-4.78545958296302,0.794772684002405,
6.13468785029002));
#39343=CARTESIAN_POINT('Ctrl Pts',(-4.83676891622233,1.06847604194729,6.11826256621009));
#39344=CARTESIAN_POINT('Ctrl Pts',(-4.84918374438527,1.18514270861426,6.10425728837294));
#39345=CARTESIAN_POINT('Ctrl Pts',(-4.85180349154136,1.30000000000278,6.08335662956008));
#39346=CARTESIAN_POINT('Ctrl Pts',(-4.79150104411294,-1.30000000000389,
5.85057075286265));
#39347=CARTESIAN_POINT('Ctrl Pts',(-4.7935807724207,-1.18514270861502,5.8854594671761));
#39348=CARTESIAN_POINT('Ctrl Pts',(-4.78613606158058,-1.06847604194768,
5.91614420454618));
#39349=CARTESIAN_POINT('Ctrl Pts',(-4.74693393044161,-0.794772684002416,
5.97732005858974));
#39350=CARTESIAN_POINT('Ctrl Pts',(-4.68372456524032,-0.636309800096449,
6.00230625476568));
#39351=CARTESIAN_POINT('Ctrl Pts',(-4.62419136920195,-0.319434907277788,
6.04700400909723));
#39352=CARTESIAN_POINT('Ctrl Pts',(-4.58507349960888,-0.158333333333644,
6.06229365668962));
#39353=CARTESIAN_POINT('Ctrl Pts',(-4.59258707820112,0.158333333333646,
6.09312584206709));
#39354=CARTESIAN_POINT('Ctrl Pts',(-4.6394286323444,0.319434907277797,6.10960059291445));
#39355=CARTESIAN_POINT('Ctrl Pts',(-4.71383847627133,0.63630980009646,6.12580692931946));
#39356=CARTESIAN_POINT('Ctrl Pts',(-4.7845831842747,0.794772684002405,6.13442406850582));
#39357=CARTESIAN_POINT('Ctrl Pts',(-4.83601036310554,1.06847604194729,6.1180308641712));
#39358=CARTESIAN_POINT('Ctrl Pts',(-4.84850568027476,1.18514270861426,6.10404893558892));
#39359=CARTESIAN_POINT('Ctrl Pts',(-4.85123539446212,1.30000000000278,6.08318108915274));
#39360=CARTESIAN_POINT('Ctrl Pts',(-4.79064879748123,-1.30000000000389,
5.85037865044717));
#39361=CARTESIAN_POINT('Ctrl Pts',(-4.79256131938749,-1.18514270861502,
5.88519857264719));
#39362=CARTESIAN_POINT('Ctrl Pts',(-4.78499472665041,-1.06847604194768,
5.91583711764781));
#39363=CARTESIAN_POINT('Ctrl Pts',(-4.74561573261963,-0.794772684002415,
5.97695846800678));
#39364=CARTESIAN_POINT('Ctrl Pts',(-4.6824408103457,-0.636309800096449,
6.00198863703091));
#39365=CARTESIAN_POINT('Ctrl Pts',(-4.62290439564666,-0.319434907277787,
6.04670719585982));
#39366=CARTESIAN_POINT('Ctrl Pts',(-4.58384189752997,-0.158333333333644,
6.06203623124653));
#39367=CARTESIAN_POINT('Ctrl Pts',(-4.59135482701311,0.158333333333646,
6.09284559935395));
#39368=CARTESIAN_POINT('Ctrl Pts',(-4.63813918883291,0.319434907277797,
6.10924228682364));
#39369=CARTESIAN_POINT('Ctrl Pts',(-4.71255331597794,0.636309800096459,
6.12541364383744));
#39370=CARTESIAN_POINT('Ctrl Pts',(-4.78326850781132,0.794772684002404,
6.13402741690736));
#39371=CARTESIAN_POINT('Ctrl Pts',(-4.83487243796819,1.06847604194729,6.11768186589438));
#39372=CARTESIAN_POINT('Ctrl Pts',(-4.84748850226198,1.18514270861426,6.10373517179134));
#39373=CARTESIAN_POINT('Ctrl Pts',(-4.85038320159871,1.30000000000278,6.08291716695642));
#39374=CARTESIAN_POINT('Ctrl Pts',(-4.78970212769114,-1.30000000000389,
5.85016849536932));
#39375=CARTESIAN_POINT('Ctrl Pts',(-4.79142904799313,-1.18514270861502,
5.8849144498525));
#39376=CARTESIAN_POINT('Ctrl Pts',(-4.78372712974911,-1.06847604194768,
5.91550308170812));
#39377=CARTESIAN_POINT('Ctrl Pts',(-4.74415165456808,-0.794772684002414,
5.9765646935901));
#39378=CARTESIAN_POINT('Ctrl Pts',(-4.68101470387775,-0.636309800096448,
6.00164031176));
#39379=CARTESIAN_POINT('Ctrl Pts',(-4.62147451839339,-0.319434907277787,
6.04637982868371));
#39380=CARTESIAN_POINT('Ctrl Pts',(-4.58247344360906,-0.158333333333644,
6.06175115231738));
#39381=CARTESIAN_POINT('Ctrl Pts',(-4.58998562257767,0.158333333333646,
6.0925352710236));
#39382=CARTESIAN_POINT('Ctrl Pts',(-4.63670660217091,0.319434907277796,
6.10884861201663));
#39383=CARTESIAN_POINT('Ctrl Pts',(-4.71112543273955,0.636309800096458,
6.1249797811688));
#39384=CARTESIAN_POINT('Ctrl Pts',(-4.78180756889426,0.794772684002403,
6.133583938481));
#39385=CARTESIAN_POINT('Ctrl Pts',(-4.83360785935252,1.06847604194728,6.11729033614163));
#39386=CARTESIAN_POINT('Ctrl Pts',(-4.84635812346542,1.18514270861425,6.10338341028972));
#39387=CARTESIAN_POINT('Ctrl Pts',(-4.84943622534175,1.30000000000278,6.08262245530113));
#39388=CARTESIAN_POINT('Ctrl Pts',(-4.78894492917833,-1.30000000000389,
5.85000225316197));
#39389=CARTESIAN_POINT('Ctrl Pts',(-4.79052351881161,-1.18514270861502,
5.88469093422728));
#39390=CARTESIAN_POINT('Ctrl Pts',(-4.78271342462246,-1.06847604194768,
5.91524073943617));
#39391=CARTESIAN_POINT('Ctrl Pts',(-4.74298080681207,-0.794772684002414,
5.97625526972861));
#39392=CARTESIAN_POINT('Ctrl Pts',(-4.67987401751868,-0.636309800096447,
6.00136483869678));
#39393=CARTESIAN_POINT('Ctrl Pts',(-4.6203306644492,-0.319434907277787,
6.04611937197189));
#39394=CARTESIAN_POINT('Ctrl Pts',(-4.58137862503731,-0.158333333333644,
6.06152297641083));
#39395=CARTESIAN_POINT('Ctrl Pts',(-4.58889018478066,0.158333333333646,
6.0922869758967));
#39396=CARTESIAN_POINT('Ctrl Pts',(-4.63556060966728,0.319434907277796,
6.10853657817495));
#39397=CARTESIAN_POINT('Ctrl Pts',(-4.70998317996087,0.636309800096458,
6.1246348456659));
#39398=CARTESIAN_POINT('Ctrl Pts',(-4.78063868238186,0.794772684002403,
6.13322692900062));
#39399=CARTESIAN_POINT('Ctrl Pts',(-4.83259604193094,1.06847604194728,6.11697421639103));
#39400=CARTESIAN_POINT('Ctrl Pts',(-4.84545369240368,1.18514270861425,6.10309959311482));
#39401=CARTESIAN_POINT('Ctrl Pts',(-4.84867857761027,1.30000000000278,6.08238554362872));
#39402=CARTESIAN_POINT('Ctrl Pts',(-4.78705216995794,-1.30000000000389,
5.84958985324092));
#39403=CARTESIAN_POINT('Ctrl Pts',(-4.78826023810035,-1.18514270861501,
5.88413897274494));
#39404=CARTESIAN_POINT('Ctrl Pts',(-4.78017987927369,-1.06847604194767,
5.91459382625139));
#39405=CARTESIAN_POINT('Ctrl Pts',(-4.74005450947193,-0.794772684002412,
5.97549205681426));
#39406=CARTESIAN_POINT('Ctrl Pts',(-4.67702271654217,-0.636309800096446,
6.00068204622885));
#39407=CARTESIAN_POINT('Ctrl Pts',(-4.61747116261762,-0.319434907277786,
6.04547075761471));
#39408=CARTESIAN_POINT('Ctrl Pts',(-4.5786415099605,-0.158333333333643,
6.06095195063578));
#39409=CARTESIAN_POINT('Ctrl Pts',(-4.58615148454829,0.158333333333645,
6.09166571508387));
#39410=CARTESIAN_POINT('Ctrl Pts',(-4.63269580912546,0.319434907277795,
6.1077614980812));
#39411=CARTESIAN_POINT('Ctrl Pts',(-4.70712768682217,0.636309800096456,
6.12377621359621));
#39412=CARTESIAN_POINT('Ctrl Pts',(-4.77771625631815,0.7947726840024,6.13233008846881));
#39413=CARTESIAN_POINT('Ctrl Pts',(-4.83006624206924,1.06847604194728,6.11617846264734));
#39414=CARTESIAN_POINT('Ctrl Pts',(-4.84319239988727,1.18514270861425,6.10238553916046));
#39415=CARTESIAN_POINT('Ctrl Pts',(-4.84678434644982,1.30000000000277,6.0817911325281));
#39416=CARTESIAN_POINT('Ctrl Pts',(-4.78232267396703,-1.30000000000387,
5.84859386619855));
#39417=CARTESIAN_POINT('Ctrl Pts',(-4.78260808356488,-1.18514270861499,
5.88283739808244));
#39418=CARTESIAN_POINT('Ctrl Pts',(-4.77385415910733,-1.06847604194765,
5.91308020204031));
#39419=CARTESIAN_POINT('Ctrl Pts',(-4.73274817241335,-0.794772684002398,
5.97370464738306));
#39420=CARTESIAN_POINT('Ctrl Pts',(-4.66989905139225,-0.636309800096434,
5.99904293743694));
#39421=CARTESIAN_POINT('Ctrl Pts',(-4.61032360362397,-0.31943490727778,
6.04387655671116));
#39422=CARTESIAN_POINT('Ctrl Pts',(-4.57179738839238,-0.158333333333641,
6.05951301291473));
#39423=CARTESIAN_POINT('Ctrl Pts',(-4.57930300663517,0.158333333333642,
6.09010245591926));
#39424=CARTESIAN_POINT('Ctrl Pts',(-4.6255356682504,0.31943490727779,6.10588183844076));
#39425=CARTESIAN_POINT('Ctrl Pts',(-4.69999044749396,0.636309800096445,
6.12167340347345));
#39426=CARTESIAN_POINT('Ctrl Pts',(-4.77040755918437,0.794772684002386,
6.13003584639514));
#39427=CARTESIAN_POINT('Ctrl Pts',(-4.82373861375105,1.06847604194726,6.11412346862001));
#39428=CARTESIAN_POINT('Ctrl Pts',(-4.83753655289709,1.18514270861423,6.10054603239835));
#39429=CARTESIAN_POINT('Ctrl Pts',(-4.84204739377757,1.30000000000275,6.08027903868217));
#39430=CARTESIAN_POINT('Ctrl Pts',(-4.77627501138971,-1.30000000000379,
5.84743290715711));
#39431=CARTESIAN_POINT('Ctrl Pts',(-4.77539694113463,-1.18514270861493,
5.88148413234476));
#39432=CARTESIAN_POINT('Ctrl Pts',(-4.76579122721606,-1.06847604194759,
5.91157346660426));
#39433=CARTESIAN_POINT('Ctrl Pts',(-4.72343750362598,-0.794772684002353,
5.9719330874767));
#39434=CARTESIAN_POINT('Ctrl Pts',(-4.66080161735695,-0.636309800096398,
5.99723877747126));
#39435=CARTESIAN_POINT('Ctrl Pts',(-4.60118031170647,-0.319434907277762,
6.04193925472643));
#39436=CARTESIAN_POINT('Ctrl Pts',(-4.56302917655413,-0.158333333333632,
6.05756656837047));
#39437=CARTESIAN_POINT('Ctrl Pts',(-4.57052736738655,0.158333333333633,
6.0880007030458));
#39438=CARTESIAN_POINT('Ctrl Pts',(-4.6163784835927,0.319434907277771,6.10370721172841));
#39439=CARTESIAN_POINT('Ctrl Pts',(-4.69086203192954,0.636309800096409,
6.11916627651037));
#39440=CARTESIAN_POINT('Ctrl Pts',(-4.76104209380644,0.794772684002341,
6.12685833128135));
#39441=CARTESIAN_POINT('Ctrl Pts',(-4.81562672710523,1.0684760419472,6.11119753499256));
#39442=CARTESIAN_POINT('Ctrl Pts',(-4.83028658473183,1.18514270861416,6.09794745392577));
#39443=CARTESIAN_POINT('Ctrl Pts',(-4.83597863478999,1.30000000000268,6.07822627021593));
#39444=CARTESIAN_POINT('Ctrl Pts',(-4.77022543175637,-1.30000000000376,
5.84627362658672));
#39445=CARTESIAN_POINT('Ctrl Pts',(-4.7681845197533,-1.1851427086149,5.88014847704338));
#39446=CARTESIAN_POINT('Ctrl Pts',(-4.75772785182655,-1.06847604194757,
5.91009960050316));
#39447=CARTESIAN_POINT('Ctrl Pts',(-4.71412877731664,-0.794772684002333,
5.97022809309519));
#39448=CARTESIAN_POINT('Ctrl Pts',(-4.6517090215279,-0.636309800096382,
5.99552776578552));
#39449=CARTESIAN_POINT('Ctrl Pts',(-4.59204348242412,-0.319434907277754,
6.0401111535088));
#39450=CARTESIAN_POINT('Ctrl Pts',(-4.55426759534573,-0.158333333333628,
6.05572325434686));
#39451=CARTESIAN_POINT('Ctrl Pts',(-4.56175638576926,0.15833333333363,6.08599115135827));
#39452=CARTESIAN_POINT('Ctrl Pts',(-4.6072219529283,0.319434907277763,6.10160387512772));
#39453=CARTESIAN_POINT('Ctrl Pts',(-4.68173242114704,0.636309800096393,
6.11672482164359));
#39454=CARTESIAN_POINT('Ctrl Pts',(-4.75167730793368,0.794772684002322,
6.12377701094137));
#39455=CARTESIAN_POINT('Ctrl Pts',(-4.80751491300795,1.06847604194717,6.10834343885876));
#39456=CARTESIAN_POINT('Ctrl Pts',(-4.82303611146367,1.18514270861413,6.09539943328269));
#39457=CARTESIAN_POINT('Ctrl Pts',(-4.82990847812561,1.30000000000264,6.0761920436149));
#39458=CARTESIAN_POINT('Ctrl Pts',(-4.76568523200038,-1.30000000000375,
5.84537209489026));
#39459=CARTESIAN_POINT('Ctrl Pts',(-4.76276723985793,-1.18514270861489,
5.87906444452569));
#39460=CARTESIAN_POINT('Ctrl Pts',(-4.75166970878787,-1.06847604194756,
5.90888582986161));
#39461=CARTESIAN_POINT('Ctrl Pts',(-4.70713582072867,-0.794772684002326,
5.96883649381953));
#39462=CARTESIAN_POINT('Ctrl Pts',(-4.64488596516521,-0.636309800096377,
5.99421317981936));
#39463=CARTESIAN_POINT('Ctrl Pts',(-4.58519342042272,-0.319434907277752,
6.03878281966128));
#39464=CARTESIAN_POINT('Ctrl Pts',(-4.54770428969278,-0.158333333333626,
6.05445557738353));
#39465=CARTESIAN_POINT('Ctrl Pts',(-4.55518551943629,0.158333333333628,
6.08459347174527));
#39466=CARTESIAN_POINT('Ctrl Pts',(-4.60035336788503,0.319434907277761,
6.10001436535062));
#39467=CARTESIAN_POINT('Ctrl Pts',(-4.67488237016258,0.636309800096388,
6.11488663820045));
#39468=CARTESIAN_POINT('Ctrl Pts',(-4.74465663872414,0.794772684002315,
6.12160101488735));
#39469=CARTESIAN_POINT('Ctrl Pts',(-4.8014344625704,1.06847604194717,6.10634068048414));
#39470=CARTESIAN_POINT('Ctrl Pts',(-4.81760103124188,1.18514270861412,6.09359999685794));
#39471=CARTESIAN_POINT('Ctrl Pts',(-4.82535715246749,1.30000000000263,6.07472426291758));
#39472=CARTESIAN_POINT('Ctrl Pts',(-4.76114118660295,-1.30000000000373,
5.8444295275307));
#39473=CARTESIAN_POINT('Ctrl Pts',(-4.75734057622045,-1.18514270861487,
5.87788182555618));
#39474=CARTESIAN_POINT('Ctrl Pts',(-4.74559912821443,-1.06847604194755,
5.90754235702996));
#39475=CARTESIAN_POINT('Ctrl Pts',(-4.7001291109825,-0.794772684002317,
5.96730437902859));
#39476=CARTESIAN_POINT('Ctrl Pts',(-4.63805715956591,-0.63630980009637,
5.99284271864704));
#39477=CARTESIAN_POINT('Ctrl Pts',(-4.57834408708591,-0.319434907277748,
6.03747567657016));
#39478=CARTESIAN_POINT('Ctrl Pts',(-4.5411474242754,-0.158333333333624,
6.05328516135936));
#39479=CARTESIAN_POINT('Ctrl Pts',(-4.5486211589217,0.158333333333626,6.08329216744718));
#39480=CARTESIAN_POINT('Ctrl Pts',(-4.59348320110659,0.319434907277756,
6.09840197555842));
#39481=CARTESIAN_POINT('Ctrl Pts',(-4.66802936642217,0.636309800096379,
6.11303286590956));
#39482=CARTESIAN_POINT('Ctrl Pts',(-4.73763869169212,0.794772684002305,
6.11955205859386));
#39483=CARTESIAN_POINT('Ctrl Pts',(-4.79535698540585,1.06847604194715,6.10446706721648));
#39484=CARTESIAN_POINT('Ctrl Pts',(-4.81216812185674,1.18514270861411,6.09190266428265));
#39485=CARTESIAN_POINT('Ctrl Pts',(-4.82080628408339,1.30000000000262,6.07330359222823));
#39486=CARTESIAN_POINT('Ctrl Pts',(-4.75204633607105,-1.3000000000037,5.84247157674721));
#39487=CARTESIAN_POINT('Ctrl Pts',(-4.74647043807593,-1.18514270861484,
5.87533933711595));
#39488=CARTESIAN_POINT('Ctrl Pts',(-4.73343521713089,-1.06847604194752,
5.90461737006026));
#39489=CARTESIAN_POINT('Ctrl Pts',(-4.68608872081418,-0.794772684002296,
5.96396249473901));
#39490=CARTESIAN_POINT('Ctrl Pts',(-4.62438259342724,-0.636309800096353,
5.9899294806832));
#39491=CARTESIAN_POINT('Ctrl Pts',(-4.56464098529988,-0.319434907277739,
6.03483539724006));
#39492=CARTESIAN_POINT('Ctrl Pts',(-4.52804496558433,-0.15833333333362,
6.05110941818164));
#39493=CARTESIAN_POINT('Ctrl Pts',(-4.53550641380118,0.158333333333622,
6.08088277914227));
#39494=CARTESIAN_POINT('Ctrl Pts',(-4.57974262825361,0.319434907277748,
6.09517289227285));
#39495=CARTESIAN_POINT('Ctrl Pts',(-4.65431857536549,0.636309800096363,
6.109302420349));
#39496=CARTESIAN_POINT('Ctrl Pts',(-4.72360073491046,0.794772684002285,
6.11557128000159));
#39497=CARTESIAN_POINT('Ctrl Pts',(-4.78320294093358,1.06847604194713,6.10086986779172));
#39498=CARTESIAN_POINT('Ctrl Pts',(-4.80130507524539,1.18514270861408,6.08865415566601));
#39499=CARTESIAN_POINT('Ctrl Pts',(-4.81170975736097,1.30000000000258,6.07058642801923));
#39500=CARTESIAN_POINT('Ctrl Pts',(-4.73839544802899,-1.30000000000347,
5.83951983631493));
#39501=CARTESIAN_POINT('Ctrl Pts',(-4.7301586668395,-1.18514270861464,5.87155305687854));
#39502=CARTESIAN_POINT('Ctrl Pts',(-4.7151830138948,-1.06847604194733,5.90027308429101));
#39503=CARTESIAN_POINT('Ctrl Pts',(-4.6650181178623,-0.794772684002159,
5.95896795405434));
#39504=CARTESIAN_POINT('Ctrl Pts',(-4.60385010015465,-0.636309800096243,
5.98546376809877));
#39505=CARTESIAN_POINT('Ctrl Pts',(-4.5440599408242,-0.319434907277684,
6.0306795094364));
#39506=CARTESIAN_POINT('Ctrl Pts',(-4.50836163191022,-0.158333333333593,
6.04753069331569));
#39507=CARTESIAN_POINT('Ctrl Pts',(-4.51581263521795,0.158333333333595,
6.07704719623594));
#39508=CARTESIAN_POINT('Ctrl Pts',(-4.55913169821868,0.319434907277693,
6.09048284576324));
#39509=CARTESIAN_POINT('Ctrl Pts',(-4.63375324468253,0.636309800096253,
6.10382098788036));
#39510=CARTESIAN_POINT('Ctrl Pts',(-4.70252536720865,0.794772684002148,
6.10926268214505));
#39511=CARTESIAN_POINT('Ctrl Pts',(-4.76494233919913,1.06847604194694,6.09498933287893));
#39512=CARTESIAN_POINT('Ctrl Pts',(-4.78497737290546,1.18514270861387,6.08329204250012));
#39513=CARTESIAN_POINT('Ctrl Pts',(-4.79802944592016,1.30000000000236,6.06607586576008));
#39514=CARTESIAN_POINT('Ctrl Pts',(-4.71419853039106,-1.30000000000326,
5.83508745077068));
#39515=CARTESIAN_POINT('Ctrl Pts',(-4.70128641819185,-1.18514270861444,
5.86629312556564));
#39516=CARTESIAN_POINT('Ctrl Pts',(-4.68289983264278,-1.06847604194715,
5.89447943720253));
#39517=CARTESIAN_POINT('Ctrl Pts',(-4.62777601319786,-0.794772684002022,
5.95262012281929));
#39518=CARTESIAN_POINT('Ctrl Pts',(-4.56756758295101,-0.636309800096134,
5.98001645391371));
#39519=CARTESIAN_POINT('Ctrl Pts',(-4.50763426831788,-0.319434907277629,
6.02520090889999));
#39520=CARTESIAN_POINT('Ctrl Pts',(-4.4734303023097,-0.158333333333566,
6.04204654909383));
#39521=CARTESIAN_POINT('Ctrl Pts',(-4.48078676006398,0.158333333333568,
6.07036303417538));
#39522=CARTESIAN_POINT('Ctrl Pts',(-4.52244787459498,0.319434907277638,
6.08189554315551));
#39523=CARTESIAN_POINT('Ctrl Pts',(-4.59716066414553,0.636309800096144,
6.09426412410944));
#39524=CARTESIAN_POINT('Ctrl Pts',(-4.66509691199277,0.794772684002011,
6.099765775605));
#39525=CARTESIAN_POINT('Ctrl Pts',(-4.73255426551456,1.06847604194676,6.08658695557659));
#39526=CARTESIAN_POINT('Ctrl Pts',(-4.75603454243535,1.18514270861367,6.07568871813639));
#39527=CARTESIAN_POINT('Ctrl Pts',(-4.77379530747862,1.30000000000213,6.05959686612286));
#39528=CARTESIAN_POINT('Ctrl Pts',(-4.6899767271724,-1.30000000000266,5.83061257312496));
#39529=CARTESIAN_POINT('Ctrl Pts',(-4.67239628145367,-1.18514270861389,
5.86104763341269));
#39530=CARTESIAN_POINT('Ctrl Pts',(-4.65059129853361,-1.06847604194666,
5.88862683954874));
#39531=CARTESIAN_POINT('Ctrl Pts',(-4.59045789986563,-0.794772684001657,
5.94574272852212));
#39532=CARTESIAN_POINT('Ctrl Pts',(-4.53107781153004,-0.636309800095843,
5.97283638745076));
#39533=CARTESIAN_POINT('Ctrl Pts',(-4.47099998458852,-0.319434907277484,
6.01798611679661));
#39534=CARTESIAN_POINT('Ctrl Pts',(-4.43838210287182,-0.158333333333493,
6.03554697854391));
#39535=CARTESIAN_POINT('Ctrl Pts',(-4.44575286345258,0.158333333333495,
6.06394314232543));
#39536=CARTESIAN_POINT('Ctrl Pts',(-4.48587786612484,0.319434907277491,
6.07537408568716));
#39537=CARTESIAN_POINT('Ctrl Pts',(-4.56069164539184,0.636309800095852,
6.08685201887608));
#39538=CARTESIAN_POINT('Ctrl Pts',(-4.62764863713308,0.794772684001649,
6.09033053580248));
#39539=CARTESIAN_POINT('Ctrl Pts',(-4.70010066093033,1.06847604194627,6.07757917622409));
#39540=CARTESIAN_POINT('Ctrl Pts',(-4.72702320461142,1.18514270861313,6.06744101183158));
#39541=CARTESIAN_POINT('Ctrl Pts',(-4.74950649548384,1.30000000000154,6.05268427412358));
#39542=CARTESIAN_POINT('Ctrl Pts',(-4.66877735037765,-1.30000000000264,
5.82675327965573));
#39543=CARTESIAN_POINT('Ctrl Pts',(-4.64706603325485,-1.18514270861388,
5.85625566876312));
#39544=CARTESIAN_POINT('Ctrl Pts',(-4.62226555204477,-1.06847604194665,
5.88336993160839));
#39545=CARTESIAN_POINT('Ctrl Pts',(-4.5578348921036,-0.794772684001648,
5.94049225356201));
#39546=CARTESIAN_POINT('Ctrl Pts',(-4.49946257054952,-0.636309800095834,
5.96973893422419));
#39547=CARTESIAN_POINT('Ctrl Pts',(-4.43931596611307,-0.319434907277479,
6.01540532493937));
#39548=CARTESIAN_POINT('Ctrl Pts',(-4.40795888236539,-0.158333333333491,
6.03257214071144));
#39549=CARTESIAN_POINT('Ctrl Pts',(-4.4152014829334,0.158333333333493,6.05973785294993));
#39550=CARTESIAN_POINT('Ctrl Pts',(-4.45384676217341,0.319434907277487,
6.0697156635662));
#39551=CARTESIAN_POINT('Ctrl Pts',(-4.52865314890444,0.636309800095844,
6.07942682304315));
#39552=CARTESIAN_POINT('Ctrl Pts',(-4.59476100455357,0.794772684001637,
6.08114178701595));
#39553=CARTESIAN_POINT('Ctrl Pts',(-4.67161008343351,1.06847604194625,6.0689607630618));
#39554=CARTESIAN_POINT('Ctrl Pts',(-4.7015700288836,1.18514270861311,6.05971218530979));
#39555=CARTESIAN_POINT('Ctrl Pts',(-4.72822480107566,1.30000000000152,6.04648774372412));
#39556=CARTESIAN_POINT('Ctrl Pts',(-4.65668899582123,-1.30000000000259,
5.82486454122853));
#39557=CARTESIAN_POINT('Ctrl Pts',(-4.63268492611192,-1.18514270861383,
5.85438347155262));
#39558=CARTESIAN_POINT('Ctrl Pts',(-4.60619833147062,-1.0684760419466,5.88143057604729));
#39559=CARTESIAN_POINT('Ctrl Pts',(-4.53927387000397,-0.794772684001615,
5.93820438603154));
#39560=CARTESIAN_POINT('Ctrl Pts',(-4.48123986180072,-0.636309800095808,
5.96667396749507));
#39561=CARTESIAN_POINT('Ctrl Pts',(-4.42100907641847,-0.319434907277466,
6.01224361017099));
#39562=CARTESIAN_POINT('Ctrl Pts',(-4.39048085176486,-0.158333333333485,
6.03003588512597));
#39563=CARTESIAN_POINT('Ctrl Pts',(-4.39774247939571,0.158333333333486,
6.05739059266253));
#39564=CARTESIAN_POINT('Ctrl Pts',(-4.43560985984673,0.319434907277474,
6.06724398831812));
#39565=CARTESIAN_POINT('Ctrl Pts',(-4.51047413856541,0.636309800095818,
6.07680124445811));
#39566=CARTESIAN_POINT('Ctrl Pts',(-4.57611344914273,0.794772684001604,
6.07816850227793));
#39567=CARTESIAN_POINT('Ctrl Pts',(-4.65545714136725,1.06847604194621,6.06609450796775));
#39568=CARTESIAN_POINT('Ctrl Pts',(-4.68713161746142,1.18514270861306,6.0569985637333));
#39569=CARTESIAN_POINT('Ctrl Pts',(-4.71613562525932,1.30000000000147,6.04403306001569));
#39570=CARTESIAN_POINT('Ctrl Pts',(-4.6385500391079,-1.30000000000254,5.82194913720228));
#39571=CARTESIAN_POINT('Ctrl Pts',(-4.6110649246645,-1.18514270861378,5.85117482972643));
#39572=CARTESIAN_POINT('Ctrl Pts',(-4.58203703282286,-1.06847604194656,
5.87804672524838));
#39573=CARTESIAN_POINT('Ctrl Pts',(-4.51141267123745,-0.794772684001582,
5.93468843765767));
#39574=CARTESIAN_POINT('Ctrl Pts',(-4.45405337867724,-0.636309800095782,
5.96342119536517));
#39575=CARTESIAN_POINT('Ctrl Pts',(-4.39376005396835,-0.319434907277453,
6.00937354447557));
#39576=CARTESIAN_POINT('Ctrl Pts',(-4.36448053136045,-0.158333333333478,
6.02816349840518));
#39577=CARTESIAN_POINT('Ctrl Pts',(-4.37165158819181,0.15833333333348,6.05464897920957));
#39578=CARTESIAN_POINT('Ctrl Pts',(-4.40812695127766,0.319434907277462,
6.06222289700424));
#39579=CARTESIAN_POINT('Ctrl Pts',(-4.48297671991519,0.636309800095792,
6.07046727421452));
#39580=CARTESIAN_POINT('Ctrl Pts',(-4.54799913250792,0.794772684001572,
6.07183807993206));
#39581=CARTESIAN_POINT('Ctrl Pts',(-4.63110244925331,1.06847604194617,6.06010258324103));
#39582=CARTESIAN_POINT('Ctrl Pts',(-4.66535361882063,1.18514270861302,6.05135680623418));
#39583=CARTESIAN_POINT('Ctrl Pts',(-4.69788361141755,1.30000000000142,6.03894511389501));
#39584=CARTESIAN_POINT('Ctrl Pts',(-4.61140095727358,-1.30000000000236,
5.81803205131993));
#39585=CARTESIAN_POINT('Ctrl Pts',(-4.57863767876715,-1.18514270861362,
5.84646339489592));
#39586=CARTESIAN_POINT('Ctrl Pts',(-4.54577035281995,-1.06847604194641,
5.87290621620585));
#39587=CARTESIAN_POINT('Ctrl Pts',(-4.46959988439323,-0.794772684001473,
5.92940053906282));
#39588=CARTESIAN_POINT('Ctrl Pts',(-4.41342115796732,-0.636309800095694,
5.95967386773921));
#39589=CARTESIAN_POINT('Ctrl Pts',(-4.35300585333055,-0.319434907277409,
6.00596677714269));
#39590=CARTESIAN_POINT('Ctrl Pts',(-4.32536175684254,-0.158333333333456,
6.02435308394741));
#39591=CARTESIAN_POINT('Ctrl Pts',(-4.33244618099113,0.158333333333458,
6.05024947851058));
#39592=CARTESIAN_POINT('Ctrl Pts',(-4.36716577455457,0.319434907277417,
6.05764609854191));
#39593=CARTESIAN_POINT('Ctrl Pts',(-4.44202972489185,0.636309800095704,
6.06433340585152));
#39594=CARTESIAN_POINT('Ctrl Pts',(-4.50585104292808,0.794772684001463,
6.06303841157629));
#39595=CARTESIAN_POINT('Ctrl Pts',(-4.59453487650259,1.06847604194602,6.05120416246776));
#39596=CARTESIAN_POINT('Ctrl Pts',(-4.63266259593145,1.18514270861285,6.04306544885702));
#39597=CARTESIAN_POINT('Ctrl Pts',(-4.67053008929466,1.30000000000123,6.03191062957247));
#39598=CARTESIAN_POINT('Ctrl Pts',(-4.57222382486624,-1.30000000000223,
5.8129401407569));
#39599=CARTESIAN_POINT('Ctrl Pts',(-4.53192410469008,-1.1851427086135,5.84097066369169));
#39600=CARTESIAN_POINT('Ctrl Pts',(-4.49355515363301,-1.06847604194631,
5.86719880429505));
#39601=CARTESIAN_POINT('Ctrl Pts',(-4.40937566392314,-0.794772684001394,
5.92362719225931));
#39602=CARTESIAN_POINT('Ctrl Pts',(-4.35463820992037,-0.636309800095632,
5.95423463035154));
#39603=CARTESIAN_POINT('Ctrl Pts',(-4.29413126263758,-0.319434907277378,
6.0016073619271));
#39604=CARTESIAN_POINT('Ctrl Pts',(-4.26923747674129,-0.158333333333441,
6.02208737503148));
#39605=CARTESIAN_POINT('Ctrl Pts',(-4.27623577636103,0.158333333333443,
6.04740990767795));
#39606=CARTESIAN_POINT('Ctrl Pts',(-4.30810217356727,0.319434907277386,
6.05218580897125));
#39607=CARTESIAN_POINT('Ctrl Pts',(-4.3829164785186,0.636309800095641,6.05652894968977));
#39608=CARTESIAN_POINT('Ctrl Pts',(-4.44517956069008,0.794772684001385,
6.05363371707215));
#39609=CARTESIAN_POINT('Ctrl Pts',(-4.54192034046459,1.06847604194591,6.04156167104665));
#39610=CARTESIAN_POINT('Ctrl Pts',(-4.5856176637484,1.18514270861273,6.03381010284268));
#39611=CARTESIAN_POINT('Ctrl Pts',(-4.6311368113508,1.30000000000111,6.02353250784577));
#39612=CARTESIAN_POINT('Ctrl Pts',(-4.5421776312674,-1.30000000000179,5.80967119057722));
#39613=CARTESIAN_POINT('Ctrl Pts',(-4.49613780399504,-1.1851427086131,5.83764276311977));
#39614=CARTESIAN_POINT('Ctrl Pts',(-4.45360293348106,-1.06847604194595,
5.86403841702219));
#39615=CARTESIAN_POINT('Ctrl Pts',(-4.36343602479835,-0.794772684001127,
5.92137697064901));
#39616=CARTESIAN_POINT('Ctrl Pts',(-4.31006770585718,-0.636309800095419,
5.95391965294267));
#39617=CARTESIAN_POINT('Ctrl Pts',(-4.24945538152908,-0.31943490727727,
6.00180978892079));
#39618=CARTESIAN_POINT('Ctrl Pts',(-4.22634870087955,-0.158333333333388,
6.02163654041449));
#39619=CARTESIAN_POINT('Ctrl Pts',(-4.23313585212819,0.15833333333339,6.0457016352853));
#39620=CARTESIAN_POINT('Ctrl Pts',(-4.262919571444,0.319434907277279,6.04960166635644));
#39621=CARTESIAN_POINT('Ctrl Pts',(-4.3375811255764,0.636309800095428,6.0514195136938));
#39622=CARTESIAN_POINT('Ctrl Pts',(-4.39840987105965,0.794772684001118,
6.04525831064287));
#39623=CARTESIAN_POINT('Ctrl Pts',(-4.50126981575944,1.06847604194556,6.03256320433072));
#39624=CARTESIAN_POINT('Ctrl Pts',(-4.54925728061249,1.18514270861234,6.02528851544578));
#39625=CARTESIAN_POINT('Ctrl Pts',(-4.60070795159461,1.30000000000067,6.01623437879837));
#39626=CARTESIAN_POINT('Ctrl Pts',(-4.51828305614685,-1.3000000000018,5.80812478043957));
#39627=CARTESIAN_POINT('Ctrl Pts',(-4.46765585165983,-1.18514270861311,
5.83630343387209));
#39628=CARTESIAN_POINT('Ctrl Pts',(-4.42177977482573,-1.06847604194595,
5.86293272402902));
#39629=CARTESIAN_POINT('Ctrl Pts',(-4.32677291519949,-0.794772684001131,
5.92087237234703));
#39630=CARTESIAN_POINT('Ctrl Pts',(-4.27437894207358,-0.636309800095424,
5.95403163528976));
#39631=CARTESIAN_POINT('Ctrl Pts',(-4.21367516448227,-0.319434907277274,
6.0023185425716));
#39632=CARTESIAN_POINT('Ctrl Pts',(-4.19210250856307,-0.158333333333389,
6.02234076606613));
#39633=CARTESIAN_POINT('Ctrl Pts',(-4.19876223512815,0.158333333333391,
6.04576448034503));
#39634=CARTESIAN_POINT('Ctrl Pts',(-4.22682600268163,0.319434907277282,
6.04858357395717));
#39635=CARTESIAN_POINT('Ctrl Pts',(-4.30143862024318,0.636309800095434,
6.04919538720387));
#39636=CARTESIAN_POINT('Ctrl Pts',(-4.36130680882284,0.794772684001125,
6.04243070845557));
#39637=CARTESIAN_POINT('Ctrl Pts',(-4.46906310127177,1.06847604194557,6.02904686633574));
#39638=CARTESIAN_POINT('Ctrl Pts',(-4.52043980609259,1.18514270861235,6.02155875226917));
#39639=CARTESIAN_POINT('Ctrl Pts',(-4.57654950949723,1.30000000000068,6.01237589346949));
#39640=CARTESIAN_POINT('Ctrl Pts',(-4.49429427127325,-1.3000000000017,5.80593985674212));
#39641=CARTESIAN_POINT('Ctrl Pts',(-4.4390616583647,-1.18514270861302,5.83405670837316));
#39642=CARTESIAN_POINT('Ctrl Pts',(-4.38985170429192,-1.06847604194588,
5.86084339263343));
#39643=CARTESIAN_POINT('Ctrl Pts',(-4.29008041270584,-0.794772684001074,
5.91965303920681));
#39644=CARTESIAN_POINT('Ctrl Pts',(-4.23877689554809,-0.636309800095377,
5.95419134348704));
#39645=CARTESIAN_POINT('Ctrl Pts',(-4.17817840066915,-0.31943490727725,
6.00392523034156));
#39646=CARTESIAN_POINT('Ctrl Pts',(-4.15837916125798,-0.158333333333377,
6.02535045698314));
#39647=CARTESIAN_POINT('Ctrl Pts',(-4.16489595666514,0.158333333333379,
6.04806704337612));
#39648=CARTESIAN_POINT('Ctrl Pts',(-4.19097706891447,0.319434907277256,
6.04857621955896));
#39649=CARTESIAN_POINT('Ctrl Pts',(-4.26532832717098,0.636309800095385,
6.04670763514851));
#39650=CARTESIAN_POINT('Ctrl Pts',(-4.32412599322238,0.794772684001067,
6.03822236852455));
#39651=CARTESIAN_POINT('Ctrl Pts',(-4.43670851265054,1.06847604194549,6.02385186523617));
#39652=CARTESIAN_POINT('Ctrl Pts',(-4.49147101150986,1.18514270861226,6.01629863735659));
#39653=CARTESIAN_POINT('Ctrl Pts',(-4.55226320816154,1.30000000000058,6.00741263999135));
#39654=CARTESIAN_POINT('Ctrl Pts',(-4.46442169461097,-1.30000000000149,
5.80418837180094));
#39655=CARTESIAN_POINT('Ctrl Pts',(-4.40347215655026,-1.18514270861283,
5.83279771823915));
#39656=CARTESIAN_POINT('Ctrl Pts',(-4.35013355197629,-1.0684760419457,5.86021766874858));
#39657=CARTESIAN_POINT('Ctrl Pts',(-4.24449348397574,-0.794772684000947,
5.92081549723424));
#39658=CARTESIAN_POINT('Ctrl Pts',(-4.19475469538735,-0.636309800095274,
5.95776264589176));
#39659=CARTESIAN_POINT('Ctrl Pts',(-4.13407346496599,-0.319434907277198,
6.00817306579063));
#39660=CARTESIAN_POINT('Ctrl Pts',(-4.11588361177796,-0.158333333333352,
6.02827899548824));
#39661=CARTESIAN_POINT('Ctrl Pts',(-4.12214305822338,0.158333333333354,
6.04987688497436));
#39662=CARTESIAN_POINT('Ctrl Pts',(-4.14622564528697,0.319434907277206,
6.05018319061237));
#39663=CARTESIAN_POINT('Ctrl Pts',(-4.22040388452318,0.636309800095284,
6.0461812086317));
#39664=CARTESIAN_POINT('Ctrl Pts',(-4.27768379963794,0.794772684000937,
6.03476888272922));
#39665=CARTESIAN_POINT('Ctrl Pts',(-4.39634270097453,1.06847604194531,6.0192033469583));
#39666=CARTESIAN_POINT('Ctrl Pts',(-4.45538559999196,1.18514270861207,6.01164888581944));
#39667=CARTESIAN_POINT('Ctrl Pts',(-4.52210835638382,1.30000000000038,6.003277707217));
#39668=CARTESIAN_POINT('Ctrl Pts',(-4.43460530968309,-1.30000000000149,
5.80256316172534));
#39669=CARTESIAN_POINT('Ctrl Pts',(-4.36805904278203,-1.18514270861283,
5.8318690467023));
#39670=CARTESIAN_POINT('Ctrl Pts',(-4.31069443391872,-1.0684760419457,5.86012150415013));
#39671=CARTESIAN_POINT('Ctrl Pts',(-4.19938217854564,-0.794772684000941,
5.92295670440955));
#39672=CARTESIAN_POINT('Ctrl Pts',(-4.15120156772676,-0.63630980009527,
5.96218462274267));
#39673=CARTESIAN_POINT('Ctrl Pts',(-4.09071095778597,-0.319434907277196,
6.01447543869057));
#39674=CARTESIAN_POINT('Ctrl Pts',(-4.07454410674807,-0.15833333333335,
6.03532811783394));
#39675=CARTESIAN_POINT('Ctrl Pts',(-4.08057825519952,0.158333333333352,
6.0560835465697));
#39676=CARTESIAN_POINT('Ctrl Pts',(-4.10229506552196,0.319434907277203,
6.05445287108395));
#39677=CARTESIAN_POINT('Ctrl Pts',(-4.17606305985547,0.636309800095278,
6.04756284550421));
#39678=CARTESIAN_POINT('Ctrl Pts',(-4.23185985371759,0.794772684000934,
6.03393132239186));
#39679=CARTESIAN_POINT('Ctrl Pts',(-4.35633249000634,1.06847604194531,6.01618889847783));
#39680=CARTESIAN_POINT('Ctrl Pts',(-4.41950097569454,1.18514270861206,6.00792908300874));
#39681=CARTESIAN_POINT('Ctrl Pts',(-4.49195835498728,1.30000000000037,5.99908948996133));
#39682=CARTESIAN_POINT('Ctrl Pts',(-4.41385708995499,-1.30000000000142,
5.80251373423967));
#39683=CARTESIAN_POINT('Ctrl Pts',(-4.34325629992991,-1.18514270861277,
5.83235874410777));
#39684=CARTESIAN_POINT('Ctrl Pts',(-4.28299099688123,-1.06847604194565,
5.86130912435199));
#39685=CARTESIAN_POINT('Ctrl Pts',(-4.16764313332899,-0.794772684000904,
5.9261235208185));
#39686=CARTESIAN_POINT('Ctrl Pts',(-4.12092017336752,-0.63630980009524,
5.96846324925116));
#39687=CARTESIAN_POINT('Ctrl Pts',(-4.06024674814721,-0.319434907277181,
6.02065767248337));
#39688=CARTESIAN_POINT('Ctrl Pts',(-4.04465236031601,-0.158333333333343,
6.03798273283064));
#39689=CARTESIAN_POINT('Ctrl Pts',(-4.05038226546884,0.158333333333345,
6.05754542838412));
#39690=CARTESIAN_POINT('Ctrl Pts',(-4.07104113219228,0.319434907277188,
6.05764658780402));
#39691=CARTESIAN_POINT('Ctrl Pts',(-4.14474138702257,0.636309800095249,
6.04965181419876));
#39692=CARTESIAN_POINT('Ctrl Pts',(-4.19931517653417,0.794772684000895,
6.03347707935452));
#39693=CARTESIAN_POINT('Ctrl Pts',(-4.32799069168609,1.06847604194526,6.01402650668398));
#39694=CARTESIAN_POINT('Ctrl Pts',(-4.39414832245677,1.185142708612,6.00525411630719));
#39695=CARTESIAN_POINT('Ctrl Pts',(-4.47076472138661,1.3000000000003,5.99612876774794));
#39696=CARTESIAN_POINT('Ctrl Pts',(-4.39907707321258,-1.3000000000014,5.80214342814134));
#39697=CARTESIAN_POINT('Ctrl Pts',(-4.32596135091668,-1.18514270861275,
5.83318873155966));
#39698=CARTESIAN_POINT('Ctrl Pts',(-4.26382414376078,-1.06847604194563,
5.86283274193729));
#39699=CARTESIAN_POINT('Ctrl Pts',(-4.14563733094301,-0.794772684000892,
5.9280790689217));
#39700=CARTESIAN_POINT('Ctrl Pts',(-4.09911568145707,-0.636309800095228,
5.96873290910518));
#39701=CARTESIAN_POINT('Ctrl Pts',(-4.03822628354595,-0.319434907277174,
6.02007589595103));
#39702=CARTESIAN_POINT('Ctrl Pts',(-4.02347322566431,-0.15833333333334,
6.03681301517062));
#39703=CARTESIAN_POINT('Ctrl Pts',(-4.02930776445731,0.158333333333342,
6.05694737783173));
#39704=CARTESIAN_POINT('Ctrl Pts',(-4.04940391664942,0.319434907277182,
6.05905497389403));
#39705=CARTESIAN_POINT('Ctrl Pts',(-4.12317888700689,0.636309800095237,
6.05135115292042));
#39706=CARTESIAN_POINT('Ctrl Pts',(-4.17687402913407,0.794772684000879,
6.03377636155464));
#39707=CARTESIAN_POINT('Ctrl Pts',(-4.30833967460458,1.06847604194524,6.01351250464339));
#39708=CARTESIAN_POINT('Ctrl Pts',(-4.37648281330616,1.18514270861198,6.00445204719333));
#39709=CARTESIAN_POINT('Ctrl Pts',(-4.45586248406738,1.30000000000029,5.99510260510017));
#39710=CARTESIAN_POINT('Ctrl Pts',(-4.38139208292461,-1.30000000000138,
5.80261733027026));
#39711=CARTESIAN_POINT('Ctrl Pts',(-4.3048977109199,-1.18514270861273,5.83519453478588));
#39712=CARTESIAN_POINT('Ctrl Pts',(-4.24018476782454,-1.06847604194561,
5.86555166982907));
#39713=CARTESIAN_POINT('Ctrl Pts',(-4.11790238114195,-0.794772684000877,
5.93055392009809));
#39714=CARTESIAN_POINT('Ctrl Pts',(-4.0711888923754,-0.636309800095217,
5.96776653449272));
#39715=CARTESIAN_POINT('Ctrl Pts',(-4.00967332532343,-0.319434907277169,
6.017042557179));
#39716=CARTESIAN_POINT('Ctrl Pts',(-3.99607174541107,-0.158333333333337,
6.03316436429983));
#39717=CARTESIAN_POINT('Ctrl Pts',(-4.00186520345239,0.158333333333339,
6.05321439144484));
#39718=CARTESIAN_POINT('Ctrl Pts',(-4.02082482242209,0.319434907277176,
6.05620237179938));
#39719=CARTESIAN_POINT('Ctrl Pts',(-4.0950281634806,0.636309800095226,6.04968201126514));
#39720=CARTESIAN_POINT('Ctrl Pts',(-4.14852774059524,0.794772684000865,
6.03365040706671));
#39721=CARTESIAN_POINT('Ctrl Pts',(-4.28409830645338,1.06847604194522,6.01340395768109));
#39722=CARTESIAN_POINT('Ctrl Pts',(-4.3549180638185,1.18514270861197,6.00393822894615));
#39723=CARTESIAN_POINT('Ctrl Pts',(-4.43787410397329,1.30000000000027,5.99377070921041));
#39724=CARTESIAN_POINT('Ctrl Pts',(-4.36932387841515,-1.30000000000134,
5.80281598958122));
#39725=CARTESIAN_POINT('Ctrl Pts',(-4.29080148664791,-1.18514270861269,
5.83777836890749));
#39726=CARTESIAN_POINT('Ctrl Pts',(-4.22452488361665,-1.06847604194558,
5.86911453240873));
#39727=CARTESIAN_POINT('Ctrl Pts',(-4.09970289376746,-0.794772684000851,
5.93313005489667));
#39728=CARTESIAN_POINT('Ctrl Pts',(-4.05265002448005,-0.636309800095197,
5.96374672476965));
#39729=CARTESIAN_POINT('Ctrl Pts',(-3.99084012998884,-0.319434907277159,
6.00955609589528));
#39730=CARTESIAN_POINT('Ctrl Pts',(-3.97832338063956,-0.158333333333332,
6.02572522045514));
#39731=CARTESIAN_POINT('Ctrl Pts',(-3.98412215794982,0.158333333333334,
6.04561777586163));
#39732=CARTESIAN_POINT('Ctrl Pts',(-4.00209599199945,0.319434907277167,
6.04853496477295));
#39733=CARTESIAN_POINT('Ctrl Pts',(-4.07641358158954,0.636309800095206,
6.04488755346973));
#39734=CARTESIAN_POINT('Ctrl Pts',(-4.12975510290133,0.79477268400084,6.03438726539486));
#39735=CARTESIAN_POINT('Ctrl Pts',(-4.26788601364085,1.06847604194518,6.01517679411596));
#39736=CARTESIAN_POINT('Ctrl Pts',(-4.34039737044277,1.18514270861192,6.00502961961175));
#39737=CARTESIAN_POINT('Ctrl Pts',(-4.42562833104214,1.30000000000022,5.99305077180184));
#39738=CARTESIAN_POINT('Ctrl Pts',(-4.36108289177568,-1.30000000000134,
5.80034987084412));
#39739=CARTESIAN_POINT('Ctrl Pts',(-4.28280795672196,-1.18514270861269,
5.83535608437193));
#39740=CARTESIAN_POINT('Ctrl Pts',(-4.21670728203319,-1.06847604194558,
5.86639564184631));
#39741=CARTESIAN_POINT('Ctrl Pts',(-4.09212647700321,-0.794772684000851,
5.92893946004396));
#39742=CARTESIAN_POINT('Ctrl Pts',(-4.04497787349015,-0.636309800095197,
5.95699216849829));
#39743=CARTESIAN_POINT('Ctrl Pts',(-3.98316982931346,-0.319434907277159,
6.00111495923036));
#39744=CARTESIAN_POINT('Ctrl Pts',(-3.97060749458543,-0.158333333333332,
6.01730981540119));
#39745=CARTESIAN_POINT('Ctrl Pts',(-3.97642822268415,0.158333333333334,
6.03696656310354));
#39746=CARTESIAN_POINT('Ctrl Pts',(-3.99446677770813,0.319434907277167,
6.03934216248958));
#39747=CARTESIAN_POINT('Ctrl Pts',(-4.06883296350448,0.636309800095206,
6.03747145037915));
#39748=CARTESIAN_POINT('Ctrl Pts',(-4.12234304385768,0.79477268400084,6.03061645411867));
#39749=CARTESIAN_POINT('Ctrl Pts',(-4.26021093575302,1.06847604194518,6.01272564041898));
#39750=CARTESIAN_POINT('Ctrl Pts',(-4.33251297633884,1.18514270861192,6.00255688732873));
#39751=CARTESIAN_POINT('Ctrl Pts',(-4.41743915561784,1.30000000000022,5.98996365147884));
#39752=CARTESIAN_POINT('Ctrl Pts',(-4.36108289177477,-1.3,5.80034987084453));
#39753=CARTESIAN_POINT('Ctrl Pts',(-4.28280795672145,-1.18514270861178,
5.83535608437217));
#39754=CARTESIAN_POINT('Ctrl Pts',(-4.21670728203298,-1.06847604194512,
5.86639564184641));
#39755=CARTESIAN_POINT('Ctrl Pts',(-4.09212647700321,-0.794772684000851,
5.92893946004396));
#39756=CARTESIAN_POINT('Ctrl Pts',(-4.04497787349015,-0.636309800095197,
5.95699216849829));
#39757=CARTESIAN_POINT('Ctrl Pts',(-3.98316982931346,-0.319434907277159,
6.00111495923036));
#39758=CARTESIAN_POINT('Ctrl Pts',(-3.97060749458543,-0.158333333333332,
6.01730981540119));
#39759=CARTESIAN_POINT('Ctrl Pts',(-3.97642822268415,0.158333333333334,
6.03696656310354));
#39760=CARTESIAN_POINT('Ctrl Pts',(-3.99446677770813,0.319434907277167,
6.03934216248958));
#39761=CARTESIAN_POINT('Ctrl Pts',(-4.06883296350448,0.636309800095206,
6.03747145037915));
#39762=CARTESIAN_POINT('Ctrl Pts',(-4.12234304385768,0.79477268400084,6.03061645411867));
#39763=CARTESIAN_POINT('Ctrl Pts',(-4.26021093575299,1.06847604194511,6.01272564041899));
#39764=CARTESIAN_POINT('Ctrl Pts',(-4.33251297633875,1.18514270861178,6.00255688732874));
#39765=CARTESIAN_POINT('Ctrl Pts',(-4.41743915561768,1.3,5.98996365147886));
#39766=CARTESIAN_POINT('',(-4.76943094974079,-1.2,5.8752251452965));
#39767=CARTESIAN_POINT('Ctrl Pts',(-4.76943094974079,-1.2,5.8752251452965));
#39768=CARTESIAN_POINT('Ctrl Pts',(-4.75137040040528,-1.21532879594667,
5.8674796759455));
#39769=CARTESIAN_POINT('Ctrl Pts',(-4.75128192428144,-1.21526382380562,
5.86695113090664));
#39770=CARTESIAN_POINT('Ctrl Pts',(-4.72841491494507,-1.23443202165904,
5.85651346558973));
#39771=CARTESIAN_POINT('Ctrl Pts',(-4.72629960582589,-1.2362463555996,5.85568195490476));
#39772=CARTESIAN_POINT('Ctrl Pts',(-4.69026521558868,-1.26666727514779,
5.84039241832176));
#39773=CARTESIAN_POINT('Ctrl Pts',(-4.67050837960332,-1.28326560327169,
5.83192379066369));
#39774=CARTESIAN_POINT('Ctrl Pts',(-4.65068316839847,-1.30000000000257,
5.82390186863356));
#39775=CARTESIAN_POINT('',(-4.80892752421831,-0.653834841417905,6.02666455497168));
#39776=CARTESIAN_POINT('Ctrl Pts',(-4.80892752424277,-0.653834841417227,
6.02666455496296));
#39777=CARTESIAN_POINT('Ctrl Pts',(-4.80506824066303,-0.718001778396551,
6.01084724107461));
#39778=CARTESIAN_POINT('Ctrl Pts',(-4.80187412133315,-0.763814897456566,
5.99800871203435));
#39779=CARTESIAN_POINT('Ctrl Pts',(-4.78912428622677,-0.949547840785904,
5.9477928208045));
#39780=CARTESIAN_POINT('Ctrl Pts',(-4.78201437664528,-1.04870126019181,
5.92052777579179));
#39781=CARTESIAN_POINT('Ctrl Pts',(-4.76943094974079,-1.2,5.8752251452965));
#39782=CARTESIAN_POINT('',(-4.84008270153004,0.653834841531101,6.16264786964614));
#39783=CARTESIAN_POINT('Ctrl Pts',(-4.84008270153004,0.653834841531101,
6.16264786964614));
#39784=CARTESIAN_POINT('Ctrl Pts',(-4.79944689285444,0.575793690744437,
6.15340775242001));
#39785=CARTESIAN_POINT('Ctrl Pts',(-4.76554165986554,0.493915978123552,
6.14498973164795));
#39786=CARTESIAN_POINT('Ctrl Pts',(-4.71701543835946,0.338192716619548,
6.13032379860722));
#39787=CARTESIAN_POINT('Ctrl Pts',(-4.70027540041615,0.265706975690616,
6.12394954385036));
#39788=CARTESIAN_POINT('Ctrl Pts',(-4.679340251876,0.129738926799289,6.11140069271612));
#39789=CARTESIAN_POINT('Ctrl Pts',(-4.67367418869134,0.0666398175577108,
6.10535820904037));
#39790=CARTESIAN_POINT('Ctrl Pts',(-4.67033333649289,-0.0595502776848976,
6.09244197012475));
#39791=CARTESIAN_POINT('Ctrl Pts',(-4.67261687834793,-0.122795537269838,
6.08547477710846));
#39792=CARTESIAN_POINT('Ctrl Pts',(-4.68654559054128,-0.260150036719889,
6.07010358967871));
#39793=CARTESIAN_POINT('Ctrl Pts',(-4.69982117916003,-0.333952578847895,
6.06166611745586));
#39794=CARTESIAN_POINT('Ctrl Pts',(-4.7411101764999,-0.491147154103011,
6.0442087836093));
#39795=CARTESIAN_POINT('Ctrl Pts',(-4.77132361579784,-0.574255930628569,
6.03514257932434));
#39796=CARTESIAN_POINT('Ctrl Pts',(-4.80892752418791,-0.653834841429502,
6.02666455494571));
#39797=CARTESIAN_POINT('',(-4.82444443480448,1.2,6.09219320480325));
#39798=CARTESIAN_POINT('Ctrl Pts',(-4.82444443480448,1.2,6.09219320480325));
#39799=CARTESIAN_POINT('Ctrl Pts',(-4.82723947618274,1.13403856392639,6.10436547336207));
#39800=CARTESIAN_POINT('Ctrl Pts',(-4.83083759668361,1.03830672751198,6.1202516992187));
#39801=CARTESIAN_POINT('Ctrl Pts',(-4.83765957916731,0.795125399809678,
6.15132335450788));
#39802=CARTESIAN_POINT('Ctrl Pts',(-4.83870912604018,0.741480188480013,
6.15623903433055));
#39803=CARTESIAN_POINT('Ctrl Pts',(-4.84008270153004,0.653834841531101,
6.16264786964614));
#39804=CARTESIAN_POINT('Ctrl Pts',(-4.70979325221221,1.30000000000036,6.04226621306413));
#39805=CARTESIAN_POINT('Ctrl Pts',(-4.72229378593043,1.28915014241713,6.04766738572323));
#39806=CARTESIAN_POINT('Ctrl Pts',(-4.72828552194237,1.28375313994558,6.04947303494543));
#39807=CARTESIAN_POINT('Ctrl Pts',(-4.75229651621339,1.26293974657568,6.06020423652264));
#39808=CARTESIAN_POINT('Ctrl Pts',(-4.75719339679975,1.25866690039675,6.06233008665453));
#39809=CARTESIAN_POINT('Ctrl Pts',(-4.77865120550695,1.23990130702929,6.07145421674264));
#39810=CARTESIAN_POINT('Ctrl Pts',(-4.80287991746654,1.21864618379946,6.08159730856588));
#39811=CARTESIAN_POINT('Ctrl Pts',(-4.82444443480448,1.2,6.09219320480325));
#39812=CARTESIAN_POINT('Ctrl Pts',(-4.36108289177477,-1.3,5.80034987084453));
#39813=CARTESIAN_POINT('Ctrl Pts',(-4.28280795672145,-1.18514270861178,
5.83535608437217));
#39814=CARTESIAN_POINT('Ctrl Pts',(-4.21670728203298,-1.06847604194512,
5.86639564184641));
#39815=CARTESIAN_POINT('Ctrl Pts',(-4.09212647700321,-0.794772684000851,
5.92893946004396));
#39816=CARTESIAN_POINT('Ctrl Pts',(-4.04497787349015,-0.636309800095197,
5.95699216849828));
#39817=CARTESIAN_POINT('Ctrl Pts',(-3.98316982931346,-0.319434907277159,
6.00111495923036));
#39818=CARTESIAN_POINT('Ctrl Pts',(-3.97060749458542,-0.158333333333333,
6.01730981540119));
#39819=CARTESIAN_POINT('Ctrl Pts',(-3.97642822268415,0.158333333333334,
6.03696656310354));
#39820=CARTESIAN_POINT('Ctrl Pts',(-3.99446677770813,0.319434907277167,
6.03934216248957));
#39821=CARTESIAN_POINT('Ctrl Pts',(-4.06883296350447,0.636309800095206,
6.03747145037914));
#39822=CARTESIAN_POINT('Ctrl Pts',(-4.12234304385768,0.79477268400084,6.03061645411867));
#39823=CARTESIAN_POINT('Ctrl Pts',(-4.26021093575298,1.06847604194511,6.01272564041899));
#39824=CARTESIAN_POINT('Ctrl Pts',(-4.33251297633875,1.18514270861178,6.00255688732874));
#39825=CARTESIAN_POINT('Ctrl Pts',(-4.41743915561768,1.3,5.98996365147886));
#39826=CARTESIAN_POINT('Ctrl Pts',(-4.33573021748671,-1.3,5.72771137429423));
#39827=CARTESIAN_POINT('Ctrl Pts',(-4.25817731391276,-1.18514270861178,
5.76429225461164));
#39828=CARTESIAN_POINT('Ctrl Pts',(-4.19261998989961,-1.06847604194512,
5.79640908596292));
#39829=CARTESIAN_POINT('Ctrl Pts',(-4.06888164522439,-0.794772684000851,
5.86029254519278));
#39830=CARTESIAN_POINT('Ctrl Pts',(-4.02167596618816,-0.636309800095197,
5.88762989336549));
#39831=CARTESIAN_POINT('Ctrl Pts',(-3.96004957503507,-0.319434907277159,
5.93111105698402));
#39832=CARTESIAN_POINT('Ctrl Pts',(-3.94727563345509,-0.158333333333333,
5.9460825267282));
#39833=CARTESIAN_POINT('Ctrl Pts',(-3.95343774500623,0.158333333333334,
5.96562835222289));
#39834=CARTESIAN_POINT('Ctrl Pts',(-3.97202419499028,0.319434907277167,
5.96911807140563));
#39835=CARTESIAN_POINT('Ctrl Pts',(-4.04691448012462,0.636309800095206,
5.96765967356581));
#39836=CARTESIAN_POINT('Ctrl Pts',(-4.10079886363323,0.79477268400084,5.96141696408104));
#39837=CARTESIAN_POINT('Ctrl Pts',(-4.2385608990303,1.06847604194511,5.94194717224782));
#39838=CARTESIAN_POINT('Ctrl Pts',(-4.3106693138487,1.18514270861178,5.93058751276968));
#39839=CARTESIAN_POINT('Ctrl Pts',(-4.39525406294861,1.3,5.91629594527112));
#39840=CARTESIAN_POINT('Ctrl Pts',(-4.31037754319864,-1.3,5.65507287774392));
#39841=CARTESIAN_POINT('Ctrl Pts',(-4.23354667110408,-1.18514270861178,
5.69322842485112));
#39842=CARTESIAN_POINT('Ctrl Pts',(-4.16853269776624,-1.06847604194512,
5.72642253007944));
#39843=CARTESIAN_POINT('Ctrl Pts',(-4.04563681344557,-0.794772684000851,
5.79164563034159));
#39844=CARTESIAN_POINT('Ctrl Pts',(-3.99837405888618,-0.636309800095197,
5.81826761823271));
#39845=CARTESIAN_POINT('Ctrl Pts',(-3.93692932075669,-0.319434907277159,
5.86110715473768));
#39846=CARTESIAN_POINT('Ctrl Pts',(-3.92394377232475,-0.158333333333333,
5.87485523805521));
#39847=CARTESIAN_POINT('Ctrl Pts',(-3.9304472673283,0.158333333333334,5.89429014134224));
#39848=CARTESIAN_POINT('Ctrl Pts',(-3.94958161227244,0.319434907277167,
5.89889398032169));
#39849=CARTESIAN_POINT('Ctrl Pts',(-4.02499599674477,0.636309800095206,
5.89784789675249));
#39850=CARTESIAN_POINT('Ctrl Pts',(-4.07925468340879,0.79477268400084,5.89221747404342));
#39851=CARTESIAN_POINT('Ctrl Pts',(-4.21691086230761,1.06847604194511,5.87116870407665));
#39852=CARTESIAN_POINT('Ctrl Pts',(-4.28882565135864,1.18514270861178,5.85861813821062));
#39853=CARTESIAN_POINT('Ctrl Pts',(-4.37306897027954,1.3,5.84262823906338));
#39854=CARTESIAN_POINT('Ctrl Pts',(-4.28502486891058,-1.3,5.58243438119362));
#39855=CARTESIAN_POINT('Ctrl Pts',(-4.20891602829539,-1.18514270861178,
5.62216459509059));
#39856=CARTESIAN_POINT('Ctrl Pts',(-4.14444540563287,-1.06847604194512,
5.65643597419595));
#39857=CARTESIAN_POINT('Ctrl Pts',(-4.02239198166675,-0.794772684000851,
5.72299871549041));
#39858=CARTESIAN_POINT('Ctrl Pts',(-3.9750721515842,-0.636309800095197,
5.74890534309992));
#39859=CARTESIAN_POINT('Ctrl Pts',(-3.91380906647831,-0.319434907277159,
5.79110325249133));
#39860=CARTESIAN_POINT('Ctrl Pts',(-3.90061191119441,-0.158333333333333,
5.80362794938222));
#39861=CARTESIAN_POINT('Ctrl Pts',(-3.90745678965038,0.158333333333334,
5.8229519304616));
#39862=CARTESIAN_POINT('Ctrl Pts',(-3.9271390295546,0.319434907277167,5.82866988923775));
#39863=CARTESIAN_POINT('Ctrl Pts',(-4.00307751336492,0.636309800095206,
5.82803611993916));
#39864=CARTESIAN_POINT('Ctrl Pts',(-4.05771050318434,0.79477268400084,5.82301798400579));
#39865=CARTESIAN_POINT('Ctrl Pts',(-4.19526082558492,1.06847604194511,5.80039023590548));
#39866=CARTESIAN_POINT('Ctrl Pts',(-4.26698198886859,1.18514270861178,5.78664876365156));
#39867=CARTESIAN_POINT('Ctrl Pts',(-4.35088387761047,1.3,5.76896053285564));
#39868=CARTESIAN_POINT('Ctrl Pts',(-4.28502486891058,-1.3,5.58243438119362));
#39869=CARTESIAN_POINT('Ctrl Pts',(-4.20891602829539,-1.18514270861178,
5.62216459509059));
#39870=CARTESIAN_POINT('Ctrl Pts',(-4.14444540563287,-1.06847604194512,
5.65643597419595));
#39871=CARTESIAN_POINT('Ctrl Pts',(-4.02239198166675,-0.794772684000851,
5.72299871549041));
#39872=CARTESIAN_POINT('Ctrl Pts',(-3.9750721515842,-0.636309800095197,
5.74890534309992));
#39873=CARTESIAN_POINT('Ctrl Pts',(-3.91380906647831,-0.319434907277159,
5.79110325249133));
#39874=CARTESIAN_POINT('Ctrl Pts',(-3.90061191119441,-0.158333333333332,
5.80362794938222));
#39875=CARTESIAN_POINT('Ctrl Pts',(-3.90745678965039,0.158333333333334,
5.8229519304616));
#39876=CARTESIAN_POINT('Ctrl Pts',(-3.9271390295546,0.319434907277167,5.82866988923776));
#39877=CARTESIAN_POINT('Ctrl Pts',(-4.00307751336492,0.636309800095206,
5.82803611993916));
#39878=CARTESIAN_POINT('Ctrl Pts',(-4.05771050318434,0.79477268400084,5.82301798400579));
#39879=CARTESIAN_POINT('Ctrl Pts',(-4.19526082558492,1.06847604194511,5.80039023590548));
#39880=CARTESIAN_POINT('Ctrl Pts',(-4.26698198886859,1.18514270861178,5.78664876365156));
#39881=CARTESIAN_POINT('Ctrl Pts',(-4.35088387761047,1.3,5.76896053285564));
#39882=CARTESIAN_POINT('Ctrl Pts',(-4.28502486891571,-1.30000000000774,
5.58243438119094));
#39883=CARTESIAN_POINT('Ctrl Pts',(-4.20891602829829,-1.18514270861703,
5.62216459508905));
#39884=CARTESIAN_POINT('Ctrl Pts',(-4.14444540563406,-1.06847604194778,
5.6564359741953));
#39885=CARTESIAN_POINT('Ctrl Pts',(-4.02239198166675,-0.794772684000851,
5.72299871549041));
#39886=CARTESIAN_POINT('Ctrl Pts',(-3.9750721515842,-0.636309800095197,
5.74890534309992));
#39887=CARTESIAN_POINT('Ctrl Pts',(-3.91380906647831,-0.319434907277159,
5.79110325249133));
#39888=CARTESIAN_POINT('Ctrl Pts',(-3.90061191119441,-0.158333333333332,
5.80362794938222));
#39889=CARTESIAN_POINT('Ctrl Pts',(-3.90745678965039,0.158333333333335,
5.8229519304616));
#39890=CARTESIAN_POINT('Ctrl Pts',(-3.9271390295546,0.319434907277167,5.82866988923776));
#39891=CARTESIAN_POINT('Ctrl Pts',(-4.00307751336492,0.636309800095206,
5.82803611993916));
#39892=CARTESIAN_POINT('Ctrl Pts',(-4.05771050318434,0.79477268400084,5.8230179840058));
#39893=CARTESIAN_POINT('Ctrl Pts',(-4.19526082558604,1.06847604194732,5.8003902359053));
#39894=CARTESIAN_POINT('Ctrl Pts',(-4.26698198887127,1.18514270861614,5.78664876365104));
#39895=CARTESIAN_POINT('Ctrl Pts',(-4.35088387761518,1.30000000000644,5.76896053285465));
#39896=CARTESIAN_POINT('Ctrl Pts',(-4.28983548714971,-1.30000000000774,
5.57512337186273));
#39897=CARTESIAN_POINT('Ctrl Pts',(-4.21384120150069,-1.18514270861703,
5.61552978208877));
#39898=CARTESIAN_POINT('Ctrl Pts',(-4.14921392204009,-1.06847604194778,
5.64994165162069));
#39899=CARTESIAN_POINT('Ctrl Pts',(-4.0261720361017,-0.794772684000851,
5.7155913661023));
#39900=CARTESIAN_POINT('Ctrl Pts',(-3.97684592438828,-0.636309800095197,
5.73844981416284));
#39901=CARTESIAN_POINT('Ctrl Pts',(-3.91457783683304,-0.319434907277159,
5.77918177958783));
#39902=CARTESIAN_POINT('Ctrl Pts',(-3.9017513801954,-0.158333333333332,
5.79210658959415));
#39903=CARTESIAN_POINT('Ctrl Pts',(-3.90875262150678,0.158333333333335,
5.81160844076292));
#39904=CARTESIAN_POINT('Ctrl Pts',(-3.9283828574657,0.319434907277167,5.81733237662104));
#39905=CARTESIAN_POINT('Ctrl Pts',(-4.00531418532216,0.636309800095206,
5.81806199192622));
#39906=CARTESIAN_POINT('Ctrl Pts',(-4.06137678322638,0.79477268400084,5.81517441552251));
#39907=CARTESIAN_POINT('Ctrl Pts',(-4.19998727432042,1.06847604194732,5.79359553632442));
#39908=CARTESIAN_POINT('Ctrl Pts',(-4.27202510727,1.18514270861614,5.77999061530212));
#39909=CARTESIAN_POINT('Ctrl Pts',(-4.35610142759883,1.30000000000644,5.76212147048619));
#39910=CARTESIAN_POINT('Ctrl Pts',(-4.29926460392529,-1.3000000000078,5.56730754667784));
#39911=CARTESIAN_POINT('Ctrl Pts',(-4.22610897742813,-1.18514270861708,
5.60781633231694));
#39912=CARTESIAN_POINT('Ctrl Pts',(-4.1632069654871,-1.06847604194782,5.64177322539493));
#39913=CARTESIAN_POINT('Ctrl Pts',(-4.04157863525366,-0.794772684000886,
5.70508425893971));
#39914=CARTESIAN_POINT('Ctrl Pts',(-3.98891499615366,-0.636309800095225,
5.72360628567257));
#39915=CARTESIAN_POINT('Ctrl Pts',(-3.92508927153551,-0.319434907277173,
5.76200735853348));
#39916=CARTESIAN_POINT('Ctrl Pts',(-3.91155422483044,-0.158333333333339,
5.77560738379245));
#39917=CARTESIAN_POINT('Ctrl Pts',(-3.91868087788676,0.158333333333341,
5.79530051439071));
#39918=CARTESIAN_POINT('Ctrl Pts',(-3.9391737882875,0.31943490727718,5.80045397900698));
#39919=CARTESIAN_POINT('Ctrl Pts',(-4.01785980381973,0.636309800095233,
5.80408037571868));
#39920=CARTESIAN_POINT('Ctrl Pts',(-4.07738162668686,0.794772684000876,
5.80643110136374));
#39921=CARTESIAN_POINT('Ctrl Pts',(-4.21455464773777,1.06847604194737,5.78710873781506));
#39922=CARTESIAN_POINT('Ctrl Pts',(-4.28480848471052,1.18514270861619,5.77367406491117));
#39923=CARTESIAN_POINT('Ctrl Pts',(-4.36593904060384,1.3000000000065,5.75516865431955));
#39924=CARTESIAN_POINT('Ctrl Pts',(-4.31087898980036,-1.3000000000078,5.55775119234527));
#39925=CARTESIAN_POINT('Ctrl Pts',(-4.24062896799711,-1.18514270861708,
5.59707972499315));
#39926=CARTESIAN_POINT('Ctrl Pts',(-4.17978777933664,-1.06847604194783,
5.6299959312519));
#39927=CARTESIAN_POINT('Ctrl Pts',(-4.0609687490848,-0.794772684000887,
5.69122519583298));
#39928=CARTESIAN_POINT('Ctrl Pts',(-4.00733049135218,-0.636309800095225,
5.70868832752417));
#39929=CARTESIAN_POINT('Ctrl Pts',(-3.94313274773527,-0.319434907277173,
5.74594287877534));
#39930=CARTESIAN_POINT('Ctrl Pts',(-3.92831311803112,-0.158333333333339,
5.75941308314454));
#39931=CARTESIAN_POINT('Ctrl Pts',(-3.93542313374035,0.158333333333342,
5.77910883389326));
#39932=CARTESIAN_POINT('Ctrl Pts',(-3.95702358944834,0.319434907277181,
5.78405811617581));
#39933=CARTESIAN_POINT('Ctrl Pts',(-4.0363744588543,0.636309800095234,5.78952204913013));
#39934=CARTESIAN_POINT('Ctrl Pts',(-4.09763070495285,0.794772684000876,
5.79465216253709));
#39935=CARTESIAN_POINT('Ctrl Pts',(-4.23209270204518,1.06847604194737,5.77753302310594));
#39936=CARTESIAN_POINT('Ctrl Pts',(-4.30017341612242,1.18514270861619,5.76481597001355));
#39937=CARTESIAN_POINT('Ctrl Pts',(-4.37813122804306,1.3000000000065,5.74679210496196));
#39938=CARTESIAN_POINT('Ctrl Pts',(-4.31756355120264,-1.30000000000782,
5.55178320730319));
#39939=CARTESIAN_POINT('Ctrl Pts',(-4.24867237672523,-1.1851427086171,5.59025076843429));
#39940=CARTESIAN_POINT('Ctrl Pts',(-4.18884808425587,-1.06847604194784,
5.62257789921357));
#39941=CARTESIAN_POINT('Ctrl Pts',(-4.07158831210657,-0.794772684000899,
5.68307441583173));
#39942=CARTESIAN_POINT('Ctrl Pts',(-4.01794799809661,-0.636309800095235,
5.70116577658724));
#39943=CARTESIAN_POINT('Ctrl Pts',(-3.95376926507575,-0.319434907277177,
5.7383041614915));
#39944=CARTESIAN_POINT('Ctrl Pts',(-3.93818730491617,-0.158333333333341,
5.75138323538562));
#39945=CARTESIAN_POINT('Ctrl Pts',(-3.94525424323687,0.158333333333344,
5.77101756308156));
#39946=CARTESIAN_POINT('Ctrl Pts',(-3.96745835523679,0.319434907277185,
5.77606932698987));
#39947=CARTESIAN_POINT('Ctrl Pts',(-4.04693793081532,0.636309800095243,
5.78198715454197));
#39948=CARTESIAN_POINT('Ctrl Pts',(-4.1086577796612,0.794772684000887,5.78746954738944));
#39949=CARTESIAN_POINT('Ctrl Pts',(-4.24166935314431,1.06847604194739,5.77125294812262));
#39950=CARTESIAN_POINT('Ctrl Pts',(-4.30870002787006,1.18514270861621,5.75901208534449));
#39951=CARTESIAN_POINT('Ctrl Pts',(-4.38518559572466,1.30000000000652,5.74154992472669));
#39952=CARTESIAN_POINT('Ctrl Pts',(-4.3267322227737,-1.30000000000783,5.5439628437342));
#39953=CARTESIAN_POINT('Ctrl Pts',(-4.25987806407973,-1.1851427086171,5.58127837497687));
#39954=CARTESIAN_POINT('Ctrl Pts',(-4.20158070045236,-1.06847604194785,
5.61286286081461));
#39955=CARTESIAN_POINT('Ctrl Pts',(-4.08667003651182,-0.794772684000902,
5.67258948017672));
#39956=CARTESIAN_POINT('Ctrl Pts',(-4.0330896730832,-0.636309800095237,
5.69197918867089));
#39957=CARTESIAN_POINT('Ctrl Pts',(-3.96886713289172,-0.319434907277179,
5.72899314540867));
#39958=CARTESIAN_POINT('Ctrl Pts',(-3.95196301927249,-0.158333333333342,
5.74113914727316));
#39959=CARTESIAN_POINT('Ctrl Pts',(-3.95891563445526,0.158333333333344,
5.76055677660053));
#39960=CARTESIAN_POINT('Ctrl Pts',(-3.98210843439915,0.319434907277186,
5.76585285006701));
#39961=CARTESIAN_POINT('Ctrl Pts',(-4.06184532639253,0.636309800095245,
5.77241526739943));
#39962=CARTESIAN_POINT('Ctrl Pts',(-4.12436285483472,0.794772684000891,
5.77854795651227));
#39963=CARTESIAN_POINT('Ctrl Pts',(-4.25514280214883,1.06847604194739,5.76328404203811));
#39964=CARTESIAN_POINT('Ctrl Pts',(-4.32053563777679,1.18514270861621,5.75147540083709));
#39965=CARTESIAN_POINT('Ctrl Pts',(-4.39471151571447,1.30000000000652,5.73446530142721));
#39966=CARTESIAN_POINT('Ctrl Pts',(-4.33567044487952,-1.30000000000787,
5.53578209593916));
#39967=CARTESIAN_POINT('Ctrl Pts',(-4.27076977516179,-1.18514270861714,
5.57178751878452));
#39968=CARTESIAN_POINT('Ctrl Pts',(-4.21397255168303,-1.06847604194788,
5.60255450794955));
#39969=CARTESIAN_POINT('Ctrl Pts',(-4.10148018510381,-0.794772684000929,
5.66153057808851));
#39970=CARTESIAN_POINT('Ctrl Pts',(-4.04815945570574,-0.636309800095257,
5.68240275508685));
#39971=CARTESIAN_POINT('Ctrl Pts',(-3.98422899902913,-0.319434907277188,
5.71981566023146));
#39972=CARTESIAN_POINT('Ctrl Pts',(-3.96623137841746,-0.158333333333347,
5.73140454462874));
#39973=CARTESIAN_POINT('Ctrl Pts',(-3.973463674695,0.158333333333349,5.75150962599252));
#39974=CARTESIAN_POINT('Ctrl Pts',(-3.99819974918407,0.319434907277196,
5.75849050162669));
#39975=CARTESIAN_POINT('Ctrl Pts',(-4.07786779404668,0.636309800095265,
5.76515753861331));
#39976=CARTESIAN_POINT('Ctrl Pts',(-4.13987208619196,0.794772684000913,
5.76911726872872));
#39977=CARTESIAN_POINT('Ctrl Pts',(-4.2681142673931,1.06847604194743,5.75422153983162));
#39978=CARTESIAN_POINT('Ctrl Pts',(-4.33195611341596,1.18514270861625,5.74306496903181));
#39979=CARTESIAN_POINT('Ctrl Pts',(-4.40412851706027,1.30000000000657,5.72719963653066));
#39980=CARTESIAN_POINT('Ctrl Pts',(-4.34632504743441,-1.30000000000789,
5.52463757271305));
#39981=CARTESIAN_POINT('Ctrl Pts',(-4.28387476894886,-1.18514270861716,
5.55912000438341));
#39982=CARTESIAN_POINT('Ctrl Pts',(-4.2289766621989,-1.0684760419479,5.58899711003865));
#39983=CARTESIAN_POINT('Ctrl Pts',(-4.11959808079522,-0.794772684000939,
5.64737997660876));
#39984=CARTESIAN_POINT('Ctrl Pts',(-4.06659446385943,-0.636309800095266,
5.67013156883144));
#39985=CARTESIAN_POINT('Ctrl Pts',(-4.00340218462963,-0.319434907277194,
5.70893556077439));
#39986=CARTESIAN_POINT('Ctrl Pts',(-3.98476119738918,-0.158333333333349,
5.72143444261475));
#39987=CARTESIAN_POINT('Ctrl Pts',(-3.99225312203943,0.158333333333352,
5.74221562590154));
#39988=CARTESIAN_POINT('Ctrl Pts',(-4.01797378492831,0.319434907277202,
5.7492518394961));
#39989=CARTESIAN_POINT('Ctrl Pts',(-4.09726629676795,0.636309800095276,
5.7553158128464));
#39990=CARTESIAN_POINT('Ctrl Pts',(-4.15896884281014,0.794772684000927,
5.75719602556793));
#39991=CARTESIAN_POINT('Ctrl Pts',(-4.28425709447938,1.06847604194744,5.7430159451123));
#39992=CARTESIAN_POINT('Ctrl Pts',(-4.34626539680437,1.18514270861627,5.73279018820648));
#39993=CARTESIAN_POINT('Ctrl Pts',(-4.41604935969341,1.30000000000659,5.71847670580035));
#39994=CARTESIAN_POINT('Ctrl Pts',(-4.35515498779441,-1.30000000000792,
5.51626230029215));
#39995=CARTESIAN_POINT('Ctrl Pts',(-4.29473922787703,-1.18514270861719,
5.54960135559851));
#39996=CARTESIAN_POINT('Ctrl Pts',(-4.24138370795419,-1.06847604194792,
5.57875750051019));
#39997=CARTESIAN_POINT('Ctrl Pts',(-4.13443234998209,-0.794772684000958,
5.63645066812221));
#39998=CARTESIAN_POINT('Ctrl Pts',(-4.08141479981886,-0.636309800095282,
5.6601675095401));
#39999=CARTESIAN_POINT('Ctrl Pts',(-4.01868156676103,-0.319434907277201,
5.69981192468275));
#40000=CARTESIAN_POINT('Ctrl Pts',(-3.99964611770337,-0.158333333333353,
5.71335837626925));
#40001=CARTESIAN_POINT('Ctrl Pts',(-4.00716314167774,0.158333333333356,
5.7342185271067));
#40002=CARTESIAN_POINT('Ctrl Pts',(-4.03324584237705,0.319434907277211,
5.74017555382292));
#40003=CARTESIAN_POINT('Ctrl Pts',(-4.11224760444397,0.636309800095291,
5.745785208225));
#40004=CARTESIAN_POINT('Ctrl Pts',(-4.1742891549149,0.794772684000945,5.74743434259157));
#40005=CARTESIAN_POINT('Ctrl Pts',(-4.29720630175374,1.06847604194747,5.73397154115603));
#40006=CARTESIAN_POINT('Ctrl Pts',(-4.35762891092206,1.1851427086163,5.7243040306088));
#40007=CARTESIAN_POINT('Ctrl Pts',(-4.42526785092076,1.30000000000662,5.71079655740988));
#40008=CARTESIAN_POINT('Ctrl Pts',(-4.37078301240193,-1.30000000000792,
5.50197740006034));
#40009=CARTESIAN_POINT('Ctrl Pts',(-4.3135809809026,-1.18514270861719,5.53274415335154));
#40010=CARTESIAN_POINT('Ctrl Pts',(-4.26268519101727,-1.06847604194793,
5.56023868567198));
#40011=CARTESIAN_POINT('Ctrl Pts',(-4.15967441440321,-0.794772684000964,
5.61619707054585));
#40012=CARTESIAN_POINT('Ctrl Pts',(-4.10683439689708,-0.636309800095286,
5.64192240980302));
#40013=CARTESIAN_POINT('Ctrl Pts',(-4.0449049345007,-0.319434907277203,
5.68296884230057));
#40014=CARTESIAN_POINT('Ctrl Pts',(-4.02497298992508,-0.158333333333354,
5.69777784326964));
#40015=CARTESIAN_POINT('Ctrl Pts',(-4.03289635293786,0.158333333333357,
5.71961533094095));
#40016=CARTESIAN_POINT('Ctrl Pts',(-4.06054091444927,0.319434907277212,
5.72594583243566));
#40017=CARTESIAN_POINT('Ctrl Pts',(-4.13903897138624,0.636309800095295,
5.73080253558442));
#40018=CARTESIAN_POINT('Ctrl Pts',(-4.20050281014632,0.794772684000951,
5.72935414887066));
#40019=CARTESIAN_POINT('Ctrl Pts',(-4.31925042598414,1.06847604194747,5.71696518890184));
#40020=CARTESIAN_POINT('Ctrl Pts',(-4.37711181961818,1.1851427086163,5.70867492566776));
#40021=CARTESIAN_POINT('Ctrl Pts',(-4.44143316402236,1.30000000000662,5.69745712091394));
#40022=CARTESIAN_POINT('Ctrl Pts',(-4.38954914692239,-1.30000000000818,
5.48121690616089));
#40023=CARTESIAN_POINT('Ctrl Pts',(-4.33633023486684,-1.18514270861742,
5.50842819923269));
#40024=CARTESIAN_POINT('Ctrl Pts',(-4.28857783106944,-1.06847604194813,
5.53376290222766));
#40025=CARTESIAN_POINT('Ctrl Pts',(-4.19088895311055,-0.794772684001115,
5.58795583584731));
#40026=CARTESIAN_POINT('Ctrl Pts',(-4.13896358606072,-0.636309800095409,
5.6174474536141));
#40027=CARTESIAN_POINT('Ctrl Pts',(-4.07860037207344,-0.319434907277266,
5.66128044194837));
#40028=CARTESIAN_POINT('Ctrl Pts',(-4.05796819861899,-0.158333333333385,
5.67873539850413));
#40029=CARTESIAN_POINT('Ctrl Pts',(-4.06601837690713,0.158333333333388,
5.70088706633193));
#40030=CARTESIAN_POINT('Ctrl Pts',(-4.09423437574826,0.319434907277274,
5.70444375388613));
#40031=CARTESIAN_POINT('Ctrl Pts',(-4.17194515055815,0.636309800095419,
5.70805426417284));
#40032=CARTESIAN_POINT('Ctrl Pts',(-4.2339664774439,0.794772684001107,5.70565218510332));
#40033=CARTESIAN_POINT('Ctrl Pts',(-4.34764865863211,1.06847604194768,5.6953488246972));
#40034=CARTESIAN_POINT('Ctrl Pts',(-4.40217130686692,1.18514270861653,5.68872907315249));
#40035=CARTESIAN_POINT('Ctrl Pts',(-4.46200779943961,1.30000000000688,5.67994951300579));
#40036=CARTESIAN_POINT('Ctrl Pts',(-4.41112472456861,-1.30000000000823,
5.45954571059543));
#40037=CARTESIAN_POINT('Ctrl Pts',(-4.36286900737893,-1.18514270861747,
5.48375018514035));
#40038=CARTESIAN_POINT('Ctrl Pts',(-4.31878817648165,-1.06847604194818,
5.50696965207528));
#40039=CARTESIAN_POINT('Ctrl Pts',(-4.22659746128865,-0.794772684001152,
5.55833570110362));
#40040=CARTESIAN_POINT('Ctrl Pts',(-4.17384714641575,-0.636309800095435,
5.58858728418216));
#40041=CARTESIAN_POINT('Ctrl Pts',(-4.114288708503,-0.319434907277277,5.63364822804344));
#40042=CARTESIAN_POINT('Ctrl Pts',(-4.09283227419875,-0.158333333333391,
5.65372521525302));
#40043=CARTESIAN_POINT('Ctrl Pts',(-4.10136977087594,0.158333333333394,
5.67693826559168));
#40044=CARTESIAN_POINT('Ctrl Pts',(-4.131191075948,0.319434907277288,5.67959205301889));
#40045=CARTESIAN_POINT('Ctrl Pts',(-4.20849140641991,0.636309800095445,
5.68279678218203));
#40046=CARTESIAN_POINT('Ctrl Pts',(-4.27071111802872,0.794772684001137,
5.67832433183507));
#40047=CARTESIAN_POINT('Ctrl Pts',(-4.37903721967095,1.06847604194772,5.67089337405542));
#40048=CARTESIAN_POINT('Ctrl Pts',(-4.43006377787937,1.18514270861658,5.66659176928105));
#40049=CARTESIAN_POINT('Ctrl Pts',(-4.48522653877245,1.30000000000693,5.66120514601103));
#40050=CARTESIAN_POINT('Ctrl Pts',(-4.42782422204453,-1.30000000000832,
5.4412447319148));
#40051=CARTESIAN_POINT('Ctrl Pts',(-4.38266614769295,-1.18514270861755,
5.46153999931372));
#40052=CARTESIAN_POINT('Ctrl Pts',(-4.34101741910968,-1.06847604194825,
5.48219429268874));
#40053=CARTESIAN_POINT('Ctrl Pts',(-4.25290781505086,-0.794772684001202,
5.53073926408937));
#40054=CARTESIAN_POINT('Ctrl Pts',(-4.20075795765716,-0.636309800095476,
5.56376099319447));
#40055=CARTESIAN_POINT('Ctrl Pts',(-4.1423804942734,-0.319434907277298,
5.61069120909608));
#40056=CARTESIAN_POINT('Ctrl Pts',(-4.12030187944122,-0.158333333333401,
5.63290628434515));
#40057=CARTESIAN_POINT('Ctrl Pts',(-4.12921724313909,0.158333333333404,
5.6568772790265));
#40058=CARTESIAN_POINT('Ctrl Pts',(-4.16008957882327,0.319434907277307,
5.65831943327165));
#40059=CARTESIAN_POINT('Ctrl Pts',(-4.23687477385054,0.636309800095485,
5.66085552466139));
#40060=CARTESIAN_POINT('Ctrl Pts',(-4.29913716795114,0.794772684001187,
5.65460753171467));
#40061=CARTESIAN_POINT('Ctrl Pts',(-4.40315349469226,1.06847604194779,5.64944089018014));
#40062=CARTESIAN_POINT('Ctrl Pts',(-4.45140790386964,1.18514270861666,5.64702901501569));
#40063=CARTESIAN_POINT('Ctrl Pts',(-4.50289190856247,1.30000000000702,5.64444171236415));
#40064=CARTESIAN_POINT('Ctrl Pts',(-4.44012243042177,-1.30000000000835,
5.42715703615215));
#40065=CARTESIAN_POINT('Ctrl Pts',(-4.39791645627916,-1.18514270861758,
5.44560341256595));
#40066=CARTESIAN_POINT('Ctrl Pts',(-4.3584859041896,-1.06847604194827,5.4650139957485));
#40067=CARTESIAN_POINT('Ctrl Pts',(-4.2738052209727,-0.79477268400122,5.51208383649821));
#40068=CARTESIAN_POINT('Ctrl Pts',(-4.22154640570247,-0.636309800095492,
5.54625319252759));
#40069=CARTESIAN_POINT('Ctrl Pts',(-4.16359851535671,-0.319434907277307,
5.59376442404522));
#40070=CARTESIAN_POINT('Ctrl Pts',(-4.14058799071849,-0.158333333333405,
5.61669015058547));
#40071=CARTESIAN_POINT('Ctrl Pts',(-4.14960969582907,0.158333333333408,
5.64090260438518));
#40072=CARTESIAN_POINT('Ctrl Pts',(-4.18143139561612,0.319434907277314,
5.64174134575178));
#40073=CARTESIAN_POINT('Ctrl Pts',(-4.25818468406121,0.6363098000955,5.64446165427731));
#40074=CARTESIAN_POINT('Ctrl Pts',(-4.32107128058956,0.794772684001208,
5.63802446775025));
#40075=CARTESIAN_POINT('Ctrl Pts',(-4.42196963571851,1.06847604194782,5.6347801551929));
#40076=CARTESIAN_POINT('Ctrl Pts',(-4.46806959498563,1.18514270861669,5.6336423111258));
#40077=CARTESIAN_POINT('Ctrl Pts',(-4.51659435423661,1.30000000000705,5.63277096568406));
#40078=CARTESIAN_POINT('Ctrl Pts',(-4.454645622087,-1.30000000000857,5.41105919281565));
#40079=CARTESIAN_POINT('Ctrl Pts',(-4.41514556095973,-1.18514270861778,
5.42611614972381));
#40080=CARTESIAN_POINT('Ctrl Pts',(-4.37779927083417,-1.06847604194846,
5.44322501577103));
#40081=CARTESIAN_POINT('Ctrl Pts',(-4.2964975114198,-0.794772684001356,
5.48749023955076));
#40082=CARTESIAN_POINT('Ctrl Pts',(-4.24439282465342,-0.636309800095601,
5.52336511487347));
#40083=CARTESIAN_POINT('Ctrl Pts',(-4.18738209157449,-0.319434907277362,
5.57228049978856));
#40084=CARTESIAN_POINT('Ctrl Pts',(-4.16403365829309,-0.158333333333432,
5.59739153873146));
#40085=CARTESIAN_POINT('Ctrl Pts',(-4.17349511325057,0.158333333333435,
5.62243620194746));
#40086=CARTESIAN_POINT('Ctrl Pts',(-4.20630986171008,0.319434907277368,
5.62237239062541));
#40087=CARTESIAN_POINT('Ctrl Pts',(-4.28258299737053,0.636309800095608,
5.62446595789768));
#40088=CARTESIAN_POINT('Ctrl Pts',(-4.34520753220417,0.794772684001345,
5.61593402713908));
#40089=CARTESIAN_POINT('Ctrl Pts',(-4.44251263710464,1.068476041948,5.61501368822388));
#40090=CARTESIAN_POINT('Ctrl Pts',(-4.48636413798361,1.18514270861689,5.61586237792014));
#40091=CARTESIAN_POINT('Ctrl Pts',(-4.53194736533916,1.30000000000727,5.61795813792712));
#40092=CARTESIAN_POINT('Ctrl Pts',(-4.47094525801616,-1.30000000000866,
5.39216627151158));
#40093=CARTESIAN_POINT('Ctrl Pts',(-4.43513973486294,-1.18514270861787,
5.40435163061268));
#40094=CARTESIAN_POINT('Ctrl Pts',(-4.40057535245081,-1.06847604194854,
5.41950137458678));
#40095=CARTESIAN_POINT('Ctrl Pts',(-4.3235919979,-0.794772684001415,5.4613486359422));
#40096=CARTESIAN_POINT('Ctrl Pts',(-4.27136350000773,-0.636309800095647,
5.4987471794917));
#40097=CARTESIAN_POINT('Ctrl Pts',(-4.21498556763763,-0.319434907277384,
5.5485128165621));
#40098=CARTESIAN_POINT('Ctrl Pts',(-4.19074131770077,-0.158333333333444,
5.57519316288732));
#40099=CARTESIAN_POINT('Ctrl Pts',(-4.20011017939256,0.158333333333446,
5.60009571229502));
#40100=CARTESIAN_POINT('Ctrl Pts',(-4.23345365297838,0.319434907277392,
5.59784807793541));
#40101=CARTESIAN_POINT('Ctrl Pts',(-4.30946451531293,0.636309800095655,
5.59976416600554));
#40102=CARTESIAN_POINT('Ctrl Pts',(-4.37321473773036,0.794772684001403,
5.5915238680523));
#40103=CARTESIAN_POINT('Ctrl Pts',(-4.46666130211471,1.06847604194808,5.59371528518928));
#40104=CARTESIAN_POINT('Ctrl Pts',(-4.50780006940397,1.18514270861698,5.59655722660272));
#40105=CARTESIAN_POINT('Ctrl Pts',(-4.54962804879656,1.30000000000736,5.60129252615098));
#40106=CARTESIAN_POINT('Ctrl Pts',(-4.48493632988914,-1.30000000000885,
5.3752561709007));
#40107=CARTESIAN_POINT('Ctrl Pts',(-4.45163533037209,-1.18514270861804,
5.38375827085221));
#40108=CARTESIAN_POINT('Ctrl Pts',(-4.41904162193305,-1.06847604194869,
5.39643844392018));
#40109=CARTESIAN_POINT('Ctrl Pts',(-4.34537761897406,-0.794772684001532,
5.43538436508636));
#40110=CARTESIAN_POINT('Ctrl Pts',(-4.2936880621305,-0.63630980009574,5.4750722726532));
#40111=CARTESIAN_POINT('Ctrl Pts',(-4.23824685917295,-0.319434907277431,
5.52615416822502));
#40112=CARTESIAN_POINT('Ctrl Pts',(-4.21330023661494,-0.158333333333467,
5.55430405446636));
#40113=CARTESIAN_POINT('Ctrl Pts',(-4.22318318569591,0.15833333333347,5.5801473341821));
#40114=CARTESIAN_POINT('Ctrl Pts',(-4.25796450582175,0.319434907277439,
5.57783932223402));
#40115=CARTESIAN_POINT('Ctrl Pts',(-4.33363484931934,0.636309800095748,
5.57940118940962));
#40116=CARTESIAN_POINT('Ctrl Pts',(-4.39684005390025,0.794772684001519,
5.56856823598866));
#40117=CARTESIAN_POINT('Ctrl Pts',(-4.48678914178438,1.06847604194824,5.57325856522636));
#40118=CARTESIAN_POINT('Ctrl Pts',(-4.52578314351235,1.18514270861715,5.5782710410378));
#40119=CARTESIAN_POINT('Ctrl Pts',(-4.56483551976503,1.30000000000755,5.58626572292747));
#40120=CARTESIAN_POINT('Ctrl Pts',(-4.498861949539,-1.30000000000899,5.35823247550946));
#40121=CARTESIAN_POINT('Ctrl Pts',(-4.46872355137842,-1.18514270861816,
5.36413287876654));
#40122=CARTESIAN_POINT('Ctrl Pts',(-4.43844643707928,-1.0684760419488,5.37491459924435));
#40123=CARTESIAN_POINT('Ctrl Pts',(-4.36817978410308,-0.794772684001614,
5.41109934970751));
#40124=CARTESIAN_POINT('Ctrl Pts',(-4.31565423214811,-0.636309800095808,
5.45083387039926));
#40125=CARTESIAN_POINT('Ctrl Pts',(-4.26086656492057,-0.319434907277466,
5.50278614645565));
#40126=CARTESIAN_POINT('Ctrl Pts',(-4.23599756233597,-0.158333333333484,
5.53373892058108));
#40127=CARTESIAN_POINT('Ctrl Pts',(-4.24621739610398,0.158333333333486,
5.56016007790502));
#40128=CARTESIAN_POINT('Ctrl Pts',(-4.28138354171649,0.319434907277472,
5.55584724853662));
#40129=CARTESIAN_POINT('Ctrl Pts',(-4.35683080108103,0.636309800095816,
5.55726731331466));
#40130=CARTESIAN_POINT('Ctrl Pts',(-4.42087067157835,0.794772684001605,
5.54641067168685));
#40131=CARTESIAN_POINT('Ctrl Pts',(-4.50748336180335,1.06847604194835,5.55387732613153));
#40132=CARTESIAN_POINT('Ctrl Pts',(-4.54415828630143,1.18514270861728,5.56072168072238));
#40133=CARTESIAN_POINT('Ctrl Pts',(-4.58001671101529,1.30000000000769,5.57117835186175));
#40134=CARTESIAN_POINT('Ctrl Pts',(-4.50921253636227,-1.30000000000911,
5.34679556586098));
#40135=CARTESIAN_POINT('Ctrl Pts',(-4.48076316876939,-1.18514270861827,
5.349916494865));
#40136=CARTESIAN_POINT('Ctrl Pts',(-4.45182716951738,-1.0684760419489,5.35883438517782));
#40137=CARTESIAN_POINT('Ctrl Pts',(-4.38385500613636,-0.794772684001686,
5.39282863611934));
#40138=CARTESIAN_POINT('Ctrl Pts',(-4.33190247816714,-0.636309800095865,
5.43450303805174));
#40139=CARTESIAN_POINT('Ctrl Pts',(-4.27758201208292,-0.319434907277494,
5.48702683718887));
#40140=CARTESIAN_POINT('Ctrl Pts',(-4.2518822176191,-0.158333333333498,
5.51844686361384));
#40141=CARTESIAN_POINT('Ctrl Pts',(-4.26207950271066,0.158333333333501,
5.5448406589144));
#40142=CARTESIAN_POINT('Ctrl Pts',(-4.2978562169275,0.319434907277501,5.53972878797136));
#40143=CARTESIAN_POINT('Ctrl Pts',(-4.37319299404238,0.636309800095873,
5.5411416915894));
#40144=CARTESIAN_POINT('Ctrl Pts',(-4.43766183316473,0.794772684001676,
5.52993599454729));
#40145=CARTESIAN_POINT('Ctrl Pts',(-4.52197796054513,1.06847604194845,5.53953275053415));
#40146=CARTESIAN_POINT('Ctrl Pts',(-4.55708058779137,1.18514270861738,5.54783679540291));
#40147=CARTESIAN_POINT('Ctrl Pts',(-4.59078851496094,1.30000000000781,5.56029080506853));
#40148=CARTESIAN_POINT('Ctrl Pts',(-4.52241367989135,-1.30000000000923,
5.32864709204046));
#40149=CARTESIAN_POINT('Ctrl Pts',(-4.49688183956528,-1.18514270861838,
5.32880335169503));
#40150=CARTESIAN_POINT('Ctrl Pts',(-4.47013069643415,-1.068476041949,5.33562922502868));
#40151=CARTESIAN_POINT('Ctrl Pts',(-4.40551337085382,-0.79477268400176,
5.36680649979061));
#40152=CARTESIAN_POINT('Ctrl Pts',(-4.35319518859154,-0.636309800095925,
5.4092594635518));
#40153=CARTESIAN_POINT('Ctrl Pts',(-4.29965614971638,-0.319434907277525,
5.46280526156545));
#40154=CARTESIAN_POINT('Ctrl Pts',(-4.27369098735892,-0.158333333333513,
5.49637428780528));
#40155=CARTESIAN_POINT('Ctrl Pts',(-4.28457445362594,0.158333333333516,
5.52393599581938));
#40156=CARTESIAN_POINT('Ctrl Pts',(-4.32174434070853,0.319434907277532,
5.51863165635827));
#40157=CARTESIAN_POINT('Ctrl Pts',(-4.39679783638627,0.636309800095934,
5.51979515593311));
#40158=CARTESIAN_POINT('Ctrl Pts',(-4.46077305529313,0.794772684001752,
5.50620273685446));
#40159=CARTESIAN_POINT('Ctrl Pts',(-4.54163194195897,1.06847604194855,5.51835365242479));
#40160=CARTESIAN_POINT('Ctrl Pts',(-4.57460044398954,1.18514270861749,5.5288139654911));
#40161=CARTESIAN_POINT('Ctrl Pts',(-4.6055366321297,1.30000000000793,5.54447491050905));
#40162=CARTESIAN_POINT('Ctrl Pts',(-4.53447732780698,-1.30000000000958,
5.31438497829742));
#40163=CARTESIAN_POINT('Ctrl Pts',(-4.5109825104172,-1.1851427086187,5.31125524905197));
#40164=CARTESIAN_POINT('Ctrl Pts',(-4.48584115885595,-1.06847604194929,
5.31586434062888));
#40165=CARTESIAN_POINT('Ctrl Pts',(-4.42395578391596,-0.794772684001975,
5.3443904884623));
#40166=CARTESIAN_POINT('Ctrl Pts',(-4.3723175462256,-0.636309800096095,
5.3891184329957));
#40167=CARTESIAN_POINT('Ctrl Pts',(-4.3192080190876,-0.319434907277609,
5.44310463691538));
#40168=CARTESIAN_POINT('Ctrl Pts',(-4.29212052481273,-0.158333333333556,
5.47701836007896));
#40169=CARTESIAN_POINT('Ctrl Pts',(-4.30275876461167,0.158333333333558,
5.50415463885691));
#40170=CARTESIAN_POINT('Ctrl Pts',(-4.34035579478986,0.319434907277619,
5.4973432969903));
#40171=CARTESIAN_POINT('Ctrl Pts',(-4.41539681098799,0.636309800096105,
5.49870078579237));
#40172=CARTESIAN_POINT('Ctrl Pts',(-4.48040915743014,0.794772684001963,
5.48561753045718));
#40173=CARTESIAN_POINT('Ctrl Pts',(-4.55881635333106,1.06847604194883,5.50084039405422));
#40174=CARTESIAN_POINT('Ctrl Pts',(-4.58998346201326,1.18514270861781,5.51318899988961));
#40175=CARTESIAN_POINT('Ctrl Pts',(-4.61837810954473,1.30000000000827,5.53129679797183));
#40176=CARTESIAN_POINT('Ctrl Pts',(-4.54622410918883,-1.30000000000978,
5.29959293032457));
#40177=CARTESIAN_POINT('Ctrl Pts',(-4.52519371057589,-1.18514270861888,
5.2938693065141));
#40178=CARTESIAN_POINT('Ctrl Pts',(-4.50184469080349,-1.06847604194945,
5.29656112542672));
#40179=CARTESIAN_POINT('Ctrl Pts',(-4.44254730545769,-0.794772684002097,
5.32222112180498));
#40180=CARTESIAN_POINT('Ctrl Pts',(-4.39012972240138,-0.636309800096193,
5.36688731062942));
#40181=CARTESIAN_POINT('Ctrl Pts',(-4.33751850654955,-0.319434907277658,
5.4214535408028));
#40182=CARTESIAN_POINT('Ctrl Pts',(-4.31045165556893,-0.15833333333358,
5.45756077992719));
#40183=CARTESIAN_POINT('Ctrl Pts',(-4.3216903872547,0.158333333333582,5.48568594651191));
#40184=CARTESIAN_POINT('Ctrl Pts',(-4.36028283544304,0.319434907277667,
5.47837482130748));
#40185=CARTESIAN_POINT('Ctrl Pts',(-4.43520221411006,0.636309800096202,
5.47973085897586));
#40186=CARTESIAN_POINT('Ctrl Pts',(-4.50017575770871,0.794772684002084,
5.46528736391715));
#40187=CARTESIAN_POINT('Ctrl Pts',(-4.57575016523733,1.068476041949,5.48291347614234));
#40188=CARTESIAN_POINT('Ctrl Pts',(-4.60508669366304,1.18514270861799,5.49709595582559));
#40189=CARTESIAN_POINT('Ctrl Pts',(-4.63104638980275,1.30000000000848,5.51783122432156));
#40190=CARTESIAN_POINT('Ctrl Pts',(-4.55380108281785,-1.30000000000987,
5.28935232644525));
#40191=CARTESIAN_POINT('Ctrl Pts',(-4.53424726420921,-1.18514270861897,
5.28165515201659));
#40192=CARTESIAN_POINT('Ctrl Pts',(-4.51202417591417,-1.06847604194953,
5.28297086445777));
#40193=CARTESIAN_POINT('Ctrl Pts',(-4.45451784927862,-0.794772684002154,
5.30683199509513));
#40194=CARTESIAN_POINT('Ctrl Pts',(-4.40211975238928,-0.636309800096239,
5.35229014717835));
#40195=CARTESIAN_POINT('Ctrl Pts',(-4.34991373095064,-0.319434907277682,
5.4073364560695));
#40196=CARTESIAN_POINT('Ctrl Pts',(-4.32259149247327,-0.158333333333591,
5.44446771120178));
#40197=CARTESIAN_POINT('Ctrl Pts',(-4.33397838104054,0.158333333333594,
5.47282131878555));
#40198=CARTESIAN_POINT('Ctrl Pts',(-4.37298997785036,0.31943490727769,5.46475274151342));
#40199=CARTESIAN_POINT('Ctrl Pts',(-4.44777416228423,0.636309800096248,
5.46601636464469));
#40200=CARTESIAN_POINT('Ctrl Pts',(-4.51290991151956,0.794772684002143,
5.45099755336283));
#40201=CARTESIAN_POINT('Ctrl Pts',(-4.58676884931904,1.06847604194907,5.47051963942771));
#40202=CARTESIAN_POINT('Ctrl Pts',(-4.61496684428607,1.18514270861808,5.48606125940474));
#40203=CARTESIAN_POINT('Ctrl Pts',(-4.63939203678979,1.30000000000857,5.50869411166581));
#40204=CARTESIAN_POINT('Ctrl Pts',(-4.55954363766313,-1.30000000000996,
5.28177408463877));
#40205=CARTESIAN_POINT('Ctrl Pts',(-4.54105222045902,-1.18514270861904,
5.27252120535695));
#40206=CARTESIAN_POINT('Ctrl Pts',(-4.51964064255725,-1.0684760419496,5.27275048042195));
#40207=CARTESIAN_POINT('Ctrl Pts',(-4.46342945884563,-0.794772684002204,
5.29518582512782));
#40208=CARTESIAN_POINT('Ctrl Pts',(-4.41102636495706,-0.636309800096279,
5.34121416803767));
#40209=CARTESIAN_POINT('Ctrl Pts',(-4.35917783714701,-0.319434907277702,
5.39671080243483));
#40210=CARTESIAN_POINT('Ctrl Pts',(-4.33181650747883,-0.158333333333601,
5.4348563220188));
#40211=CARTESIAN_POINT('Ctrl Pts',(-4.34330364603402,0.158333333333604,
5.46336204431361));
#40212=CARTESIAN_POINT('Ctrl Pts',(-4.38248057779019,0.31943490727771,5.4544820666224));
#40213=CARTESIAN_POINT('Ctrl Pts',(-4.45705852316959,0.636309800096288,
5.45550183824744));
#40214=CARTESIAN_POINT('Ctrl Pts',(-4.52224796629623,0.794772684002193,
5.43993533592643));
#40215=CARTESIAN_POINT('Ctrl Pts',(-4.59484958762752,1.06847604194914,5.46092555646331));
#40216=CARTESIAN_POINT('Ctrl Pts',(-4.62223636980904,1.18514270861815,5.47755649337426));
#40217=CARTESIAN_POINT('Ctrl Pts',(-4.64558338245264,1.30000000000865,5.50173247848997));
#40218=CARTESIAN_POINT('Ctrl Pts',(-4.56528629909216,-1.30000000001002,
5.27419824733449));
#40219=CARTESIAN_POINT('Ctrl Pts',(-4.54793752677531,-1.1851427086191,5.26352024146501));
#40220=CARTESIAN_POINT('Ctrl Pts',(-4.52738073179939,-1.06847604194965,
5.26273417553866));
#40221=CARTESIAN_POINT('Ctrl Pts',(-4.47247924892776,-0.794772684002245,
5.28377056614099));
#40222=CARTESIAN_POINT('Ctrl Pts',(-4.41992575934956,-0.636309800096313,
5.33013966639362));
#40223=CARTESIAN_POINT('Ctrl Pts',(-4.36837877093283,-0.31943490727772,
5.38599536878684));
#40224=CARTESIAN_POINT('Ctrl Pts',(-4.34097756808678,-0.15833333333361,
5.42514489833329));
#40225=CARTESIAN_POINT('Ctrl Pts',(-4.35260577087264,0.158333333333612,
5.45386967431965));
#40226=CARTESIAN_POINT('Ctrl Pts',(-4.39203663865104,0.319434907277726,
5.44433054874481));
#40227=CARTESIAN_POINT('Ctrl Pts',(-4.46645168939803,0.636309800096322,
5.44518118634463));
#40228=CARTESIAN_POINT('Ctrl Pts',(-4.53168185947985,0.794772684002236,
5.42904743639257));
#40229=CARTESIAN_POINT('Ctrl Pts',(-4.60300086052549,1.0684760419492,5.45146138928091));
#40230=CARTESIAN_POINT('Ctrl Pts',(-4.62955813691869,1.18514270861822,5.46914905507073));
#40231=CARTESIAN_POINT('Ctrl Pts',(-4.65180133678155,1.30000000000872,5.49482221696372));
#40232=CARTESIAN_POINT('Ctrl Pts',(-4.56948242172079,-1.30000000001006,
5.26835641752427));
#40233=CARTESIAN_POINT('Ctrl Pts',(-4.55288253832511,-1.18514270861914,
5.25645103233099));
#40234=CARTESIAN_POINT('Ctrl Pts',(-4.53291476005948,-1.06847604194968,
5.25482746551733));
#40235=CARTESIAN_POINT('Ctrl Pts',(-4.47900468683155,-0.794772684002266,
5.27482975871175));
#40236=CARTESIAN_POINT('Ctrl Pts',(-4.42662566433208,-0.636309800096331,
5.3218843316876));
#40237=CARTESIAN_POINT('Ctrl Pts',(-4.37532764569018,-0.319434907277728,
5.37803351666651));
#40238=CARTESIAN_POINT('Ctrl Pts',(-4.34766886857733,-0.158333333333614,
5.4175747831348));
#40239=CARTESIAN_POINT('Ctrl Pts',(-4.3594022483002,0.158333333333617,5.4464640643126));
#40240=CARTESIAN_POINT('Ctrl Pts',(-4.39916950767834,0.319434907277735,
5.43666623015078));
#40241=CARTESIAN_POINT('Ctrl Pts',(-4.47360351911369,0.636309800096339,
5.43762258648556));
#40242=CARTESIAN_POINT('Ctrl Pts',(-4.53901285539156,0.794772684002258,
5.42131440253097));
#40243=CARTESIAN_POINT('Ctrl Pts',(-4.60934782008004,1.06847604194923,5.44475704572301));
#40244=CARTESIAN_POINT('Ctrl Pts',(-4.63522574210525,1.18514270861825,5.46313998662896));
#40245=CARTESIAN_POINT('Ctrl Pts',(-4.65653618610901,1.30000000000876,5.48975841683847));
#40246=CARTESIAN_POINT('Ctrl Pts',(-4.57226309969796,-1.30000000001008,
5.26443910125368));
#40247=CARTESIAN_POINT('Ctrl Pts',(-4.55614439737282,-1.18514270861916,
5.25168907646359));
#40248=CARTESIAN_POINT('Ctrl Pts',(-4.53655907295875,-1.0684760419497,5.24949230992485));
#40249=CARTESIAN_POINT('Ctrl Pts',(-4.48330446501139,-0.794772684002281,
5.26879747749121));
#40250=CARTESIAN_POINT('Ctrl Pts',(-4.4310764076616,-0.636309800096343,
5.31636164782972));
#40251=CARTESIAN_POINT('Ctrl Pts',(-4.37994355381527,-0.319434907277734,
5.37270246234844));
#40252=CARTESIAN_POINT('Ctrl Pts',(-4.35208463527993,-0.158333333333617,
5.41245690758916));
#40253=CARTESIAN_POINT('Ctrl Pts',(-4.36388315554926,0.158333333333619,
5.44144657099326));
#40254=CARTESIAN_POINT('Ctrl Pts',(-4.40388525801494,0.319434907277741,
5.43149382375963));
#40255=CARTESIAN_POINT('Ctrl Pts',(-4.47834879306739,0.63630980009635,5.4325488102522));
#40256=CARTESIAN_POINT('Ctrl Pts',(-4.54389890576145,0.794772684002272,
5.41616089186566));
#40257=CARTESIAN_POINT('Ctrl Pts',(-4.61358662515068,1.06847604194925,5.44030332760959));
#40258=CARTESIAN_POINT('Ctrl Pts',(-4.63901156673434,1.18514270861827,5.45914904729804));
#40259=CARTESIAN_POINT('Ctrl Pts',(-4.65969621836226,1.30000000000878,5.48639012080671));
#40260=CARTESIAN_POINT('Ctrl Pts',(-4.5741188519777,-1.30000000001009,5.26183096309819));
#40261=CARTESIAN_POINT('Ctrl Pts',(-4.55832262344367,-1.18514270861917,
5.24852040473667));
#40262=CARTESIAN_POINT('Ctrl Pts',(-4.53899243564442,-1.06847604194971,
5.24594177814312));
#40263=CARTESIAN_POINT('Ctrl Pts',(-4.48617168196922,-0.794772684002287,
5.26477754415892));
#40264=CARTESIAN_POINT('Ctrl Pts',(-4.434033615713,-0.636309800096347,5.31266555574856));
#40265=CARTESIAN_POINT('Ctrl Pts',(-4.38300947242625,-0.319434907277736,
5.36913184462045));
#40266=CARTESIAN_POINT('Ctrl Pts',(-4.35502611025119,-0.158333333333618,
5.40904168442021));
#40267=CARTESIAN_POINT('Ctrl Pts',(-4.36686780005815,0.15833333333362,5.43809739240082));
#40268=CARTESIAN_POINT('Ctrl Pts',(-4.40701985920357,0.319434907277743,
5.42803103189341));
#40269=CARTESIAN_POINT('Ctrl Pts',(-4.4814985819506,0.636309800096354,5.42914449465699));
#40270=CARTESIAN_POINT('Ctrl Pts',(-4.54713803730562,0.794772684002278,
5.41269591781254));
#40271=CARTESIAN_POINT('Ctrl Pts',(-4.61639854019045,1.06847604194926,5.43731193015391));
#40272=CARTESIAN_POINT('Ctrl Pts',(-4.64152561010396,1.18514270861828,5.45647294845647));
#40273=CARTESIAN_POINT('Ctrl Pts',(-4.66179944458639,1.30000000000879,5.48413962543206));
#40274=CARTESIAN_POINT('Ctrl Pts',(-4.57644778804015,-1.30000000001011,
5.25858548016582));
#40275=CARTESIAN_POINT('Ctrl Pts',(-4.56106380680746,-1.18514270861919,
5.24458808378279));
#40276=CARTESIAN_POINT('Ctrl Pts',(-4.54205553892619,-1.06847604194973,
5.24153671058873));
#40277=CARTESIAN_POINT('Ctrl Pts',(-4.48976981033586,-0.794772684002301,
5.25977493139605));
#40278=CARTESIAN_POINT('Ctrl Pts',(-4.43770668269,-0.636309800096359,5.30801150492459));
#40279=CARTESIAN_POINT('Ctrl Pts',(-4.38681366613632,-0.319434907277742,
5.36462748309272));
#40280=CARTESIAN_POINT('Ctrl Pts',(-4.35870442655486,-0.158333333333621,
5.40477642123583));
#40281=CARTESIAN_POINT('Ctrl Pts',(-4.37059989637588,0.158333333333623,
5.43391337566916));
#40282=CARTESIAN_POINT('Ctrl Pts',(-4.41091950780841,0.319434907277749,
5.42367376371536));
#40283=CARTESIAN_POINT('Ctrl Pts',(-4.48540130712376,0.636309800096367,
5.42483439814329));
#40284=CARTESIAN_POINT('Ctrl Pts',(-4.55113497936443,0.794772684002292,
5.40828071637679));
#40285=CARTESIAN_POINT('Ctrl Pts',(-4.61987196733546,1.06847604194928,5.43350599349821));
#40286=CARTESIAN_POINT('Ctrl Pts',(-4.64463852227565,1.1851427086183,5.45308067856541));
#40287=CARTESIAN_POINT('Ctrl Pts',(-4.6644179370195,1.30000000000881,5.48131096092248));
#40288=CARTESIAN_POINT('Ctrl Pts',(-4.57856707538984,-1.30000000001014,
5.25570001012011));
#40289=CARTESIAN_POINT('Ctrl Pts',(-4.56357914844702,-1.18514270861921,
5.24112202841535));
#40290=CARTESIAN_POINT('Ctrl Pts',(-4.54487067682979,-1.06847604194975,
5.23766032289636));
#40291=CARTESIAN_POINT('Ctrl Pts',(-4.49305516228741,-0.794772684002316,
5.25534391242805));
#40292=CARTESIAN_POINT('Ctrl Pts',(-4.44097465579337,-0.636309800096371,
5.30376671552586));
#40293=CARTESIAN_POINT('Ctrl Pts',(-4.39018970784945,-0.319434907277748,
5.36050340088851));
#40294=CARTESIAN_POINT('Ctrl Pts',(-4.36203206360161,-0.158333333333624,
5.40096741366718));
#40295=CARTESIAN_POINT('Ctrl Pts',(-4.37397750911205,0.158333333333626,
5.43017854321455));
#40296=CARTESIAN_POINT('Ctrl Pts',(-4.41440851291143,0.319434907277755,
5.41972070094411));
#40297=CARTESIAN_POINT('Ctrl Pts',(-4.48885753596838,0.636309800096378,
5.42086554200589));
#40298=CARTESIAN_POINT('Ctrl Pts',(-4.55463482495819,0.794772684002307,
5.4041480378201));
#40299=CARTESIAN_POINT('Ctrl Pts',(-4.62291649322507,1.0684760419493,5.4299478453989));
#40300=CARTESIAN_POINT('Ctrl Pts',(-4.64738044212327,1.18514270861832,5.44993113752389));
#40301=CARTESIAN_POINT('Ctrl Pts',(-4.6667517358118,1.30000000000884,5.47872994104999));
#40302=CARTESIAN_POINT('Ctrl Pts',(-4.57998763858014,-1.30000000001015,
5.25378819732745));
#40303=CARTESIAN_POINT('Ctrl Pts',(-4.56527256586436,-1.18514270861922,
5.23883649972994));
#40304=CARTESIAN_POINT('Ctrl Pts',(-4.54676749277986,-1.06847604194975,
5.23510661561415));
#40305=CARTESIAN_POINT('Ctrl Pts',(-4.49526141298941,-0.79477268400232,
5.25241447120459));
#40306=CARTESIAN_POINT('Ctrl Pts',(-4.44313980655772,-0.636309800096374,
5.30091693696236));
#40307=CARTESIAN_POINT('Ctrl Pts',(-4.39242242526843,-0.31943490727775,
5.35772759265388));
#40308=CARTESIAN_POINT('Ctrl Pts',(-4.36425314259276,-0.158333333333625,
5.39843341442863));
#40309=CARTESIAN_POINT('Ctrl Pts',(-4.37623252610293,0.158333333333627,
5.42769446121915));
#40310=CARTESIAN_POINT('Ctrl Pts',(-4.41672627203826,0.319434907277756,
5.41707285569079));
#40311=CARTESIAN_POINT('Ctrl Pts',(-4.49114189239036,0.636309800096382,
5.41818810853485));
#40312=CARTESIAN_POINT('Ctrl Pts',(-4.55693359486649,0.794772684002312,
5.40133680343764));
#40313=CARTESIAN_POINT('Ctrl Pts',(-4.62491658247708,1.0684760419493,5.42752749481234));
#40314=CARTESIAN_POINT('Ctrl Pts',(-4.64918596137114,1.18514270861833,5.44779498551626));
#40315=CARTESIAN_POINT('Ctrl Pts',(-4.66829740284029,1.30000000000884,5.4769929870886));
#40316=CARTESIAN_POINT('Ctrl Pts',(-4.58069913722931,-1.30000000001015,
5.25283418642123));
#40317=CARTESIAN_POINT('Ctrl Pts',(-4.56612184637048,-1.18514270861922,
5.23769769344442));
#40318=CARTESIAN_POINT('Ctrl Pts',(-4.54771899138673,-1.06847604194975,
5.23383451727211));
#40319=CARTESIAN_POINT('Ctrl Pts',(-4.49636689646632,-0.79477268400232,
5.25095342452577));
#40320=CARTESIAN_POINT('Ctrl Pts',(-4.44422005583735,-0.636309800096374,
5.29948864824094));
#40321=CARTESIAN_POINT('Ctrl Pts',(-4.39353557103492,-0.31943490727775,
5.35633497402513));
#40322=CARTESIAN_POINT('Ctrl Pts',(-4.36536345533378,-0.158333333333625,
5.39716628380688));
#40323=CARTESIAN_POINT('Ctrl Pts',(-4.37735990023755,0.158333333333627,
5.42645234708054));
#40324=CARTESIAN_POINT('Ctrl Pts',(-4.41788351356185,0.319434907277757,
5.41574646919451));
#40325=CARTESIAN_POINT('Ctrl Pts',(-4.4922806760358,0.636309800096382,5.41684401218561));
#40326=CARTESIAN_POINT('Ctrl Pts',(-4.55807708845598,0.794772684002312,
5.39992163775985));
#40327=CARTESIAN_POINT('Ctrl Pts',(-4.62591147829473,1.0684760419493,5.42630893740137));
#40328=CARTESIAN_POINT('Ctrl Pts',(-4.65008471562182,1.18514270861833,5.44672038689974));
#40329=CARTESIAN_POINT('Ctrl Pts',(-4.66906819642635,1.30000000000884,5.47612120162733));
#40330=CARTESIAN_POINT('Ctrl Pts',(-4.58129282510572,-1.30000000001015,
5.25204039785036));
#40331=CARTESIAN_POINT('Ctrl Pts',(-4.5668312977909,-1.18514270861922,5.23675135951165));
#40332=CARTESIAN_POINT('Ctrl Pts',(-4.54851397789909,-1.06847604194976,
5.23277765717448));
#40333=CARTESIAN_POINT('Ctrl Pts',(-4.49728965238091,-0.794772684002322,
5.24973829962777));
#40334=CARTESIAN_POINT('Ctrl Pts',(-4.44511843149432,-0.636309800096376,
5.29829575089737));
#40335=CARTESIAN_POINT('Ctrl Pts',(-4.3944607273938,-0.319434907277751,
5.35517085551875));
#40336=CARTESIAN_POINT('Ctrl Pts',(-4.36628839287869,-0.158333333333625,
5.39611001880934));
#40337=CARTESIAN_POINT('Ctrl Pts',(-4.37829914571928,0.158333333333628,
5.42541700288283));
#40338=CARTESIAN_POINT('Ctrl Pts',(-4.41884657258655,0.319434907277757,
5.41463918881924));
#40339=CARTESIAN_POINT('Ctrl Pts',(-4.49322718206872,0.636309800096384,
5.41572002028131));
#40340=CARTESIAN_POINT('Ctrl Pts',(-4.55902592254007,0.794772684002315,
5.39873574736935));
#40341=CARTESIAN_POINT('Ctrl Pts',(-4.62673696750234,1.0684760419493,5.42528763006261));
#40342=CARTESIAN_POINT('Ctrl Pts',(-4.65083083054437,1.18514270861833,5.44582024270707));
#40343=CARTESIAN_POINT('Ctrl Pts',(-4.66970895420543,1.30000000000885,5.47539214182216));
#40344=CARTESIAN_POINT('Ctrl Pts',(-4.58170873549506,-1.30000000001015,
5.25148528385598));
#40345=CARTESIAN_POINT('Ctrl Pts',(-4.56732852626551,-1.18514270861922,
5.23608990939209));
#40346=CARTESIAN_POINT('Ctrl Pts',(-4.54907116358769,-1.06847604194975,
5.23203897466044));
#40347=CARTESIAN_POINT('Ctrl Pts',(-4.4979360033423,-0.794772684002322,
5.24888843027225));
#40348=CARTESIAN_POINT('Ctrl Pts',(-4.44574659464001,-0.636309800096376,
5.2974597341343));
#40349=CARTESIAN_POINT('Ctrl Pts',(-4.39510719845474,-0.319434907277751,
5.35435430888612));
#40350=CARTESIAN_POINT('Ctrl Pts',(-4.36693505035454,-0.158333333333625,
5.39536947651554));
#40351=CARTESIAN_POINT('Ctrl Pts',(-4.37895582240997,0.158333333333628,
5.42469108545479));
#40352=CARTESIAN_POINT('Ctrl Pts',(-4.41951997902849,0.319434907277757,
5.41386300497789));
#40353=CARTESIAN_POINT('Ctrl Pts',(-4.49388864042137,0.636309800096383,
5.41493151960541));
#40354=CARTESIAN_POINT('Ctrl Pts',(-4.55968810386129,0.794772684002314,
5.39790242646855));
#40355=CARTESIAN_POINT('Ctrl Pts',(-4.62731296829461,1.0684760419493,5.42456973425715));
#40356=CARTESIAN_POINT('Ctrl Pts',(-4.65135158615395,1.18514270861833,5.4451876535451));
#40357=CARTESIAN_POINT('Ctrl Pts',(-4.67015652380732,1.30000000000885,5.47488020270033));
#40358=CARTESIAN_POINT('Ctrl Pts',(-4.5819463590888,-1.30000000001015,5.25116801734297));
#40359=CARTESIAN_POINT('Ctrl Pts',(-4.56761274025231,-1.18514270861922,
5.23571206996149));
#40360=CARTESIAN_POINT('Ctrl Pts',(-4.54938969344282,-1.06847604194976,
5.23161708847656));
#40361=CARTESIAN_POINT('Ctrl Pts',(-4.49830545311051,-0.794772684002324,
5.24840296602242));
#40362=CARTESIAN_POINT('Ctrl Pts',(-4.44610524235701,-0.636309800096377,
5.29698156640216));
#40363=CARTESIAN_POINT('Ctrl Pts',(-4.39547634965677,-0.319434907277752,
5.35388733063218));
#40364=CARTESIAN_POINT('Ctrl Pts',(-4.36730476756172,-0.158333333333626,
5.39494662952139));
#40365=CARTESIAN_POINT('Ctrl Pts',(-4.37933130144857,0.158333333333628,
5.4242766377249));
#40366=CARTESIAN_POINT('Ctrl Pts',(-4.41990464680665,0.319434907277758,
5.41341924517007));
#40367=CARTESIAN_POINT('Ctrl Pts',(-4.49426640787336,0.636309800096385,
5.4144806021061));
#40368=CARTESIAN_POINT('Ctrl Pts',(-4.56006650367745,0.794772684002316,
5.39742624635705));
#40369=CARTESIAN_POINT('Ctrl Pts',(-4.62764213807441,1.06847604194931,5.42415953464588));
#40370=CARTESIAN_POINT('Ctrl Pts',(-4.65164916232392,1.18514270861834,5.44482615986139));
#40371=CARTESIAN_POINT('Ctrl Pts',(-4.67041222261625,1.30000000000885,5.47458756035798));
#40372=CARTESIAN_POINT('Ctrl Pts',(-4.5896776835703,-1.30000000000998,5.24087078904587));
#40373=CARTESIAN_POINT('Ctrl Pts',(-4.57685555325251,-1.18514270861906,
5.22344232441515));
#40374=CARTESIAN_POINT('Ctrl Pts',(-4.55974551517167,-1.06847604194961,
5.21791249958274));
#40375=CARTESIAN_POINT('Ctrl Pts',(-4.51031197962849,-0.794772684002216,
5.2326257362309));
#40376=CARTESIAN_POINT('Ctrl Pts',(-4.45776460123848,-0.636309800096291,
5.28144707494063));
#40377=CARTESIAN_POINT('Ctrl Pts',(-4.40746454541298,-0.319434907277709,
5.33869713889282));
#40378=CARTESIAN_POINT('Ctrl Pts',(-4.37928687943884,-0.158333333333604,
5.38115302849488));
#40379=CARTESIAN_POINT('Ctrl Pts',(-4.39149847991096,0.158333333333606,
5.41075297103868));
#40380=CARTESIAN_POINT('Ctrl Pts',(-4.43239750422643,0.319434907277714,
5.39898567727831));
#40381=CARTESIAN_POINT('Ctrl Pts',(-4.50653337087347,0.636309800096298,
5.39981105663908));
#40382=CARTESIAN_POINT('Ctrl Pts',(-4.57232169147551,0.794772684002208,
5.38188329400092));
#40383=CARTESIAN_POINT('Ctrl Pts',(-4.63829918072036,1.06847604194916,5.41076288483102));
#40384=CARTESIAN_POINT('Ctrl Pts',(-4.66128704727822,1.18514270861817,5.4330242182846));
#40385=CARTESIAN_POINT('Ctrl Pts',(-4.67870357000646,1.30000000000867,5.46504598041558));
#40386=CARTESIAN_POINT('Ctrl Pts',(-4.60062712095472,-1.30000000000845,
5.22482344032791));
#40387=CARTESIAN_POINT('Ctrl Pts',(-4.58971953854938,-1.18514270861767,
5.20400024324085));
#40388=CARTESIAN_POINT('Ctrl Pts',(-4.57409395527427,-1.06847604194836,
5.19610612076081));
#40389=CARTESIAN_POINT('Ctrl Pts',(-4.52709620618016,-0.794772684001287,
5.20773786741273));
#40390=CARTESIAN_POINT('Ctrl Pts',(-4.47476552804312,-0.636309800095545,
5.25800147984835));
#40391=CARTESIAN_POINT('Ctrl Pts',(-4.4251161255172,-0.319434907277333,
5.31597655950532));
#40392=CARTESIAN_POINT('Ctrl Pts',(-4.39653103096014,-0.158333333333419,
5.35985818511565));
#40393=CARTESIAN_POINT('Ctrl Pts',(-4.40909476686169,0.158333333333421,
5.38997142220023));
#40394=CARTESIAN_POINT('Ctrl Pts',(-4.45065571899694,0.319434907277343,
5.37714567020242));
#40395=CARTESIAN_POINT('Ctrl Pts',(-4.52505708475374,0.636309800095555,
5.37858900352638));
#40396=CARTESIAN_POINT('Ctrl Pts',(-4.59201094519908,0.794772684001275,
5.36131287512466));
#40397=CARTESIAN_POINT('Ctrl Pts',(-4.65531542587047,1.06847604194791,5.39282328721827));
#40398=CARTESIAN_POINT('Ctrl Pts',(-4.6763049397076,1.18514270861679,5.41661523283239));
#40399=CARTESIAN_POINT('Ctrl Pts',(-4.6908818033611,1.30000000000715,5.45055943424102));
#40400=CARTESIAN_POINT('Ctrl Pts',(-4.61560427125043,-1.30000000000843,
5.20428584956671));
#40401=CARTESIAN_POINT('Ctrl Pts',(-4.60721582813338,-1.18514270861765,
5.17894198652733));
#40402=CARTESIAN_POINT('Ctrl Pts',(-4.59353793472172,-1.06847604194834,
5.16788666297074));
#40403=CARTESIAN_POINT('Ctrl Pts',(-4.54971957635672,-0.794772684001272,
5.17535603856278));
#40404=CARTESIAN_POINT('Ctrl Pts',(-4.49766388251748,-0.636309800095534,
5.22748590960429));
#40405=CARTESIAN_POINT('Ctrl Pts',(-4.44877749627254,-0.319434907277328,
5.28627334674993));
#40406=CARTESIAN_POINT('Ctrl Pts',(-4.41960624761064,-0.158333333333416,
5.33200674040388));
#40407=CARTESIAN_POINT('Ctrl Pts',(-4.43242015699473,0.158333333333418,
5.36246973164054));
#40408=CARTESIAN_POINT('Ctrl Pts',(-4.47489349638911,0.319434907277335,
5.34829149709891));
#40409=CARTESIAN_POINT('Ctrl Pts',(-4.54888650316088,0.636309800095542,
5.34933031237017));
#40410=CARTESIAN_POINT('Ctrl Pts',(-4.61553439221572,0.794772684001263,
5.32988210434617));
#40411=CARTESIAN_POINT('Ctrl Pts',(-4.6759182053292,1.06847604194789,5.36597580363968));
#40412=CARTESIAN_POINT('Ctrl Pts',(-4.69509996469825,1.18514270861676,5.39322292659584));
#40413=CARTESIAN_POINT('Ctrl Pts',(-4.70732556818005,1.30000000000713,5.4320935474872));
#40414=CARTESIAN_POINT('Ctrl Pts',(-4.62268404883095,-1.30000000000774,
5.19340317858565));
#40415=CARTESIAN_POINT('Ctrl Pts',(-4.61569350574113,-1.18514270861703,
5.16602552974015));
#40416=CARTESIAN_POINT('Ctrl Pts',(-4.60305483470086,-1.06847604194778,
5.15350263191577));
#40417=CARTESIAN_POINT('Ctrl Pts',(-4.56080867077122,-0.794772684000851,
5.15888967928581));
#40418=CARTESIAN_POINT('Ctrl Pts',(-4.50854513869897,-0.636309800095197,
5.2114509203725));
#40419=CARTESIAN_POINT('Ctrl Pts',(-4.45994161137855,-0.319434907277159,
5.2704792232101));
#40420=CARTESIAN_POINT('Ctrl Pts',(-4.43050381798302,-0.158333333333332,
5.31712145281223));
#40421=CARTESIAN_POINT('Ctrl Pts',(-4.44367001134335,0.158333333333335,
5.34809023449043));
#40422=CARTESIAN_POINT('Ctrl Pts',(-4.48691159332261,0.319434907277167,
5.33373581427421));
#40423=CARTESIAN_POINT('Ctrl Pts',(-4.56103497295898,0.636309800095206,
5.33510192542139));
#40424=CARTESIAN_POINT('Ctrl Pts',(-4.62791448441862,0.79477268400084,5.31522003750839));
#40425=CARTESIAN_POINT('Ctrl Pts',(-4.68657619398998,1.06847604194732,5.35312981420995));
#40426=CARTESIAN_POINT('Ctrl Pts',(-4.70457535664068,1.18514270861614,5.38161490460393));
#40427=CARTESIAN_POINT('Ctrl Pts',(-4.71518120149896,1.30000000000644,5.42217534775329));
#40428=CARTESIAN_POINT('Ctrl Pts',(-4.62624077063454,-1.30000000000774,
5.18799189686137));
#40429=CARTESIAN_POINT('Ctrl Pts',(-4.61995220105655,-1.18514270861703,
5.15960337168817));
#40430=CARTESIAN_POINT('Ctrl Pts',(-4.60783501082469,-1.06847604194778,
5.14635039002685));
#40431=CARTESIAN_POINT('Ctrl Pts',(-4.566376597632,-0.794772684000851,5.15069948450678));
#40432=CARTESIAN_POINT('Ctrl Pts',(-4.5139835392274,-0.636309800095197,
5.20343425858748));
#40433=CARTESIAN_POINT('Ctrl Pts',(-4.46556375514821,-0.319434907277159,
5.26264955034744));
#40434=CARTESIAN_POINT('Ctrl Pts',(-4.43611716307415,-0.158333333333332,
5.30994285314818));
#40435=CARTESIAN_POINT('Ctrl Pts',(-4.44941966576161,0.158333333333335,
5.34110298165354));
#40436=CARTESIAN_POINT('Ctrl Pts',(-4.49284772594685,0.319434907277167,
5.32635100323495));
#40437=CARTESIAN_POINT('Ctrl Pts',(-4.56698074650739,0.636309800095206,
5.32779325308506));
#40438=CARTESIAN_POINT('Ctrl Pts',(-4.63406245451013,0.79477268400084,5.30782498057273));
#40439=CARTESIAN_POINT('Ctrl Pts',(-4.69192014515469,1.06847604194732,5.34673782657625));
#40440=CARTESIAN_POINT('Ctrl Pts',(-4.70935397490061,1.18514270861614,5.37588728519524));
#40441=CARTESIAN_POINT('Ctrl Pts',(-4.71917718395088,1.30000000000644,5.41734227326118));
#40442=CARTESIAN_POINT('',(-4.63725024984735,1.2,5.46840821199375));
#40443=CARTESIAN_POINT('Ctrl Pts',(-4.63725024984735,1.2,5.46840821199376));
#40444=CARTESIAN_POINT('Ctrl Pts',(-4.62623288747658,1.21680927464258,5.48695510237328));
#40445=CARTESIAN_POINT('Ctrl Pts',(-4.61595325414295,1.23316098172227,5.50634587166694));
#40446=CARTESIAN_POINT('Ctrl Pts',(-4.59367983320334,1.26666762025062,5.54312911943321));
#40447=CARTESIAN_POINT('Ctrl Pts',(-4.58868040342263,1.27448084893935,5.55224217132525));
#40448=CARTESIAN_POINT('Ctrl Pts',(-4.57136452279491,1.30000000000761,5.5797758180862));
#40449=CARTESIAN_POINT('',(-4.58017335384877,0.653834841338402,5.32263161625288));
#40450=CARTESIAN_POINT('Ctrl Pts',(-4.58017335390807,0.653834841323774,
5.3226316162909));
#40451=CARTESIAN_POINT('Ctrl Pts',(-4.58566039843636,0.710876435607271,
5.33601823521891));
#40452=CARTESIAN_POINT('Ctrl Pts',(-4.59154716380413,0.767442498216031,
5.3505545328843));
#40453=CARTESIAN_POINT('Ctrl Pts',(-4.60348776625804,0.881812809428854,
5.38047657158293));
#40454=CARTESIAN_POINT('Ctrl Pts',(-4.60916965496843,0.939315063510303,
5.39489255928413));
#40455=CARTESIAN_POINT('Ctrl Pts',(-4.61960617994113,1.03703221706045,5.42184408062769));
#40456=CARTESIAN_POINT('Ctrl Pts',(-4.62007222621881,1.04047637892618,5.42298882183644));
#40457=CARTESIAN_POINT('Ctrl Pts',(-4.63064770978488,1.13868342304201,5.45079102623296));
#40458=CARTESIAN_POINT('Ctrl Pts',(-4.63355571084997,1.16612797337853,5.45851413533704));
#40459=CARTESIAN_POINT('Ctrl Pts',(-4.63725024984735,1.2,5.46840821199376));
#40460=CARTESIAN_POINT('',(-4.52544944337377,-0.653834841531101,5.19430627077111));
#40461=CARTESIAN_POINT('Ctrl Pts',(-4.52544944337376,-0.653834841531102,
5.19430627077111));
#40462=CARTESIAN_POINT('Ctrl Pts',(-4.49798587443275,-0.575737631362572,
5.22568933893298));
#40463=CARTESIAN_POINT('Ctrl Pts',(-4.47558879617822,-0.493703172347255,
5.25273934756678));
#40464=CARTESIAN_POINT('Ctrl Pts',(-4.44500736577266,-0.338082431543929,
5.29312978320453));
#40465=CARTESIAN_POINT('Ctrl Pts',(-4.43523489250357,-0.265627281829756,
5.30816486560134));
#40466=CARTESIAN_POINT('Ctrl Pts',(-4.42569301093367,-0.129696671635448,
5.33064595190667));
#40467=CARTESIAN_POINT('Ctrl Pts',(-4.42464816556244,-0.066641443281186,
5.33882442907362));
#40468=CARTESIAN_POINT('Ctrl Pts',(-4.42950987352535,0.0594827545774232,
5.35118240948938));
#40469=CARTESIAN_POINT('Ctrl Pts',(-4.43543101216695,0.122684205165005,
5.35544646033219));
#40470=CARTESIAN_POINT('Ctrl Pts',(-4.4556613000911,0.260063037905712,5.35953858680526));
#40471=CARTESIAN_POINT('Ctrl Pts',(-4.47132565790492,0.333932211455017,
5.35845298339707));
#40472=CARTESIAN_POINT('Ctrl Pts',(-4.51502626842882,0.491503249588507,
5.348104651279));
#40473=CARTESIAN_POINT('Ctrl Pts',(-4.54505774438011,0.574911307367796,
5.33774599738179));
#40474=CARTESIAN_POINT('Ctrl Pts',(-4.58017335385184,0.653834841359911,
5.32263161637234));
#40475=CARTESIAN_POINT('',(-4.55425078118152,-1.2,5.26059291996045));
#40476=CARTESIAN_POINT('Ctrl Pts',(-4.55425078118152,-1.2,5.26059291996045));
#40477=CARTESIAN_POINT('Ctrl Pts',(-4.54944661068513,-1.13516581515213,
5.24931143219995));
#40478=CARTESIAN_POINT('Ctrl Pts',(-4.54291543586199,-1.03784493433457,
5.23409938464372));
#40479=CARTESIAN_POINT('Ctrl Pts',(-4.52921603512606,-0.776832222371542,
5.20276554770155));
#40480=CARTESIAN_POINT('Ctrl Pts',(-4.52760510110744,-0.724975474669047,
5.19917008419827));
#40481=CARTESIAN_POINT('Ctrl Pts',(-4.52544944337376,-0.653834841531101,
5.19430627077111));
#40482=CARTESIAN_POINT('Ctrl Pts',(-4.49074887227402,-1.30000000000891,
5.36814996080924));
#40483=CARTESIAN_POINT('Ctrl Pts',(-4.50169806910935,-1.28307064772788,
5.35016963244304));
#40484=CARTESIAN_POINT('Ctrl Pts',(-4.51244888709795,-1.26620626769394,
5.33200719241798));
#40485=CARTESIAN_POINT('Ctrl Pts',(-4.53220866142032,-1.23557956131176,
5.29981330135354));
#40486=CARTESIAN_POINT('Ctrl Pts',(-4.54172259503861,-1.22080224198256,
5.28426747325981));
#40487=CARTESIAN_POINT('Ctrl Pts',(-4.55425078118152,-1.2,5.26059291996044));
#40488=CARTESIAN_POINT('Origin',(0.,1.25,7.2));
#40489=CARTESIAN_POINT('Origin',(0.,1.2,7.2));
#40490=CARTESIAN_POINT('Origin',(0.,0.92691742076555,7.2));
#40491=CARTESIAN_POINT('Origin',(0.,0.653834841531101,7.2));
#40492=CARTESIAN_POINT('Origin',(0.,0.,7.2));
#40493=CARTESIAN_POINT('Origin',(0.,-0.653834841531101,7.2));
#40494=CARTESIAN_POINT('Origin',(0.,-0.926917420765551,7.2));
#40495=CARTESIAN_POINT('Origin',(0.,-1.2,7.2));
#40496=CARTESIAN_POINT('Origin',(0.,-1.25,7.2));
#40497=CARTESIAN_POINT('Ctrl Pts',(-4.48251875583975,-1.30000000000134,
4.88579874085794));
#40498=CARTESIAN_POINT('Ctrl Pts',(-4.50675280588359,-1.18514270861269,
4.92083760913291));
#40499=CARTESIAN_POINT('Ctrl Pts',(-4.51674956615302,-1.06847604194558,
4.95329826441664));
#40500=CARTESIAN_POINT('Ctrl Pts',(-4.50695309468148,-0.794772684000851,
5.02233268407423));
#40501=CARTESIAN_POINT('Ctrl Pts',(-4.44722735233531,-0.636309800095196,
5.05882272596845));
#40502=CARTESIAN_POINT('Ctrl Pts',(-4.39869447984843,-0.319434907277159,
5.11487935011235));
#40503=CARTESIAN_POINT('Ctrl Pts',(-4.35867257917745,-0.158333333333332,
5.13728168805474));
#40504=CARTESIAN_POINT('Ctrl Pts',(-4.37292795574814,0.158333333333335,
5.16801756977376));
#40505=CARTESIAN_POINT('Ctrl Pts',(-4.42777734501438,0.319434907277167,
5.17777988362547));
#40506=CARTESIAN_POINT('Ctrl Pts',(-4.50418204215396,0.636309800095206,
5.18141973571819));
#40507=CARTESIAN_POINT('Ctrl Pts',(-4.57842941556978,0.79477268400084,5.17777055683287));
#40508=CARTESIAN_POINT('Ctrl Pts',(-4.60940251578666,1.06847604194529,5.14987106382276));
#40509=CARTESIAN_POINT('Ctrl Pts',(-4.60766161389184,1.18514270861212,5.1319982609474));
#40510=CARTESIAN_POINT('Ctrl Pts',(-4.59077270268479,1.30000000000051,5.10832931194267));
#40511=CARTESIAN_POINT('Ctrl Pts',(-4.4699877389614,-1.30000000000134,4.88527001206655));
#40512=CARTESIAN_POINT('Ctrl Pts',(-4.49184486502941,-1.18514270861269,
4.9202749690669));
#40513=CARTESIAN_POINT('Ctrl Pts',(-4.50009761859441,-1.06847604194558,
4.95268677456364));
#40514=CARTESIAN_POINT('Ctrl Pts',(-4.48773430825989,-0.794772684000851,
5.02157383048891));
#40515=CARTESIAN_POINT('Ctrl Pts',(-4.42840755020082,-0.636309800095196,
5.05787895493427));
#40516=CARTESIAN_POINT('Ctrl Pts',(-4.37977441560886,-0.319434907277159,
5.11381935640681));
#40517=CARTESIAN_POINT('Ctrl Pts',(-4.34059295813843,-0.158333333333332,
5.13647657043832));
#40518=CARTESIAN_POINT('Ctrl Pts',(-4.35474635538549,0.158333333333335,
5.16675378497832));
#40519=CARTESIAN_POINT('Ctrl Pts',(-4.40861628637067,0.319434907277167,
5.17565787020395));
#40520=CARTESIAN_POINT('Ctrl Pts',(-4.48498896024595,0.636309800095206,
5.17877438660596));
#40521=CARTESIAN_POINT('Ctrl Pts',(-4.55880507325988,0.79477268400084,5.17508548891478));
#40522=CARTESIAN_POINT('Ctrl Pts',(-4.5923750883726,1.06847604194529,5.14740422222997));
#40523=CARTESIAN_POINT('Ctrl Pts',(-4.59241718007822,1.18514270861212,5.12973339070156));
#40524=CARTESIAN_POINT('Ctrl Pts',(-4.57797014783881,1.30000000000051,5.10637392230058));
#40525=CARTESIAN_POINT('Ctrl Pts',(-4.44513420311915,-1.30000000000135,
4.884733481637));
#40526=CARTESIAN_POINT('Ctrl Pts',(-4.46183589072991,-1.1851427086127,4.91840088906111));
#40527=CARTESIAN_POINT('Ctrl Pts',(-4.46637007123737,-1.06847604194559,
4.95000485425187));
#40528=CARTESIAN_POINT('Ctrl Pts',(-4.44873555975923,-0.794772684000863,
5.01824937184472));
#40529=CARTESIAN_POINT('Ctrl Pts',(-4.39084884309672,-0.636309800095208,
5.05638495800233));
#40530=CARTESIAN_POINT('Ctrl Pts',(-4.34217768828529,-0.319434907277166,
5.11265667084935));
#40531=CARTESIAN_POINT('Ctrl Pts',(-4.30445024732938,-0.158333333333335,
5.13496435846389));
#40532=CARTESIAN_POINT('Ctrl Pts',(-4.31843105932074,0.158333333333337,
5.16449168967078));
#40533=CARTESIAN_POINT('Ctrl Pts',(-4.37054787014169,0.319434907277172,
5.17256490560895));
#40534=CARTESIAN_POINT('Ctrl Pts',(-4.44686472935605,0.636309800095217,
5.17469957498278));
#40535=CARTESIAN_POINT('Ctrl Pts',(-4.51958918518332,0.794772684000857,
5.17002379850672));
#40536=CARTESIAN_POINT('Ctrl Pts',(-4.55836725083314,1.06847604194531,5.14277837197072));
#40537=CARTESIAN_POINT('Ctrl Pts',(-4.56202829741646,1.18514270861214,5.12568088174935));
#40538=CARTESIAN_POINT('Ctrl Pts',(-4.55256480283223,1.30000000000053,5.1032794369115));
#40539=CARTESIAN_POINT('Ctrl Pts',(-4.41974762070072,-1.30000000000138,
4.88408701534507));
#40540=CARTESIAN_POINT('Ctrl Pts',(-4.43179506545039,-1.18514270861273,
4.918318362789));
#40541=CARTESIAN_POINT('Ctrl Pts',(-4.43288914505467,-1.06847604194561,
4.95020390402413));
#40542=CARTESIAN_POINT('Ctrl Pts',(-4.41011222311145,-0.794772684000876,
5.0184466013386));
#40543=CARTESIAN_POINT('Ctrl Pts',(-4.35279015042126,-0.636309800095215,
5.05537792340058));
#40544=CARTESIAN_POINT('Ctrl Pts',(-4.30383441342919,-0.319434907277168,
5.11115473037836));
#40545=CARTESIAN_POINT('Ctrl Pts',(-4.26781347477672,-0.158333333333337,
5.13391900831901));
#40546=CARTESIAN_POINT('Ctrl Pts',(-4.28165805458559,0.158333333333339,
5.16286598935209));
#40547=CARTESIAN_POINT('Ctrl Pts',(-4.33200506651174,0.319434907277176,
5.17020279615525));
#40548=CARTESIAN_POINT('Ctrl Pts',(-4.40818044821254,0.636309800095224,
5.17103807912951));
#40549=CARTESIAN_POINT('Ctrl Pts',(-4.4795930281415,0.794772684000863,5.16458266721689));
#40550=CARTESIAN_POINT('Ctrl Pts',(-4.52365135936066,1.06847604194532,5.13766996221811));
#40551=CARTESIAN_POINT('Ctrl Pts',(-4.53102975534213,1.18514270861216,5.12126379080107));
#40552=CARTESIAN_POINT('Ctrl Pts',(-4.52671532824235,1.30000000000055,5.10010096074699));
#40553=CARTESIAN_POINT('Ctrl Pts',(-4.40650823227987,-1.30000000000138,
4.88380066054156));
#40554=CARTESIAN_POINT('Ctrl Pts',(-4.4158561187712,-1.18514270861273,4.91749327588164));
#40555=CARTESIAN_POINT('Ctrl Pts',(-4.41499837703178,-1.06847604194561,
4.94905656639272));
#40556=CARTESIAN_POINT('Ctrl Pts',(-4.38943977918113,-0.794772684000877,
5.01705491536285));
#40557=CARTESIAN_POINT('Ctrl Pts',(-4.33280187742144,-0.636309800095216,
5.0546567043112));
#40558=CARTESIAN_POINT('Ctrl Pts',(-4.28386852637352,-0.319434907277168,
5.11076200910592));
#40559=CARTESIAN_POINT('Ctrl Pts',(-4.24876292279781,-0.158333333333337,
5.13383636233795));
#40560=CARTESIAN_POINT('Ctrl Pts',(-4.26252502549056,0.158333333333339,
5.16244103234912));
#40561=CARTESIAN_POINT('Ctrl Pts',(-4.31179509598092,0.319434907277178,
5.16885016149766));
#40562=CARTESIAN_POINT('Ctrl Pts',(-4.38794127236082,0.636309800095226,
5.16922043239121));
#40563=CARTESIAN_POINT('Ctrl Pts',(-4.45892689575222,0.794772684000865,
5.16288729977276));
#40564=CARTESIAN_POINT('Ctrl Pts',(-4.50575118631774,1.06847604194532,5.13614182005032));
#40565=CARTESIAN_POINT('Ctrl Pts',(-4.51502186722484,1.18514270861216,5.11986708838312));
#40566=CARTESIAN_POINT('Ctrl Pts',(-4.5132947286642,1.30000000000055,5.09889475220289));
#40567=CARTESIAN_POINT('Ctrl Pts',(-4.4049564025435,-1.30000000000138,4.88378526077544));
#40568=CARTESIAN_POINT('Ctrl Pts',(-4.41398817097975,-1.18514270861273,
4.9174205499076));
#40569=CARTESIAN_POINT('Ctrl Pts',(-4.41290137938959,-1.06847604194561,
4.94894863383354));
#40570=CARTESIAN_POINT('Ctrl Pts',(-4.38701477553246,-0.794772684000877,
5.01691674930255));
#40571=CARTESIAN_POINT('Ctrl Pts',(-4.33045200394104,-0.636309800095216,
5.05457857089677));
#40572=CARTESIAN_POINT('Ctrl Pts',(-4.28152103228337,-0.319434907277168,
5.11072235315133));
#40573=CARTESIAN_POINT('Ctrl Pts',(-4.24652789605534,-0.158333333333337,
5.13385058759899));
#40574=CARTESIAN_POINT('Ctrl Pts',(-4.26028051529038,0.158333333333339,
5.16241615203963));
#40575=CARTESIAN_POINT('Ctrl Pts',(-4.30942099036749,0.319434907277178,
5.16870609135895));
#40576=CARTESIAN_POINT('Ctrl Pts',(-4.38556104175245,0.636309800095226,
5.16901160327323));
#40577=CARTESIAN_POINT('Ctrl Pts',(-4.45649411099206,0.794772684000865,
5.16268349828159));
#40578=CARTESIAN_POINT('Ctrl Pts',(-4.50364335604791,1.06847604194532,5.13595538713736));
#40579=CARTESIAN_POINT('Ctrl Pts',(-4.51313708026413,1.18514270861216,5.11969742432234));
#40580=CARTESIAN_POINT('Ctrl Pts',(-4.5117153675636,1.30000000000055,5.09875110763252));
#40581=CARTESIAN_POINT('Ctrl Pts',(-4.40224219033075,-1.30000000000138,
4.88376394744154));
#40582=CARTESIAN_POINT('Ctrl Pts',(-4.41072430196735,-1.18514270861273,
4.91731017602045));
#40583=CARTESIAN_POINT('Ctrl Pts',(-4.40923886277722,-1.06847604194561,
4.9487836208545));
#40584=CARTESIAN_POINT('Ctrl Pts',(-4.38278016467548,-0.794772684000877,
5.01670502955251));
#40585=CARTESIAN_POINT('Ctrl Pts',(-4.32634622956166,-0.636309800095216,
5.05446426311587));
#40586=CARTESIAN_POINT('Ctrl Pts',(-4.27741512031746,-0.319434907277168,
5.11066084001742));
#40587=CARTESIAN_POINT('Ctrl Pts',(-4.2426120790421,-0.158333333333337,
5.13385937190239));
#40588=CARTESIAN_POINT('Ctrl Pts',(-4.2563478462777,0.158333333333339,5.1623560768868));
#40589=CARTESIAN_POINT('Ctrl Pts',(-4.305269806891,0.319434907277178,5.16846781015905));
#40590=CARTESIAN_POINT('Ctrl Pts',(-4.38139923174149,0.636309800095227,
5.16865980598617));
#40591=CARTESIAN_POINT('Ctrl Pts',(-4.45223248915185,0.794772684000865,
5.16231031191246));
#40592=CARTESIAN_POINT('Ctrl Pts',(-4.49994911871515,1.06847604194532,5.13560794980462));
#40593=CARTESIAN_POINT('Ctrl Pts',(-4.50983384256683,1.18514270861216,5.11938217847402));
#40594=CARTESIAN_POINT('Ctrl Pts',(-4.50894852940762,1.30000000000055,5.09848909894929));
#40595=CARTESIAN_POINT('Ctrl Pts',(-4.39682707636092,-1.30000000000137,
4.88376677553948));
#40596=CARTESIAN_POINT('Ctrl Pts',(-4.4042228376766,-1.18514270861272,4.91717843866259));
#40597=CARTESIAN_POINT('Ctrl Pts',(-4.40194760492648,-1.06847604194561,
4.94856799844571));
#40598=CARTESIAN_POINT('Ctrl Pts',(-4.37434943114728,-0.794772684000875,
5.01641269776876));
#40599=CARTESIAN_POINT('Ctrl Pts',(-4.31815519215306,-0.636309800095215,
5.05430786254906));
#40600=CARTESIAN_POINT('Ctrl Pts',(-4.2692143702594,-0.319434907277168,
5.11057919803083));
#40601=CARTESIAN_POINT('Ctrl Pts',(-4.23478747864304,-0.158333333333337,
5.13390345071257));
#40602=CARTESIAN_POINT('Ctrl Pts',(-4.24848968363826,0.158333333333339,
5.16226517782403));
#40603=CARTESIAN_POINT('Ctrl Pts',(-4.29698668137947,0.319434907277177,
5.16806751836705));
#40604=CARTESIAN_POINT('Ctrl Pts',(-4.3730885201456,0.636309800095226,5.16800900169859));
#40605=CARTESIAN_POINT('Ctrl Pts',(-4.44369767060591,0.794772684000865,
5.1615231738282));
#40606=CARTESIAN_POINT('Ctrl Pts',(-4.49254607107023,1.06847604194532,5.13485966923599));
#40607=CARTESIAN_POINT('Ctrl Pts',(-4.50321621625043,1.18514270861216,5.11871051274717));
#40608=CARTESIAN_POINT('Ctrl Pts',(-4.50341184406145,1.30000000000055,5.09795384292729));
#40609=CARTESIAN_POINT('Ctrl Pts',(-4.38606558456593,-1.30000000000137,
4.8840266581289));
#40610=CARTESIAN_POINT('Ctrl Pts',(-4.39142503744879,-1.18514270861272,
4.9176134919098));
#40611=CARTESIAN_POINT('Ctrl Pts',(-4.38765033200399,-1.06847604194561,
4.94909627641851));
#40612=CARTESIAN_POINT('Ctrl Pts',(-4.35782827428032,-0.794772684000875,
5.01696703201057));
#40613=CARTESIAN_POINT('Ctrl Pts',(-4.30195661046983,-0.636309800095214,
5.0546304847714));
#40614=CARTESIAN_POINT('Ctrl Pts',(-4.25285778594573,-0.319434907277167,
5.11058605655013));
#40615=CARTESIAN_POINT('Ctrl Pts',(-4.21903395867086,-0.158333333333337,
5.13363428064143));
#40616=CARTESIAN_POINT('Ctrl Pts',(-4.23266654153631,0.158333333333339,
5.1617335078417));
#40617=CARTESIAN_POINT('Ctrl Pts',(-4.28053461320322,0.319434907277177,
5.16773276128116));
#40618=CARTESIAN_POINT('Ctrl Pts',(-4.35656350255669,0.636309800095225,
5.16708177445095));
#40619=CARTESIAN_POINT('Ctrl Pts',(-4.42647160968918,0.794772684000862,
5.15932956521396));
#40620=CARTESIAN_POINT('Ctrl Pts',(-4.4775477256098,1.06847604194531,5.13260801730426));
#40621=CARTESIAN_POINT('Ctrl Pts',(-4.4898161662824,1.18514270861216,5.1167254228346));
#40622=CARTESIAN_POINT('Ctrl Pts',(-4.49224408960217,1.30000000000055,5.09652700185447));
#40623=CARTESIAN_POINT('Ctrl Pts',(-4.37060167768334,-1.30000000000137,
4.88410602866374));
#40624=CARTESIAN_POINT('Ctrl Pts',(-4.37292250382272,-1.18514270861271,
4.91752711815292));
#40625=CARTESIAN_POINT('Ctrl Pts',(-4.36694158973788,-1.0684760419456,4.94893796562093));
#40626=CARTESIAN_POINT('Ctrl Pts',(-4.33394580104886,-0.794772684000867,
5.01685924577397));
#40627=CARTESIAN_POINT('Ctrl Pts',(-4.27876641146177,-0.636309800095212,
5.05493001675094));
#40628=CARTESIAN_POINT('Ctrl Pts',(-4.22965716001968,-0.319434907277167,
5.11114702069444));
#40629=CARTESIAN_POINT('Ctrl Pts',(-4.19690370361186,-0.158333333333336,
5.134513836664));
#40630=CARTESIAN_POINT('Ctrl Pts',(-4.21041567571181,0.158333333333339,
5.16217342131387));
#40631=CARTESIAN_POINT('Ctrl Pts',(-4.25703639618286,0.319434907277176,
5.16724835790094));
#40632=CARTESIAN_POINT('Ctrl Pts',(-4.33294485775093,0.636309800095223,
5.16577871662493));
#40633=CARTESIAN_POINT('Ctrl Pts',(-4.40219369493682,0.794772684000861,
5.15757132101997));
#40634=CARTESIAN_POINT('Ctrl Pts',(-4.45647104436528,1.06847604194531,5.13082793493229));
#40635=CARTESIAN_POINT('Ctrl Pts',(-4.47097018224745,1.18514270861215,5.11510038944369));
#40636=CARTESIAN_POINT('Ctrl Pts',(-4.47647380461819,1.30000000000054,5.09522151936374));
#40637=CARTESIAN_POINT('Ctrl Pts',(-4.35196499893507,-1.30000000000136,
4.88399187949457));
#40638=CARTESIAN_POINT('Ctrl Pts',(-4.35056153135029,-1.18514270861271,
4.91699062520585));
#40639=CARTESIAN_POINT('Ctrl Pts',(-4.34188287937219,-1.0684760419456,4.94817247295909));
#40640=CARTESIAN_POINT('Ctrl Pts',(-4.3050263258002,-0.79477268400087,5.01601138142398));
#40641=CARTESIAN_POINT('Ctrl Pts',(-4.25072828537927,-0.636309800095212,
5.05472404794897));
#40642=CARTESIAN_POINT('Ctrl Pts',(-4.20167033752839,-0.319434907277167,
5.11145251868633));
#40643=CARTESIAN_POINT('Ctrl Pts',(-4.17027754713746,-0.158333333333336,
5.13542659898148));
#40644=CARTESIAN_POINT('Ctrl Pts',(-4.18369951910936,0.158333333333338,
5.16273757843257));
#40645=CARTESIAN_POINT('Ctrl Pts',(-4.22883734848563,0.319434907277175,
5.16678173691335));
#40646=CARTESIAN_POINT('Ctrl Pts',(-4.30457682258443,0.636309800095222,
5.16424312854174));
#40647=CARTESIAN_POINT('Ctrl Pts',(-4.37296413646412,0.794772684000861,
5.15522516137196));
#40648=CARTESIAN_POINT('Ctrl Pts',(-4.43103930909429,1.06847604194531,5.1282867857786));
#40649=CARTESIAN_POINT('Ctrl Pts',(-4.44820285993171,1.18514270861215,5.11269495333857));
#40650=CARTESIAN_POINT('Ctrl Pts',(-4.45739137127217,1.30000000000054,5.09317191308771));
#40651=CARTESIAN_POINT('Ctrl Pts',(-4.32737417007851,-1.30000000000136,
4.88468811680626));
#40652=CARTESIAN_POINT('Ctrl Pts',(-4.32124043958264,-1.18514270861271,
4.91789151964559));
#40653=CARTESIAN_POINT('Ctrl Pts',(-4.30911969341762,-1.0684760419456,4.94927348967718));
#40654=CARTESIAN_POINT('Ctrl Pts',(-4.26728714113541,-0.794772684000867,
5.01756424422933));
#40655=CARTESIAN_POINT('Ctrl Pts',(-4.2140559268287,-0.63630980009521,5.05677413527469));
#40656=CARTESIAN_POINT('Ctrl Pts',(-4.1648465877658,-0.319434907277165,
5.11348677088921));
#40657=CARTESIAN_POINT('Ctrl Pts',(-4.13494732008885,-0.158333333333336,
5.13724902899869));
#40658=CARTESIAN_POINT('Ctrl Pts',(-4.14806315658605,0.158333333333338,
5.16352102529718));
#40659=CARTESIAN_POINT('Ctrl Pts',(-4.19122796504154,0.319434907277177,
5.16619566615263));
#40660=CARTESIAN_POINT('Ctrl Pts',(-4.26684838183568,0.636309800095222,
5.16266130049346));
#40661=CARTESIAN_POINT('Ctrl Pts',(-4.33434492497626,0.794772684000858,
5.15357916495107));
#40662=CARTESIAN_POINT('Ctrl Pts',(-4.39758617759598,1.06847604194531,5.12669405868028));
#40663=CARTESIAN_POINT('Ctrl Pts',(-4.4183085151726,1.18514270861215,5.11124790801923));
#40664=CARTESIAN_POINT('Ctrl Pts',(-4.43237839538611,1.30000000000054,5.09199317301038));
#40665=CARTESIAN_POINT('Ctrl Pts',(-4.30272254767684,-1.30000000000136,
4.88526757993008));
#40666=CARTESIAN_POINT('Ctrl Pts',(-4.29183336543115,-1.18514270861271,
4.91860694219569));
#40667=CARTESIAN_POINT('Ctrl Pts',(-4.27623603569334,-1.06847604194559,
4.95009040893693));
#40668=CARTESIAN_POINT('Ctrl Pts',(-4.22932632119549,-0.794772684000859,
5.01853602542309));
#40669=CARTESIAN_POINT('Ctrl Pts',(-4.17698541530236,-0.636309800095208,
5.05771031248182));
#40670=CARTESIAN_POINT('Ctrl Pts',(-4.12765193878455,-0.319434907277166,
5.11448930759117));
#40671=CARTESIAN_POINT('Ctrl Pts',(-4.09939356743927,-0.158333333333336,
5.13843780656823));
#40672=CARTESIAN_POINT('Ctrl Pts',(-4.11244871156721,0.158333333333338,
5.16449616510372));
#40673=CARTESIAN_POINT('Ctrl Pts',(-4.15396287852574,0.319434907277175,
5.16698457503574));
#40674=CARTESIAN_POINT('Ctrl Pts',(-4.2294800310024,0.63630980009522,5.16251350014463));
#40675=CARTESIAN_POINT('Ctrl Pts',(-4.29575238020146,0.794772684000857,
5.1521719621219));
#40676=CARTESIAN_POINT('Ctrl Pts',(-4.36396151425919,1.06847604194531,5.12463779817001));
#40677=CARTESIAN_POINT('Ctrl Pts',(-4.38817637480601,1.18514270861215,5.10910488156731));
#40678=CARTESIAN_POINT('Ctrl Pts',(-4.40708088916356,1.30000000000054,5.08995756769537));
#40679=CARTESIAN_POINT('Ctrl Pts',(-4.27815205391509,-1.30000000000136,
4.88612008534165));
#40680=CARTESIAN_POINT('Ctrl Pts',(-4.26247420431945,-1.18514270861271,
4.91954146733436));
#40681=CARTESIAN_POINT('Ctrl Pts',(-4.24343209635956,-1.0684760419456,4.95125381830094));
#40682=CARTESIAN_POINT('Ctrl Pts',(-4.19166890777269,-0.794772684000865,
5.02056748950684));
#40683=CARTESIAN_POINT('Ctrl Pts',(-4.14075814958985,-0.636309800095208,
5.06129138348443));
#40684=CARTESIAN_POINT('Ctrl Pts',(-4.09139626798141,-0.319434907277164,
5.1184462415078));
#40685=CARTESIAN_POINT('Ctrl Pts',(-4.06445906870166,-0.158333333333335,
5.14166936941548));
#40686=CARTESIAN_POINT('Ctrl Pts',(-4.077222140461,0.158333333333337,5.16683024787989));
#40687=CARTESIAN_POINT('Ctrl Pts',(-4.11699151010801,0.319434907277173,
5.16882586619956));
#40688=CARTESIAN_POINT('Ctrl Pts',(-4.19221010102953,0.636309800095218,
5.16280403349833));
#40689=CARTESIAN_POINT('Ctrl Pts',(-4.25705109432503,0.794772684000854,
5.15054725916305));
#40690=CARTESIAN_POINT('Ctrl Pts',(-4.33027708204415,1.06847604194531,5.12250447261737));
#40691=CARTESIAN_POINT('Ctrl Pts',(-4.3580759818353,1.18514270861215,5.1071645586451));
#40692=CARTESIAN_POINT('Ctrl Pts',(-4.38197696462424,1.30000000000054,5.08862341390855));
#40693=CARTESIAN_POINT('Ctrl Pts',(-4.25367312510128,-1.30000000000136,
4.88733406444623));
#40694=CARTESIAN_POINT('Ctrl Pts',(-4.23349817359138,-1.1851427086127,4.92168444828486));
#40695=CARTESIAN_POINT('Ctrl Pts',(-4.21113464578801,-1.06847604194559,
4.95398061417029));
#40696=CARTESIAN_POINT('Ctrl Pts',(-4.15441437369286,-0.79477268400086,
5.02384556377463));
#40697=CARTESIAN_POINT('Ctrl Pts',(-4.10397583550923,-0.636309800095207,
5.06331287038023));
#40698=CARTESIAN_POINT('Ctrl Pts',(-4.05453479166089,-0.319434907277165,
5.12067245588504));
#40699=CARTESIAN_POINT('Ctrl Pts',(-4.02967050652154,-0.158333333333335,
5.14532610117804));
#40700=CARTESIAN_POINT('Ctrl Pts',(-4.04233335055355,0.158333333333337,
5.17017149405673));
#40701=CARTESIAN_POINT('Ctrl Pts',(-4.07995175634696,0.319434907277172,
5.17049886858399));
#40702=CARTESIAN_POINT('Ctrl Pts',(-4.15500017782648,0.636309800095217,
5.16347129713085));
#40703=CARTESIAN_POINT('Ctrl Pts',(-4.21902871529604,0.794772684000855,
5.1514565662729));
#40704=CARTESIAN_POINT('Ctrl Pts',(-4.29723796226783,1.0684760419453,5.12277114120179));
#40705=CARTESIAN_POINT('Ctrl Pts',(-4.32846609096306,1.18514270861214,5.10706392718239));
#40706=CARTESIAN_POINT('Ctrl Pts',(-4.35706846327762,1.30000000000053,5.08806635675711));
#40707=CARTESIAN_POINT('Ctrl Pts',(-4.22347137391488,-1.30000000000136,
4.88985984435287));
#40708=CARTESIAN_POINT('Ctrl Pts',(-4.19726403779595,-1.18514270861271,
4.92425217904836));
#40709=CARTESIAN_POINT('Ctrl Pts',(-4.17057834860845,-1.06847604194559,
4.95683493041622));
#40710=CARTESIAN_POINT('Ctrl Pts',(-4.10782397684903,-0.79477268400086,
5.02792710474016));
#40711=CARTESIAN_POINT('Ctrl Pts',(-4.05936422436221,-0.636309800095202,
5.06979779123566));
#40712=CARTESIAN_POINT('Ctrl Pts',(-4.00989238454398,-0.31943490727716,
5.12764546106457));
#40713=CARTESIAN_POINT('Ctrl Pts',(-3.98654644901798,-0.158333333333334,
5.15103547557789));
#40714=CARTESIAN_POINT('Ctrl Pts',(-3.99873859858878,0.158333333333336,
5.1745258202819));
#40715=CARTESIAN_POINT('Ctrl Pts',(-4.0341451811996,0.319434907277171,5.17421957459374));
#40716=CARTESIAN_POINT('Ctrl Pts',(-4.10871941292505,0.636309800095212,
5.16504821135669));
#40717=CARTESIAN_POINT('Ctrl Pts',(-4.17095302500774,0.794772684000845,
5.150729827345));
#40718=CARTESIAN_POINT('Ctrl Pts',(-4.25523270922204,1.06847604194529,5.12075283767295));
#40719=CARTESIAN_POINT('Ctrl Pts',(-4.29082094784555,1.18514270861214,5.10486131848044));
#40720=CARTESIAN_POINT('Ctrl Pts',(-4.32551587266625,1.30000000000053,5.08605420816752));
#40721=CARTESIAN_POINT('Ctrl Pts',(-4.19598697828295,-1.30000000000135,
4.89148680791286));
#40722=CARTESIAN_POINT('Ctrl Pts',(-4.1646778729705,-1.1851427086127,4.92683910406031));
#40723=CARTESIAN_POINT('Ctrl Pts',(-4.13427147073223,-1.06847604194559,
4.96014889185388));
#40724=CARTESIAN_POINT('Ctrl Pts',(-4.06611202346847,-0.794772684000858,
5.03238256235729));
#40725=CARTESIAN_POINT('Ctrl Pts',(-4.01854562515569,-0.636309800095203,
5.07387317587653));
#40726=CARTESIAN_POINT('Ctrl Pts',(-3.96924679223899,-0.319434907277162,
5.13265453529849));
#40727=CARTESIAN_POINT('Ctrl Pts',(-3.94828394958136,-0.158333333333334,
5.1576571823155));
#40728=CARTESIAN_POINT('Ctrl Pts',(-3.96041752040512,0.158333333333336,
5.18102679218327));
#40729=CARTESIAN_POINT('Ctrl Pts',(-3.99345908856316,0.31943490727717,5.17927584842867));
#40730=CARTESIAN_POINT('Ctrl Pts',(-4.06758484757638,0.636309800095213,
5.16833686890515));
#40731=CARTESIAN_POINT('Ctrl Pts',(-4.12834371072759,0.794772684000849,
5.15257450864102));
#40732=CARTESIAN_POINT('Ctrl Pts',(-4.2181230949946,1.0684760419453,5.12153335051156));
#40733=CARTESIAN_POINT('Ctrl Pts',(-4.25763397221813,1.18514270861214,5.1054019255452));
#40734=CARTESIAN_POINT('Ctrl Pts',(-4.29779355787003,1.30000000000053,5.08657564277847));
#40735=CARTESIAN_POINT('Ctrl Pts',(-4.17817781145185,-1.30000000000135,
4.89391064073081));
#40736=CARTESIAN_POINT('Ctrl Pts',(-4.14343156900407,-1.1851427086127,4.9298229981819));
#40737=CARTESIAN_POINT('Ctrl Pts',(-4.11053739623518,-1.06847604194558,
4.96361408938916));
#40738=CARTESIAN_POINT('Ctrl Pts',(-4.03882392814598,-0.794772684000855,
5.03677772058128));
#40739=CARTESIAN_POINT('Ctrl Pts',(-3.99217793424401,-0.636309800095202,
5.07891426934365));
#40740=CARTESIAN_POINT('Ctrl Pts',(-3.94275628542362,-0.319434907277162,
5.13770211516119));
#40741=CARTESIAN_POINT('Ctrl Pts',(-3.92269078973397,-0.158333333333334,
5.16192232746968));
#40742=CARTESIAN_POINT('Ctrl Pts',(-3.93459308666009,0.158333333333336,
5.18469929682841));
#40743=CARTESIAN_POINT('Ctrl Pts',(-3.9664220559315,0.319434907277171,5.18295439880769));
#40744=CARTESIAN_POINT('Ctrl Pts',(-4.04037059975343,0.636309800095213,
5.17117604923734));
#40745=CARTESIAN_POINT('Ctrl Pts',(-4.10022631076594,0.794772684000849,
5.15474803524041));
#40746=CARTESIAN_POINT('Ctrl Pts',(-4.19346831247043,1.0684760419453,5.12236157619796));
#40747=CARTESIAN_POINT('Ctrl Pts',(-4.23543357124736,1.18514270861213,5.10556374198919));
#40748=CARTESIAN_POINT('Ctrl Pts',(-4.27900308121998,1.30000000000052,5.08598697165455));
#40749=CARTESIAN_POINT('Ctrl Pts',(-4.16614832183943,-1.30000000000135,
4.89515416503372));
#40750=CARTESIAN_POINT('Ctrl Pts',(-4.12927305326624,-1.1851427086127,4.93187374670616));
#40751=CARTESIAN_POINT('Ctrl Pts',(-4.09481646701293,-1.06847604194558,
4.96624192261934));
#40752=CARTESIAN_POINT('Ctrl Pts',(-4.02080249976618,-0.794772684000856,
5.04020706660765));
#40753=CARTESIAN_POINT('Ctrl Pts',(-3.97448924330781,-0.636309800095203,
5.0820240583604));
#40754=CARTESIAN_POINT('Ctrl Pts',(-3.92502015216261,-0.319434907277163,
5.14089736102373));
#40755=CARTESIAN_POINT('Ctrl Pts',(-3.90579764168114,-0.158333333333334,
5.16522599392556));
#40756=CARTESIAN_POINT('Ctrl Pts',(-3.91763888697422,0.158333333333336,
5.18786464483484));
#40757=CARTESIAN_POINT('Ctrl Pts',(-3.94860628975023,0.31943490727717,5.18601843378387));
#40758=CARTESIAN_POINT('Ctrl Pts',(-4.02239140907987,0.636309800095213,
5.1735766603289));
#40759=CARTESIAN_POINT('Ctrl Pts',(-4.08155211767191,0.794772684000849,
5.15644136256273));
#40760=CARTESIAN_POINT('Ctrl Pts',(-4.1771132744239,1.0684760419453,5.1231992607686));
#40761=CARTESIAN_POINT('Ctrl Pts',(-4.220744319771,1.18514270861214,5.10604551223169));
#40762=CARTESIAN_POINT('Ctrl Pts',(-4.26664152659707,1.30000000000053,5.0861272892833));
#40763=CARTESIAN_POINT('Ctrl Pts',(-4.1508669168539,-1.30000000000135,4.89606494834189));
#40764=CARTESIAN_POINT('Ctrl Pts',(-4.11107919495639,-1.1851427086127,4.93312453755988));
#40765=CARTESIAN_POINT('Ctrl Pts',(-4.07455046284514,-1.06847604194559,
4.9678928592167));
#40766=CARTESIAN_POINT('Ctrl Pts',(-3.99769070248542,-0.794772684000857,
5.04292135118991));
#40767=CARTESIAN_POINT('Ctrl Pts',(-3.95237996500392,-0.636309800095203,
5.08586704224943));
#40768=CARTESIAN_POINT('Ctrl Pts',(-3.90310151350184,-0.319434907277162,
5.1455008236609));
#40769=CARTESIAN_POINT('Ctrl Pts',(-3.88492029224199,-0.158333333333334,
5.16994987776997));
#40770=CARTESIAN_POINT('Ctrl Pts',(-3.89655168321942,0.158333333333336,
5.19206004283178));
#40771=CARTESIAN_POINT('Ctrl Pts',(-3.9261827815684,0.319434907277171,5.1894116045783));
#40772=CARTESIAN_POINT('Ctrl Pts',(-3.99952326972462,0.636309800095214,
5.17544516685783));
#40773=CARTESIAN_POINT('Ctrl Pts',(-4.05759908040726,0.794772684000849,
5.15669555841508));
#40774=CARTESIAN_POINT('Ctrl Pts',(-4.15617967915481,1.0684760419453,5.12274651323053));
#40775=CARTESIAN_POINT('Ctrl Pts',(-4.20203738654327,1.18514270861213,5.10559522792422));
#40776=CARTESIAN_POINT('Ctrl Pts',(-4.25108091289353,1.30000000000052,5.08598794103589));
#40777=CARTESIAN_POINT('Ctrl Pts',(-4.13323139050191,-1.30000000000135,
4.89899172467419));
#40778=CARTESIAN_POINT('Ctrl Pts',(-4.09014474267955,-1.1851427086127,4.93699722021868));
#40779=CARTESIAN_POINT('Ctrl Pts',(-4.05121499879604,-1.06847604194558,
4.97248672392271));
#40780=CARTESIAN_POINT('Ctrl Pts',(-3.97088278224124,-0.794772684000856,
5.04866213265584));
#40781=CARTESIAN_POINT('Ctrl Pts',(-3.92632338133767,-0.636309800095201,
5.09175632655176));
#40782=CARTESIAN_POINT('Ctrl Pts',(-3.87691545645197,-0.319434907277162,
5.15138050949605));
#40783=CARTESIAN_POINT('Ctrl Pts',(-3.85972265622446,-0.158333333333333,
5.17531708798847));
#40784=CARTESIAN_POINT('Ctrl Pts',(-3.87114337975094,0.158333333333336,
5.19692904080684));
#40785=CARTESIAN_POINT('Ctrl Pts',(-3.89949164386545,0.31943490727717,5.19410951983121));
#40786=CARTESIAN_POINT('Ctrl Pts',(-3.97270307504151,0.636309800095212,
5.17951539476134));
#40787=CARTESIAN_POINT('Ctrl Pts',(-4.03003677717091,0.794772684000847,
5.16065805954507));
#40788=CARTESIAN_POINT('Ctrl Pts',(-4.13208575882067,1.06847604194529,5.12540031643046));
#40789=CARTESIAN_POINT('Ctrl Pts',(-4.18036558146868,1.18514270861213,5.1074772650306));
#40790=CARTESIAN_POINT('Ctrl Pts',(-4.23275200389592,1.30000000000052,5.08689293279707));
#40791=CARTESIAN_POINT('Ctrl Pts',(-4.10625889988844,-1.30000000000135,
4.90204030255314));
#40792=CARTESIAN_POINT('Ctrl Pts',(-4.05808112442856,-1.1851427086127,4.94104135877227));
#40793=CARTESIAN_POINT('Ctrl Pts',(-4.01551425518549,-1.06847604194559,
4.97747714274429));
#40794=CARTESIAN_POINT('Ctrl Pts',(-3.93013858757992,-0.794772684000858,
5.05572480060138));
#40795=CARTESIAN_POINT('Ctrl Pts',(-3.88710540052421,-0.636309800095203,
5.10008878779615));
#40796=CARTESIAN_POINT('Ctrl Pts',(-3.83817100406078,-0.319434907277162,
5.16133735665563));
#40797=CARTESIAN_POINT('Ctrl Pts',(-3.82328588369641,-0.158333333333334,
5.18648529424092));
#40798=CARTESIAN_POINT('Ctrl Pts',(-3.83439947201774,0.158333333333336,
5.20739268922943));
#40799=CARTESIAN_POINT('Ctrl Pts',(-3.86001471967997,0.31943490727717,5.20245646788849));
#40800=CARTESIAN_POINT('Ctrl Pts',(-3.93236777784375,0.636309800095212,
5.18521180474951));
#40801=CARTESIAN_POINT('Ctrl Pts',(-3.98813117380777,0.79477268400085,5.16473826409429));
#40802=CARTESIAN_POINT('Ctrl Pts',(-4.09528276000506,1.06847604194529,5.12731890285593));
#40803=CARTESIAN_POINT('Ctrl Pts',(-4.14728494579063,1.18514270861213,5.10855990412802));
#40804=CARTESIAN_POINT('Ctrl Pts',(-4.20490736605451,1.30000000000052,5.08723936162831));
#40805=CARTESIAN_POINT('Ctrl Pts',(-4.07668616191916,-1.30000000000134,
4.90655222882955));
#40806=CARTESIAN_POINT('Ctrl Pts',(-4.02302103967041,-1.18514270861269,
4.94721000383966));
#40807=CARTESIAN_POINT('Ctrl Pts',(-3.97655137533068,-1.06847604194558,
4.98511937718202));
#40808=CARTESIAN_POINT('Ctrl Pts',(-3.88582010169789,-0.794772684000854,
5.0663482556785));
#40809=CARTESIAN_POINT('Ctrl Pts',(-3.84484404947985,-0.636309800095198,
5.11281258867805));
#40810=CARTESIAN_POINT('Ctrl Pts',(-3.79596540058121,-0.319434907277159,
5.17472528225949));
#40811=CARTESIAN_POINT('Ctrl Pts',(-3.7823500380607,-0.158333333333333,
5.19817022424681));
#40812=CARTESIAN_POINT('Ctrl Pts',(-3.79296246664124,0.158333333333335,
5.21799372334928));
#40813=CARTESIAN_POINT('Ctrl Pts',(-3.81658630793045,0.319434907277169,
5.21329214661253));
#40814=CARTESIAN_POINT('Ctrl Pts',(-3.88831191200828,0.636309800095209,
5.19395864824761));
#40815=CARTESIAN_POINT('Ctrl Pts',(-3.94196785883248,0.794772684000841,
5.1708896797082));
#40816=CARTESIAN_POINT('Ctrl Pts',(-4.05479149099295,1.06847604194529,5.13099102890868));
#40817=CARTESIAN_POINT('Ctrl Pts',(-4.11096942696579,1.18514270861213,5.1113232273092));
#40818=CARTESIAN_POINT('Ctrl Pts',(-4.17448812907675,1.30000000000052,5.08925827165065));
#40819=CARTESIAN_POINT('Ctrl Pts',(-4.04716803737985,-1.30000000000135,
4.91112623751931));
#40820=CARTESIAN_POINT('Ctrl Pts',(-3.9881710480236,-1.1851427086127,4.95362920167102));
#40821=CARTESIAN_POINT('Ctrl Pts',(-3.93793472154304,-1.06847604194558,
4.99319008793396));
#40822=CARTESIAN_POINT('Ctrl Pts',(-3.84211764143791,-0.794772684000852,
5.07778686084563));
#40823=CARTESIAN_POINT('Ctrl Pts',(-3.80313764148869,-0.636309800095198,
5.12615186704337));
#40824=CARTESIAN_POINT('Ctrl Pts',(-3.75484016665707,-0.319434907277159,
5.18987579309421));
#40825=CARTESIAN_POINT('Ctrl Pts',(-3.74336735637233,-0.158333333333332,
5.21365277657516));
#40826=CARTESIAN_POINT('Ctrl Pts',(-3.75358889560144,0.158333333333335,
5.23271082624441));
#40827=CARTESIAN_POINT('Ctrl Pts',(-3.77449313381615,0.319434907277168,
5.22659823861587));
#40828=CARTESIAN_POINT('Ctrl Pts',(-3.84522054790868,0.636309800095208,
5.20453295999464));
#40829=CARTESIAN_POINT('Ctrl Pts',(-3.89696787912242,0.794772684000843,
5.17961206984491));
#40830=CARTESIAN_POINT('Ctrl Pts',(-4.01503333068514,1.06847604194529,5.13639017041117));
#40831=CARTESIAN_POINT('Ctrl Pts',(-4.07510406689772,1.18514270861212,5.11518154429486));
#40832=CARTESIAN_POINT('Ctrl Pts',(-4.14413938009749,1.30000000000051,5.0914734507979));
#40833=CARTESIAN_POINT('Ctrl Pts',(-4.02686024311897,-1.30000000000134,
4.91538283693451));
#40834=CARTESIAN_POINT('Ctrl Pts',(-3.96400923923139,-1.1851427086127,4.95925335681388));
#40835=CARTESIAN_POINT('Ctrl Pts',(-3.91108111387555,-1.06847604194558,
5.00009937316502));
#40836=CARTESIAN_POINT('Ctrl Pts',(-3.81173039054196,-0.794772684000857,
5.08747463395353));
#40837=CARTESIAN_POINT('Ctrl Pts',(-3.77482876016749,-0.636309800095199,
5.13859565593173));
#40838=CARTESIAN_POINT('Ctrl Pts',(-3.72633243605006,-0.319434907277159,
5.20226275136205));
#40839=CARTESIAN_POINT('Ctrl Pts',(-3.71468118444881,-0.158333333333333,
5.22245677431171));
#40840=CARTESIAN_POINT('Ctrl Pts',(-3.72435431344552,0.158333333333335,
5.2404040033757));
#40841=CARTESIAN_POINT('Ctrl Pts',(-3.74458434460951,0.319434907277169,
5.23620771392481));
#40842=CARTESIAN_POINT('Ctrl Pts',(-3.81501324700601,0.636309800095209,
5.21306881395242));
#40843=CARTESIAN_POINT('Ctrl Pts',(-3.86503295408965,0.794772684000844,
5.18590559368825));
#40844=CARTESIAN_POINT('Ctrl Pts',(-3.9868511233865,1.06847604194529,5.14013147276438));
#40845=CARTESIAN_POINT('Ctrl Pts',(-4.04973779600462,1.18514270861212,5.11779749257155));
#40846=CARTESIAN_POINT('Ctrl Pts',(-4.12278056956027,1.30000000000051,5.09294345303549));
#40847=CARTESIAN_POINT('Ctrl Pts',(-4.01232252275008,-1.30000000000134,
4.91808539201452));
#40848=CARTESIAN_POINT('Ctrl Pts',(-3.94726047781966,-1.18514270861269,
4.96365346105024));
#40849=CARTESIAN_POINT('Ctrl Pts',(-3.89264513091886,-1.06847604194558,
5.00556768762124));
#40850=CARTESIAN_POINT('Ctrl Pts',(-3.79060671611871,-0.794772684000853,
5.09395682887023));
#40851=CARTESIAN_POINT('Ctrl Pts',(-3.75355156744856,-0.636309800095198,
5.14338738082634));
#40852=CARTESIAN_POINT('Ctrl Pts',(-3.70466736151699,-0.319434907277159,
5.20626768635415));
#40853=CARTESIAN_POINT('Ctrl Pts',(-3.69371769727687,-0.158333333333333,
5.22571268347603));
#40854=CARTESIAN_POINT('Ctrl Pts',(-3.70361224364535,0.158333333333335,
5.2441977360215));
#40855=CARTESIAN_POINT('Ctrl Pts',(-3.72370836064582,0.319434907277169,
5.24208037810435));
#40856=CARTESIAN_POINT('Ctrl Pts',(-3.79427085791425,0.636309800095209,
5.21921036128222));
#40857=CARTESIAN_POINT('Ctrl Pts',(-3.8431400259095,0.794772684000843,5.19086038002993));
#40858=CARTESIAN_POINT('Ctrl Pts',(-3.96751938670524,1.06847604194529,5.14371082198786));
#40859=CARTESIAN_POINT('Ctrl Pts',(-4.03228901928671,1.18514270861212,5.12068238772968));
#40860=CARTESIAN_POINT('Ctrl Pts',(-4.10798906787067,1.30000000000051,5.09503481582645));
#40861=CARTESIAN_POINT('Ctrl Pts',(-3.99512086302667,-1.30000000000134,
4.92222147175269));
#40862=CARTESIAN_POINT('Ctrl Pts',(-3.92707232624567,-1.18514270861269,
4.96998997195516));
#40863=CARTESIAN_POINT('Ctrl Pts',(-3.87008579662005,-1.06847604194558,
5.01313728134372));
#40864=CARTESIAN_POINT('Ctrl Pts',(-3.76399096254472,-0.794772684000854,
5.10214032237463));
#40865=CARTESIAN_POINT('Ctrl Pts',(-3.72603399380682,-0.636309800095198,
5.14824835584075));
#40866=CARTESIAN_POINT('Ctrl Pts',(-3.67610766531818,-0.319434907277159,
5.20923720889898));
#40867=CARTESIAN_POINT('Ctrl Pts',(-3.6661554730306,-0.158333333333333,
5.22783807506664));
#40868=CARTESIAN_POINT('Ctrl Pts',(-3.67599170976141,0.158333333333335,
5.2462475697323));
#40869=CARTESIAN_POINT('Ctrl Pts',(-3.69515914265524,0.319434907277168,
5.24522806832112));
#40870=CARTESIAN_POINT('Ctrl Pts',(-3.76638610152451,0.636309800095208,
5.22342487136686));
#40871=CARTESIAN_POINT('Ctrl Pts',(-3.81538419450183,0.794772684000843,
5.19662287275888));
#40872=CARTESIAN_POINT('Ctrl Pts',(-3.94378191370543,1.06847604194529,5.14863512557791));
#40873=CARTESIAN_POINT('Ctrl Pts',(-4.01108528305494,1.18514270861213,5.12465321506705));
#40874=CARTESIAN_POINT('Ctrl Pts',(-4.09011340671507,1.30000000000051,5.09746151167872));
#40875=CARTESIAN_POINT('Ctrl Pts',(-3.983352778511,-1.30000000000134,4.92491429713353));
#40876=CARTESIAN_POINT('Ctrl Pts',(-3.91381537680073,-1.18514270861269,
4.97543838782684));
#40877=CARTESIAN_POINT('Ctrl Pts',(-3.8555022312982,-1.06847604194558,5.01986946156966));
#40878=CARTESIAN_POINT('Ctrl Pts',(-3.74671747692744,-0.794772684000851,
5.10843804226175));
#40879=CARTESIAN_POINT('Ctrl Pts',(-3.70705838932681,-0.636309800095196,
5.14816850605185));
#40880=CARTESIAN_POINT('Ctrl Pts',(-3.65612349313465,-0.319434907277159,
5.20582783218244));
#40881=CARTESIAN_POINT('Ctrl Pts',(-3.64724201481597,-0.158333333333332,
5.22424600109739));
#40882=CARTESIAN_POINT('Ctrl Pts',(-3.65704996975845,0.158333333333335,
5.24249822284547));
#40883=CARTESIAN_POINT('Ctrl Pts',(-3.67523755008907,0.319434907277167,
5.24161469395223));
#40884=CARTESIAN_POINT('Ctrl Pts',(-3.74717278258778,0.636309800095206,
5.22259549162792));
#40885=CARTESIAN_POINT('Ctrl Pts',(-3.79716553103066,0.79477268400084,5.20123433415373));
#40886=CARTESIAN_POINT('Ctrl Pts',(-3.92828386839274,1.06847604194529,5.15372462655724));
#40887=CARTESIAN_POINT('Ctrl Pts',(-3.99710096186636,1.18514270861212,5.12872323336551));
#40888=CARTESIAN_POINT('Ctrl Pts',(-4.07797887898274,1.30000000000051,5.09928563899242));
#40889=CARTESIAN_POINT('Ctrl Pts',(-3.97477914228554,-1.30000000000134,
4.92421546647393));
#40890=CARTESIAN_POINT('Ctrl Pts',(-3.90549290340884,-1.18514270861269,
4.9747309843426));
#40891=CARTESIAN_POINT('Ctrl Pts',(-3.84729017393187,-1.06847604194558,
5.01883535605274));
#40892=CARTESIAN_POINT('Ctrl Pts',(-3.73843534938597,-0.794772684000851,
5.10591424758072));
#40893=CARTESIAN_POINT('Ctrl Pts',(-3.69814954202848,-0.636309800095196,
5.14315668292551));
#40894=CARTESIAN_POINT('Ctrl Pts',(-3.64686579593571,-0.319434907277159,
5.19916589978869));
#40895=CARTESIAN_POINT('Ctrl Pts',(-3.6379450782909,-0.158333333333332,
5.21761871575033));
#40896=CARTESIAN_POINT('Ctrl Pts',(-3.64772547716596,0.158333333333335,
5.23563571893282));
#40897=CARTESIAN_POINT('Ctrl Pts',(-3.66586376136843,0.319434907277167,
5.23420897929763));
#40898=CARTESIAN_POINT('Ctrl Pts',(-3.73821592466294,0.636309800095206,
5.21691754730656));
#40899=CARTESIAN_POINT('Ctrl Pts',(-3.78913144751244,0.79477268400084,5.19908697787931));
#40900=CARTESIAN_POINT('Ctrl Pts',(-3.92026688586173,1.06847604194529,5.15292277487033));
#40901=CARTESIAN_POINT('Ctrl Pts',(-3.98887475074047,1.18514270861212,5.12794379392484));
#40902=CARTESIAN_POINT('Ctrl Pts',(-4.06932680828339,1.30000000000051,5.09796860496417));
#40903=CARTESIAN_POINT('Ctrl Pts',(-3.97477914228473,-1.3,4.92421546647452));
#40904=CARTESIAN_POINT('Ctrl Pts',(-3.90549290340839,-1.18514270861178,
4.97473098434294));
#40905=CARTESIAN_POINT('Ctrl Pts',(-3.84729017393168,-1.06847604194512,
5.01883535605289));
#40906=CARTESIAN_POINT('Ctrl Pts',(-3.73843534938597,-0.794772684000851,
5.10591424758072));
#40907=CARTESIAN_POINT('Ctrl Pts',(-3.69814954202848,-0.636309800095197,
5.14315668292551));
#40908=CARTESIAN_POINT('Ctrl Pts',(-3.64686579593571,-0.319434907277159,
5.19916589978868));
#40909=CARTESIAN_POINT('Ctrl Pts',(-3.6379450782909,-0.158333333333332,
5.21761871575033));
#40910=CARTESIAN_POINT('Ctrl Pts',(-3.64772547716596,0.158333333333334,
5.23563571893282));
#40911=CARTESIAN_POINT('Ctrl Pts',(-3.66586376136842,0.319434907277167,
5.23420897929763));
#40912=CARTESIAN_POINT('Ctrl Pts',(-3.73821592466293,0.636309800095206,
5.21691754730656));
#40913=CARTESIAN_POINT('Ctrl Pts',(-3.78913144751243,0.79477268400084,5.19908697787931));
#40914=CARTESIAN_POINT('Ctrl Pts',(-3.92026688586164,1.06847604194511,5.15292277487035));
#40915=CARTESIAN_POINT('Ctrl Pts',(-3.98887475074027,1.18514270861178,5.12794379392492));
#40916=CARTESIAN_POINT('Ctrl Pts',(-4.06932680828303,1.3,5.09796860496431));
#40917=CARTESIAN_POINT('',(-4.38974166843611,-1.2,4.91249741324829));
#40918=CARTESIAN_POINT('Ctrl Pts',(-4.38974166843611,-1.2,4.91249741324829));
#40919=CARTESIAN_POINT('Ctrl Pts',(-4.37461051593519,-1.211983516113,4.90939208523401));
#40920=CARTESIAN_POINT('Ctrl Pts',(-4.34731408198419,-1.23320834189274,
4.90307035926027));
#40921=CARTESIAN_POINT('Ctrl Pts',(-4.30332881373785,-1.26800264000266,
4.89446891161289));
#40922=CARTESIAN_POINT('Ctrl Pts',(-4.28396809346178,-1.28318693061577,
4.89052779190164));
#40923=CARTESIAN_POINT('Ctrl Pts',(-4.26288026198571,-1.29999999996411,
4.88691723617146));
#40924=CARTESIAN_POINT('',(-4.45989076532205,-0.653834841370044,5.05247250051788));
#40925=CARTESIAN_POINT('Ctrl Pts',(-4.45989076535295,-0.653834841368788,
5.0524725004975));
#40926=CARTESIAN_POINT('Ctrl Pts',(-4.45290452376729,-0.71730390830208,
5.03796378089337));
#40927=CARTESIAN_POINT('Ctrl Pts',(-4.44705077906394,-0.764712012454701,
5.0259462125413));
#40928=CARTESIAN_POINT('Ctrl Pts',(-4.42424443208212,-0.949624929693292,
4.97968576415318));
#40929=CARTESIAN_POINT('Ctrl Pts',(-4.41009602593574,-1.05881338582905,
4.95155764066304));
#40930=CARTESIAN_POINT('Ctrl Pts',(-4.38974166843611,-1.2,4.91249741324829));
#40931=CARTESIAN_POINT('',(-4.51863764645953,0.653834841531101,5.17900672440537));
#40932=CARTESIAN_POINT('Ctrl Pts',(-4.51863764645953,0.653834841531102,
5.17900672440538));
#40933=CARTESIAN_POINT('Ctrl Pts',(-4.47706146767404,0.575967435244021,
5.1784184981011));
#40934=CARTESIAN_POINT('Ctrl Pts',(-4.44192892421759,0.49363270220023,5.17716396632452));
#40935=CARTESIAN_POINT('Ctrl Pts',(-4.39149772313144,0.338127729760966,
5.17291995537731));
#40936=CARTESIAN_POINT('Ctrl Pts',(-4.37381871579893,0.265652356086789,
5.17019838028741));
#40937=CARTESIAN_POINT('Ctrl Pts',(-4.35075689041254,0.129712176552852,
5.16231216794911));
#40938=CARTESIAN_POINT('Ctrl Pts',(-4.34396311929369,0.0666225871102778,
5.1575862721065));
#40939=CARTESIAN_POINT('Ctrl Pts',(-4.3380158949138,-0.0595427376094998,
5.14565883562823));
#40940=CARTESIAN_POINT('Ctrl Pts',(-4.33880327069977,-0.122774428304041,
5.13837690399667));
#40941=CARTESIAN_POINT('Ctrl Pts',(-4.34923014512322,-0.260123906820502,
5.12045087664636));
#40942=CARTESIAN_POINT('Ctrl Pts',(-4.36045995272139,-0.333941086098924,
5.10943130653841));
#40943=CARTESIAN_POINT('Ctrl Pts',(-4.3972325539662,-0.491209295028013,
5.08375339409386));
#40944=CARTESIAN_POINT('Ctrl Pts',(-4.42491420924364,-0.574352714525261,
5.06856467535912));
#40945=CARTESIAN_POINT('Ctrl Pts',(-4.45989076527149,-0.65383484138658,
5.05247250048966));
#40946=CARTESIAN_POINT('',(-4.48863704729437,1.2,5.11322318930451));
#40947=CARTESIAN_POINT('Ctrl Pts',(-4.48863704729437,1.2,5.11322318930451));
#40948=CARTESIAN_POINT('Ctrl Pts',(-4.49416731133851,1.13013423818568,5.12511873459839));
#40949=CARTESIAN_POINT('Ctrl Pts',(-4.49993170183524,1.05323108968555,5.13758912248786));
#40950=CARTESIAN_POINT('Ctrl Pts',(-4.5137823832937,0.796443355018211,5.16814456459401));
#40951=CARTESIAN_POINT('Ctrl Pts',(-4.51601205652913,0.739828131497515,
5.17313629937876));
#40952=CARTESIAN_POINT('Ctrl Pts',(-4.51863764645953,0.653834841531102,
5.17900672440538));
#40953=CARTESIAN_POINT('Ctrl Pts',(-4.36610424565707,1.30000000000001,5.08821551382361));
#40954=CARTESIAN_POINT('Ctrl Pts',(-4.38654452017538,1.28314808556143,5.09177297168868));
#40955=CARTESIAN_POINT('Ctrl Pts',(-4.40703706424362,1.26652555865796,5.09607491528727));
#40956=CARTESIAN_POINT('Ctrl Pts',(-4.44785780404133,1.2330928376765,5.10412551204498));
#40957=CARTESIAN_POINT('Ctrl Pts',(-4.46873140079917,1.21600397350301,5.10836902693465));
#40958=CARTESIAN_POINT('Ctrl Pts',(-4.48863704729437,1.2,5.11322318930451));
#40959=CARTESIAN_POINT('Ctrl Pts',(-3.97477914228473,-1.3,4.92421546647452));
#40960=CARTESIAN_POINT('Ctrl Pts',(-3.90549290340839,-1.18514270861178,
4.97473098434294));
#40961=CARTESIAN_POINT('Ctrl Pts',(-3.84729017393168,-1.06847604194512,
5.01883535605288));
#40962=CARTESIAN_POINT('Ctrl Pts',(-3.73843534938597,-0.794772684000851,
5.10591424758072));
#40963=CARTESIAN_POINT('Ctrl Pts',(-3.69814954202848,-0.636309800095196,
5.1431566829255));
#40964=CARTESIAN_POINT('Ctrl Pts',(-3.64686579593571,-0.319434907277159,
5.19916589978868));
#40965=CARTESIAN_POINT('Ctrl Pts',(-3.63794507829089,-0.158333333333332,
5.21761871575032));
#40966=CARTESIAN_POINT('Ctrl Pts',(-3.64772547716596,0.158333333333334,
5.23563571893282));
#40967=CARTESIAN_POINT('Ctrl Pts',(-3.66586376136842,0.319434907277167,
5.23420897929763));
#40968=CARTESIAN_POINT('Ctrl Pts',(-3.73821592466293,0.636309800095206,
5.21691754730656));
#40969=CARTESIAN_POINT('Ctrl Pts',(-3.78913144751243,0.79477268400084,5.19908697787931));
#40970=CARTESIAN_POINT('Ctrl Pts',(-3.92026688586164,1.06847604194511,5.15292277487035));
#40971=CARTESIAN_POINT('Ctrl Pts',(-3.98887475074026,1.18514270861178,5.12794379392492));
#40972=CARTESIAN_POINT('Ctrl Pts',(-4.06932680828303,1.3,5.09796860496431));
#40973=CARTESIAN_POINT('Ctrl Pts',(-3.93487809212144,-1.3,4.85843541273091));
#40974=CARTESIAN_POINT('Ctrl Pts',(-3.86662549823904,-1.18514270861178,
4.91034106835601));
#40975=CARTESIAN_POINT('Ctrl Pts',(-3.809178223755,-1.06847604194512,4.9553862039665));
#40976=CARTESIAN_POINT('Ctrl Pts',(-3.70142597681593,-0.794772684000851,
5.04360030479917));
#40977=CARTESIAN_POINT('Ctrl Pts',(-3.6609356094067,-0.636309800095196,
5.08015487886936));
#40978=CARTESIAN_POINT('Ctrl Pts',(-3.60969614500507,-0.319434907277159,
5.13549872192357));
#40979=CARTESIAN_POINT('Ctrl Pts',(-3.60031408828523,-0.158333333333332,
5.1527988809256));
#40980=CARTESIAN_POINT('Ctrl Pts',(-3.61040534854147,0.158333333333334,
5.17063640820599));
#40981=CARTESIAN_POINT('Ctrl Pts',(-3.62931119341529,0.319434907277167,
5.17018552840934));
#40982=CARTESIAN_POINT('Ctrl Pts',(-3.70226172817696,0.636309800095206,
5.1531884342533));
#40983=CARTESIAN_POINT('Ctrl Pts',(-3.75367067633866,0.79477268400084,5.13587894966475));
#40984=CARTESIAN_POINT('Ctrl Pts',(-3.88437428339459,1.06847604194511,5.08819228178639));
#40985=CARTESIAN_POINT('Ctrl Pts',(-3.95254515033271,1.18514270861178,5.06208867567562));
#40986=CARTESIAN_POINT('Ctrl Pts',(-4.0323101357604,1.3,5.03052325501342));
#40987=CARTESIAN_POINT('Ctrl Pts',(-3.89497704195815,-1.3,4.7926553589873));
#40988=CARTESIAN_POINT('Ctrl Pts',(-3.8277580930697,-1.18514270861178,4.84595115236908));
#40989=CARTESIAN_POINT('Ctrl Pts',(-3.77106627357833,-1.06847604194512,
4.89193705188011));
#40990=CARTESIAN_POINT('Ctrl Pts',(-3.66441660424588,-0.794772684000851,
4.98128636201762));
#40991=CARTESIAN_POINT('Ctrl Pts',(-3.62372167678492,-0.636309800095196,
5.01715307481322));
#40992=CARTESIAN_POINT('Ctrl Pts',(-3.57252649407444,-0.319434907277159,
5.07183154405846));
#40993=CARTESIAN_POINT('Ctrl Pts',(-3.56268309827957,-0.158333333333332,
5.08797904610087));
#40994=CARTESIAN_POINT('Ctrl Pts',(-3.57308521991697,0.158333333333334,
5.10563709747917));
#40995=CARTESIAN_POINT('Ctrl Pts',(-3.59275862546217,0.319434907277167,
5.10616207752106));
#40996=CARTESIAN_POINT('Ctrl Pts',(-3.66630753169098,0.636309800095206,
5.08945932120005));
#40997=CARTESIAN_POINT('Ctrl Pts',(-3.71820990516489,0.79477268400084,5.07267092145019));
#40998=CARTESIAN_POINT('Ctrl Pts',(-3.84848168092753,1.06847604194511,5.02346178870243));
#40999=CARTESIAN_POINT('Ctrl Pts',(-3.91621554992515,1.18514270861178,4.99623355742632));
#41000=CARTESIAN_POINT('Ctrl Pts',(-3.99529346323778,1.3,4.96307790506253));
#41001=CARTESIAN_POINT('Ctrl Pts',(-3.85507599179486,-1.3,4.7268753052437));
#41002=CARTESIAN_POINT('Ctrl Pts',(-3.78889068790036,-1.18514270861178,
4.78156123638215));
#41003=CARTESIAN_POINT('Ctrl Pts',(-3.73295432340165,-1.06847604194512,
4.82848789979372));
#41004=CARTESIAN_POINT('Ctrl Pts',(-3.62740723167583,-0.794772684000851,
4.91897241923607));
#41005=CARTESIAN_POINT('Ctrl Pts',(-3.58650774416313,-0.636309800095196,
4.95415127075708));
#41006=CARTESIAN_POINT('Ctrl Pts',(-3.5353568431438,-0.319434907277159,
5.00816436619335));
#41007=CARTESIAN_POINT('Ctrl Pts',(-3.52505210827391,-0.158333333333332,
5.02315921127615));
#41008=CARTESIAN_POINT('Ctrl Pts',(-3.53576509129248,0.158333333333334,
5.04063778675235));
#41009=CARTESIAN_POINT('Ctrl Pts',(-3.55620605750904,0.319434907277167,
5.04213862663277));
#41010=CARTESIAN_POINT('Ctrl Pts',(-3.630353335205,0.636309800095206,5.02573020814679));
#41011=CARTESIAN_POINT('Ctrl Pts',(-3.68274913399112,0.79477268400084,5.00946289323563));
#41012=CARTESIAN_POINT('Ctrl Pts',(-3.81258907846048,1.06847604194511,4.95873129561847));
#41013=CARTESIAN_POINT('Ctrl Pts',(-3.8798859495176,1.18514270861178,4.93037843917702));
#41014=CARTESIAN_POINT('Ctrl Pts',(-3.95827679071515,1.3,4.89563255511164));
#41015=CARTESIAN_POINT('Ctrl Pts',(-3.85507599179486,-1.3,4.7268753052437));
#41016=CARTESIAN_POINT('Ctrl Pts',(-3.78889068790036,-1.18514270861178,
4.78156123638215));
#41017=CARTESIAN_POINT('Ctrl Pts',(-3.73295432340165,-1.06847604194512,
4.82848789979373));
#41018=CARTESIAN_POINT('Ctrl Pts',(-3.62740723167583,-0.794772684000851,
4.91897241923607));
#41019=CARTESIAN_POINT('Ctrl Pts',(-3.58650774416314,-0.636309800095197,
4.95415127075708));
#41020=CARTESIAN_POINT('Ctrl Pts',(-3.5353568431438,-0.319434907277159,
5.00816436619336));
#41021=CARTESIAN_POINT('Ctrl Pts',(-3.52505210827391,-0.158333333333332,
5.02315921127615));
#41022=CARTESIAN_POINT('Ctrl Pts',(-3.53576509129248,0.158333333333334,
5.04063778675235));
#41023=CARTESIAN_POINT('Ctrl Pts',(-3.55620605750904,0.319434907277167,
5.04213862663277));
#41024=CARTESIAN_POINT('Ctrl Pts',(-3.630353335205,0.636309800095206,5.0257302081468));
#41025=CARTESIAN_POINT('Ctrl Pts',(-3.68274913399112,0.79477268400084,5.00946289323563));
#41026=CARTESIAN_POINT('Ctrl Pts',(-3.81258907846048,1.06847604194511,4.95873129561847));
#41027=CARTESIAN_POINT('Ctrl Pts',(-3.87988594951759,1.18514270861178,4.93037843917702));
#41028=CARTESIAN_POINT('Ctrl Pts',(-3.95827679071515,1.3,4.89563255511164));
#41029=CARTESIAN_POINT('Ctrl Pts',(-3.85507599179492,-1.30000000000009,
4.72687530524365));
#41030=CARTESIAN_POINT('Ctrl Pts',(-3.78889068790039,-1.18514270861184,
4.78156123638212));
#41031=CARTESIAN_POINT('Ctrl Pts',(-3.73295432340166,-1.06847604194515,
4.82848789979372));
#41032=CARTESIAN_POINT('Ctrl Pts',(-3.62740723167584,-0.794772684000851,
4.91897241923607));
#41033=CARTESIAN_POINT('Ctrl Pts',(-3.58650774416314,-0.636309800095197,
4.95415127075708));
#41034=CARTESIAN_POINT('Ctrl Pts',(-3.53535684314381,-0.319434907277159,
5.00816436619336));
#41035=CARTESIAN_POINT('Ctrl Pts',(-3.52505210827391,-0.158333333333332,
5.02315921127615));
#41036=CARTESIAN_POINT('Ctrl Pts',(-3.53576509129248,0.158333333333334,
5.04063778675235));
#41037=CARTESIAN_POINT('Ctrl Pts',(-3.55620605750904,0.319434907277167,
5.04213862663278));
#41038=CARTESIAN_POINT('Ctrl Pts',(-3.630353335205,0.636309800095206,5.0257302081468));
#41039=CARTESIAN_POINT('Ctrl Pts',(-3.68274913399112,0.79477268400084,5.00946289323563));
#41040=CARTESIAN_POINT('Ctrl Pts',(-3.81258907846121,1.06847604194665,4.95873129561818));
#41041=CARTESIAN_POINT('Ctrl Pts',(-3.87988594951935,1.18514270861482,4.93037843917628));
#41042=CARTESIAN_POINT('Ctrl Pts',(-3.95827679071822,1.30000000000449,4.89563255511028));
#41043=CARTESIAN_POINT('Ctrl Pts',(-3.85719962537667,-1.30000000000009,
4.72144101857419));
#41044=CARTESIAN_POINT('Ctrl Pts',(-3.79118274867503,-1.18514270861184,
4.77655201804504));
#41045=CARTESIAN_POINT('Ctrl Pts',(-3.73516370159793,-1.06847604194515,
4.82359200889143));
#41046=CARTESIAN_POINT('Ctrl Pts',(-3.62884548276946,-0.794772684000851,
4.91361815354223));
#41047=CARTESIAN_POINT('Ctrl Pts',(-3.58621520077171,-0.636309800095197,
4.94708737832572));
#41048=CARTESIAN_POINT('Ctrl Pts',(-3.53420574800354,-0.319434907277159,
5.00028383521863));
#41049=CARTESIAN_POINT('Ctrl Pts',(-3.52419820392418,-0.158333333333332,
5.01548821170247));
#41050=CARTESIAN_POINT('Ctrl Pts',(-3.53503780509133,0.158333333333334,
5.03306110286902));
#41051=CARTESIAN_POINT('Ctrl Pts',(-3.55544568808847,0.319434907277167,
5.03457304854717));
#41052=CARTESIAN_POINT('Ctrl Pts',(-3.63042937353099,0.636309800095206,
5.01891607505766));
#41053=CARTESIAN_POINT('Ctrl Pts',(-3.68405272961868,0.79477268400084,5.00383993978519));
#41054=CARTESIAN_POINT('Ctrl Pts',(-3.81472938980192,1.06847604194665,4.95364536025774));
#41055=CARTESIAN_POINT('Ctrl Pts',(-3.88225168770668,1.18514270861482,4.92533765577221));
#41056=CARTESIAN_POINT('Ctrl Pts',(-3.96073119936994,1.30000000000449,4.89044962038628));
#41057=CARTESIAN_POINT('Ctrl Pts',(-3.86187573129453,-1.30000000000009,
4.71383403293714));
#41058=CARTESIAN_POINT('Ctrl Pts',(-3.79719254535568,-1.18514270861185,
4.76895782901383));
#41059=CARTESIAN_POINT('Ctrl Pts',(-3.74183062561163,-1.06847604194515,
4.8157035538932));
#41060=CARTESIAN_POINT('Ctrl Pts',(-3.63546750551163,-0.794772684000853,
4.90434050932157));
#41061=CARTESIAN_POINT('Ctrl Pts',(-3.5900034586632,-0.636309800095197,
4.93531705592154));
#41062=CARTESIAN_POINT('Ctrl Pts',(-3.53661622228163,-0.319434907277158,
4.9872084206034));
#41063=CARTESIAN_POINT('Ctrl Pts',(-3.526536583893,-0.158333333333332,5.00288186391973));
#41064=CARTESIAN_POINT('Ctrl Pts',(-3.5375239175476,0.158333333333335,5.0205842461583));
#41065=CARTESIAN_POINT('Ctrl Pts',(-3.55824068036155,0.319434907277168,
5.02179590511999));
#41066=CARTESIAN_POINT('Ctrl Pts',(-3.63472167526744,0.636309800095207,
5.00762775887785));
#41067=CARTESIAN_POINT('Ctrl Pts',(-3.69099520684581,0.79477268400084,4.99509019029861));
#41068=CARTESIAN_POINT('Ctrl Pts',(-3.82174855505815,1.06847604194665,4.94631026905389));
#41069=CARTESIAN_POINT('Ctrl Pts',(-3.88865832024127,1.18514270861482,4.91828639197139));
#41070=CARTESIAN_POINT('Ctrl Pts',(-3.96587957105504,1.30000000000449,4.88335365823918));
#41071=CARTESIAN_POINT('Ctrl Pts',(-3.86961810893474,-1.30000000000009,
4.70440940889747));
#41072=CARTESIAN_POINT('Ctrl Pts',(-3.80754393917446,-1.18514270861185,
4.75854778066665));
#41073=CARTESIAN_POINT('Ctrl Pts',(-3.75381010225335,-1.06847604194515,
4.80426737477683));
#41074=CARTESIAN_POINT('Ctrl Pts',(-3.6489420268847,-0.794772684000851,
4.89043972278178));
#41075=CARTESIAN_POINT('Ctrl Pts',(-3.60079303589911,-0.636309800095196,
4.91916901559123));
#41076=CARTESIAN_POINT('Ctrl Pts',(-3.5460877997684,-0.319434907277158,
4.96957153261453));
#41077=CARTESIAN_POINT('Ctrl Pts',(-3.53514448494892,-0.158333333333332,
4.98573028016685));
#41078=CARTESIAN_POINT('Ctrl Pts',(-3.54619199064349,0.158333333333334,
5.00349880643113));
#41079=CARTESIAN_POINT('Ctrl Pts',(-3.56772207273765,0.319434907277168,
5.00409256128365));
#41080=CARTESIAN_POINT('Ctrl Pts',(-3.64586877350843,0.636309800095207,
4.99195282032989));
#41081=CARTESIAN_POINT('Ctrl Pts',(-3.70552748394763,0.794772684000839,
4.98285922822908));
#41082=CARTESIAN_POINT('Ctrl Pts',(-3.83480395680561,1.06847604194665,4.93653280029006));
#41083=CARTESIAN_POINT('Ctrl Pts',(-3.89992716386784,1.18514270861482,4.909242080837));
#41084=CARTESIAN_POINT('Ctrl Pts',(-3.97421458305709,1.30000000000449,4.8747136360225));
#41085=CARTESIAN_POINT('Ctrl Pts',(-3.87691755596594,-1.30000000000009,
4.69490664118848));
#41086=CARTESIAN_POINT('Ctrl Pts',(-3.81674813898273,-1.18514270861185,
4.74765414340193));
#41087=CARTESIAN_POINT('Ctrl Pts',(-3.76434400552701,-1.06847604194515,
4.79224680303008));
#41088=CARTESIAN_POINT('Ctrl Pts',(-3.66121933222148,-0.794772684000854,
4.87642544975936));
#41089=CARTESIAN_POINT('Ctrl Pts',(-3.61227744010187,-0.636309800095198,
4.90461839926761));
#41090=CARTESIAN_POINT('Ctrl Pts',(-3.55719693985597,-0.31943490727716,
4.95430228759037));
#41091=CARTESIAN_POINT('Ctrl Pts',(-3.54533126716359,-0.158333333333332,
4.97059092996656));
#41092=CARTESIAN_POINT('Ctrl Pts',(-3.55641159744232,0.158333333333335,
4.98842836728334));
#41093=CARTESIAN_POINT('Ctrl Pts',(-3.57877257621962,0.319434907277167,
4.98880961480654));
#41094=CARTESIAN_POINT('Ctrl Pts',(-3.65761456359265,0.636309800095207,
4.9778375119829));
#41095=CARTESIAN_POINT('Ctrl Pts',(-3.71873653204119,0.794772684000842,
4.97018331391904));
#41096=CARTESIAN_POINT('Ctrl Pts',(-3.84636899840465,1.06847604194666,4.9259261637555));
#41097=CARTESIAN_POINT('Ctrl Pts',(-3.91006561500535,1.18514270861482,4.89959200043321));
#41098=CARTESIAN_POINT('Ctrl Pts',(-3.98221148276658,1.3000000000045,4.86608095420555));
#41099=CARTESIAN_POINT('Ctrl Pts',(-3.88601526735229,-1.3000000000001,4.68298671678652));
#41100=CARTESIAN_POINT('Ctrl Pts',(-3.82789893469574,-1.18514270861185,
4.73382883581962));
#41101=CARTESIAN_POINT('Ctrl Pts',(-3.77707208302522,-1.06847604194515,
4.77714616311773));
#41102=CARTESIAN_POINT('Ctrl Pts',(-3.67649204712285,-0.794772684000852,
4.85983408054075));
#41103=CARTESIAN_POINT('Ctrl Pts',(-3.62803813052283,-0.636309800095198,
4.88966447649553));
#41104=CARTESIAN_POINT('Ctrl Pts',(-3.57285551823652,-0.319434907277159,
4.93918402311753));
#41105=CARTESIAN_POINT('Ctrl Pts',(-3.55916791444883,-0.158333333333333,
4.9546365788754));
#41106=CARTESIAN_POINT('Ctrl Pts',(-3.56990613195591,0.158333333333335,
4.97203904858936));
#41107=CARTESIAN_POINT('Ctrl Pts',(-3.59322204533834,0.319434907277168,
4.97211877620001));
#41108=CARTESIAN_POINT('Ctrl Pts',(-3.67253843601065,0.636309800095208,
4.96185624229368));
#41109=CARTESIAN_POINT('Ctrl Pts',(-3.73506171307405,0.794772684000842,
4.955175041043));
#41110=CARTESIAN_POINT('Ctrl Pts',(-3.86047195508732,1.06847604194666,4.91278091488119));
#41111=CARTESIAN_POINT('Ctrl Pts',(-3.92239820161952,1.18514270861482,4.88740444501922));
#41112=CARTESIAN_POINT('Ctrl Pts',(-3.99196524782343,1.3000000000045,4.85500235165368));
#41113=CARTESIAN_POINT('Ctrl Pts',(-3.89491361629381,-1.3000000000001,4.67070753187993));
#41114=CARTESIAN_POINT('Ctrl Pts',(-3.83893894854118,-1.18514270861185,
4.71945502898068));
#41115=CARTESIAN_POINT('Ctrl Pts',(-3.78979225765621,-1.06847604194515,
4.76138456315725));
#41116=CARTESIAN_POINT('Ctrl Pts',(-3.69202756244646,-0.794772684000855,
4.84249931679602));
#41117=CARTESIAN_POINT('Ctrl Pts',(-3.64419754857245,-0.636309800095201,
4.87401768374301));
#41118=CARTESIAN_POINT('Ctrl Pts',(-3.58939362681402,-0.319434907277161,
4.92386667443013));
#41119=CARTESIAN_POINT('Ctrl Pts',(-3.57413548094992,-0.158333333333333,
4.93886520909327));
#41120=CARTESIAN_POINT('Ctrl Pts',(-3.58534511953175,0.158333333333335,
4.95696636476547));
#41121=CARTESIAN_POINT('Ctrl Pts',(-3.61097395478874,0.319434907277168,
4.95861683227717));
#41122=CARTESIAN_POINT('Ctrl Pts',(-3.69031998230916,0.636309800095209,
4.94859652448346));
#41123=CARTESIAN_POINT('Ctrl Pts',(-3.75189333622018,0.794772684000847,
4.93969710293881));
#41124=CARTESIAN_POINT('Ctrl Pts',(-3.87425501353822,1.06847604194666,4.89845975445627));
#41125=CARTESIAN_POINT('Ctrl Pts',(-3.93437172036864,1.18514270861483,4.87424558338349));
#41126=CARTESIAN_POINT('Ctrl Pts',(-4.00163929786509,1.3000000000045,4.84366736140181));
#41127=CARTESIAN_POINT('Ctrl Pts',(-3.90299367365699,-1.3000000000001,4.65757823073421));
#41128=CARTESIAN_POINT('Ctrl Pts',(-3.84907963830677,-1.18514270861185,
4.7043243450785));
#41129=CARTESIAN_POINT('Ctrl Pts',(-3.80159394234937,-1.06847604194515,
4.74498916226841));
#41130=CARTESIAN_POINT('Ctrl Pts',(-3.70674323518918,-0.794772684000856,
4.82488401195993));
#41131=CARTESIAN_POINT('Ctrl Pts',(-3.65963597807638,-0.636309800095201,
4.85818914450328));
#41132=CARTESIAN_POINT('Ctrl Pts',(-3.60586222489922,-0.319434907277161,
4.90926246644672));
#41133=CARTESIAN_POINT('Ctrl Pts',(-3.59017934567842,-0.158333333333333,
4.92529238592121));
#41134=CARTESIAN_POINT('Ctrl Pts',(-3.60179395376847,0.158333333333335,
4.94401705810809));
#41135=CARTESIAN_POINT('Ctrl Pts',(-3.62840541558098,0.319434907277168,
4.94554572747288));
#41136=CARTESIAN_POINT('Ctrl Pts',(-3.70723467370267,0.636309800095209,
4.93498844237129));
#41137=CARTESIAN_POINT('Ctrl Pts',(-3.76801153668662,0.794772684000845,
4.92403147914096));
#41138=CARTESIAN_POINT('Ctrl Pts',(-3.88764112416407,1.06847604194666,4.88409836430707));
#41139=CARTESIAN_POINT('Ctrl Pts',(-3.9461792048465,1.18514270861483,4.86118862156217));
#41140=CARTESIAN_POINT('Ctrl Pts',(-4.01147215050509,1.3000000000045,4.83265470181636));
#41141=CARTESIAN_POINT('Ctrl Pts',(-3.90989779693675,-1.30000000000011,
4.64755288062261));
#41142=CARTESIAN_POINT('Ctrl Pts',(-3.85774919301543,-1.18514270861186,
4.6927615254062));
#41143=CARTESIAN_POINT('Ctrl Pts',(-3.81163105041348,-1.06847604194516,
4.73240221316335));
#41144=CARTESIAN_POINT('Ctrl Pts',(-3.71902048713749,-0.794772684000856,
4.81111703737771));
#41145=CARTESIAN_POINT('Ctrl Pts',(-3.67209309642864,-0.636309800095202,
4.84536348279141));
#41146=CARTESIAN_POINT('Ctrl Pts',(-3.61893232916747,-0.319434907277161,
4.89715154894492));
#41147=CARTESIAN_POINT('Ctrl Pts',(-3.60306622995126,-0.158333333333333,
4.91427581209853));
#41148=CARTESIAN_POINT('Ctrl Pts',(-3.61471415449658,0.158333333333336,
4.93306287156498));
#41149=CARTESIAN_POINT('Ctrl Pts',(-3.64145681552091,0.319434907277169,
4.93345505829791));
#41150=CARTESIAN_POINT('Ctrl Pts',(-3.71991477675818,0.636309800095211,
4.9225230197917));
#41151=CARTESIAN_POINT('Ctrl Pts',(-3.78099635420355,0.794772684000847,
4.91129657713904));
#41152=CARTESIAN_POINT('Ctrl Pts',(-3.89845061218902,1.06847604194666,4.87256374236237));
#41153=CARTESIAN_POINT('Ctrl Pts',(-3.95554548416997,1.18514270861483,4.85052729323673));
#41154=CARTESIAN_POINT('Ctrl Pts',(-4.01889363195879,1.3000000000045,4.82322040396743));
#41155=CARTESIAN_POINT('Ctrl Pts',(-3.92221206525848,-1.30000000000011,
4.63033050218808));
#41156=CARTESIAN_POINT('Ctrl Pts',(-3.8726683820101,-1.18514270861186,4.67235347215618));
#41157=CARTESIAN_POINT('Ctrl Pts',(-3.82860854712782,-1.06847604194516,
4.70985685555733));
#41158=CARTESIAN_POINT('Ctrl Pts',(-3.73949030117575,-0.794772684000857,
4.7860560246303));
#41159=CARTESIAN_POINT('Ctrl Pts',(-3.69315893855885,-0.636309800095202,
4.82223357701685));
#41160=CARTESIAN_POINT('Ctrl Pts',(-3.64107903602519,-0.319434907277161,
4.87522861122178));
#41161=CARTESIAN_POINT('Ctrl Pts',(-3.62459994389214,-0.158333333333333,
4.89377442775102));
#41162=CARTESIAN_POINT('Ctrl Pts',(-3.63685055307432,0.158333333333336,
4.91343611787957));
#41163=CARTESIAN_POINT('Ctrl Pts',(-3.66520128415716,0.31943490727717,4.91387516116949));
#41164=CARTESIAN_POINT('Ctrl Pts',(-3.74300673059837,0.636309800095211,
4.90230822867458));
#41165=CARTESIAN_POINT('Ctrl Pts',(-3.80286755801116,0.794772684000846,
4.88815756908362));
#41166=CARTESIAN_POINT('Ctrl Pts',(-3.91646823347156,1.06847604194666,4.85134128532008));
#41167=CARTESIAN_POINT('Ctrl Pts',(-3.97134781558832,1.18514270861483,4.83118714834847));
#41168=CARTESIAN_POINT('Ctrl Pts',(-4.03193345673457,1.30000000000451,4.80681527946886));
#41169=CARTESIAN_POINT('Ctrl Pts',(-3.93623661697016,-1.30000000000012,
4.60609932986889));
#41170=CARTESIAN_POINT('Ctrl Pts',(-3.88988848758903,-1.18514270861187,
4.64384498320135));
#41171=CARTESIAN_POINT('Ctrl Pts',(-3.84848197627912,-1.06847604194517,
4.67860153774707));
#41172=CARTESIAN_POINT('Ctrl Pts',(-3.76424077812082,-0.794772684000869,
4.75199071560809));
#41173=CARTESIAN_POINT('Ctrl Pts',(-3.71958858051035,-0.636309800095212,
4.79165991930544));
#41174=CARTESIAN_POINT('Ctrl Pts',(-3.66959157094361,-0.319434907277166,
4.84701784672139));
#41175=CARTESIAN_POINT('Ctrl Pts',(-3.65291612803299,-0.158333333333335,
4.8682313224775));
#41176=CARTESIAN_POINT('Ctrl Pts',(-3.66532599911306,0.158333333333338,
4.88814222567686));
#41177=CARTESIAN_POINT('Ctrl Pts',(-3.69367882888989,0.319434907277172,
4.88577252352626));
#41178=CARTESIAN_POINT('Ctrl Pts',(-3.77044586990941,0.636309800095218,
4.87314533844164));
#41179=CARTESIAN_POINT('Ctrl Pts',(-3.83063440064933,0.794772684000859,
4.85792393697454));
#41180=CARTESIAN_POINT('Ctrl Pts',(-3.93970515880007,1.06847604194668,4.82420737950992));
#41181=CARTESIAN_POINT('Ctrl Pts',(-3.99166519338934,1.18514270861485,4.80639044485926));
#41182=CARTESIAN_POINT('Ctrl Pts',(-4.048372572834,1.30000000000452,4.78535122396292));
#41183=CARTESIAN_POINT('Ctrl Pts',(-3.95284745610305,-1.30000000000013,
4.58042969910378));
#41184=CARTESIAN_POINT('Ctrl Pts',(-3.91072378417741,-1.18514270861188,
4.61419652857939));
#41185=CARTESIAN_POINT('Ctrl Pts',(-3.87246653076059,-1.06847604194518,
4.64611776351736));
#41186=CARTESIAN_POINT('Ctrl Pts',(-3.79301682226017,-0.794772684000873,
4.71559850945336));
#41187=CARTESIAN_POINT('Ctrl Pts',(-3.74773301943357,-0.636309800095213,
4.75619944846116));
#41188=CARTESIAN_POINT('Ctrl Pts',(-3.6987758134057,-0.319434907277167,
4.81258658242706));
#41189=CARTESIAN_POINT('Ctrl Pts',(-3.68181816367919,-0.158333333333336,
4.83651187898168));
#41190=CARTESIAN_POINT('Ctrl Pts',(-3.69492372703802,0.158333333333338,
4.85735934309548));
#41191=CARTESIAN_POINT('Ctrl Pts',(-3.72467603759297,0.319434907277175,
4.85379520621468));
#41192=CARTESIAN_POINT('Ctrl Pts',(-3.80096161861959,0.636309800095222,
4.84086342271053));
#41193=CARTESIAN_POINT('Ctrl Pts',(-3.86090246302895,0.79477268400086,4.8235616603301));
#41194=CARTESIAN_POINT('Ctrl Pts',(-3.9653366829377,1.06847604194668,4.79377615092503));
#41195=CARTESIAN_POINT('Ctrl Pts',(-4.01436420907048,1.18514270861485,4.77896071898002));
#41196=CARTESIAN_POINT('Ctrl Pts',(-4.06721355720645,1.30000000000453,4.76222289844965));
#41197=CARTESIAN_POINT('Ctrl Pts',(-3.96535170192484,-1.30000000000013,
4.5590274851764));
#41198=CARTESIAN_POINT('Ctrl Pts',(-3.92546910793081,-1.18514270861188,
4.58834962547774));
#41199=CARTESIAN_POINT('Ctrl Pts',(-3.88907325183375,-1.06847604194518,
4.61727115350065));
#41200=CARTESIAN_POINT('Ctrl Pts',(-3.81304660534494,-0.794772684000875,
4.68316017446002));
#41201=CARTESIAN_POINT('Ctrl Pts',(-3.76891047771894,-0.636309800095216,
4.726329929948));
#41202=CARTESIAN_POINT('Ctrl Pts',(-3.72148492134035,-0.319434907277169,
4.78428593600164));
#41203=CARTESIAN_POINT('Ctrl Pts',(-3.70435257527215,-0.158333333333337,
4.81042011216846));
#41204=CARTESIAN_POINT('Ctrl Pts',(-3.71797010330905,0.158333333333339,
4.83191259389462));
#41205=CARTESIAN_POINT('Ctrl Pts',(-3.7484901200146,0.319434907277175,4.82693408344865));
#41206=CARTESIAN_POINT('Ctrl Pts',(-3.82412180348236,0.636309800095224,
4.81344278511243));
#41207=CARTESIAN_POINT('Ctrl Pts',(-3.88373399482127,0.794772684000864,
4.79439433692748));
#41208=CARTESIAN_POINT('Ctrl Pts',(-3.98441581257107,1.06847604194669,4.76771271056547));
#41209=CARTESIAN_POINT('Ctrl Pts',(-4.03112104102182,1.18514270861486,4.75531895237286));
#41210=CARTESIAN_POINT('Ctrl Pts',(-4.08095006964814,1.30000000000453,4.74208092338814));
#41211=CARTESIAN_POINT('Ctrl Pts',(-3.97449901676934,-1.30000000000014,
4.54274237531137));
#41212=CARTESIAN_POINT('Ctrl Pts',(-3.93709157683421,-1.18514270861188,
4.56961294297179));
#41213=CARTESIAN_POINT('Ctrl Pts',(-3.90259013536087,-1.06847604194518,
4.59683916670406));
#41214=CARTESIAN_POINT('Ctrl Pts',(-3.8295983413575,-0.794772684000875,
4.6605588267877));
#41215=CARTESIAN_POINT('Ctrl Pts',(-3.78563727997431,-0.636309800095219,
4.70491822702643));
#41216=CARTESIAN_POINT('Ctrl Pts',(-3.73875498329855,-0.319434907277172,
4.76335431154097));
#41217=CARTESIAN_POINT('Ctrl Pts',(-3.72082588163312,-0.158333333333338,
4.7903395778526));
#41218=CARTESIAN_POINT('Ctrl Pts',(-3.73460539730176,0.15833333333334,4.81205747381827));
#41219=CARTESIAN_POINT('Ctrl Pts',(-3.76596561796686,0.319434907277177,
4.80633812157363));
#41220=CARTESIAN_POINT('Ctrl Pts',(-3.84162545483092,0.636309800095228,
4.79306048198457));
#41221=CARTESIAN_POINT('Ctrl Pts',(-3.9017991424465,0.794772684000869,4.77368450597758));
#41222=CARTESIAN_POINT('Ctrl Pts',(-3.99984738133293,1.06847604194669,4.74955254208256));
#41223=CARTESIAN_POINT('Ctrl Pts',(-4.0447207637576,1.18514270861486,4.73886648778137));
#41224=CARTESIAN_POINT('Ctrl Pts',(-4.09202607903803,1.30000000000454,4.72794021217183));
#41225=CARTESIAN_POINT('Ctrl Pts',(-3.98365558285505,-1.30000000000014,
4.52648867384936));
#41226=CARTESIAN_POINT('Ctrl Pts',(-3.94802546111216,-1.18514270861189,
4.55015011718819));
#41227=CARTESIAN_POINT('Ctrl Pts',(-3.91493284176103,-1.06847604194519,
4.57514792636692));
#41228=CARTESIAN_POINT('Ctrl Pts',(-3.84434440905465,-0.79477268400088,
4.63598513879361));
#41229=CARTESIAN_POINT('Ctrl Pts',(-3.80070404932378,-0.636309800095222,
4.68163239936094));
#41230=CARTESIAN_POINT('Ctrl Pts',(-3.7548189954872,-0.319434907277172,
4.74103728856512));
#41231=CARTESIAN_POINT('Ctrl Pts',(-3.73701840812171,-0.158333333333338,
4.76994052592333));
#41232=CARTESIAN_POINT('Ctrl Pts',(-3.75125591399722,0.15833333333334,4.79220492185405));
#41233=CARTESIAN_POINT('Ctrl Pts',(-3.78319980310662,0.319434907277177,
4.78544165923762));
#41234=CARTESIAN_POINT('Ctrl Pts',(-3.85827751831032,0.636309800095229,
4.77164117845782));
#41235=CARTESIAN_POINT('Ctrl Pts',(-3.91787090844986,0.794772684000871,
4.75057341116541));
#41236=CARTESIAN_POINT('Ctrl Pts',(-4.01327299532946,1.0684760419467,4.72897368026303));
#41237=CARTESIAN_POINT('Ctrl Pts',(-4.0565883586806,1.18514270861487,4.72032166145382));
#41238=CARTESIAN_POINT('Ctrl Pts',(-4.10192305696814,1.30000000000455,4.71236734699421));
#41239=CARTESIAN_POINT('Ctrl Pts',(-3.99622589356072,-1.30000000000016,
4.50522626952481));
#41240=CARTESIAN_POINT('Ctrl Pts',(-3.96314346622973,-1.1851427086119,4.52480713643115));
#41241=CARTESIAN_POINT('Ctrl Pts',(-3.93206737704905,-1.0684760419452,4.54698942543475));
#41242=CARTESIAN_POINT('Ctrl Pts',(-3.86491043678513,-0.79477268400089,
4.6042447560422));
#41243=CARTESIAN_POINT('Ctrl Pts',(-3.82191124009897,-0.636309800095231,
4.65186512030542));
#41244=CARTESIAN_POINT('Ctrl Pts',(-3.77703914577215,-0.319434907277177,
4.71221083099536));
#41245=CARTESIAN_POINT('Ctrl Pts',(-3.75874478410963,-0.15833333333334,
4.74291980786877));
#41246=CARTESIAN_POINT('Ctrl Pts',(-3.77306480043963,0.158333333333343,
4.76531045862233));
#41247=CARTESIAN_POINT('Ctrl Pts',(-3.80530761257115,0.319434907277183,
4.75658141089551));
#41248=CARTESIAN_POINT('Ctrl Pts',(-3.88010540199207,0.636309800095239,
4.74268045395068));
#41249=CARTESIAN_POINT('Ctrl Pts',(-3.94055736214315,0.794772684000886,
4.72130122573096));
#41250=CARTESIAN_POINT('Ctrl Pts',(-4.0327770399233,1.06847604194671,4.70349046048285));
#41251=CARTESIAN_POINT('Ctrl Pts',(-4.07387487551302,1.18514270861488,4.6973834864128));
#41252=CARTESIAN_POINT('Ctrl Pts',(-4.11615206525699,1.30000000000456,4.69287915859477));
#41253=CARTESIAN_POINT('Ctrl Pts',(-4.01031583526455,-1.30000000000017,
4.47694433028216));
#41254=CARTESIAN_POINT('Ctrl Pts',(-3.98029476906993,-1.18514270861191,
4.49132307749177));
#41255=CARTESIAN_POINT('Ctrl Pts',(-3.95161936908155,-1.06847604194521,
4.50987032045911));
#41256=CARTESIAN_POINT('Ctrl Pts',(-3.88848221675032,-0.794772684000896,
4.56234822118198));
#41257=CARTESIAN_POINT('Ctrl Pts',(-3.84583979836555,-0.636309800095234,
4.61188462104922));
#41258=CARTESIAN_POINT('Ctrl Pts',(-3.80253997352847,-0.319434907277178,
4.67367470421467));
#41259=CARTESIAN_POINT('Ctrl Pts',(-3.78430984984646,-0.158333333333341,
4.70731587685121));
#41260=CARTESIAN_POINT('Ctrl Pts',(-3.79966229070426,0.158333333333344,
4.73088970509215));
#41261=CARTESIAN_POINT('Ctrl Pts',(-3.83342601590674,0.319434907277185,
4.72108767838593));
#41262=CARTESIAN_POINT('Ctrl Pts',(-3.90762864613288,0.636309800095243,
4.70677535294558));
#41263=CARTESIAN_POINT('Ctrl Pts',(-3.96698159486524,0.794772684000887,
4.68245666916534));
#41264=CARTESIAN_POINT('Ctrl Pts',(-4.05510064076927,1.06847604194672,4.66923727521721));
#41265=CARTESIAN_POINT('Ctrl Pts',(-4.09379252591144,1.18514270861489,4.66674044423394));
#41266=CARTESIAN_POINT('Ctrl Pts',(-4.13303282635611,1.30000000000457,4.66746896808078));
#41267=CARTESIAN_POINT('Ctrl Pts',(-4.02533150000358,-1.30000000000019,
4.44972631117233));
#41268=CARTESIAN_POINT('Ctrl Pts',(-3.99818829069229,-1.18514270861194,
4.45873161766262));
#41269=CARTESIAN_POINT('Ctrl Pts',(-3.97173680431925,-1.06847604194523,
4.47346910582672));
#41270=CARTESIAN_POINT('Ctrl Pts',(-3.91222659756186,-0.794772684000915,
4.52075813809573));
#41271=CARTESIAN_POINT('Ctrl Pts',(-3.86967653948471,-0.636309800095248,
4.57189844720796));
#41272=CARTESIAN_POINT('Ctrl Pts',(-3.82766115997983,-0.319434907277185,
4.63479501999804));
#41273=CARTESIAN_POINT('Ctrl Pts',(-3.80975372220844,-0.158333333333345,
4.67164424552778));
#41274=CARTESIAN_POINT('Ctrl Pts',(-3.82541765453887,0.158333333333347,
4.69556075515344));
#41275=CARTESIAN_POINT('Ctrl Pts',(-3.85900783513208,0.319434907277191,
4.68273321963391));
#41276=CARTESIAN_POINT('Ctrl Pts',(-3.93289120133694,0.636309800095256,
4.66833861003533));
#41277=CARTESIAN_POINT('Ctrl Pts',(-3.9936989809741,0.794772684000906,4.64407164915053));
#41278=CARTESIAN_POINT('Ctrl Pts',(-4.07811909590979,1.06847604194674,4.63587130536479));
#41279=CARTESIAN_POINT('Ctrl Pts',(-4.11414421160011,1.18514270861491,4.63665058559084));
#41280=CARTESIAN_POINT('Ctrl Pts',(-4.14965210329837,1.30000000000459,4.64175877101514));
#41281=CARTESIAN_POINT('Ctrl Pts',(-4.0360507106705,-1.30000000000021,4.42659910168526));
#41282=CARTESIAN_POINT('Ctrl Pts',(-4.01146896352685,-1.18514270861195,
4.43159793854085));
#41283=CARTESIAN_POINT('Ctrl Pts',(-3.98697845367857,-1.06847604194524,
4.4434927580042));
#41284=CARTESIAN_POINT('Ctrl Pts',(-3.93061125302358,-0.794772684000924,
4.48690326987556));
#41285=CARTESIAN_POINT('Ctrl Pts',(-3.88813086765443,-0.636309800095255,
4.53933364653334));
#41286=CARTESIAN_POINT('Ctrl Pts',(-3.84690700499389,-0.319434907277188,
4.60282749835033));
#41287=CARTESIAN_POINT('Ctrl Pts',(-3.82843070636847,-0.158333333333347,
4.64126716597781));
#41288=CARTESIAN_POINT('Ctrl Pts',(-3.84484044798012,0.158333333333349,
4.66599872978517));
#41289=CARTESIAN_POINT('Ctrl Pts',(-3.8802125113638,0.319434907277196,4.65293701987225));
#41290=CARTESIAN_POINT('Ctrl Pts',(-3.95387184199184,0.636309800095264,
4.63850292495207));
#41291=CARTESIAN_POINT('Ctrl Pts',(-4.01366771231441,0.794772684000916,
4.61179490949894));
#41292=CARTESIAN_POINT('Ctrl Pts',(-4.09496763252197,1.06847604194675,4.60742569516046));
#41293=CARTESIAN_POINT('Ctrl Pts',(-4.12917353775639,1.18514270861492,4.61118505258874));
#41294=CARTESIAN_POINT('Ctrl Pts',(-4.16239362522605,1.3000000000046,4.6205950384371));
#41295=CARTESIAN_POINT('Ctrl Pts',(-4.04477970179641,-1.30000000000023,
4.41003624342554));
#41296=CARTESIAN_POINT('Ctrl Pts',(-4.02136831371039,-1.18514270861197,
4.41125620031957));
#41297=CARTESIAN_POINT('Ctrl Pts',(-3.99789837729298,-1.06847604194526,
4.42055226385903));
#41298=CARTESIAN_POINT('Ctrl Pts',(-3.94354287066604,-0.794772684000933,
4.46068545227691));
#41299=CARTESIAN_POINT('Ctrl Pts',(-3.90219970141365,-0.636309800095262,
4.51518220755499));
#41300=CARTESIAN_POINT('Ctrl Pts',(-3.86170898623137,-0.319434907277191,
4.57925305208586));
#41301=CARTESIAN_POINT('Ctrl Pts',(-3.84262697093746,-0.158333333333348,
4.61872494239754));
#41302=CARTESIAN_POINT('Ctrl Pts',(-3.85883879658361,0.158333333333351,
4.64323152261604));
#41303=CARTESIAN_POINT('Ctrl Pts',(-3.89409505320355,0.319434907277199,
4.62836362481254));
#41304=CARTESIAN_POINT('Ctrl Pts',(-3.96768464649077,0.636309800095271,
4.6140124978342));
#41305=CARTESIAN_POINT('Ctrl Pts',(-4.02858131432634,0.794772684000922,
4.58756582937971));
#41306=CARTESIAN_POINT('Ctrl Pts',(-4.10809241924047,1.06847604194676,4.58667675920439));
#41307=CARTESIAN_POINT('Ctrl Pts',(-4.14092316209739,1.18514270861494,4.59265010414313));
#41308=CARTESIAN_POINT('Ctrl Pts',(-4.17216723667044,1.30000000000462,4.60498163955622));
#41309=CARTESIAN_POINT('Ctrl Pts',(-4.05315766169742,-1.30000000000024,
4.39308255428406));
#41310=CARTESIAN_POINT('Ctrl Pts',(-4.03176153817544,-1.18514270861198,
4.3914028397508));
#41311=CARTESIAN_POINT('Ctrl Pts',(-4.00973387879023,-1.06847604194527,
4.39854270840336));
#41312=CARTESIAN_POINT('Ctrl Pts',(-3.95738660480989,-0.794772684000944,
4.43541223482741));
#41313=CARTESIAN_POINT('Ctrl Pts',(-3.91512622505095,-0.636309800095271,
4.48986981328023));
#41314=CARTESIAN_POINT('Ctrl Pts',(-3.87511537833164,-0.319434907277196,
4.55426694040123));
#41315=CARTESIAN_POINT('Ctrl Pts',(-3.85635181656492,-0.158333333333351,
4.59570057419642));
#41316=CARTESIAN_POINT('Ctrl Pts',(-3.87336540944652,0.158333333333353,
4.62105810311818));
#41317=CARTESIAN_POINT('Ctrl Pts',(-3.90969641020897,0.319434907277205,
4.60572169867666));
#41318=CARTESIAN_POINT('Ctrl Pts',(-3.98323457595251,0.636309800095281,
4.59146931564705));
#41319=CARTESIAN_POINT('Ctrl Pts',(-4.04374029903339,0.794772684000934,
4.56362142462193));
#41320=CARTESIAN_POINT('Ctrl Pts',(-4.12095507618445,1.06847604194678,4.565645711017));
#41321=CARTESIAN_POINT('Ctrl Pts',(-4.15236704819326,1.18514270861496,4.57378414311225));
#41322=CARTESIAN_POINT('Ctrl Pts',(-4.18176757627142,1.30000000000464,4.58918476872954));
#41323=CARTESIAN_POINT('Ctrl Pts',(-4.05971024575106,-1.30000000000026,
4.37855021491459));
#41324=CARTESIAN_POINT('Ctrl Pts',(-4.03944010098985,-1.185142708612,4.37390448857528));
#41325=CARTESIAN_POINT('Ctrl Pts',(-4.01834201970723,-1.06847604194529,
4.37897822127184));
#41326=CARTESIAN_POINT('Ctrl Pts',(-3.96768853229509,-0.794772684000953,
4.41315345354163));
#41327=CARTESIAN_POINT('Ctrl Pts',(-3.92596056098777,-0.636309800095277,
4.46888157145737));
#41328=CARTESIAN_POINT('Ctrl Pts',(-3.88669101787428,-0.319434907277199,
4.53388301937142));
#41329=CARTESIAN_POINT('Ctrl Pts',(-3.86791555360218,-0.158333333333352,
4.5766746106872));
#41330=CARTESIAN_POINT('Ctrl Pts',(-3.88503542645838,0.158333333333355,
4.60212638313186));
#41331=CARTESIAN_POINT('Ctrl Pts',(-3.92138353528705,0.319434907277208,
4.58543081985728));
#41332=CARTESIAN_POINT('Ctrl Pts',(-3.99460276338386,0.636309800095287,
4.57096049756234));
#41333=CARTESIAN_POINT('Ctrl Pts',(-4.05521956108513,0.794772684000941,
4.54243681909545));
#41334=CARTESIAN_POINT('Ctrl Pts',(-4.13093904277844,1.06847604194679,4.54734319695209));
#41335=CARTESIAN_POINT('Ctrl Pts',(-4.16138437224898,1.18514270861497,4.55751673590934));
#41336=CARTESIAN_POINT('Ctrl Pts',(-4.18949887324812,1.30000000000466,4.57574002464891));
#41337=CARTESIAN_POINT('Ctrl Pts',(-4.06445732467908,-1.30000000000026,
4.36854383193775));
#41338=CARTESIAN_POINT('Ctrl Pts',(-4.04514166945636,-1.185142708612,4.3619891298598));
#41339=CARTESIAN_POINT('Ctrl Pts',(-4.02476778473141,-1.06847604194529,
4.36569082763837));
#41340=CARTESIAN_POINT('Ctrl Pts',(-3.97525531338687,-0.794772684000957,
4.3979368254833));
#41341=CARTESIAN_POINT('Ctrl Pts',(-3.93341152373033,-0.636309800095281,
4.45406514905449));
#41342=CARTESIAN_POINT('Ctrl Pts',(-3.89458212873724,-0.319434907277201,
4.51941368543153));
#41343=CARTESIAN_POINT('Ctrl Pts',(-3.8760499641768,-0.158333333333353,
4.56340730429001));
#41344=CARTESIAN_POINT('Ctrl Pts',(-3.89339287804238,0.158333333333355,
4.58908470969992));
#41345=CARTESIAN_POINT('Ctrl Pts',(-3.92985203416142,0.31943490727721,4.57155721434891));
#41346=CARTESIAN_POINT('Ctrl Pts',(-4.00281797176179,0.636309800095291,
4.55690514198218));
#41347=CARTESIAN_POINT('Ctrl Pts',(-4.06330625342903,0.794772684000946,
4.52768205603544));
#41348=CARTESIAN_POINT('Ctrl Pts',(-4.13790416980033,1.06847604194679,4.53452040294592));
#41349=CARTESIAN_POINT('Ctrl Pts',(-4.16766698018009,1.18514270861497,4.54610951803909));
#41350=CARTESIAN_POINT('Ctrl Pts',(-4.19490192706749,1.30000000000466,4.5663276812336));
#41351=CARTESIAN_POINT('Ctrl Pts',(-4.06705508691299,-1.30000000000026,
4.36271599905377));
#41352=CARTESIAN_POINT('Ctrl Pts',(-4.04819781681766,-1.185142708612,4.35498856748228));
#41353=CARTESIAN_POINT('Ctrl Pts',(-4.02819820124502,-1.06847604194529,
4.35786950352306));
#41354=CARTESIAN_POINT('Ctrl Pts',(-3.97935604178485,-0.794772684000958,
4.38903249348759));
#41355=CARTESIAN_POINT('Ctrl Pts',(-3.93770563105166,-0.636309800095281,
4.44564169612304));
#41356=CARTESIAN_POINT('Ctrl Pts',(-3.89913897665286,-0.319434907277201,
4.51119311873859));
#41357=CARTESIAN_POINT('Ctrl Pts',(-3.88051985306727,-0.158333333333353,
4.55564108778732));
#41358=CARTESIAN_POINT('Ctrl Pts',(-3.89798339080602,0.158333333333356,
4.58144045044047));
#41359=CARTESIAN_POINT('Ctrl Pts',(-3.93464408535983,0.31943490727721,4.56358073874647));
#41360=CARTESIAN_POINT('Ctrl Pts',(-4.00760529664738,0.636309800095291,
4.54897383853482));
#41361=CARTESIAN_POINT('Ctrl Pts',(-4.06817540954463,0.794772684000946,
4.51952082489925));
#41362=CARTESIAN_POINT('Ctrl Pts',(-4.14211531990086,1.06847604194679,4.52744400370944));
#41363=CARTESIAN_POINT('Ctrl Pts',(-4.17143295339994,1.18514270861497,4.53978182164816));
#41364=CARTESIAN_POINT('Ctrl Pts',(-4.19806237294838,1.30000000000466,4.56102780700135));
#41365=CARTESIAN_POINT('Ctrl Pts',(-4.06960995733231,-1.30000000000027,
4.35684872627253));
#41366=CARTESIAN_POINT('Ctrl Pts',(-4.05116147748774,-1.185142708612,4.34790089113822));
#41367=CARTESIAN_POINT('Ctrl Pts',(-4.03151088950341,-1.06847604194529,
4.34993686239268));
#41368=CARTESIAN_POINT('Ctrl Pts',(-3.98333698988926,-0.794772684000959,
4.38001515334615));
#41369=CARTESIAN_POINT('Ctrl Pts',(-3.9419995353561,-0.636309800095282,
4.43722225727209));
#41370=CARTESIAN_POINT('Ctrl Pts',(-3.90370251970226,-0.319434907277201,
4.50298036197511));
#41371=CARTESIAN_POINT('Ctrl Pts',(-3.88490128407447,-0.158333333333353,
4.54778387694354));
#41372=CARTESIAN_POINT('Ctrl Pts',(-3.90248210251331,0.158333333333356,
4.57370156077579));
#41373=CARTESIAN_POINT('Ctrl Pts',(-3.93940097966221,0.319434907277211,
4.55556904755597));
#41374=CARTESIAN_POINT('Ctrl Pts',(-4.01241538664902,0.636309800095292,
4.54106894432917));
#41375=CARTESIAN_POINT('Ctrl Pts',(-4.07312995568607,0.794772684000947,
4.51145405644919));
#41376=CARTESIAN_POINT('Ctrl Pts',(-4.14640902016603,1.0684760419468,4.52045822043791));
#41377=CARTESIAN_POINT('Ctrl Pts',(-4.17526173596065,1.18514270861498,4.53352292266838));
#41378=CARTESIAN_POINT('Ctrl Pts',(-4.20124737579323,1.30000000000467,4.55575475817572));
#41379=CARTESIAN_POINT('Ctrl Pts',(-4.07182740503528,-1.30000000000027,
4.35169963014855));
#41380=CARTESIAN_POINT('Ctrl Pts',(-4.05371561684914,-1.18514270861201,
4.34166407547363));
#41381=CARTESIAN_POINT('Ctrl Pts',(-4.03435707227047,-1.0684760419453,4.34294808869059));
#41382=CARTESIAN_POINT('Ctrl Pts',(-3.98675470495063,-0.794772684000962,
4.37206488238973));
#41383=CARTESIAN_POINT('Ctrl Pts',(-3.94571668949595,-0.636309800095284,
4.42982081128793));
#41384=CARTESIAN_POINT('Ctrl Pts',(-3.90765324417452,-0.319434907277203,
4.49575512646909));
#41385=CARTESIAN_POINT('Ctrl Pts',(-3.88867494866334,-0.158333333333354,
4.54084804338412));
#41386=CARTESIAN_POINT('Ctrl Pts',(-3.90635099096263,0.158333333333356,
4.56686010837275));
#41387=CARTESIAN_POINT('Ctrl Pts',(-3.94349412896054,0.319434907277212,
4.54848825366666));
#41388=CARTESIAN_POINT('Ctrl Pts',(-4.01656674894129,0.636309800095295,
4.53409446564822));
#41389=CARTESIAN_POINT('Ctrl Pts',(-4.07742558185216,0.79477268400095,4.504357605896));
#41390=CARTESIAN_POINT('Ctrl Pts',(-4.15014770605485,1.0684760419468,4.51432989344033));
#41391=CARTESIAN_POINT('Ctrl Pts',(-4.17860290790803,1.18514270861498,4.52804006765191));
#41392=CARTESIAN_POINT('Ctrl Pts',(-4.20403459866709,1.30000000000467,4.55114378230678));
#41393=CARTESIAN_POINT('Ctrl Pts',(-4.07378205567366,-1.30000000000027,
4.34733952649448));
#41394=CARTESIAN_POINT('Ctrl Pts',(-4.05601587975433,-1.18514270861201,
4.33642721040689));
#41395=CARTESIAN_POINT('Ctrl Pts',(-4.03693065025124,-1.0684760419453,4.33708909914715));
#41396=CARTESIAN_POINT('Ctrl Pts',(-3.98979267445783,-0.794772684000963,
4.36535692311163));
#41397=CARTESIAN_POINT('Ctrl Pts',(-3.94881824813616,-0.636309800095285,
4.4233944643206));
#41398=CARTESIAN_POINT('Ctrl Pts',(-3.91093324152037,-0.319434907277203,
4.48945994370647));
#41399=CARTESIAN_POINT('Ctrl Pts',(-3.89195250433436,-0.158333333333354,
4.5349504853283));
#41400=CARTESIAN_POINT('Ctrl Pts',(-3.90971358737913,0.158333333333357,
4.56104504815378));
#41401=CARTESIAN_POINT('Ctrl Pts',(-3.94695751173222,0.319434907277212,
4.54237412458506));
#41402=CARTESIAN_POINT('Ctrl Pts',(-4.01999781572536,0.636309800095296,
4.52798450551081));
#41403=CARTESIAN_POINT('Ctrl Pts',(-4.08088588357391,0.794772684000951,
4.49804108521699));
#41404=CARTESIAN_POINT('Ctrl Pts',(-4.15316659797322,1.0684760419468,4.50888162745255));
#41405=CARTESIAN_POINT('Ctrl Pts',(-4.1813310257165,1.18514270861498,4.52319857025606));
#41406=CARTESIAN_POINT('Ctrl Pts',(-4.2063722382038,1.30000000000467,4.54713998681093));
#41407=CARTESIAN_POINT('Ctrl Pts',(-4.07476796326869,-1.30000000000027,
4.34516801520838));
#41408=CARTESIAN_POINT('Ctrl Pts',(-4.0571842873435,-1.18514270861201,4.33382683689759));
#41409=CARTESIAN_POINT('Ctrl Pts',(-4.03823961387944,-1.0684760419453,4.33418150808252));
#41410=CARTESIAN_POINT('Ctrl Pts',(-3.99132945172717,-0.794772684000963,
4.36202062155324));
#41411=CARTESIAN_POINT('Ctrl Pts',(-3.95035421507057,-0.636309800095285,
4.42016702771697));
#41412=CARTESIAN_POINT('Ctrl Pts',(-3.91255408456978,-0.319434907277203,
4.48629402063484));
#41413=CARTESIAN_POINT('Ctrl Pts',(-3.89359611246056,-0.158333333333354,
4.53200735080797));
#41414=CARTESIAN_POINT('Ctrl Pts',(-3.91140026048978,0.158333333333357,
4.55814338650856));
#41415=CARTESIAN_POINT('Ctrl Pts',(-3.94868044270104,0.319434907277212,
4.53930842922341));
#41416=CARTESIAN_POINT('Ctrl Pts',(-4.02169108565547,0.636309800095296,
4.52490657176991));
#41417=CARTESIAN_POINT('Ctrl Pts',(-4.08257726430552,0.794772684000951,
4.49484203590736));
#41418=CARTESIAN_POINT('Ctrl Pts',(-4.15464328483979,1.0684760419468,4.50612305542115));
#41419=CARTESIAN_POINT('Ctrl Pts',(-4.18267079146387,1.18514270861498,4.5207524088254));
#41420=CARTESIAN_POINT('Ctrl Pts',(-4.20753109473177,1.30000000000467,4.54512798028933));
#41421=CARTESIAN_POINT('Ctrl Pts',(-4.0755963351847,-1.30000000000027,4.343365203512));
#41422=CARTESIAN_POINT('Ctrl Pts',(-4.05817216723079,-1.18514270861201,
4.33167394277198));
#41423=CARTESIAN_POINT('Ctrl Pts',(-4.03934756240527,-1.0684760419453,4.33177550395673));
#41424=CARTESIAN_POINT('Ctrl Pts',(-3.99262367007915,-0.794772684000964,
4.35925390840294));
#41425=CARTESIAN_POINT('Ctrl Pts',(-3.95162253941972,-0.636309800095286,
4.4174663035074));
#41426=CARTESIAN_POINT('Ctrl Pts',(-3.91388933069293,-0.319434907277203,
4.48364095991923));
#41427=CARTESIAN_POINT('Ctrl Pts',(-3.89496806491384,-0.158333333333354,
4.52955769033492));
#41428=CARTESIAN_POINT('Ctrl Pts',(-3.91280861896672,0.158333333333357,
4.55572856504316));
#41429=CARTESIAN_POINT('Ctrl Pts',(-3.95010917144022,0.319434907277213,
4.53674679937419));
#41430=CARTESIAN_POINT('Ctrl Pts',(-4.02308494460944,0.636309800095296,
4.52232393398548));
#41431=CARTESIAN_POINT('Ctrl Pts',(-4.08395642161417,0.794772684000952,
4.49214430080419));
#41432=CARTESIAN_POINT('Ctrl Pts',(-4.15584772598368,1.0684760419468,4.50379674968262));
#41433=CARTESIAN_POINT('Ctrl Pts',(-4.18376742435588,1.18514270861498,4.51869311565342));
#41434=CARTESIAN_POINT('Ctrl Pts',(-4.20848773927385,1.30000000000467,4.54344193424129));
#41435=CARTESIAN_POINT('Ctrl Pts',(-4.07617844698269,-1.30000000000027,
4.34210553749473));
#41436=CARTESIAN_POINT('Ctrl Pts',(-4.05886853271517,-1.18514270861201,
4.33017180869061));
#41437=CARTESIAN_POINT('Ctrl Pts',(-4.04012894708355,-1.0684760419453,4.33009717417551));
#41438=CARTESIAN_POINT('Ctrl Pts',(-3.99353392857743,-0.794772684000964,
4.35732163372633));
#41439=CARTESIAN_POINT('Ctrl Pts',(-3.95250552735942,-0.636309800095285,
4.41557122350499));
#41440=CARTESIAN_POINT('Ctrl Pts',(-3.91481729305289,-0.319434907277203,
4.48177742096665));
#41441=CARTESIAN_POINT('Ctrl Pts',(-3.89592732961037,-0.158333333333354,
4.52784211054421));
#41442=CARTESIAN_POINT('Ctrl Pts',(-3.91379354357892,0.158333333333357,
4.5540374451459));
#41443=CARTESIAN_POINT('Ctrl Pts',(-3.95110567192063,0.319434907277212,
4.53495015271741));
#41444=CARTESIAN_POINT('Ctrl Pts',(-4.02405366565505,0.636309800095296,
4.52050896061406));
#41445=CARTESIAN_POINT('Ctrl Pts',(-4.08490984854949,0.794772684000951,
4.49024337789042));
#41446=CARTESIAN_POINT('Ctrl Pts',(-4.15668026845033,1.0684760419468,4.50215724002482));
#41447=CARTESIAN_POINT('Ctrl Pts',(-4.18452673106562,1.18514270861498,4.51724284036248));
#41448=CARTESIAN_POINT('Ctrl Pts',(-4.20915290087706,1.30000000000467,4.54225697157188));
#41449=CARTESIAN_POINT('Ctrl Pts',(-4.07651119518558,-1.30000000000027,
4.34138587295175));
#41450=CARTESIAN_POINT('Ctrl Pts',(-4.05926672083395,-1.18514270861201,
4.32931375912153));
#41451=CARTESIAN_POINT('Ctrl Pts',(-4.04057572742151,-1.0684760419453,4.32913846182814));
#41452=CARTESIAN_POINT('Ctrl Pts',(-3.99405404511275,-0.794772684000964,
4.35621751616241));
#41453=CARTESIAN_POINT('Ctrl Pts',(-3.95300924305191,-0.636309800095286,
4.41448753386619));
#41454=CARTESIAN_POINT('Ctrl Pts',(-3.91534619356815,-0.319434907277203,
4.48071122904653));
#41455=CARTESIAN_POINT('Ctrl Pts',(-3.8964740374384,-0.158333333333354,
4.52686037862302));
#41456=CARTESIAN_POINT('Ctrl Pts',(-3.91435493136644,0.158333333333357,
4.55306968517405));
#41457=CARTESIAN_POINT('Ctrl Pts',(-3.95167403545791,0.319434907277213,
4.53392243415286));
#41458=CARTESIAN_POINT('Ctrl Pts',(-4.02460616709662,0.636309800095296,
4.51947075644012));
#41459=CARTESIAN_POINT('Ctrl Pts',(-4.08545325821297,0.794772684000952,
4.48915571499051));
#41460=CARTESIAN_POINT('Ctrl Pts',(-4.15715456522845,1.0684760419468,4.50121887134314));
#41461=CARTESIAN_POINT('Ctrl Pts',(-4.18495922253128,1.18514270861498,4.51641261846914));
#41462=CARTESIAN_POINT('Ctrl Pts',(-4.20953169812499,1.30000000000467,4.54157841932003));
#41463=CARTESIAN_POINT('Ctrl Pts',(-4.0806826240262,-1.30000000000026,4.33240215395594));
#41464=CARTESIAN_POINT('Ctrl Pts',(-4.0642693119333,-1.185142708612,4.31861318319468));
#41465=CARTESIAN_POINT('Ctrl Pts',(-4.04619118718315,-1.06847604194529,
4.31718503134182));
#41466=CARTESIAN_POINT('Ctrl Pts',(-4.00058105221098,-0.794772684000956,
4.34244167931267));
#41467=CARTESIAN_POINT('Ctrl Pts',(-3.95928783985939,-0.63630980009528,
4.40092469193015));
#41468=CARTESIAN_POINT('Ctrl Pts',(-3.9219354987454,-0.3194349072772,4.46736338887183));
#41469=CARTESIAN_POINT('Ctrl Pts',(-3.90332070102475,-0.158333333333353,
4.51460279714578));
#41470=CARTESIAN_POINT('Ctrl Pts',(-3.92138590261326,0.158333333333355,
4.54098727600189));
#41471=CARTESIAN_POINT('Ctrl Pts',(-3.95877154922175,0.319434907277209,
4.52106999256588));
#41472=CARTESIAN_POINT('Ctrl Pts',(-4.03148405249346,0.63630980009529,4.50646466195632));
#41473=CARTESIAN_POINT('Ctrl Pts',(-4.0921896614291,0.794772684000944,4.47550072168819));
#41474=CARTESIAN_POINT('Ctrl Pts',(-4.16303645037653,1.06847604194679,4.48944001093828));
#41475=CARTESIAN_POINT('Ctrl Pts',(-4.19033219163003,1.18514270861497,4.50600028157021));
#41476=CARTESIAN_POINT('Ctrl Pts',(-4.21425672433371,1.30000000000466,4.53308702101923));
#41477=CARTESIAN_POINT('Ctrl Pts',(-4.08578157732975,-1.30000000000017,
4.32042629907166));
#41478=CARTESIAN_POINT('Ctrl Pts',(-4.07007024809314,-1.18514270861192,
4.30404680569939));
#41479=CARTESIAN_POINT('Ctrl Pts',(-4.05259844372008,-1.06847604194522,
4.30081044198283));
#41480=CARTESIAN_POINT('Ctrl Pts',(-4.00816803064877,-0.794772684000903,
4.323697053144));
#41481=CARTESIAN_POINT('Ctrl Pts',(-3.96756936439682,-0.636309800095236,
4.38344510315474));
#41482=CARTESIAN_POINT('Ctrl Pts',(-3.93051351281629,-0.319434907277178,
4.45003209527494));
#41483=CARTESIAN_POINT('Ctrl Pts',(-3.91109268706373,-0.158333333333342,
4.49752712836088));
#41484=CARTESIAN_POINT('Ctrl Pts',(-3.92937723674118,0.158333333333344,
4.52411954299308));
#41485=CARTESIAN_POINT('Ctrl Pts',(-3.96770347442269,0.319434907277188,
4.50407794674818));
#41486=CARTESIAN_POINT('Ctrl Pts',(-4.04073898546218,0.636309800095246,
4.48990394827263));
#41487=CARTESIAN_POINT('Ctrl Pts',(-4.10178143156629,0.794772684000887,
4.45866869142062));
#41488=CARTESIAN_POINT('Ctrl Pts',(-4.17122427188609,1.06847604194672,4.47470220563348));
#41489=CARTESIAN_POINT('Ctrl Pts',(-4.19750573591507,1.18514270861489,4.49264029465091));
#41490=CARTESIAN_POINT('Ctrl Pts',(-4.22000943150921,1.30000000000458,4.52157615848325));
#41491=CARTESIAN_POINT('Ctrl Pts',(-4.09331244521649,-1.30000000000017,
4.30275010216493));
#41492=CARTESIAN_POINT('Ctrl Pts',(-4.07889947091004,-1.18514270861191,
4.28280901708745));
#41493=CARTESIAN_POINT('Ctrl Pts',(-4.0624485095636,-1.06847604194521,4.27703120279117));
#41494=CARTESIAN_POINT('Ctrl Pts',(-4.01973534008945,-0.794772684000897,
4.29640328477619));
#41495=CARTESIAN_POINT('Ctrl Pts',(-3.97918498540679,-0.636309800095234,
4.35705200337412));
#41496=CARTESIAN_POINT('Ctrl Pts',(-3.94305310777462,-0.319434907277177,
4.4243589211843));
#41497=CARTESIAN_POINT('Ctrl Pts',(-3.9242643166955,-0.158333333333341,
4.47407181160574));
#41498=CARTESIAN_POINT('Ctrl Pts',(-3.94294764768243,0.158333333333344,
4.50103789779718));
#41499=CARTESIAN_POINT('Ctrl Pts',(-3.98106324580862,0.319434907277186,
4.47918045867553));
#41500=CARTESIAN_POINT('Ctrl Pts',(-4.05394100901404,0.636309800095243,
4.46498994412542));
#41501=CARTESIAN_POINT('Ctrl Pts',(-4.11561930612219,0.794772684000886,
4.43346165272628));
#41502=CARTESIAN_POINT('Ctrl Pts',(-4.18338547543249,1.06847604194672,4.45303985345004));
#41503=CARTESIAN_POINT('Ctrl Pts',(-4.20846400323075,1.18514270861489,4.47335156716181));
#41504=CARTESIAN_POINT('Ctrl Pts',(-4.22928759511669,1.30000000000457,4.50550031693583));
#41505=CARTESIAN_POINT('Ctrl Pts',(-4.09981791650217,-1.30000000000014,
4.28826914137295));
#41506=CARTESIAN_POINT('Ctrl Pts',(-4.08628630099172,-1.18514270861189,
4.26516743964962));
#41507=CARTESIAN_POINT('Ctrl Pts',(-4.07057910070482,-1.06847604194519,
4.25716837306077));
#41508=CARTESIAN_POINT('Ctrl Pts',(-4.02926628976959,-0.794772684000882,
4.27357903746517));
#41509=CARTESIAN_POINT('Ctrl Pts',(-3.98935503195134,-0.636309800095219,
4.33555643280158));
#41510=CARTESIAN_POINT('Ctrl Pts',(-3.95369594844587,-0.319434907277169,
4.40315775455899));
#41511=CARTESIAN_POINT('Ctrl Pts',(-3.93440263235354,-0.158333333333338,
4.45368910120049));
#41512=CARTESIAN_POINT('Ctrl Pts',(-3.95325279450177,0.15833333333334,4.48080656867185));
#41513=CARTESIAN_POINT('Ctrl Pts',(-3.9920825684725,0.31943490727718,4.45834310390304));
#41514=CARTESIAN_POINT('Ctrl Pts',(-4.06474014002973,0.63630980009523,4.44404218515899));
#41515=CARTESIAN_POINT('Ctrl Pts',(-4.12579708803599,0.794772684000868,
4.41107252450283));
#41516=CARTESIAN_POINT('Ctrl Pts',(-4.19234153738619,1.06847604194669,4.43379393986699));
#41517=CARTESIAN_POINT('Ctrl Pts',(-4.21676455980824,1.18514270861486,4.45644933462131));
#41518=CARTESIAN_POINT('Ctrl Pts',(-4.23680597824331,1.30000000000454,4.49192486533015));
#41519=CARTESIAN_POINT('Ctrl Pts',(-4.10447237338379,-1.30000000000009,
4.27614207678306));
#41520=CARTESIAN_POINT('Ctrl Pts',(-4.09194245717073,-1.18514270861184,
4.2508161108859));
#41521=CARTESIAN_POINT('Ctrl Pts',(-4.07697631455589,-1.06847604194515,
4.24119459589098));
#41522=CARTESIAN_POINT('Ctrl Pts',(-4.03677336079552,-0.794772684000851,
4.25524739472406));
#41523=CARTESIAN_POINT('Ctrl Pts',(-3.99658000879901,-0.636309800095196,
4.31752624590585));
#41524=CARTESIAN_POINT('Ctrl Pts',(-3.96131125941241,-0.319434907277159,
4.38536988024674));
#41525=CARTESIAN_POINT('Ctrl Pts',(-3.94221421725175,-0.158333333333332,
4.43711332662375));
#41526=CARTESIAN_POINT('Ctrl Pts',(-3.96153146945923,0.158333333333334,
4.46466796059675));
#41527=CARTESIAN_POINT('Ctrl Pts',(-4.00084366734633,0.319434907277167,
4.44163678847937));
#41528=CARTESIAN_POINT('Ctrl Pts',(-4.07363130377439,0.636309800095206,
4.42756192963099));
#41529=CARTESIAN_POINT('Ctrl Pts',(-4.13491566051425,0.79477268400084,4.39420947636221));
#41530=CARTESIAN_POINT('Ctrl Pts',(-4.2001773567588,1.06847604194665,4.41909437826389));
#41531=CARTESIAN_POINT('Ctrl Pts',(-4.2237055778276,1.18514270861482,4.44321476474922));
#41532=CARTESIAN_POINT('Ctrl Pts',(-4.24251264984492,1.30000000000449,4.48068378576307));
#41533=CARTESIAN_POINT('Ctrl Pts',(-4.1068263035497,-1.30000000000009,4.27010956050353));
#41534=CARTESIAN_POINT('Ctrl Pts',(-4.09477284803651,-1.18514270861184,
4.24364885985208));
#41535=CARTESIAN_POINT('Ctrl Pts',(-4.08016499765827,-1.06847604194515,
4.23320479314715));
#41536=CARTESIAN_POINT('Ctrl Pts',(-4.04051677785084,-0.794772684000851,
4.24607853826344));
#41537=CARTESIAN_POINT('Ctrl Pts',(-4.00023280952129,-0.636309800095196,
4.30855406036573));
#41538=CARTESIAN_POINT('Ctrl Pts',(-3.96518266532825,-0.319434907277159,
4.37654239510443));
#41539=CARTESIAN_POINT('Ctrl Pts',(-3.94621238249089,-0.158333333333332,
4.42892451651668));
#41540=CARTESIAN_POINT('Ctrl Pts',(-3.96570274858202,0.158333333333334,
4.4566379756269));
#41541=CARTESIAN_POINT('Ctrl Pts',(-4.00511469268083,0.319434907277167,
4.43317916190864));
#41542=CARTESIAN_POINT('Ctrl Pts',(-4.07792758948219,0.636309800095206,
4.41917677348901));
#41543=CARTESIAN_POINT('Ctrl Pts',(-4.13939176391744,0.79477268400084,4.38569778430648));
#41544=CARTESIAN_POINT('Ctrl Pts',(-4.20407556081238,1.06847604194665,4.41173100097376));
#41545=CARTESIAN_POINT('Ctrl Pts',(-4.22718893277774,1.18514270861482,4.4366187769645));
#41546=CARTESIAN_POINT('Ctrl Pts',(-4.24541645780335,1.30000000000449,4.47512551407637));
#41547=CARTESIAN_POINT('',(-4.17593868493484,1.2,4.54217455432741));
#41548=CARTESIAN_POINT('Ctrl Pts',(-4.17593868493484,1.2,4.54217455432741));
#41549=CARTESIAN_POINT('Ctrl Pts',(-4.16901601660958,1.21680579524014,4.56259728301513));
#41550=CARTESIAN_POINT('Ctrl Pts',(-4.16300578492447,1.23314690844626,4.58370303854393));
#41551=CARTESIAN_POINT('Ctrl Pts',(-4.1545018888868,1.25329336998206,4.60811707509031));
#41552=CARTESIAN_POINT('Ctrl Pts',(-4.14807300204321,1.2694610942917,4.62828193480215));
#41553=CARTESIAN_POINT('Ctrl Pts',(-4.13466409677427,1.30000000000457,4.66483672975458));
#41554=CARTESIAN_POINT('',(-4.08975874196504,0.653834841344428,4.41138503336645));
#41555=CARTESIAN_POINT('Ctrl Pts',(-4.08975874202889,0.653834841330258,
4.41138503339054));
#41556=CARTESIAN_POINT('Ctrl Pts',(-4.09901811358657,0.718638123439281,
4.42496474813322));
#41557=CARTESIAN_POINT('Ctrl Pts',(-4.10674533909062,0.76741425862607,4.43641655083457));
#41558=CARTESIAN_POINT('Ctrl Pts',(-4.13510310832554,0.949812869163378,
4.47884925432005));
#41559=CARTESIAN_POINT('Ctrl Pts',(-4.15038021112835,1.04737206040077,4.50201743277146));
#41560=CARTESIAN_POINT('Ctrl Pts',(-4.17593868493484,1.2,4.54217455432741));
#41561=CARTESIAN_POINT('',(-4.00955034077163,-0.653834841531101,4.2972416454658));
#41562=CARTESIAN_POINT('Ctrl Pts',(-4.00955034077163,-0.653834841531101,
4.2972416454658));
#41563=CARTESIAN_POINT('Ctrl Pts',(-3.98922114642734,-0.575773430286786,
4.33363222664404));
#41564=CARTESIAN_POINT('Ctrl Pts',(-3.97295095567435,-0.493715214159444,
4.36480298849665));
#41565=CARTESIAN_POINT('Ctrl Pts',(-3.95138355862527,-0.337919910603026,
4.41065868247051));
#41566=CARTESIAN_POINT('Ctrl Pts',(-3.94493706115634,-0.265431772585284,
4.42737607545058));
#41567=CARTESIAN_POINT('Ctrl Pts',(-3.94024074313496,-0.129514456287131,
4.45124910131288));
#41568=CARTESIAN_POINT('Ctrl Pts',(-3.94090248953005,-0.0665357281317122,
4.45942280949019));
#41569=CARTESIAN_POINT('Ctrl Pts',(-3.94821669426181,0.059433837259308,
4.47048031964631));
#41570=CARTESIAN_POINT('Ctrl Pts',(-3.95489966438366,0.122552721787618,
4.47343903772257));
#41571=CARTESIAN_POINT('Ctrl Pts',(-3.97557216957931,0.259899473210395,
4.47332978277809));
#41572=CARTESIAN_POINT('Ctrl Pts',(-3.99068691758134,0.33378875434452,4.46904341456148));
#41573=CARTESIAN_POINT('Ctrl Pts',(-4.03133525559469,0.491508692492687,
4.44985940941304));
#41574=CARTESIAN_POINT('Ctrl Pts',(-4.05855333857085,0.57491234045661,4.43346975741753));
#41575=CARTESIAN_POINT('Ctrl Pts',(-4.08975874199201,0.653834841365264,
4.41138503347903));
#41576=CARTESIAN_POINT('',(-4.05151251933775,-1.2,4.35610367529872));
#41577=CARTESIAN_POINT('Ctrl Pts',(-4.05151251933775,-1.2,4.35610367529872));
#41578=CARTESIAN_POINT('Ctrl Pts',(-4.0362541407868,-1.0595561432162,4.33436606440657));
#41579=CARTESIAN_POINT('Ctrl Pts',(-4.03163913266016,-0.995649072863461,
4.32796968390379));
#41580=CARTESIAN_POINT('Ctrl Pts',(-4.01413485426632,-0.767227637119597,
4.30353523810531));
#41581=CARTESIAN_POINT('Ctrl Pts',(-4.0115930994257,-0.700415831212995,
4.30006328704156));
#41582=CARTESIAN_POINT('Ctrl Pts',(-4.00955034077163,-0.653834841531101,
4.2972416454658));
#41583=CARTESIAN_POINT('Ctrl Pts',(-4.01183482598955,-1.30000000000003,
4.47462271804853));
#41584=CARTESIAN_POINT('Ctrl Pts',(-4.01895306804897,-1.2829962502188,4.45484161273068));
#41585=CARTESIAN_POINT('Ctrl Pts',(-4.02279613541952,-1.27299706132954,
4.44272395376719));
#41586=CARTESIAN_POINT('Ctrl Pts',(-4.03630670458889,-1.23988587305819,
4.40402165458145));
#41587=CARTESIAN_POINT('Ctrl Pts',(-4.0448273625933,-1.21898355874907,4.37962197974009));
#41588=CARTESIAN_POINT('Ctrl Pts',(-4.05151251933775,-1.2,4.35610367529872));
#41589=CARTESIAN_POINT('Origin',(0.,1.25,7.2));
#41590=CARTESIAN_POINT('Origin',(0.,1.2,7.2));
#41591=CARTESIAN_POINT('Origin',(0.,0.92691742076555,7.2));
#41592=CARTESIAN_POINT('Origin',(0.,0.653834841531101,7.2));
#41593=CARTESIAN_POINT('Origin',(0.,0.,7.2));
#41594=CARTESIAN_POINT('Origin',(0.,-0.653834841531101,7.2));
#41595=CARTESIAN_POINT('Origin',(0.,-0.926917420765551,7.2));
#41596=CARTESIAN_POINT('Origin',(0.,-1.2,7.2));
#41597=CARTESIAN_POINT('Origin',(0.,-1.25,7.2));
#41598=CARTESIAN_POINT('Ctrl Pts',(-3.90341546958844,-1.30000000000013,
4.00440153710639));
#41599=CARTESIAN_POINT('Ctrl Pts',(-3.93440493784207,-1.18514270861187,
4.0336361797219));
#41600=CARTESIAN_POINT('Ctrl Pts',(-3.95093219463971,-1.06847604194516,
4.06330904847551));
#41601=CARTESIAN_POINT('Ctrl Pts',(-3.9557028624898,-0.794772684000851,
4.13287170137922));
#41602=CARTESIAN_POINT('Ctrl Pts',(-3.90486897722008,-0.636309800095197,
4.18098202838527));
#41603=CARTESIAN_POINT('Ctrl Pts',(-3.86905149194761,-0.319434907277159,
4.24590423237585));
#41604=CARTESIAN_POINT('Ctrl Pts',(-3.83456187378936,-0.158333333333332,
4.27613804652327));
#41605=CARTESIAN_POINT('Ctrl Pts',(-3.85489608531651,0.158333333333334,
4.30323841603711));
#41606=CARTESIAN_POINT('Ctrl Pts',(-3.9105765830082,0.319434907277167,4.30138357064611));
#41607=CARTESIAN_POINT('Ctrl Pts',(-3.986068422003,0.636309800095206,4.28905845346891));
#41608=CARTESIAN_POINT('Ctrl Pts',(-4.05793460521832,0.794772684000841,
4.27005212095193));
#41609=CARTESIAN_POINT('Ctrl Pts',(-4.08243023811812,1.06847604194587,4.23632262916638));
#41610=CARTESIAN_POINT('Ctrl Pts',(-4.07701141444102,1.18514270861327,4.21920234377186));
#41611=CARTESIAN_POINT('Ctrl Pts',(-4.05557051525711,1.30000000000221,4.199562020176));
#41612=CARTESIAN_POINT('Ctrl Pts',(-3.89104835659712,-1.30000000000013,
4.00648970721449));
#41613=CARTESIAN_POINT('Ctrl Pts',(-3.91970579181625,-1.18514270861187,
4.03618536988084));
#41614=CARTESIAN_POINT('Ctrl Pts',(-3.9345169961985,-1.06847604194516,4.06617305571521));
#41615=CARTESIAN_POINT('Ctrl Pts',(-3.93674627813055,-0.794772684000851,
4.13612524094578));
#41616=CARTESIAN_POINT('Ctrl Pts',(-3.8862642118845,-0.636309800095197,
4.18397173789519));
#41617=CARTESIAN_POINT('Ctrl Pts',(-3.8503244914224,-0.319434907277159,
4.24880110462245));
#41618=CARTESIAN_POINT('Ctrl Pts',(-3.81670994248296,-0.158333333333332,
4.27910948723805));
#41619=CARTESIAN_POINT('Ctrl Pts',(-3.83684904091065,0.158333333333334,
4.3057824152448));
#41620=CARTESIAN_POINT('Ctrl Pts',(-3.89139304806992,0.319434907277167,
4.30329173640962));
#41621=CARTESIAN_POINT('Ctrl Pts',(-3.96674475597724,0.636309800095206,
4.2904613776932));
#41622=CARTESIAN_POINT('Ctrl Pts',(-4.0381808448611,0.794772684000841,4.27150585840089));
#41623=CARTESIAN_POINT('Ctrl Pts',(-4.06526201563984,1.06847604194587,4.23744989520493));
#41624=CARTESIAN_POINT('Ctrl Pts',(-4.06162921507938,1.18514270861327,4.22015646238466));
#41625=CARTESIAN_POINT('Ctrl Pts',(-4.04264117858458,1.30000000000221,4.2003111613139));
#41626=CARTESIAN_POINT('Ctrl Pts',(-3.86661484837121,-1.30000000000009,
4.01111768457726));
#41627=CARTESIAN_POINT('Ctrl Pts',(-3.88996380996409,-1.18514270861183,
4.04060036765782));
#41628=CARTESIAN_POINT('Ctrl Pts',(-3.9009745686697,-1.06847604194513,4.0705809196837));
#41629=CARTESIAN_POINT('Ctrl Pts',(-3.89790790705575,-0.794772684000829,
4.1409921693144));
#41630=CARTESIAN_POINT('Ctrl Pts',(-3.84917492123562,-0.63630980009518,
4.19026026497731));
#41631=CARTESIAN_POINT('Ctrl Pts',(-3.81325488317549,-0.319434907277152,
4.2554023339609));
#41632=CARTESIAN_POINT('Ctrl Pts',(-3.78099858233076,-0.158333333333329,
4.28508308114211));
#41633=CARTESIAN_POINT('Ctrl Pts',(-3.80083048546607,0.158333333333331,
4.31108897200467));
#41634=CARTESIAN_POINT('Ctrl Pts',(-3.85350460551506,0.319434907277162,
4.3081787780579));
#41635=CARTESIAN_POINT('Ctrl Pts',(-3.92862733347231,0.636309800095193,
4.2944512740811));
#41636=CARTESIAN_POINT('Ctrl Pts',(-3.99882638092636,0.794772684000823,
4.27482471898379));
#41637=CARTESIAN_POINT('Ctrl Pts',(-4.03108771157174,1.06847604194584,4.24009901002036));
#41638=CARTESIAN_POINT('Ctrl Pts',(-4.03110099808034,1.18514270861324,4.22258713986118));
#41639=CARTESIAN_POINT('Ctrl Pts',(-4.01716283646121,1.30000000000217,4.2025948722388));
#41640=CARTESIAN_POINT('Ctrl Pts',(-3.84163939128475,-1.30000000000008,
4.01575214899236));
#41641=CARTESIAN_POINT('Ctrl Pts',(-3.86056353497618,-1.18514270861182,
4.04677393771985));
#41642=CARTESIAN_POINT('Ctrl Pts',(-3.86827184668624,-1.06847604194511,
4.07775329050274));
#41643=CARTESIAN_POINT('Ctrl Pts',(-3.8601687731825,-0.794772684000817,
4.14922375730824));
#41644=CARTESIAN_POINT('Ctrl Pts',(-3.81170264137483,-0.636309800095171,
4.19713572363613));
#41645=CARTESIAN_POINT('Ctrl Pts',(-3.77539078952671,-0.319434907277146,
4.26183594430695));
#41646=CARTESIAN_POINT('Ctrl Pts',(-3.74490615950961,-0.158333333333326,
4.2916228682938));
#41647=CARTESIAN_POINT('Ctrl Pts',(-3.76449993658487,0.158333333333328,
4.31711707741851));
#41648=CARTESIAN_POINT('Ctrl Pts',(-3.81530634625955,0.319434907277153,
4.31388176381152));
#41649=CARTESIAN_POINT('Ctrl Pts',(-3.89004642236894,0.63630980009518,4.29895756126248));
#41650=CARTESIAN_POINT('Ctrl Pts',(-3.95862216654278,0.79477268400081,4.27791873481429));
#41651=CARTESIAN_POINT('Ctrl Pts',(-3.99611319657198,1.06847604194582,4.24240864936715));
#41652=CARTESIAN_POINT('Ctrl Pts',(-3.99989511980788,1.18514270861322,4.224777018362));
#41653=CARTESIAN_POINT('Ctrl Pts',(-3.99123048855958,1.30000000000215,4.20488475656349));
#41654=CARTESIAN_POINT('Ctrl Pts',(-3.8286278109767,-1.30000000000007,4.01822206427942));
#41655=CARTESIAN_POINT('Ctrl Pts',(-3.84480093063131,-1.18514270861181,
4.04928111560884));
#41656=CARTESIAN_POINT('Ctrl Pts',(-3.85053359401985,-1.06847604194511,
4.08035218408484));
#41657=CARTESIAN_POINT('Ctrl Pts',(-3.83965765068204,-0.794772684000815,
4.15216033002293));
#41658=CARTESIAN_POINT('Ctrl Pts',(-3.79199422350366,-0.636309800095168,
4.20057565258571));
#41659=CARTESIAN_POINT('Ctrl Pts',(-3.7557711364051,-0.319434907277145,
4.26559035383413));
#41660=CARTESIAN_POINT('Ctrl Pts',(-3.72624824301149,-0.158333333333325,
4.29549393781957));
#41661=CARTESIAN_POINT('Ctrl Pts',(-3.74569302684835,0.158333333333327,
4.32067544009606));
#41662=CARTESIAN_POINT('Ctrl Pts',(-3.79525526709828,0.319434907277153,
4.31675986160739));
#41663=CARTESIAN_POINT('Ctrl Pts',(-3.86987489674091,0.636309800095178,
4.30139527837829));
#41664=CARTESIAN_POINT('Ctrl Pts',(-3.93806495582426,0.794772684000808,
4.28057716166906));
#41665=CARTESIAN_POINT('Ctrl Pts',(-3.97829562722386,1.06847604194582,4.24465368868101));
#41666=CARTESIAN_POINT('Ctrl Pts',(-3.98395365181045,1.18514270861321,4.22675274202847));
#41667=CARTESIAN_POINT('Ctrl Pts',(-3.97785533402799,1.30000000000214,4.20650078908409));
#41668=CARTESIAN_POINT('Ctrl Pts',(-3.82710684528072,-1.30000000000007,
4.01852991983173));
#41669=CARTESIAN_POINT('Ctrl Pts',(-3.84295899747086,-1.18514270861181,
4.04959891491916));
#41670=CARTESIAN_POINT('Ctrl Pts',(-3.84846039396343,-1.06847604194511,
4.08068334373606));
#41671=CARTESIAN_POINT('Ctrl Pts',(-3.83725740408892,-0.794772684000815,
4.15253024772438));
#41672=CARTESIAN_POINT('Ctrl Pts',(-3.78967982079165,-0.636309800095169,
4.20098843507329));
#41673=CARTESIAN_POINT('Ctrl Pts',(-3.75346683494883,-0.319434907277145,
4.26603985549636));
#41674=CARTESIAN_POINT('Ctrl Pts',(-3.72406481821863,-0.158333333333325,
4.29597213108033));
#41675=CARTESIAN_POINT('Ctrl Pts',(-3.74349214685304,0.158333333333327,
4.32111727724511));
#41676=CARTESIAN_POINT('Ctrl Pts',(-3.79290325446431,0.319434907277153,
4.31711286623261));
#41677=CARTESIAN_POINT('Ctrl Pts',(-3.86750330211314,0.636309800095178,
4.30168595699973));
#41678=CARTESIAN_POINT('Ctrl Pts',(-3.93564235693815,0.794772684000808,
4.28088239017744));
#41679=CARTESIAN_POINT('Ctrl Pts',(-3.97619443018704,1.06847604194582,4.24490823250405));
#41680=CARTESIAN_POINT('Ctrl Pts',(-3.98207420706277,1.18514270861321,4.22697751851431));
#41681=CARTESIAN_POINT('Ctrl Pts',(-3.97628027090713,1.30000000000214,4.20668797041776));
#41682=CARTESIAN_POINT('Ctrl Pts',(-3.82444661259715,-1.30000000000007,
4.01907178088306));
#41683=CARTESIAN_POINT('Ctrl Pts',(-3.83974163577605,-1.18514270861181,
4.05016618767936));
#41684=CARTESIAN_POINT('Ctrl Pts',(-3.84484114962181,-1.06847604194511,
4.08127899892876));
#41685=CARTESIAN_POINT('Ctrl Pts',(-3.83306838059555,-0.794772684000815,
4.15319833497988));
#41686=CARTESIAN_POINT('Ctrl Pts',(-3.78563780298979,-0.636309800095169,
4.20172638828723));
#41687=CARTESIAN_POINT('Ctrl Pts',(-3.74943701118573,-0.319434907277146,
4.26683200753139));
#41688=CARTESIAN_POINT('Ctrl Pts',(-3.72023757771806,-0.158333333333325,
4.29679732018735));
#41689=CARTESIAN_POINT('Ctrl Pts',(-3.73963440904793,0.158333333333328,
4.32187909990591));
#41690=CARTESIAN_POINT('Ctrl Pts',(-3.78879227213193,0.319434907277153,
4.31774099149246));
#41691=CARTESIAN_POINT('Ctrl Pts',(-3.86335907746366,0.636309800095178,
4.30220677550402));
#41692=CARTESIAN_POINT('Ctrl Pts',(-3.9313998840663,0.794772684000808,4.28141073634073));
#41693=CARTESIAN_POINT('Ctrl Pts',(-3.97251266409711,1.06847604194582,4.24534445646052));
#41694=CARTESIAN_POINT('Ctrl Pts',(-3.9787810112287,1.18514270861321,4.2273627215518));
#41695=CARTESIAN_POINT('Ctrl Pts',(-3.97352150639511,1.30000000000214,4.20701100790716));
#41696=CARTESIAN_POINT('Ctrl Pts',(-3.81915395213725,-1.30000000000007,
4.02020751913203));
#41697=CARTESIAN_POINT('Ctrl Pts',(-3.83336539572861,-1.18514270861181,
4.05140900057002));
#41698=CARTESIAN_POINT('Ctrl Pts',(-3.83767878966736,-1.06847604194511,
4.08261106947747));
#41699=CARTESIAN_POINT('Ctrl Pts',(-3.82477711776183,-0.794772684000815,
4.15469544777816));
#41700=CARTESIAN_POINT('Ctrl Pts',(-3.7775995078436,-0.636309800095168,
4.20328916354697));
#41701=CARTESIAN_POINT('Ctrl Pts',(-3.74139562495426,-0.319434907277145,
4.26845329303305));
#41702=CARTESIAN_POINT('Ctrl Pts',(-3.7125803976688,-0.158333333333325,
4.29844492512511));
#41703=CARTESIAN_POINT('Ctrl Pts',(-3.73191725698259,0.158333333333327,
4.32340352741718));
#41704=CARTESIAN_POINT('Ctrl Pts',(-3.78061130320096,0.319434907277153,
4.3190820784816));
#41705=CARTESIAN_POINT('Ctrl Pts',(-3.8550990434907,0.636309800095178,4.30330738580016));
#41706=CARTESIAN_POINT('Ctrl Pts',(-3.92287596258615,0.794772684000807,
4.28239104658693));
#41707=CARTESIAN_POINT('Ctrl Pts',(-3.96510110964664,1.06847604194582,4.24612188585345));
#41708=CARTESIAN_POINT('Ctrl Pts',(-3.97215501839537,1.18514270861321,4.22805477717417));
#41709=CARTESIAN_POINT('Ctrl Pts',(-3.96798513432618,1.30000000000214,4.20762013559235));
#41710=CARTESIAN_POINT('Ctrl Pts',(-3.81315583966002,-1.30000000000007,
4.0216054592221));
#41711=CARTESIAN_POINT('Ctrl Pts',(-3.8262311916753,-1.18514270861182,4.05311260169393));
#41712=CARTESIAN_POINT('Ctrl Pts',(-3.82970664459084,-1.06847604194511,
4.08452506541706));
#41713=CARTESIAN_POINT('Ctrl Pts',(-3.81555794871411,-0.794772684000816,
4.15687541380941));
#41714=CARTESIAN_POINT('Ctrl Pts',(-3.76855240047573,-0.63630980009517,
4.20533651202818));
#41715=CARTESIAN_POINT('Ctrl Pts',(-3.73224815440427,-0.319434907277146,
4.27039003013774));
#41716=CARTESIAN_POINT('Ctrl Pts',(-3.70377100950362,-0.158333333333325,
4.30021903851715));
#41717=CARTESIAN_POINT('Ctrl Pts',(-3.72304001329379,0.158333333333328,
4.32504230140401));
#41718=CARTESIAN_POINT('Ctrl Pts',(-3.77135999334345,0.319434907277154,
4.32081643901291));
#41719=CARTESIAN_POINT('Ctrl Pts',(-3.84574495956043,0.63630980009518,4.30473755434541));
#41720=CARTESIAN_POINT('Ctrl Pts',(-3.91304112819147,0.794772684000809,
4.28332116762538));
#41721=CARTESIAN_POINT('Ctrl Pts',(-3.956511644309,1.06847604194582,4.24676844297429));
#41722=CARTESIAN_POINT('Ctrl Pts',(-3.96448243439118,1.18514270861322,4.22864330258963));
#41723=CARTESIAN_POINT('Ctrl Pts',(-3.96160723886955,1.30000000000215,4.2082153419099));
#41724=CARTESIAN_POINT('Ctrl Pts',(-3.80715438504397,-1.30000000000007,
4.02300105414969));
#41725=CARTESIAN_POINT('Ctrl Pts',(-3.81909176514673,-1.18514270861182,
4.05481311590196));
#41726=CARTESIAN_POINT('Ctrl Pts',(-3.82173114234454,-1.06847604194511,
4.08644103377522));
#41727=CARTESIAN_POINT('Ctrl Pts',(-3.80634838490757,-0.794772684000818,
4.15908244200738));
#41728=CARTESIAN_POINT('Ctrl Pts',(-3.75954037010185,-0.636309800095171,
4.20745421948047));
#41729=CARTESIAN_POINT('Ctrl Pts',(-3.72315249890494,-0.319434907277147,
4.27242666413317));
#41730=CARTESIAN_POINT('Ctrl Pts',(-3.69501795631059,-0.158333333333326,
4.30210029916821));
#41731=CARTESIAN_POINT('Ctrl Pts',(-3.71421357862602,0.158333333333328,
4.32678066237708));
#41732=CARTESIAN_POINT('Ctrl Pts',(-3.76214214475683,0.319434907277154,
4.32262400819918));
#41733=CARTESIAN_POINT('Ctrl Pts',(-3.83641121627868,0.636309800095181,
4.30621955644676));
#41734=CARTESIAN_POINT('Ctrl Pts',(-3.90322589564299,0.79477268400081,4.28430194023565));
#41735=CARTESIAN_POINT('Ctrl Pts',(-3.94793323256432,1.06847604194582,4.24744674986031));
#41736=CARTESIAN_POINT('Ctrl Pts',(-3.95681676141385,1.18514270861322,4.22925357514636));
#41737=CARTESIAN_POINT('Ctrl Pts',(-3.9552316695297,1.30000000000215,4.2088204720126));
#41738=CARTESIAN_POINT('Ctrl Pts',(-3.80114234291894,-1.30000000000007,
4.0243783591317));
#41739=CARTESIAN_POINT('Ctrl Pts',(-3.81192416135968,-1.18514270861182,
4.05646416886568));
#41740=CARTESIAN_POINT('Ctrl Pts',(-3.81371945824022,-1.06847604194511,
4.08829360459836));
#41741=CARTESIAN_POINT('Ctrl Pts',(-3.79710629063061,-0.794772684000818,
4.16123369336721));
#41742=CARTESIAN_POINT('Ctrl Pts',(-3.75053327720066,-0.636309800095171,
4.20958397466905));
#41743=CARTESIAN_POINT('Ctrl Pts',(-3.71409328185195,-0.319434907277147,
4.27453344748291));
#41744=CARTESIAN_POINT('Ctrl Pts',(-3.68633034992726,-0.158333333333326,
4.30410581984449));
#41745=CARTESIAN_POINT('Ctrl Pts',(-3.70544254508084,0.158333333333328,
4.3286249931167));
#41746=CARTESIAN_POINT('Ctrl Pts',(-3.75290823669572,0.319434907277154,
4.32440253561861));
#41747=CARTESIAN_POINT('Ctrl Pts',(-3.82707546000951,0.63630980009518,4.30770469251513));
#41748=CARTESIAN_POINT('Ctrl Pts',(-3.89351928822256,0.794772684000811,
4.28550667350574));
#41749=CARTESIAN_POINT('Ctrl Pts',(-3.93946473095619,1.06847604194583,4.24835060648487));
#41750=CARTESIAN_POINT('Ctrl Pts',(-3.94923896567685,1.18514270861322,4.23004437469339));
#41751=CARTESIAN_POINT('Ctrl Pts',(-3.94889935540516,1.30000000000215,4.20951539575585));
#41752=CARTESIAN_POINT('Ctrl Pts',(-3.78440028110535,-1.30000000000008,
4.02778953669477));
#41753=CARTESIAN_POINT('Ctrl Pts',(-3.79171108268268,-1.18514270861182,
4.06011172210803));
#41754=CARTESIAN_POINT('Ctrl Pts',(-3.79101861768583,-1.06847604194512,
4.09220196366834));
#41755=CARTESIAN_POINT('Ctrl Pts',(-3.77092973818161,-0.794772684000821,
4.16580100460297));
#41756=CARTESIAN_POINT('Ctrl Pts',(-3.72537387638473,-0.636309800095172,
4.21473776392922));
#41757=CARTESIAN_POINT('Ctrl Pts',(-3.68913832694495,-0.319434907277146,
4.28025055716962));
#41758=CARTESIAN_POINT('Ctrl Pts',(-3.66274336562862,-0.158333333333326,
4.31018669309415));
#41759=CARTESIAN_POINT('Ctrl Pts',(-3.68168289994384,0.158333333333328,
4.33436533221495));
#41760=CARTESIAN_POINT('Ctrl Pts',(-3.72752328510863,0.319434907277155,
4.32930246592143));
#41761=CARTESIAN_POINT('Ctrl Pts',(-3.80130684170286,0.636309800095182,
4.311624907316));
#41762=CARTESIAN_POINT('Ctrl Pts',(-3.86685632366673,0.794772684000811,
4.2889357991253));
#41763=CARTESIAN_POINT('Ctrl Pts',(-3.9162208030225,1.06847604194583,4.25097921818241));
#41764=CARTESIAN_POINT('Ctrl Pts',(-3.92843965377663,1.18514270861322,4.23234236241147));
#41765=CARTESIAN_POINT('Ctrl Pts',(-3.93150930130592,1.30000000000215,4.21149864832987));
#41766=CARTESIAN_POINT('Ctrl Pts',(-3.75431580962117,-1.30000000000009,
4.03469504713538));
#41767=CARTESIAN_POINT('Ctrl Pts',(-3.75593416776671,-1.18514270861183,
4.06853321701457));
#41768=CARTESIAN_POINT('Ctrl Pts',(-3.75106608557199,-1.06847604194513,
4.10171222975162));
#41769=CARTESIAN_POINT('Ctrl Pts',(-3.72483486705178,-0.794772684000829,
4.17683960175068));
#41770=CARTESIAN_POINT('Ctrl Pts',(-3.68022258902514,-0.636309800095178,
4.22530365278323));
#41771=CARTESIAN_POINT('Ctrl Pts',(-3.64379213672342,-0.31943490727715,
4.29082854797332));
#41772=CARTESIAN_POINT('Ctrl Pts',(-3.61957756337174,-0.158333333333327,
4.32080382713417));
#41773=CARTESIAN_POINT('Ctrl Pts',(-3.63812902402165,0.15833333333333,4.34421786945562));
#41774=CARTESIAN_POINT('Ctrl Pts',(-3.68120840915105,0.319434907277156,
4.33799029755456));
#41775=CARTESIAN_POINT('Ctrl Pts',(-3.75478857736182,0.636309800095186,
4.31947846925158));
#41776=CARTESIAN_POINT('Ctrl Pts',(-3.81957493385749,0.794772684000819,
4.29756971904014));
#41777=CARTESIAN_POINT('Ctrl Pts',(-3.87514362963652,1.06847604194584,4.25811941793536));
#41778=CARTESIAN_POINT('Ctrl Pts',(-3.89158284045524,1.18514270861323,4.23843792787219));
#41779=CARTESIAN_POINT('Ctrl Pts',(-3.90040763271295,1.30000000000216,4.21615152131645));
#41780=CARTESIAN_POINT('Ctrl Pts',(-3.71845854499846,-1.30000000000011,
4.04341913141646));
#41781=CARTESIAN_POINT('Ctrl Pts',(-3.71281545479014,-1.18514270861185,
4.07842216145478));
#41782=CARTESIAN_POINT('Ctrl Pts',(-3.70278387581907,-1.06847604194514,
4.11269641728366));
#41783=CARTESIAN_POINT('Ctrl Pts',(-3.66947063462934,-0.794772684000839,
4.19019319057521));
#41784=CARTESIAN_POINT('Ctrl Pts',(-3.62762195270144,-0.636309800095187,
4.24076083845827));
#41785=CARTESIAN_POINT('Ctrl Pts',(-3.5912064928209,-0.319434907277154,
4.30672857459846));
#41786=CARTESIAN_POINT('Ctrl Pts',(-3.56856204276642,-0.15833333333333,
4.33500412610548));
#41787=CARTESIAN_POINT('Ctrl Pts',(-3.58636155667854,0.158333333333332,
4.35711349894132));
#41788=CARTESIAN_POINT('Ctrl Pts',(-3.62682870546288,0.319434907277161,
4.3508833371881));
#41789=CARTESIAN_POINT('Ctrl Pts',(-3.69945326777052,0.636309800095196,
4.33008113051802));
#41790=CARTESIAN_POINT('Ctrl Pts',(-3.76132565597827,0.79477268400083,4.30531932672598));
#41791=CARTESIAN_POINT('Ctrl Pts',(-3.82420327488111,1.06847604194585,4.2637660533126));
#41792=CARTESIAN_POINT('Ctrl Pts',(-3.84607635354761,1.18514270861325,4.24349148729524));
#41793=CARTESIAN_POINT('Ctrl Pts',(-3.86260511950287,1.30000000000218,4.2209292276207));
#41794=CARTESIAN_POINT('Ctrl Pts',(-3.68860773760897,-1.30000000000011,
4.05087423379425));
#41795=CARTESIAN_POINT('Ctrl Pts',(-3.67760555817564,-1.18514270861185,
4.08800447745914));
#41796=CARTESIAN_POINT('Ctrl Pts',(-3.66363318323603,-1.06847604194514,
4.12379980892036));
#41797=CARTESIAN_POINT('Ctrl Pts',(-3.62449245615642,-0.794772684000841,
4.20341027118856));
#41798=CARTESIAN_POINT('Ctrl Pts',(-3.58335565480229,-0.636309800095186,
4.25310147302822));
#41799=CARTESIAN_POINT('Ctrl Pts',(-3.54690519449343,-0.319434907277153,
4.31936861187515));
#41800=CARTESIAN_POINT('Ctrl Pts',(-3.52667420534236,-0.15833333333333,
4.34804547385783));
#41801=CARTESIAN_POINT('Ctrl Pts',(-3.54433517289505,0.158333333333332,
4.36990767094282));
#41802=CARTESIAN_POINT('Ctrl Pts',(-3.58234467633409,0.319434907277164,
4.36321247602415));
#41803=CARTESIAN_POINT('Ctrl Pts',(-3.65452982167986,0.636309800095198,
4.34123370676381));
#41804=CARTESIAN_POINT('Ctrl Pts',(-3.71489062245268,0.794772684000828,
4.3159194258204));
#41805=CARTESIAN_POINT('Ctrl Pts',(-3.78361743146054,1.06847604194585,4.27215390529769));
#41806=CARTESIAN_POINT('Ctrl Pts',(-3.80964766432572,1.18514270861325,4.25065806866689));
#41807=CARTESIAN_POINT('Ctrl Pts',(-3.83195884101573,1.30000000000218,4.22661086756729));
#41808=CARTESIAN_POINT('Ctrl Pts',(-3.6713578924185,-1.30000000000011,4.05637552490219));
#41809=CARTESIAN_POINT('Ctrl Pts',(-3.65681897753628,-1.18514270861185,
4.0942929127349));
#41810=CARTESIAN_POINT('Ctrl Pts',(-3.6403280952585,-1.06847604194515,4.13077476054769));
#41811=CARTESIAN_POINT('Ctrl Pts',(-3.59772142303366,-0.79477268400084,
4.21173874253912));
#41812=CARTESIAN_POINT('Ctrl Pts',(-3.55785138804934,-0.636309800095187,
4.26226292612346));
#41813=CARTESIAN_POINT('Ctrl Pts',(-3.52149059562518,-0.319434907277154,
4.32889163046889));
#41814=CARTESIAN_POINT('Ctrl Pts',(-3.50238889835621,-0.15833333333333,
4.35729267517949));
#41815=CARTESIAN_POINT('Ctrl Pts',(-3.51943719293129,0.158333333333332,
4.37812398711004));
#41816=CARTESIAN_POINT('Ctrl Pts',(-3.55538048430167,0.319434907277164,
4.37016213958272));
#41817=CARTESIAN_POINT('Ctrl Pts',(-3.62688845923927,0.636309800095198,
4.34676402724258));
#41818=CARTESIAN_POINT('Ctrl Pts',(-3.68630461596718,0.794772684000829,
4.32100136029989));
#41819=CARTESIAN_POINT('Ctrl Pts',(-3.75871889523108,1.06847604194585,4.27621495187951));
#41820=CARTESIAN_POINT('Ctrl Pts',(-3.78740784200528,1.18514270861325,4.25427972662216));
#41821=CARTESIAN_POINT('Ctrl Pts',(-3.81344027727371,1.30000000000218,4.22979565281272));
#41822=CARTESIAN_POINT('Ctrl Pts',(-3.65953806887845,-1.30000000000011,
4.05956467038674));
#41823=CARTESIAN_POINT('Ctrl Pts',(-3.64275164454373,-1.18514270861185,
4.09817936736322));
#41824=CARTESIAN_POINT('Ctrl Pts',(-3.62465461865293,-1.06847604194515,
4.13523172571671));
#41825=CARTESIAN_POINT('Ctrl Pts',(-3.57981911676806,-0.79477268400084,
4.21722077104828));
#41826=CARTESIAN_POINT('Ctrl Pts',(-3.54071399063127,-0.636309800095187,
4.26816764904755));
#41827=CARTESIAN_POINT('Ctrl Pts',(-3.50437272359351,-0.319434907277154,
4.33496727815371));
#41828=CARTESIAN_POINT('Ctrl Pts',(-3.48584156137425,-0.15833333333333,
4.36287047623089));
#41829=CARTESIAN_POINT('Ctrl Pts',(-3.50275255446116,0.158333333333332,
4.38348922139645));
#41830=CARTESIAN_POINT('Ctrl Pts',(-3.53796421858062,0.319434907277164,
4.37580411999686));
#41831=CARTESIAN_POINT('Ctrl Pts',(-3.60922145485592,0.636309800095198,
4.35181948231638));
#41832=CARTESIAN_POINT('Ctrl Pts',(-3.66769099794688,0.794772684000829,
4.32523451559654));
#41833=CARTESIAN_POINT('Ctrl Pts',(-3.74237473288132,1.06847604194585,4.2794300918488));
#41834=CARTESIAN_POINT('Ctrl Pts',(-3.77275449553502,1.18514270861325,4.25704763651013));
#41835=CARTESIAN_POINT('Ctrl Pts',(-3.80118619929431,1.30000000000218,4.23210976365206));
#41836=CARTESIAN_POINT('Ctrl Pts',(-3.64763149426099,-1.30000000000011,
4.06262355022668));
#41837=CARTESIAN_POINT('Ctrl Pts',(-3.62864155950371,-1.18514270861185,
4.10200475472687));
#41838=CARTESIAN_POINT('Ctrl Pts',(-3.60894451243852,-1.06847604194515,
4.13963634627431));
#41839=CARTESIAN_POINT('Ctrl Pts',(-3.56180682244858,-0.79477268400084,
4.22253089499322));
#41840=CARTESIAN_POINT('Ctrl Pts',(-3.52315869206691,-0.636309800095187,
4.2734045470392));
#41841=CARTESIAN_POINT('Ctrl Pts',(-3.4868951844582,-0.319434907277153,
4.34047108936095));
#41842=CARTESIAN_POINT('Ctrl Pts',(-3.46930116449699,-0.15833333333333,
4.36847389132249));
#41843=CARTESIAN_POINT('Ctrl Pts',(-3.48621641437049,0.158333333333332,
4.38910402940942));
#41844=CARTESIAN_POINT('Ctrl Pts',(-3.52056315194149,0.319434907277165,
4.38145890581359));
#41845=CARTESIAN_POINT('Ctrl Pts',(-3.59161287212262,0.636309800095199,
4.35696945019006));
#41846=CARTESIAN_POINT('Ctrl Pts',(-3.64938437719694,0.794772684000828,
4.33002585779554));
#41847=CARTESIAN_POINT('Ctrl Pts',(-3.72617585145565,1.06847604194585,4.28292121233611));
#41848=CARTESIAN_POINT('Ctrl Pts',(-3.75808826963396,1.18514270861325,4.25980910066091));
#41849=CARTESIAN_POINT('Ctrl Pts',(-3.78867292218844,1.30000000000218,4.23397473293081));
#41850=CARTESIAN_POINT('Ctrl Pts',(-3.63356070629899,-1.30000000000011,
4.06771912618167));
#41851=CARTESIAN_POINT('Ctrl Pts',(-3.61190523818026,-1.18514270861185,
4.10821439751999));
#41852=CARTESIAN_POINT('Ctrl Pts',(-3.59025924039026,-1.06847604194514,
4.14666172767279));
#41853=CARTESIAN_POINT('Ctrl Pts',(-3.54027453358219,-0.794772684000836,
4.23075159786));
#41854=CARTESIAN_POINT('Ctrl Pts',(-3.50209435486207,-0.636309800095187,
4.28136659178616));
#41855=CARTESIAN_POINT('Ctrl Pts',(-3.46581721460012,-0.319434907277155,
4.34858660764036));
#41856=CARTESIAN_POINT('Ctrl Pts',(-3.44938662503235,-0.15833333333333,
4.37668899529829));
#41857=CARTESIAN_POINT('Ctrl Pts',(-3.46605537953192,0.158333333333332,
4.39693214740327));
#41858=CARTESIAN_POINT('Ctrl Pts',(-3.49899661499291,0.319434907277164,
4.3888337043609));
#41859=CARTESIAN_POINT('Ctrl Pts',(-3.56954886382728,0.636309800095199,
4.36333478022166));
#41860=CARTESIAN_POINT('Ctrl Pts',(-3.62626490666719,0.79477268400083,4.33560657240965));
#41861=CARTESIAN_POINT('Ctrl Pts',(-3.70599662287337,1.06847604194585,4.28742033396522));
#41862=CARTESIAN_POINT('Ctrl Pts',(-3.74008348373225,1.18514270861325,4.26385395901444));
#41863=CARTESIAN_POINT('Ctrl Pts',(-3.77374429985551,1.30000000000219,4.23757924625945));
#41864=CARTESIAN_POINT('Ctrl Pts',(-3.61556442432805,-1.30000000000011,
4.07212390020608));
#41865=CARTESIAN_POINT('Ctrl Pts',(-3.59052030686365,-1.18514270861186,
4.11364527817067));
#41866=CARTESIAN_POINT('Ctrl Pts',(-3.56647933735157,-1.06847604194515,
4.15297548954064));
#41867=CARTESIAN_POINT('Ctrl Pts',(-3.51325736084816,-0.79477268400084,
4.23877411261215));
#41868=CARTESIAN_POINT('Ctrl Pts',(-3.47636400274692,-0.636309800095187,
4.29023140353388));
#41869=CARTESIAN_POINT('Ctrl Pts',(-3.44039829889856,-0.319434907277154,
4.3581552682494));
#41870=CARTESIAN_POINT('Ctrl Pts',(-3.42520449940565,-0.15833333333333,
4.38612618263592));
#41871=CARTESIAN_POINT('Ctrl Pts',(-3.44162252975853,0.158333333333333,
4.40597806540559));
#41872=CARTESIAN_POINT('Ctrl Pts',(-3.47291449043845,0.319434907277166,
4.39739377561058));
#41873=CARTESIAN_POINT('Ctrl Pts',(-3.54297409043778,0.636309800095201,
4.37085446412307));
#41874=CARTESIAN_POINT('Ctrl Pts',(-3.59866509550172,0.794772684000828,
4.34260442254614));
#41875=CARTESIAN_POINT('Ctrl Pts',(-3.68176721306064,1.06847604194585,4.29282591017169));
#41876=CARTESIAN_POINT('Ctrl Pts',(-3.71830307599038,1.18514270861325,4.26842376765041));
#41877=CARTESIAN_POINT('Ctrl Pts',(-3.75540297439542,1.30000000000219,4.24116675613916));
#41878=CARTESIAN_POINT('Ctrl Pts',(-3.58711823022728,-1.30000000000012,
4.08187617918603));
#41879=CARTESIAN_POINT('Ctrl Pts',(-3.55703818746489,-1.18514270861186,
4.12606687667337));
#41880=CARTESIAN_POINT('Ctrl Pts',(-3.52932505513652,-1.06847604194515,
4.16736681533446));
#41881=CARTESIAN_POINT('Ctrl Pts',(-3.4707702120663,-0.794772684000845,
4.25609970448304));
#41882=CARTESIAN_POINT('Ctrl Pts',(-3.43493185365833,-0.636309800095188,
4.3072299850739));
#41883=CARTESIAN_POINT('Ctrl Pts',(-3.39880756631888,-0.319434907277153,
4.37525690461322));
#41884=CARTESIAN_POINT('Ctrl Pts',(-3.38531233642891,-0.15833333333333,
4.40243413564541));
#41885=CARTESIAN_POINT('Ctrl Pts',(-3.4013848592705,0.158333333333332,4.42178376594812));
#41886=CARTESIAN_POINT('Ctrl Pts',(-3.43075527646008,0.319434907277165,
4.41374302140569));
#41887=CARTESIAN_POINT('Ctrl Pts',(-3.50002009385822,0.636309800095199,
4.38556406417354));
#41888=CARTESIAN_POINT('Ctrl Pts',(-3.55338726970055,0.794772684000829,
4.35551705671428));
#41889=CARTESIAN_POINT('Ctrl Pts',(-3.64165109224554,1.06847604194585,4.3023569314744));
#41890=CARTESIAN_POINT('Ctrl Pts',(-3.68208795061293,1.18514270861325,4.27625721711571));
#41891=CARTESIAN_POINT('Ctrl Pts',(-3.7247555290648,1.30000000000219,4.24706883683798));
#41892=CARTESIAN_POINT('Ctrl Pts',(-3.55260469525799,-1.30000000000013,
4.09307313514165));
#41893=CARTESIAN_POINT('Ctrl Pts',(-3.51599860018384,-1.18514270861187,
4.13977663726978));
#41894=CARTESIAN_POINT('Ctrl Pts',(-3.4836881878147,-1.06847604194516,4.18318196651927));
#41895=CARTESIAN_POINT('Ctrl Pts',(-3.41896855796307,-0.794772684000852,
4.27583752114506));
#41896=CARTESIAN_POINT('Ctrl Pts',(-3.38579619940448,-0.636309800095194,
4.32868261121145));
#41897=CARTESIAN_POINT('Ctrl Pts',(-3.35021088767458,-0.319434907277156,
4.39795974131661));
#41898=CARTESIAN_POINT('Ctrl Pts',(-3.33895965600612,-0.158333333333331,
4.42451926233091));
#41899=CARTESIAN_POINT('Ctrl Pts',(-3.35416769676493,0.158333333333334,
4.44259925854089));
#41900=CARTESIAN_POINT('Ctrl Pts',(-3.3798535907571,0.319434907277166,4.43309851697437));
#41901=CARTESIAN_POINT('Ctrl Pts',(-3.44799190268464,0.636309800095204,
4.40272918236057));
#41902=CARTESIAN_POINT('Ctrl Pts',(-3.49965209936142,0.794772684000837,
4.37224889095022));
#41903=CARTESIAN_POINT('Ctrl Pts',(-3.59461129635381,1.06847604194586,4.31581467525283));
#41904=CARTESIAN_POINT('Ctrl Pts',(-3.63986382502676,1.18514270861326,4.28787725427043));
#41905=CARTESIAN_POINT('Ctrl Pts',(-3.68926456457954,1.3000000000022,4.25643069318731));
#41906=CARTESIAN_POINT('Ctrl Pts',(-3.51930456141979,-1.30000000000012,
4.10610119875616));
#41907=CARTESIAN_POINT('Ctrl Pts',(-3.47679339664398,-1.18514270861187,
4.15620402739542));
#41908=CARTESIAN_POINT('Ctrl Pts',(-3.44027748426465,-1.06847604194516,
4.20225635359855));
#41909=CARTESIAN_POINT('Ctrl Pts',(-3.36976865406716,-0.794772684000851,
4.29928896893633));
#41910=CARTESIAN_POINT('Ctrl Pts',(-3.33846439006812,-0.636309800095195,
4.35256429357893));
#41911=CARTESIAN_POINT('Ctrl Pts',(-3.30350362107075,-0.319434907277157,
4.42313821531253));
#41912=CARTESIAN_POINT('Ctrl Pts',(-3.2950140387051,-0.158333333333331,
4.44979162859018));
#41913=CARTESIAN_POINT('Ctrl Pts',(-3.30974033139481,0.158333333333334,
4.46726854132644));
#41914=CARTESIAN_POINT('Ctrl Pts',(-3.33228828599363,0.319434907277166,
4.4573449276509));
#41915=CARTESIAN_POINT('Ctrl Pts',(-3.39860595874978,0.636309800095204,
4.42389203444187));
#41916=CARTESIAN_POINT('Ctrl Pts',(-3.44700228067872,0.794772684000838,
4.3906779224758));
#41917=CARTESIAN_POINT('Ctrl Pts',(-3.54746472936924,1.06847604194586,4.32916181010615));
#41918=CARTESIAN_POINT('Ctrl Pts',(-3.59712526653284,1.18514270861326,4.29874098381307));
#41919=CARTESIAN_POINT('Ctrl Pts',(-3.65295986932236,1.3000000000022,4.26452737687521));
#41920=CARTESIAN_POINT('Ctrl Pts',(-3.49661091395701,-1.30000000000013,
4.11413655268895));
#41921=CARTESIAN_POINT('Ctrl Pts',(-3.45011915750405,-1.18514270861187,
4.16652547909603));
#41922=CARTESIAN_POINT('Ctrl Pts',(-3.41086452260909,-1.06847604194516,
4.21449705032962));
#41923=CARTESIAN_POINT('Ctrl Pts',(-3.33689766171916,-0.794772684000854,
4.31511600241951));
#41924=CARTESIAN_POINT('Ctrl Pts',(-3.30782791401481,-0.636309800095197,
4.37008747128378));
#41925=CARTESIAN_POINT('Ctrl Pts',(-3.27333584165758,-0.319434907277158,
4.44160920954462));
#41926=CARTESIAN_POINT('Ctrl Pts',(-3.26576691168355,-0.158333333333332,
4.46697499616923));
#41927=CARTESIAN_POINT('Ctrl Pts',(-3.27995148589563,0.158333333333334,
4.48374512833731));
#41928=CARTESIAN_POINT('Ctrl Pts',(-3.30069357725885,0.319434907277166,
4.47396915205645));
#41929=CARTESIAN_POINT('Ctrl Pts',(-3.36613878105895,0.636309800095205,
4.43901119610255));
#41930=CARTESIAN_POINT('Ctrl Pts',(-3.41270262200034,0.794772684000842,
4.40457380667172));
#41931=CARTESIAN_POINT('Ctrl Pts',(-3.51714301368748,1.06847604194587,4.34010113139227));
#41932=CARTESIAN_POINT('Ctrl Pts',(-3.56984368213801,1.18514270861327,4.30813563801336));
#41933=CARTESIAN_POINT('Ctrl Pts',(-3.63003664337549,1.3000000000022,4.27211248343603));
#41934=CARTESIAN_POINT('Ctrl Pts',(-3.48026786811643,-1.30000000000013,
4.12106457332582));
#41935=CARTESIAN_POINT('Ctrl Pts',(-3.43093260187443,-1.18514270861187,
4.17522456495776));
#41936=CARTESIAN_POINT('Ctrl Pts',(-3.38969237482348,-1.06847604194516,
4.22461579029388));
#41937=CARTESIAN_POINT('Ctrl Pts',(-3.31312036019499,-0.794772684000855,
4.32770259736936));
#41938=CARTESIAN_POINT('Ctrl Pts',(-3.2852530347015,-0.636309800095197,
4.38320513518303));
#41939=CARTESIAN_POINT('Ctrl Pts',(-3.25127324659019,-0.319434907277158,
4.45562741250426));
#41940=CARTESIAN_POINT('Ctrl Pts',(-3.24509750630817,-0.158333333333332,
4.4811080411042));
#41941=CARTESIAN_POINT('Ctrl Pts',(-3.25898349185269,0.158333333333334,
4.49753113167441));
#41942=CARTESIAN_POINT('Ctrl Pts',(-3.27800174177641,0.319434907277166,
4.48731914643));
#41943=CARTESIAN_POINT('Ctrl Pts',(-3.34239176789908,0.636309800095205,
4.45070104795185));
#41944=CARTESIAN_POINT('Ctrl Pts',(-3.38742168602886,0.794772684000841,
4.41514966687841));
#41945=CARTESIAN_POINT('Ctrl Pts',(-3.49425950296388,1.06847604194587,4.34772615902328));
#41946=CARTESIAN_POINT('Ctrl Pts',(-3.54892812844116,1.18514270861327,4.31421384968507));
#41947=CARTESIAN_POINT('Ctrl Pts',(-3.61201924717566,1.30000000000221,4.27637436927206));
#41948=CARTESIAN_POINT('Ctrl Pts',(-3.46382778992357,-1.30000000000013,
4.12803241400119));
#41949=CARTESIAN_POINT('Ctrl Pts',(-3.41146750570951,-1.18514270861187,
4.18402399680214));
#41950=CARTESIAN_POINT('Ctrl Pts',(-3.3681873035808,-1.06847604194516,4.23499486878468));
#41951=CARTESIAN_POINT('Ctrl Pts',(-3.28917818457007,-0.794772684000853,
4.3411489333721));
#41952=CARTESIAN_POINT('Ctrl Pts',(-3.26373615514406,-0.636309800095198,
4.39887115096453));
#41953=CARTESIAN_POINT('Ctrl Pts',(-3.22952693615524,-0.319434907277159,
4.47121868105204));
#41954=CARTESIAN_POINT('Ctrl Pts',(-3.22229030655688,-0.158333333333332,
4.49332297409223));
#41955=CARTESIAN_POINT('Ctrl Pts',(-3.23547273092916,0.158333333333335,
4.50884588070143));
#41956=CARTESIAN_POINT('Ctrl Pts',(-3.25440588827726,0.319434907277168,
4.50056659336102));
#41957=CARTESIAN_POINT('Ctrl Pts',(-3.31849342097841,0.636309800095207,
4.46329660824968));
#41958=CARTESIAN_POINT('Ctrl Pts',(-3.36175685995594,0.794772684000843,
4.4262982431313));
#41959=CARTESIAN_POINT('Ctrl Pts',(-3.47143153257499,1.06847604194587,4.35623152583864));
#41960=CARTESIAN_POINT('Ctrl Pts',(-3.52832586892842,1.18514270861327,4.32133830834972));
#41961=CARTESIAN_POINT('Ctrl Pts',(-3.59464043970546,1.3000000000022,4.28188115906025));
#41962=CARTESIAN_POINT('Ctrl Pts',(-3.45023815468823,-1.30000000000013,
4.13378441999163));
#41963=CARTESIAN_POINT('Ctrl Pts',(-3.3960810685282,-1.18514270861187,4.19189169633376));
#41964=CARTESIAN_POINT('Ctrl Pts',(-3.35137666661798,-1.06847604194516,
4.24424595181811));
#41965=CARTESIAN_POINT('Ctrl Pts',(-3.26993814674045,-0.794772684000854,
4.35190412635052));
#41966=CARTESIAN_POINT('Ctrl Pts',(-3.24392557829603,-0.636309800095196,
4.40789981041734));
#41967=CARTESIAN_POINT('Ctrl Pts',(-3.20919341227392,-0.319434907277158,
4.47958200878044));
#41968=CARTESIAN_POINT('Ctrl Pts',(-3.20258671706639,-0.158333333333332,
4.50096078898671));
#41969=CARTESIAN_POINT('Ctrl Pts',(-3.21611606139103,0.158333333333334,
4.51699295065536));
#41970=CARTESIAN_POINT('Ctrl Pts',(-3.23530081306674,0.319434907277167,
4.51069926136688));
#41971=CARTESIAN_POINT('Ctrl Pts',(-3.29952898420167,0.636309800095206,
4.47360253689704));
#41972=CARTESIAN_POINT('Ctrl Pts',(-3.34140203455991,0.79477268400084,4.43565677950861));
#41973=CARTESIAN_POINT('Ctrl Pts',(-3.4532367242705,1.06847604194587,4.36364692568768));
#41974=CARTESIAN_POINT('Ctrl Pts',(-3.51179788486564,1.18514270861327,4.32765145244664));
#41975=CARTESIAN_POINT('Ctrl Pts',(-3.5805111127637,1.3000000000022,4.28683090345569));
#41976=CARTESIAN_POINT('Ctrl Pts',(-3.43424348033285,-1.30000000000013,
4.14136931464995));
#41977=CARTESIAN_POINT('Ctrl Pts',(-3.37761591825326,-1.18514270861187,
4.20224824815626));
#41978=CARTESIAN_POINT('Ctrl Pts',(-3.33084628881046,-1.06847604194516,
4.25630452445111));
#41979=CARTESIAN_POINT('Ctrl Pts',(-3.24557288502897,-0.794772684000852,
4.36542363358686));
#41980=CARTESIAN_POINT('Ctrl Pts',(-3.21802118521138,-0.636309800095197,
4.41840494779706));
#41981=CARTESIAN_POINT('Ctrl Pts',(-3.18186739102292,-0.319434907277158,
4.48844291347954));
#41982=CARTESIAN_POINT('Ctrl Pts',(-3.17601304436626,-0.158333333333332,
4.50871929661483));
#41983=CARTESIAN_POINT('Ctrl Pts',(-3.18946211499878,0.158333333333334,
4.5246793556689));
#41984=CARTESIAN_POINT('Ctrl Pts',(-3.20799122165873,0.319434907277167,
4.51968844978846));
#41985=CARTESIAN_POINT('Ctrl Pts',(-3.27311701935999,0.636309800095206,
4.48353404979024));
#41986=CARTESIAN_POINT('Ctrl Pts',(-3.31545583686005,0.794772684000839,
4.44710357338116));
#41987=CARTESIAN_POINT('Ctrl Pts',(-3.43107074058742,1.06847604194587,4.37346615706425));
#41988=CARTESIAN_POINT('Ctrl Pts',(-3.49192164587793,1.18514270861327,4.3360203117187));
#41989=CARTESIAN_POINT('Ctrl Pts',(-3.5635780485896,1.30000000000221,4.29300353001613));
#41990=CARTESIAN_POINT('Ctrl Pts',(-3.42329004793798,-1.30000000000013,
4.14644476697421));
#41991=CARTESIAN_POINT('Ctrl Pts',(-3.36577675441716,-1.18514270861187,
4.2103224238295));
#41992=CARTESIAN_POINT('Ctrl Pts',(-3.31797563071955,-1.06847604194516,
4.26590655668718));
#41993=CARTESIAN_POINT('Ctrl Pts',(-3.22998252760054,-0.794772684000851,
4.3751573236078));
#41994=CARTESIAN_POINT('Ctrl Pts',(-3.19945051412029,-0.636309800095197,
4.42226516939946));
#41995=CARTESIAN_POINT('Ctrl Pts',(-3.16161671560352,-0.319434907277159,
4.48925446130297));
#41996=CARTESIAN_POINT('Ctrl Pts',(-3.15675867153595,-0.158333333333332,
4.50911671221123));
#41997=CARTESIAN_POINT('Ctrl Pts',(-3.17014714941586,0.158333333333334,
4.52493089062661));
#41998=CARTESIAN_POINT('Ctrl Pts',(-3.18775359149336,0.319434907277167,
4.52028525838109));
#41999=CARTESIAN_POINT('Ctrl Pts',(-3.25416255205695,0.636309800095206,
4.48672549544153));
#42000=CARTESIAN_POINT('Ctrl Pts',(-3.29862160463215,0.794772684000841,
4.45543705365187));
#42001=CARTESIAN_POINT('Ctrl Pts',(-3.41699686809868,1.06847604194587,4.38170451193648));
#42002=CARTESIAN_POINT('Ctrl Pts',(-3.47911206103844,1.18514270861327,4.3429415809095));
#42003=CARTESIAN_POINT('Ctrl Pts',(-3.55210218159892,1.30000000000221,4.29733180410432));
#42004=CARTESIAN_POINT('Ctrl Pts',(-3.41475847117046,-1.30000000000013,
4.14754376664529));
#42005=CARTESIAN_POINT('Ctrl Pts',(-3.35748906958223,-1.18514270861187,
4.21136081832333));
#42006=CARTESIAN_POINT('Ctrl Pts',(-3.30972802388308,-1.06847604194516,
4.26660243158902));
#42007=CARTESIAN_POINT('Ctrl Pts',(-3.22135665799747,-0.794772684000851,
4.37441063103652));
#42008=CARTESIAN_POINT('Ctrl Pts',(-3.18969432988981,-0.636309800095197,
4.41921512013816));
#42009=CARTESIAN_POINT('Ctrl Pts',(-3.15117622767193,-0.319434907277159,
4.48466289159347));
#42010=CARTESIAN_POINT('Ctrl Pts',(-3.14628700527777,-0.158333333333332,
4.50456719074197));
#42011=CARTESIAN_POINT('Ctrl Pts',(-3.15959962456678,0.158333333333334,
4.52015701991036));
#42012=CARTESIAN_POINT('Ctrl Pts',(-3.17704490789093,0.319434907277167,
4.51499029662226));
#42013=CARTESIAN_POINT('Ctrl Pts',(-3.24422091196343,0.636309800095206,
4.48303386330206));
#42014=CARTESIAN_POINT('Ctrl Pts',(-3.29031662464092,0.794772684000841,
4.45500700215256));
#42015=CARTESIAN_POINT('Ctrl Pts',(-3.40898836153085,1.06847604194587,4.38258700702605));
#42016=CARTESIAN_POINT('Ctrl Pts',(-3.47090355779054,1.18514270861327,4.34388949955489));
#42017=CARTESIAN_POINT('Ctrl Pts',(-3.54336535263131,1.30000000000221,4.29784241707766));
#42018=CARTESIAN_POINT('Ctrl Pts',(-3.4147584711704,-1.3,4.14754376664537));
#42019=CARTESIAN_POINT('Ctrl Pts',(-3.35748906958219,-1.18514270861178,
4.21136081832337));
#42020=CARTESIAN_POINT('Ctrl Pts',(-3.30972802388306,-1.06847604194512,
4.26660243158903));
#42021=CARTESIAN_POINT('Ctrl Pts',(-3.22135665799746,-0.794772684000851,
4.37441063103652));
#42022=CARTESIAN_POINT('Ctrl Pts',(-3.18969432988981,-0.636309800095197,
4.41921512013816));
#42023=CARTESIAN_POINT('Ctrl Pts',(-3.15117622767193,-0.319434907277159,
4.48466289159347));
#42024=CARTESIAN_POINT('Ctrl Pts',(-3.14628700527777,-0.158333333333332,
4.50456719074197));
#42025=CARTESIAN_POINT('Ctrl Pts',(-3.15959962456677,0.158333333333334,
4.52015701991036));
#42026=CARTESIAN_POINT('Ctrl Pts',(-3.17704490789093,0.319434907277167,
4.51499029662225));
#42027=CARTESIAN_POINT('Ctrl Pts',(-3.24422091196343,0.636309800095206,
4.48303386330206));
#42028=CARTESIAN_POINT('Ctrl Pts',(-3.29031662464091,0.79477268400084,4.45500700215256));
#42029=CARTESIAN_POINT('Ctrl Pts',(-3.40898836153052,1.06847604194511,4.38258700702625));
#42030=CARTESIAN_POINT('Ctrl Pts',(-3.47090355778974,1.18514270861178,4.34388949955539));
#42031=CARTESIAN_POINT('Ctrl Pts',(-3.54336535262991,1.3,4.29784241707854));
#42032=CARTESIAN_POINT('',(-3.81821580258393,-1.2,4.04980507192042));
#42033=CARTESIAN_POINT('Ctrl Pts',(-3.81821580258393,-1.2,4.04980507192042));
#42034=CARTESIAN_POINT('Ctrl Pts',(-3.79663896512829,-1.21681884435473,
4.05008069226545));
#42035=CARTESIAN_POINT('Ctrl Pts',(-3.77476731607508,-1.23326256677479,
4.04950363407841));
#42036=CARTESIAN_POINT('Ctrl Pts',(-3.73353702923591,-1.26513182561291,
4.04995352778724));
#42037=CARTESIAN_POINT('Ctrl Pts',(-3.70428420443725,-1.28769911124913,
4.05034302515998));
#42038=CARTESIAN_POINT('Ctrl Pts',(-3.68874885778907,-1.30000000000011,
4.05109036900727));
#42039=CARTESIAN_POINT('',(-3.9159353778062,-0.653834841366393,4.17213769856117));
#42040=CARTESIAN_POINT('Ctrl Pts',(-3.91593537783278,-0.653834841365109,
4.17213769853421));
#42041=CARTESIAN_POINT('Ctrl Pts',(-3.90613053706298,-0.717011608251444,
4.1594570945233));
#42042=CARTESIAN_POINT('Ctrl Pts',(-3.89800867385936,-0.763800251277795,
4.14904820577532));
#42043=CARTESIAN_POINT('Ctrl Pts',(-3.86595009357095,-0.949632484189618,
4.10837225465677));
#42044=CARTESIAN_POINT('Ctrl Pts',(-3.84681431306324,-1.05559152095179,
4.08446809663331));
#42045=CARTESIAN_POINT('Ctrl Pts',(-3.81821580258393,-1.2,4.04980507192042));
#42046=CARTESIAN_POINT('',(-3.99970644340963,0.653834841531101,4.28369268310978));
#42047=CARTESIAN_POINT('Ctrl Pts',(-3.99970644340963,0.6538348415311,4.28369268310978));
#42048=CARTESIAN_POINT('Ctrl Pts',(-3.95893262294855,0.57599820463906,4.29175829619443));
#42049=CARTESIAN_POINT('Ctrl Pts',(-3.92430183446496,0.493642228123361,
4.29784729680954));
#42050=CARTESIAN_POINT('Ctrl Pts',(-3.87408300678057,0.338139647427855,
4.30417357553207));
#42051=CARTESIAN_POINT('Ctrl Pts',(-3.85621798073113,0.265662533938239,
4.30517989396827));
#42052=CARTESIAN_POINT('Ctrl Pts',(-3.83201526376916,0.129716559933793,
4.30225619578907));
#42053=CARTESIAN_POINT('Ctrl Pts',(-3.82438757785205,0.0666261450806326,
4.29904673876848));
#42054=CARTESIAN_POINT('Ctrl Pts',(-3.81608778926841,-0.0595425750673727,
4.28861323503182));
#42055=CARTESIAN_POINT('Ctrl Pts',(-3.8153399913931,-0.122776762279469,
4.28132116280713));
#42056=CARTESIAN_POINT('Ctrl Pts',(-3.82180214781733,-0.260118331359305,
4.26160750787843));
#42057=CARTESIAN_POINT('Ctrl Pts',(-3.83048941390645,-0.333929032933066,
4.24848954767565));
#42058=CARTESIAN_POINT('Ctrl Pts',(-3.86113063405387,-0.491198314909897,
4.21574382130922));
#42059=CARTESIAN_POINT('Ctrl Pts',(-3.88506981710094,-0.574355267118962,
4.19514942756914));
#42060=CARTESIAN_POINT('Ctrl Pts',(-3.91593537774962,-0.653834841383305,
4.17213769854369));
#42061=CARTESIAN_POINT('',(-3.95679688799543,1.2,4.22573397505373));
#42062=CARTESIAN_POINT('Ctrl Pts',(-3.95679688799543,1.2,4.22573397505373));
#42063=CARTESIAN_POINT('Ctrl Pts',(-3.96321789915741,1.1438091496454,4.23427612857006));
#42064=CARTESIAN_POINT('Ctrl Pts',(-3.97238904100963,1.06112401913765,4.24651281010962));
#42065=CARTESIAN_POINT('Ctrl Pts',(-3.99275128256726,0.796649264003109,
4.27414929727633));
#42066=CARTESIAN_POINT('Ctrl Pts',(-3.99594086764057,0.739302270217887,
4.27852820761727));
#42067=CARTESIAN_POINT('Ctrl Pts',(-3.99970644340963,0.653834841531101,
4.28369268310978));
#42068=CARTESIAN_POINT('Ctrl Pts',(-3.83164255233655,1.30000000000218,4.22661550567326));
#42069=CARTESIAN_POINT('Ctrl Pts',(-3.85239777077144,1.28312717632915,4.22583975108101));
#42070=CARTESIAN_POINT('Ctrl Pts',(-3.87333078582076,1.26644671368672,4.22568281356069));
#42071=CARTESIAN_POINT('Ctrl Pts',(-3.92060649073197,1.2288596279006,4.22565598187284));
#42072=CARTESIAN_POINT('Ctrl Pts',(-3.93585305697864,1.21625420944408,4.22492296870073));
#42073=CARTESIAN_POINT('Ctrl Pts',(-3.95679688799543,1.2,4.22573397505373));
#42074=CARTESIAN_POINT('Ctrl Pts',(-3.4147584711704,-1.3,4.14754376664537));
#42075=CARTESIAN_POINT('Ctrl Pts',(-3.35748906958219,-1.18514270861178,
4.21136081832337));
#42076=CARTESIAN_POINT('Ctrl Pts',(-3.30972802388306,-1.06847604194512,
4.26660243158904));
#42077=CARTESIAN_POINT('Ctrl Pts',(-3.22135665799747,-0.794772684000851,
4.37441063103652));
#42078=CARTESIAN_POINT('Ctrl Pts',(-3.18969432988981,-0.636309800095197,
4.41921512013816));
#42079=CARTESIAN_POINT('Ctrl Pts',(-3.15117622767193,-0.319434907277159,
4.48466289159347));
#42080=CARTESIAN_POINT('Ctrl Pts',(-3.14628700527777,-0.158333333333332,
4.50456719074198));
#42081=CARTESIAN_POINT('Ctrl Pts',(-3.15959962456678,0.158333333333334,
4.52015701991036));
#42082=CARTESIAN_POINT('Ctrl Pts',(-3.17704490789093,0.319434907277167,
4.51499029662225));
#42083=CARTESIAN_POINT('Ctrl Pts',(-3.24422091196343,0.636309800095206,
4.48303386330206));
#42084=CARTESIAN_POINT('Ctrl Pts',(-3.29031662464091,0.79477268400084,4.45500700215256));
#42085=CARTESIAN_POINT('Ctrl Pts',(-3.40898836153052,1.06847604194511,4.38258700702625));
#42086=CARTESIAN_POINT('Ctrl Pts',(-3.47090355778975,1.18514270861178,4.34388949955539));
#42087=CARTESIAN_POINT('Ctrl Pts',(-3.54336535262991,1.3,4.29784241707854));
#42088=CARTESIAN_POINT('Ctrl Pts',(-3.3620529124905,-1.3,4.09149705970477));
#42089=CARTESIAN_POINT('Ctrl Pts',(-3.30608359416459,-1.18514270861178,
4.15645896441576));
#42090=CARTESIAN_POINT('Ctrl Pts',(-3.25925709076723,-1.06847604194512,
4.21246371570874));
#42091=CARTESIAN_POINT('Ctrl Pts',(-3.17220023180818,-0.794772684000851,
4.32115307863962));
#42092=CARTESIAN_POINT('Ctrl Pts',(-3.14019479937607,-0.636309800095197,
4.36532726831211));
#42093=CARTESIAN_POINT('Ctrl Pts',(-3.10158167219449,-0.319434907277159,
4.43011499929132));
#42094=CARTESIAN_POINT('Ctrl Pts',(-3.09600154123356,-0.158333333333332,
4.44898774758743));
#42095=CARTESIAN_POINT('Ctrl Pts',(-3.10958091369845,0.158333333333334,
4.46433739111742));
#42096=CARTESIAN_POINT('Ctrl Pts',(-3.12797987732075,0.319434907277167,
4.45996561795205));
#42097=CARTESIAN_POINT('Ctrl Pts',(-3.19580237328514,0.636309800095206,
4.42817268205552));
#42098=CARTESIAN_POINT('Ctrl Pts',(-3.24248906837777,0.79477268400084,4.40055292989982));
#42099=CARTESIAN_POINT('Ctrl Pts',(-3.36042187227873,1.06847604194511,4.32673352218863));
#42100=CARTESIAN_POINT('Ctrl Pts',(-3.42167579733126,1.18514270861178,4.28702682229126));
#42101=CARTESIAN_POINT('Ctrl Pts',(-3.49313490646867,1.3,4.23956710881605));
#42102=CARTESIAN_POINT('Ctrl Pts',(-3.3093473538106,-1.3,4.03545035276417));
#42103=CARTESIAN_POINT('Ctrl Pts',(-3.25467811874699,-1.18514270861178,
4.10155711050815));
#42104=CARTESIAN_POINT('Ctrl Pts',(-3.20878615765139,-1.06847604194512,
4.15832499982844));
#42105=CARTESIAN_POINT('Ctrl Pts',(-3.12304380561889,-0.794772684000851,
4.26789552624273));
#42106=CARTESIAN_POINT('Ctrl Pts',(-3.09069526886232,-0.636309800095197,
4.31143941648607));
#42107=CARTESIAN_POINT('Ctrl Pts',(-3.05198711671704,-0.319434907277159,
4.37556710698916));
#42108=CARTESIAN_POINT('Ctrl Pts',(-3.04571607718935,-0.158333333333332,
4.39340830443289));
#42109=CARTESIAN_POINT('Ctrl Pts',(-3.05956220283012,0.158333333333334,
4.40851776232448));
#42110=CARTESIAN_POINT('Ctrl Pts',(-3.07891484675056,0.319434907277167,
4.40494093928184));
#42111=CARTESIAN_POINT('Ctrl Pts',(-3.14738383460685,0.636309800095206,
4.37331150080897));
#42112=CARTESIAN_POINT('Ctrl Pts',(-3.19466151211463,0.79477268400084,4.34609885764707));
#42113=CARTESIAN_POINT('Ctrl Pts',(-3.31185538302693,1.06847604194511,4.27088003735101));
#42114=CARTESIAN_POINT('Ctrl Pts',(-3.37244803687278,1.18514270861178,4.23016414502714));
#42115=CARTESIAN_POINT('Ctrl Pts',(-3.44290446030743,1.3,4.18129180055356));
#42116=CARTESIAN_POINT('Ctrl Pts',(-3.25664179513071,-1.3,3.97940364582358));
#42117=CARTESIAN_POINT('Ctrl Pts',(-3.20327264332939,-1.18514270861178,
4.04665525660054));
#42118=CARTESIAN_POINT('Ctrl Pts',(-3.15831522453555,-1.06847604194512,
4.10418628394814));
#42119=CARTESIAN_POINT('Ctrl Pts',(-3.0738873794296,-0.794772684000851,
4.21463797384583));
#42120=CARTESIAN_POINT('Ctrl Pts',(-3.04119573834857,-0.636309800095197,
4.25755156466003));
#42121=CARTESIAN_POINT('Ctrl Pts',(-3.0023925612396,-0.319434907277159,
4.321019214687));
#42122=CARTESIAN_POINT('Ctrl Pts',(-2.99543061314513,-0.158333333333332,
4.33782886127834));
#42123=CARTESIAN_POINT('Ctrl Pts',(-3.00954349196179,0.158333333333334,
4.35269813353154));
#42124=CARTESIAN_POINT('Ctrl Pts',(-3.02984981618038,0.319434907277167,
4.34991626061163));
#42125=CARTESIAN_POINT('Ctrl Pts',(-3.09896529592856,0.636309800095206,
4.31845031956243));
#42126=CARTESIAN_POINT('Ctrl Pts',(-3.14683395585149,0.79477268400084,4.29164478539433));
#42127=CARTESIAN_POINT('Ctrl Pts',(-3.26328889377514,1.06847604194511,4.21502655251339));
#42128=CARTESIAN_POINT('Ctrl Pts',(-3.32322027641429,1.18514270861178,4.17330146776301));
#42129=CARTESIAN_POINT('Ctrl Pts',(-3.39267401414619,1.3,4.12301649229107));
#42130=CARTESIAN_POINT('Ctrl Pts',(-3.2566417951307,-1.3,3.97940364582357));
#42131=CARTESIAN_POINT('Ctrl Pts',(-3.20327264332939,-1.18514270861178,
4.04665525660054));
#42132=CARTESIAN_POINT('Ctrl Pts',(-3.15831522453555,-1.06847604194512,
4.10418628394814));
#42133=CARTESIAN_POINT('Ctrl Pts',(-3.0738873794296,-0.794772684000851,
4.21463797384583));
#42134=CARTESIAN_POINT('Ctrl Pts',(-3.04119573834857,-0.636309800095197,
4.25755156466003));
#42135=CARTESIAN_POINT('Ctrl Pts',(-3.0023925612396,-0.319434907277159,
4.321019214687));
#42136=CARTESIAN_POINT('Ctrl Pts',(-2.99543061314513,-0.158333333333332,
4.33782886127834));
#42137=CARTESIAN_POINT('Ctrl Pts',(-3.00954349196179,0.158333333333334,
4.35269813353154));
#42138=CARTESIAN_POINT('Ctrl Pts',(-3.02984981618038,0.319434907277167,
4.34991626061163));
#42139=CARTESIAN_POINT('Ctrl Pts',(-3.09896529592856,0.636309800095206,
4.31845031956243));
#42140=CARTESIAN_POINT('Ctrl Pts',(-3.14683395585149,0.79477268400084,4.29164478539433));
#42141=CARTESIAN_POINT('Ctrl Pts',(-3.26328889377514,1.06847604194511,4.21502655251339));
#42142=CARTESIAN_POINT('Ctrl Pts',(-3.32322027641429,1.18514270861178,4.17330146776301));
#42143=CARTESIAN_POINT('Ctrl Pts',(-3.39267401414619,1.3,4.12301649229107));
#42144=CARTESIAN_POINT('Ctrl Pts',(-3.25664179513354,-1.30000000000611,
3.97940364582));
#42145=CARTESIAN_POINT('Ctrl Pts',(-3.20327264333099,-1.18514270861592,
4.0466552565985));
#42146=CARTESIAN_POINT('Ctrl Pts',(-3.15831522453619,-1.06847604194722,
4.10418628394729));
#42147=CARTESIAN_POINT('Ctrl Pts',(-3.0738873794296,-0.794772684000851,
4.21463797384583));
#42148=CARTESIAN_POINT('Ctrl Pts',(-3.04119573834857,-0.636309800095196,
4.25755156466002));
#42149=CARTESIAN_POINT('Ctrl Pts',(-3.0023925612396,-0.319434907277159,
4.321019214687));
#42150=CARTESIAN_POINT('Ctrl Pts',(-2.99543061314513,-0.158333333333332,
4.33782886127834));
#42151=CARTESIAN_POINT('Ctrl Pts',(-3.00954349196179,0.158333333333335,
4.35269813353154));
#42152=CARTESIAN_POINT('Ctrl Pts',(-3.02984981618038,0.319434907277167,
4.34991626061163));
#42153=CARTESIAN_POINT('Ctrl Pts',(-3.09896529592856,0.636309800095206,
4.31845031956243));
#42154=CARTESIAN_POINT('Ctrl Pts',(-3.1468339558515,0.79477268400084,4.29164478539433));
#42155=CARTESIAN_POINT('Ctrl Pts',(-3.26328889377516,1.06847604194515,4.21502655251339));
#42156=CARTESIAN_POINT('Ctrl Pts',(-3.32322027641433,1.18514270861185,4.17330146776299));
#42157=CARTESIAN_POINT('Ctrl Pts',(-3.39267401414626,1.30000000000011,4.12301649229103));
#42158=CARTESIAN_POINT('Ctrl Pts',(-3.25806285817801,-1.30000000000611,
3.97076805174582));
#42159=CARTESIAN_POINT('Ctrl Pts',(-3.205073391371,-1.18514270861592,4.03859080490488));
#42160=CARTESIAN_POINT('Ctrl Pts',(-3.1600300020756,-1.06847604194722,4.09631389470334));
#42161=CARTESIAN_POINT('Ctrl Pts',(-3.07432779056413,-0.794772684000851,
4.20633353680762));
#42162=CARTESIAN_POINT('Ctrl Pts',(-3.03856351369519,-0.636309800095196,
4.24727850529637));
#42163=CARTESIAN_POINT('Ctrl Pts',(-2.99824596803585,-0.319434907277159,
4.3098157201942));
#42164=CARTESIAN_POINT('Ctrl Pts',(-2.99178541067128,-0.158333333333332,
4.32684011158175));
#42165=CARTESIAN_POINT('Ctrl Pts',(-3.00611348034728,0.158333333333335,
4.34180827774425));
#42166=CARTESIAN_POINT('Ctrl Pts',(-3.02637472769607,0.319434907277167,
4.33905301707054));
#42167=CARTESIAN_POINT('Ctrl Pts',(-3.0969517540897,0.636309800095206,4.30842876377872));
#42168=CARTESIAN_POINT('Ctrl Pts',(-3.14699300261569,0.79477268400084,4.28298811859785));
#42169=CARTESIAN_POINT('Ctrl Pts',(-3.26484306624896,1.06847604194515,4.20689686568334));
#42170=CARTESIAN_POINT('Ctrl Pts',(-3.32511928141128,1.18514270861185,4.16516772553438));
#42171=CARTESIAN_POINT('Ctrl Pts',(-3.39465878596431,1.30000000000011,4.11464652916436));
#42172=CARTESIAN_POINT('Ctrl Pts',(-3.26355683794006,-1.30000000000611,
3.95979817224215));
#42173=CARTESIAN_POINT('Ctrl Pts',(-3.21328208042939,-1.18514270861592,
4.0265607791208));
#42174=CARTESIAN_POINT('Ctrl Pts',(-3.16968027363,-1.06847604194722,4.08316229727592));
#42175=CARTESIAN_POINT('Ctrl Pts',(-3.08436722847501,-0.794772684000851,
4.19044897963791));
#42176=CARTESIAN_POINT('Ctrl Pts',(-3.04372887954816,-0.636309800095196,
4.22876197668635));
#42177=CARTESIAN_POINT('Ctrl Pts',(-3.00097363294721,-0.319434907277158,
4.28975854866143));
#42178=CARTESIAN_POINT('Ctrl Pts',(-2.9940717486982,-0.158333333333332,
4.30766530460587));
#42179=CARTESIAN_POINT('Ctrl Pts',(-3.00853457043408,0.158333333333334,
4.32270439001546));
#42180=CARTESIAN_POINT('Ctrl Pts',(-3.02930099488942,0.319434907277168,
4.31898820290654));
#42181=CARTESIAN_POINT('Ctrl Pts',(-3.10273462440665,0.636309800095207,
4.29035353222686));
#42182=CARTESIAN_POINT('Ctrl Pts',(-3.15832171757233,0.794772684000839,
4.2685072783921));
#42183=CARTESIAN_POINT('Ctrl Pts',(-3.27575339640767,1.06847604194515,4.19510813771776));
#42184=CARTESIAN_POINT('Ctrl Pts',(-3.33439709308209,1.18514270861185,4.15424263112017));
#42185=CARTESIAN_POINT('Ctrl Pts',(-3.40085266393565,1.30000000000011,4.10428338621672));
#42186=CARTESIAN_POINT('Ctrl Pts',(-3.27139143945092,-1.30000000000611,
3.94354916079341));
#42187=CARTESIAN_POINT('Ctrl Pts',(-3.2236147785624,-1.18514270861592,4.00762409194011));
#42188=CARTESIAN_POINT('Ctrl Pts',(-3.1817037058285,-1.06847604194722,4.06211089398943));
#42189=CARTESIAN_POINT('Ctrl Pts',(-3.09843142557671,-0.794772684000852,
4.16583581045613));
#42190=CARTESIAN_POINT('Ctrl Pts',(-3.05636248871783,-0.636309800095195,
4.20354929061984));
#42191=CARTESIAN_POINT('Ctrl Pts',(-3.0127970512512,-0.319434907277157,
4.26358364111853));
#42192=CARTESIAN_POINT('Ctrl Pts',(-3.00456157037485,-0.158333333333332,
4.28203282078132));
#42193=CARTESIAN_POINT('Ctrl Pts',(-3.01907439990511,0.158333333333334,
4.29714778439741));
#42194=CARTESIAN_POINT('Ctrl Pts',(-3.04094799380849,0.319434907277168,
4.29274048634797));
#42195=CARTESIAN_POINT('Ctrl Pts',(-3.11585675460528,0.636309800095206,
4.2656800191969));
#42196=CARTESIAN_POINT('Ctrl Pts',(-3.17432845417982,0.794772684000837,
4.24572071661066));
#42197=CARTESIAN_POINT('Ctrl Pts',(-3.28992154460439,1.06847604194514,4.17598916099776));
#42198=CARTESIAN_POINT('Ctrl Pts',(-3.34665848187483,1.18514270861185,4.13699699483715));
#42199=CARTESIAN_POINT('Ctrl Pts',(-3.41009639071706,1.30000000000011,4.08919686913195));
#42200=CARTESIAN_POINT('Ctrl Pts',(-3.27795985063405,-1.30000000000611,
3.93013440105912));
#42201=CARTESIAN_POINT('Ctrl Pts',(-3.23176837726564,-1.18514270861592,
3.99193424901875));
#42202=CARTESIAN_POINT('Ctrl Pts',(-3.19110448689979,-1.06847604194722,
4.04484845525556));
#42203=CARTESIAN_POINT('Ctrl Pts',(-3.10993258789721,-0.79477268400085,
4.14656324716606));
#42204=CARTESIAN_POINT('Ctrl Pts',(-3.06862068700424,-0.636309800095195,
4.18572618426736));
#42205=CARTESIAN_POINT('Ctrl Pts',(-3.0248287334282,-0.319434907277157,
4.24554097765999));
#42206=CARTESIAN_POINT('Ctrl Pts',(-3.01456605891873,-0.158333333333332,
4.26346731127332));
#42207=CARTESIAN_POINT('Ctrl Pts',(-3.02863558681848,0.158333333333334,
4.27820542858103));
#42208=CARTESIAN_POINT('Ctrl Pts',(-3.05144876662552,0.319434907277168,
4.27337147994046));
#42209=CARTESIAN_POINT('Ctrl Pts',(-3.12699347516112,0.636309800095206,
4.24692940859356));
#42210=CARTESIAN_POINT('Ctrl Pts',(-3.18702881370645,0.794772684000838,
4.22764105496139));
#42211=CARTESIAN_POINT('Ctrl Pts',(-3.30082919306778,1.06847604194514,4.16015384976511));
#42212=CARTESIAN_POINT('Ctrl Pts',(-3.35602879228581,1.18514270861185,4.12243609134989));
#42213=CARTESIAN_POINT('Ctrl Pts',(-3.41716802321599,1.30000000000011,4.07621328500152));
#42214=CARTESIAN_POINT('Ctrl Pts',(-3.28595994929404,-1.30000000000611,
3.91027551687813));
#42215=CARTESIAN_POINT('Ctrl Pts',(-3.2420905880153,-1.18514270861592,3.968611702584));
#42216=CARTESIAN_POINT('Ctrl Pts',(-3.20336557148759,-1.06847604194722,
4.01919298846687));
#42217=CARTESIAN_POINT('Ctrl Pts',(-3.12578750189388,-0.794772684000852,
4.11813050765343));
#42218=CARTESIAN_POINT('Ctrl Pts',(-3.08610042440403,-0.636309800095197,
4.1596488236161));
#42219=CARTESIAN_POINT('Ctrl Pts',(-3.04324732235638,-0.319434907277159,
4.22008752447184));
#42220=CARTESIAN_POINT('Ctrl Pts',(-3.0309531963189,-0.158333333333332,
4.23806527243021));
#42221=CARTESIAN_POINT('Ctrl Pts',(-3.04589376909181,0.158333333333335,
4.25365591864516));
#42222=CARTESIAN_POINT('Ctrl Pts',(-3.07203097741551,0.319434907277168,
4.25007434060128));
#42223=CARTESIAN_POINT('Ctrl Pts',(-3.14755245954411,0.636309800095207,
4.22382572574053));
#42224=CARTESIAN_POINT('Ctrl Pts',(-3.20561951200525,0.794772684000841,
4.20171706188599));
#42225=CARTESIAN_POINT('Ctrl Pts',(-3.3156778941382,1.06847604194515,4.13672768270597));
#42226=CARTESIAN_POINT('Ctrl Pts',(-3.36881803271244,1.18514270861185,4.10116981737023));
#42227=CARTESIAN_POINT('Ctrl Pts',(-3.42745811430053,1.30000000000011,4.05818558085193));
#42228=CARTESIAN_POINT('Ctrl Pts',(-3.29748931314334,-1.30000000000611,
3.88213052763613));
#42229=CARTESIAN_POINT('Ctrl Pts',(-3.2569492466075,-1.18514270861592,3.93577431355857));
#42230=CARTESIAN_POINT('Ctrl Pts',(-3.22092245125702,-1.06847604194722,
3.98315214489975));
#42231=CARTESIAN_POINT('Ctrl Pts',(-3.14811990617741,-0.794772684000853,
4.07812880461706));
#42232=CARTESIAN_POINT('Ctrl Pts',(-3.10947546491154,-0.636309800095198,
4.12194180838791));
#42233=CARTESIAN_POINT('Ctrl Pts',(-3.06883066630633,-0.319434907277159,
4.18411013249147));
#42234=CARTESIAN_POINT('Ctrl Pts',(-3.05699213746686,-0.158333333333333,
4.20506573259321));
#42235=CARTESIAN_POINT('Ctrl Pts',(-3.07256295007946,0.158333333333335,
4.22128286789914));
#42236=CARTESIAN_POINT('Ctrl Pts',(-3.0991454499967,0.319434907277169,4.21564572797228));
#42237=CARTESIAN_POINT('Ctrl Pts',(-3.17319108942998,0.636309800095209,
4.18834107734958));
#42238=CARTESIAN_POINT('Ctrl Pts',(-3.23007521026095,0.794772684000841,
4.16375332661296));
#42239=CARTESIAN_POINT('Ctrl Pts',(-3.33538101452519,1.06847604194515,4.10257677300761));
#42240=CARTESIAN_POINT('Ctrl Pts',(-3.38579275753287,1.18514270861186,4.07009490138206));
#42241=CARTESIAN_POINT('Ctrl Pts',(-3.44103326284687,1.30000000000012,4.03161222137201));
#42242=CARTESIAN_POINT('Ctrl Pts',(-3.30875979617058,-1.30000000000611,
3.85378158568818));
#42243=CARTESIAN_POINT('Ctrl Pts',(-3.27064737527123,-1.18514270861592,
3.9019632576688));
#42244=CARTESIAN_POINT('Ctrl Pts',(-3.23673083703896,-1.06847604194722,
3.94561126100005));
#42245=CARTESIAN_POINT('Ctrl Pts',(-3.16807017708734,-0.794772684000851,
4.03597319891018));
#42246=CARTESIAN_POINT('Ctrl Pts',(-3.13150462642579,-0.636309800095197,
4.0827832669738));
#42247=CARTESIAN_POINT('Ctrl Pts',(-3.09279402632734,-0.319434907277159,
4.146306287326));
#42248=CARTESIAN_POINT('Ctrl Pts',(-3.08017399670196,-0.158333333333332,
4.16914997500591));
#42249=CARTESIAN_POINT('Ctrl Pts',(-3.09653279165281,0.158333333333335,
4.18611012399854));
#42250=CARTESIAN_POINT('Ctrl Pts',(-3.12489551101782,0.319434907277167,
4.17959188889426));
#42251=CARTESIAN_POINT('Ctrl Pts',(-3.19818276051303,0.636309800095207,
4.15190830177058));
#42252=CARTESIAN_POINT('Ctrl Pts',(-3.25373505452989,0.794772684000841,
4.12473716299461));
#42253=CARTESIAN_POINT('Ctrl Pts',(-3.35449395304018,1.06847604194515,4.06769620182046));
#42254=CARTESIAN_POINT('Ctrl Pts',(-3.40226962042289,1.18514270861185,4.03845444996479));
#42255=CARTESIAN_POINT('Ctrl Pts',(-3.45420616150834,1.30000000000011,4.00466186476983));
#42256=CARTESIAN_POINT('Ctrl Pts',(-3.32193490365172,-1.30000000000611,
3.81588673765455));
#42257=CARTESIAN_POINT('Ctrl Pts',(-3.2875391164165,-1.18514270861592,3.85747304046494));
#42258=CARTESIAN_POINT('Ctrl Pts',(-3.25661318991723,-1.06847604194721,
3.8965122795001));
#42259=CARTESIAN_POINT('Ctrl Pts',(-3.19318418543743,-0.794772684000845,
3.98081650458433));
#42260=CARTESIAN_POINT('Ctrl Pts',(-3.15739817658905,-0.636309800095194,
4.02997403698598));
#42261=CARTESIAN_POINT('Ctrl Pts',(-3.12146849871559,-0.319434907277158,
4.09548539166518));
#42262=CARTESIAN_POINT('Ctrl Pts',(-3.11025557411671,-0.158333333333332,
4.12276309903158));
#42263=CARTESIAN_POINT('Ctrl Pts',(-3.1275586928241,0.158333333333334,4.14054924283807));
#42264=CARTESIAN_POINT('Ctrl Pts',(-3.15583820679444,0.319434907277169,
4.13078769536379));
#42265=CARTESIAN_POINT('Ctrl Pts',(-3.2274948848356,0.636309800095207,4.10205537276763));
#42266=CARTESIAN_POINT('Ctrl Pts',(-3.28207121742321,0.794772684000837,
4.07229262101088));
#42267=CARTESIAN_POINT('Ctrl Pts',(-3.37785103265727,1.06847604194514,4.02135229624977));
#42268=CARTESIAN_POINT('Ctrl Pts',(-3.42272547575968,1.18514270861185,3.99670187214208));
#42269=CARTESIAN_POINT('Ctrl Pts',(-3.4710148289416,1.30000000000011,3.96945120299074));
#42270=CARTESIAN_POINT('Ctrl Pts',(-3.33101474967611,-1.30000000000612,
3.78965575124489));
#42271=CARTESIAN_POINT('Ctrl Pts',(-3.29858563030453,-1.18514270861593,
3.82621989841157));
#42272=CARTESIAN_POINT('Ctrl Pts',(-3.26933486265743,-1.06847604194723,
3.86176300858679));
#42273=CARTESIAN_POINT('Ctrl Pts',(-3.20910236610783,-0.794772684000861,
3.94151590375758));
#42274=CARTESIAN_POINT('Ctrl Pts',(-3.17470958618622,-0.636309800095198,
3.99291442590289));
#42275=CARTESIAN_POINT('Ctrl Pts',(-3.14021637230009,-0.319434907277157,
4.05932035846933));
#42276=CARTESIAN_POINT('Ctrl Pts',(-3.12848888765305,-0.158333333333333,
4.08838076058789));
#42277=CARTESIAN_POINT('Ctrl Pts',(-3.14639876148324,0.158333333333335,
4.10668526422045));
#42278=CARTESIAN_POINT('Ctrl Pts',(-3.17576205181717,0.31943490727717,4.0956754808042));
#42279=CARTESIAN_POINT('Ctrl Pts',(-3.24729464621603,0.63630980009521,4.06707164949187));
#42280=CARTESIAN_POINT('Ctrl Pts',(-3.30201291805993,0.79477268400084,4.03617403304907));
#42281=CARTESIAN_POINT('Ctrl Pts',(-3.39445885475758,1.06847604194515,3.98957972939292));
#42282=CARTESIAN_POINT('Ctrl Pts',(-3.4371405930767,1.18514270861185,3.96797542650248));
#42283=CARTESIAN_POINT('Ctrl Pts',(-3.48248764917809,1.30000000000012,3.94493576828523));
#42284=CARTESIAN_POINT('Ctrl Pts',(-3.3399062448374,-1.30000000000612,3.75968650438954));
#42285=CARTESIAN_POINT('Ctrl Pts',(-3.30990435433654,-1.18514270861593,
3.79086721926482));
#42286=CARTESIAN_POINT('Ctrl Pts',(-3.28263249593294,-1.06847604194722,
3.82262158044737));
#42287=CARTESIAN_POINT('Ctrl Pts',(-3.22593596759032,-0.794772684000856,
3.89730574494384));
#42288=CARTESIAN_POINT('Ctrl Pts',(-3.19242642144331,-0.6363098000952,3.95066436682348));
#42289=CARTESIAN_POINT('Ctrl Pts',(-3.15954151902818,-0.31943490727716,
4.01805835857427));
#42290=CARTESIAN_POINT('Ctrl Pts',(-3.14791830028498,-0.158333333333333,
4.04962461397864));
#42291=CARTESIAN_POINT('Ctrl Pts',(-3.16645071717067,0.158333333333336,
4.0684300663336));
#42292=CARTESIAN_POINT('Ctrl Pts',(-3.19653610248528,0.319434907277171,
4.05560767286993));
#42293=CARTESIAN_POINT('Ctrl Pts',(-3.26731329855029,0.636309800095212,
4.02664448876788));
#42294=CARTESIAN_POINT('Ctrl Pts',(-3.32125873700668,0.794772684000845,
3.99378941694402));
#42295=CARTESIAN_POINT('Ctrl Pts',(-3.41034596179839,1.06847604194515,3.95229414260646));
#42296=CARTESIAN_POINT('Ctrl Pts',(-3.45105881184621,1.18514270861186,3.93443571615802));
#42297=CARTESIAN_POINT('Ctrl Pts',(-3.49392195333653,1.30000000000012,3.91668062997042));
#42298=CARTESIAN_POINT('Ctrl Pts',(-3.34788849600256,-1.30000000000612,
3.73634894724596));
#42299=CARTESIAN_POINT('Ctrl Pts',(-3.31937411472217,-1.18514270861593,
3.76289356830514));
#42300=CARTESIAN_POINT('Ctrl Pts',(-3.29337082538162,-1.06847604194722,
3.79138747063358));
#42301=CARTESIAN_POINT('Ctrl Pts',(-3.23909914978854,-0.794772684000859,
3.86171731488158));
#42302=CARTESIAN_POINT('Ctrl Pts',(-3.2065171165066,-0.6363098000952,3.91679063131027));
#42303=CARTESIAN_POINT('Ctrl Pts',(-3.17499828999647,-0.319434907277159,
3.98503060092698));
#42304=CARTESIAN_POINT('Ctrl Pts',(-3.16371986733513,-0.158333333333333,
4.01880826653251));
#42305=CARTESIAN_POINT('Ctrl Pts',(-3.18254911001473,0.158333333333336,
4.03785829462972));
#42306=CARTESIAN_POINT('Ctrl Pts',(-3.21244993587892,0.319434907277171,
4.02299152238729));
#42307=CARTESIAN_POINT('Ctrl Pts',(-3.28274389109813,0.636309800095212,
3.99383849579238));
#42308=CARTESIAN_POINT('Ctrl Pts',(-3.33709854669969,0.794772684000844,
3.96021965052572));
#42309=CARTESIAN_POINT('Ctrl Pts',(-3.42376567995241,1.06847604194515,3.92302093447304));
#42310=CARTESIAN_POINT('Ctrl Pts',(-3.4628662367082,1.18514270861185,3.90813573323397));
#42311=CARTESIAN_POINT('Ctrl Pts',(-3.50355235956844,1.30000000000012,3.89446727658678));
#42312=CARTESIAN_POINT('Ctrl Pts',(-3.35676926861817,-1.30000000000612,
3.70282586044512));
#42313=CARTESIAN_POINT('Ctrl Pts',(-3.33044341345346,-1.18514270861593,
3.72314360027605));
#42314=CARTESIAN_POINT('Ctrl Pts',(-3.30627800160764,-1.06847604194723,
3.74724744299701));
#42315=CARTESIAN_POINT('Ctrl Pts',(-3.25544212223206,-0.79477268400086,
3.81167879672225));
#42316=CARTESIAN_POINT('Ctrl Pts',(-3.22403125657669,-0.636309800095206,
3.86898925355682));
#42317=CARTESIAN_POINT('Ctrl Pts',(-3.19432000284549,-0.319434907277165,
3.93827378933774));
#42318=CARTESIAN_POINT('Ctrl Pts',(-3.18317958250032,-0.158333333333334,
3.97475658534395));
#42319=CARTESIAN_POINT('Ctrl Pts',(-3.20290264786813,0.158333333333337,
3.99448700000565));
#42320=CARTESIAN_POINT('Ctrl Pts',(-3.23381791153657,0.319434907277169,
3.97783115213726));
#42321=CARTESIAN_POINT('Ctrl Pts',(-3.30359816134704,0.636309800095214,
3.94853941864496));
#42322=CARTESIAN_POINT('Ctrl Pts',(-3.3571095554096,0.794772684000856,3.91277821411019));
#42323=CARTESIAN_POINT('Ctrl Pts',(-3.44061455907929,1.06847604194516,3.88159668193594));
#42324=CARTESIAN_POINT('Ctrl Pts',(-3.4778644029592,1.18514270861186,3.87107111210848));
#42325=CARTESIAN_POINT('Ctrl Pts',(-3.51621786879574,1.30000000000012,3.86351730234215));
#42326=CARTESIAN_POINT('Ctrl Pts',(-3.36716075715539,-1.30000000000613,
3.66682073682202));
#42327=CARTESIAN_POINT('Ctrl Pts',(-3.34305466705167,-1.18514270861594,
3.68024022105575));
#42328=CARTESIAN_POINT('Ctrl Pts',(-3.3206574889083,-1.06847604194723,3.6993943697633));
#42329=CARTESIAN_POINT('Ctrl Pts',(-3.27286345535249,-0.794772684000868,
3.7568925072017));
#42330=CARTESIAN_POINT('Ctrl Pts',(-3.24167631719755,-0.636309800095208,
3.81587829399618));
#42331=CARTESIAN_POINT('Ctrl Pts',(-3.21373542909072,-0.319434907277165,
3.88613588118528));
#42332=CARTESIAN_POINT('Ctrl Pts',(-3.20374354149421,-0.158333333333335,
3.92626801976877));
#42333=CARTESIAN_POINT('Ctrl Pts',(-3.22437374685318,0.158333333333337,
3.94665109634336));
#42334=CARTESIAN_POINT('Ctrl Pts',(-3.25532686899206,0.319434907277173,
3.92722022169921));
#42335=CARTESIAN_POINT('Ctrl Pts',(-3.32461571737934,0.636309800095218,
3.89783336911054));
#42336=CARTESIAN_POINT('Ctrl Pts',(-3.37849095171978,0.794772684000857,
3.86076254193301));
#42337=CARTESIAN_POINT('Ctrl Pts',(-3.45862581829949,1.06847604194517,3.83618478432541));
#42338=CARTESIAN_POINT('Ctrl Pts',(-3.49365249706183,1.18514270861187,3.8302359484682));
#42339=CARTESIAN_POINT('Ctrl Pts',(-3.5290184401336,1.30000000000013,3.82897707732643));
#42340=CARTESIAN_POINT('Ctrl Pts',(-3.37613355071707,-1.30000000000613,
3.6299006776286));
#42341=CARTESIAN_POINT('Ctrl Pts',(-3.35360976259546,-1.18514270861594,
3.63602839514691));
#42342=CARTESIAN_POINT('Ctrl Pts',(-3.33267522134864,-1.06847604194723,
3.65004964033677));
#42343=CARTESIAN_POINT('Ctrl Pts',(-3.2879837213368,-0.794772684000865,
3.70067714968141));
#42344=CARTESIAN_POINT('Ctrl Pts',(-3.25891404695727,-0.636309800095211,
3.76260732504619));
#42345=CARTESIAN_POINT('Ctrl Pts',(-3.23251598801179,-0.319434907277168,
3.83361198066054));
#42346=CARTESIAN_POINT('Ctrl Pts',(-3.22162837572759,-0.158333333333335,
3.87588330921695));
#42347=CARTESIAN_POINT('Ctrl Pts',(-3.24278997166649,0.158333333333337,
3.89664102996846));
#42348=CARTESIAN_POINT('Ctrl Pts',(-3.27503321896417,0.31943490727717,3.87539089328648));
#42349=CARTESIAN_POINT('Ctrl Pts',(-3.34414068152806,0.636309800095217,
3.8461315485306));
#42350=CARTESIAN_POINT('Ctrl Pts',(-3.39755546629246,0.794772684000862,
3.80710534260456));
#42351=CARTESIAN_POINT('Ctrl Pts',(-3.47488930401332,1.06847604194517,3.78953560103793));
#42352=CARTESIAN_POINT('Ctrl Pts',(-3.5081939264536,1.18514270861187,3.78853090162309));
#42353=CARTESIAN_POINT('Ctrl Pts',(-3.54132821848589,1.30000000000013,3.79412679289453));
#42354=CARTESIAN_POINT('Ctrl Pts',(-3.38313772104073,-1.30000000000614,
3.60245047971202));
#42355=CARTESIAN_POINT('Ctrl Pts',(-3.3620903583262,-1.18514270861595,3.60332356220316));
#42356=CARTESIAN_POINT('Ctrl Pts',(-3.34227587486447,-1.06847604194724,
3.61352266758018));
#42357=CARTESIAN_POINT('Ctrl Pts',(-3.29934865190506,-0.79477268400087,
3.65862961985557));
#42358=CARTESIAN_POINT('Ctrl Pts',(-3.26989719363775,-0.636309800095214,
3.72141918826026));
#42359=CARTESIAN_POINT('Ctrl Pts',(-3.24457504885916,-0.319434907277169,
3.79292662824594));
#42360=CARTESIAN_POINT('Ctrl Pts',(-3.23475116607984,-0.158333333333336,
3.83798840641589));
#42361=CARTESIAN_POINT('Ctrl Pts',(-3.25678466785586,0.158333333333339,
3.85932996227175));
#42362=CARTESIAN_POINT('Ctrl Pts',(-3.28925648289735,0.319434907277174,
3.83617137686758));
#42363=CARTESIAN_POINT('Ctrl Pts',(-3.35820773366914,0.636309800095222,
3.80699113557097));
#42364=CARTESIAN_POINT('Ctrl Pts',(-3.41172663140231,0.794772684000866,
3.76685913072204));
#42365=CARTESIAN_POINT('Ctrl Pts',(-3.48704582484666,1.06847604194518,3.75459317631157));
#42366=CARTESIAN_POINT('Ctrl Pts',(-3.51902987619849,1.18514270861188,3.75725936825981));
#42367=CARTESIAN_POINT('Ctrl Pts',(-3.55039509091127,1.30000000000014,3.76790122932218));
#42368=CARTESIAN_POINT('Ctrl Pts',(-3.38728869726105,-1.30000000000614,
3.58381770307506));
#42369=CARTESIAN_POINT('Ctrl Pts',(-3.36704988134032,-1.18514270861595,
3.58108052935757));
#42370=CARTESIAN_POINT('Ctrl Pts',(-3.34791840522007,-1.06847604194724,
3.58869613419906));
#42371=CARTESIAN_POINT('Ctrl Pts',(-3.30627904460568,-0.794772684000871,
3.63020669441649));
#42372=CARTESIAN_POINT('Ctrl Pts',(-3.27715565086726,-0.636309800095213,
3.69395775582164));
#42373=CARTESIAN_POINT('Ctrl Pts',(-3.25278861508665,-0.319434907277168,
3.76595015077511));
#42374=CARTESIAN_POINT('Ctrl Pts',(-3.24365681828501,-0.158333333333336,
3.81284424669156));
#42375=CARTESIAN_POINT('Ctrl Pts',(-3.26602170365329,0.158333333333338,
3.83439736280539));
#42376=CARTESIAN_POINT('Ctrl Pts',(-3.29827221014194,0.319434907277173,
3.80972345816915));
#42377=CARTESIAN_POINT('Ctrl Pts',(-3.36665942123245,0.636309800095221,
3.78027442478073));
#42378=CARTESIAN_POINT('Ctrl Pts',(-3.41969919892025,0.794772684000864,
3.73900508051313));
#42379=CARTESIAN_POINT('Ctrl Pts',(-3.49390610955008,1.06847604194518,3.73043394287847));
#42380=CARTESIAN_POINT('Ctrl Pts',(-3.52531250203841,1.18514270861188,3.7357606961922));
#42381=CARTESIAN_POINT('Ctrl Pts',(-3.55600386504045,1.30000000000014,3.75012433070975));
#42382=CARTESIAN_POINT('Ctrl Pts',(-3.38926080300867,-1.30000000000614,
3.57444602733469));
#42383=CARTESIAN_POINT('Ctrl Pts',(-3.36929494337846,-1.18514270861595,
3.5698257263846));
#42384=CARTESIAN_POINT('Ctrl Pts',(-3.35043925926547,-1.06847604194724,
3.57611046617764));
#42385=CARTESIAN_POINT('Ctrl Pts',(-3.30944358443281,-0.794772684000869,
3.61582229801963));
#42386=CARTESIAN_POINT('Ctrl Pts',(-3.28084291417713,-0.636309800095212,
3.68027275809969));
#42387=CARTESIAN_POINT('Ctrl Pts',(-3.25691196489572,-0.319434907277168,
3.75247029427834));
#42388=CARTESIAN_POINT('Ctrl Pts',(-3.2476757322749,-0.158333333333336,
3.79997891584379));
#42389=CARTESIAN_POINT('Ctrl Pts',(-3.27028036494494,0.158333333333338,
3.8216909020588));
#42390=CARTESIAN_POINT('Ctrl Pts',(-3.30284156658081,0.319434907277174,
3.79654749839507));
#42391=CARTESIAN_POINT('Ctrl Pts',(-3.37134925175474,0.636309800095222,
3.76724512890989));
#42392=CARTESIAN_POINT('Ctrl Pts',(-3.42455080838407,0.794772684000863,
3.72569454678701));
#42393=CARTESIAN_POINT('Ctrl Pts',(-3.49809669875276,1.06847604194517,3.71889511869807));
#42394=CARTESIAN_POINT('Ctrl Pts',(-3.52902804544423,1.18514270861188,3.72541911643121));
#42395=CARTESIAN_POINT('Ctrl Pts',(-3.55905544803037,1.30000000000014,3.74141033237353));
#42396=CARTESIAN_POINT('Ctrl Pts',(-3.39080022004117,-1.30000000000614,
3.56657258907557));
#42397=CARTESIAN_POINT('Ctrl Pts',(-3.37096541358638,-1.18514270861595,
3.56032254232818));
#42398=CARTESIAN_POINT('Ctrl Pts',(-3.35228764005807,-1.06847604194724,
3.56546600434905));
#42399=CARTESIAN_POINT('Ctrl Pts',(-3.31181122425609,-0.794772684000869,
3.60366971508127));
#42400=CARTESIAN_POINT('Ctrl Pts',(-3.28384244468666,-0.636309800095213,
3.66883132141165));
#42401=CARTESIAN_POINT('Ctrl Pts',(-3.26030123191267,-0.319434907277168,
3.74121307600204));
#42402=CARTESIAN_POINT('Ctrl Pts',(-3.25088044244533,-0.158333333333336,
3.78916350670144));
#42403=CARTESIAN_POINT('Ctrl Pts',(-3.2736344675113,0.158333333333338,3.81097066546428));
#42404=CARTESIAN_POINT('Ctrl Pts',(-3.30643375805074,0.319434907277174,
3.78542225373319));
#42405=CARTESIAN_POINT('Ctrl Pts',(-3.3750512688792,0.636309800095221,3.756248423968));
#42406=CARTESIAN_POINT('Ctrl Pts',(-3.42842023428127,0.794772684000864,
3.71448645638646));
#42407=CARTESIAN_POINT('Ctrl Pts',(-3.50147954230933,1.06847604194518,3.70920741083224));
#42408=CARTESIAN_POINT('Ctrl Pts',(-3.53204973076412,1.18514270861188,3.71675273500996));
#42409=CARTESIAN_POINT('Ctrl Pts',(-3.56156544034252,1.30000000000014,3.73412848657792));
#42410=CARTESIAN_POINT('Ctrl Pts',(-3.39199100145532,-1.30000000000614,
3.56113432904435));
#42411=CARTESIAN_POINT('Ctrl Pts',(-3.37235755683788,-1.18514270861595,
3.55381257366595));
#42412=CARTESIAN_POINT('Ctrl Pts',(-3.35384901121602,-1.06847604194724,
3.55818516674942));
#42413=CARTESIAN_POINT('Ctrl Pts',(-3.31368930992307,-0.794772684000869,
3.59530301589943));
#42414=CARTESIAN_POINT('Ctrl Pts',(-3.28579838077169,-0.636309800095212,
3.66073041711429));
#42415=CARTESIAN_POINT('Ctrl Pts',(-3.26248485028938,-0.319434907277167,
3.73321397902517));
#42416=CARTESIAN_POINT('Ctrl Pts',(-3.25320340928079,-0.158333333333336,
3.78164852128053));
#42417=CARTESIAN_POINT('Ctrl Pts',(-3.27607811504414,0.158333333333338,
3.80353128302652));
#42418=CARTESIAN_POINT('Ctrl Pts',(-3.30889516405502,0.319434907277174,
3.77760062047387));
#42419=CARTESIAN_POINT('Ctrl Pts',(-3.37745661286962,0.636309800095221,
3.74842549607253));
#42420=CARTESIAN_POINT('Ctrl Pts',(-3.43078684621723,0.794772684000862,
3.70640534718603));
#42421=CARTESIAN_POINT('Ctrl Pts',(-3.50356138026373,1.06847604194517,3.70222983579113));
#42422=CARTESIAN_POINT('Ctrl Pts',(-3.53395864103283,1.18514270861188,3.71054615707037));
#42423=CARTESIAN_POINT('Ctrl Pts',(-3.56325176334453,1.30000000000014,3.72898622379376));
#42424=CARTESIAN_POINT('Ctrl Pts',(-3.3925988698541,-1.30000000000614,3.55842326075474));
#42425=CARTESIAN_POINT('Ctrl Pts',(-3.37308151150911,-1.18514270861595,
3.55057546246673));
#42426=CARTESIAN_POINT('Ctrl Pts',(-3.35466355614072,-1.06847604194724,
3.55456645795605));
#42427=CARTESIAN_POINT('Ctrl Pts',(-3.31465423555151,-0.79477268400087,
3.59113643790015));
#42428=CARTESIAN_POINT('Ctrl Pts',(-3.28674928219221,-0.636309800095213,
3.65666323743037));
#42429=CARTESIAN_POINT('Ctrl Pts',(-3.26354044548759,-0.319434907277168,
3.7291920642993));
#42430=CARTESIAN_POINT('Ctrl Pts',(-3.25436486975235,-0.158333333333336,
3.77789205702812));
#42431=CARTESIAN_POINT('Ctrl Pts',(-3.27729915242542,0.158333333333338,
3.79981160017967));
#42432=CARTESIAN_POINT('Ctrl Pts',(-3.31010431598875,0.319434907277174,
3.77367584924757));
#42433=CARTESIAN_POINT('Ctrl Pts',(-3.37861234863815,0.636309800095221,
3.74448234879849));
#42434=CARTESIAN_POINT('Ctrl Pts',(-3.43188705685757,0.794772684000863,
3.70230766822783));
#42435=CARTESIAN_POINT('Ctrl Pts',(-3.50453022588138,1.06847604194517,3.69869139277083));
#42436=CARTESIAN_POINT('Ctrl Pts',(-3.53485775210915,1.18514270861188,3.7074047832426));
#42437=CARTESIAN_POINT('Ctrl Pts',(-3.564068268389,1.30000000000014,3.72639691583526));
#42438=CARTESIAN_POINT('Ctrl Pts',(-3.39294995992423,-1.30000000000614,
3.5568765891777));
#42439=CARTESIAN_POINT('Ctrl Pts',(-3.37350207458928,-1.18514270861595,
3.54873017946487));
#42440=CARTESIAN_POINT('Ctrl Pts',(-3.35513703086187,-1.06847604194724,
3.55250383045926));
#42441=CARTESIAN_POINT('Ctrl Pts',(-3.31521168667268,-0.794772684000869,
3.58875944400585));
#42442=CARTESIAN_POINT('Ctrl Pts',(-3.28728630738722,-0.636309800095212,
3.6543350335598));
#42443=CARTESIAN_POINT('Ctrl Pts',(-3.26413716692034,-0.319434907277167,
3.72688968551762));
#42444=CARTESIAN_POINT('Ctrl Pts',(-3.25503424564992,-0.158333333333336,
3.77574933319419));
#42445=CARTESIAN_POINT('Ctrl Pts',(-3.27800290583528,0.158333333333338,
3.79769006677565));
#42446=CARTESIAN_POINT('Ctrl Pts',(-3.31079220769387,0.319434907277174,
3.77143113154901));
#42447=CARTESIAN_POINT('Ctrl Pts',(-3.37926491037695,0.636309800095221,
3.74222384467635));
#42448=CARTESIAN_POINT('Ctrl Pts',(-3.43250619377278,0.794772684000862,
3.69995947942588));
#42449=CARTESIAN_POINT('Ctrl Pts',(-3.50507659147902,1.06847604194517,3.69666438138917));
#42450=CARTESIAN_POINT('Ctrl Pts',(-3.53536657239264,1.18514270861188,3.70560631562752));
#42451=CARTESIAN_POINT('Ctrl Pts',(-3.56453349805111,1.30000000000014,3.7249165099489));
#42452=CARTESIAN_POINT('Ctrl Pts',(-3.39595090217982,-1.30000000000614,
3.54374063920193));
#42453=CARTESIAN_POINT('Ctrl Pts',(-3.37712431335929,-1.18514270861595,
3.53307659206714));
#42454=CARTESIAN_POINT('Ctrl Pts',(-3.35922077748584,-1.06847604194724,
3.53501108173953));
#42455=CARTESIAN_POINT('Ctrl Pts',(-3.3199924649923,-0.794772684000869,
3.56858528022899));
#42456=CARTESIAN_POINT('Ctrl Pts',(-3.29181540136125,-0.636309800095212,
3.63452697929673));
#42457=CARTESIAN_POINT('Ctrl Pts',(-3.26909728302276,-0.319434907277167,
3.70725154333468));
#42458=CARTESIAN_POINT('Ctrl Pts',(-3.26054283291219,-0.158333333333336,
3.75742121604236));
#42459=CARTESIAN_POINT('Ctrl Pts',(-3.28381007894358,0.158333333333338,
3.77954503560209));
#42460=CARTESIAN_POINT('Ctrl Pts',(-3.31658660801587,0.319434907277172,
3.75231918720872));
#42461=CARTESIAN_POINT('Ctrl Pts',(-3.3847535052942,0.636309800095219,3.72298896000326));
#42462=CARTESIAN_POINT('Ctrl Pts',(-3.43756942643472,0.794772684000863,
3.67986752481284));
#42463=CARTESIAN_POINT('Ctrl Pts',(-3.50951277420466,1.06847604194517,3.67929368192812));
#42464=CARTESIAN_POINT('Ctrl Pts',(-3.53950604440435,1.18514270861188,3.69019148901067));
#42465=CARTESIAN_POINT('Ctrl Pts',(-3.56835097531788,1.30000000000013,3.71223549849759));
#42466=CARTESIAN_POINT('Ctrl Pts',(-3.40091752166454,-1.30000000000612,
3.51817485258119));
#42467=CARTESIAN_POINT('Ctrl Pts',(-3.3825190627201,-1.18514270861593,3.50224067487218));
#42468=CARTESIAN_POINT('Ctrl Pts',(-3.36511610557604,-1.06847604194723,
3.50043212764256));
#42469=CARTESIAN_POINT('Ctrl Pts',(-3.32721160143233,-0.794772684000861,
3.52888705397335));
#42470=CARTESIAN_POINT('Ctrl Pts',(-3.30030872076733,-0.636309800095203,
3.59661809923234));
#42471=CARTESIAN_POINT('Ctrl Pts',(-3.27877017942277,-0.319434907277162,
3.66986977447395));
#42472=CARTESIAN_POINT('Ctrl Pts',(-3.2703562795432,-0.158333333333334,
3.72194050984075));
#42473=CARTESIAN_POINT('Ctrl Pts',(-3.29412609583291,0.158333333333336,
3.74436766369114));
#42474=CARTESIAN_POINT('Ctrl Pts',(-3.32699824865703,0.319434907277173,
3.71537912026337));
#42475=CARTESIAN_POINT('Ctrl Pts',(-3.39555189840338,0.636309800095215,
3.68647567718409));
#42476=CARTESIAN_POINT('Ctrl Pts',(-3.44969761789044,0.794772684000848,
3.64319747826915));
#42477=CARTESIAN_POINT('Ctrl Pts',(-3.52005275577435,1.06847604194516,3.6475149776169));
#42478=CARTESIAN_POINT('Ctrl Pts',(-3.54871229088136,1.18514270861187,3.66159565030966));
#42479=CARTESIAN_POINT('Ctrl Pts',(-3.57557722882024,1.30000000000013,3.68788811020667));
#42480=CARTESIAN_POINT('Ctrl Pts',(-3.405827299293,-1.30000000000611,3.49305769738095));
#42481=CARTESIAN_POINT('Ctrl Pts',(-3.38807550315117,-1.18514270861592,
3.47209928049423));
#42482=CARTESIAN_POINT('Ctrl Pts',(-3.37125653663434,-1.06847604194722,
3.46667872482858));
#42483=CARTESIAN_POINT('Ctrl Pts',(-3.33455638240376,-0.794772684000851,
3.49005172462144));
#42484=CARTESIAN_POINT('Ctrl Pts',(-3.30823759879945,-0.636309800095196,
3.55911508787058));
#42485=CARTESIAN_POINT('Ctrl Pts',(-3.28760112788313,-0.319434907277159,
3.63271287357265));
#42486=CARTESIAN_POINT('Ctrl Pts',(-3.27942269200311,-0.158333333333332,
3.68669773611711));
#42487=CARTESIAN_POINT('Ctrl Pts',(-3.30384439390905,0.158333333333334,
3.70951459063184));
#42488=CARTESIAN_POINT('Ctrl Pts',(-3.3375004211861,0.319434907277167,3.67925227436011));
#42489=CARTESIAN_POINT('Ctrl Pts',(-3.40573136959718,0.636309800095206,
3.65028594953744));
#42490=CARTESIAN_POINT('Ctrl Pts',(-3.4585925712012,0.794772684000842,3.60508175016501));
#42491=CARTESIAN_POINT('Ctrl Pts',(-3.52792852763024,1.06847604194515,3.61461081427897));
#42492=CARTESIAN_POINT('Ctrl Pts',(-3.55620374536085,1.18514270861185,3.63247544804156));
#42493=CARTESIAN_POINT('Ctrl Pts',(-3.58274121443434,1.30000000000011,3.66407993679843));
#42494=CARTESIAN_POINT('Ctrl Pts',(-3.40792382026203,-1.30000000000611,
3.48027749552897));
#42495=CARTESIAN_POINT('Ctrl Pts',(-3.39063227265826,-1.18514270861592,
3.45690107898799));
#42496=CARTESIAN_POINT('Ctrl Pts',(-3.37417219529096,-1.06847604194722,
3.4497223830696));
#42497=CARTESIAN_POINT('Ctrl Pts',(-3.33806698632697,-0.794772684000851,
3.4705581343858));
#42498=CARTESIAN_POINT('Ctrl Pts',(-3.31165271079239,-0.636309800095196,
3.54004392440299));
#42499=CARTESIAN_POINT('Ctrl Pts',(-3.29150406597601,-0.319434907277159,
3.61383388564811));
#42500=CARTESIAN_POINT('Ctrl Pts',(-3.28383918476484,-0.158333333333332,
3.66901547560886));
#42501=CARTESIAN_POINT('Ctrl Pts',(-3.30866559173632,0.158333333333334,
3.69207105417689));
#42502=CARTESIAN_POINT('Ctrl Pts',(-3.34233892867208,0.319434907277167,
3.66093066788631));
#42503=CARTESIAN_POINT('Ctrl Pts',(-3.410649428729,0.636309800095206,3.6320956127618));
#42504=CARTESIAN_POINT('Ctrl Pts',(-3.46380979023612,0.79477268400084,3.58656909938636));
#42505=CARTESIAN_POINT('Ctrl Pts',(-3.5324927010696,1.06847604194515,3.59858491022785));
#42506=CARTESIAN_POINT('Ctrl Pts',(-3.56027544998898,1.18514270861185,3.61812328835454));
#42507=CARTESIAN_POINT('Ctrl Pts',(-3.58611066068062,1.30000000000011,3.65199884532431));
#42508=CARTESIAN_POINT('',(-3.53205673212874,1.2,3.73199261231698));
#42509=CARTESIAN_POINT('Ctrl Pts',(-3.53205673212874,1.2,3.73199261231698));
#42510=CARTESIAN_POINT('Ctrl Pts',(-3.52948084971163,1.21683760541185,3.75340201998427));
#42511=CARTESIAN_POINT('Ctrl Pts',(-3.52780194167531,1.23326792451706,3.77522907381777));
#42512=CARTESIAN_POINT('Ctrl Pts',(-3.52211206890299,1.27112122678138,3.82383590222122));
#42513=CARTESIAN_POINT('Ctrl Pts',(-3.51997651543627,1.28438964967196,3.84082124280845));
#42514=CARTESIAN_POINT('Ctrl Pts',(-3.51715936788841,1.30000000000012,3.86052549330383));
#42515=CARTESIAN_POINT('',(-3.42060206188123,0.653834841369693,3.62201431893726));
#42516=CARTESIAN_POINT('Ctrl Pts',(-3.42060206191022,0.653834841368434,
3.62201431891412));
#42517=CARTESIAN_POINT('Ctrl Pts',(-3.43225912838132,0.717398299039534,
3.63315863003243));
#42518=CARTESIAN_POINT('Ctrl Pts',(-3.44169414240865,0.763866154347927,
3.6422587392106));
#42519=CARTESIAN_POINT('Ctrl Pts',(-3.47884866191347,0.949862607754481,
3.6784459127313));
#42520=CARTESIAN_POINT('Ctrl Pts',(-3.50142427864103,1.05920663100849,3.70079441938718));
#42521=CARTESIAN_POINT('Ctrl Pts',(-3.53205673212874,1.2,3.73199261231697));
#42522=CARTESIAN_POINT('',(-3.3184146483206,-0.653834841531101,3.52704148923361));
#42523=CARTESIAN_POINT('Ctrl Pts',(-3.3184146483206,-0.6538348415311,3.52704148923361));
#42524=CARTESIAN_POINT('Ctrl Pts',(-3.30612811194715,-0.575978670096729,
3.56675882559093));
#42525=CARTESIAN_POINT('Ctrl Pts',(-3.29645819180146,-0.493638820710554,
3.60055778198947));
#42526=CARTESIAN_POINT('Ctrl Pts',(-3.28491094893504,-0.33813590691445,
3.64983331844457));
#42527=CARTESIAN_POINT('Ctrl Pts',(-3.28203919381975,-0.265660385906066,
3.66749140295376));
#42528=CARTESIAN_POINT('Ctrl Pts',(-3.28241544521535,-0.129716867465535,
3.69186530924249));
#42529=CARTESIAN_POINT('Ctrl Pts',(-3.28481094186636,-0.0666253188345313,
3.69978762165696));
#42530=CARTESIAN_POINT('Ctrl Pts',(-3.29431793587721,0.0595444211916306,
3.70913066613523));
#42531=CARTESIAN_POINT('Ctrl Pts',(-3.30148802195868,0.122778732322982,
3.71063286763887));
#42532=CARTESIAN_POINT('Ctrl Pts',(-3.32176075453611,0.260129204703633,
3.706256674953));
#42533=CARTESIAN_POINT('Ctrl Pts',(-3.33571117140391,0.333944924094639,
3.69898184713565));
#42534=CARTESIAN_POINT('Ctrl Pts',(-3.37149269979535,0.491211330758176,
3.67194126002883));
#42535=CARTESIAN_POINT('Ctrl Pts',(-3.39448994830551,0.57435513917775,3.65030538941433));
#42536=CARTESIAN_POINT('Ctrl Pts',(-3.42060206189246,0.653834841386266,
3.6220143189942));
#42537=CARTESIAN_POINT('',(-3.37166915868338,-1.2,3.57586602284307));
#42538=CARTESIAN_POINT('Ctrl Pts',(-3.37166915868338,-1.2,3.57586602284307));
#42539=CARTESIAN_POINT('Ctrl Pts',(-3.36161693023492,-1.12735839874247,
3.56651405383493));
#42540=CARTESIAN_POINT('Ctrl Pts',(-3.3499116696866,-1.03209555687847,3.55570207735526));
#42541=CARTESIAN_POINT('Ctrl Pts',(-3.32722961700632,-0.796656601307582,
3.535001960447));
#42542=CARTESIAN_POINT('Ctrl Pts',(-3.32318655071222,-0.739830804734627,
3.53135276875128));
#42543=CARTESIAN_POINT('Ctrl Pts',(-3.3184146483206,-0.653834841531101,
3.52704148923361));
#42544=CARTESIAN_POINT('Ctrl Pts',(-3.35764585633179,-1.3,3.70018367575412));
#42545=CARTESIAN_POINT('Ctrl Pts',(-3.36040387352645,-1.28300448077975,
3.67927748627612));
#42546=CARTESIAN_POINT('Ctrl Pts',(-3.36304294190339,-1.2660224815296,3.65834194442482));
#42547=CARTESIAN_POINT('Ctrl Pts',(-3.36818942120242,-1.22837741622835,
3.61141873178763));
#42548=CARTESIAN_POINT('Ctrl Pts',(-3.37032016522922,-1.21502229683377,
3.59512911028479));
#42549=CARTESIAN_POINT('Ctrl Pts',(-3.37166915868338,-1.2,3.57586602284307));
#42550=CARTESIAN_POINT('Origin',(0.,1.25,7.2));
#42551=CARTESIAN_POINT('Origin',(0.,1.2,7.2));
#42552=CARTESIAN_POINT('Origin',(0.,0.92691742076555,7.2));
#42553=CARTESIAN_POINT('Origin',(0.,0.653834841531101,7.2));
#42554=CARTESIAN_POINT('Origin',(0.,0.,7.2));
#42555=CARTESIAN_POINT('Origin',(0.,-0.653834841531101,7.2));
#42556=CARTESIAN_POINT('Origin',(0.,-0.926917420765551,7.2));
#42557=CARTESIAN_POINT('Origin',(0.,-1.2,7.2));
#42558=CARTESIAN_POINT('Origin',(0.,-1.25,7.2));
#42559=CARTESIAN_POINT('Ctrl Pts',(-3.15371419665032,-1.30000000000011,
3.26266732036565));
#42560=CARTESIAN_POINT('Ctrl Pts',(-3.19010469464727,-1.18514270861185,
3.28482004315617));
#42561=CARTESIAN_POINT('Ctrl Pts',(-3.21244012754456,-1.06847604194515,
3.31040827862903));
#42562=CARTESIAN_POINT('Ctrl Pts',(-3.231569433639,-0.794772684000851,3.37745894304843));
#42563=CARTESIAN_POINT('Ctrl Pts',(-3.19184909016007,-0.636309800095197,
3.43508690301717));
#42564=CARTESIAN_POINT('Ctrl Pts',(-3.17031238807978,-0.319434907277159,
3.50603727500875));
#42565=CARTESIAN_POINT('Ctrl Pts',(-3.14286241424732,-0.158333333333332,
3.54278120260502));
#42566=CARTESIAN_POINT('Ctrl Pts',(-3.16838675811282,0.158333333333334,
3.56506164372392));
#42567=CARTESIAN_POINT('Ctrl Pts',(-3.22246485929617,0.319434907277167,
3.55167070473433));
#42568=CARTESIAN_POINT('Ctrl Pts',(-3.29374448453208,0.636309800095206,
3.52391928505034));
#42569=CARTESIAN_POINT('Ctrl Pts',(-3.36008858048819,0.79477268400084,3.49038646683519));
#42570=CARTESIAN_POINT('Ctrl Pts',(-3.37703616936998,1.0684760419452,3.45230111691743));
#42571=CARTESIAN_POINT('Ctrl Pts',(-3.36817625250791,1.18514270861195,3.43668158762793));
#42572=CARTESIAN_POINT('Ctrl Pts',(-3.3431204355269,1.30000000000025,3.42192826582706));
#42573=CARTESIAN_POINT('Ctrl Pts',(-3.14205148972774,-1.30000000000011,
3.26728112631937));
#42574=CARTESIAN_POINT('Ctrl Pts',(-3.17625676666542,-1.18514270861185,
3.29036965169776));
#42575=CARTESIAN_POINT('Ctrl Pts',(-3.19697910116141,-1.06847604194515,
3.31662261210206));
#42576=CARTESIAN_POINT('Ctrl Pts',(-3.2137035450423,-0.794772684000851,
3.38458268047563));
#42577=CARTESIAN_POINT('Ctrl Pts',(-3.17427247914414,-0.636309800095197,
3.44187942841939));
#42578=CARTESIAN_POINT('Ctrl Pts',(-3.152596911054,-0.319434907277159,3.51276440598953));
#42579=CARTESIAN_POINT('Ctrl Pts',(-3.12601838773468,-0.158333333333332,
3.54939933543317));
#42580=CARTESIAN_POINT('Ctrl Pts',(-3.1512630121036,0.158333333333334,3.57130224196186));
#42581=CARTESIAN_POINT('Ctrl Pts',(-3.20409726059295,0.319434907277167,
3.55752565368255));
#42582=CARTESIAN_POINT('Ctrl Pts',(-3.27513477131917,0.636309800095206,
3.52930916809052));
#42583=CARTESIAN_POINT('Ctrl Pts',(-3.34106873620035,0.794772684000841,
3.49591547434885));
#42584=CARTESIAN_POINT('Ctrl Pts',(-3.3604774855321,1.06847604194519,3.45697322365221));
#42585=CARTESIAN_POINT('Ctrl Pts',(-3.35332856352237,1.18514270861194,3.44081299553763));
#42586=CARTESIAN_POINT('Ctrl Pts',(-3.33062939108222,1.30000000000025,3.42534919668245));
#42587=CARTESIAN_POINT('Ctrl Pts',(-3.11914435783443,-1.3,3.27690233901048));
#42588=CARTESIAN_POINT('Ctrl Pts',(-3.14787640739775,-1.18514270861176,
3.30061684476125));
#42589=CARTESIAN_POINT('Ctrl Pts',(-3.16474054018966,-1.06847604194507,
3.32749513738329));
#42590=CARTESIAN_POINT('Ctrl Pts',(-3.17628279868663,-0.794772684000792,
3.39689835091026));
#42591=CARTESIAN_POINT('Ctrl Pts',(-3.13918954893612,-0.636309800095149,
3.4556066653861));
#42592=CARTESIAN_POINT('Ctrl Pts',(-3.11771305468591,-0.319434907277135,
3.52692777173361));
#42593=CARTESIAN_POINT('Ctrl Pts',(-3.09226790959551,-0.15833333333332,
3.56258567354113));
#42594=CARTESIAN_POINT('Ctrl Pts',(-3.11713198495812,0.158333333333322,
3.58397698227228));
#42595=CARTESIAN_POINT('Ctrl Pts',(-3.16816605272952,0.319434907277142,
3.57033367148446));
#42596=CARTESIAN_POINT('Ctrl Pts',(-3.23881241642369,0.636309800095157,
3.54131553965297));
#42597=CARTESIAN_POINT('Ctrl Pts',(-3.3032657471794,0.794772684000782,3.50735791283628));
#42598=CARTESIAN_POINT('Ctrl Pts',(-3.32762855144439,1.06847604194511,3.4667109095563));
#42599=CARTESIAN_POINT('Ctrl Pts',(-3.32404137473076,1.18514270861185,3.44962602756524));
#42600=CARTESIAN_POINT('Ctrl Pts',(-3.30632126606804,1.30000000000015,3.43305084518312));
#42601=CARTESIAN_POINT('Ctrl Pts',(-3.09566895515122,-1.29999999999991,
3.28663238688277));
#42602=CARTESIAN_POINT('Ctrl Pts',(-3.12059772278264,-1.18514270861168,
3.31300758471133));
#42603=CARTESIAN_POINT('Ctrl Pts',(-3.13456318990637,-1.06847604194499,
3.34169118337383));
#42604=CARTESIAN_POINT('Ctrl Pts',(-3.14149879537078,-0.794772684000733,
3.41328890213884));
#42605=CARTESIAN_POINT('Ctrl Pts',(-3.10412801503358,-0.6363098000951,3.47031589024842));
#42606=CARTESIAN_POINT('Ctrl Pts',(-3.0820837770709,-0.31943490727711,3.5411760881235));
#42607=CARTESIAN_POINT('Ctrl Pts',(-3.05843946489796,-0.158333333333308,
3.57662503034522));
#42608=CARTESIAN_POINT('Ctrl Pts',(-3.08288767088593,0.15833333333331,3.59746865711391));
#42609=CARTESIAN_POINT('Ctrl Pts',(-3.13190938357248,0.31943490727712,3.58374411199378));
#42610=CARTESIAN_POINT('Ctrl Pts',(-3.20186015445897,0.636309800095111,
3.55354681530502));
#42611=CARTESIAN_POINT('Ctrl Pts',(-3.26445103385548,0.79477268400072,3.51857734110229));
#42612=CARTESIAN_POINT('Ctrl Pts',(-3.29376359632755,1.06847604194503,3.47607578299549));
#42613=CARTESIAN_POINT('Ctrl Pts',(-3.29383959420351,1.18514270861177,3.45809270241767));
#42614=CARTESIAN_POINT('Ctrl Pts',(-3.28130326779873,1.30000000000005,3.44052389092852));
#42615=CARTESIAN_POINT('Ctrl Pts',(-3.08348406279076,-1.29999999999989,
3.29178592705251));
#42616=CARTESIAN_POINT('Ctrl Pts',(-3.10574135532356,-1.18514270861166,
3.31878401257237));
#42617=CARTESIAN_POINT('Ctrl Pts',(-3.1177990022455,-1.06847604194498,3.34797513593898));
#42618=CARTESIAN_POINT('Ctrl Pts',(-3.12209135696599,-0.794772684000721,
3.42047882672178));
#42619=CARTESIAN_POINT('Ctrl Pts',(-3.08557745324672,-0.636309800095091,
3.47779171195928));
#42620=CARTESIAN_POINT('Ctrl Pts',(-3.06368580467661,-0.319434907277105,
3.54894189029846));
#42621=CARTESIAN_POINT('Ctrl Pts',(-3.04103908370401,-0.158333333333306,
3.58434443660176));
#42622=CARTESIAN_POINT('Ctrl Pts',(-3.06527529127201,0.158333333333308,
3.60491194509535));
#42623=CARTESIAN_POINT('Ctrl Pts',(-3.1129143893084,0.319434907277115,3.59075180290206));
#42624=CARTESIAN_POINT('Ctrl Pts',(-3.18263318481277,0.636309800095101,
3.560121444678));
#42625=CARTESIAN_POINT('Ctrl Pts',(-3.24487283518939,0.794772684000708,
3.52542348705439));
#42626=CARTESIAN_POINT('Ctrl Pts',(-3.27677865511172,1.06847604194502,3.48194717796983));
#42627=CARTESIAN_POINT('Ctrl Pts',(-3.2786394826502,1.18514270861175,3.46331755726819));
#42628=CARTESIAN_POINT('Ctrl Pts',(-3.26855029050992,1.30000000000003,3.44487759911162));
#42629=CARTESIAN_POINT('Ctrl Pts',(-3.08205935007171,-1.29999999999989,
3.29240216820087));
#42630=CARTESIAN_POINT('Ctrl Pts',(-3.10400423132416,-1.18514270861166,
3.31947608592427));
#42631=CARTESIAN_POINT('Ctrl Pts',(-3.11583818999718,-1.06847604194498,
3.34872805720068));
#42632=CARTESIAN_POINT('Ctrl Pts',(-3.11981874806555,-0.794772684000722,
3.42133770211157));
#42633=CARTESIAN_POINT('Ctrl Pts',(-3.08339916127519,-0.636309800095091,
3.47867637348839));
#42634=CARTESIAN_POINT('Ctrl Pts',(-3.06152505959721,-0.319434907277105,
3.54986039366487));
#42635=CARTESIAN_POINT('Ctrl Pts',(-3.03900126112515,-0.158333333333306,
3.58526433599475));
#42636=CARTESIAN_POINT('Ctrl Pts',(-3.06321279567437,0.158333333333308,
3.60579986109024));
#42637=CARTESIAN_POINT('Ctrl Pts',(-3.11068637074057,0.319434907277115,
3.5915851808083));
#42638=CARTESIAN_POINT('Ctrl Pts',(-3.18037387911668,0.636309800095102,
3.56089893154296));
#42639=CARTESIAN_POINT('Ctrl Pts',(-3.24256754226884,0.794772684000709,
3.52622689366647));
#42640=CARTESIAN_POINT('Ctrl Pts',(-3.27477723977453,1.06847604194502,3.48263421993515));
#42641=CARTESIAN_POINT('Ctrl Pts',(-3.27684855707369,1.18514270861175,3.46392909138567));
#42642=CARTESIAN_POINT('Ctrl Pts',(-3.26704880710871,1.30000000000003,3.44538848747727));
#42643=CARTESIAN_POINT('Ctrl Pts',(-3.07957071202657,-1.29999999999989,
3.29348617113064));
#42644=CARTESIAN_POINT('Ctrl Pts',(-3.10097599588882,-1.18514270861166,
3.3207009380138));
#42645=CARTESIAN_POINT('Ctrl Pts',(-3.11242278613173,-1.06847604194498,
3.3500643110132));
#42646=CARTESIAN_POINT('Ctrl Pts',(-3.11586104906488,-0.794772684000723,
3.42286328672011));
#42647=CARTESIAN_POINT('Ctrl Pts',(-3.07959939578454,-0.636309800095091,
3.48023920795107));
#42648=CARTESIAN_POINT('Ctrl Pts',(-3.05774875845631,-0.319434907277105,
3.55147401268194));
#42649=CARTESIAN_POINT('Ctrl Pts',(-3.03543093345207,-0.158333333333306,
3.58686927769264));
#42650=CARTESIAN_POINT('Ctrl Pts',(-3.05959934586064,0.158333333333308,
3.60734904397365));
#42651=CARTESIAN_POINT('Ctrl Pts',(-3.10679673806732,0.319434907277115,
3.59305548667019));
#42652=CARTESIAN_POINT('Ctrl Pts',(-3.1764281201781,0.636309800095102,3.56226964135765));
#42653=CARTESIAN_POINT('Ctrl Pts',(-3.23852516459111,0.794772684000709,
3.52762287869824));
#42654=CARTESIAN_POINT('Ctrl Pts',(-3.27126447143197,1.06847604194502,3.48382384133118));
#42655=CARTESIAN_POINT('Ctrl Pts',(-3.27370599441798,1.18514270861175,3.46498887056446));
#42656=CARTESIAN_POINT('Ctrl Pts',(-3.26441740756945,1.30000000000003,3.44627790939293));
#42657=CARTESIAN_POINT('Ctrl Pts',(-3.07462972908329,-1.29999999999989,
3.29569736909264));
#42658=CARTESIAN_POINT('Ctrl Pts',(-3.0949973182512,-1.18514270861166,3.32324213265696));
#42659=CARTESIAN_POINT('Ctrl Pts',(-3.1056939176873,-1.06847604194498,3.35285651108147));
#42660=CARTESIAN_POINT('Ctrl Pts',(-3.1080632812767,-0.794772684000723,
3.42605287393027));
#42661=CARTESIAN_POINT('Ctrl Pts',(-3.07206550985617,-0.636309800095092,
3.48344369259152));
#42662=CARTESIAN_POINT('Ctrl Pts',(-3.05022332264847,-0.319434907277106,
3.55473556987429));
#42663=CARTESIAN_POINT('Ctrl Pts',(-3.02828321681205,-0.158333333333306,
3.59007251318586));
#42664=CARTESIAN_POINT('Ctrl Pts',(-3.05236555158785,0.158333333333308,
3.61044215962353));
#42665=CARTESIAN_POINT('Ctrl Pts',(-3.09907076018363,0.319434907277115,
3.59606523135911));
#42666=CARTESIAN_POINT('Ctrl Pts',(-3.1685761801224,0.636309800095102,3.56506231885714));
#42667=CARTESIAN_POINT('Ctrl Pts',(-3.23039443701896,0.79477268400071,3.53035810324074));
#42668=CARTESIAN_POINT('Ctrl Pts',(-3.26417942019128,1.06847604194502,3.48612906482662));
#42669=CARTESIAN_POINT('Ctrl Pts',(-3.26737047710198,1.18514270861175,3.46704586685332));
#42670=CARTESIAN_POINT('Ctrl Pts',(-3.25912832356508,1.30000000000004,3.44802458278879));
#42671=CARTESIAN_POINT('Ctrl Pts',(-3.0676595775245,-1.2999999999999,3.29896557246829));
#42672=CARTESIAN_POINT('Ctrl Pts',(-3.0867124448927,-1.18514270861167,3.32717423455316));
#42673=CARTESIAN_POINT('Ctrl Pts',(-3.09643635911263,-1.06847604194499,
3.35726087101869));
#42674=CARTESIAN_POINT('Ctrl Pts',(-3.09734879819989,-0.794772684000731,
3.43110551657187));
#42675=CARTESIAN_POINT('Ctrl Pts',(-3.06153419114781,-0.636309800095098,
3.48829716508222));
#42676=CARTESIAN_POINT('Ctrl Pts',(-3.03954610633718,-0.319434907277109,
3.5594860621202));
#42677=CARTESIAN_POINT('Ctrl Pts',(-3.01798147324096,-0.158333333333308,
3.59454111589124));
#42678=CARTESIAN_POINT('Ctrl Pts',(-3.04194629752898,0.15833333333331,3.6147638751156));
#42679=CARTESIAN_POINT('Ctrl Pts',(-3.08821940758376,0.319434907277118,
3.6006024733673));
#42680=CARTESIAN_POINT('Ctrl Pts',(-3.15750734699938,0.636309800095107,
3.56923932045797));
#42681=CARTESIAN_POINT('Ctrl Pts',(-3.2185773149754,0.794772684000717,3.53401193423179));
#42682=CARTESIAN_POINT('Ctrl Pts',(-3.25381704576848,1.06847604194503,3.48911870634936));
#42683=CARTESIAN_POINT('Ctrl Pts',(-3.25812502168796,1.18514270861176,3.46973891452785));
#42684=CARTESIAN_POINT('Ctrl Pts',(-3.25148699982729,1.30000000000005,3.45041194577712));
#42685=CARTESIAN_POINT('Ctrl Pts',(-3.05929002312837,-1.29999999999991,
3.30288696422167));
#42686=CARTESIAN_POINT('Ctrl Pts',(-3.07677393383664,-1.18514270861168,
3.33190463910303));
#42687=CARTESIAN_POINT('Ctrl Pts',(-3.08534480279262,-1.06847604194499,
3.3625757915735));
#42688=CARTESIAN_POINT('Ctrl Pts',(-3.08455431518175,-0.794772684000734,
3.43725215353119));
#42689=CARTESIAN_POINT('Ctrl Pts',(-3.04902433433522,-0.636309800095101,
3.49427720425505));
#42690=CARTESIAN_POINT('Ctrl Pts',(-3.02689025391295,-0.31943490727711,
3.56537546901684));
#42691=CARTESIAN_POINT('Ctrl Pts',(-3.00576181446938,-0.158333333333308,
3.60007454025842));
#42692=CARTESIAN_POINT('Ctrl Pts',(-3.02955809413638,0.15833333333331,3.62009213531368));
#42693=CARTESIAN_POINT('Ctrl Pts',(-3.0752577679684,0.319434907277119,3.6061306943942));
#42694=CARTESIAN_POINT('Ctrl Pts',(-3.14428462971439,0.63630980009511,3.57434016945101));
#42695=CARTESIAN_POINT('Ctrl Pts',(-3.20455259630907,0.794772684000721,
3.53860178011621));
#42696=CARTESIAN_POINT('Ctrl Pts',(-3.2414986960271,1.06847604194503,3.49286218100061));
#42697=CARTESIAN_POINT('Ctrl Pts',(-3.24710266824222,1.18514270861176,3.47307108281982));
#42698=CARTESIAN_POINT('Ctrl Pts',(-3.24231801509243,1.30000000000005,3.45328786409621));
#42699=CARTESIAN_POINT('Ctrl Pts',(-3.04795105160112,-1.29999999999992,
3.30790732462681));
#42700=CARTESIAN_POINT('Ctrl Pts',(-3.06306779676184,-1.18514270861169,
3.3376911266136));
#42701=CARTESIAN_POINT('Ctrl Pts',(-3.06994766037203,-1.068476041945,3.3689676250005));
#42702=CARTESIAN_POINT('Ctrl Pts',(-3.06681267745931,-0.794772684000742,
3.44467102041343));
#42703=CARTESIAN_POINT('Ctrl Pts',(-3.03201375931715,-0.636309800095107,
3.5018731381446));
#42704=CARTESIAN_POINT('Ctrl Pts',(-3.01005996212089,-0.319434907277114,
3.5732854451987));
#42705=CARTESIAN_POINT('Ctrl Pts',(-2.98993876061887,-0.15833333333331,
3.60801054982657));
#42706=CARTESIAN_POINT('Ctrl Pts',(-3.01352943923577,0.158333333333312,
3.62777471043105));
#42707=CARTESIAN_POINT('Ctrl Pts',(-3.05789486132607,0.319434907277123,
3.61339757444287));
#42708=CARTESIAN_POINT('Ctrl Pts',(-3.12656995434065,0.636309800095117,
3.58105426454118));
#42709=CARTESIAN_POINT('Ctrl Pts',(-3.18632522509441,0.79477268400073,3.54534842162168));
#42710=CARTESIAN_POINT('Ctrl Pts',(-3.22561348356767,1.06847604194504,3.4985584054285));
#42711=CARTESIAN_POINT('Ctrl Pts',(-3.23288148404397,1.18514270861178,3.4781295861752));
#42712=CARTESIAN_POINT('Ctrl Pts',(-3.23041105367694,1.30000000000006,3.45752561193765));
#42713=CARTESIAN_POINT('Ctrl Pts',(-3.03373374036243,-1.29999999999993,
3.31415100966446));
#42714=CARTESIAN_POINT('Ctrl Pts',(-3.04590402957723,-1.1851427086117,3.34491311200048));
#42715=CARTESIAN_POINT('Ctrl Pts',(-3.05066932831086,-1.06847604194501,
3.37694967666605));
#42716=CARTESIAN_POINT('Ctrl Pts',(-3.04457111230556,-0.79477268400075,
3.45390481287289));
#42717=CARTESIAN_POINT('Ctrl Pts',(-3.01060375645462,-0.636309800095113,
3.51123269374844));
#42718=CARTESIAN_POINT('Ctrl Pts',(-2.98882960655681,-0.319434907277116,
3.58297929310441));
#42719=CARTESIAN_POINT('Ctrl Pts',(-2.96993063132861,-0.158333333333311,
3.61768107744254));
#42720=CARTESIAN_POINT('Ctrl Pts',(-2.99334906214383,0.158333333333313,
3.63722700691804));
#42721=CARTESIAN_POINT('Ctrl Pts',(-3.03630252279416,0.319434907277125,
3.62264763423389));
#42722=CARTESIAN_POINT('Ctrl Pts',(-3.10448273264278,0.636309800095122,
3.58954043317641));
#42723=CARTESIAN_POINT('Ctrl Pts',(-3.16322206646095,0.794772684000737,
3.55340286023055));
#42724=CARTESIAN_POINT('Ctrl Pts',(-3.2053322025275,1.06847604194505,3.50517104413015));
#42725=CARTESIAN_POINT('Ctrl Pts',(-3.21468940920784,1.18514270861179,3.48395990632891));
#42726=CARTESIAN_POINT('Ctrl Pts',(-3.21517590499961,1.30000000000008,3.46241539675136));
#42727=CARTESIAN_POINT('Ctrl Pts',(-3.01156878373355,-1.29999999999995,
3.32480522646398));
#42728=CARTESIAN_POINT('Ctrl Pts',(-3.01948628977715,-1.18514270861172,
3.35766374866596));
#42729=CARTESIAN_POINT('Ctrl Pts',(-3.02118250681312,-1.06847604194503,
3.39127799568841));
#42730=CARTESIAN_POINT('Ctrl Pts',(-3.01072868532105,-0.79477268400076,
3.47067950633485));
#42731=CARTESIAN_POINT('Ctrl Pts',(-2.97799510066786,-0.636309800095124,
3.52809178122447));
#42732=CARTESIAN_POINT('Ctrl Pts',(-2.95606711952232,-0.319434907277123,
3.59987576902135));
#42733=CARTESIAN_POINT('Ctrl Pts',(-2.93838859947651,-0.158333333333314,
3.63371139851771));
#42734=CARTESIAN_POINT('Ctrl Pts',(-2.96107261811187,0.158333333333316,
3.65239614836563));
#42735=CARTESIAN_POINT('Ctrl Pts',(-3.00164930281178,0.319434907277132,
3.63734668426724));
#42736=CARTESIAN_POINT('Ctrl Pts',(-3.06934679659287,0.636309800095134,
3.6034156103906));
#42737=CARTESIAN_POINT('Ctrl Pts',(-3.12735313425804,0.794772684000753,
3.56771055434906));
#42738=CARTESIAN_POINT('Ctrl Pts',(-3.17419280791191,1.06847604194507,3.51741101880181));
#42739=CARTESIAN_POINT('Ctrl Pts',(-3.18682899964134,1.18514270861181,3.49484687460461));
#42740=CARTESIAN_POINT('Ctrl Pts',(-3.19182622395639,1.3000000000001,3.47149139136714));
#42741=CARTESIAN_POINT('Ctrl Pts',(-2.98920415737631,-1.29999999999999,
3.33528254069167));
#42742=CARTESIAN_POINT('Ctrl Pts',(-2.99287348828336,-1.18514270861175,
3.37024236873661));
#42743=CARTESIAN_POINT('Ctrl Pts',(-2.99145726917786,-1.06847604194506,
3.40538690733707));
#42744=CARTESIAN_POINT('Ctrl Pts',(-2.97643688184066,-0.794772684000781,
3.48700454047947));
#42745=CARTESIAN_POINT('Ctrl Pts',(-2.94442040650366,-0.636309800095141,
3.54393732114147));
#42746=CARTESIAN_POINT('Ctrl Pts',(-2.92239826111222,-0.319434907277131,
3.61582450591124));
#42747=CARTESIAN_POINT('Ctrl Pts',(-2.90632539982685,-0.158333333333318,
3.6491943202188));
#42748=CARTESIAN_POINT('Ctrl Pts',(-2.92891834946343,0.15833333333332,3.66776284890486));
#42749=CARTESIAN_POINT('Ctrl Pts',(-2.96796626022347,0.31943490727714,3.65327266521064));
#42750=CARTESIAN_POINT('Ctrl Pts',(-3.03523030742018,0.636309800095151,
3.61857454417012));
#42751=CARTESIAN_POINT('Ctrl Pts',(-3.09163350657476,0.794772684000771,
3.58225353266621));
#42752=CARTESIAN_POINT('Ctrl Pts',(-3.14269960151707,1.0684760419451,3.52928505221333));
#42753=CARTESIAN_POINT('Ctrl Pts',(-3.15845027867044,1.18514270861184,3.505173206469));
#42754=CARTESIAN_POINT('Ctrl Pts',(-3.16784701266196,1.30000000000014,3.47987760749274));
#42755=CARTESIAN_POINT('Ctrl Pts',(-2.96717582248572,-1.3,3.34612443025397));
#42756=CARTESIAN_POINT('Ctrl Pts',(-2.96644096907686,-1.18514270861176,
3.38304333254976));
#42757=CARTESIAN_POINT('Ctrl Pts',(-2.96194864866568,-1.06847604194507,
3.41977717338575));
#42758=CARTESIAN_POINT('Ctrl Pts',(-2.94288998937622,-0.79477268400079,
3.50421216530303));
#42759=CARTESIAN_POINT('Ctrl Pts',(-2.91305103557942,-0.636309800095149,
3.56223763206484));
#42760=CARTESIAN_POINT('Ctrl Pts',(-2.89118884891162,-0.319434907277136,
3.63451512537704));
#42761=CARTESIAN_POINT('Ctrl Pts',(-2.87592686550002,-0.15833333333332,
3.66657569218735));
#42762=CARTESIAN_POINT('Ctrl Pts',(-2.89772479923798,0.158333333333322,
3.68426376399353));
#42763=CARTESIAN_POINT('Ctrl Pts',(-2.93478382345054,0.319434907277142,
3.66981881317108));
#42764=CARTESIAN_POINT('Ctrl Pts',(-3.00104865048769,0.636309800095157,
3.6337182358295));
#42765=CARTESIAN_POINT('Ctrl Pts',(-3.05541968820448,0.794772684000783,
3.59628564676238));
#42766=CARTESIAN_POINT('Ctrl Pts',(-3.11093941743452,1.06847604194512,3.54089763150643));
#42767=CARTESIAN_POINT('Ctrl Pts',(-3.13009221058491,1.18514270861186,3.51556002773706));
#42768=CARTESIAN_POINT('Ctrl Pts',(-3.14436536331071,1.30000000000015,3.48886023967439));
#42769=CARTESIAN_POINT('Ctrl Pts',(-2.95059618965475,-1.30000000000001,
3.35424938277405));
#42770=CARTESIAN_POINT('Ctrl Pts',(-2.94719414326373,-1.18514270861177,
3.39331003261898));
#42771=CARTESIAN_POINT('Ctrl Pts',(-2.94065773409478,-1.06847604194508,
3.43150988911155));
#42772=CARTESIAN_POINT('Ctrl Pts',(-2.9183163162662,-0.794772684000798,
3.5177705946194));
#42773=CARTESIAN_POINT('Ctrl Pts',(-2.8879929083895,-0.636309800095153,
3.57433989673292));
#42774=CARTESIAN_POINT('Ctrl Pts',(-2.86607142352026,-0.319434907277137,
3.64670989540203));
#42775=CARTESIAN_POINT('Ctrl Pts',(-2.85281501287045,-0.158333333333321,
3.67927548148163));
#42776=CARTESIAN_POINT('Ctrl Pts',(-2.87473723910272,0.158333333333323,
3.69709296118341));
#42777=CARTESIAN_POINT('Ctrl Pts',(-2.91016801870854,0.319434907277144,
3.682547053866));
#42778=CARTESIAN_POINT('Ctrl Pts',(-2.97622990338684,0.636309800095162,
3.64605811352108));
#42779=CARTESIAN_POINT('Ctrl Pts',(-3.03014457191045,0.794772684000788,
3.60909008270178));
#42780=CARTESIAN_POINT('Ctrl Pts',(-3.08869601229283,1.06847604194512,3.55153153788718));
#42781=CARTESIAN_POINT('Ctrl Pts',(-3.10993754230562,1.18514270861186,3.5247245089168));
#42782=CARTESIAN_POINT('Ctrl Pts',(-3.12707585333436,1.30000000000016,3.496025412272));
#42783=CARTESIAN_POINT('Ctrl Pts',(-2.93496317665334,-1.30000000000002,
3.3633063159341));
#42784=CARTESIAN_POINT('Ctrl Pts',(-2.92816594708533,-1.18514270861178,
3.40376717196528));
#42785=CARTESIAN_POINT('Ctrl Pts',(-2.91928145969323,-1.06847604194509,
3.44313428112175));
#42786=CARTESIAN_POINT('Ctrl Pts',(-2.89393453335372,-0.794772684000804,
3.5315534045525));
#42787=CARTESIAN_POINT('Ctrl Pts',(-2.86549588577109,-0.636309800095158,
3.5891825598255));
#42788=CARTESIAN_POINT('Ctrl Pts',(-2.84376814101127,-0.31943490727714,
3.66192324514565));
#42789=CARTESIAN_POINT('Ctrl Pts',(-2.83123177913598,-0.158333333333322,
3.69363560007842));
#42790=CARTESIAN_POINT('Ctrl Pts',(-2.85212603576051,0.158333333333324,
3.7103411018121));
#42791=CARTESIAN_POINT('Ctrl Pts',(-2.88524411637506,0.319434907277146,
3.69495745864312));
#42792=CARTESIAN_POINT('Ctrl Pts',(-2.95016857461147,0.636309800095166,
3.65701217155733));
#42793=CARTESIAN_POINT('Ctrl Pts',(-3.00278299985719,0.794772684000794,
3.6194600238106));
#42794=CARTESIAN_POINT('Ctrl Pts',(-3.06482687763757,1.06847604194513,3.56024830517271));
#42795=CARTESIAN_POINT('Ctrl Pts',(-3.08871428890777,1.18514270861187,3.53261894563116));
#42796=CARTESIAN_POINT('Ctrl Pts',(-3.10963261570928,1.30000000000017,3.50299078553598));
#42797=CARTESIAN_POINT('Ctrl Pts',(-2.91812360584106,-1.30000000000003,
3.37118251970176));
#42798=CARTESIAN_POINT('Ctrl Pts',(-2.90835133164569,-1.18514270861179,
3.41346968432624));
#42799=CARTESIAN_POINT('Ctrl Pts',(-2.89732666173695,-1.06847604194509,
3.45420874668576));
#42800=CARTESIAN_POINT('Ctrl Pts',(-2.86896418413129,-0.79477268400081,
3.54474770462891));
#42801=CARTESIAN_POINT('Ctrl Pts',(-2.84132230949808,-0.636309800095161,
3.60227634535726));
#42802=CARTESIAN_POINT('Ctrl Pts',(-2.81975603492678,-0.31943490727714,
3.67534138165594));
#42803=CARTESIAN_POINT('Ctrl Pts',(-2.80832531294812,-0.158333333333323,
3.70658812804784));
#42804=CARTESIAN_POINT('Ctrl Pts',(-2.82933027822802,0.158333333333325,
3.72342674960999));
#42805=CARTESIAN_POINT('Ctrl Pts',(-2.86165499703511,0.31943490727715,3.70888506187108));
#42806=CARTESIAN_POINT('Ctrl Pts',(-2.92623290821954,0.636309800095171,
3.6703911433026));
#42807=CARTESIAN_POINT('Ctrl Pts',(-2.97738454099281,0.794772684000797,
3.63216348213907));
#42808=CARTESIAN_POINT('Ctrl Pts',(-3.04213962224978,1.06847604194513,3.57041424133755));
#42809=CARTESIAN_POINT('Ctrl Pts',(-3.06811606390625,1.18514270861188,3.5413129890768));
#42810=CARTESIAN_POINT('Ctrl Pts',(-3.09203887195526,1.30000000000018,3.50983944286344));
#42811=CARTESIAN_POINT('Ctrl Pts',(-2.90564932299591,-1.30000000000003,
3.37931771926188));
#42812=CARTESIAN_POINT('Ctrl Pts',(-2.89344317979173,-1.18514270861179,
3.42319211348459));
#42813=CARTESIAN_POINT('Ctrl Pts',(-2.88063148381286,-1.06847604194509,
3.46508542032316));
#42814=CARTESIAN_POINT('Ctrl Pts',(-2.84963495508069,-0.79477268400081,
3.55729063167506));
#42815=CARTESIAN_POINT('Ctrl Pts',(-2.82234920049889,-0.636309800095163,
3.61442241467706));
#42816=CARTESIAN_POINT('Ctrl Pts',(-2.80075798336809,-0.319434907277142,
3.68759947538144));
#42817=CARTESIAN_POINT('Ctrl Pts',(-2.79049462724478,-0.158333333333324,
3.71871421775334));
#42818=CARTESIAN_POINT('Ctrl Pts',(-2.81118495158267,0.158333333333326,
3.73522940676952));
#42819=CARTESIAN_POINT('Ctrl Pts',(-2.84203410447534,0.319434907277151,
3.72051732347584));
#42820=CARTESIAN_POINT('Ctrl Pts',(-2.90598293766052,0.636309800095173,
3.68120972904556));
#42821=CARTESIAN_POINT('Ctrl Pts',(-2.95615812849188,0.794772684000799,
3.64268392562299));
#42822=CARTESIAN_POINT('Ctrl Pts',(-3.02343030207539,1.06847604194514,3.57911464656462));
#42823=CARTESIAN_POINT('Ctrl Pts',(-3.05130248589471,1.18514270861188,3.5489630235154));
#42824=CARTESIAN_POINT('Ctrl Pts',(-3.07792722226875,1.30000000000018,3.51617656284739));
#42825=CARTESIAN_POINT('Ctrl Pts',(-2.89444547446341,-1.30000000000004,
3.38460967377958));
#42826=CARTESIAN_POINT('Ctrl Pts',(-2.88025475037004,-1.18514270861179,
3.42970791994923));
#42827=CARTESIAN_POINT('Ctrl Pts',(-2.86605623064443,-1.0684760419451,3.47256285200525));
#42828=CARTESIAN_POINT('Ctrl Pts',(-2.83323680020414,-0.794772684000812,
3.56638381377852));
#42829=CARTESIAN_POINT('Ctrl Pts',(-2.806797447228,-0.636309800095164,3.623775853036));
#42830=CARTESIAN_POINT('Ctrl Pts',(-2.785528981377,-0.319434907277142,3.69738903397588));
#42831=CARTESIAN_POINT('Ctrl Pts',(-2.77617802870274,-0.158333333333324,
3.72836872085716));
#42832=CARTESIAN_POINT('Ctrl Pts',(-2.79663721708606,0.158333333333326,
3.74464778453676));
#42833=CARTESIAN_POINT('Ctrl Pts',(-2.82624199019963,0.319434907277151,
3.72974883334975));
#42834=CARTESIAN_POINT('Ctrl Pts',(-2.88960266939197,0.636309800095174,
3.68969891281971));
#42835=CARTESIAN_POINT('Ctrl Pts',(-2.93881369270205,0.7947726840008,3.65072013162558));
#42836=CARTESIAN_POINT('Ctrl Pts',(-3.00821350617473,1.06847604194514,3.58581320002371));
#42837=CARTESIAN_POINT('Ctrl Pts',(-3.03772064583979,1.18514270861188,3.55494927288839));
#42838=CARTESIAN_POINT('Ctrl Pts',(-3.06669431743411,1.30000000000018,3.52131722426934));
#42839=CARTESIAN_POINT('Ctrl Pts',(-2.87330971922871,-1.30000000000004,
3.39645550931658));
#42840=CARTESIAN_POINT('Ctrl Pts',(-2.8551151553052,-1.1851427086118,3.44396806456762));
#42841=CARTESIAN_POINT('Ctrl Pts',(-2.83807033144944,-1.0684760419451,3.48867366979621));
#42842=CARTESIAN_POINT('Ctrl Pts',(-2.80134950809849,-0.794772684000815,
3.58546794511965));
#42843=CARTESIAN_POINT('Ctrl Pts',(-2.77633178278127,-0.636309800095167,
3.64310304084678));
#42844=CARTESIAN_POINT('Ctrl Pts',(-2.75528781624004,-0.319434907277144,
3.71716182931582));
#42845=CARTESIAN_POINT('Ctrl Pts',(-2.74728825573495,-0.158333333333325,
3.74738689262068));
#42846=CARTESIAN_POINT('Ctrl Pts',(-2.76738199808109,0.158333333333327,
3.76330543314258));
#42847=CARTESIAN_POINT('Ctrl Pts',(-2.79518745255115,0.319434907277151,
3.74874413442973));
#42848=CARTESIAN_POINT('Ctrl Pts',(-2.85774725188071,0.636309800095175,
3.70762922705557));
#42849=CARTESIAN_POINT('Ctrl Pts',(-2.90540089433975,0.794772684000803,
3.66821008494076));
#42850=CARTESIAN_POINT('Ctrl Pts',(-2.97837586044864,1.06847604194514,3.59988687467182));
#42851=CARTESIAN_POINT('Ctrl Pts',(-3.01059956725001,1.18514270861189,3.56698250495343));
#42852=CARTESIAN_POINT('Ctrl Pts',(-3.04345882201318,1.30000000000019,3.53074835161764));
#42853=CARTESIAN_POINT('Ctrl Pts',(-2.84986342692003,-1.30000000000005,
3.41016373782283));
#42854=CARTESIAN_POINT('Ctrl Pts',(-2.8278002227937,-1.18514270861181,3.46104959590005));
#42855=CARTESIAN_POINT('Ctrl Pts',(-2.80797992245507,-1.06847604194511,
3.50827599494446));
#42856=CARTESIAN_POINT('Ctrl Pts',(-2.76737262007632,-0.794772684000818,
3.60892434190774));
#42857=CARTESIAN_POINT('Ctrl Pts',(-2.74358827141872,-0.63630980009517,
3.66642463388269));
#42858=CARTESIAN_POINT('Ctrl Pts',(-2.7225206234019,-0.319434907277146,
3.74071141836457));
#42859=CARTESIAN_POINT('Ctrl Pts',(-2.71569615971129,-0.158333333333326,
3.76977449773877));
#42860=CARTESIAN_POINT('Ctrl Pts',(-2.73515410718614,0.158333333333328,
3.78508150889321));
#42861=CARTESIAN_POINT('Ctrl Pts',(-2.76108477126121,0.319434907277156,
3.77105713136288));
#42862=CARTESIAN_POINT('Ctrl Pts',(-2.82250334076209,0.636309800095182,
3.7284961532079));
#42863=CARTESIAN_POINT('Ctrl Pts',(-2.86770375781189,0.794772684000808,
3.68782644460456));
#42864=CARTESIAN_POINT('Ctrl Pts',(-2.9449882645546,1.06847604194515,3.61598218052369));
#42865=CARTESIAN_POINT('Ctrl Pts',(-2.98061577717813,1.1851427086119,3.58116393341142));
#42866=CARTESIAN_POINT('Ctrl Pts',(-3.01841720312947,1.3000000000002,3.54262615901515));
#42867=CARTESIAN_POINT('Ctrl Pts',(-2.81674957134945,-1.30000000000007,
3.43070471365389));
#42868=CARTESIAN_POINT('Ctrl Pts',(-2.78856312709208,-1.18514270861182,
3.48590126687021));
#42869=CARTESIAN_POINT('Ctrl Pts',(-2.76447074598642,-1.06847604194512,
3.5364820539981));
#42870=CARTESIAN_POINT('Ctrl Pts',(-2.71827063086294,-0.794772684000828,
3.64267044787023));
#42871=CARTESIAN_POINT('Ctrl Pts',(-2.69707890134858,-0.636309800095181,
3.7007813262518));
#42872=CARTESIAN_POINT('Ctrl Pts',(-2.67718366416938,-0.319434907277152,
3.77653842687141));
#42873=CARTESIAN_POINT('Ctrl Pts',(-2.67360251051884,-0.158333333333328,
3.80535560502423));
#42874=CARTESIAN_POINT('Ctrl Pts',(-2.69217396507023,0.15833333333333,3.81984616809613));
#42875=CARTESIAN_POINT('Ctrl Pts',(-2.71361121935058,0.319434907277159,
3.80495169052859));
#42876=CARTESIAN_POINT('Ctrl Pts',(-2.77279229669294,0.63630980009519,3.75986751852911));
#42877=CARTESIAN_POINT('Ctrl Pts',(-2.81558792137091,0.794772684000822,
3.71868470650039));
#42878=CARTESIAN_POINT('Ctrl Pts',(-2.89829007054551,1.06847604194517,3.64094211848186));
#42879=CARTESIAN_POINT('Ctrl Pts',(-2.93814406855001,1.18514270861192,3.60262063460224));
#42880=CARTESIAN_POINT('Ctrl Pts',(-2.98205336859798,1.30000000000022,3.55962955254944));
#42881=CARTESIAN_POINT('Ctrl Pts',(-2.79130385555554,-1.30000000000009,
3.44659963092747));
#42882=CARTESIAN_POINT('Ctrl Pts',(-2.75880839581699,-1.18514270861184,
3.50557743686655));
#42883=CARTESIAN_POINT('Ctrl Pts',(-2.73177596756767,-1.06847604194514,
3.55912180261392));
#42884=CARTESIAN_POINT('Ctrl Pts',(-2.68194634610882,-0.794772684000846,
3.6702676652052));
#42885=CARTESIAN_POINT('Ctrl Pts',(-2.66344640491833,-0.63630980009519,
3.72941821861195));
#42886=CARTESIAN_POINT('Ctrl Pts',(-2.64402530993783,-0.319434907277155,
3.80590712414196));
#42887=CARTESIAN_POINT('Ctrl Pts',(-2.6411804093813,-0.158333333333331,
3.83290762524055));
#42888=CARTESIAN_POINT('Ctrl Pts',(-2.65893027932983,0.158333333333333,
3.8466908829489));
#42889=CARTESIAN_POINT('Ctrl Pts',(-2.67853367145776,0.319434907277164,
3.83273256017458));
#42890=CARTESIAN_POINT('Ctrl Pts',(-2.73612933986299,0.6363098000952,3.78582868351487));
#42891=CARTESIAN_POINT('Ctrl Pts',(-2.77568686749433,0.794772684000833,
3.74284458125839));
#42892=CARTESIAN_POINT('Ctrl Pts',(-2.86255676382707,1.06847604194518,3.66051962129997));
#42893=CARTESIAN_POINT('Ctrl Pts',(-2.90591827320911,1.18514270861193,3.61973496937537));
#42894=CARTESIAN_POINT('Ctrl Pts',(-2.95503853269762,1.30000000000023,3.57380109025177));
#42895=CARTESIAN_POINT('Ctrl Pts',(-2.76631964265226,-1.3000000000001,3.46290077644001));
#42896=CARTESIAN_POINT('Ctrl Pts',(-2.72970063932157,-1.18514270861185,
3.52572570840152));
#42897=CARTESIAN_POINT('Ctrl Pts',(-2.6998918952725,-1.06847604194514,3.58230084560764));
#42898=CARTESIAN_POINT('Ctrl Pts',(-2.64676079462857,-0.794772684000846,
3.69856245421907));
#42899=CARTESIAN_POINT('Ctrl Pts',(-2.63084342365516,-0.636309800095192,
3.75862307933041));
#42900=CARTESIAN_POINT('Ctrl Pts',(-2.61262197752267,-0.319434907277157,
3.83646439589201));
#42901=CARTESIAN_POINT('Ctrl Pts',(-2.61177277019272,-0.158333333333331,
3.8628068404394));
#42902=CARTESIAN_POINT('Ctrl Pts',(-2.62883796386496,0.158333333333333,
3.87603367277299));
#42903=CARTESIAN_POINT('Ctrl Pts',(-2.64544299217718,0.319434907277164,
3.86194356483978));
#42904=CARTESIAN_POINT('Ctrl Pts',(-2.7010921069768,0.636309800095201,3.81302933099263));
#42905=CARTESIAN_POINT('Ctrl Pts',(-2.73826067334614,0.794772684000835,
3.76925102704878));
#42906=CARTESIAN_POINT('Ctrl Pts',(-2.82855844984348,1.06847604194519,3.68175244662319));
#42907=CARTESIAN_POINT('Ctrl Pts',(-2.87481506609588,1.18514270861194,3.63794176287807));
#42908=CARTESIAN_POINT('Ctrl Pts',(-2.92824173701734,1.30000000000024,3.58819528871212));
#42909=CARTESIAN_POINT('Ctrl Pts',(-2.74946991434193,-1.3000000000001,3.4750205202169));
#42910=CARTESIAN_POINT('Ctrl Pts',(-2.70989262720101,-1.18514270861185,
3.54066783837951));
#42911=CARTESIAN_POINT('Ctrl Pts',(-2.67815184852736,-1.06847604194515,
3.59951550166289));
#42912=CARTESIAN_POINT('Ctrl Pts',(-2.62292820231771,-0.79477268400085,
3.71975681324494));
#42913=CARTESIAN_POINT('Ctrl Pts',(-2.61001698334349,-0.636309800095195,
3.78147580120014));
#42914=CARTESIAN_POINT('Ctrl Pts',(-2.59160966732343,-0.319434907277159,
3.85936426630499));
#42915=CARTESIAN_POINT('Ctrl Pts',(-2.58917887281194,-0.158333333333332,
3.88254430379007));
#42916=CARTESIAN_POINT('Ctrl Pts',(-2.60530601519066,0.158333333333334,
3.89499485143002));
#42917=CARTESIAN_POINT('Ctrl Pts',(-2.62206510686829,0.319434907277166,
3.88292248440957));
#42918=CARTESIAN_POINT('Ctrl Pts',(-2.67698636889789,0.636309800095204,
3.83313023249387));
#42919=CARTESIAN_POINT('Ctrl Pts',(-2.7116317122864,0.79477268400084,3.78796944947533));
#42920=CARTESIAN_POINT('Ctrl Pts',(-2.80431412364808,1.06847604194519,3.69660834519858));
#42921=CARTESIAN_POINT('Ctrl Pts',(-2.85269008915142,1.18514270861194,3.65063022732966));
#42922=CARTESIAN_POINT('Ctrl Pts',(-2.9093232385014,1.30000000000025,3.59822082837069));
#42923=CARTESIAN_POINT('Ctrl Pts',(-2.73730164354872,-1.3000000000001,3.48341371040716));
#42924=CARTESIAN_POINT('Ctrl Pts',(-2.69639517330247,-1.18514270861185,
3.55150847404721));
#42925=CARTESIAN_POINT('Ctrl Pts',(-2.66354727608036,-1.06847604194515,
3.61201581798988));
#42926=CARTESIAN_POINT('Ctrl Pts',(-2.60627897809573,-0.794772684000851,
3.73427142959104));
#42927=CARTESIAN_POINT('Ctrl Pts',(-2.59253840770018,-0.636309800095194,
3.79450670463528));
#42928=CARTESIAN_POINT('Ctrl Pts',(-2.57345094230685,-0.319434907277157,
3.87182862652423));
#42929=CARTESIAN_POINT('Ctrl Pts',(-2.57134736188519,-0.158333333333332,
3.89403237082244));
#42930=CARTESIAN_POINT('Ctrl Pts',(-2.58789598152809,0.158333333333334,
3.90688493738757));
#42931=CARTESIAN_POINT('Ctrl Pts',(-2.60538706360735,0.319434907277166,
3.89677292530911));
#42932=CARTESIAN_POINT('Ctrl Pts',(-2.6605479894059,0.636309800095203,3.84718052087746));
#42933=CARTESIAN_POINT('Ctrl Pts',(-2.6936693350233,0.794772684000836,3.80141423297618));
#42934=CARTESIAN_POINT('Ctrl Pts',(-2.78812801035164,1.06847604194519,3.70775389303389));
#42935=CARTESIAN_POINT('Ctrl Pts',(-2.8379363203858,1.18514270861194,3.66037192978858));
#42936=CARTESIAN_POINT('Ctrl Pts',(-2.89666527994333,1.30000000000025,3.60615009400136));
#42937=CARTESIAN_POINT('Ctrl Pts',(-2.72326627312501,-1.3000000000001,3.49418507966825));
#42938=CARTESIAN_POINT('Ctrl Pts',(-2.68052794672654,-1.18514270861185,
3.56550529007524));
#42939=CARTESIAN_POINT('Ctrl Pts',(-2.64601630303685,-1.06847604194515,
3.62810375107432));
#42940=CARTESIAN_POINT('Ctrl Pts',(-2.58529278488251,-0.79477268400085,
3.75256973284915));
#42941=CARTESIAN_POINT('Ctrl Pts',(-2.56937357584712,-0.636309800095195,
3.81013291795898));
#42942=CARTESIAN_POINT('Ctrl Pts',(-2.5485676946795,-0.319434907277158,
3.88615363414296));
#42943=CARTESIAN_POINT('Ctrl Pts',(-2.54703863299078,-0.158333333333332,
3.9071876744658));
#42944=CARTESIAN_POINT('Ctrl Pts',(-2.56350678782447,0.158333333333334,
3.91999872873124));
#42945=CARTESIAN_POINT('Ctrl Pts',(-2.58059607962984,0.319434907277166,
3.91126747183114));
#42946=CARTESIAN_POINT('Ctrl Pts',(-2.63679578372307,0.636309800095204,
3.86237726186916));
#42947=CARTESIAN_POINT('Ctrl Pts',(-2.67065942773071,0.794772684000837,
3.81796691311235));
#42948=CARTESIAN_POINT('Ctrl Pts',(-2.76844578138871,1.06847604194519,3.72190506081139));
#42949=CARTESIAN_POINT('Ctrl Pts',(-2.82018062835327,1.18514270861195,3.67262192434545));
#42950=CARTESIAN_POINT('Ctrl Pts',(-2.88132223312535,1.30000000000025,3.61563726783222));
#42951=CARTESIAN_POINT('Ctrl Pts',(-2.71361311550265,-1.30000000000011,
3.50143025308128));
#42952=CARTESIAN_POINT('Ctrl Pts',(-2.67063753707723,-1.18514270861185,
3.57586971597518));
#42953=CARTESIAN_POINT('Ctrl Pts',(-2.63543757366511,-1.06847604194515,
3.64017761461974));
#42954=CARTESIAN_POINT('Ctrl Pts',(-2.57208184264171,-0.794772684000851,
3.76533578501125));
#42955=CARTESIAN_POINT('Ctrl Pts',(-2.55201129877974,-0.636309800095197,
3.81776217389487));
#42956=CARTESIAN_POINT('Ctrl Pts',(-2.52893211648025,-0.319434907277159,
3.89115367806483));
#42957=CARTESIAN_POINT('Ctrl Pts',(-2.52830982650113,-0.158333333333332,
3.91159193529207));
#42958=CARTESIAN_POINT('Ctrl Pts',(-2.54469368659007,0.158333333333334,
3.92427691489317));
#42959=CARTESIAN_POINT('Ctrl Pts',(-2.56094950441052,0.319434907277167,
3.9160722157167));
#42960=CARTESIAN_POINT('Ctrl Pts',(-2.61892980279681,0.636309800095206,
3.86943861483994));
#42961=CARTESIAN_POINT('Ctrl Pts',(-2.65591208556864,0.79477268400084,3.82959034377962));
#42962=CARTESIAN_POINT('Ctrl Pts',(-2.75637070809807,1.0684760419452,3.73285743382662));
#42963=CARTESIAN_POINT('Ctrl Pts',(-2.80906926850999,1.18514270861195,3.68202709105594));
#42964=CARTESIAN_POINT('Ctrl Pts',(-2.87098157399966,1.30000000000025,3.62223849792565));
#42965=CARTESIAN_POINT('Ctrl Pts',(-2.70549646903683,-1.30000000000011,
3.50427905152384));
#42966=CARTESIAN_POINT('Ctrl Pts',(-2.66274685239523,-1.18514270861185,
3.57860852562495));
#42967=CARTESIAN_POINT('Ctrl Pts',(-2.62751487735364,-1.06847604194515,
3.64257305686797));
#42968=CARTESIAN_POINT('Ctrl Pts',(-2.56348922287021,-0.794772684000851,
3.76639882859812));
#42969=CARTESIAN_POINT('Ctrl Pts',(-2.54183416968341,-0.636309800095197,
3.81680720028708));
#42970=CARTESIAN_POINT('Ctrl Pts',(-2.5177651372377,-0.319434907277159,
3.88883314466868));
#42971=CARTESIAN_POINT('Ctrl Pts',(-2.5171210925739,-0.158333333333332,
3.90931901361983));
#42972=CARTESIAN_POINT('Ctrl Pts',(-2.53338410693288,0.158333333333334,
3.92180031843115));
#42973=CARTESIAN_POINT('Ctrl Pts',(-2.54937394678571,0.319434907277167,
3.91311942209051));
#42974=CARTESIAN_POINT('Ctrl Pts',(-2.60843787791201,0.636309800095206,
3.86789463692126));
#42975=CARTESIAN_POINT('Ctrl Pts',(-2.64769917658169,0.79477268400084,3.83089639236956));
#42976=CARTESIAN_POINT('Ctrl Pts',(-2.74872068765948,1.0684760419452,3.73538570642258));
#42977=CARTESIAN_POINT('Ctrl Pts',(-2.80123722412075,1.18514270861195,3.68466093919396));
#42978=CARTESIAN_POINT('Ctrl Pts',(-2.8625418281136,1.30000000000025,3.62455444166347));
#42979=CARTESIAN_POINT('Ctrl Pts',(-2.70549646903679,-1.3,3.50427905152391));
#42980=CARTESIAN_POINT('Ctrl Pts',(-2.6627468523952,-1.18514270861178,3.57860852562499));
#42981=CARTESIAN_POINT('Ctrl Pts',(-2.62751487735363,-1.06847604194512,
3.64257305686799));
#42982=CARTESIAN_POINT('Ctrl Pts',(-2.56348922287021,-0.794772684000851,
3.76639882859813));
#42983=CARTESIAN_POINT('Ctrl Pts',(-2.54183416968341,-0.636309800095197,
3.81680720028709));
#42984=CARTESIAN_POINT('Ctrl Pts',(-2.5177651372377,-0.319434907277159,
3.88883314466869));
#42985=CARTESIAN_POINT('Ctrl Pts',(-2.5171210925739,-0.158333333333332,
3.90931901361984));
#42986=CARTESIAN_POINT('Ctrl Pts',(-2.53338410693288,0.158333333333334,
3.92180031843115));
#42987=CARTESIAN_POINT('Ctrl Pts',(-2.54937394678571,0.319434907277167,
3.91311942209052));
#42988=CARTESIAN_POINT('Ctrl Pts',(-2.60843787791201,0.636309800095206,
3.86789463692126));
#42989=CARTESIAN_POINT('Ctrl Pts',(-2.64769917658169,0.79477268400084,3.83089639236956));
#42990=CARTESIAN_POINT('Ctrl Pts',(-2.74872068765945,1.06847604194511,3.73538570642261));
#42991=CARTESIAN_POINT('Ctrl Pts',(-2.80123722412067,1.18514270861178,3.68466093919403));
#42992=CARTESIAN_POINT('Ctrl Pts',(-2.86254182811346,1.3,3.6245544416636));
#42993=CARTESIAN_POINT('',(-3.07985614647943,-1.2,3.32482437598077));
#42994=CARTESIAN_POINT('Ctrl Pts',(-3.07985614647943,-1.2,3.32482437598077));
#42995=CARTESIAN_POINT('Ctrl Pts',(-3.05880159510405,-1.21682960324337,
3.32958843015044));
#42996=CARTESIAN_POINT('Ctrl Pts',(-3.03724401462398,-1.23325611740907,
3.33351507474704));
#42997=CARTESIAN_POINT('Ctrl Pts',(-3.00530433450824,-1.258663098968,3.3408068297737));
#42998=CARTESIAN_POINT('Ctrl Pts',(-2.99504539268032,-1.26676816617002,
3.34309739992352));
#42999=CARTESIAN_POINT('Ctrl Pts',(-2.97658205919368,-1.28145232253012,
3.34737148534885));
#43000=CARTESIAN_POINT('Ctrl Pts',(-2.96351143750541,-1.29188182284861,
3.35046321236999));
#43001=CARTESIAN_POINT('Ctrl Pts',(-2.95536211928798,-1.29845781721288,
3.35249474764391));
#43002=CARTESIAN_POINT('Ctrl Pts',(-2.95440882469644,-1.29922951092393,
3.35273562153213));
#43003=CARTESIAN_POINT('Ctrl Pts',(-2.95346134579773,-1.30000000000001,
3.35297958429143));
#43004=CARTESIAN_POINT('',(-3.20083482100771,-0.653834841416722,3.42413500660232));
#43005=CARTESIAN_POINT('Ctrl Pts',(-3.20083482102253,-0.653834841416035,
3.42413500658066));
#43006=CARTESIAN_POINT('Ctrl Pts',(-3.18844346496178,-0.717856496133803,
3.41363074225233));
#43007=CARTESIAN_POINT('Ctrl Pts',(-3.17828009865403,-0.76380352052981,
3.40509366942734));
#43008=CARTESIAN_POINT('Ctrl Pts',(-3.13843063020648,-0.949540435597171,
3.37194717193105));
#43009=CARTESIAN_POINT('Ctrl Pts',(-3.11738257533065,-1.04584243573993,
3.35464908943026));
#43010=CARTESIAN_POINT('Ctrl Pts',(-3.07985614647943,-1.2,3.32482437598077));
#43011=CARTESIAN_POINT('',(-3.30596887606183,0.653834841531101,3.5158352655574));
#43012=CARTESIAN_POINT('Ctrl Pts',(-3.30596887606183,0.653834841531103,
3.5158352655574));
#43013=CARTESIAN_POINT('Ctrl Pts',(-3.26766136519301,0.57579115138873,3.53224551669641));
#43014=CARTESIAN_POINT('Ctrl Pts',(-3.23529265065951,0.493921174124157,
3.54536768290475));
#43015=CARTESIAN_POINT('Ctrl Pts',(-3.18741895852824,0.338203882217178,
3.56202990461054));
#43016=CARTESIAN_POINT('Ctrl Pts',(-3.17012611474238,0.26571581271928,3.566711121231));
#43017=CARTESIAN_POINT('Ctrl Pts',(-3.14580748980259,0.129742913188357,
3.56886089494024));
#43018=CARTESIAN_POINT('Ctrl Pts',(-3.13766993333606,0.0666421442921237,
3.56730149091443));
#43019=CARTESIAN_POINT('Ctrl Pts',(-3.12737311469443,-0.059551760498374,
3.55881396747486));
#43020=CARTESIAN_POINT('Ctrl Pts',(-3.12512389889361,-0.12280055430268,
3.55183348127266));
#43021=CARTESIAN_POINT('Ctrl Pts',(-3.12735116187767,-0.260149022110592,
3.531205618682));
#43022=CARTESIAN_POINT('Ctrl Pts',(-3.1331253832472,-0.333947687247939,
3.51657228235298));
#43023=CARTESIAN_POINT('Ctrl Pts',(-3.15628326243836,-0.491233450801308,
3.47816085215487));
#43024=CARTESIAN_POINT('Ctrl Pts',(-3.17536914576921,-0.57417245107474,
3.45312723759055));
#43025=CARTESIAN_POINT('Ctrl Pts',(-3.20083482096744,-0.653834841428439,
3.42413500659914));
#43026=CARTESIAN_POINT('',(-3.25186354350228,1.2,3.46799202915631));
#43027=CARTESIAN_POINT('Ctrl Pts',(-3.25186354350228,1.2,3.46799202915631));
#43028=CARTESIAN_POINT('Ctrl Pts',(-3.26156466363528,1.13197267961548,3.47644504403145));
#43029=CARTESIAN_POINT('Ctrl Pts',(-3.27383226153768,1.03501542741823,3.48720372632373));
#43030=CARTESIAN_POINT('Ctrl Pts',(-3.29731825275506,0.795382507989234,
3.50806756723355));
#43031=CARTESIAN_POINT('Ctrl Pts',(-3.30107256523771,0.741804412431255,
3.51144158276664));
#43032=CARTESIAN_POINT('Ctrl Pts',(-3.30596887606183,0.653834841531101,
3.5158352655574));
#43033=CARTESIAN_POINT('Ctrl Pts',(-3.12967817046589,1.29999999999997,3.4949204395439));
#43034=CARTESIAN_POINT('Ctrl Pts',(-3.14980150842174,1.28313646799302,3.48984401448758));
#43035=CARTESIAN_POINT('Ctrl Pts',(-3.1703340625042,1.26654363612861,3.48553070234103));
#43036=CARTESIAN_POINT('Ctrl Pts',(-3.20568221938911,1.23742285157402,3.47748741921129));
#43037=CARTESIAN_POINT('Ctrl Pts',(-3.22638995040895,1.22006242765915,3.47240583757775));
#43038=CARTESIAN_POINT('Ctrl Pts',(-3.25186354350228,1.2,3.46799202915631));
#43039=CARTESIAN_POINT('Ctrl Pts',(-2.70549646903679,-1.3,3.50427905152391));
#43040=CARTESIAN_POINT('Ctrl Pts',(-2.6627468523952,-1.18514270861178,3.57860852562499));
#43041=CARTESIAN_POINT('Ctrl Pts',(-2.62751487735363,-1.06847604194512,
3.64257305686799));
#43042=CARTESIAN_POINT('Ctrl Pts',(-2.56348922287021,-0.794772684000851,
3.76639882859812));
#43043=CARTESIAN_POINT('Ctrl Pts',(-2.54183416968341,-0.636309800095197,
3.81680720028708));
#43044=CARTESIAN_POINT('Ctrl Pts',(-2.5177651372377,-0.319434907277159,
3.88883314466869));
#43045=CARTESIAN_POINT('Ctrl Pts',(-2.5171210925739,-0.158333333333332,
3.90931901361984));
#43046=CARTESIAN_POINT('Ctrl Pts',(-2.53338410693288,0.158333333333335,
3.92180031843115));
#43047=CARTESIAN_POINT('Ctrl Pts',(-2.54937394678571,0.319434907277167,
3.91311942209052));
#43048=CARTESIAN_POINT('Ctrl Pts',(-2.60843787791201,0.636309800095206,
3.86789463692126));
#43049=CARTESIAN_POINT('Ctrl Pts',(-2.64769917658169,0.79477268400084,3.83089639236956));
#43050=CARTESIAN_POINT('Ctrl Pts',(-2.74872068765945,1.06847604194511,3.73538570642261));
#43051=CARTESIAN_POINT('Ctrl Pts',(-2.80123722412067,1.18514270861178,3.68466093919403));
#43052=CARTESIAN_POINT('Ctrl Pts',(-2.86254182811346,1.3,3.6245544416636));
#43053=CARTESIAN_POINT('Ctrl Pts',(-2.64228988766393,-1.3,3.46041520142157));
#43054=CARTESIAN_POINT('Ctrl Pts',(-2.60104997267594,-1.18514270861178,
3.53559420826078));
#43055=CARTESIAN_POINT('Ctrl Pts',(-2.5668907832622,-1.06847604194512,3.60011089886413));
#43056=CARTESIAN_POINT('Ctrl Pts',(-2.50433411476486,-0.794772684000851,
3.72452527718372));
#43057=CARTESIAN_POINT('Ctrl Pts',(-2.48221240828625,-0.636309800095197,
3.77438845839854));
#43058=CARTESIAN_POINT('Ctrl Pts',(-2.45791319726889,-0.319434907277159,
3.84578854257292));
#43059=CARTESIAN_POINT('Ctrl Pts',(-2.4563788705663,-0.158333333333332,
3.86540905050109));
#43060=CARTESIAN_POINT('Ctrl Pts',(-2.47285287150207,0.158333333333335,
3.87759995720264));
#43061=CARTESIAN_POINT('Ctrl Pts',(-2.48994083087453,0.319434907277167,
3.86949835813398));
#43062=CARTESIAN_POINT('Ctrl Pts',(-2.54967111951957,0.636309800095206,
3.82429908435506));
#43063=CARTESIAN_POINT('Ctrl Pts',(-2.58959512893996,0.79477268400084,3.7875761803357));
#43064=CARTESIAN_POINT('Ctrl Pts',(-2.68960290025109,1.06847604194511,3.69085029513349));
#43065=CARTESIAN_POINT('Ctrl Pts',(-2.7412627929643,1.18514270861178,3.63927587476892));
#43066=CARTESIAN_POINT('Ctrl Pts',(-2.80129291984328,1.3,3.57799608569654));
#43067=CARTESIAN_POINT('Ctrl Pts',(-2.57908330629107,-1.3,3.41655135131923));
#43068=CARTESIAN_POINT('Ctrl Pts',(-2.53935309295667,-1.18514270861178,
3.49257989089658));
#43069=CARTESIAN_POINT('Ctrl Pts',(-2.50626668917078,-1.06847604194512,
3.55764874086027));
#43070=CARTESIAN_POINT('Ctrl Pts',(-2.4451790066595,-0.794772684000851,
3.68265172576931));
#43071=CARTESIAN_POINT('Ctrl Pts',(-2.42259064688909,-0.636309800095197,
3.73196971650999));
#43072=CARTESIAN_POINT('Ctrl Pts',(-2.39806125730008,-0.319434907277159,
3.80274394047715));
#43073=CARTESIAN_POINT('Ctrl Pts',(-2.3956366485587,-0.158333333333332,
3.82149908738234));
#43074=CARTESIAN_POINT('Ctrl Pts',(-2.41232163607126,0.158333333333335,
3.83339959597414));
#43075=CARTESIAN_POINT('Ctrl Pts',(-2.43050771496334,0.319434907277167,
3.82587729417744));
#43076=CARTESIAN_POINT('Ctrl Pts',(-2.49090436112714,0.636309800095206,
3.78070353178886));
#43077=CARTESIAN_POINT('Ctrl Pts',(-2.53149108129823,0.79477268400084,3.74425596830185));
#43078=CARTESIAN_POINT('Ctrl Pts',(-2.63048511284273,1.06847604194511,3.64631488384437));
#43079=CARTESIAN_POINT('Ctrl Pts',(-2.68128836180793,1.18514270861178,3.59389081034381));
#43080=CARTESIAN_POINT('Ctrl Pts',(-2.74004401157309,1.3,3.53143772972948));
#43081=CARTESIAN_POINT('Ctrl Pts',(-2.5158767249182,-1.3,3.37268750121688));
#43082=CARTESIAN_POINT('Ctrl Pts',(-2.47765621323741,-1.18514270861178,
3.44956557353237));
#43083=CARTESIAN_POINT('Ctrl Pts',(-2.44564259507935,-1.06847604194512,
3.51518658285641));
#43084=CARTESIAN_POINT('Ctrl Pts',(-2.38602389855415,-0.794772684000851,
3.64077817435491));
#43085=CARTESIAN_POINT('Ctrl Pts',(-2.36296888549193,-0.636309800095197,
3.68955097462145));
#43086=CARTESIAN_POINT('Ctrl Pts',(-2.33820931733128,-0.319434907277159,
3.75969933838138));
#43087=CARTESIAN_POINT('Ctrl Pts',(-2.33489442655109,-0.158333333333332,
3.77758912426359));
#43088=CARTESIAN_POINT('Ctrl Pts',(-2.35179040064045,0.158333333333335,
3.78919923474563));
#43089=CARTESIAN_POINT('Ctrl Pts',(-2.37107459905216,0.319434907277167,
3.7822562302209));
#43090=CARTESIAN_POINT('Ctrl Pts',(-2.43213760273471,0.636309800095206,
3.73710797922266));
#43091=CARTESIAN_POINT('Ctrl Pts',(-2.4733870336565,0.79477268400084,3.70093575626799));
#43092=CARTESIAN_POINT('Ctrl Pts',(-2.57136732543437,1.06847604194511,3.60177947255526));
#43093=CARTESIAN_POINT('Ctrl Pts',(-2.62131393065155,1.18514270861178,3.54850574591871));
#43094=CARTESIAN_POINT('Ctrl Pts',(-2.67879510330291,1.3,3.48487937376242));
#43095=CARTESIAN_POINT('Ctrl Pts',(-2.5158767249182,-1.3,3.37268750121688));
#43096=CARTESIAN_POINT('Ctrl Pts',(-2.47765621323741,-1.18514270861178,
3.44956557353237));
#43097=CARTESIAN_POINT('Ctrl Pts',(-2.44564259507935,-1.06847604194512,
3.51518658285641));
#43098=CARTESIAN_POINT('Ctrl Pts',(-2.38602389855415,-0.794772684000851,
3.64077817435491));
#43099=CARTESIAN_POINT('Ctrl Pts',(-2.36296888549193,-0.636309800095197,
3.68955097462145));
#43100=CARTESIAN_POINT('Ctrl Pts',(-2.33820931733128,-0.319434907277159,
3.75969933838138));
#43101=CARTESIAN_POINT('Ctrl Pts',(-2.33489442655109,-0.158333333333332,
3.77758912426359));
#43102=CARTESIAN_POINT('Ctrl Pts',(-2.35179040064045,0.158333333333334,
3.78919923474563));
#43103=CARTESIAN_POINT('Ctrl Pts',(-2.37107459905216,0.319434907277167,
3.7822562302209));
#43104=CARTESIAN_POINT('Ctrl Pts',(-2.4321376027347,0.636309800095206,3.73710797922267));
#43105=CARTESIAN_POINT('Ctrl Pts',(-2.4733870336565,0.79477268400084,3.70093575626799));
#43106=CARTESIAN_POINT('Ctrl Pts',(-2.57136732543437,1.06847604194511,3.60177947255526));
#43107=CARTESIAN_POINT('Ctrl Pts',(-2.62131393065155,1.18514270861178,3.54850574591871));
#43108=CARTESIAN_POINT('Ctrl Pts',(-2.67879510330291,1.3,3.48487937376242));
#43109=CARTESIAN_POINT('Ctrl Pts',(-2.51587672491883,-1.30000000000188,
3.37268750121562));
#43110=CARTESIAN_POINT('Ctrl Pts',(-2.47765621323776,-1.18514270861306,
3.44956557353166));
#43111=CARTESIAN_POINT('Ctrl Pts',(-2.44564259507949,-1.06847604194576,
3.51518658285611));
#43112=CARTESIAN_POINT('Ctrl Pts',(-2.38602389855415,-0.794772684000851,
3.64077817435491));
#43113=CARTESIAN_POINT('Ctrl Pts',(-2.36296888549193,-0.636309800095197,
3.68955097462145));
#43114=CARTESIAN_POINT('Ctrl Pts',(-2.33820931733127,-0.319434907277159,
3.75969933838138));
#43115=CARTESIAN_POINT('Ctrl Pts',(-2.33489442655109,-0.158333333333332,
3.77758912426359));
#43116=CARTESIAN_POINT('Ctrl Pts',(-2.35179040064045,0.158333333333335,
3.78919923474563));
#43117=CARTESIAN_POINT('Ctrl Pts',(-2.37107459905216,0.319434907277167,
3.7822562302209));
#43118=CARTESIAN_POINT('Ctrl Pts',(-2.43213760273471,0.636309800095207,
3.73710797922267));
#43119=CARTESIAN_POINT('Ctrl Pts',(-2.4733870336565,0.79477268400084,3.70093575626799));
#43120=CARTESIAN_POINT('Ctrl Pts',(-2.57136732543453,1.06847604194556,3.6017794725551));
#43121=CARTESIAN_POINT('Ctrl Pts',(-2.62131393065193,1.18514270861267,3.5485057459183));
#43122=CARTESIAN_POINT('Ctrl Pts',(-2.67879510330356,1.30000000000132,3.48487937376169));
#43123=CARTESIAN_POINT('Ctrl Pts',(-2.51547129336111,-1.30000000000188,
3.36394515997075));
#43124=CARTESIAN_POINT('Ctrl Pts',(-2.47774091682546,-1.18514270861306,
3.44130295288659));
#43125=CARTESIAN_POINT('Ctrl Pts',(-2.44568313885693,-1.06847604194576,
3.50712970190754));
#43126=CARTESIAN_POINT('Ctrl Pts',(-2.38472809610279,-0.794772684000851,
3.63256364256694));
#43127=CARTESIAN_POINT('Ctrl Pts',(-2.35825829212047,-0.636309800095197,
3.68004967653104));
#43128=CARTESIAN_POINT('Ctrl Pts',(-2.33182399965475,-0.319434907277159,
3.74960279232756));
#43129=CARTESIAN_POINT('Ctrl Pts',(-2.32904419096771,-0.158333333333332,
3.76759838532249));
#43130=CARTESIAN_POINT('Ctrl Pts',(-2.34617121467972,0.158333333333335,
3.77926048794922));
#43131=CARTESIAN_POINT('Ctrl Pts',(-2.36541685425652,0.319434907277167,
3.77235288613749));
#43132=CARTESIAN_POINT('Ctrl Pts',(-2.42808446300845,0.636309800095207,
3.72772405736545));
#43133=CARTESIAN_POINT('Ctrl Pts',(-2.47174278263682,0.79477268400084,3.69243519072899));
#43134=CARTESIAN_POINT('Ctrl Pts',(-2.57119727857627,1.06847604194556,3.59350430826072));
#43135=CARTESIAN_POINT('Ctrl Pts',(-2.62148033773407,1.18514270861267,3.54015492013262));
#43136=CARTESIAN_POINT('Ctrl Pts',(-2.67899628990966,1.30000000000132,3.47627965714654));
#43137=CARTESIAN_POINT('Ctrl Pts',(-2.51853827080824,-1.30000000000189,
3.35206487685959));
#43138=CARTESIAN_POINT('Ctrl Pts',(-2.48323413486177,-1.18514270861306,
3.42782456306498));
#43139=CARTESIAN_POINT('Ctrl Pts',(-2.45234882369544,-1.06847604194577,
3.49225791361269));
#43140=CARTESIAN_POINT('Ctrl Pts',(-2.39120594554101,-0.794772684000855,
3.61494574203019));
#43141=CARTESIAN_POINT('Ctrl Pts',(-2.3594335950636,-0.6363098000952,3.66087544146455));
#43142=CARTESIAN_POINT('Ctrl Pts',(-2.33031342459444,-0.319434907277161,
3.72943794009915));
#43143=CARTESIAN_POINT('Ctrl Pts',(-2.32730904942448,-0.158333333333333,
3.74839715610966));
#43144=CARTESIAN_POINT('Ctrl Pts',(-2.34458564073266,0.158333333333335,
3.76010251086989));
#43145=CARTESIAN_POINT('Ctrl Pts',(-2.36410755575917,0.319434907277168,
3.75214497427109));
#43146=CARTESIAN_POINT('Ctrl Pts',(-2.42996503192065,0.636309800095209,
3.70885877648818));
#43147=CARTESIAN_POINT('Ctrl Pts',(-2.47977225887544,0.794772684000846,
3.67592019371372));
#43148=CARTESIAN_POINT('Ctrl Pts',(-2.57938359964614,1.06847604194557,3.57970434673727));
#43149=CARTESIAN_POINT('Ctrl Pts',(-2.62825978626735,1.18514270861267,3.52753909508197));
#43150=CARTESIAN_POINT('Ctrl Pts',(-2.68289410105402,1.30000000000132,3.46485686677906));
#43151=CARTESIAN_POINT('Ctrl Pts',(-2.52292752087448,-1.30000000000189,
3.33458767675074));
#43152=CARTESIAN_POINT('Ctrl Pts',(-2.48950805307769,-1.18514270861306,
3.40719198419399));
#43153=CARTESIAN_POINT('Ctrl Pts',(-2.45982937263478,-1.06847604194577,
3.46919618877897));
#43154=CARTESIAN_POINT('Ctrl Pts',(-2.39990765074157,-0.794772684000851,
3.58794994712263));
#43155=CARTESIAN_POINT('Ctrl Pts',(-2.36656127553431,-0.636309800095197,
3.63356590556153));
#43156=CARTESIAN_POINT('Ctrl Pts',(-2.33639476318404,-0.319434907277158,
3.70132582143229));
#43157=CARTESIAN_POINT('Ctrl Pts',(-2.3321583303109,-0.158333333333332,
3.72107192945569));
#43158=CARTESIAN_POINT('Ctrl Pts',(-2.34950231633539,0.158333333333335,
3.73284122474502));
#43159=CARTESIAN_POINT('Ctrl Pts',(-2.37002428895053,0.319434907277167,
3.72400619726931));
#43160=CARTESIAN_POINT('Ctrl Pts',(-2.43767523089105,0.636309800095207,
3.68196761012071));
#43161=CARTESIAN_POINT('Ctrl Pts',(-2.49068724875985,0.79477268400084,3.65027347088613));
#43162=CARTESIAN_POINT('Ctrl Pts',(-2.58924608413157,1.06847604194556,3.55802851883701));
#43163=CARTESIAN_POINT('Ctrl Pts',(-2.63663527394617,1.18514270861267,3.50809174964151));
#43164=CARTESIAN_POINT('Ctrl Pts',(-2.68875118570763,1.30000000000132,3.4481476329803));
#43165=CARTESIAN_POINT('Ctrl Pts',(-2.52626319062645,-1.30000000000189,
3.31997332758331));
#43166=CARTESIAN_POINT('Ctrl Pts',(-2.49390945973534,-1.18514270861307,
3.39004411305226));
#43167=CARTESIAN_POINT('Ctrl Pts',(-2.46513663227325,-1.06847604194577,
3.45027777812963));
#43168=CARTESIAN_POINT('Ctrl Pts',(-2.40693824812987,-0.794772684000855,
3.56670387814771));
#43169=CARTESIAN_POINT('Ctrl Pts',(-2.37477597879238,-0.6363098000952,3.61364878594488));
#43170=CARTESIAN_POINT('Ctrl Pts',(-2.34450584441073,-0.31943490727716,
3.68133034339864));
#43171=CARTESIAN_POINT('Ctrl Pts',(-2.3383164193559,-0.158333333333333,
3.70105402547771));
#43172=CARTESIAN_POINT('Ctrl Pts',(-2.35514613629035,0.158333333333335,
3.71254944309585));
#43173=CARTESIAN_POINT('Ctrl Pts',(-2.37631674908184,0.319434907277168,
3.70302032704325));
#43174=CARTESIAN_POINT('Ctrl Pts',(-2.44463312595647,0.636309800095209,
3.66140384860793));
#43175=CARTESIAN_POINT('Ctrl Pts',(-2.49930521873998,0.794772684000844,
3.63002735427069));
#43176=CARTESIAN_POINT('Ctrl Pts',(-2.59662799796044,1.06847604194557,3.54034136887886));
#43177=CARTESIAN_POINT('Ctrl Pts',(-2.64282176914256,1.18514270861267,3.49197249566252));
#43178=CARTESIAN_POINT('Ctrl Pts',(-2.69308188654657,1.30000000000132,3.43405648911277));
#43179=CARTESIAN_POINT('Ctrl Pts',(-2.52947109631203,-1.3000000000019,3.30515554054755));
#43180=CARTESIAN_POINT('Ctrl Pts',(-2.4982353574683,-1.18514270861307,3.37242269051184));
#43181=CARTESIAN_POINT('Ctrl Pts',(-2.47043731159163,-1.06847604194577,
3.43068854649148));
#43182=CARTESIAN_POINT('Ctrl Pts',(-2.4141600230987,-0.794772684000854,
3.54449954004145));
#43183=CARTESIAN_POINT('Ctrl Pts',(-2.38321138359984,-0.636309800095201,
3.59271601910825));
#43184=CARTESIAN_POINT('Ctrl Pts',(-2.35338894010272,-0.319434907277161,
3.66052836665431));
#43185=CARTESIAN_POINT('Ctrl Pts',(-2.3455486272765,-0.158333333333333,
3.6804690126673));
#43186=CARTESIAN_POINT('Ctrl Pts',(-2.36312304611341,0.158333333333335,
3.69242853718606));
#43187=CARTESIAN_POINT('Ctrl Pts',(-2.38713818590456,0.319434907277169,
3.68343593736614));
#43188=CARTESIAN_POINT('Ctrl Pts',(-2.45560932304154,0.63630980009521,3.642044588671));
#43189=CARTESIAN_POINT('Ctrl Pts',(-2.50846844727388,0.794772684000845,
3.60899746335514));
#43190=CARTESIAN_POINT('Ctrl Pts',(-2.60345505149333,1.06847604194557,3.52162332902105));
#43191=CARTESIAN_POINT('Ctrl Pts',(-2.6484597732741,1.18514270861268,3.47506651058648));
#43192=CARTESIAN_POINT('Ctrl Pts',(-2.69735303546953,1.30000000000133,3.41977389893987));
#43193=CARTESIAN_POINT('Ctrl Pts',(-2.53134877776986,-1.3000000000019,3.28980202776907));
#43194=CARTESIAN_POINT('Ctrl Pts',(-2.50121228756566,-1.18514270861307,
3.35442528940338));
#43195=CARTESIAN_POINT('Ctrl Pts',(-2.47444764782297,-1.06847604194577,
3.41088093356189));
#43196=CARTESIAN_POINT('Ctrl Pts',(-2.42040562487214,-0.794772684000858,
3.52243593518531));
#43197=CARTESIAN_POINT('Ctrl Pts',(-2.39088943992526,-0.636309800095202,
3.57201352308727));
#43198=CARTESIAN_POINT('Ctrl Pts',(-2.36256753038988,-0.31943490727716,
3.64055918748032));
#43199=CARTESIAN_POINT('Ctrl Pts',(-2.35485164728609,-0.158333333333334,
3.66166760646211));
#43200=CARTESIAN_POINT('Ctrl Pts',(-2.3729430685714,0.158333333333336,3.67396851024435));
#43201=CARTESIAN_POINT('Ctrl Pts',(-2.39748268499734,0.319434907277171,
3.66427636246471));
#43202=CARTESIAN_POINT('Ctrl Pts',(-2.46523770616973,0.636309800095212,
3.62258868625159));
#43203=CARTESIAN_POINT('Ctrl Pts',(-2.51686220295093,0.794772684000845,
3.58818042239233));
#43204=CARTESIAN_POINT('Ctrl Pts',(-2.60992269931834,1.06847604194557,3.50312536915743));
#43205=CARTESIAN_POINT('Ctrl Pts',(-2.65397997707813,1.18514270861268,3.45837677647556));
#43206=CARTESIAN_POINT('Ctrl Pts',(-2.70181209195141,1.30000000000133,3.40569677205695));
#43207=CARTESIAN_POINT('Ctrl Pts',(-2.53635588003711,-1.3000000000019,3.26613435433843));
#43208=CARTESIAN_POINT('Ctrl Pts',(-2.50805836951591,-1.18514270861307,
3.3264578589723));
#43209=CARTESIAN_POINT('Ctrl Pts',(-2.48283369508773,-1.06847604194577,
3.3798771798381));
#43210=CARTESIAN_POINT('Ctrl Pts',(-2.43165851707361,-0.794772684000857,
3.48733645185484));
#43211=CARTESIAN_POINT('Ctrl Pts',(-2.40309141806982,-0.6363098000952,3.53841937537954));
#43212=CARTESIAN_POINT('Ctrl Pts',(-2.37626797477541,-0.319434907277159,
3.60766339284895));
#43213=CARTESIAN_POINT('Ctrl Pts',(-2.36878433321108,-0.158333333333333,
3.63071322404922));
#43214=CARTESIAN_POINT('Ctrl Pts',(-2.38740199596886,0.158333333333336,
3.64334586191059));
#43215=CARTESIAN_POINT('Ctrl Pts',(-2.41247548198169,0.319434907277172,
3.63220119159509));
#43216=CARTESIAN_POINT('Ctrl Pts',(-2.4793153556881,0.636309800095213,3.59017076609043));
#43217=CARTESIAN_POINT('Ctrl Pts',(-2.52996061380194,0.794772684000844,
3.55424616566083));
#43218=CARTESIAN_POINT('Ctrl Pts',(-2.61989032360897,1.06847604194557,3.47305078123809));
#43219=CARTESIAN_POINT('Ctrl Pts',(-2.66218344562222,1.18514270861267,3.4311513215582));
#43220=CARTESIAN_POINT('Ctrl Pts',(-2.70784245049735,1.30000000000132,3.38249887552958));
#43221=CARTESIAN_POINT('Ctrl Pts',(-2.54098117524275,-1.30000000000194,
3.23262551129656));
#43222=CARTESIAN_POINT('Ctrl Pts',(-2.5137239795217,-1.18514270861311,3.2864637443441));
#43223=CARTESIAN_POINT('Ctrl Pts',(-2.48977880870604,-1.0684760419458,3.3353958627565));
#43224=CARTESIAN_POINT('Ctrl Pts',(-2.44211211400679,-0.79477268400088,
3.43710473885357));
#43225=CARTESIAN_POINT('Ctrl Pts',(-2.41706898213178,-0.636309800095219,
3.4911932805752));
#43226=CARTESIAN_POINT('Ctrl Pts',(-2.39356025850244,-0.319434907277169,
3.56193348901071));
#43227=CARTESIAN_POINT('Ctrl Pts',(-2.38679878295003,-0.158333333333338,
3.58777302468684));
#43228=CARTESIAN_POINT('Ctrl Pts',(-2.40650274675603,0.15833333333334,3.60107340307502));
#43229=CARTESIAN_POINT('Ctrl Pts',(-2.43222643859139,0.31943490727718,3.58806460049873));
#43230=CARTESIAN_POINT('Ctrl Pts',(-2.49738160405796,0.63630980009523,3.54537293881767));
#43231=CARTESIAN_POINT('Ctrl Pts',(-2.5454550115792,0.794772684000866,3.50665907806544));
#43232=CARTESIAN_POINT('Ctrl Pts',(-2.63149657495587,1.0684760419456,3.43086506796219));
#43233=CARTESIAN_POINT('Ctrl Pts',(-2.67191622125882,1.18514270861271,3.39310031169925));
#43234=CARTESIAN_POINT('Ctrl Pts',(-2.71551130923304,1.30000000000137,3.35037921770225));
#43235=CARTESIAN_POINT('Ctrl Pts',(-2.54607194775883,-1.30000000000194,
3.19608939128788));
#43236=CARTESIAN_POINT('Ctrl Pts',(-2.52146571190023,-1.18514270861311,
3.24347357409477));
#43237=CARTESIAN_POINT('Ctrl Pts',(-2.49960544585642,-1.06847604194581,
3.28775993886287));
#43238=CARTESIAN_POINT('Ctrl Pts',(-2.45544759776561,-0.794772684000886,
3.38291372154783));
#43239=CARTESIAN_POINT('Ctrl Pts',(-2.430480323573,-0.636309800095224,3.43848528660745));
#43240=CARTESIAN_POINT('Ctrl Pts',(-2.40891442716951,-0.319434907277172,
3.50999985813467));
#43241=CARTESIAN_POINT('Ctrl Pts',(-2.40350022809356,-0.158333333333339,
3.53915059384038));
#43242=CARTESIAN_POINT('Ctrl Pts',(-2.42416152391693,0.158333333333341,
3.55297228552503));
#43243=CARTESIAN_POINT('Ctrl Pts',(-2.44991916944357,0.319434907277179,
3.53741124744924));
#43244=CARTESIAN_POINT('Ctrl Pts',(-2.51421807406285,0.636309800095232,
3.49452302187417));
#43245=CARTESIAN_POINT('Ctrl Pts',(-2.56169302483603,0.794772684000873,
3.45408481116691));
#43246=CARTESIAN_POINT('Ctrl Pts',(-2.64468685271695,1.06847604194561,3.38495701231189));
#43247=CARTESIAN_POINT('Ctrl Pts',(-2.68331682422934,1.18514270861272,3.35190032778415));
#43248=CARTESIAN_POINT('Ctrl Pts',(-2.72465181438882,1.30000000000137,3.31570982141567));
#43249=CARTESIAN_POINT('Ctrl Pts',(-2.54893825527318,-1.30000000000195,
3.1715295558725));
#43250=CARTESIAN_POINT('Ctrl Pts',(-2.52456767240702,-1.18514270861312,
3.2139499308541));
#43251=CARTESIAN_POINT('Ctrl Pts',(-2.50318298479296,-1.06847604194582,
3.25474400510964));
#43252=CARTESIAN_POINT('Ctrl Pts',(-2.46067809377112,-0.794772684000895,
3.34522939744867));
#43253=CARTESIAN_POINT('Ctrl Pts',(-2.43785098142268,-0.636309800095231,
3.40270562498112));
#43254=CARTESIAN_POINT('Ctrl Pts',(-2.41819118871568,-0.319434907277175,
3.47496318623089));
#43255=CARTESIAN_POINT('Ctrl Pts',(-2.41324425637799,-0.158333333333341,
3.50605275406172));
#43256=CARTESIAN_POINT('Ctrl Pts',(-2.43459928047454,0.158333333333343,
3.52024485921037));
#43257=CARTESIAN_POINT('Ctrl Pts',(-2.46065104029608,0.319434907277184,
3.50319259994508));
#43258=CARTESIAN_POINT('Ctrl Pts',(-2.52431911196031,0.63630980009524,3.46015864451169));
#43259=CARTESIAN_POINT('Ctrl Pts',(-2.57105352724188,0.794772684000883,
3.41837301501752));
#43260=CARTESIAN_POINT('Ctrl Pts',(-2.65183111157973,1.06847604194562,3.35356418715493));
#43261=CARTESIAN_POINT('Ctrl Pts',(-2.68921977408514,1.18514270861273,3.32360433739698));
#43262=CARTESIAN_POINT('Ctrl Pts',(-2.72903147594052,1.30000000000138,3.29173797805909));
#43263=CARTESIAN_POINT('Ctrl Pts',(-2.55043866196968,-1.30000000000196,
3.15283126618602));
#43264=CARTESIAN_POINT('Ctrl Pts',(-2.52735906897743,-1.18514270861313,
3.19201784177817));
#43265=CARTESIAN_POINT('Ctrl Pts',(-2.50701882331754,-1.06847604194582,
3.23049388197808));
#43266=CARTESIAN_POINT('Ctrl Pts',(-2.46635722713344,-0.794772684000895,
3.31773975304688));
#43267=CARTESIAN_POINT('Ctrl Pts',(-2.44399336583575,-0.636309800095233,
3.37614613933208));
#43268=CARTESIAN_POINT('Ctrl Pts',(-2.42503654909892,-0.319434907277177,
3.44862255465249));
#43269=CARTESIAN_POINT('Ctrl Pts',(-2.41986793208942,-0.158333333333341,
3.48088506283785));
#43270=CARTESIAN_POINT('Ctrl Pts',(-2.44157186869421,0.158333333333343,
3.49526279903694));
#43271=CARTESIAN_POINT('Ctrl Pts',(-2.46817051309274,0.319434907277183,
3.47722483799343));
#43272=CARTESIAN_POINT('Ctrl Pts',(-2.53189461930863,0.636309800095241,
3.43434687115883));
#43273=CARTESIAN_POINT('Ctrl Pts',(-2.57870590041425,0.794772684000886,
3.39189384649464));
#43274=CARTESIAN_POINT('Ctrl Pts',(-2.65818528340837,1.06847604194562,3.33052500181169));
#43275=CARTESIAN_POINT('Ctrl Pts',(-2.69470560532199,1.18514270861274,3.30292603445292));
#43276=CARTESIAN_POINT('Ctrl Pts',(-2.73334256925239,1.30000000000139,3.27429239865887));
#43277=CARTESIAN_POINT('Ctrl Pts',(-2.55358415559061,-1.30000000000197,
3.12519350169584));
#43278=CARTESIAN_POINT('Ctrl Pts',(-2.53103602156771,-1.18514270861314,
3.15892145377589));
#43279=CARTESIAN_POINT('Ctrl Pts',(-2.51131793932318,-1.06847604194584,
3.19350862461068));
#43280=CARTESIAN_POINT('Ctrl Pts',(-2.4723032105075,-0.794772684000908,
3.27539687558823));
#43281=CARTESIAN_POINT('Ctrl Pts',(-2.45134421773899,-0.636309800095241,
3.33546738470793));
#43282=CARTESIAN_POINT('Ctrl Pts',(-2.43421476586456,-0.319434907277181,
3.40861739061838));
#43283=CARTESIAN_POINT('Ctrl Pts',(-2.43012713057062,-0.158333333333343,
3.44332102563396));
#43284=CARTESIAN_POINT('Ctrl Pts',(-2.45236775886849,0.158333333333345,
3.45797138395048));
#43285=CARTESIAN_POINT('Ctrl Pts',(-2.47853889838145,0.319434907277189,
3.43785084550915));
#43286=CARTESIAN_POINT('Ctrl Pts',(-2.54129095915557,0.63630980009525,3.39467957195464));
#43287=CARTESIAN_POINT('Ctrl Pts',(-2.58736634141913,0.794772684000896,
3.35079547747347));
#43288=CARTESIAN_POINT('Ctrl Pts',(-2.66489054887304,1.06847604194564,3.29456729103865));
#43289=CARTESIAN_POINT('Ctrl Pts',(-2.70037289791079,1.18514270861275,3.27063264666337));
#43290=CARTESIAN_POINT('Ctrl Pts',(-2.73778023913444,1.30000000000141,3.24710245636084));
#43291=CARTESIAN_POINT('Ctrl Pts',(-2.55593709808298,-1.30000000000202,
3.08759717673342));
#43292=CARTESIAN_POINT('Ctrl Pts',(-2.53449134505796,-1.18514270861318,
3.11424537955628));
#43293=CARTESIAN_POINT('Ctrl Pts',(-2.51587115807294,-1.06847604194588,
3.14377869822358));
#43294=CARTESIAN_POINT('Ctrl Pts',(-2.47938242398696,-0.794772684000935,
3.21867176723112));
#43295=CARTESIAN_POINT('Ctrl Pts',(-2.46021519347327,-0.636309800095264,
3.28089625856297));
#43296=CARTESIAN_POINT('Ctrl Pts',(-2.44514895149305,-0.319434907277192,
3.35472334103413));
#43297=CARTESIAN_POINT('Ctrl Pts',(-2.44164372936051,-0.158333333333349,
3.39222589801146));
#43298=CARTESIAN_POINT('Ctrl Pts',(-2.46468090308572,0.158333333333351,
3.40726305730602));
#43299=CARTESIAN_POINT('Ctrl Pts',(-2.49106278789201,0.319434907277199,
3.38476509205472));
#43300=CARTESIAN_POINT('Ctrl Pts',(-2.55338104347357,0.636309800095272,
3.34163395814732));
#43301=CARTESIAN_POINT('Ctrl Pts',(-2.59898610889037,0.794772684000924,
3.29609989894042));
#43302=CARTESIAN_POINT('Ctrl Pts',(-2.67459867825352,1.06847604194568,3.24706841498202));
#43303=CARTESIAN_POINT('Ctrl Pts',(-2.70896671379464,1.18514270861279,3.22815047231979));
#43304=CARTESIAN_POINT('Ctrl Pts',(-2.74497290532134,1.30000000000146,3.21153849960543));
#43305=CARTESIAN_POINT('Ctrl Pts',(-2.55909406402193,-1.30000000000205,
3.04400046157339));
#43306=CARTESIAN_POINT('Ctrl Pts',(-2.5382866672259,-1.18514270861321,3.06214142930381));
#43307=CARTESIAN_POINT('Ctrl Pts',(-2.52034870426,-1.0684760419459,3.08553727610246));
#43308=CARTESIAN_POINT('Ctrl Pts',(-2.48553738750759,-0.794772684000951,
3.15172618441284));
#43309=CARTESIAN_POINT('Ctrl Pts',(-2.46731670249777,-0.636309800095274,
3.2159249062016));
#43310=CARTESIAN_POINT('Ctrl Pts',(-2.45457240355061,-0.319434907277196,
3.29045296825996));
#43311=CARTESIAN_POINT('Ctrl Pts',(-2.45309797862502,-0.158333333333352,
3.33175999081764));
#43312=CARTESIAN_POINT('Ctrl Pts',(-2.4775003642474,0.158333333333354,3.34740226567864));
#43313=CARTESIAN_POINT('Ctrl Pts',(-2.50375051020395,0.319434907277208,
3.32197121857406));
#43314=CARTESIAN_POINT('Ctrl Pts',(-2.56544025428757,0.636309800095285,
3.27882931284725));
#43315=CARTESIAN_POINT('Ctrl Pts',(-2.61047096591202,0.794772684000935,
3.23138292291287));
#43316=CARTESIAN_POINT('Ctrl Pts',(-2.68375360165742,1.06847604194569,3.19067109065635));
#43317=CARTESIAN_POINT('Ctrl Pts',(-2.71677357684178,1.18514270861281,3.17755924429881));
#43318=CARTESIAN_POINT('Ctrl Pts',(-2.75109218958555,1.30000000000148,3.16895819524558));
#43319=CARTESIAN_POINT('Ctrl Pts',(-2.55969404135944,-1.30000000000211,
3.01222601946097));
#43320=CARTESIAN_POINT('Ctrl Pts',(-2.53876245937103,-1.18514270861326,
3.02409177121432));
#43321=CARTESIAN_POINT('Ctrl Pts',(-2.52106667650709,-1.06847604194595,
3.043027194833));
#43322=CARTESIAN_POINT('Ctrl Pts',(-2.48766122135914,-0.794772684000989,
3.10310416770247));
#43323=CARTESIAN_POINT('Ctrl Pts',(-2.47212874699672,-0.636309800095306,
3.16950845560562));
#43324=CARTESIAN_POINT('Ctrl Pts',(-2.46094251411636,-0.319434907277213,
3.24444466879074));
#43325=CARTESIAN_POINT('Ctrl Pts',(-2.4590317912922,-0.158333333333359,
3.28762636471884));
#43326=CARTESIAN_POINT('Ctrl Pts',(-2.48383371179482,0.158333333333362,
3.30343883720611));
#43327=CARTESIAN_POINT('Ctrl Pts',(-2.51066893582012,0.319434907277222,
3.27622966764146));
#43328=CARTESIAN_POINT('Ctrl Pts',(-2.57212520691001,0.636309800095316,
3.2331763041556));
#43329=CARTESIAN_POINT('Ctrl Pts',(-2.61640131477568,0.794772684000977,
3.18420338560199));
#43330=CARTESIAN_POINT('Ctrl Pts',(-2.68867278939858,1.06847604194574,3.14971672375969));
#43331=CARTESIAN_POINT('Ctrl Pts',(-2.72120196670161,1.18514270861287,3.14095830281351));
#43332=CARTESIAN_POINT('Ctrl Pts',(-2.75497667786541,1.30000000000154,3.13836945897594));
#43333=CARTESIAN_POINT('Ctrl Pts',(-2.56116907507594,-1.30000000000213,
2.98723486350912));
#43334=CARTESIAN_POINT('Ctrl Pts',(-2.54075722636678,-1.18514270861329,
2.99432776760199));
#43335=CARTESIAN_POINT('Ctrl Pts',(-2.52343611256515,-1.06847604194597,
3.00976701257515));
#43336=CARTESIAN_POINT('Ctrl Pts',(-2.49056109054234,-0.794772684001007,
3.06471647418665));
#43337=CARTESIAN_POINT('Ctrl Pts',(-2.47447675889149,-0.636309800095319,
3.13180258532495));
#43338=CARTESIAN_POINT('Ctrl Pts',(-2.46408895434673,-0.319434907277219,
3.20688977378303));
#43339=CARTESIAN_POINT('Ctrl Pts',(-2.46347706359624,-0.158333333333363,
3.25223928787584));
#43340=CARTESIAN_POINT('Ctrl Pts',(-2.48922823124499,0.158333333333365,
3.26843939953327));
#43341=CARTESIAN_POINT('Ctrl Pts',(-2.51624885866665,0.31943490727723,3.23967905792092));
#43342=CARTESIAN_POINT('Ctrl Pts',(-2.5777505168142,0.63630980009533,3.19679784157907));
#43343=CARTESIAN_POINT('Ctrl Pts',(-2.62193161309762,0.794772684000992,
3.14684768294999));
#43344=CARTESIAN_POINT('Ctrl Pts',(-2.6932852563524,1.06847604194577,3.11728699184811));
#43345=CARTESIAN_POINT('Ctrl Pts',(-2.72522894628803,1.1851427086129,3.11191854353062));
#43346=CARTESIAN_POINT('Ctrl Pts',(-2.7582299779073,1.30000000000157,3.11397737474212));
#43347=CARTESIAN_POINT('Ctrl Pts',(-2.56104903447691,-1.30000000000216,
2.97280661034047));
#43348=CARTESIAN_POINT('Ctrl Pts',(-2.54061337483588,-1.18514270861331,
2.97710536479362));
#43349=CARTESIAN_POINT('Ctrl Pts',(-2.52338049166604,-1.06847604194599,
2.99053937526616));
#43350=CARTESIAN_POINT('Ctrl Pts',(-2.49096813847904,-0.794772684001021,
3.04267889582866));
#43351=CARTESIAN_POINT('Ctrl Pts',(-2.47557323327233,-0.636309800095332,
3.11052944246156));
#43352=CARTESIAN_POINT('Ctrl Pts',(-2.46599547637307,-0.319434907277227,
3.18583494016677));
#43353=CARTESIAN_POINT('Ctrl Pts',(-2.4659166650027,-0.158333333333366,
3.23232159152127));
#43354=CARTESIAN_POINT('Ctrl Pts',(-2.49195600008211,0.158333333333368,
3.24863192396712));
#43355=CARTESIAN_POINT('Ctrl Pts',(-2.5187862531373,0.319434907277236,3.21887732256778));
#43356=CARTESIAN_POINT('Ctrl Pts',(-2.57995375081713,0.636309800095343,
3.1759357894701));
#43357=CARTESIAN_POINT('Ctrl Pts',(-2.62365207930783,0.79477268400101,3.12524345459197));
#43358=CARTESIAN_POINT('Ctrl Pts',(-2.69472279222533,1.06847604194579,3.09855134679839));
#43359=CARTESIAN_POINT('Ctrl Pts',(-2.72660847127242,1.18514270861292,3.09520649332736));
#43360=CARTESIAN_POINT('Ctrl Pts',(-2.759615951174,1.30000000000159,3.1000708108091));
#43361=CARTESIAN_POINT('Ctrl Pts',(-2.56127831437987,-1.30000000000217,
2.96331663785848));
#43362=CARTESIAN_POINT('Ctrl Pts',(-2.54088772104557,-1.18514270861332,
2.96577295199612));
#43363=CARTESIAN_POINT('Ctrl Pts',(-2.52372474541954,-1.06847604194599,
2.97787241373934));
#43364=CARTESIAN_POINT('Ctrl Pts',(-2.49153128087079,-0.794772684001023,
3.02810219092903));
#43365=CARTESIAN_POINT('Ctrl Pts',(-2.47626833169421,-0.636309800095335,
3.09633903590505));
#43366=CARTESIAN_POINT('Ctrl Pts',(-2.46717038202176,-0.319434907277228,
3.17176849844764));
#43367=CARTESIAN_POINT('Ctrl Pts',(-2.46767312849726,-0.158333333333367,
3.21910192517114));
#43368=CARTESIAN_POINT('Ctrl Pts',(-2.49392386739101,0.158333333333369,
3.23549299195286));
#43369=CARTESIAN_POINT('Ctrl Pts',(-2.52048923570689,0.319434907277237,
3.20501930950502));
#43370=CARTESIAN_POINT('Ctrl Pts',(-2.58139311453956,0.636309800095345,
3.1620226074916));
#43371=CARTESIAN_POINT('Ctrl Pts',(-2.62481842336647,0.794772684001014,
3.1108597619245));
#43372=CARTESIAN_POINT('Ctrl Pts',(-2.69570834867789,1.06847604194579,3.08608229682891));
#43373=CARTESIAN_POINT('Ctrl Pts',(-2.72755502603203,1.18514270861292,3.08408474375722));
#43374=CARTESIAN_POINT('Ctrl Pts',(-2.76056275880354,1.3000000000016,3.09081488415818));
#43375=CARTESIAN_POINT('Ctrl Pts',(-2.56135590679036,-1.30000000000217,
2.95696190589203));
#43376=CARTESIAN_POINT('Ctrl Pts',(-2.54098096164571,-1.18514270861332,
2.958186745425));
#43377=CARTESIAN_POINT('Ctrl Pts',(-2.5238612674274,-1.068476041946,2.96939659408028));
#43378=CARTESIAN_POINT('Ctrl Pts',(-2.4918316298507,-0.794772684001025,
3.01836095556312));
#43379=CARTESIAN_POINT('Ctrl Pts',(-2.47673724160775,-0.636309800095336,
3.08688334195185));
#43380=CARTESIAN_POINT('Ctrl Pts',(-2.46795275175855,-0.319434907277229,
3.16239073869001));
#43381=CARTESIAN_POINT('Ctrl Pts',(-2.46873478549739,-0.158333333333367,
3.21024437564977));
#43382=CARTESIAN_POINT('Ctrl Pts',(-2.49514977379312,0.158333333333369,
3.2266994418965));
#43383=CARTESIAN_POINT('Ctrl Pts',(-2.52165728592964,0.319434907277237,
3.19579667183401));
#43384=CARTESIAN_POINT('Ctrl Pts',(-2.58246579417548,0.636309800095345,
3.15279715001001));
#43385=CARTESIAN_POINT('Ctrl Pts',(-2.62574992097367,0.794772684001014,
3.10133790237474));
#43386=CARTESIAN_POINT('Ctrl Pts',(-2.69649403174895,1.0684760419458,3.07782558277605));
#43387=CARTESIAN_POINT('Ctrl Pts',(-2.72828231736828,1.18514270861293,3.07671215017822));
#43388=CARTESIAN_POINT('Ctrl Pts',(-2.76123638437994,1.3000000000016,3.08466289691952));
#43389=CARTESIAN_POINT('Ctrl Pts',(-2.56131487123015,-1.30000000000217,
2.94897114298167));
#43390=CARTESIAN_POINT('Ctrl Pts',(-2.54081396862634,-1.18514270861332,
2.94860460594914));
#43391=CARTESIAN_POINT('Ctrl Pts',(-2.52367827482182,-1.068476041946,2.95867756677743));
#43392=CARTESIAN_POINT('Ctrl Pts',(-2.49186569968375,-0.794772684001026,
3.00606544985243));
#43393=CARTESIAN_POINT('Ctrl Pts',(-2.47737488468038,-0.636309800095337,
3.07508978567909));
#43394=CARTESIAN_POINT('Ctrl Pts',(-2.46900076333603,-0.319434907277229,
3.15069628767783));
#43395=CARTESIAN_POINT('Ctrl Pts',(-2.4697992228176,-0.158333333333367,
3.19906700330485));
#43396=CARTESIAN_POINT('Ctrl Pts',(-2.49641269429515,0.15833333333337,3.21559961047872));
#43397=CARTESIAN_POINT('Ctrl Pts',(-2.52305451573685,0.319434907277238,
3.18424456747001));
#43398=CARTESIAN_POINT('Ctrl Pts',(-2.58395421093877,0.636309800095347,
3.14132982636881));
#43399=CARTESIAN_POINT('Ctrl Pts',(-2.62729716662013,0.794772684001016,
3.0896021960587));
#43400=CARTESIAN_POINT('Ctrl Pts',(-2.69782820934637,1.0684760419458,3.06765706675948));
#43401=CARTESIAN_POINT('Ctrl Pts',(-2.72945689966399,1.18514270861293,3.06761092476609));
#43402=CARTESIAN_POINT('Ctrl Pts',(-2.76218400533566,1.3000000000016,3.07701787410579));
#43403=CARTESIAN_POINT('Ctrl Pts',(-2.56121597939136,-1.30000000000218,
2.94175952744392));
#43404=CARTESIAN_POINT('Ctrl Pts',(-2.5405367478716,-1.18514270861333,2.93993767742452));
#43405=CARTESIAN_POINT('Ctrl Pts',(-2.52334870506496,-1.06847604194601,
2.94897403450116));
#43406=CARTESIAN_POINT('Ctrl Pts',(-2.49170623206277,-0.794772684001033,
2.9949344576338));
#43407=CARTESIAN_POINT('Ctrl Pts',(-2.4778709967323,-0.636309800095342,
3.06445299246228));
#43408=CARTESIAN_POINT('Ctrl Pts',(-2.46986253282946,-0.319434907277232,
3.14014390285027));
#43409=CARTESIAN_POINT('Ctrl Pts',(-2.47058571822193,-0.158333333333368,
3.18894004954346));
#43410=CARTESIAN_POINT('Ctrl Pts',(-2.49736140057388,0.158333333333371,
3.20553401239655));
#43411=CARTESIAN_POINT('Ctrl Pts',(-2.52415581516235,0.31943490727724,3.17378572875201));
#43412=CARTESIAN_POINT('Ctrl Pts',(-2.5851931833126,0.636309800095352,3.13097096387433));
#43413=CARTESIAN_POINT('Ctrl Pts',(-2.62865750910726,0.794772684001022,
3.07903191620791));
#43414=CARTESIAN_POINT('Ctrl Pts',(-2.69903491426331,1.06847604194581,3.05851252393744));
#43415=CARTESIAN_POINT('Ctrl Pts',(-2.73052608489709,1.18514270861294,3.05942872360747));
#43416=CARTESIAN_POINT('Ctrl Pts',(-2.76304465521239,1.30000000000161,3.07014320754303));
#43417=CARTESIAN_POINT('Ctrl Pts',(-2.56122885626145,-1.30000000000218,
2.93698156749451));
#43418=CARTESIAN_POINT('Ctrl Pts',(-2.54051001622556,-1.18514270861333,
2.93421867273334));
#43419=CARTESIAN_POINT('Ctrl Pts',(-2.52331921064371,-1.06847604194601,
2.94257575738084));
#43420=CARTESIAN_POINT('Ctrl Pts',(-2.49175547611056,-0.794772684001034,
2.9875716717238));
#43421=CARTESIAN_POINT('Ctrl Pts',(-2.47808947499982,-0.636309800095343,
3.057320333101));
#43422=CARTESIAN_POINT('Ctrl Pts',(-2.47029675512753,-0.319434907277232,
3.13305829083749));
#43423=CARTESIAN_POINT('Ctrl Pts',(-2.47118148600144,-0.158333333333369,
3.18221951764537));
#43424=CARTESIAN_POINT('Ctrl Pts',(-2.49806846737449,0.158333333333371,
3.19885423538708));
#43425=CARTESIAN_POINT('Ctrl Pts',(-2.52483193154344,0.319434907277241,
3.16679107533292));
#43426=CARTESIAN_POINT('Ctrl Pts',(-2.58584095910954,0.636309800095353,
3.12399303132165));
#43427=CARTESIAN_POINT('Ctrl Pts',(-2.62924834691998,0.794772684001023,
3.07185364297797));
#43428=CARTESIAN_POINT('Ctrl Pts',(-2.69957568789046,1.06847604194581,3.05230697577233));
#43429=CARTESIAN_POINT('Ctrl Pts',(-2.73104801847194,1.18514270861294,3.05389572675833));
#43430=CARTESIAN_POINT('Ctrl Pts',(-2.76355057961355,1.30000000000162,3.06553425668826));
#43431=CARTESIAN_POINT('Ctrl Pts',(-2.56124558852298,-1.30000000000218,
2.93459651930118));
#43432=CARTESIAN_POINT('Ctrl Pts',(-2.54051875074545,-1.18514270861333,
2.93136751692711));
#43433=CARTESIAN_POINT('Ctrl Pts',(-2.52333126833281,-1.06847604194601,
2.93938673770933));
#43434=CARTESIAN_POINT('Ctrl Pts',(-2.49180136455417,-0.794772684001035,
2.98389838764611));
#43435=CARTESIAN_POINT('Ctrl Pts',(-2.4781799529861,-0.636309800095344,
3.05374721821014));
#43436=CARTESIAN_POINT('Ctrl Pts',(-2.47048954832231,-0.319434907277232,
3.12950674724737));
#43437=CARTESIAN_POINT('Ctrl Pts',(-2.47148414771184,-0.158333333333369,
3.17886164663329));
#43438=CARTESIAN_POINT('Ctrl Pts',(-2.49842744874293,0.158333333333371,
3.19551677007893));
#43439=CARTESIAN_POINT('Ctrl Pts',(-2.52515869307151,0.319434907277241,
3.16328952071116));
#43440=CARTESIAN_POINT('Ctrl Pts',(-2.58613667884508,0.636309800095353,
3.12049277631889));
#43441=CARTESIAN_POINT('Ctrl Pts',(-2.62949397568524,0.794772684001024,
3.06824394144028));
#43442=CARTESIAN_POINT('Ctrl Pts',(-2.69980382558699,1.06847604194581,3.04918675646232));
#43443=CARTESIAN_POINT('Ctrl Pts',(-2.73127752759753,1.18514270861294,3.05111631983744));
#43444=CARTESIAN_POINT('Ctrl Pts',(-2.76379040283277,1.30000000000162,3.06322459582634));
#43445=CARTESIAN_POINT('Ctrl Pts',(-2.56126911392072,-1.30000000000218,
2.93261264944325));
#43446=CARTESIAN_POINT('Ctrl Pts',(-2.5405458456593,-1.18514270861333,2.92899904773324));
#43447=CARTESIAN_POINT('Ctrl Pts',(-2.52336522141286,-1.06847604194601,
2.93673825224489));
#43448=CARTESIAN_POINT('Ctrl Pts',(-2.49185875880972,-0.794772684001035,
2.98084461638238));
#43449=CARTESIAN_POINT('Ctrl Pts',(-2.47823984512274,-0.636309800095344,
3.050764003082));
#43450=CARTESIAN_POINT('Ctrl Pts',(-2.47063003330241,-0.319434907277232,
3.12653989178922));
#43451=CARTESIAN_POINT('Ctrl Pts',(-2.47174166797301,-0.158333333333369,
3.17606598907416));
#43452=CARTESIAN_POINT('Ctrl Pts',(-2.49873241433156,0.158333333333371,
3.19273812989693));
#43453=CARTESIAN_POINT('Ctrl Pts',(-2.52542186010774,0.319434907277241,
3.1603681777678));
#43454=CARTESIAN_POINT('Ctrl Pts',(-2.5863592866705,0.636309800095354,3.11756635750561));
#43455=CARTESIAN_POINT('Ctrl Pts',(-2.62965670193438,0.794772684001024,
3.06521852198832));
#43456=CARTESIAN_POINT('Ctrl Pts',(-2.69995809385392,1.06847604194581,3.04657175301279));
#43457=CARTESIAN_POINT('Ctrl Pts',(-2.73144190887693,1.18514270861294,3.04878909121335));
#43458=CARTESIAN_POINT('Ctrl Pts',(-2.76397867128422,1.30000000000162,3.06129526297312));
#43459=CARTESIAN_POINT('Ctrl Pts',(-2.5612881662613,-1.30000000000218,2.93122497760151));
#43460=CARTESIAN_POINT('Ctrl Pts',(-2.54057050258479,-1.18514270861333,
2.92734335101429));
#43461=CARTESIAN_POINT('Ctrl Pts',(-2.52339581008036,-1.06847604194601,
2.93488699092271));
#43462=CARTESIAN_POINT('Ctrl Pts',(-2.49190380678617,-0.794772684001035,
2.97870895943272));
#43463=CARTESIAN_POINT('Ctrl Pts',(-2.47827575857435,-0.636309800095344,
3.04867365985667));
#43464=CARTESIAN_POINT('Ctrl Pts',(-2.47071941768915,-0.319434907277232,
3.12445989077146));
#43465=CARTESIAN_POINT('Ctrl Pts',(-2.47191831288654,-0.158333333333369,
3.17410783091974));
#43466=CARTESIAN_POINT('Ctrl Pts',(-2.49894254244825,0.158333333333371,
3.19079190973));
#43467=CARTESIAN_POINT('Ctrl Pts',(-2.52560116743548,0.319434907277241,
3.15832142852038));
#43468=CARTESIAN_POINT('Ctrl Pts',(-2.58650656512886,0.636309800095354,
3.11551448505154));
#43469=CARTESIAN_POINT('Ctrl Pts',(-2.62975530020764,0.794772684001024,
3.06309450093283));
#43470=CARTESIAN_POINT('Ctrl Pts',(-2.70005209913077,1.06847604194581,3.04473548722388));
#43471=CARTESIAN_POINT('Ctrl Pts',(-2.73154553314448,1.18514270861294,3.04715527914781));
#43472=CARTESIAN_POINT('Ctrl Pts',(-2.76410352167112,1.30000000000162,3.05994179976178));
#43473=CARTESIAN_POINT('Ctrl Pts',(-2.56129985436376,-1.30000000000218,
2.93043234734907));
#43474=CARTESIAN_POINT('Ctrl Pts',(-2.54058590945191,-1.18514270861333,
2.92639775725202));
#43475=CARTESIAN_POINT('Ctrl Pts',(-2.52341477430191,-1.06847604194601,
2.93382970795896));
#43476=CARTESIAN_POINT('Ctrl Pts',(-2.49193061631822,-0.794772684001036,
2.97748900397935));
#43477=CARTESIAN_POINT('Ctrl Pts',(-2.47829498062337,-0.636309800095344,
3.04747869460039));
#43478=CARTESIAN_POINT('Ctrl Pts',(-2.47076939216646,-0.319434907277233,
3.12327092089488));
#43479=CARTESIAN_POINT('Ctrl Pts',(-2.47202102417737,-0.158333333333369,
3.17298960622546));
#43480=CARTESIAN_POINT('Ctrl Pts',(-2.49906424625836,0.158333333333371,
3.18968044522044));
#43481=CARTESIAN_POINT('Ctrl Pts',(-2.52570272600367,0.319434907277241,
3.1571515288977));
#43482=CARTESIAN_POINT('Ctrl Pts',(-2.58658835737259,0.636309800095354,
3.11434105534365));
#43483=CARTESIAN_POINT('Ctrl Pts',(-2.62980856665228,0.794772684001024,
3.06187948966555));
#43484=CARTESIAN_POINT('Ctrl Pts',(-2.70010357285852,1.06847604194581,3.04368526313072));
#43485=CARTESIAN_POINT('Ctrl Pts',(-2.73160332904789,1.18514270861294,3.04622110339926));
#43486=CARTESIAN_POINT('Ctrl Pts',(-2.76417473792659,1.30000000000162,3.05916839044075));
#43487=CARTESIAN_POINT('Ctrl Pts',(-2.56149026715371,-1.30000000000216,
2.91735327145688));
#43488=CARTESIAN_POINT('Ctrl Pts',(-2.54084897406474,-1.18514270861331,
2.91079953441578));
#43489=CARTESIAN_POINT('Ctrl Pts',(-2.52374038681034,-1.06847604194599,
2.91639044658124));
#43490=CARTESIAN_POINT('Ctrl Pts',(-2.49237738488491,-0.794772684001022,
2.95736314133742));
#43491=CARTESIAN_POINT('Ctrl Pts',(-2.47858976511407,-0.636309800095333,
3.0277554918797));
#43492=CARTESIAN_POINT('Ctrl Pts',(-2.47153047171005,-0.319434907277227,
3.10363055568692));
#43493=CARTESIAN_POINT('Ctrl Pts',(-2.47359874066084,-0.158333333333366,
3.15449480879278));
#43494=CARTESIAN_POINT('Ctrl Pts',(-2.50096233759851,0.158333333333368,
3.17129923809903));
#43495=CARTESIAN_POINT('Ctrl Pts',(-2.52734748101025,0.319434907277235,
3.13783675396691));
#43496=CARTESIAN_POINT('Ctrl Pts',(-2.5879245755808,0.636309800095342,3.09497436480464));
#43497=CARTESIAN_POINT('Ctrl Pts',(-2.63063176748115,0.794772684001011,
3.04181088542121));
#43498=CARTESIAN_POINT('Ctrl Pts',(-2.70087971632417,1.06847604194579,3.02632671178359));
#43499=CARTESIAN_POINT('Ctrl Pts',(-2.73247885494392,1.18514270861292,3.03077395956638));
#43500=CARTESIAN_POINT('Ctrl Pts',(-2.76526939807227,1.30000000000159,3.04637098015453));
#43501=CARTESIAN_POINT('Ctrl Pts',(-2.56087008524915,-1.30000000000202,
2.89145016916653));
#43502=CARTESIAN_POINT('Ctrl Pts',(-2.53960255952203,-1.18514270861318,
2.87970907731183));
#43503=CARTESIAN_POINT('Ctrl Pts',(-2.52223142494676,-1.06847604194587,
2.88157206655941));
#43504=CARTESIAN_POINT('Ctrl Pts',(-2.49110207202559,-0.794772684000928,
2.91730409324431));
#43505=CARTESIAN_POINT('Ctrl Pts',(-2.4787850160475,-0.636309800095263,
2.9891211391137));
#43506=CARTESIAN_POINT('Ctrl Pts',(-2.47303673739557,-0.319434907277193,
3.06528465111095));
#43507=CARTESIAN_POINT('Ctrl Pts',(-2.4758155227965,-0.158333333333348,
3.11803020288129));
#43508=CARTESIAN_POINT('Ctrl Pts',(-2.50383353435718,0.158333333333351,
3.13506318529158));
#43509=CARTESIAN_POINT('Ctrl Pts',(-2.52987163915752,0.319434907277197,
3.09984011298672));
#43510=CARTESIAN_POINT('Ctrl Pts',(-2.59106333172505,0.63630980009527,3.05737448948734));
#43511=CARTESIAN_POINT('Ctrl Pts',(-2.63544492476371,0.794772684000922,
3.00395850467053));
#43512=CARTESIAN_POINT('Ctrl Pts',(-2.70502550336271,1.06847604194568,2.99349161372486));
#43513=CARTESIAN_POINT('Ctrl Pts',(-2.73580288446904,1.18514270861279,3.00122553922847));
#43514=CARTESIAN_POINT('Ctrl Pts',(-2.76723879242068,1.30000000000146,3.02122411948956));
#43515=CARTESIAN_POINT('Ctrl Pts',(-2.56068515941495,-1.30000000000188,
2.86595196820463));
#43516=CARTESIAN_POINT('Ctrl Pts',(-2.53896378271869,-1.18514270861306,
2.84914234896317));
#43517=CARTESIAN_POINT('Ctrl Pts',(-2.52138535408007,-1.06847604194576,
2.8473371052107));
#43518=CARTESIAN_POINT('Ctrl Pts',(-2.49034670617944,-0.794772684000851,
2.87782973999923));
#43519=CARTESIAN_POINT('Ctrl Pts',(-2.47896213176933,-0.636309800095197,
2.95085588585943));
#43520=CARTESIAN_POINT('Ctrl Pts',(-2.47407845732068,-0.319434907277159,
3.02713594692395));
#43521=CARTESIAN_POINT('Ctrl Pts',(-2.47730282393709,-0.158333333333332,
3.08164150312981));
#43522=CARTESIAN_POINT('Ctrl Pts',(-2.50593474386354,0.158333333333335,
3.09888219729377));
#43523=CARTESIAN_POINT('Ctrl Pts',(-2.5325634168507,0.319434907277167,3.06228370370256));
#43524=CARTESIAN_POINT('Ctrl Pts',(-2.59328091776413,0.636309800095207,
3.01976435072494));
#43525=CARTESIAN_POINT('Ctrl Pts',(-2.63558849376141,0.79477268400084,2.96455750976156));
#43526=CARTESIAN_POINT('Ctrl Pts',(-2.70539049701901,1.06847604194556,2.95946258502623));
#43527=CARTESIAN_POINT('Ctrl Pts',(-2.73676209961397,1.18514270861267,2.97105808535257));
#43528=CARTESIAN_POINT('Ctrl Pts',(-2.76929060401276,1.30000000000132,2.99645449013761));
#43529=CARTESIAN_POINT('Ctrl Pts',(-2.56007871299464,-1.30000000000188,
2.85301515320661));
#43530=CARTESIAN_POINT('Ctrl Pts',(-2.53830479690512,-1.18514270861306,
2.83374468235308));
#43531=CARTESIAN_POINT('Ctrl Pts',(-2.52071187691441,-1.06847604194576,
2.83014510068077));
#43532=CARTESIAN_POINT('Ctrl Pts',(-2.48972764967806,-0.794772684000851,
2.85803223588308));
#43533=CARTESIAN_POINT('Ctrl Pts',(-2.47833749752908,-0.636309800095197,
2.93149143136161));
#43534=CARTESIAN_POINT('Ctrl Pts',(-2.47397094455174,-0.319434907277159,
3.00785804372322));
#43535=CARTESIAN_POINT('Ctrl Pts',(-2.47794645705588,-0.158333333333332,
3.06342740196054));
#43536=CARTESIAN_POINT('Ctrl Pts',(-2.50702387179274,0.158333333333335,
3.08081746057002));
#43537=CARTESIAN_POINT('Ctrl Pts',(-2.53348691515876,0.319434907277167,
3.04335648601618));
#43538=CARTESIAN_POINT('Ctrl Pts',(-2.5943095218286,0.636309800095207,3.00094899446167));
#43539=CARTESIAN_POINT('Ctrl Pts',(-2.63684270751801,0.79477268400084,2.94536468398828));
#43540=CARTESIAN_POINT('Ctrl Pts',(-2.70652295950989,1.06847604194556,2.94283794041207));
#43541=CARTESIAN_POINT('Ctrl Pts',(-2.73776084593945,1.18514270861267,2.95617299979562));
#43542=CARTESIAN_POINT('Ctrl Pts',(-2.77007461961902,1.30000000000132,2.98393685223179));
#43543=CARTESIAN_POINT('',(-2.73381727423405,1.2,3.07341023227417));
#43544=CARTESIAN_POINT('Ctrl Pts',(-2.73381727423405,1.2,3.07341023227417));
#43545=CARTESIAN_POINT('Ctrl Pts',(-2.73580502907171,1.21681156976446,3.09489320825098));
#43546=CARTESIAN_POINT('Ctrl Pts',(-2.73871695256444,1.23323051929576,3.11658988393981));
#43547=CARTESIAN_POINT('Ctrl Pts',(-2.74231883146871,1.26415219681706,3.15632227320206));
#43548=CARTESIAN_POINT('Ctrl Pts',(-2.74473649442256,1.28359571150105,3.18148300895735));
#43549=CARTESIAN_POINT('Ctrl Pts',(-2.74608525934289,1.30000000000146,3.2023111991545));
#43550=CARTESIAN_POINT('',(-2.60194865074143,0.653834841416716,2.98901873446979));
#43551=CARTESIAN_POINT('Ctrl Pts',(-2.60194865075745,0.65383484141603,2.989018734449));
#43552=CARTESIAN_POINT('Ctrl Pts',(-2.61579853831374,0.71799825259359,2.99757652513191));
#43553=CARTESIAN_POINT('Ctrl Pts',(-2.62696193981467,0.76351236162102,3.00454348125093));
#43554=CARTESIAN_POINT('Ctrl Pts',(-2.67092267687889,0.949774304316204,
3.03227820052749));
#43555=CARTESIAN_POINT('Ctrl Pts',(-2.69392872614227,1.04621155459823,3.04698453746189));
#43556=CARTESIAN_POINT('Ctrl Pts',(-2.73381727423405,1.2,3.07341023227417));
#43557=CARTESIAN_POINT('',(-2.48224831221779,-0.653834841531101,2.91736724473229));
#43558=CARTESIAN_POINT('Ctrl Pts',(-2.48224831221779,-0.653834841531099,
2.91736724473229));
#43559=CARTESIAN_POINT('Ctrl Pts',(-2.4784792853279,-0.575798967915911,
2.958866742215));
#43560=CARTESIAN_POINT('Ctrl Pts',(-2.47600965983172,-0.493921361947821,
2.99371556393921));
#43561=CARTESIAN_POINT('Ctrl Pts',(-2.47496436360723,-0.338198104431773,
3.04440076767245));
#43562=CARTESIAN_POINT('Ctrl Pts',(-2.47585304481096,-0.265712087248226,
3.06229123000691));
#43563=CARTESIAN_POINT('Ctrl Pts',(-2.48131735719936,-0.129742360743047,
3.08607972132565));
#43564=CARTESIAN_POINT('Ctrl Pts',(-2.48531283701423,-0.0666417585396564,
3.09333573958426));
#43565=CARTESIAN_POINT('Ctrl Pts',(-2.49656567467154,0.0595518523103038,
3.10050515929398));
#43566=CARTESIAN_POINT('Ctrl Pts',(-2.5038994701171,0.122798807524931,3.10048726948258));
#43567=CARTESIAN_POINT('Ctrl Pts',(-2.52282835424652,0.260150875487055,
3.09199370964883));
#43568=CARTESIAN_POINT('Ctrl Pts',(-2.53495970880385,0.333952437389984,
3.08197833173551));
#43569=CARTESIAN_POINT('Ctrl Pts',(-2.56433395610792,0.49123816976692,3.04808238203451));
#43570=CARTESIAN_POINT('Ctrl Pts',(-2.58224470446943,0.574172359428836,
3.02219716120638));
#43571=CARTESIAN_POINT('Ctrl Pts',(-2.6019486507569,0.653834841428434,2.98901873450711));
#43572=CARTESIAN_POINT('',(-2.54441412395572,-1.2,2.9540069752984));
#43573=CARTESIAN_POINT('Ctrl Pts',(-2.54441412395572,-1.2,2.9540069752984));
#43574=CARTESIAN_POINT('Ctrl Pts',(-2.53391960792159,-1.13536848923257,
2.94771812963474));
#43575=CARTESIAN_POINT('Ctrl Pts',(-2.51976513845017,-1.03917846089085,
2.93929182203061));
#43576=CARTESIAN_POINT('Ctrl Pts',(-2.49231083191816,-0.795650855253786,
2.92319530513295));
#43577=CARTESIAN_POINT('Ctrl Pts',(-2.4879173222092,-0.741453969039744,
2.92065304841597));
#43578=CARTESIAN_POINT('Ctrl Pts',(-2.48224831221779,-0.653834841531101,
2.91736724473229));
#43579=CARTESIAN_POINT('Ctrl Pts',(-2.5566292407628,-1.30000000000004,3.07857464882885));
#43580=CARTESIAN_POINT('Ctrl Pts',(-2.55515567833128,-1.2829468561125,3.05759280558607));
#43581=CARTESIAN_POINT('Ctrl Pts',(-2.55296732838268,-1.26611601653633,
3.03648706140119));
#43582=CARTESIAN_POINT('Ctrl Pts',(-2.54981115104406,-1.23888922084291,
3.00267573436432));
#43583=CARTESIAN_POINT('Ctrl Pts',(-2.54792518421048,-1.21938151191995,
2.97870604444334));
#43584=CARTESIAN_POINT('Ctrl Pts',(-2.54441412395572,-1.2,2.9540069752984));
#43585=CARTESIAN_POINT('Origin',(0.,1.25,7.2));
#43586=CARTESIAN_POINT('Origin',(0.,1.2,7.2));
#43587=CARTESIAN_POINT('Origin',(0.,0.92691742076555,7.2));
#43588=CARTESIAN_POINT('Origin',(0.,0.653834841531101,7.2));
#43589=CARTESIAN_POINT('Origin',(0.,0.,7.2));
#43590=CARTESIAN_POINT('Origin',(0.,-0.653834841531101,7.2));
#43591=CARTESIAN_POINT('Origin',(0.,-0.926917420765551,7.2));
#43592=CARTESIAN_POINT('Origin',(0.,-1.2,7.2));
#43593=CARTESIAN_POINT('Origin',(0.,-1.25,7.2));
#43594=CARTESIAN_POINT('Ctrl Pts',(-2.26618048011826,-1.30000000000181,
2.69301343514311));
#43595=CARTESIAN_POINT('Ctrl Pts',(-2.3063815684754,-1.18514270861301,2.70711605782214));
#43596=CARTESIAN_POINT('Ctrl Pts',(-2.33354901187764,-1.06847604194574,
2.72750133133817));
#43597=CARTESIAN_POINT('Ctrl Pts',(-2.36620091374758,-0.794772684000851,
2.78910957149348));
#43598=CARTESIAN_POINT('Ctrl Pts',(-2.33933008166882,-0.636309800095197,
2.85373654604466));
#43599=CARTESIAN_POINT('Ctrl Pts',(-2.33301542000619,-0.319434907277159,
2.92761421432354));
#43600=CARTESIAN_POINT('Ctrl Pts',(-2.31380478607559,-0.158333333333332,
2.96926236941578));
#43601=CARTESIAN_POINT('Ctrl Pts',(-2.34340372597314,0.158333333333334,
2.98574911994944));
#43602=CARTESIAN_POINT('Ctrl Pts',(-2.3935159581309,0.319434907277167,2.96140733565195));
#43603=CARTESIAN_POINT('Ctrl Pts',(-2.45746810794752,0.636309800095206,
2.91944248366745));
#43604=CARTESIAN_POINT('Ctrl Pts',(-2.51539056129684,0.79477268400084,2.87284872481844));
#43605=CARTESIAN_POINT('Ctrl Pts',(-2.52404941520302,1.06847604194579,2.83207202931349));
#43606=CARTESIAN_POINT('Ctrl Pts',(-2.51213562603719,1.18514270861311,2.81863590450963));
#43607=CARTESIAN_POINT('Ctrl Pts',(-2.4845599506917,1.30000000000198,2.80941437546059));
#43608=CARTESIAN_POINT('Ctrl Pts',(-2.25573189552084,-1.30000000000181,
2.69995123148277));
#43609=CARTESIAN_POINT('Ctrl Pts',(-2.2939900794401,-1.185142708613,2.71542354022312));
#43610=CARTESIAN_POINT('Ctrl Pts',(-2.31971787859578,-1.06847604194573,
2.73679439485206));
#43611=CARTESIAN_POINT('Ctrl Pts',(-2.35020654597518,-0.794772684000847,
2.79979216527225));
#43612=CARTESIAN_POINT('Ctrl Pts',(-2.32354980721586,-0.636309800095194,
2.86403502138493));
#43613=CARTESIAN_POINT('Ctrl Pts',(-2.31708571783413,-0.319434907277157,
2.93787759613429));
#43614=CARTESIAN_POINT('Ctrl Pts',(-2.2987048291419,-0.158333333333332,
2.9792379501954));
#43615=CARTESIAN_POINT('Ctrl Pts',(-2.32795166822999,0.158333333333334,
2.99541357312894));
#43616=CARTESIAN_POINT('Ctrl Pts',(-2.37676704786357,0.319434907277166,
2.97095317842074));
#43617=CARTESIAN_POINT('Ctrl Pts',(-2.44038568131416,0.636309800095204,
2.92858376177118));
#43618=CARTESIAN_POINT('Ctrl Pts',(-2.49793589154108,0.794772684000836,
2.88221135823736));
#43619=CARTESIAN_POINT('Ctrl Pts',(-2.50882396394661,1.06847604194578,2.84008478326095));
#43620=CARTESIAN_POINT('Ctrl Pts',(-2.49847136268352,1.18514270861311,2.82576403936588));
#43621=CARTESIAN_POINT('Ctrl Pts',(-2.47305311705583,1.30000000000198,2.81535758493964));
#43622=CARTESIAN_POINT('Ctrl Pts',(-2.24023758932582,-1.30000000000177,
2.71044742385437));
#43623=CARTESIAN_POINT('Ctrl Pts',(-2.27464917943828,-1.18514270861297,
2.72728042721628));
#43624=CARTESIAN_POINT('Ctrl Pts',(-2.29769987754193,-1.06847604194571,
2.74975004762311));
#43625=CARTESIAN_POINT('Ctrl Pts',(-2.32470566815866,-0.794772684000827,
2.81468107877005));
#43626=CARTESIAN_POINT('Ctrl Pts',(-2.30007955902539,-0.636309800095177,
2.87967363864554));
#43627=CARTESIAN_POINT('Ctrl Pts',(-2.29369713320137,-0.319434907277148,
2.95370134444852));
#43628=CARTESIAN_POINT('Ctrl Pts',(-2.27561853252957,-0.158333333333327,
2.99387261037791));
#43629=CARTESIAN_POINT('Ctrl Pts',(-2.30447284024276,0.158333333333329,
3.00970660738443));
#43630=CARTESIAN_POINT('Ctrl Pts',(-2.35230439668206,0.319434907277157,
2.98587434975564));
#43631=CARTESIAN_POINT('Ctrl Pts',(-2.41563048835693,0.636309800095186,
2.94307068412525));
#43632=CARTESIAN_POINT('Ctrl Pts',(-2.47192554671346,0.794772684000815,
2.89644828076972));
#43633=CARTESIAN_POINT('Ctrl Pts',(-2.48619431364992,1.06847604194576,2.85230756492692));
#43634=CARTESIAN_POINT('Ctrl Pts',(-2.47832233997716,1.18514270861308,2.83676282415757));
#43635=CARTESIAN_POINT('Ctrl Pts',(-2.45640197213473,1.30000000000194,2.82478022293255));
#43636=CARTESIAN_POINT('Ctrl Pts',(-2.22015396647836,-1.30000000000176,
2.72496915303494));
#43637=CARTESIAN_POINT('Ctrl Pts',(-2.25087006485636,-1.18514270861296,
2.74472365449367));
#43638=CARTESIAN_POINT('Ctrl Pts',(-2.27113584128439,-1.06847604194569,
2.76926324165332));
#43639=CARTESIAN_POINT('Ctrl Pts',(-2.29381150470358,-0.794772684000816,
2.83700910234178));
#43640=CARTESIAN_POINT('Ctrl Pts',(-2.26906479704234,-0.636309800095173,
2.90079934686356));
#43641=CARTESIAN_POINT('Ctrl Pts',(-2.26248272481726,-0.319434907277148,
2.97484635426529));
#43642=CARTESIAN_POINT('Ctrl Pts',(-2.24666840933008,-0.158333333333326,
3.01490679633203));
#43643=CARTESIAN_POINT('Ctrl Pts',(-2.27501627587942,0.158333333333328,
3.03030387788487));
#43644=CARTESIAN_POINT('Ctrl Pts',(-2.32020441102578,0.319434907277153,
3.00625628639059));
#43645=CARTESIAN_POINT('Ctrl Pts',(-2.38243925368409,0.63630980009518,2.96231774832919));
#43646=CARTESIAN_POINT('Ctrl Pts',(-2.43709121076443,0.794772684000812,
2.91538998751791));
#43647=CARTESIAN_POINT('Ctrl Pts',(-2.45575844588796,1.06847604194575,2.86846020459651));
#43648=CARTESIAN_POINT('Ctrl Pts',(-2.4511861078754,1.18514270861307,2.85126535631407));
#43649=CARTESIAN_POINT('Ctrl Pts',(-2.43396107745452,1.30000000000192,2.83718982385607));
#43650=CARTESIAN_POINT('Ctrl Pts',(-2.20918327510351,-1.30000000000174,
2.73201602488139));
#43651=CARTESIAN_POINT('Ctrl Pts',(-2.23786695827226,-1.18514270861294,
2.75316866377135));
#43652=CARTESIAN_POINT('Ctrl Pts',(-2.25666445064859,-1.06847604194567,
2.77874389990702));
#43653=CARTESIAN_POINT('Ctrl Pts',(-2.27725134000709,-0.794772684000803,
2.84804489606377));
#43654=CARTESIAN_POINT('Ctrl Pts',(-2.25314430197671,-0.63630980009516,
2.91177053549845));
#43655=CARTESIAN_POINT('Ctrl Pts',(-2.24635850625787,-0.319434907277141,
2.98574247512785));
#43656=CARTESIAN_POINT('Ctrl Pts',(-2.23079433029514,-0.158333333333323,
3.02501430692331));
#43657=CARTESIAN_POINT('Ctrl Pts',(-2.25886970073135,0.158333333333325,
3.04017865402025));
#43658=CARTESIAN_POINT('Ctrl Pts',(-2.30343128907705,0.319434907277148,
3.01660940791817));
#43659=CARTESIAN_POINT('Ctrl Pts',(-2.36552645982439,0.636309800095169,
2.97242979818955));
#43660=CARTESIAN_POINT('Ctrl Pts',(-2.4194102278767,0.794772684000795,2.92542134923293));
#43661=CARTESIAN_POINT('Ctrl Pts',(-2.44036738855896,1.06847604194573,2.8770660452405));
#43662=CARTESIAN_POINT('Ctrl Pts',(-2.43745361027784,1.18514270861305,2.85897966453637));
#43663=CARTESIAN_POINT('Ctrl Pts',(-2.42255447539554,1.3000000000019,2.8437381224859));
#43664=CARTESIAN_POINT('Ctrl Pts',(-2.20346973531821,-1.30000000000173,
2.73604655795091));
#43665=CARTESIAN_POINT('Ctrl Pts',(-2.23082832504476,-1.18514270861294,
2.7578092215297));
#43666=CARTESIAN_POINT('Ctrl Pts',(-2.24868608239779,-1.06847604194567,
2.78385225923261));
#43667=CARTESIAN_POINT('Ctrl Pts',(-2.26799225089751,-0.794772684000801,
2.85390540673059));
#43668=CARTESIAN_POINT('Ctrl Pts',(-2.24435183302002,-0.636309800095158,
2.91767688584819));
#43669=CARTESIAN_POINT('Ctrl Pts',(-2.2376941901163,-0.31943490727714,2.99179590928583));
#43670=CARTESIAN_POINT('Ctrl Pts',(-2.22268877944014,-0.158333333333323,
3.0309717544654));
#43671=CARTESIAN_POINT('Ctrl Pts',(-2.25062408390699,0.158333333333325,
3.046016730154));
#43672=CARTESIAN_POINT('Ctrl Pts',(-2.29437339664253,0.319434907277148,
3.02233571445109));
#43673=CARTESIAN_POINT('Ctrl Pts',(-2.35628618826155,0.636309800095168,
2.97794590344119));
#43674=CARTESIAN_POINT('Ctrl Pts',(-2.41003977131771,0.794772684000792,
2.9311343199028));
#43675=CARTESIAN_POINT('Ctrl Pts',(-2.43223231681768,1.06847604194572,2.88198830670547));
#43676=CARTESIAN_POINT('Ctrl Pts',(-2.43016869531126,1.18514270861304,2.8633680524723));
#43677=CARTESIAN_POINT('Ctrl Pts',(-2.41643512166632,1.3000000000019,2.84740103207989));
#43678=CARTESIAN_POINT('Ctrl Pts',(-2.20220161285603,-1.30000000000173,
2.736943664336));
#43679=CARTESIAN_POINT('Ctrl Pts',(-2.22927156689297,-1.18514270861294,
2.75884624111174));
#43680=CARTESIAN_POINT('Ctrl Pts',(-2.24692402372033,-1.06847604194567,
2.78499587321189));
#43681=CARTESIAN_POINT('Ctrl Pts',(-2.26594842783543,-0.794772684000802,
2.85521830199896));
#43682=CARTESIAN_POINT('Ctrl Pts',(-2.2424061778417,-0.636309800095159,
2.91899593966009));
#43683=CARTESIAN_POINT('Ctrl Pts',(-2.23577092804783,-0.31943490727714,
2.99314298560829));
#43684=CARTESIAN_POINT('Ctrl Pts',(-2.22088144654913,-0.158333333333323,
3.03229096841701));
#43685=CARTESIAN_POINT('Ctrl Pts',(-2.24878591432589,0.158333333333325,
3.04730973287704));
#43686=CARTESIAN_POINT('Ctrl Pts',(-2.29236670423403,0.319434907277148,
3.02361353216002));
#43687=CARTESIAN_POINT('Ctrl Pts',(-2.35423860798645,0.636309800095168,
2.97917660229254));
#43688=CARTESIAN_POINT('Ctrl Pts',(-2.40795028438503,0.794772684000792,
2.93239806134971));
#43689=CARTESIAN_POINT('Ctrl Pts',(-2.43041593543582,1.06847604194572,2.88307512146419));
#43690=CARTESIAN_POINT('Ctrl Pts',(-2.42854286265926,1.18514270861304,2.86433755511563));
#43691=CARTESIAN_POINT('Ctrl Pts',(-2.41507216920065,1.3000000000019,2.84821249549997));
#43692=CARTESIAN_POINT('Ctrl Pts',(-2.19999465780069,-1.30000000000173,
2.73852275171296));
#43693=CARTESIAN_POINT('Ctrl Pts',(-2.2265649885852,-1.18514270861294,2.76067455593726));
#43694=CARTESIAN_POINT('Ctrl Pts',(-2.24386117344665,-1.06847604194567,
2.78701316951011));
#43695=CARTESIAN_POINT('Ctrl Pts',(-2.2623936881977,-0.794772684000802,
2.85753300304829));
#43696=CARTESIAN_POINT('Ctrl Pts',(-2.2390139300092,-0.636309800095159,
2.92131431647447));
#43697=CARTESIAN_POINT('Ctrl Pts',(-2.23241366923983,-0.31943490727714,
2.99550733624859));
#43698=CARTESIAN_POINT('Ctrl Pts',(-2.21772704650828,-0.158333333333323,
3.03460660392587));
#43699=CARTESIAN_POINT('Ctrl Pts',(-2.24557742550624,0.158333333333325,
3.04957956852225));
#43700=CARTESIAN_POINT('Ctrl Pts',(-2.28886747707637,0.319434907277148,
3.02586029132576));
#43701=CARTESIAN_POINT('Ctrl Pts',(-2.35066304626681,0.636309800095168,
2.98133703992553));
#43702=CARTESIAN_POINT('Ctrl Pts',(-2.40428872280094,0.794772684000793,
2.93460592573491));
#43703=CARTESIAN_POINT('Ctrl Pts',(-2.42722935465882,1.06847604194573,2.88497087357005));
#43704=CARTESIAN_POINT('Ctrl Pts',(-2.425690744435,1.18514270861304,2.86602878533394));
#43705=CARTESIAN_POINT('Ctrl Pts',(-2.41268337449024,1.3000000000019,2.84962978378401));
#43706=CARTESIAN_POINT('Ctrl Pts',(-2.19687172842388,-1.30000000000173,
2.74080211112429));
#43707=CARTESIAN_POINT('Ctrl Pts',(-2.22276863898883,-1.18514270861294,
2.76334050676099));
#43708=CARTESIAN_POINT('Ctrl Pts',(-2.23957943286202,-1.06847604194567,
2.78996699298122));
#43709=CARTESIAN_POINT('Ctrl Pts',(-2.25742498246745,-0.794772684000802,
2.86092380982778));
#43710=CARTESIAN_POINT('Ctrl Pts',(-2.23422822527225,-0.636309800095159,
2.92467365053622));
#43711=CARTESIAN_POINT('Ctrl Pts',(-2.22763998419137,-0.31943490727714,
2.99890348786697));
#43712=CARTESIAN_POINT('Ctrl Pts',(-2.21320683729874,-0.158333333333323,
3.03790452917699));
#43713=CARTESIAN_POINT('Ctrl Pts',(-2.24098092916929,0.158333333333325,
3.05281353014586));
#43714=CARTESIAN_POINT('Ctrl Pts',(-2.28391842045281,0.319434907277148,
3.02911205885407));
#43715=CARTESIAN_POINT('Ctrl Pts',(-2.34559301506903,0.636309800095169,
2.98445522198158));
#43716=CARTESIAN_POINT('Ctrl Pts',(-2.39900929438297,0.794772684000794,
2.93772042282925));
#43717=CARTESIAN_POINT('Ctrl Pts',(-2.42261750004445,1.06847604194573,2.88763026047032));
#43718=CARTESIAN_POINT('Ctrl Pts',(-2.4215675118097,1.18514270861305,2.86840485303774));
#43719=CARTESIAN_POINT('Ctrl Pts',(-2.40924841787956,1.3000000000019,2.85163621343437));
#43720=CARTESIAN_POINT('Ctrl Pts',(-2.19316744487638,-1.30000000000174,
2.74357227885489));
#43721=CARTESIAN_POINT('Ctrl Pts',(-2.21833012274304,-1.18514270861294,
2.7666303563685));
#43722=CARTESIAN_POINT('Ctrl Pts',(-2.23460232797405,-1.06847604194567,
2.79363545208276));
#43723=CARTESIAN_POINT('Ctrl Pts',(-2.25165560697981,-0.794772684000803,
2.86514102717516));
#43724=CARTESIAN_POINT('Ctrl Pts',(-2.22859618268033,-0.63630980009516,
2.92879166006676));
#43725=CARTESIAN_POINT('Ctrl Pts',(-2.22195206858178,-0.31943490727714,
3.00301196088743));
#43726=CARTESIAN_POINT('Ctrl Pts',(-2.2077469105008,-0.158333333333323,
3.04183500405772));
#43727=CARTESIAN_POINT('Ctrl Pts',(-2.23542982559815,0.158333333333325,
3.05666885096073));
#43728=CARTESIAN_POINT('Ctrl Pts',(-2.2780636700841,0.319434907277148,3.03308550913707));
#43729=CARTESIAN_POINT('Ctrl Pts',(-2.33957680654361,0.636309800095169,
2.98825399010626));
#43730=CARTESIAN_POINT('Ctrl Pts',(-2.39259171033951,0.794772684000794,
2.94139027310225));
#43731=CARTESIAN_POINT('Ctrl Pts',(-2.4169793379928,1.06847604194573,2.89073594490276));
#43732=CARTESIAN_POINT('Ctrl Pts',(-2.41653230162815,1.18514270861305,2.87118437238136));
#43733=CARTESIAN_POINT('Ctrl Pts',(-2.40508172853836,1.3000000000019,2.85400760908834));
#43734=CARTESIAN_POINT('Ctrl Pts',(-2.1882615792186,-1.30000000000174,2.74729347372498));
#43735=CARTESIAN_POINT('Ctrl Pts',(-2.21251194251739,-1.18514270861294,
2.77109483631768));
#43736=CARTESIAN_POINT('Ctrl Pts',(-2.22810677709066,-1.06847604194568,
2.79863555033522));
#43737=CARTESIAN_POINT('Ctrl Pts',(-2.24413796180227,-0.794772684000805,
2.87089875906258));
#43738=CARTESIAN_POINT('Ctrl Pts',(-2.22119516131167,-0.636309800095161,
2.93436736296658));
#43739=CARTESIAN_POINT('Ctrl Pts',(-2.21442134321395,-0.319434907277141,
3.00853253480121));
#43740=CARTESIAN_POINT('Ctrl Pts',(-2.20045776457667,-0.158333333333323,
3.04706852295238));
#43741=CARTESIAN_POINT('Ctrl Pts',(-2.22801848204205,0.158333333333325,
3.06180316130134));
#43742=CARTESIAN_POINT('Ctrl Pts',(-2.2703440691031,0.319434907277149,3.038456775792));
#43743=CARTESIAN_POINT('Ctrl Pts',(-2.33162491225292,0.63630980009517,2.99337827183899));
#43744=CARTESIAN_POINT('Ctrl Pts',(-2.38397630173446,0.794772684000795,
2.94623641534027));
#43745=CARTESIAN_POINT('Ctrl Pts',(-2.40938468889191,1.06847604194573,2.8948141664764));
#43746=CARTESIAN_POINT('Ctrl Pts',(-2.40975612978786,1.18514270861305,2.87483947628986));
#43747=CARTESIAN_POINT('Ctrl Pts',(-2.3995006622528,1.3000000000019,2.85714888206791));
#43748=CARTESIAN_POINT('Ctrl Pts',(-2.18212017945675,-1.30000000000174,
2.75194076206201));
#43749=CARTESIAN_POINT('Ctrl Pts',(-2.20522580669821,-1.18514270861294,
2.77666914190148));
#43750=CARTESIAN_POINT('Ctrl Pts',(-2.21997833269593,-1.06847604194568,
2.80488347370449));
#43751=CARTESIAN_POINT('Ctrl Pts',(-2.23476228407815,-0.794772684000806,
2.87811747082507));
#43752=CARTESIAN_POINT('Ctrl Pts',(-2.2120269831232,-0.636309800095161,
2.94140396771728));
#43753=CARTESIAN_POINT('Ctrl Pts',(-2.20512598857467,-0.319434907277141,
3.01552645780187));
#43754=CARTESIAN_POINT('Ctrl Pts',(-2.19146800850019,-0.158333333333323,
3.0537060746734));
#43755=CARTESIAN_POINT('Ctrl Pts',(-2.21885670803492,0.158333333333325,
3.06830343605117));
#43756=CARTESIAN_POINT('Ctrl Pts',(-2.26073620860078,0.319434907277149,
3.0452087803244));
#43757=CARTESIAN_POINT('Ctrl Pts',(-2.32172961572616,0.63630980009517,2.99982685870441));
#43758=CARTESIAN_POINT('Ctrl Pts',(-2.37334890728109,0.794772684000796,
2.95241607700585));
#43759=CARTESIAN_POINT('Ctrl Pts',(-2.40000587537004,1.06847604194573,2.90001138005715));
#43760=CARTESIAN_POINT('Ctrl Pts',(-2.40136335569043,1.18514270861305,2.87947725010413));
#43761=CARTESIAN_POINT('Ctrl Pts',(-2.3925395025835,1.30000000000191,2.86109304172183));
#43762=CARTESIAN_POINT('Ctrl Pts',(-2.17208212925898,-1.30000000000174,
2.75921618055832));
#43763=CARTESIAN_POINT('Ctrl Pts',(-2.19303494876364,-1.18514270861295,
2.78518939374164));
#43764=CARTESIAN_POINT('Ctrl Pts',(-2.20626192734724,-1.06847604194568,
2.8143499086739));
#43765=CARTESIAN_POINT('Ctrl Pts',(-2.21897065584651,-0.794772684000809,
2.88907983636582));
#43766=CARTESIAN_POINT('Ctrl Pts',(-2.19699313048707,-0.636309800095163,
2.95239100512114));
#43767=CARTESIAN_POINT('Ctrl Pts',(-2.1903252370132,-0.319434907277142,
3.02677694489908));
#43768=CARTESIAN_POINT('Ctrl Pts',(-2.17763876613698,-0.158333333333324,
3.06475897608085));
#43769=CARTESIAN_POINT('Ctrl Pts',(-2.2047633195661,0.158333333333326,3.0791437952662));
#43770=CARTESIAN_POINT('Ctrl Pts',(-2.24525338460493,0.319434907277149,
3.05592173076589));
#43771=CARTESIAN_POINT('Ctrl Pts',(-2.30578888329971,0.636309800095172,
3.01007248348909));
#43772=CARTESIAN_POINT('Ctrl Pts',(-2.35692263128715,0.794772684000799,
2.96280581578494));
#43773=CARTESIAN_POINT('Ctrl Pts',(-2.3856458783688,1.06847604194573,2.90888116363136));
#43774=CARTESIAN_POINT('Ctrl Pts',(-2.38849242500615,1.18514270861305,2.88737253804549));
#43775=CARTESIAN_POINT('Ctrl Pts',(-2.38175228892037,1.30000000000191,2.86769727068581));
#43776=CARTESIAN_POINT('Ctrl Pts',(-2.15949961246368,-1.30000000000175,
2.76829662997937));
#43777=CARTESIAN_POINT('Ctrl Pts',(-2.17777936667385,-1.18514270861295,
2.79584352702837));
#43778=CARTESIAN_POINT('Ctrl Pts',(-2.18909913156332,-1.06847604194569,
2.82618941541642));
#43779=CARTESIAN_POINT('Ctrl Pts',(-2.19917108529723,-0.794772684000813,
2.90276071819625));
#43780=CARTESIAN_POINT('Ctrl Pts',(-2.1780294378193,-0.636309800095167,
2.96601852987045));
#43781=CARTESIAN_POINT('Ctrl Pts',(-2.17159203546571,-0.319434907277144,
3.04068386847602));
#43782=CARTESIAN_POINT('Ctrl Pts',(-2.16007347128678,-0.158333333333325,
3.07837413098288));
#43783=CARTESIAN_POINT('Ctrl Pts',(-2.18697813276709,0.158333333333327,
3.09257702156199));
#43784=CARTESIAN_POINT('Ctrl Pts',(-2.22605377032027,0.319434907277152,
3.06945503396162));
#43785=CARTESIAN_POINT('Ctrl Pts',(-2.28596511485657,0.636309800095176,
3.02297569925729));
#43786=CARTESIAN_POINT('Ctrl Pts',(-2.33604912362317,0.794772684000802,
2.97552561301708));
#43787=CARTESIAN_POINT('Ctrl Pts',(-2.36723098225282,1.06847604194574,2.91960304856153));
#43788=CARTESIAN_POINT('Ctrl Pts',(-2.37194882244496,1.18514270861306,2.89688745512843));
#43789=CARTESIAN_POINT('Ctrl Pts',(-2.36788703163017,1.30000000000192,2.87566307427989));
#43790=CARTESIAN_POINT('Ctrl Pts',(-2.1400296612085,-1.30000000000177,2.78332408910354));
#43791=CARTESIAN_POINT('Ctrl Pts',(-2.15457256128359,-1.18514270861297,
2.81379802010596));
#43792=CARTESIAN_POINT('Ctrl Pts',(-2.16321725789178,-1.0684760419457,2.84632547071609));
#43793=CARTESIAN_POINT('Ctrl Pts',(-2.16956220648216,-0.794772684000821,
2.92621442981849));
#43794=CARTESIAN_POINT('Ctrl Pts',(-2.14972875993447,-0.636309800095173,
2.98935755509729));
#43795=CARTESIAN_POINT('Ctrl Pts',(-2.14315859529316,-0.319434907277147,
3.06409898165379));
#43796=CARTESIAN_POINT('Ctrl Pts',(-2.13261471316304,-0.158333333333326,
3.10066177827065));
#43797=CARTESIAN_POINT('Ctrl Pts',(-2.15855621259014,0.158333333333328,
3.11412656762498));
#43798=CARTESIAN_POINT('Ctrl Pts',(-2.19511681652783,0.319434907277155,
3.09096870395781));
#43799=CARTESIAN_POINT('Ctrl Pts',(-2.25437472507939,0.636309800095182,
3.04377600700554));
#43800=CARTESIAN_POINT('Ctrl Pts',(-2.3039528815301,0.79477268400081,2.99699282002359));
#43801=CARTESIAN_POINT('Ctrl Pts',(-2.33931845409527,1.06847604194575,2.9380534808914));
#43802=CARTESIAN_POINT('Ctrl Pts',(-2.34693156225004,1.18514270861307,2.91330860187064));
#43803=CARTESIAN_POINT('Ctrl Pts',(-2.34684933261967,1.30000000000193,2.88933149982177));
#43804=CARTESIAN_POINT('Ctrl Pts',(-2.12052229387443,-1.30000000000177,
2.79835037140423));
#43805=CARTESIAN_POINT('Ctrl Pts',(-2.13136849242446,-1.18514270861297,
2.83178169880633));
#43806=CARTESIAN_POINT('Ctrl Pts',(-2.13727436244986,-1.06847604194571,
2.86644568934175));
#43807=CARTESIAN_POINT('Ctrl Pts',(-2.13950495647254,-0.794772684000832,
2.94937414041727));
#43808=CARTESIAN_POINT('Ctrl Pts',(-2.12000342318202,-0.636309800095182,
3.01169593614363));
#43809=CARTESIAN_POINT('Ctrl Pts',(-2.11330403078325,-0.319434907277152,
3.08651916057855));
#43810=CARTESIAN_POINT('Ctrl Pts',(-2.10434476941678,-0.158333333333328,
3.12238322192707));
#43811=CARTESIAN_POINT('Ctrl Pts',(-2.13034146592244,0.158333333333331,
3.13588233349007));
#43812=CARTESIAN_POINT('Ctrl Pts',(-2.16577982275893,0.319434907277158,
3.11378008751628));
#43813=CARTESIAN_POINT('Ctrl Pts',(-2.22445000215898,0.63630980009519,3.0659184726177));
#43814=CARTESIAN_POINT('Ctrl Pts',(-2.27190223565677,0.794772684000822,
3.01853364691345));
#43815=CARTESIAN_POINT('Ctrl Pts',(-2.31094248435717,1.06847604194576,2.9561752512662));
#43816=CARTESIAN_POINT('Ctrl Pts',(-2.32142648933868,1.18514270861309,2.92938028086924));
#43817=CARTESIAN_POINT('Ctrl Pts',(-2.32549542222303,1.30000000000195,2.9027829789448));
#43818=CARTESIAN_POINT('Ctrl Pts',(-2.10347617539217,-1.30000000000177,
2.81152704880114));
#43819=CARTESIAN_POINT('Ctrl Pts',(-2.11086560738165,-1.18514270861298,
2.8474047904178));
#43820=CARTESIAN_POINT('Ctrl Pts',(-2.1144218880465,-1.06847604194571,2.88398421097988));
#43821=CARTESIAN_POINT('Ctrl Pts',(-2.1137822614346,-0.794772684000831,
2.97011100890035));
#43822=CARTESIAN_POINT('Ctrl Pts',(-2.0965574929,-0.636309800095182,3.03312580480178));
#43823=CARTESIAN_POINT('Ctrl Pts',(-2.09019094570269,-0.319434907277152,
3.10834249787361));
#43824=CARTESIAN_POINT('Ctrl Pts',(-2.08177200594073,-0.158333333333328,
3.14299917059874));
#43825=CARTESIAN_POINT('Ctrl Pts',(-2.10676491187636,0.158333333333331,
3.15576783442169));
#43826=CARTESIAN_POINT('Ctrl Pts',(-2.14013723911703,0.319434907277159,
3.13379548380685));
#43827=CARTESIAN_POINT('Ctrl Pts',(-2.19749303240763,0.636309800095191,
3.08475943756395));
#43828=CARTESIAN_POINT('Ctrl Pts',(-2.24307107389101,0.794772684000823,
3.03682872907093));
#43829=CARTESIAN_POINT('Ctrl Pts',(-2.28547810640088,1.06847604194576,2.97158445453326));
#43830=CARTESIAN_POINT('Ctrl Pts',(-2.29865486786559,1.18514270861309,2.94312676280035));
#43831=CARTESIAN_POINT('Ctrl Pts',(-2.30665195775685,1.30000000000195,2.91445320824332));
#43832=CARTESIAN_POINT('Ctrl Pts',(-2.09398294748795,-1.30000000000178,
2.8192464505879));
#43833=CARTESIAN_POINT('Ctrl Pts',(-2.09985007592462,-1.18514270861298,
2.85683927055206));
#43834=CARTESIAN_POINT('Ctrl Pts',(-2.10222809132688,-1.06847604194571,
2.89462699936486));
#43835=CARTESIAN_POINT('Ctrl Pts',(-2.09966123352232,-0.794772684000831,
2.98237449076318));
#43836=CARTESIAN_POINT('Ctrl Pts',(-2.08208718234733,-0.636309800095182,
3.04461861941498));
#43837=CARTESIAN_POINT('Ctrl Pts',(-2.07559300407143,-0.319434907277152,
3.11983369483043));
#43838=CARTESIAN_POINT('Ctrl Pts',(-2.06819301628649,-0.158333333333329,
3.15429316403017));
#43839=CARTESIAN_POINT('Ctrl Pts',(-2.09333845137421,0.158333333333331,
3.16717379427419));
#43840=CARTESIAN_POINT('Ctrl Pts',(-2.12609654828513,0.319434907277159,
3.14569509865548));
#43841=CARTESIAN_POINT('Ctrl Pts',(-2.18337696560044,0.636309800095192,
3.09651295484401));
#43842=CARTESIAN_POINT('Ctrl Pts',(-2.22838428511871,0.794772684000823,
3.04869857741907));
#43843=CARTESIAN_POINT('Ctrl Pts',(-2.27254192517896,1.06847604194577,2.9816729024378));
#43844=CARTESIAN_POINT('Ctrl Pts',(-2.28698030954534,1.18514270861309,2.95204360255291));
#43845=CARTESIAN_POINT('Ctrl Pts',(-2.2967428720978,1.30000000000195,2.92179793393659));
#43846=CARTESIAN_POINT('Ctrl Pts',(-2.07970877079305,-1.30000000000178,
2.8307951811348));
#43847=CARTESIAN_POINT('Ctrl Pts',(-2.08302898344803,-1.18514270861298,
2.87077956661394));
#43848=CARTESIAN_POINT('Ctrl Pts',(-2.0835761767988,-1.06847604194571,2.91033894438351));
#43849=CARTESIAN_POINT('Ctrl Pts',(-2.07843407357136,-0.794772684000834,
3.00074716802572));
#43850=CARTESIAN_POINT('Ctrl Pts',(-2.06151116195105,-0.636309800095184,
3.06266775736981));
#43851=CARTESIAN_POINT('Ctrl Pts',(-2.05524410150916,-0.319434907277153,
3.13817562028094));
#43852=CARTESIAN_POINT('Ctrl Pts',(-2.04939411901467,-0.158333333333329,
3.17235824501512));
#43853=CARTESIAN_POINT('Ctrl Pts',(-2.07382117261851,0.158333333333331,
3.18471694876148));
#43854=CARTESIAN_POINT('Ctrl Pts',(-2.10395999875305,0.31943490727716,3.1627504266277));
#43855=CARTESIAN_POINT('Ctrl Pts',(-2.16026473232455,0.636309800095193,
3.11270682165839));
#43856=CARTESIAN_POINT('Ctrl Pts',(-2.20487943480485,0.794772684000825,
3.06536588123936));
#43857=CARTESIAN_POINT('Ctrl Pts',(-2.25180834481438,1.06847604194577,2.99577491820494));
#43858=CARTESIAN_POINT('Ctrl Pts',(-2.268229373859,1.18514270861309,2.96446341176438));
#43859=CARTESIAN_POINT('Ctrl Pts',(-2.28075764569255,1.30000000000195,2.93196374818161));
#43860=CARTESIAN_POINT('Ctrl Pts',(-2.05852013350791,-1.30000000000178,
2.84828080309916));
#43861=CARTESIAN_POINT('Ctrl Pts',(-2.05770642325508,-1.18514270861298,
2.89165118560606));
#43862=CARTESIAN_POINT('Ctrl Pts',(-2.05536294566111,-1.06847604194572,
2.93377693261711));
#43863=CARTESIAN_POINT('Ctrl Pts',(-2.04641497502104,-0.794772684000837,
3.02822047845532));
#43864=CARTESIAN_POINT('Ctrl Pts',(-2.03146347072319,-0.636309800095184,
3.09031719439697));
#43865=CARTESIAN_POINT('Ctrl Pts',(-2.02542091010615,-0.319434907277152,
3.16617875754651));
#43866=CARTESIAN_POINT('Ctrl Pts',(-2.02041466212552,-0.158333333333329,
3.19890879492926));
#43867=CARTESIAN_POINT('Ctrl Pts',(-2.04436817801832,0.158333333333332,
3.21095252400229));
#43868=CARTESIAN_POINT('Ctrl Pts',(-2.07318118945325,0.319434907277163,
3.1901606890519));
#43869=CARTESIAN_POINT('Ctrl Pts',(-2.12831426138427,0.636309800095196,
3.13904628501572));
#43870=CARTESIAN_POINT('Ctrl Pts',(-2.17009567002426,0.794772684000824,
3.09077697976127));
#43871=CARTESIAN_POINT('Ctrl Pts',(-2.22069839553814,1.06847604194577,3.01697886521116));
#43872=CARTESIAN_POINT('Ctrl Pts',(-2.24018483798486,1.18514270861309,2.98320571956108));
#43873=CARTESIAN_POINT('Ctrl Pts',(-2.25725367801904,1.30000000000195,2.94760389756012));
#43874=CARTESIAN_POINT('Ctrl Pts',(-2.03123509006447,-1.30000000000179,
2.87227242206237));
#43875=CARTESIAN_POINT('Ctrl Pts',(-2.02551307888917,-1.18514270861299,
2.92058116074944));
#43876=CARTESIAN_POINT('Ctrl Pts',(-2.01962846565359,-1.06847604194572,
2.96635206631251));
#43877=CARTESIAN_POINT('Ctrl Pts',(-2.00565818857887,-0.79477268400084,
3.06622911239301));
#43878=CARTESIAN_POINT('Ctrl Pts',(-1.99181080380806,-0.636309800095189,
3.12752722261015));
#43879=CARTESIAN_POINT('Ctrl Pts',(-1.98623956884247,-0.319434907277156,
3.20398179778877));
#43880=CARTESIAN_POINT('Ctrl Pts',(-1.9840531135405,-0.15833333333333,3.23592205753177));
#43881=CARTESIAN_POINT('Ctrl Pts',(-2.00742959667819,0.158333333333333,
3.24758646395566));
#43882=CARTESIAN_POINT('Ctrl Pts',(-2.03277848779165,0.319434907277164,
3.22718563067376));
#43883=CARTESIAN_POINT('Ctrl Pts',(-2.08640193473761,0.6363098000952,3.17474518670082));
#43884=CARTESIAN_POINT('Ctrl Pts',(-2.12635002237642,0.794772684000832,
3.12672289098513));
#43885=CARTESIAN_POINT('Ctrl Pts',(-2.18177959699018,1.06847604194578,3.04725857901514));
#43886=CARTESIAN_POINT('Ctrl Pts',(-2.20492375066508,1.1851427086131,3.00986786508781));
#43887=CARTESIAN_POINT('Ctrl Pts',(-2.22721864903267,1.30000000000196,2.96948359344209));
#43888=CARTESIAN_POINT('Ctrl Pts',(-2.00791251142467,-1.3000000000018,2.8919145647167));
#43889=CARTESIAN_POINT('Ctrl Pts',(-1.9982083112576,-1.185142708613,2.94439906337569));
#43890=CARTESIAN_POINT('Ctrl Pts',(-1.98961105134247,-1.06847604194573,
2.99335513283515));
#43891=CARTESIAN_POINT('Ctrl Pts',(-1.97230691448723,-0.794772684000846,
3.09830206960359));
#43892=CARTESIAN_POINT('Ctrl Pts',(-1.96086800613691,-0.636309800095193,
3.15990898663756));
#43893=CARTESIAN_POINT('Ctrl Pts',(-1.95598036571629,-0.319434907277157,
3.23703223019669));
#43894=CARTESIAN_POINT('Ctrl Pts',(-1.9550549983292,-0.158333333333331,
3.26756876591028));
#43895=CARTESIAN_POINT('Ctrl Pts',(-1.97758329963365,0.158333333333334,
3.27869728916384));
#43896=CARTESIAN_POINT('Ctrl Pts',(-2.00066280746554,0.319434907277165,
3.25911472318076));
#43897=CARTESIAN_POINT('Ctrl Pts',(-2.05220111428241,0.636309800095203,
3.20501503316702));
#43898=CARTESIAN_POINT('Ctrl Pts',(-2.08860480006725,0.794772684000836,
3.15574523365688));
#43899=CARTESIAN_POINT('Ctrl Pts',(-2.14776574424549,1.06847604194578,3.07136984319128));
#43900=CARTESIAN_POINT('Ctrl Pts',(-2.17424128073391,1.18514270861311,3.0311778824398));
#43901=CARTESIAN_POINT('Ctrl Pts',(-2.20158377310493,1.30000000000197,2.98731694105318));
#43902=CARTESIAN_POINT('Ctrl Pts',(-1.99091305460786,-1.3000000000018,2.90872364328237));
#43903=CARTESIAN_POINT('Ctrl Pts',(-1.97826555025034,-1.185142708613,2.96473708658292));
#43904=CARTESIAN_POINT('Ctrl Pts',(-1.96758712102958,-1.06847604194573,
3.01631961176005));
#43905=CARTESIAN_POINT('Ctrl Pts',(-1.94746677079526,-0.794772684000843,
3.12524925670047));
#43906=CARTESIAN_POINT('Ctrl Pts',(-1.93723551063555,-0.636309800095191,
3.18660767585824));
#43907=CARTESIAN_POINT('Ctrl Pts',(-1.93242227851553,-0.319434907277156,
3.26396326267609));
#43908=CARTESIAN_POINT('Ctrl Pts',(-1.93235644974084,-0.158333333333331,
3.29329477084362));
#43909=CARTESIAN_POINT('Ctrl Pts',(-1.95417726778959,0.158333333333333,
3.30399040075478));
#43910=CARTESIAN_POINT('Ctrl Pts',(-1.97540017859542,0.319434907277166,
3.28501519179955));
#43911=CARTESIAN_POINT('Ctrl Pts',(-2.02601282840697,0.636309800095202,
3.23013702520077));
#43912=CARTESIAN_POINT('Ctrl Pts',(-2.06124729895273,0.794772684000832,
3.18111749727711));
#43913=CARTESIAN_POINT('Ctrl Pts',(-2.1232755139284,1.06847604194578,3.09271303762915));
#43914=CARTESIAN_POINT('Ctrl Pts',(-2.15194224912549,1.18514270861311,3.04991798288438));
#43915=CARTESIAN_POINT('Ctrl Pts',(-2.18242600362851,1.30000000000197,3.00259488826848));
#43916=CARTESIAN_POINT('Ctrl Pts',(-1.96891126495522,-1.30000000000181,
2.92924299368055));
#43917=CARTESIAN_POINT('Ctrl Pts',(-1.95238134199195,-1.18514270861301,
2.98950952795956));
#43918=CARTESIAN_POINT('Ctrl Pts',(-1.93907081124648,-1.06847604194574,
3.04433306419302));
#43919=CARTESIAN_POINT('Ctrl Pts',(-1.91575826252225,-0.794772684000849,
3.15841198594957));
#43920=CARTESIAN_POINT('Ctrl Pts',(-1.90770834455703,-0.636309800095193,
3.21988669858922));
#43921=CARTESIAN_POINT('Ctrl Pts',(-1.90414604058418,-0.319434907277156,
3.29824867101159));
#43922=CARTESIAN_POINT('Ctrl Pts',(-1.90653906674807,-0.158333333333331,
3.32692479228438));
#43923=CARTESIAN_POINT('Ctrl Pts',(-1.92757773297685,0.158333333333334,
3.33716497021942));
#43924=CARTESIAN_POINT('Ctrl Pts',(-1.94526711991391,0.319434907277167,
3.31825387261697));
#43925=CARTESIAN_POINT('Ctrl Pts',(-1.9936314909294,0.636309800095204,3.26171826035597));
#43926=CARTESIAN_POINT('Ctrl Pts',(-2.02662383139231,0.794772684000835,
3.21243371031589));
#43927=CARTESIAN_POINT('Ctrl Pts',(-2.0918247018996,1.06847604194578,3.11874594249202));
#43928=CARTESIAN_POINT('Ctrl Pts',(-2.12322116663215,1.18514270861311,3.07271557600675));
#43929=CARTESIAN_POINT('Ctrl Pts',(-2.15779105518492,1.30000000000197,3.02120880625334));
#43930=CARTESIAN_POINT('Ctrl Pts',(-1.94765865101397,-1.30000000000181,
2.95030374733435));
#43931=CARTESIAN_POINT('Ctrl Pts',(-1.92790508340059,-1.18514270861301,
3.01529722891932));
#43932=CARTESIAN_POINT('Ctrl Pts',(-1.91241996451229,-1.06847604194574,
3.07368996789426));
#43933=CARTESIAN_POINT('Ctrl Pts',(-1.8865072125481,-0.79477268400085,3.19333984045024));
#43934=CARTESIAN_POINT('Ctrl Pts',(-1.88064166515752,-0.636309800095194,
3.25489131573297));
#43935=CARTESIAN_POINT('Ctrl Pts',(-1.87760737563781,-0.319434907277157,
3.33380328845345));
#43936=CARTESIAN_POINT('Ctrl Pts',(-1.88074975802209,-0.158333333333332,
3.36074548314115));
#43937=CARTESIAN_POINT('Ctrl Pts',(-1.90100645273083,0.158333333333334,
3.37055545712555));
#43938=CARTESIAN_POINT('Ctrl Pts',(-1.91703990929339,0.319434907277168,
3.35292765819496));
#43939=CARTESIAN_POINT('Ctrl Pts',(-1.96353725276719,0.636309800095206,
3.29500735330529));
#43940=CARTESIAN_POINT('Ctrl Pts',(-1.99317440489421,0.794772684000836,
3.24479804609362));
#43941=CARTESIAN_POINT('Ctrl Pts',(-2.06134479848186,1.06847604194578,3.14565226416201));
#43942=CARTESIAN_POINT('Ctrl Pts',(-2.09551677023677,1.18514270861311,3.09637362817448));
#43943=CARTESIAN_POINT('Ctrl Pts',(-2.13435227632445,1.30000000000197,3.04073289148445));
#43944=CARTESIAN_POINT('Ctrl Pts',(-1.92692142534705,-1.30000000000181,
2.97161824960565));
#43945=CARTESIAN_POINT('Ctrl Pts',(-1.90386729002269,-1.18514270861301,
3.04116990549215));
#43946=CARTESIAN_POINT('Ctrl Pts',(-1.88627914618779,-1.06847604194574,
3.1030746797732));
#43947=CARTESIAN_POINT('Ctrl Pts',(-1.85827454924163,-0.794772684000848,
3.22842126610778));
#43948=CARTESIAN_POINT('Ctrl Pts',(-1.85546010955687,-0.636309800095197,
3.29049806719072));
#43949=CARTESIAN_POINT('Ctrl Pts',(-1.85388606537692,-0.31943490727716,
3.37048814797755));
#43950=CARTESIAN_POINT('Ctrl Pts',(-1.85855087100812,-0.158333333333332,
3.39623907172838));
#43951=CARTESIAN_POINT('Ctrl Pts',(-1.87792710232795,0.158333333333335,
3.40560369589062));
#43952=CARTESIAN_POINT('Ctrl Pts',(-1.89118745073622,0.319434907277167,
3.38857027282163));
#43953=CARTESIAN_POINT('Ctrl Pts',(-1.93518522291873,0.636309800095207,
3.32897340111308));
#43954=CARTESIAN_POINT('Ctrl Pts',(-1.96192720746975,0.794772684000843,
3.27822717572058));
#43955=CARTESIAN_POINT('Ctrl Pts',(-2.03215435767296,1.06847604194579,3.17319269348169));
#43956=CARTESIAN_POINT('Ctrl Pts',(-2.06847889453793,1.18514270861311,3.12033804137314));
#43957=CARTESIAN_POINT('Ctrl Pts',(-2.11072923711717,1.30000000000197,3.06009427260624));
#43958=CARTESIAN_POINT('Ctrl Pts',(-1.9148887376745,-1.30000000000181,2.98475844866592));
#43959=CARTESIAN_POINT('Ctrl Pts',(-1.88985290696311,-1.18514270861301,
3.05722651271223));
#43960=CARTESIAN_POINT('Ctrl Pts',(-1.87105265739054,-1.06847604194574,
3.12140222165167));
#43961=CARTESIAN_POINT('Ctrl Pts',(-1.84202575975531,-0.79477268400085,
3.25050394843119));
#43962=CARTESIAN_POINT('Ctrl Pts',(-1.84214725933546,-0.636309800095196,
3.31351072436173));
#43963=CARTESIAN_POINT('Ctrl Pts',(-1.84031348410914,-0.319434907277158,
3.39351117217984));
#43964=CARTESIAN_POINT('Ctrl Pts',(-1.84277573687377,-0.158333333333332,
3.41669588220879));
#43965=CARTESIAN_POINT('Ctrl Pts',(-1.8611725008453,0.158333333333335,3.42554170833206));
#43966=CARTESIAN_POINT('Ctrl Pts',(-1.87510093760627,0.319434907277169,
3.41028277821626));
#43967=CARTESIAN_POINT('Ctrl Pts',(-1.91849382563582,0.636309800095207,
3.35017470917515));
#43968=CARTESIAN_POINT('Ctrl Pts',(-1.94297883551598,0.794772684000839,
3.29878979088092));
#43969=CARTESIAN_POINT('Ctrl Pts',(-2.01463555477941,1.06847604194579,3.19013975303558));
#43970=CARTESIAN_POINT('Ctrl Pts',(-2.05239181690791,1.18514270861311,3.13509827737979));
#43971=CARTESIAN_POINT('Ctrl Pts',(-2.09688680253882,1.30000000000198,3.07204590157093));
#43972=CARTESIAN_POINT('Ctrl Pts',(-1.90476633611223,-1.30000000000181,
2.9955128759078));
#43973=CARTESIAN_POINT('Ctrl Pts',(-1.87892882368393,-1.18514270861301,
3.07063333458284));
#43974=CARTESIAN_POINT('Ctrl Pts',(-1.85938481786887,-1.06847604194574,
3.13665012918577));
#43975=CARTESIAN_POINT('Ctrl Pts',(-1.82877351395948,-0.794772684000852,
3.26813084614438));
#43976=CARTESIAN_POINT('Ctrl Pts',(-1.82777277121735,-0.636309800095196,
3.32985571507095));
#43977=CARTESIAN_POINT('Ctrl Pts',(-1.82519920803595,-0.319434907277158,
3.40946759971276));
#43978=CARTESIAN_POINT('Ctrl Pts',(-1.82786500157534,-0.158333333333332,
3.43168651366379));
#43979=CARTESIAN_POINT('Ctrl Pts',(-1.84675980907114,0.158333333333334,
3.44083983489165));
#43980=CARTESIAN_POINT('Ctrl Pts',(-1.8617377834321,0.319434907277168,3.42729831431622));
#43981=CARTESIAN_POINT('Ctrl Pts',(-1.90534698658927,0.636309800095207,
3.36730051672168));
#43982=CARTESIAN_POINT('Ctrl Pts',(-1.92818929679077,0.79477268400084,3.31562202142933));
#43983=CARTESIAN_POINT('Ctrl Pts',(-2.00107159200056,1.06847604194579,3.20434538599608));
#43984=CARTESIAN_POINT('Ctrl Pts',(-2.03992589311055,1.18514270861311,3.14763454428652));
#43985=CARTESIAN_POINT('Ctrl Pts',(-2.08608645028931,1.30000000000198,3.08238039314089));
#43986=CARTESIAN_POINT('Ctrl Pts',(-1.89326780681869,-1.30000000000181,
3.00896395652527));
#43987=CARTESIAN_POINT('Ctrl Pts',(-1.86630488495873,-1.18514270861301,
3.0876216818592));
#43988=CARTESIAN_POINT('Ctrl Pts',(-1.84556737380607,-1.06847604194574,
3.15603233359385));
#43989=CARTESIAN_POINT('Ctrl Pts',(-1.81204151864165,-0.794772684000851,
3.29040183467012));
#43990=CARTESIAN_POINT('Ctrl Pts',(-1.80838728385254,-0.636309800095196,
3.34998635143928));
#43991=CARTESIAN_POINT('Ctrl Pts',(-1.80384325729454,-0.319434907277158,
3.42867224736089));
#43992=CARTESIAN_POINT('Ctrl Pts',(-1.80676462972489,-0.158333333333332,
3.44958860602811));
#43993=CARTESIAN_POINT('Ctrl Pts',(-1.82555746981584,0.158333333333334,
3.45870878323941));
#43994=CARTESIAN_POINT('Ctrl Pts',(-1.84045866753833,0.319434907277167,
3.44661867877365));
#43995=CARTESIAN_POINT('Ctrl Pts',(-1.8852587262344,0.636309800095206,3.3871086271648));
#43996=CARTESIAN_POINT('Ctrl Pts',(-1.90913160377284,0.79477268400084,3.33661715000765));
#43997=CARTESIAN_POINT('Ctrl Pts',(-1.98479359038803,1.06847604194579,3.22231077812534));
#43998=CARTESIAN_POINT('Ctrl Pts',(-2.02514552074472,1.18514270861311,3.1633424593463));
#43999=CARTESIAN_POINT('Ctrl Pts',(-2.07309811100521,1.30000000000198,3.0948848147077));
#44000=CARTESIAN_POINT('Ctrl Pts',(-1.88533826855982,-1.30000000000181,
3.01806098483422));
#44001=CARTESIAN_POINT('Ctrl Pts',(-1.8587786442265,-1.18514270861301,3.09980889203863));
#44002=CARTESIAN_POINT('Ctrl Pts',(-1.83771824840901,-1.06847604194574,
3.17002999271618));
#44003=CARTESIAN_POINT('Ctrl Pts',(-1.80176883894142,-0.794772684000851,
3.30562555395723));
#44004=CARTESIAN_POINT('Ctrl Pts',(-1.79303694377367,-0.636309800095197,
3.36107920116882));
#44005=CARTESIAN_POINT('Ctrl Pts',(-1.78572104870416,-0.319434907277159,
3.43766535670148));
#44006=CARTESIAN_POINT('Ctrl Pts',(-1.78936170987159,-0.158333333333332,
3.45778637033323));
#44007=CARTESIAN_POINT('Ctrl Pts',(-1.8080248988652,0.158333333333334,3.4667877566422));
#44008=CARTESIAN_POINT('Ctrl Pts',(-1.82221963518582,0.319434907277167,
3.45538257525931));
#44009=CARTESIAN_POINT('Ctrl Pts',(-1.869237254135,0.636309800095206,3.39771324857652));
#44010=CARTESIAN_POINT('Ctrl Pts',(-1.89712646388558,0.79477268400084,3.35104670890408));
#44011=CARTESIAN_POINT('Ctrl Pts',(-1.97527792161989,1.06847604194579,3.23554112305398));
#44012=CARTESIAN_POINT('Ctrl Pts',(-2.01625666953888,1.18514270861311,3.1748648984291));
#44013=CARTESIAN_POINT('Ctrl Pts',(-2.06438529512048,1.30000000000198,3.10351053739022));
#44014=CARTESIAN_POINT('Ctrl Pts',(-1.87799128879426,-1.30000000000181,
3.02253507588625));
#44015=CARTESIAN_POINT('Ctrl Pts',(-1.85162982048175,-1.18514270861301,
3.10412841772033));
#44016=CARTESIAN_POINT('Ctrl Pts',(-1.83046672246869,-1.06847604194574,
3.17402030998991));
#44017=CARTESIAN_POINT('Ctrl Pts',(-1.79358500771746,-0.794772684000851,
3.30845187359642));
#44018=CARTESIAN_POINT('Ctrl Pts',(-1.78288365918825,-0.636309800095197,
3.36226104014369));
#44019=CARTESIAN_POINT('Ctrl Pts',(-1.77431562872861,-0.319434907277159,
3.43771727806328));
#44020=CARTESIAN_POINT('Ctrl Pts',(-1.77794490963746,-0.158333333333332,
3.4578893860418));
#44021=CARTESIAN_POINT('Ctrl Pts',(-1.79644754730033,0.158333333333334,
3.46671667358385));
#44022=CARTESIAN_POINT('Ctrl Pts',(-1.8102831109525,0.319434907277167,3.45490100101633));
#44023=CARTESIAN_POINT('Ctrl Pts',(-1.85865359192218,0.636309800095206,
3.39838440412251));
#44024=CARTESIAN_POINT('Ctrl Pts',(-1.8893645694356,0.79477268400084,3.35403177699279));
#44025=CARTESIAN_POINT('Ctrl Pts',(-1.96832072991261,1.06847604194579,3.23960467551191));
#44026=CARTESIAN_POINT('Ctrl Pts',(-2.00914338193045,1.18514270861311,3.17906956425754));
#44027=CARTESIAN_POINT('Ctrl Pts',(-2.05661148970959,1.30000000000198,3.10753059403805));
#44028=CARTESIAN_POINT('Ctrl Pts',(-1.87799128879384,-1.3,3.02253507588753));
#44029=CARTESIAN_POINT('Ctrl Pts',(-1.85162982048153,-1.18514270861178,
3.10412841772107));
#44030=CARTESIAN_POINT('Ctrl Pts',(-1.8304667224686,-1.06847604194512,3.17402030999021));
#44031=CARTESIAN_POINT('Ctrl Pts',(-1.79358500771746,-0.794772684000851,
3.30845187359642));
#44032=CARTESIAN_POINT('Ctrl Pts',(-1.78288365918825,-0.636309800095197,
3.36226104014369));
#44033=CARTESIAN_POINT('Ctrl Pts',(-1.77431562872862,-0.319434907277159,
3.43771727806328));
#44034=CARTESIAN_POINT('Ctrl Pts',(-1.77794490963746,-0.158333333333332,
3.45788938604181));
#44035=CARTESIAN_POINT('Ctrl Pts',(-1.79644754730033,0.158333333333334,
3.46671667358385));
#44036=CARTESIAN_POINT('Ctrl Pts',(-1.8102831109525,0.319434907277167,3.45490100101633));
#44037=CARTESIAN_POINT('Ctrl Pts',(-1.85865359192218,0.636309800095206,
3.39838440412251));
#44038=CARTESIAN_POINT('Ctrl Pts',(-1.8893645694356,0.79477268400084,3.35403177699279));
#44039=CARTESIAN_POINT('Ctrl Pts',(-1.96832072991242,1.06847604194511,3.23960467551219));
#44040=CARTESIAN_POINT('Ctrl Pts',(-2.00914338192998,1.18514270861178,3.17906956425824));
#44041=CARTESIAN_POINT('Ctrl Pts',(-2.05661148970878,1.3,3.10753059403928));
#44042=CARTESIAN_POINT('',(-2.20676493717361,-1.2,2.76912102263432));
#44043=CARTESIAN_POINT('Ctrl Pts',(-2.20676493717361,-1.2,2.76912102263432));
#44044=CARTESIAN_POINT('Ctrl Pts',(-2.18959342499164,-1.21474920900201,
2.77704610786863));
#44045=CARTESIAN_POINT('Ctrl Pts',(-2.18825900990267,-1.21544842993642,
2.77717319380777));
#44046=CARTESIAN_POINT('Ctrl Pts',(-2.16536120078355,-1.23449324006335,
2.78712413918319));
#44047=CARTESIAN_POINT('Ctrl Pts',(-2.16384270892882,-1.23586773324202,
2.78790177160257));
#44048=CARTESIAN_POINT('Ctrl Pts',(-2.12798513336799,-1.26665429549693,
2.80466996299418));
#44049=CARTESIAN_POINT('Ctrl Pts',(-2.11236536519738,-1.2798581653664,2.81178284923323));
#44050=CARTESIAN_POINT('Ctrl Pts',(-2.08925763079311,-1.30000000000178,
2.82307156191063));
#44051=CARTESIAN_POINT('',(-2.3458424267643,-0.653834841421144,2.84115573706238));
#44052=CARTESIAN_POINT('Ctrl Pts',(-2.34584242677385,-0.653834841420469,
2.84115573703903));
#44053=CARTESIAN_POINT('Ctrl Pts',(-2.33125630278765,-0.719118562165429,
2.83330577809928));
#44054=CARTESIAN_POINT('Ctrl Pts',(-2.31992974450258,-0.763459406308881,
2.82727725267908));
#44055=CARTESIAN_POINT('Ctrl Pts',(-2.27425749731053,-0.94963865469992,
2.80324291065325));
#44056=CARTESIAN_POINT('Ctrl Pts',(-2.24776174106812,-1.05261022998892,
2.78953916310548));
#44057=CARTESIAN_POINT('Ctrl Pts',(-2.20676493717361,-1.2,2.76912102263432));
#44058=CARTESIAN_POINT('',(-2.46774460503139,0.653834841531101,2.90899352548397));
#44059=CARTESIAN_POINT('Ctrl Pts',(-2.46774460503139,0.6538348415311,2.90899352548397));
#44060=CARTESIAN_POINT('Ctrl Pts',(-2.43367455207709,0.575764716732145,
2.93301788730227));
#44061=CARTESIAN_POINT('Ctrl Pts',(-2.40473079536294,0.49386600743549,2.95258260670437));
#44062=CARTESIAN_POINT('Ctrl Pts',(-2.3613241452078,0.338182309445636,2.97879498027382));
#44063=CARTESIAN_POINT('Ctrl Pts',(-2.34534839465029,0.26570061668282,2.98694809138619));
#44064=CARTESIAN_POINT('Ctrl Pts',(-2.32198141046681,0.129734501997336,
2.99409093181665));
#44065=CARTESIAN_POINT('Ctrl Pts',(-2.3137066916505,0.0666508202182009,
2.99426128761355));
#44066=CARTESIAN_POINT('Ctrl Pts',(-2.30187610082096,-0.0595255417580441,
2.98810497259799));
#44067=CARTESIAN_POINT('Ctrl Pts',(-2.29822356580874,-0.122765063402191,
2.98174712248733));
#44068=CARTESIAN_POINT('Ctrl Pts',(-2.29616337797591,-0.260131979528658,
2.96113524134179));
#44069=CARTESIAN_POINT('Ctrl Pts',(-2.29882503835795,-0.333936745811711,
2.94565054396205));
#44070=CARTESIAN_POINT('Ctrl Pts',(-2.31352704947006,-0.49110863627357,
2.90332005827053));
#44071=CARTESIAN_POINT('Ctrl Pts',(-2.32698048328179,-0.574253237247853,
2.87477504935862));
#44072=CARTESIAN_POINT('Ctrl Pts',(-2.34584242672574,-0.65383484143241,
2.84115573706742));
#44073=CARTESIAN_POINT('',(-2.40496089006672,1.2,2.8734929657691));
#44074=CARTESIAN_POINT('Ctrl Pts',(-2.40496089006672,1.2,2.8734929657691));
#44075=CARTESIAN_POINT('Ctrl Pts',(-2.41287040100767,1.15218563167953,2.87788959897044));
#44076=CARTESIAN_POINT('Ctrl Pts',(-2.42731667097231,1.06332654423114,2.88594041030948));
#44077=CARTESIAN_POINT('Ctrl Pts',(-2.45656691359185,0.804836252522856,
2.90256835751397));
#44078=CARTESIAN_POINT('Ctrl Pts',(-2.46205856622822,0.741545664188083,
2.90572350208414));
#44079=CARTESIAN_POINT('Ctrl Pts',(-2.46774460503139,0.653834841531101,
2.90899352548397));
#44080=CARTESIAN_POINT('Ctrl Pts',(-2.29120499224679,1.30000000000195,2.92532110171016));
#44081=CARTESIAN_POINT('Ctrl Pts',(-2.29212457406799,1.29919343636464,2.92489887509983));
#44082=CARTESIAN_POINT('Ctrl Pts',(-2.29304015951971,1.29838659872316,2.92447432719573));
#44083=CARTESIAN_POINT('Ctrl Pts',(-2.31180419504521,1.28165454130476,2.91555298390577));
#44084=CARTESIAN_POINT('Ctrl Pts',(-2.3297873229645,1.26578478037346,2.90724018576387));
#44085=CARTESIAN_POINT('Ctrl Pts',(-2.35953440176376,1.23935794201536,2.89336991066159));
#44086=CARTESIAN_POINT('Ctrl Pts',(-2.38221727164868,1.21902715818375,2.88261970932993));
#44087=CARTESIAN_POINT('Ctrl Pts',(-2.40496089006672,1.2,2.8734929657691));
#44088=CARTESIAN_POINT('Ctrl Pts',(-1.87799128879384,-1.3,3.02253507588753));
#44089=CARTESIAN_POINT('Ctrl Pts',(-1.85162982048153,-1.18514270861178,
3.10412841772107));
#44090=CARTESIAN_POINT('Ctrl Pts',(-1.8304667224686,-1.06847604194512,3.17402030999022));
#44091=CARTESIAN_POINT('Ctrl Pts',(-1.79358500771746,-0.794772684000851,
3.30845187359642));
#44092=CARTESIAN_POINT('Ctrl Pts',(-1.78288365918825,-0.636309800095196,
3.36226104014369));
#44093=CARTESIAN_POINT('Ctrl Pts',(-1.77431562872861,-0.319434907277159,
3.43771727806328));
#44094=CARTESIAN_POINT('Ctrl Pts',(-1.77794490963746,-0.158333333333332,
3.4578893860418));
#44095=CARTESIAN_POINT('Ctrl Pts',(-1.79644754730033,0.158333333333335,
3.46671667358385));
#44096=CARTESIAN_POINT('Ctrl Pts',(-1.8102831109525,0.319434907277167,3.45490100101633));
#44097=CARTESIAN_POINT('Ctrl Pts',(-1.85865359192218,0.636309800095206,
3.39838440412251));
#44098=CARTESIAN_POINT('Ctrl Pts',(-1.8893645694356,0.79477268400084,3.35403177699279));
#44099=CARTESIAN_POINT('Ctrl Pts',(-1.96832072991242,1.06847604194511,3.23960467551219));
#44100=CARTESIAN_POINT('Ctrl Pts',(-2.00914338192998,1.18514270861178,3.17906956425824));
#44101=CARTESIAN_POINT('Ctrl Pts',(-2.05661148970878,1.3,3.10753059403928));
#44102=CARTESIAN_POINT('Ctrl Pts',(-1.80704611563284,-1.3,2.99277114335502));
#44103=CARTESIAN_POINT('Ctrl Pts',(-1.78233798615881,-1.18514270861178,
3.07488156897468));
#44104=CARTESIAN_POINT('Ctrl Pts',(-1.76233903122006,-1.06847604194512,
3.14509050992361));
#44105=CARTESIAN_POINT('Ctrl Pts',(-1.72701657977794,-0.794772684000851,
3.27979239829291));
#44106=CARTESIAN_POINT('Ctrl Pts',(-1.71574542397768,-0.636309800095196,
3.33316531076088));
#44107=CARTESIAN_POINT('Ctrl Pts',(-1.70682212124655,-0.319434907277159,
3.4080572218364));
#44108=CARTESIAN_POINT('Ctrl Pts',(-1.70940065624172,-0.158333333333332,
3.42756797905052));
#44109=CARTESIAN_POINT('Ctrl Pts',(-1.72804929275646,0.158333333333335,
3.43606734780233));
#44110=CARTESIAN_POINT('Ctrl Pts',(-1.74307942205737,0.319434907277167,
3.42459000158545));
#44111=CARTESIAN_POINT('Ctrl Pts',(-1.79210700315155,0.636309800095206,
3.36795981507847));
#44112=CARTESIAN_POINT('Ctrl Pts',(-1.82352345611137,0.79477268400084,3.32373872631714));
#44113=CARTESIAN_POINT('Ctrl Pts',(-1.90123537533585,1.06847604194511,3.20833374894953));
#44114=CARTESIAN_POINT('Ctrl Pts',(-1.9410434505065,1.18514270861178,3.14714565776922));
#44115=CARTESIAN_POINT('Ctrl Pts',(-1.98702099052592,1.3,3.07472401393519));
#44116=CARTESIAN_POINT('Ctrl Pts',(-1.73610094247183,-1.3,2.96300721082251));
#44117=CARTESIAN_POINT('Ctrl Pts',(-1.71304615183608,-1.18514270861178,
3.0456347202283));
#44118=CARTESIAN_POINT('Ctrl Pts',(-1.69421133997151,-1.06847604194512,
3.11616070985699));
#44119=CARTESIAN_POINT('Ctrl Pts',(-1.66044815183843,-0.794772684000851,
3.2511329229894));
#44120=CARTESIAN_POINT('Ctrl Pts',(-1.64860718876712,-0.636309800095196,
3.30406958137807));
#44121=CARTESIAN_POINT('Ctrl Pts',(-1.63932861376449,-0.319434907277159,
3.37839716560952));
#44122=CARTESIAN_POINT('Ctrl Pts',(-1.64085640284598,-0.158333333333332,
3.39724657205923));
#44123=CARTESIAN_POINT('Ctrl Pts',(-1.65965103821258,0.158333333333335,
3.4054180220208));
#44124=CARTESIAN_POINT('Ctrl Pts',(-1.67587573316224,0.319434907277167,
3.39427900215456));
#44125=CARTESIAN_POINT('Ctrl Pts',(-1.72556041438091,0.636309800095206,
3.33753522603443));
#44126=CARTESIAN_POINT('Ctrl Pts',(-1.75768234278715,0.79477268400084,3.29344567564149));
#44127=CARTESIAN_POINT('Ctrl Pts',(-1.83415002075929,1.06847604194511,3.17706282238686));
#44128=CARTESIAN_POINT('Ctrl Pts',(-1.87294351908302,1.18514270861178,3.11522175128021));
#44129=CARTESIAN_POINT('Ctrl Pts',(-1.91743049134307,1.3,3.04191743383109));
#44130=CARTESIAN_POINT('Ctrl Pts',(-1.66515576931082,-1.3,2.93324327829));
#44131=CARTESIAN_POINT('Ctrl Pts',(-1.64375431751336,-1.18514270861178,
3.01638787148191));
#44132=CARTESIAN_POINT('Ctrl Pts',(-1.62608364872297,-1.06847604194512,
3.08723090979038));
#44133=CARTESIAN_POINT('Ctrl Pts',(-1.59387972389892,-0.794772684000851,
3.22247344768588));
#44134=CARTESIAN_POINT('Ctrl Pts',(-1.58146895355655,-0.636309800095196,
3.27497385199526));
#44135=CARTESIAN_POINT('Ctrl Pts',(-1.57183510628243,-0.319434907277159,
3.34873710938264));
#44136=CARTESIAN_POINT('Ctrl Pts',(-1.57231214945024,-0.158333333333332,
3.36692516506794));
#44137=CARTESIAN_POINT('Ctrl Pts',(-1.5912527836687,0.158333333333335,3.37476869623928));
#44138=CARTESIAN_POINT('Ctrl Pts',(-1.6086720442671,0.319434907277167,3.36396800272368));
#44139=CARTESIAN_POINT('Ctrl Pts',(-1.65901382561028,0.636309800095206,
3.30711063699039));
#44140=CARTESIAN_POINT('Ctrl Pts',(-1.69184122946292,0.79477268400084,3.26315262496584));
#44141=CARTESIAN_POINT('Ctrl Pts',(-1.76706466618272,1.06847604194511,3.1457918958242));
#44142=CARTESIAN_POINT('Ctrl Pts',(-1.80484358765954,1.18514270861178,3.08329784479119));
#44143=CARTESIAN_POINT('Ctrl Pts',(-1.84783999216022,1.3,3.00911085372699));
#44144=CARTESIAN_POINT('Ctrl Pts',(-1.66515576931082,-1.3,2.93324327829));
#44145=CARTESIAN_POINT('Ctrl Pts',(-1.64375431751336,-1.18514270861178,
3.01638787148191));
#44146=CARTESIAN_POINT('Ctrl Pts',(-1.62608364872297,-1.06847604194512,
3.08723090979038));
#44147=CARTESIAN_POINT('Ctrl Pts',(-1.59387972389891,-0.794772684000851,
3.22247344768589));
#44148=CARTESIAN_POINT('Ctrl Pts',(-1.58146895355655,-0.636309800095197,
3.27497385199526));
#44149=CARTESIAN_POINT('Ctrl Pts',(-1.57183510628243,-0.319434907277159,
3.34873710938264));
#44150=CARTESIAN_POINT('Ctrl Pts',(-1.57231214945024,-0.158333333333332,
3.36692516506795));
#44151=CARTESIAN_POINT('Ctrl Pts',(-1.5912527836687,0.158333333333334,3.37476869623928));
#44152=CARTESIAN_POINT('Ctrl Pts',(-1.6086720442671,0.319434907277167,3.36396800272368));
#44153=CARTESIAN_POINT('Ctrl Pts',(-1.65901382561028,0.636309800095206,
3.30711063699039));
#44154=CARTESIAN_POINT('Ctrl Pts',(-1.69184122946292,0.79477268400084,3.26315262496584));
#44155=CARTESIAN_POINT('Ctrl Pts',(-1.76706466618272,1.06847604194511,3.1457918958242));
#44156=CARTESIAN_POINT('Ctrl Pts',(-1.80484358765954,1.18514270861178,3.08329784479119));
#44157=CARTESIAN_POINT('Ctrl Pts',(-1.84783999216021,1.3,3.00911085372699));
#44158=CARTESIAN_POINT('Ctrl Pts',(-1.6651557693112,-1.30000000000205,2.93324327828851));
#44159=CARTESIAN_POINT('Ctrl Pts',(-1.64375431751357,-1.18514270861317,
3.01638787148107));
#44160=CARTESIAN_POINT('Ctrl Pts',(-1.62608364872305,-1.06847604194582,
3.08723090979004));
#44161=CARTESIAN_POINT('Ctrl Pts',(-1.59387972389891,-0.794772684000851,
3.22247344768589));
#44162=CARTESIAN_POINT('Ctrl Pts',(-1.58146895355655,-0.636309800095197,
3.27497385199526));
#44163=CARTESIAN_POINT('Ctrl Pts',(-1.57183510628243,-0.319434907277159,
3.34873710938264));
#44164=CARTESIAN_POINT('Ctrl Pts',(-1.57231214945024,-0.158333333333332,
3.36692516506795));
#44165=CARTESIAN_POINT('Ctrl Pts',(-1.5912527836687,0.158333333333334,3.37476869623928));
#44166=CARTESIAN_POINT('Ctrl Pts',(-1.6086720442671,0.319434907277167,3.36396800272368));
#44167=CARTESIAN_POINT('Ctrl Pts',(-1.65901382561028,0.636309800095206,
3.30711063699039));
#44168=CARTESIAN_POINT('Ctrl Pts',(-1.69184122946292,0.79477268400084,3.26315262496584));
#44169=CARTESIAN_POINT('Ctrl Pts',(-1.76706466618285,1.06847604194558,3.145791895824));
#44170=CARTESIAN_POINT('Ctrl Pts',(-1.80484358765984,1.1851427086127,3.0832978447907));
#44171=CARTESIAN_POINT('Ctrl Pts',(-1.84783999216072,1.30000000000136,3.00911085372612));
#44172=CARTESIAN_POINT('Ctrl Pts',(-1.66294156245583,-1.30000000000205,
2.92477627213571));
#44173=CARTESIAN_POINT('Ctrl Pts',(-1.64211927469575,-1.18514270861317,
3.00828819805516));
#44174=CARTESIAN_POINT('Ctrl Pts',(-1.62444818678095,-1.06847604194582,
3.07934166149543));
#44175=CARTESIAN_POINT('Ctrl Pts',(-1.59090434064678,-0.794772684000851,
3.21470783560491));
#44176=CARTESIAN_POINT('Ctrl Pts',(-1.57488586700129,-0.636309800095197,
3.26665956749681));
#44177=CARTESIAN_POINT('Ctrl Pts',(-1.56349013315575,-0.319434907277159,
3.34018877927888));
#44178=CARTESIAN_POINT('Ctrl Pts',(-1.56451256412486,-0.158333333333332,
3.35836908011497));
#44179=CARTESIAN_POINT('Ctrl Pts',(-1.5836900087521,0.158333333333334,3.3662154293602));
#44180=CARTESIAN_POINT('Ctrl Pts',(-1.60107891375656,0.319434907277167,
3.35545738175593));
#44181=CARTESIAN_POINT('Ctrl Pts',(-1.65309822965177,0.636309800095206,
3.29877447147387));
#44182=CARTESIAN_POINT('Ctrl Pts',(-1.6884655423189,0.79477268400084,3.25517967618859));
#44183=CARTESIAN_POINT('Ctrl Pts',(-1.7651778318562,1.06847604194558,3.13773291845356));
#44184=CARTESIAN_POINT('Ctrl Pts',(-1.80327012403915,1.1851427086127,3.07509490660645));
#44185=CARTESIAN_POINT('Ctrl Pts',(-1.84624880073476,1.30000000000136,3.00065723250455));
#44186=CARTESIAN_POINT('Ctrl Pts',(-1.6634305875893,-1.30000000000205,2.91253818382459));
#44187=CARTESIAN_POINT('Ctrl Pts',(-1.64459250993632,-1.18514270861317,
2.99401342938536));
#44188=CARTESIAN_POINT('Ctrl Pts',(-1.62774351228504,-1.06847604194582,
3.06348347679413));
#44189=CARTESIAN_POINT('Ctrl Pts',(-1.59341412979825,-0.794772684000852,
3.19623877438057));
#44190=CARTESIAN_POINT('Ctrl Pts',(-1.57193522590822,-0.636309800095198,
3.24776859715612));
#44191=CARTESIAN_POINT('Ctrl Pts',(-1.5577591921755,-0.31943490727716,3.32089454575369));
#44192=CARTESIAN_POINT('Ctrl Pts',(-1.55879969010269,-0.158333333333332,
3.34004933420448));
#44193=CARTESIAN_POINT('Ctrl Pts',(-1.5782014042107,0.158333333333335,3.34793016181554));
#44194=CARTESIAN_POINT('Ctrl Pts',(-1.59575204221966,0.319434907277167,
3.33615308111097));
#44195=CARTESIAN_POINT('Ctrl Pts',(-1.65109905999309,0.636309800095207,
3.28010462985753));
#44196=CARTESIAN_POINT('Ctrl Pts',(-1.69266556144995,0.794772684000843,
3.23744188421739));
#44197=CARTESIAN_POINT('Ctrl Pts',(-1.77009640342744,1.06847604194558,3.12257100392356));
#44198=CARTESIAN_POINT('Ctrl Pts',(-1.80712529462456,1.1851427086127,3.06137163709183));
#44199=CARTESIAN_POINT('Ctrl Pts',(-1.84766613462215,1.30000000000136,2.98869625112208));
#44200=CARTESIAN_POINT('Ctrl Pts',(-1.66409924349422,-1.30000000000205,
2.89751233934654));
#44201=CARTESIAN_POINT('Ctrl Pts',(-1.64632958993895,-1.18514270861317,
2.97603885688088));
#44202=CARTESIAN_POINT('Ctrl Pts',(-1.63008699942642,-1.06847604194582,
3.0432812599093));
#44203=CARTESIAN_POINT('Ctrl Pts',(-1.59609118714013,-0.794772684000853,
3.17255610081311));
#44204=CARTESIAN_POINT('Ctrl Pts',(-1.57317224543321,-0.636309800095198,
3.22410152369958));
#44205=CARTESIAN_POINT('Ctrl Pts',(-1.55789432690329,-0.31943490727716,
3.2967365657438));
#44206=CARTESIAN_POINT('Ctrl Pts',(-1.55797756487196,-0.158333333333332,
3.31675875423184));
#44207=CARTESIAN_POINT('Ctrl Pts',(-1.57736992673725,0.158333333333335,
3.32465368269152));
#44208=CARTESIAN_POINT('Ctrl Pts',(-1.59551109084602,0.319434907277167,
3.31191728904508));
#44209=CARTESIAN_POINT('Ctrl Pts',(-1.65266890419111,0.636309800095207,
3.25660440914048));
#44210=CARTESIAN_POINT('Ctrl Pts',(-1.69746082551081,0.794772684000843,
3.2145123098584));
#44211=CARTESIAN_POINT('Ctrl Pts',(-1.77471532910312,1.06847604194558,3.10313038179039));
#44212=CARTESIAN_POINT('Ctrl Pts',(-1.81082374324295,1.1851427086127,3.04402618572621));
#44213=CARTESIAN_POINT('Ctrl Pts',(-1.84959995947889,1.30000000000136,2.97403090315142));
#44214=CARTESIAN_POINT('Ctrl Pts',(-1.66413304228575,-1.30000000000205,
2.88855088157018));
#44215=CARTESIAN_POINT('Ctrl Pts',(-1.64663626767473,-1.18514270861317,
2.96549279537844));
#44216=CARTESIAN_POINT('Ctrl Pts',(-1.63063860211263,-1.06847604194582,
3.03158626229152));
#44217=CARTESIAN_POINT('Ctrl Pts',(-1.59714403614094,-0.794772684000851,
3.15921331026086));
#44218=CARTESIAN_POINT('Ctrl Pts',(-1.57468838437964,-0.636309800095196,
3.21118033024189));
#44219=CARTESIAN_POINT('Ctrl Pts',(-1.55933444655545,-0.319434907277159,
3.2837230199588));
#44220=CARTESIAN_POINT('Ctrl Pts',(-1.55861332258574,-0.158333333333332,
3.3040487115858));
#44221=CARTESIAN_POINT('Ctrl Pts',(-1.57793062519727,0.158333333333334,
3.31193446863975));
#44222=CARTESIAN_POINT('Ctrl Pts',(-1.59655517071776,0.319434907277167,
3.29881934722603));
#44223=CARTESIAN_POINT('Ctrl Pts',(-1.6541370369876,0.636309800095206,3.24371468381404));
#44224=CARTESIAN_POINT('Ctrl Pts',(-1.69949833972927,0.79477268400084,3.20151300621913));
#44225=CARTESIAN_POINT('Ctrl Pts',(-1.77645424648232,1.06847604194558,3.09181239223893));
#44226=CARTESIAN_POINT('Ctrl Pts',(-1.81221516246302,1.1851427086127,3.03380698464707));
#44227=CARTESIAN_POINT('Ctrl Pts',(-1.85042563388831,1.30000000000136,2.96528150044712));
#44228=CARTESIAN_POINT('Ctrl Pts',(-1.66445586874822,-1.30000000000205,
2.87650429183539));
#44229=CARTESIAN_POINT('Ctrl Pts',(-1.64746654614293,-1.18514270861317,
2.9511617041883));
#44230=CARTESIAN_POINT('Ctrl Pts',(-1.63193905490586,-1.06847604194582,
3.01562362169735));
#44231=CARTESIAN_POINT('Ctrl Pts',(-1.59944456678331,-0.79477268400085,
3.14098991401421));
#44232=CARTESIAN_POINT('Ctrl Pts',(-1.57799348539188,-0.636309800095196,
3.19378108820808));
#44233=CARTESIAN_POINT('Ctrl Pts',(-1.56251739556673,-0.319434907277159,
3.26627299656452));
#44234=CARTESIAN_POINT('Ctrl Pts',(-1.56021766016936,-0.158333333333332,
3.2869567263082));
#44235=CARTESIAN_POINT('Ctrl Pts',(-1.579297386822,0.158333333333334,3.29478244210874));
#44236=CARTESIAN_POINT('Ctrl Pts',(-1.59876559119614,0.319434907277167,
3.28109624173003));
#44237=CARTESIAN_POINT('Ctrl Pts',(-1.65699880469742,0.636309800095206,
3.22623170912691));
#44238=CARTESIAN_POINT('Ctrl Pts',(-1.70337675684885,0.794772684000841,
3.18387226395826));
#44239=CARTESIAN_POINT('Ctrl Pts',(-1.77954758974758,1.06847604194558,3.07646752958768));
#44240=CARTESIAN_POINT('Ctrl Pts',(-1.81453396341162,1.1851427086127,3.01996849556075));
#44241=CARTESIAN_POINT('Ctrl Pts',(-1.8515351795853,1.30000000000136,2.95346195727836));
#44242=CARTESIAN_POINT('Ctrl Pts',(-1.6643498478883,-1.30000000000205,2.86438665854125));
#44243=CARTESIAN_POINT('Ctrl Pts',(-1.64770189067232,-1.18514270861317,
2.93671789636582));
#44244=CARTESIAN_POINT('Ctrl Pts',(-1.63257569066065,-1.06847604194582,
2.99951947166058));
#44245=CARTESIAN_POINT('Ctrl Pts',(-1.60114670621631,-0.794772684000852,
3.12258824715685));
#44246=CARTESIAN_POINT('Ctrl Pts',(-1.58096527207976,-0.636309800095197,
3.17617757885722));
#44247=CARTESIAN_POINT('Ctrl Pts',(-1.56597543955806,-0.319434907277159,
3.24871816508311));
#44248=CARTESIAN_POINT('Ctrl Pts',(-1.5625222458354,-0.158333333333332,
3.26983928041926));
#44249=CARTESIAN_POINT('Ctrl Pts',(-1.58229897393715,0.158333333333335,
3.27791706510464));
#44250=CARTESIAN_POINT('Ctrl Pts',(-1.60405941583045,0.319434907277167,
3.26421397218699));
#44251=CARTESIAN_POINT('Ctrl Pts',(-1.66232624433739,0.636309800095206,
3.2094711399786));
#44252=CARTESIAN_POINT('Ctrl Pts',(-1.70674106971239,0.794772684000841,
3.16603757837));
#44253=CARTESIAN_POINT('Ctrl Pts',(-1.7814897873636,1.06847604194558,3.06076487540826));
#44254=CARTESIAN_POINT('Ctrl Pts',(-1.81592523135305,1.1851427086127,3.00585484616171));
#44255=CARTESIAN_POINT('Ctrl Pts',(-1.85244016917363,1.30000000000136,2.94160344004275));
#44256=CARTESIAN_POINT('Ctrl Pts',(-1.6631939573514,-1.30000000000205,2.84901103609872));
#44257=CARTESIAN_POINT('Ctrl Pts',(-1.64705706006683,-1.18514270861317,
2.9185030775211));
#44258=CARTESIAN_POINT('Ctrl Pts',(-1.63254236060157,-1.06847604194582,
2.97929848142592));
#44259=CARTESIAN_POINT('Ctrl Pts',(-1.60275810266336,-0.794772684000852,
3.09965705410264));
#44260=CARTESIAN_POINT('Ctrl Pts',(-1.58418289260517,-0.636309800095198,
3.15426789047404));
#44261=CARTESIAN_POINT('Ctrl Pts',(-1.57071860895688,-0.31943490727716,
3.22719026526377));
#44262=CARTESIAN_POINT('Ctrl Pts',(-1.56750832525203,-0.158333333333333,
3.24939746337031));
#44263=CARTESIAN_POINT('Ctrl Pts',(-1.58796133864451,0.158333333333335,
3.25773482052459));
#44264=CARTESIAN_POINT('Ctrl Pts',(-1.61042546287198,0.319434907277168,
3.24333833946108));
#44265=CARTESIAN_POINT('Ctrl Pts',(-1.66799369092752,0.636309800095208,
3.18847128887226));
#44266=CARTESIAN_POINT('Ctrl Pts',(-1.71065823061011,0.794772684000842,
3.14386957635525));
#44267=CARTESIAN_POINT('Ctrl Pts',(-1.78396337875779,1.06847604194558,3.04127089324132));
#44268=CARTESIAN_POINT('Ctrl Pts',(-1.81786493103005,1.1851427086127,2.98834641861744));
#44269=CARTESIAN_POINT('Ctrl Pts',(-1.85393695316482,1.30000000000136,2.92690863763393));
#44270=CARTESIAN_POINT('Ctrl Pts',(-1.66287285385524,-1.30000000000205,
2.83684381205742));
#44271=CARTESIAN_POINT('Ctrl Pts',(-1.64725497954519,-1.18514270861317,
2.90406038665813));
#44272=CARTESIAN_POINT('Ctrl Pts',(-1.63324137758571,-1.06847604194582,
2.96322801795107));
#44273=CARTESIAN_POINT('Ctrl Pts',(-1.60457334371134,-0.794772684000851,
3.08132241345498));
#44274=CARTESIAN_POINT('Ctrl Pts',(-1.58670059956992,-0.636309800095199,
3.13658864538851));
#44275=CARTESIAN_POINT('Ctrl Pts',(-1.57416217922139,-0.319434907277161,
3.20973093233505));
#44276=CARTESIAN_POINT('Ctrl Pts',(-1.57145871032908,-0.158333333333333,
3.23293006393472));
#44277=CARTESIAN_POINT('Ctrl Pts',(-1.59198547972842,0.158333333333335,
3.24130131732167));
#44278=CARTESIAN_POINT('Ctrl Pts',(-1.61389591587228,0.319434907277167,
3.2259155780679));
#44279=CARTESIAN_POINT('Ctrl Pts',(-1.67093422945697,0.636309800095208,
3.17096125429362));
#44280=CARTESIAN_POINT('Ctrl Pts',(-1.71365199342114,0.794772684000845,
3.12595232475909));
#44281=CARTESIAN_POINT('Ctrl Pts',(-1.78590535661653,1.06847604194558,3.02559590726589));
#44282=CARTESIAN_POINT('Ctrl Pts',(-1.81916201847011,1.1851427086127,2.97422359191595));
#44283=CARTESIAN_POINT('Ctrl Pts',(-1.85439953850088,1.30000000000137,2.91491953577721));
#44284=CARTESIAN_POINT('Ctrl Pts',(-1.66271526553442,-1.30000000000205,
2.81567174026498));
#44285=CARTESIAN_POINT('Ctrl Pts',(-1.64733326715726,-1.18514270861317,
2.87877836473091));
#44286=CARTESIAN_POINT('Ctrl Pts',(-1.63372876473195,-1.06847604194582,
2.93500590630431));
#44287=CARTESIAN_POINT('Ctrl Pts',(-1.60640601379383,-0.794772684000853,
3.04901071798214));
#44288=CARTESIAN_POINT('Ctrl Pts',(-1.59014548366958,-0.636309800095198,
3.10548900822069));
#44289=CARTESIAN_POINT('Ctrl Pts',(-1.57918993708349,-0.31943490727716,
3.17897283262899));
#44290=CARTESIAN_POINT('Ctrl Pts',(-1.57682954384601,-0.158333333333333,
3.20368408591858));
#44291=CARTESIAN_POINT('Ctrl Pts',(-1.59835814895341,0.158333333333335,
3.21240825833507));
#44292=CARTESIAN_POINT('Ctrl Pts',(-1.62159262469254,0.319434907277169,
3.19611224149114));
#44293=CARTESIAN_POINT('Ctrl Pts',(-1.67773360519212,0.636309800095209,
3.14102820846237));
#44294=CARTESIAN_POINT('Ctrl Pts',(-1.71775765489709,0.794772684000843,
3.09437447173804));
#44295=CARTESIAN_POINT('Ctrl Pts',(-1.78801951448282,1.06847604194558,2.99783516422076));
#44296=CARTESIAN_POINT('Ctrl Pts',(-1.82058725945667,1.1851427086127,2.94928807339681));
#44297=CARTESIAN_POINT('Ctrl Pts',(-1.85530899384812,1.30000000000136,2.89398218083932));
#44298=CARTESIAN_POINT('Ctrl Pts',(-1.65979832631176,-1.30000000000206,
2.78782357681252));
#44299=CARTESIAN_POINT('Ctrl Pts',(-1.64451139891587,-1.18514270861318,
2.84560432644518));
#44300=CARTESIAN_POINT('Ctrl Pts',(-1.63145107469241,-1.06847604194583,
2.89805914319504));
#44301=CARTESIAN_POINT('Ctrl Pts',(-1.60642301178616,-0.794772684000855,
3.00693629302853));
#44302=CARTESIAN_POINT('Ctrl Pts',(-1.59352139913235,-0.6363098000952,3.06524726776171));
#44303=CARTESIAN_POINT('Ctrl Pts',(-1.5856238781577,-0.319434907277161,
3.13941797151494));
#44304=CARTESIAN_POINT('Ctrl Pts',(-1.58468073357809,-0.158333333333333,
3.16639877628142));
#44305=CARTESIAN_POINT('Ctrl Pts',(-1.60650273181183,0.158333333333336,
3.1752338562451));
#44306=CARTESIAN_POINT('Ctrl Pts',(-1.62810716868432,0.319434907277171,
3.15667163125066));
#44307=CARTESIAN_POINT('Ctrl Pts',(-1.68281880325298,0.636309800095212,
3.10134573013792));
#44308=CARTESIAN_POINT('Ctrl Pts',(-1.72250898922017,0.794772684000845,
3.05363894723006));
#44309=CARTESIAN_POINT('Ctrl Pts',(-1.79094505544908,1.06847604194558,2.96226328258396));
#44310=CARTESIAN_POINT('Ctrl Pts',(-1.82252646622328,1.18514270861271,2.91731703719297));
#44311=CARTESIAN_POINT('Ctrl Pts',(-1.85606585050729,1.30000000000137,2.86697768583429));
#44312=CARTESIAN_POINT('Ctrl Pts',(-1.65813795427186,-1.30000000000206,
2.75729053581678));
#44313=CARTESIAN_POINT('Ctrl Pts',(-1.64390914515786,-1.18514270861318,
2.8093649400208));
#44314=CARTESIAN_POINT('Ctrl Pts',(-1.63171417909869,-1.06847604194583,
2.85767162458352));
#44315=CARTESIAN_POINT('Ctrl Pts',(-1.60823995223305,-0.794772684000857,
2.96056554354104));
#44316=CARTESIAN_POINT('Ctrl Pts',(-1.59535384607131,-0.636309800095199,
3.01999716620689));
#44317=CARTESIAN_POINT('Ctrl Pts',(-1.58893802195987,-0.319434907277159,
3.0943983470608));
#44318=CARTESIAN_POINT('Ctrl Pts',(-1.58943971299835,-0.158333333333333,
3.12375775987157));
#44319=CARTESIAN_POINT('Ctrl Pts',(-1.61241973646776,0.158333333333335,
3.13295204857722));
#44320=CARTESIAN_POINT('Ctrl Pts',(-1.63445324641201,0.319434907277171,
3.11260068244772));
#44321=CARTESIAN_POINT('Ctrl Pts',(-1.68858379509115,0.636309800095212,
3.05730696727029));
#44322=CARTESIAN_POINT('Ctrl Pts',(-1.72680330457903,0.794772684000844,
3.00804889397381));
#44323=CARTESIAN_POINT('Ctrl Pts',(-1.79379646466053,1.06847604194558,2.92257770154279));
#44324=CARTESIAN_POINT('Ctrl Pts',(-1.82477850626238,1.1851427086127,2.88178580755026));
#44325=CARTESIAN_POINT('Ctrl Pts',(-1.85774373280798,1.30000000000137,2.83719933174886));
#44326=CARTESIAN_POINT('Ctrl Pts',(-1.65570779467915,-1.30000000000206,
2.73263328270126));
#44327=CARTESIAN_POINT('Ctrl Pts',(-1.6407096481972,-1.18514270861318,2.77980265176276));
#44328=CARTESIAN_POINT('Ctrl Pts',(-1.62827778845606,-1.06847604194583,
2.82459427115372));
#44329=CARTESIAN_POINT('Ctrl Pts',(-1.60548634122433,-0.794772684000854,
2.92257879507314));
#44330=CARTESIAN_POINT('Ctrl Pts',(-1.59504082893022,-0.636309800095202,
2.98341758453039));
#44331=CARTESIAN_POINT('Ctrl Pts',(-1.59073845452414,-0.319434907277163,
3.058177072881));
#44332=CARTESIAN_POINT('Ctrl Pts',(-1.59232101440582,-0.158333333333334,
3.08940613991731));
#44333=CARTESIAN_POINT('Ctrl Pts',(-1.616032042732,0.158333333333336,3.09880489324563));
#44334=CARTESIAN_POINT('Ctrl Pts',(-1.63781874036801,0.319434907277172,
3.07684736794034));
#44335=CARTESIAN_POINT('Ctrl Pts',(-1.69111493475241,0.636309800095214,
3.02149158425097));
#44336=CARTESIAN_POINT('Ctrl Pts',(-1.72816231837234,0.794772684000848,
2.97104767819662));
#44337=CARTESIAN_POINT('Ctrl Pts',(-1.79394620683948,1.06847604194559,2.89029168350367));
#44338=CARTESIAN_POINT('Ctrl Pts',(-1.82444853281462,1.18514270861271,2.85281575960377));
#44339=CARTESIAN_POINT('Ctrl Pts',(-1.85697777698072,1.30000000000138,2.8128201896021));
#44340=CARTESIAN_POINT('Ctrl Pts',(-1.6535760658804,-1.30000000000206,2.71409163860464));
#44341=CARTESIAN_POINT('Ctrl Pts',(-1.63905181668487,-1.18514270861318,
2.75780601699314));
#44342=CARTESIAN_POINT('Ctrl Pts',(-1.62709515198573,-1.06847604194583,
2.80010088337208));
#44343=CARTESIAN_POINT('Ctrl Pts',(-1.60540449843839,-0.794772684000856,
2.8945311290517));
#44344=CARTESIAN_POINT('Ctrl Pts',(-1.59579211137064,-0.636309800095201,
2.95622529437884));
#44345=CARTESIAN_POINT('Ctrl Pts',(-1.59231902228133,-0.319434907277162,
3.03107887714456));
#44346=CARTESIAN_POINT('Ctrl Pts',(-1.59397995331801,-0.158333333333334,
3.06351789461748));
#44347=CARTESIAN_POINT('Ctrl Pts',(-1.61802231115706,0.158333333333336,
3.07301813934396));
#44348=CARTESIAN_POINT('Ctrl Pts',(-1.63995039656627,0.319434907277172,
3.04994084003861));
#44349=CARTESIAN_POINT('Ctrl Pts',(-1.69331946124273,0.636309800095213,
2.99472074036669));
#44350=CARTESIAN_POINT('Ctrl Pts',(-1.73056578233587,0.794772684000846,
2.94366555047251));
#44351=CARTESIAN_POINT('Ctrl Pts',(-1.79568322889274,1.06847604194558,2.86651029602232));
#44352=CARTESIAN_POINT('Ctrl Pts',(-1.82570445831112,1.18514270861271,2.83149135893238));
#44353=CARTESIAN_POINT('Ctrl Pts',(-1.85755998737255,1.30000000000137,2.79485113552013));
#44354=CARTESIAN_POINT('Ctrl Pts',(-1.65142819925317,-1.30000000000207,
2.69555803570173));
#44355=CARTESIAN_POINT('Ctrl Pts',(-1.63652140704014,-1.18514270861319,
2.73564493465463));
#44356=CARTESIAN_POINT('Ctrl Pts',(-1.62445167600304,-1.06847604194583,
2.77532087071986));
#44357=CARTESIAN_POINT('Ctrl Pts',(-1.60312236163452,-0.794772684000861,
2.86603081369074));
#44358=CARTESIAN_POINT('Ctrl Pts',(-1.59467568431381,-0.636309800095204,
2.9286131284341));
#44359=CARTESIAN_POINT('Ctrl Pts',(-1.59244392772632,-0.319434907277163,
3.00363546569633));
#44360=CARTESIAN_POINT('Ctrl Pts',(-1.59497869398103,-0.158333333333334,
3.0374717690488));
#44361=CARTESIAN_POINT('Ctrl Pts',(-1.61951237737304,0.158333333333337,
3.04710102064039));
#44362=CARTESIAN_POINT('Ctrl Pts',(-1.64131649243037,0.319434907277172,
3.02284038948529));
#44363=CARTESIAN_POINT('Ctrl Pts',(-1.69391839341423,0.636309800095215,
2.9675412817542));
#44364=CARTESIAN_POINT('Ctrl Pts',(-1.72981398463404,0.79477268400085,2.91548409447979));
#44365=CARTESIAN_POINT('Ctrl Pts',(-1.79427708629069,1.06847604194559,2.84192785080469));
#44366=CARTESIAN_POINT('Ctrl Pts',(-1.82420907094672,1.18514270861271,2.80946186186775));
#44367=CARTESIAN_POINT('Ctrl Pts',(-1.85616935214488,1.30000000000138,2.77636965635346));
#44368=CARTESIAN_POINT('Ctrl Pts',(-1.64970395610035,-1.30000000000206,
2.67712374665188));
#44369=CARTESIAN_POINT('Ctrl Pts',(-1.63440903515699,-1.18514270861318,
2.71358619627383));
#44370=CARTESIAN_POINT('Ctrl Pts',(-1.62220300990044,-1.06847604194583,
2.75064175423077));
#44371=CARTESIAN_POINT('Ctrl Pts',(-1.60114061671888,-0.79477268400086,
2.83761770495476));
#44372=CARTESIAN_POINT('Ctrl Pts',(-1.59362974755288,-0.636309800095204,
2.90104169110795));
#44373=CARTESIAN_POINT('Ctrl Pts',(-1.59270208718653,-0.319434907277163,
2.97624828130659));
#44374=CARTESIAN_POINT('Ctrl Pts',(-1.59648220610092,-0.158333333333334,
3.01156179865048));
#44375=CARTESIAN_POINT('Ctrl Pts',(-1.62153353448204,0.158333333333336,
3.02132088132003));
#44376=CARTESIAN_POINT('Ctrl Pts',(-1.6425998838543,0.319434907277172,2.99572297667271));
#44377=CARTESIAN_POINT('Ctrl Pts',(-1.69497258163952,0.636309800095215,
2.9404834803997));
#44378=CARTESIAN_POINT('Ctrl Pts',(-1.73105396418615,0.79477268400085,2.88781469783114));
#44379=CARTESIAN_POINT('Ctrl Pts',(-1.79525935632945,1.06847604194559,2.81796705538706));
#44380=CARTESIAN_POINT('Ctrl Pts',(-1.8250096066763,1.18514270861271,2.78803607922216));
#44381=CARTESIAN_POINT('Ctrl Pts',(-1.85671797215536,1.30000000000137,2.75840858319625));
#44382=CARTESIAN_POINT('Ctrl Pts',(-1.64667893682967,-1.30000000000207,
2.65843106406495));
#44383=CARTESIAN_POINT('Ctrl Pts',(-1.63153020095824,-1.18514270861319,
2.69137902331279));
#44384=CARTESIAN_POINT('Ctrl Pts',(-1.61958797589396,-1.06847604194584,
2.72589590660544));
#44385=CARTESIAN_POINT('Ctrl Pts',(-1.59940672838645,-0.794772684000862,
2.80926134049572));
#44386=CARTESIAN_POINT('Ctrl Pts',(-1.59315953932626,-0.636309800095206,
2.87360157089387));
#44387=CARTESIAN_POINT('Ctrl Pts',(-1.5929026847311,-0.319434907277164,
2.94883520381411));
#44388=CARTESIAN_POINT('Ctrl Pts',(-1.59639986569456,-0.158333333333335,
2.98526311606199));
#44389=CARTESIAN_POINT('Ctrl Pts',(-1.62132464236181,0.158333333333337,
2.99500225307932));
#44390=CARTESIAN_POINT('Ctrl Pts',(-1.64226956594183,0.319434907277172,
2.96822463560951));
#44391=CARTESIAN_POINT('Ctrl Pts',(-1.69427956432727,0.636309800095216,
2.91300988879695));
#44392=CARTESIAN_POINT('Ctrl Pts',(-1.72997844828931,0.794772684000853,
2.85958385827857));
#44393=CARTESIAN_POINT('Ctrl Pts',(-1.79388216221858,1.06847604194559,2.79341742157915));
#44394=CARTESIAN_POINT('Ctrl Pts',(-1.8235455079832,1.18514270861271,2.76603529463722));
#44395=CARTESIAN_POINT('Ctrl Pts',(-1.85521064961836,1.30000000000138,2.73991203949251));
#44396=CARTESIAN_POINT('Ctrl Pts',(-1.64412111466084,-1.30000000000207,
2.6398651645125));
#44397=CARTESIAN_POINT('Ctrl Pts',(-1.62798260075153,-1.18514270861319,
2.66908877628028));
#44398=CARTESIAN_POINT('Ctrl Pts',(-1.6154792907022,-1.06847604194584,2.70090983214457));
#44399=CARTESIAN_POINT('Ctrl Pts',(-1.59499219134632,-0.794772684000864,
2.78042345245108));
#44400=CARTESIAN_POINT('Ctrl Pts',(-1.58973719006436,-0.636309800095206,
2.84557205418552));
#44401=CARTESIAN_POINT('Ctrl Pts',(-1.59118661578248,-0.319434907277163,
2.9210401630057));
#44402=CARTESIAN_POINT('Ctrl Pts',(-1.59649715240767,-0.158333333333335,
2.95903747823188));
#44403=CARTESIAN_POINT('Ctrl Pts',(-1.62285437331818,0.158333333333337,
2.96910203929093));
#44404=CARTESIAN_POINT('Ctrl Pts',(-1.64419807136409,0.319434907277175,
2.94127779762337));
#44405=CARTESIAN_POINT('Ctrl Pts',(-1.69583141121319,0.636309800095219,
2.88608944285955));
#44406=CARTESIAN_POINT('Ctrl Pts',(-1.72975502771052,0.794772684000852,
2.83157946580677));
#44407=CARTESIAN_POINT('Ctrl Pts',(-1.79329774536375,1.06847604194559,2.76909658247525));
#44408=CARTESIAN_POINT('Ctrl Pts',(-1.823107272097,1.18514270861271,2.7443281138452));
#44409=CARTESIAN_POINT('Ctrl Pts',(-1.85522103758111,1.30000000000138,2.72183770156036));
#44410=CARTESIAN_POINT('Ctrl Pts',(-1.64094945361943,-1.30000000000208,
2.61515000440255));
#44411=CARTESIAN_POINT('Ctrl Pts',(-1.62468107455144,-1.1851427086132,2.63963826366359));
#44412=CARTESIAN_POINT('Ctrl Pts',(-1.61217517672228,-1.06847604194585,
2.66801224695561));
#44413=CARTESIAN_POINT('Ctrl Pts',(-1.59197613528423,-0.79477268400087,
2.74253862440383));
#44414=CARTESIAN_POINT('Ctrl Pts',(-1.58721925808487,-0.636309800095212,
2.80864512682796));
#44415=CARTESIAN_POINT('Ctrl Pts',(-1.58961959416009,-0.319434907277167,
2.88415188749081));
#44416=CARTESIAN_POINT('Ctrl Pts',(-1.5962106690206,-0.158333333333336,
2.92397834243149));
#44417=CARTESIAN_POINT('Ctrl Pts',(-1.6224445641406,0.158333333333338,2.93401310656952));
#44418=CARTESIAN_POINT('Ctrl Pts',(-1.64189888908404,0.319434907277176,
2.90423138779478));
#44419=CARTESIAN_POINT('Ctrl Pts',(-1.69331905985183,0.636309800095222,
2.84914440685121));
#44420=CARTESIAN_POINT('Ctrl Pts',(-1.72885664617953,0.79477268400086,2.79412538512413));
#44421=CARTESIAN_POINT('Ctrl Pts',(-1.79247296240661,1.0684760419456,2.73665013861037));
#44422=CARTESIAN_POINT('Ctrl Pts',(-1.82203822932527,1.18514270861273,2.71524106197467));
#44423=CARTESIAN_POINT('Ctrl Pts',(-1.85363161708467,1.30000000000139,2.69730181325134));
#44424=CARTESIAN_POINT('Ctrl Pts',(-1.6362445112492,-1.30000000000209,2.59017900567184));
#44425=CARTESIAN_POINT('Ctrl Pts',(-1.61935634141682,-1.18514270861321,
2.60985405552272));
#44426=CARTESIAN_POINT('Ctrl Pts',(-1.60655803475591,-1.06847604194585,
2.63473402983644));
#44427=CARTESIAN_POINT('Ctrl Pts',(-1.58643978817718,-0.794772684000877,
2.70423616447344));
#44428=CARTESIAN_POINT('Ctrl Pts',(-1.58274842400019,-0.636309800095214,
2.77138539803646));
#44429=CARTESIAN_POINT('Ctrl Pts',(-1.58654761135435,-0.319434907277167,
2.84699453149146));
#44430=CARTESIAN_POINT('Ctrl Pts',(-1.59403516911422,-0.158333333333337,
2.88853699146736));
#44431=CARTESIAN_POINT('Ctrl Pts',(-1.62180505785957,0.158333333333339,
2.89889527495238));
#44432=CARTESIAN_POINT('Ctrl Pts',(-1.64291504432118,0.319434907277178,
2.86795875947623));
#44433=CARTESIAN_POINT('Ctrl Pts',(-1.69399524623128,0.636309800095225,
2.81294423600424));
#44434=CARTESIAN_POINT('Ctrl Pts',(-1.72652996574593,0.794772684000862,
2.75637597115294));
#44435=CARTESIAN_POINT('Ctrl Pts',(-1.78960294812671,1.0684760419456,2.70378004334336));
#44436=CARTESIAN_POINT('Ctrl Pts',(-1.81943005640006,1.18514270861273,2.68585139577623));
#44437=CARTESIAN_POINT('Ctrl Pts',(-1.85178231595841,1.30000000000139,2.67276092891958));
#44438=CARTESIAN_POINT('Ctrl Pts',(-1.63234955645659,-1.3000000000021,2.56539932197508));
#44439=CARTESIAN_POINT('Ctrl Pts',(-1.61422340273142,-1.18514270861321,
2.58016419306643));
#44440=CARTESIAN_POINT('Ctrl Pts',(-1.60076142905862,-1.06847604194586,
2.60149109593607));
#44441=CARTESIAN_POINT('Ctrl Pts',(-1.58043676580292,-0.794772684000878,
2.66592011413487));
#44442=CARTESIAN_POINT('Ctrl Pts',(-1.57894742814013,-0.636309800095219,
2.7342993560036));
#44443=CARTESIAN_POINT('Ctrl Pts',(-1.58377104162534,-0.31943490727717,
2.80991755850134));
#44444=CARTESIAN_POINT('Ctrl Pts',(-1.5914330166678,-0.158333333333338,
2.85304301060135));
#44445=CARTESIAN_POINT('Ctrl Pts',(-1.61892764149841,0.15833333333334,2.86333412198892));
#44446=CARTESIAN_POINT('Ctrl Pts',(-1.63880461079261,0.319434907277178,
2.83060339342189));
#44447=CARTESIAN_POINT('Ctrl Pts',(-1.68989529276597,0.636309800095229,
2.77573639335614));
#44448=CARTESIAN_POINT('Ctrl Pts',(-1.72352228384938,0.794772684000869,
2.71852594707303));
#44449=CARTESIAN_POINT('Ctrl Pts',(-1.78730622572994,1.06847604194561,2.67106706560053));
#44450=CARTESIAN_POINT('Ctrl Pts',(-1.81738454011351,1.18514270861274,2.65660361998266));
#44451=CARTESIAN_POINT('Ctrl Pts',(-1.84993146386848,1.3000000000014,2.64821992001154));
#44452=CARTESIAN_POINT('Ctrl Pts',(-1.62923415387097,-1.3000000000021,2.54677610074369));
#44453=CARTESIAN_POINT('Ctrl Pts',(-1.6108894203325,-1.18514270861322,2.55798510922409));
#44454=CARTESIAN_POINT('Ctrl Pts',(-1.59724221540616,-1.06847604194586,
2.57670468010306));
#44455=CARTESIAN_POINT('Ctrl Pts',(-1.57656667274378,-0.794772684000883,
2.63730153529417));
#44456=CARTESIAN_POINT('Ctrl Pts',(-1.57451719774664,-0.636309800095222,
2.70622110562794));
#44457=CARTESIAN_POINT('Ctrl Pts',(-1.57999669011221,-0.319434907277172,
2.7818349079464));
#44458=CARTESIAN_POINT('Ctrl Pts',(-1.58906586793436,-0.158333333333339,
2.82636372819642));
#44459=CARTESIAN_POINT('Ctrl Pts',(-1.61768822563586,0.158333333333341,
2.83686870991166));
#44460=CARTESIAN_POINT('Ctrl Pts',(-1.63807626269469,0.31943490727718,2.80310903570228));
#44461=CARTESIAN_POINT('Ctrl Pts',(-1.68919790812606,0.636309800095232,
2.74835504104364));
#44462=CARTESIAN_POINT('Ctrl Pts',(-1.72180197162245,0.794772684000873,
2.69026507416506));
#44463=CARTESIAN_POINT('Ctrl Pts',(-1.78546486858486,1.06847604194562,2.64651824311741));
#44464=CARTESIAN_POINT('Ctrl Pts',(-1.81565969751708,1.18514270861275,2.63463881062376));
#44465=CARTESIAN_POINT('Ctrl Pts',(-1.84849204622925,1.30000000000141,2.62981632781718));
#44466=CARTESIAN_POINT('Ctrl Pts',(-1.62566884587422,-1.30000000000211,
2.52960364403045));
#44467=CARTESIAN_POINT('Ctrl Pts',(-1.60649968537675,-1.18514270861322,
2.53746013654931));
#44468=CARTESIAN_POINT('Ctrl Pts',(-1.59239171942472,-1.06847604194587,
2.55374804287688));
#44469=CARTESIAN_POINT('Ctrl Pts',(-1.57149186767519,-0.794772684000888,
2.61085461747457));
#44470=CARTESIAN_POINT('Ctrl Pts',(-1.57054210463338,-0.636309800095227,
2.68052984997528));
#44471=CARTESIAN_POINT('Ctrl Pts',(-1.57704051133011,-0.319434907277174,
2.75619800745381));
#44472=CARTESIAN_POINT('Ctrl Pts',(-1.58707769310611,-0.15833333333334,
2.80195951806694));
#44473=CARTESIAN_POINT('Ctrl Pts',(-1.61588562542525,0.158333333333342,
2.81248517859209));
#44474=CARTESIAN_POINT('Ctrl Pts',(-1.63540582925339,0.319434907277182,
2.77750541926282));
#44475=CARTESIAN_POINT('Ctrl Pts',(-1.68606052407164,0.636309800095236,
2.72275563596497));
#44476=CARTESIAN_POINT('Ctrl Pts',(-1.71823122031223,0.794772684000878,
2.66397315520516));
#44477=CARTESIAN_POINT('Ctrl Pts',(-1.78242013395345,1.06847604194563,2.62375631750794));
#44478=CARTESIAN_POINT('Ctrl Pts',(-1.8130888217976,1.18514270861275,2.61431643519053));
#44479=CARTESIAN_POINT('Ctrl Pts',(-1.84664119520423,1.30000000000142,2.61284504941418));
#44480=CARTESIAN_POINT('Ctrl Pts',(-1.62331482812817,-1.30000000000211,
2.51716170796398));
#44481=CARTESIAN_POINT('Ctrl Pts',(-1.60372347681876,-1.18514270861323,
2.52260971504939));
#44482=CARTESIAN_POINT('Ctrl Pts',(-1.58935222110575,-1.06847604194587,
2.53714147663927));
#44483=CARTESIAN_POINT('Ctrl Pts',(-1.56821121055313,-0.794772684000889,
2.59169804308482));
#44484=CARTESIAN_POINT('Ctrl Pts',(-1.56747946744677,-0.636309800095227,
2.66182785185384));
#44485=CARTESIAN_POINT('Ctrl Pts',(-1.57461975734037,-0.319434907277174,
2.73752053848879));
#44486=CARTESIAN_POINT('Ctrl Pts',(-1.58562722961563,-0.15833333333334,
2.78421941340941));
#44487=CARTESIAN_POINT('Ctrl Pts',(-1.6148195448593,0.158333333333342,2.79480947981818));
#44488=CARTESIAN_POINT('Ctrl Pts',(-1.63396495408773,0.319434907277182,
2.75900164171681));
#44489=CARTESIAN_POINT('Ctrl Pts',(-1.68433070412041,0.636309800095237,
2.70426710279089));
#44490=CARTESIAN_POINT('Ctrl Pts',(-1.71596433378824,0.794772684000879,
2.64493461636281));
#44491=CARTESIAN_POINT('Ctrl Pts',(-1.78038983077672,1.06847604194563,2.60725219541814));
#44492=CARTESIAN_POINT('Ctrl Pts',(-1.81134588447279,1.18514270861276,2.59957287367714));
#44493=CARTESIAN_POINT('Ctrl Pts',(-1.84537058141848,1.30000000000142,2.6005255539508));
#44494=CARTESIAN_POINT('Ctrl Pts',(-1.62120595304708,-1.30000000000211,
2.50778328167275));
#44495=CARTESIAN_POINT('Ctrl Pts',(-1.6010197698275,-1.18514270861323,2.51138821153288));
#44496=CARTESIAN_POINT('Ctrl Pts',(-1.58632213734058,-1.06847604194587,
2.52458646089038));
#44497=CARTESIAN_POINT('Ctrl Pts',(-1.56504731621779,-0.794772684000891,
2.5772395443827));
#44498=CARTESIAN_POINT('Ctrl Pts',(-1.56528632124749,-0.636309800095228,
2.64782812100501));
#44499=CARTESIAN_POINT('Ctrl Pts',(-1.57293731981988,-0.319434907277175,
2.72353329223748));
#44500=CARTESIAN_POINT('Ctrl Pts',(-1.58397757912001,-0.15833333333334,
2.7708141309076));
#44501=CARTESIAN_POINT('Ctrl Pts',(-1.61340988959623,0.158333333333342,
2.78144311075226));
#44502=CARTESIAN_POINT('Ctrl Pts',(-1.63265735838685,0.319434907277183,
2.74508128852036));
#44503=CARTESIAN_POINT('Ctrl Pts',(-1.68321543296914,0.636309800095237,
2.69043580026173));
#44504=CARTESIAN_POINT('Ctrl Pts',(-1.71492527071949,0.79477268400088,2.63078860133227));
#44505=CARTESIAN_POINT('Ctrl Pts',(-1.77949867744253,1.06847604194563,2.59500012320804));
#44506=CARTESIAN_POINT('Ctrl Pts',(-1.81051752399895,1.18514270861276,2.58861007352683));
#44507=CARTESIAN_POINT('Ctrl Pts',(-1.84460378202186,1.30000000000142,2.59132148025061));
#44508=CARTESIAN_POINT('Ctrl Pts',(-1.61998967096031,-1.30000000000212,
2.50231677111702));
#44509=CARTESIAN_POINT('Ctrl Pts',(-1.59944335020525,-1.18514270861323,
2.50484457426506));
#44510=CARTESIAN_POINT('Ctrl Pts',(-1.58454208979709,-1.06847604194588,
2.51726296944205));
#44511=CARTESIAN_POINT('Ctrl Pts',(-1.56315841595922,-0.794772684000892,
2.56880119278524));
#44512=CARTESIAN_POINT('Ctrl Pts',(-1.56393073117033,-0.63630980009523,
2.63965316376642));
#44513=CARTESIAN_POINT('Ctrl Pts',(-1.57187486651392,-0.319434907277175,
2.71536415798917));
#44514=CARTESIAN_POINT('Ctrl Pts',(-1.5829735170385,-0.15833333333334,2.7629886917636));
#44515=CARTESIAN_POINT('Ctrl Pts',(-1.61254266333681,0.158333333333343,
2.77363889973037));
#44516=CARTESIAN_POINT('Ctrl Pts',(-1.63181530847559,0.319434907277183,
2.73694898722863));
#44517=CARTESIAN_POINT('Ctrl Pts',(-1.68246747459253,0.636309800095239,
2.68235237036807));
#44518=CARTESIAN_POINT('Ctrl Pts',(-1.71420345164054,0.794772684000881,
2.62251781380482));
#44519=CARTESIAN_POINT('Ctrl Pts',(-1.77889739114558,1.06847604194563,2.58784029560954));
#44520=CARTESIAN_POINT('Ctrl Pts',(-1.8099805829054,1.18514270861276,2.58220738149782));
#44521=CARTESIAN_POINT('Ctrl Pts',(-1.84414335715996,1.30000000000143,2.58595216597246));
#44522=CARTESIAN_POINT('Ctrl Pts',(-1.61900425859119,-1.30000000000212,
2.49763984030326));
#44523=CARTESIAN_POINT('Ctrl Pts',(-1.59822013030825,-1.18514270861323,
2.49925493119758));
#44524=CARTESIAN_POINT('Ctrl Pts',(-1.58317352130879,-1.06847604194588,
2.51100928224148));
#44525=CARTESIAN_POINT('Ctrl Pts',(-1.56166766178791,-0.794772684000893,
2.56158790390019));
#44526=CARTESIAN_POINT('Ctrl Pts',(-1.56266468437642,-0.63630980009523,
2.63263142885374));
#44527=CARTESIAN_POINT('Ctrl Pts',(-1.57083050532711,-0.319434907277176,
2.7083436091765));
#44528=CARTESIAN_POINT('Ctrl Pts',(-1.58215381353722,-0.15833333333334,
2.75629009811465));
#44529=CARTESIAN_POINT('Ctrl Pts',(-1.61183972911496,0.158333333333343,
2.76695697053588));
#44530=CARTESIAN_POINT('Ctrl Pts',(-1.63102197382705,0.319434907277183,
2.72996647897455));
#44531=CARTESIAN_POINT('Ctrl Pts',(-1.68165468319656,0.636309800095239,
2.67539302301664));
#44532=CARTESIAN_POINT('Ctrl Pts',(-1.71329828605972,0.794772684000882,
2.61537529648118));
#44533=CARTESIAN_POINT('Ctrl Pts',(-1.7781446537935,1.06847604194563,2.58165950682896));
#44534=CARTESIAN_POINT('Ctrl Pts',(-1.80934725931507,1.18514270861276,2.57668799123382));
#44535=CARTESIAN_POINT('Ctrl Pts',(-1.84368288056094,1.30000000000143,2.5813392760909));
#44536=CARTESIAN_POINT('Ctrl Pts',(-1.61852730161631,-1.30000000000212,
2.49530381627404));
#44537=CARTESIAN_POINT('Ctrl Pts',(-1.59764011390879,-1.18514270861323,
2.4964648606895));
#44538=CARTESIAN_POINT('Ctrl Pts',(-1.58252720222537,-1.06847604194588,
2.50788812094456));
#44539=CARTESIAN_POINT('Ctrl Pts',(-1.56095308566473,-0.794772684000893,
2.55798590888769));
#44540=CARTESIAN_POINT('Ctrl Pts',(-1.56200858938868,-0.63630980009523,
2.62911727391898));
#44541=CARTESIAN_POINT('Ctrl Pts',(-1.57027928739533,-0.319434907277176,
2.70482939298503));
#44542=CARTESIAN_POINT('Ctrl Pts',(-1.58175670986222,-0.158333333333341,
2.75294354038181));
#44543=CARTESIAN_POINT('Ctrl Pts',(-1.61150219129874,0.158333333333343,
2.76361871218339));
#44544=CARTESIAN_POINT('Ctrl Pts',(-1.63061450625396,0.319434907277183,
2.72647371958498));
#44545=CARTESIAN_POINT('Ctrl Pts',(-1.68121352353356,0.636309800095239,
2.67190733464389));
#44546=CARTESIAN_POINT('Ctrl Pts',(-1.71278158764814,0.794772684000882,
2.6117921551272));
#44547=CARTESIAN_POINT('Ctrl Pts',(-1.77771405955071,1.06847604194563,2.5785591023655));
#44548=CARTESIAN_POINT('Ctrl Pts',(-1.80899089960785,1.18514270861276,2.5739210942678));
#44549=CARTESIAN_POINT('Ctrl Pts',(-1.84343771862066,1.30000000000143,2.57903043520702));
#44550=CARTESIAN_POINT('Ctrl Pts',(-1.61805756187616,-1.30000000000212,
2.49296899520644));
#44551=CARTESIAN_POINT('Ctrl Pts',(-1.59707587812017,-1.18514270861323,
2.49367732789126));
#44552=CARTESIAN_POINT('Ctrl Pts',(-1.58189991142332,-1.06847604194588,
2.50477002389613));
#44553=CARTESIAN_POINT('Ctrl Pts',(-1.56025276024826,-0.794772684000893,
2.55438632740748));
#44554=CARTESIAN_POINT('Ctrl Pts',(-1.56133713044918,-0.63630980009523,
2.62560110280928));
#44555=CARTESIAN_POINT('Ctrl Pts',(-1.56970645949404,-0.319434907277176,
2.70131223625752));
#44556=CARTESIAN_POINT('Ctrl Pts',(-1.58135592754541,-0.158333333333341,
2.74959680823923));
#44557=CARTESIAN_POINT('Ctrl Pts',(-1.61116114362569,0.158333333333343,
2.76028010748835));
#44558=CARTESIAN_POINT('Ctrl Pts',(-1.63019435625302,0.319434907277183,
2.72297900142918));
#44559=CARTESIAN_POINT('Ctrl Pts',(-1.68074877410949,0.636309800095239,
2.66841756142733));
#44560=CARTESIAN_POINT('Ctrl Pts',(-1.71222593475649,0.794772684000882,
2.60820195246472));
#44561=CARTESIAN_POINT('Ctrl Pts',(-1.77724894761959,1.06847604194563,2.57545233030315));
#44562=CARTESIAN_POINT('Ctrl Pts',(-1.80860698165484,1.18514270861276,2.57114907090689));
#44563=CARTESIAN_POINT('Ctrl Pts',(-1.84317699679694,1.30000000000143,2.57671865005504));
#44564=CARTESIAN_POINT('Ctrl Pts',(-1.61593270096015,-1.30000000000211,
2.48208353539143));
#44565=CARTESIAN_POINT('Ctrl Pts',(-1.59458499586163,-1.18514270861323,
2.48069034169533));
#44566=CARTESIAN_POINT('Ctrl Pts',(-1.57914568209439,-1.06847604194587,
2.49024505217354));
#44567=CARTESIAN_POINT('Ctrl Pts',(-1.55712734461286,-0.794772684000891,
2.53761019355471));
#44568=CARTESIAN_POINT('Ctrl Pts',(-1.55809913997242,-0.636309800095228,
2.60917757859137));
#44569=CARTESIAN_POINT('Ctrl Pts',(-1.56690123771344,-0.319434907277175,
2.68488108825686));
#44570=CARTESIAN_POINT('Ctrl Pts',(-1.57954395119173,-0.15833333333334,
2.73399152492558));
#44571=CARTESIAN_POINT('Ctrl Pts',(-1.6096330744329,0.158333333333342,2.74471260480286));
#44572=CARTESIAN_POINT('Ctrl Pts',(-1.62818552780862,0.319434907277182,
2.70666397085689));
#44573=CARTESIAN_POINT('Ctrl Pts',(-1.67841987641955,0.636309800095237,
2.65210450105468));
#44574=CARTESIAN_POINT('Ctrl Pts',(-1.70933004796508,0.794772684000879,
2.59139161815161));
#44575=CARTESIAN_POINT('Ctrl Pts',(-1.77482473182672,1.06847604194563,2.56090741895018));
#44576=CARTESIAN_POINT('Ctrl Pts',(-1.80663255816778,1.18514270861276,2.55818010876215));
#44577=CARTESIAN_POINT('Ctrl Pts',(-1.84189798902335,1.30000000000143,2.5659209686695));
#44578=CARTESIAN_POINT('Ctrl Pts',(-1.61289545439995,-1.30000000000208,
2.46881380796962));
#44579=CARTESIAN_POINT('Ctrl Pts',(-1.59055835390608,-1.1851427086132,2.46479767353596));
#44580=CARTESIAN_POINT('Ctrl Pts',(-1.57452299098335,-1.06847604194584,
2.47244942941252));
#44581=CARTESIAN_POINT('Ctrl Pts',(-1.5520363692162,-0.79477268400087,2.51708167698579));
#44582=CARTESIAN_POINT('Ctrl Pts',(-1.5543243501601,-0.636309800095212,
2.58928478249518));
#44583=CARTESIAN_POINT('Ctrl Pts',(-1.56347676621394,-0.319434907277167,
2.66493381116114));
#44584=CARTESIAN_POINT('Ctrl Pts',(-1.57565570893638,-0.158333333333336,
2.71476774826991));
#44585=CARTESIAN_POINT('Ctrl Pts',(-1.60606953040166,0.158333333333338,
2.7255321629494));
#44586=CARTESIAN_POINT('Ctrl Pts',(-1.62530771097436,0.319434907277174,
2.68679337701408));
#44587=CARTESIAN_POINT('Ctrl Pts',(-1.67606240579018,0.636309800095221,
2.63239699956226));
#44588=CARTESIAN_POINT('Ctrl Pts',(-1.70707773163962,0.79477268400086,2.57124503444124));
#44589=CARTESIAN_POINT('Ctrl Pts',(-1.77268191365742,1.0684760419456,2.54339878674876));
#44590=CARTESIAN_POINT('Ctrl Pts',(-1.80448939996189,1.18514270861273,2.54246350348996));
#44591=CARTESIAN_POINT('Ctrl Pts',(-1.83970675304978,1.30000000000139,2.55264654579327));
#44592=CARTESIAN_POINT('Ctrl Pts',(-1.6085954580606,-1.30000000000208,2.45008653506969));
#44593=CARTESIAN_POINT('Ctrl Pts',(-1.58521230478708,-1.18514270861319,
2.44242543180878));
#44594=CARTESIAN_POINT('Ctrl Pts',(-1.56850756594605,-1.06847604194584,
2.44742086826609));
#44595=CARTESIAN_POINT('Ctrl Pts',(-1.54534475080307,-0.794772684000867,
2.48820046449719));
#44596=CARTESIAN_POINT('Ctrl Pts',(-1.54820936146995,-0.636309800095211,
2.56110497709644));
#44597=CARTESIAN_POINT('Ctrl Pts',(-1.55853298333244,-0.319434907277166,
2.63679338908053));
#44598=CARTESIAN_POINT('Ctrl Pts',(-1.5725199715987,-0.158333333333336,
2.68804907051085));
#44599=CARTESIAN_POINT('Ctrl Pts',(-1.60347643686853,0.158333333333338,
2.69888149381968));
#44600=CARTESIAN_POINT('Ctrl Pts',(-1.62148176391517,0.319434907277173,
2.65879822403054));
#44601=CARTESIAN_POINT('Ctrl Pts',(-1.6721042809138,0.636309800095219,2.60448214661314));
#44602=CARTESIAN_POINT('Ctrl Pts',(-1.70346837844412,0.794772684000858,
2.54272074724158));
#44603=CARTESIAN_POINT('Ctrl Pts',(-1.76979719708233,1.0684760419456,2.51872721614525));
#44604=CARTESIAN_POINT('Ctrl Pts',(-1.80202329644897,1.18514270861272,2.52041860498502));
#44605=CARTESIAN_POINT('Ctrl Pts',(-1.83776420731868,1.30000000000139,2.53418729322825));
#44606=CARTESIAN_POINT('Ctrl Pts',(-1.60534913147455,-1.30000000000206,
2.43454767824767));
#44607=CARTESIAN_POINT('Ctrl Pts',(-1.58082296890353,-1.18514270861318,
2.42381174236594));
#44608=CARTESIAN_POINT('Ctrl Pts',(-1.5634146055833,-1.06847604194583,2.42657298233486));
#44609=CARTESIAN_POINT('Ctrl Pts',(-1.53964134396266,-0.794772684000859,
2.46413317536291));
#44610=CARTESIAN_POINT('Ctrl Pts',(-1.54379214603354,-0.636309800095206,
2.53773502783626));
#44611=CARTESIAN_POINT('Ctrl Pts',(-1.55467398927249,-0.319434907277165,
2.61338443365141));
#44612=CARTESIAN_POINT('Ctrl Pts',(-1.56874971205332,-0.158333333333334,
2.66560188014383));
#44613=CARTESIAN_POINT('Ctrl Pts',(-1.59993362305996,0.158333333333337,
2.67645941661085));
#44614=CARTESIAN_POINT('Ctrl Pts',(-1.61815211777964,0.31943490727717,2.63546438865947));
#44615=CARTESIAN_POINT('Ctrl Pts',(-1.66852804156187,0.636309800095214,
2.5811877643467));
#44616=CARTESIAN_POINT('Ctrl Pts',(-1.69854082941393,0.794772684000854,
2.51862531634145));
#44617=CARTESIAN_POINT('Ctrl Pts',(-1.76573087147969,1.06847604194559,2.49789326835724));
#44618=CARTESIAN_POINT('Ctrl Pts',(-1.79880622192406,1.18514270861272,2.501866430681));
#44619=CARTESIAN_POINT('Ctrl Pts',(-1.83587284323888,1.30000000000138,2.51878689070282));
#44620=CARTESIAN_POINT('Ctrl Pts',(-1.60198733594496,-1.30000000000205,
2.42200092146299));
#44621=CARTESIAN_POINT('Ctrl Pts',(-1.57696419153587,-1.18514270861317,
2.40887668461549));
#44622=CARTESIAN_POINT('Ctrl Pts',(-1.55920094320137,-1.06847604194582,
2.4098895933856));
#44623=CARTESIAN_POINT('Ctrl Pts',(-1.53493609829261,-0.794772684000851,
2.44488924977912));
#44624=CARTESIAN_POINT('Ctrl Pts',(-1.53902558372091,-0.636309800095197,
2.51889895831909));
#44625=CARTESIAN_POINT('Ctrl Pts',(-1.55037005382429,-0.319434907277159,
2.59451606221727));
#44626=CARTESIAN_POINT('Ctrl Pts',(-1.56533425685721,-0.158333333333332,
2.64760234942825));
#44627=CARTESIAN_POINT('Ctrl Pts',(-1.59715844965934,0.158333333333334,
2.65854012062382));
#44628=CARTESIAN_POINT('Ctrl Pts',(-1.61542530252264,0.319434907277167,
2.61680038082727));
#44629=CARTESIAN_POINT('Ctrl Pts',(-1.66603874291415,0.636309800095206,
2.56263008158386));
#44630=CARTESIAN_POINT('Ctrl Pts',(-1.69601474884685,0.79477268400084,2.49962533899737));
#44631=CARTESIAN_POINT('Ctrl Pts',(-1.76343954853272,1.06847604194558,2.48139778494711));
#44632=CARTESIAN_POINT('Ctrl Pts',(-1.79665188668013,1.1851427086127,2.48708204616755));
#44633=CARTESIAN_POINT('Ctrl Pts',(-1.83389086552595,1.30000000000136,2.50634060135935));
#44634=CARTESIAN_POINT('Ctrl Pts',(-1.60034588134944,-1.30000000000205,
2.41573690783759));
#44635=CARTESIAN_POINT('Ctrl Pts',(-1.57504122138986,-1.18514270861317,
2.40141459471707));
#44636=CARTESIAN_POINT('Ctrl Pts',(-1.55708435379931,-1.06847604194582,
2.40155144628234));
#44637=CARTESIAN_POINT('Ctrl Pts',(-1.53257526769946,-0.794772684000851,
2.43527116374521));
#44638=CARTESIAN_POINT('Ctrl Pts',(-1.53670704324099,-0.636309800095197,
2.50949324534634));
#44639=CARTESIAN_POINT('Ctrl Pts',(-1.54831342142086,-0.319434907277159,
2.58509892141659));
#44640=CARTESIAN_POINT('Ctrl Pts',(-1.56375557866725,-0.158333333333332,
2.63862740032413));
#44641=CARTESIAN_POINT('Ctrl Pts',(-1.59581317861656,0.158333333333334,
2.64959190996706));
#44642=CARTESIAN_POINT('Ctrl Pts',(-1.61390936643398,0.319434907277167,
2.60744757149566));
#44643=CARTESIAN_POINT('Ctrl Pts',(-1.66458583994602,0.636309800095206,
2.55332105438581));
#44644=CARTESIAN_POINT('Ctrl Pts',(-1.69463294550622,0.79477268400084,2.49010824790527));
#44645=CARTESIAN_POINT('Ctrl Pts',(-1.76226517728142,1.06847604194558,2.47314938073029));
#44646=CARTESIAN_POINT('Ctrl Pts',(-1.79559295568808,1.1851427086127,2.47969831528682));
#44647=CARTESIAN_POINT('Ctrl Pts',(-1.83297302538704,1.30000000000136,2.50013704961196));
#44648=CARTESIAN_POINT('',(-1.81613517243772,1.2,2.59520325796734));
#44649=CARTESIAN_POINT('Ctrl Pts',(-1.81613517243772,1.2,2.59520325796734));
#44650=CARTESIAN_POINT('Ctrl Pts',(-1.82250678261496,1.21684007853956,2.61581873774569));
#44651=CARTESIAN_POINT('Ctrl Pts',(-1.83001234347906,1.23321800531665,2.63645045406549));
#44652=CARTESIAN_POINT('Ctrl Pts',(-1.84225408385894,1.26589996427597,2.67664972145215));
#44653=CARTESIAN_POINT('Ctrl Pts',(-1.8510324951693,1.28855401991379,2.70473410601027));
#44654=CARTESIAN_POINT('Ctrl Pts',(-1.85490568620932,1.30000000000138,2.71872508149132));
#44655=CARTESIAN_POINT('',(-1.66957757316342,0.653834841343326,2.54006322716652));
#44656=CARTESIAN_POINT('Ctrl Pts',(-1.66957757323826,0.653834841326689,
2.54006322715213));
#44657=CARTESIAN_POINT('Ctrl Pts',(-1.68487397676607,0.717899058900883,
2.54554367324531));
#44658=CARTESIAN_POINT('Ctrl Pts',(-1.69802885347761,0.767415508768553,
2.55032811960476));
#44659=CARTESIAN_POINT('Ctrl Pts',(-1.74589484775824,0.949818223351814,
2.56798214841286));
#44660=CARTESIAN_POINT('Ctrl Pts',(-1.77255449741379,1.04964523963697,2.5780150081523));
#44661=CARTESIAN_POINT('Ctrl Pts',(-1.81613517243772,1.2,2.59520325796734));
#44662=CARTESIAN_POINT('',(-1.53759581372214,-0.653834841531101,2.49486460198815));
#44663=CARTESIAN_POINT('Ctrl Pts',(-1.53759581372214,-0.6538348415311,2.49486460198815));
#44664=CARTESIAN_POINT('Ctrl Pts',(-1.54253896106846,-0.575773996990663,
2.5362541007448));
#44665=CARTESIAN_POINT('Ctrl Pts',(-1.54771098720326,-0.493714162387373,
2.57104087379186));
#44666=CARTESIAN_POINT('Ctrl Pts',(-1.55721339216251,-0.337911306543783,
2.62081608951078));
#44667=CARTESIAN_POINT('Ctrl Pts',(-1.56181618753724,-0.265423834229001,
2.63812662410482));
#44668=CARTESIAN_POINT('Ctrl Pts',(-1.57204015447595,-0.129509891678934,
2.66019653582912));
#44669=CARTESIAN_POINT('Ctrl Pts',(-1.57737847383145,-0.0665328266301909,
2.66641946766735));
#44670=CARTESIAN_POINT('Ctrl Pts',(-1.58979323208528,0.0594341807793119,
2.67106517994948));
#44671=CARTESIAN_POINT('Ctrl Pts',(-1.59693716234678,0.122550355968248,
2.66953017416603));
#44672=CARTESIAN_POINT('Ctrl Pts',(-1.61359765438044,0.259896461491062,
2.65729142037106));
#44673=CARTESIAN_POINT('Ctrl Pts',(-1.62330966879801,0.333789134744896,
2.64494004755738));
#44674=CARTESIAN_POINT('Ctrl Pts',(-1.64492474574799,0.491517033436927,
2.60552673792889));
#44675=CARTESIAN_POINT('Ctrl Pts',(-1.65731436333269,0.574921799602958,
2.57626786129867));
#44676=CARTESIAN_POINT('Ctrl Pts',(-1.66957757326119,0.6538348413646,2.540063227246));
#44677=CARTESIAN_POINT('',(-1.6061456467244,-1.2,2.51782142998494));
#44678=CARTESIAN_POINT('Ctrl Pts',(-1.6061456467244,-1.2,2.51782142998494));
#44679=CARTESIAN_POINT('Ctrl Pts',(-1.59629030340056,-1.14500162986664,
2.51444071382048));
#44680=CARTESIAN_POINT('Ctrl Pts',(-1.58195573524929,-1.06328611335836,
2.50954158073653));
#44681=CARTESIAN_POINT('Ctrl Pts',(-1.54495003427023,-0.766654883195457,
2.49724355903312));
#44682=CARTESIAN_POINT('Ctrl Pts',(-1.54083638237218,-0.699422956716546,
2.49592359059717));
#44683=CARTESIAN_POINT('Ctrl Pts',(-1.53759581372214,-0.653834841531101,
2.49486460198815));
#44684=CARTESIAN_POINT('Ctrl Pts',(-1.64377746965492,-1.30000000000001,
2.63705187074685));
#44685=CARTESIAN_POINT('Ctrl Pts',(-1.63611465680649,-1.27671330627714,
2.60953974040605));
#44686=CARTESIAN_POINT('Ctrl Pts',(-1.63296016223809,-1.27025479401098,
2.60156608361734));
#44687=CARTESIAN_POINT('Ctrl Pts',(-1.6216712464152,-1.2389971406116,2.5644647456061));
#44688=CARTESIAN_POINT('Ctrl Pts',(-1.6142786492348,-1.21821497175287,2.53986819629468));
#44689=CARTESIAN_POINT('Ctrl Pts',(-1.6061456467244,-1.2,2.51782142998494));
#44690=CARTESIAN_POINT('Origin',(0.,1.25,7.2));
#44691=CARTESIAN_POINT('Origin',(0.,1.2,7.2));
#44692=CARTESIAN_POINT('Origin',(0.,0.92691742076555,7.2));
#44693=CARTESIAN_POINT('Origin',(0.,0.653834841531101,7.2));
#44694=CARTESIAN_POINT('Origin',(0.,0.,7.2));
#44695=CARTESIAN_POINT('Origin',(0.,-0.653834841531101,7.2));
#44696=CARTESIAN_POINT('Origin',(0.,-0.926917420765551,7.2));
#44697=CARTESIAN_POINT('Origin',(0.,-1.2,7.2));
#44698=CARTESIAN_POINT('Origin',(0.,-1.25,7.2));
#44699=CARTESIAN_POINT('Ctrl Pts',(-1.27960380226531,-1.30000000000134,
2.32033648972617));
#44700=CARTESIAN_POINT('Ctrl Pts',(-1.32185850051481,-1.18514270861269,
2.32577266001068));
#44701=CARTESIAN_POINT('Ctrl Pts',(-1.35267060678123,-1.06847604194558,
2.34006403729773));
#44702=CARTESIAN_POINT('Ctrl Pts',(-1.39741805963368,-0.794772684000851,
2.39353727746485));
#44703=CARTESIAN_POINT('Ctrl Pts',(-1.38457112325749,-0.636309800095196,
2.46233875769595));
#44704=CARTESIAN_POINT('Ctrl Pts',(-1.39375448302828,-0.319434907277159,
2.53591491365396));
#44705=CARTESIAN_POINT('Ctrl Pts',(-1.38362278588515,-0.158333333333332,
2.58064707201462));
#44706=CARTESIAN_POINT('Ctrl Pts',(-1.41600270610974,0.158333333333334,
2.5906195818525));
#44707=CARTESIAN_POINT('Ctrl Pts',(-1.45995892423147,0.319434907277167,
2.55639080502576));
#44708=CARTESIAN_POINT('Ctrl Pts',(-1.51378858280534,0.636309800095206,
2.50204658614216));
#44709=CARTESIAN_POINT('Ctrl Pts',(-1.56075790439375,0.79477268400084,2.44442825750267));
#44710=CARTESIAN_POINT('Ctrl Pts',(-1.56074958985878,1.06847604194605,2.40274235367243));
#44711=CARTESIAN_POINT('Ctrl Pts',(-1.54630261814451,1.18514270861363,2.39207685648188));
#44712=CARTESIAN_POINT('Ctrl Pts',(-1.51741227377006,1.30000000000274,2.38879014525401));
#44713=CARTESIAN_POINT('Ctrl Pts',(-1.27082599327781,-1.30000000000134,
2.32929506146048));
#44714=CARTESIAN_POINT('Ctrl Pts',(-1.31146501795783,-1.18514270861269,
2.33647493942641));
#44715=CARTESIAN_POINT('Ctrl Pts',(-1.34107385349419,-1.06847604194558,
2.35202967938385));
#44716=CARTESIAN_POINT('Ctrl Pts',(-1.3839942433067,-0.794772684000851,
2.40731184698627));
#44717=CARTESIAN_POINT('Ctrl Pts',(-1.37127685908323,-0.636309800095196,
2.47569309018433));
#44718=CARTESIAN_POINT('Ctrl Pts',(-1.38030676013404,-0.319434907277159,
2.54926598726038));
#44719=CARTESIAN_POINT('Ctrl Pts',(-1.37092683910606,-0.158333333333332,
2.59354411999748));
#44720=CARTESIAN_POINT('Ctrl Pts',(-1.40289766570327,0.158333333333334,
2.60328550699441));
#44721=CARTESIAN_POINT('Ctrl Pts',(-1.44556071014892,0.319434907277167,
2.56921034248006));
#44722=CARTESIAN_POINT('Ctrl Pts',(-1.49898002676599,0.636309800095206,
2.51453974159158));
#44723=CARTESIAN_POINT('Ctrl Pts',(-1.54563126199517,0.79477268400084,2.45721532481951));
#44724=CARTESIAN_POINT('Ctrl Pts',(-1.54752279646356,1.06847604194605,2.41374555903559));
#44725=CARTESIAN_POINT('Ctrl Pts',(-1.53441897429966,1.18514270861363,2.40189018458686));
#44726=CARTESIAN_POINT('Ctrl Pts',(-1.50739255478877,1.30000000000274,2.39699588658379));
#44727=CARTESIAN_POINT('Ctrl Pts',(-1.25382084875496,-1.30000000000134,
2.34740604253439));
#44728=CARTESIAN_POINT('Ctrl Pts',(-1.28972468822729,-1.18514270861269,
2.35739030091737));
#44729=CARTESIAN_POINT('Ctrl Pts',(-1.31607146455883,-1.06847604194558,
2.3750904551144));
#44730=CARTESIAN_POINT('Ctrl Pts',(-1.35485906080004,-0.794772684000855,
2.43380661510325));
#44731=CARTESIAN_POINT('Ctrl Pts',(-1.34486661414017,-0.6363098000952,2.50253171557404));
#44732=CARTESIAN_POINT('Ctrl Pts',(-1.35423783295285,-0.319434907277161,
2.57641427780022));
#44733=CARTESIAN_POINT('Ctrl Pts',(-1.34545299100441,-0.158333333333334,
2.61932084915137));
#44734=CARTESIAN_POINT('Ctrl Pts',(-1.37684147327064,0.158333333333336,
2.62873770546943));
#44735=CARTESIAN_POINT('Ctrl Pts',(-1.41790578277615,0.319434907277172,
2.59551147340387));
#44736=CARTESIAN_POINT('Ctrl Pts',(-1.47065576940973,0.636309800095213,
2.54027367362798));
#44737=CARTESIAN_POINT('Ctrl Pts',(-1.51577444849718,0.794772684000848,
2.48306023107429));
#44738=CARTESIAN_POINT('Ctrl Pts',(-1.52150372805259,1.06847604194606,2.43601887531454));
#44739=CARTESIAN_POINT('Ctrl Pts',(-1.5112701521532,1.18514270861364,2.42186535768253));
#44740=CARTESIAN_POINT('Ctrl Pts',(-1.48832300752561,1.30000000000274,2.41392078227297));
#44741=CARTESIAN_POINT('Ctrl Pts',(-1.23606661107331,-1.30000000000135,
2.36612763766972));
#44742=CARTESIAN_POINT('Ctrl Pts',(-1.26952116487824,-1.1851427086127,2.38014288421496));
#44743=CARTESIAN_POINT('Ctrl Pts',(-1.29391544109559,-1.06847604194558,
2.40071154454898));
#44744=CARTESIAN_POINT('Ctrl Pts',(-1.32934004548617,-0.794772684000857,
2.46336896152491));
#44745=CARTESIAN_POINT('Ctrl Pts',(-1.31845784775975,-0.636309800095201,
2.53067644404618));
#44746=CARTESIAN_POINT('Ctrl Pts',(-1.32710927339012,-0.319434907277161,
2.60436541489617));
#44747=CARTESIAN_POINT('Ctrl Pts',(-1.31985493597403,-0.158333333333333,
2.64631125420172));
#44748=CARTESIAN_POINT('Ctrl Pts',(-1.35060848262527,0.158333333333336,
2.65538195322451));
#44749=CARTESIAN_POINT('Ctrl Pts',(-1.38976931133031,0.319434907277169,
2.62290932667077));
#44750=CARTESIAN_POINT('Ctrl Pts',(-1.44141218068745,0.63630980009521,2.56687682513414));
#44751=CARTESIAN_POINT('Ctrl Pts',(-1.48444786746984,0.794772684000846,
2.5095245660064));
#44752=CARTESIAN_POINT('Ctrl Pts',(-1.49401219558044,1.06847604194606,2.45872137820305));
#44753=CARTESIAN_POINT('Ctrl Pts',(-1.48679726350359,1.18514270861364,2.44221646020226));
#44754=CARTESIAN_POINT('Ctrl Pts',(-1.46822735610409,1.30000000000275,2.4311974417572));
#44755=CARTESIAN_POINT('Ctrl Pts',(-1.22651188656258,-1.30000000000135,
2.37636511902976));
#44756=CARTESIAN_POINT('Ctrl Pts',(-1.25763623352574,-1.1851427086127,2.39212732521069));
#44757=CARTESIAN_POINT('Ctrl Pts',(-1.28039582820086,-1.06847604194559,
2.41400536023505));
#44758=CARTESIAN_POINT('Ctrl Pts',(-1.31365079379327,-0.794772684000859,
2.47867678592274));
#44759=CARTESIAN_POINT('Ctrl Pts',(-1.30374727333792,-0.636309800095202,
2.54590402804441));
#44760=CARTESIAN_POINT('Ctrl Pts',(-1.31267808242576,-0.319434907277161,
2.61981138305767));
#44761=CARTESIAN_POINT('Ctrl Pts',(-1.30636129182997,-0.158333333333333,
2.66127968119591));
#44762=CARTESIAN_POINT('Ctrl Pts',(-1.33678585930284,0.158333333333336,
2.67017251962692));
#44763=CARTESIAN_POINT('Ctrl Pts',(-1.37441375777697,0.31943490727717,2.6378700495204));
#44764=CARTESIAN_POINT('Ctrl Pts',(-1.42564978301686,0.636309800095211,
2.58152070592476));
#44765=CARTESIAN_POINT('Ctrl Pts',(-1.46848285180204,0.794772684000847,
2.52459274777525));
#44766=CARTESIAN_POINT('Ctrl Pts',(-1.48013482532484,1.06847604194606,2.47172882045556));
#44767=CARTESIAN_POINT('Ctrl Pts',(-1.47436292824239,1.18514270861364,2.45382693016231));
#44768=CARTESIAN_POINT('Ctrl Pts',(-1.45777542648761,1.30000000000275,2.44090598491105));
#44769=CARTESIAN_POINT('Ctrl Pts',(-1.22442444283596,-1.30000000000135,
2.37865686158716));
#44770=CARTESIAN_POINT('Ctrl Pts',(-1.25505289579091,-1.1851427086127,2.39481804511272));
#44771=CARTESIAN_POINT('Ctrl Pts',(-1.27746084760478,-1.06847604194559,
2.41699283710455));
#44772=CARTESIAN_POINT('Ctrl Pts',(-1.31023669684865,-0.794772684000858,
2.48211368123284));
#44773=CARTESIAN_POINT('Ctrl Pts',(-1.30050800650126,-0.636309800095202,
2.54930273424566));
#44774=CARTESIAN_POINT('Ctrl Pts',(-1.30948713094632,-0.319434907277161,
2.62325238428033));
#44775=CARTESIAN_POINT('Ctrl Pts',(-1.3033888994581,-0.158333333333333,
2.66461967637659));
#44776=CARTESIAN_POINT('Ctrl Pts',(-1.33374295960405,0.158333333333336,
2.6734746150652));
#44777=CARTESIAN_POINT('Ctrl Pts',(-1.37104104789581,0.31943490727717,2.64121584584354));
#44778=CARTESIAN_POINT('Ctrl Pts',(-1.42216813151107,0.636309800095211,
2.58478653561258));
#44779=CARTESIAN_POINT('Ctrl Pts',(-1.46490901723515,0.794772684000847,
2.52792818187656));
#44780=CARTESIAN_POINT('Ctrl Pts',(-1.47701727843428,1.06847604194606,2.47460218551256));
#44781=CARTESIAN_POINT('Ctrl Pts',(-1.47157205898242,1.18514270861364,2.45639289956961));
#44782=CARTESIAN_POINT('Ctrl Pts',(-1.45544040246087,1.30000000000275,2.44305717558686));
#44783=CARTESIAN_POINT('Ctrl Pts',(-1.22080579827408,-1.30000000000135,
2.38268464037354));
#44784=CARTESIAN_POINT('Ctrl Pts',(-1.25061899143135,-1.1851427086127,2.39956860112986));
#44785=CARTESIAN_POINT('Ctrl Pts',(-1.27244311645034,-1.06847604194558,
2.42227751873145));
#44786=CARTESIAN_POINT('Ctrl Pts',(-1.30440486553836,-0.794772684000858,
2.48819647688559));
#44787=CARTESIAN_POINT('Ctrl Pts',(-1.29492903164232,-0.636309800095202,
2.55529457763855));
#44788=CARTESIAN_POINT('Ctrl Pts',(-1.3039387637522,-0.319434907277161,
2.62929274909087));
#44789=CARTESIAN_POINT('Ctrl Pts',(-1.29815594019608,-0.158333333333334,
2.67045024651218));
#44790=CARTESIAN_POINT('Ctrl Pts',(-1.32838573362059,0.158333333333336,
2.67923917825606));
#44791=CARTESIAN_POINT('Ctrl Pts',(-1.36520310306176,0.31943490727717,2.64710577115188));
#44792=CARTESIAN_POINT('Ctrl Pts',(-1.41613006072221,0.636309800095211,
2.59053101975602));
#44793=CARTESIAN_POINT('Ctrl Pts',(-1.45859660002129,0.794772684000847,
2.53373553247143));
#44794=CARTESIAN_POINT('Ctrl Pts',(-1.4714859764512,1.06847604194606,2.47959175086073));
#44795=CARTESIAN_POINT('Ctrl Pts',(-1.46662397060643,1.18514270861364,2.46085052592493));
#44796=CARTESIAN_POINT('Ctrl Pts',(-1.45132062545884,1.30000000000275,2.44680491288787));
#44797=CARTESIAN_POINT('Ctrl Pts',(-1.21577198318697,-1.30000000000135,
2.38850735409311));
#44798=CARTESIAN_POINT('Ctrl Pts',(-1.24465532214333,-1.1851427086127,2.40653337468798));
#44799=CARTESIAN_POINT('Ctrl Pts',(-1.26578380340772,-1.06847604194558,
2.43006992306755));
#44800=CARTESIAN_POINT('Ctrl Pts',(-1.29667954924419,-0.794772684000858,
2.49717447985452));
#44801=CARTESIAN_POINT('Ctrl Pts',(-1.28729106307725,-0.636309800095202,
2.56401627618933));
#44802=CARTESIAN_POINT('Ctrl Pts',(-1.29612334487574,-0.319434907277161,
2.63797875212365));
#44803=CARTESIAN_POINT('Ctrl Pts',(-1.29056461674117,-0.158333333333333,
2.67872437044246));
#44804=CARTESIAN_POINT('Ctrl Pts',(-1.32062377343709,0.158333333333336,
2.6874253957819));
#44805=CARTESIAN_POINT('Ctrl Pts',(-1.35713237397202,0.319434907277169,
2.65566379602382));
#44806=CARTESIAN_POINT('Ctrl Pts',(-1.4077141062757,0.636309800095211,2.59884824539572));
#44807=CARTESIAN_POINT('Ctrl Pts',(-1.44928781318403,0.794772684000847,
2.54188064926633));
#44808=CARTESIAN_POINT('Ctrl Pts',(-1.46323621952018,1.06847604194606,2.48653823443745));
#44809=CARTESIAN_POINT('Ctrl Pts',(-1.4592733781514,1.18514270861364,2.46707138622253));
#44810=CARTESIAN_POINT('Ctrl Pts',(-1.44530994715028,1.30000000000275,2.45209337053365));
#44811=CARTESIAN_POINT('Ctrl Pts',(-1.20972245596778,-1.30000000000135,
2.39549447794725));
#44812=CARTESIAN_POINT('Ctrl Pts',(-1.237498558214,-1.1851427086127,2.4148965304242));
#44813=CARTESIAN_POINT('Ctrl Pts',(-1.25780946550937,-1.06847604194558,
2.43943527698712));
#44814=CARTESIAN_POINT('Ctrl Pts',(-1.28748563080113,-0.794772684000858,
2.50799148143747));
#44815=CARTESIAN_POINT('Ctrl Pts',(-1.27829104603458,-0.636309800095201,
2.57456596436313));
#44816=CARTESIAN_POINT('Ctrl Pts',(-1.28695534553385,-0.319434907277161,
2.64850621105546));
#44817=CARTESIAN_POINT('Ctrl Pts',(-1.2816533068698,-0.158333333333333,
2.68875081698848));
#44818=CARTESIAN_POINT('Ctrl Pts',(-1.31147697540735,0.158333333333336,
2.69733396568411));
#44819=CARTESIAN_POINT('Ctrl Pts',(-1.34754226237417,0.31943490727717,2.66598781839734));
#44820=CARTESIAN_POINT('Ctrl Pts',(-1.39771277198078,0.636309800095211,
2.60888856392443));
#44821=CARTESIAN_POINT('Ctrl Pts',(-1.43834600690956,0.794772684000846,
2.55178056358252));
#44822=CARTESIAN_POINT('Ctrl Pts',(-1.45351266470549,1.06847604194606,2.49497238712087));
#44823=CARTESIAN_POINT('Ctrl Pts',(-1.450568752393,1.18514270861364,2.47460353456611));
#44824=CARTESIAN_POINT('Ctrl Pts',(-1.43811584358821,1.30000000000275,2.45845598409654));
#44825=CARTESIAN_POINT('Ctrl Pts',(-1.20140969808998,-1.30000000000135,
2.40469480865862));
#44826=CARTESIAN_POINT('Ctrl Pts',(-1.2273339447754,-1.1851427086127,2.42575973931006));
#44827=CARTESIAN_POINT('Ctrl Pts',(-1.24634695325279,-1.06847604194558,
2.45154000943944));
#44828=CARTESIAN_POINT('Ctrl Pts',(-1.27430446352586,-0.794772684000857,
2.52199096825796));
#44829=CARTESIAN_POINT('Ctrl Pts',(-1.2658664144435,-0.636309800095202,
2.58843684601312));
#44830=CARTESIAN_POINT('Ctrl Pts',(-1.27481917442567,-0.319434907277161,
2.66258895868815));
#44831=CARTESIAN_POINT('Ctrl Pts',(-1.2704285554692,-0.158333333333333,
2.70243931345991));
#44832=CARTESIAN_POINT('Ctrl Pts',(-1.29994796313376,0.158333333333336,
2.71086864410593));
#44833=CARTESIAN_POINT('Ctrl Pts',(-1.33461834788419,0.319434907277169,
2.67968218340169));
#44834=CARTESIAN_POINT('Ctrl Pts',(-1.38424570108484,0.636309800095211,
2.62222222152023));
#44835=CARTESIAN_POINT('Ctrl Pts',(-1.42444637983391,0.794772684000847,
2.56536279772913));
#44836=CARTESIAN_POINT('Ctrl Pts',(-1.44132255025392,1.06847604194606,2.50664038232994));
#44837=CARTESIAN_POINT('Ctrl Pts',(-1.4396328321968,1.18514270861364,2.4850086975055));
#44838=CARTESIAN_POINT('Ctrl Pts',(-1.42894832723144,1.30000000000275,2.4671640856031));
#44839=CARTESIAN_POINT('Ctrl Pts',(-1.19097545539289,-1.30000000000135,
2.41618611254718));
#44840=CARTESIAN_POINT('Ctrl Pts',(-1.21459984897074,-1.1851427086127,2.43934036867706));
#44841=CARTESIAN_POINT('Ctrl Pts',(-1.23198527911806,-1.06847604194558,
2.46667277011588));
#44842=CARTESIAN_POINT('Ctrl Pts',(-1.25773584707679,-0.794772684000856,
2.53946843676631));
#44843=CARTESIAN_POINT('Ctrl Pts',(-1.25010458507922,-0.636309800095201,
2.605689091021));
#44844=CARTESIAN_POINT('Ctrl Pts',(-1.25935605916739,-0.319434907277161,
2.68007355808535));
#44845=CARTESIAN_POINT('Ctrl Pts',(-1.25607343829891,-0.158333333333333,
2.71940706193143));
#44846=CARTESIAN_POINT('Ctrl Pts',(-1.28535661586508,0.158333333333336,
2.72771186106723));
#44847=CARTESIAN_POINT('Ctrl Pts',(-1.3186670069989,0.31943490727717,2.69691930460369));
#44848=CARTESIAN_POINT('Ctrl Pts',(-1.36754657543854,0.636309800095211,
2.63897009843824));
#44849=CARTESIAN_POINT('Ctrl Pts',(-1.40664865630924,0.794772684000846,
2.5821337587119));
#44850=CARTESIAN_POINT('Ctrl Pts',(-1.42552979444646,1.06847604194606,2.52095287146528));
#44851=CARTESIAN_POINT('Ctrl Pts',(-1.42543679622289,1.18514270861364,2.49775939915589));
#44852=CARTESIAN_POINT('Ctrl Pts',(-1.41707785469123,1.30000000000275,2.477855393651));
#44853=CARTESIAN_POINT('Ctrl Pts',(-1.17502706764918,-1.30000000000135,
2.43492203179261));
#44854=CARTESIAN_POINT('Ctrl Pts',(-1.19560300398521,-1.1851427086127,2.4617154878452));
#44855=CARTESIAN_POINT('Ctrl Pts',(-1.21082849739992,-1.06847604194558,
2.49173942274355));
#44856=CARTESIAN_POINT('Ctrl Pts',(-1.23364183953669,-0.794772684000853,
2.56856377101498));
#44857=CARTESIAN_POINT('Ctrl Pts',(-1.22731190864551,-0.636309800095201,
2.63442149983078));
#44858=CARTESIAN_POINT('Ctrl Pts',(-1.23645105326258,-0.319434907277162,
2.70890849458993));
#44859=CARTESIAN_POINT('Ctrl Pts',(-1.23384956357613,-0.158333333333333,
2.74691835519408));
#44860=CARTESIAN_POINT('Ctrl Pts',(-1.26201512338157,0.158333333333336,
2.75469106909033));
#44861=CARTESIAN_POINT('Ctrl Pts',(-1.29284074214967,0.319434907277169,
2.72437826502062));
#44862=CARTESIAN_POINT('Ctrl Pts',(-1.34095351347016,0.636309800095211,
2.66587783741269));
#44863=CARTESIAN_POINT('Ctrl Pts',(-1.37977554459473,0.794772684000847,
2.60983700343105));
#44864=CARTESIAN_POINT('Ctrl Pts',(-1.40211676589996,1.06847604194606,2.54483262312023));
#44865=CARTESIAN_POINT('Ctrl Pts',(-1.40441378045019,1.18514270861364,2.51904198433771));
#44866=CARTESIAN_POINT('Ctrl Pts',(-1.39933712267143,1.30000000000275,2.49559869435967));
#44867=CARTESIAN_POINT('Ctrl Pts',(-1.15904906517621,-1.30000000000135,
2.4536662687705));
#44868=CARTESIAN_POINT('Ctrl Pts',(-1.17661739972832,-1.1851427086127,2.48411798698703));
#44869=CARTESIAN_POINT('Ctrl Pts',(-1.18960431632116,-1.06847604194559,
2.51679950600914));
#44870=CARTESIAN_POINT('Ctrl Pts',(-1.20902269967893,-0.794772684000857,
2.59745163879659));
#44871=CARTESIAN_POINT('Ctrl Pts',(-1.20286196424972,-0.6363098000952,2.66244534596457));
#44872=CARTESIAN_POINT('Ctrl Pts',(-1.21188397483891,-0.31943490727716,
2.73703530247258));
#44873=CARTESIAN_POINT('Ctrl Pts',(-1.21065438480207,-0.158333333333333,
2.77401500061943));
#44874=CARTESIAN_POINT('Ctrl Pts',(-1.23889099773402,0.158333333333335,
2.78181435464434));
#44875=CARTESIAN_POINT('Ctrl Pts',(-1.26888848540362,0.319434907277168,
2.75279259424705));
#44876=CARTESIAN_POINT('Ctrl Pts',(-1.31630023357142,0.636309800095209,
2.69376633668697));
#44877=CARTESIAN_POINT('Ctrl Pts',(-1.352883146608,0.794772684000843,2.6375618120723));
#44878=CARTESIAN_POINT('Ctrl Pts',(-1.37811171409883,1.06847604194606,2.56845034247818));
#44879=CARTESIAN_POINT('Ctrl Pts',(-1.38279858713534,1.18514270861364,2.54006106243875));
#44880=CARTESIAN_POINT('Ctrl Pts',(-1.38125182115209,1.30000000000275,2.51319829671497));
#44881=CARTESIAN_POINT('Ctrl Pts',(-1.14511474947587,-1.30000000000135,
2.47009903743856));
#44882=CARTESIAN_POINT('Ctrl Pts',(-1.15981125650959,-1.1851427086127,2.50366280614491));
#44883=CARTESIAN_POINT('Ctrl Pts',(-1.17089890385113,-1.06847604194558,
2.53870677723349));
#44884=CARTESIAN_POINT('Ctrl Pts',(-1.1881763994475,-0.794772684000857,
2.62308492458678));
#44885=CARTESIAN_POINT('Ctrl Pts',(-1.18438946463272,-0.636309800095201,
2.68828438577407));
#44886=CARTESIAN_POINT('Ctrl Pts',(-1.19381691865822,-0.31943490727716,
2.76318909900355));
#44887=CARTESIAN_POINT('Ctrl Pts',(-1.19285882411596,-0.158333333333333,
2.79887261784234));
#44888=CARTESIAN_POINT('Ctrl Pts',(-1.21995946483943,0.158333333333335,
2.80616514085504));
#44889=CARTESIAN_POINT('Ctrl Pts',(-1.24796444411868,0.319434907277168,
2.77770066340956));
#44890=CARTESIAN_POINT('Ctrl Pts',(-1.29384854100992,0.636309800095209,
2.71779997124574));
#44891=CARTESIAN_POINT('Ctrl Pts',(-1.32848976308691,0.794772684000844,
2.66145357782913));
#44892=CARTESIAN_POINT('Ctrl Pts',(-1.35641019534391,1.06847604194606,2.58881860913373));
#44893=CARTESIAN_POINT('Ctrl Pts',(-1.36338321274031,1.18514270861364,2.55824206200308));
#44894=CARTESIAN_POINT('Ctrl Pts',(-1.36524352696298,1.30000000000275,2.52852995429933));
#44895=CARTESIAN_POINT('Ctrl Pts',(-1.13743240009045,-1.30000000000135,
2.47962282172612));
#44896=CARTESIAN_POINT('Ctrl Pts',(-1.1509959570983,-1.1851427086127,2.5151804811712));
#44897=CARTESIAN_POINT('Ctrl Pts',(-1.16118204640611,-1.06847604194558,
2.55165123117717));
#44898=CARTESIAN_POINT('Ctrl Pts',(-1.17691132438011,-0.794772684000856,
2.63801538149813));
#44899=CARTESIAN_POINT('Ctrl Pts',(-1.1726240599699,-0.6363098000952,2.70253446010115));
#44900=CARTESIAN_POINT('Ctrl Pts',(-1.18192552938848,-0.31943490727716,
2.77746372964283));
#44901=CARTESIAN_POINT('Ctrl Pts',(-1.18191990276965,-0.158333333333333,
2.81274083764786));
#44902=CARTESIAN_POINT('Ctrl Pts',(-1.20919352209051,0.158333333333335,
2.82011139846522));
#44903=CARTESIAN_POINT('Ctrl Pts',(-1.23670432785443,0.319434907277169,
2.79225951297756));
#44904=CARTESIAN_POINT('Ctrl Pts',(-1.28248558653756,0.636309800095209,
2.73223220317571));
#44905=CARTESIAN_POINT('Ctrl Pts',(-1.3165906333875,0.794772684000844,2.67611720090248));
#44906=CARTESIAN_POINT('Ctrl Pts',(-1.34585334028077,1.06847604194606,2.60137585827352));
#44907=CARTESIAN_POINT('Ctrl Pts',(-1.35381729827139,1.18514270861364,2.56939118976514));
#44908=CARTESIAN_POINT('Ctrl Pts',(-1.35707847272864,1.30000000000275,2.5377746105329));
#44909=CARTESIAN_POINT('Ctrl Pts',(-1.12587093071343,-1.30000000000135,
2.49388678129842));
#44910=CARTESIAN_POINT('Ctrl Pts',(-1.13743996805866,-1.1851427086127,2.5323131421853));
#44911=CARTESIAN_POINT('Ctrl Pts',(-1.14620340056342,-1.06847604194558,
2.57089746517517));
#44912=CARTESIAN_POINT('Ctrl Pts',(-1.15996717432731,-0.794772684000856,
2.66039989410707));
#44913=CARTESIAN_POINT('Ctrl Pts',(-1.15625211606956,-0.6363098000952,2.7244683950529));
#44914=CARTESIAN_POINT('Ctrl Pts',(-1.16583526707528,-0.31943490727716,
2.79963620118662));
#44915=CARTESIAN_POINT('Ctrl Pts',(-1.16728340571542,-0.158333333333333,
2.83431784556207));
#44916=CARTESIAN_POINT('Ctrl Pts',(-1.19374519866423,0.158333333333335,
2.84132697013958));
#44917=CARTESIAN_POINT('Ctrl Pts',(-1.2185960758806,0.319434907277168,2.81354432854277));
#44918=CARTESIAN_POINT('Ctrl Pts',(-1.26324525701596,0.636309800095209,
2.75287791467498));
#44919=CARTESIAN_POINT('Ctrl Pts',(-1.29706389338153,0.794772684000844,
2.69730718173339));
#44920=CARTESIAN_POINT('Ctrl Pts',(-1.3285043772527,1.06847604194606,2.61948048286637));
#44921=CARTESIAN_POINT('Ctrl Pts',(-1.33805819666283,1.18514270861364,2.58543820887738));
#44922=CARTESIAN_POINT('Ctrl Pts',(-1.34355641499993,1.30000000000275,2.55104195507566));
#44923=CARTESIAN_POINT('Ctrl Pts',(-1.10877976373815,-1.30000000000134,
2.51539512337627));
#44924=CARTESIAN_POINT('Ctrl Pts',(-1.11700749000313,-1.18514270861269,
2.55799245825637));
#44925=CARTESIAN_POINT('Ctrl Pts',(-1.12347620234645,-1.06847604194558,
2.59968793273419));
#44926=CARTESIAN_POINT('Ctrl Pts',(-1.13435654787238,-0.794772684000852,
2.69392934198306));
#44927=CARTESIAN_POINT('Ctrl Pts',(-1.13261330572799,-0.636309800095198,
2.75776369374303));
#44928=CARTESIAN_POINT('Ctrl Pts',(-1.14248599893863,-0.31943490727716,
2.83322910662972));
#44929=CARTESIAN_POINT('Ctrl Pts',(-1.14444452168738,-0.158333333333333,
2.86630795981827));
#44930=CARTESIAN_POINT('Ctrl Pts',(-1.17037651905704,0.158333333333335,
2.87310697666088));
#44931=CARTESIAN_POINT('Ctrl Pts',(-1.19418540652733,0.319434907277169,
2.84675453602205));
#44932=CARTESIAN_POINT('Ctrl Pts',(-1.23746957696803,0.636309800095209,
2.78528612061526));
#44933=CARTESIAN_POINT('Ctrl Pts',(-1.26831972181169,0.794772684000843,
2.72939423054381));
#44934=CARTESIAN_POINT('Ctrl Pts',(-1.30248061882999,1.06847604194605,2.64668881184621));
#44935=CARTESIAN_POINT('Ctrl Pts',(-1.31452253467142,1.18514270861363,2.60960180882215));
#44936=CARTESIAN_POINT('Ctrl Pts',(-1.32381937982096,1.30000000000274,2.57122791399057));
#44937=CARTESIAN_POINT('Ctrl Pts',(-1.08708000619844,-1.30000000000135,
2.5445357914544));
#44938=CARTESIAN_POINT('Ctrl Pts',(-1.09153397709107,-1.1851427086127,2.59298467877558));
#44939=CARTESIAN_POINT('Ctrl Pts',(-1.09529707688984,-1.06847604194558,
2.63898235718083));
#44940=CARTESIAN_POINT('Ctrl Pts',(-1.10239453979543,-0.794772684000857,
2.73958341314233));
#44941=CARTESIAN_POINT('Ctrl Pts',(-1.10156616025283,-0.636309800095197,
2.80240803093196));
#44942=CARTESIAN_POINT('Ctrl Pts',(-1.11201856565858,-0.319434907277157,
2.87835347963024));
#44943=CARTESIAN_POINT('Ctrl Pts',(-1.11656121087504,-0.158333333333332,
2.91006832634054));
#44944=CARTESIAN_POINT('Ctrl Pts',(-1.14185015937106,0.158333333333334,
2.91661637012575));
#44945=CARTESIAN_POINT('Ctrl Pts',(-1.16236219873307,0.319434907277167,
2.89137191942179));
#44946=CARTESIAN_POINT('Ctrl Pts',(-1.20389873928152,0.636309800095206,
2.82892252737393));
#44947=CARTESIAN_POINT('Ctrl Pts',(-1.23300565158259,0.794772684000839,
2.77365267741555));
#44948=CARTESIAN_POINT('Ctrl Pts',(-1.27070968714585,1.06847604194605,2.68440060237138));
#44949=CARTESIAN_POINT('Ctrl Pts',(-1.28557693600659,1.18514270861364,2.6430140566728));
#44950=CARTESIAN_POINT('Ctrl Pts',(-1.29899075380489,1.30000000000275,2.59887488144712));
#44951=CARTESIAN_POINT('Ctrl Pts',(-1.06835320849412,-1.30000000000135,
2.56859872678655));
#44952=CARTESIAN_POINT('Ctrl Pts',(-1.0697813225491,-1.18514270861269,2.62196120870789));
#44953=CARTESIAN_POINT('Ctrl Pts',(-1.07155378605604,-1.06847604194558,
2.67163925621292));
#44954=CARTESIAN_POINT('Ctrl Pts',(-1.07644404745808,-0.79477268400085,
2.77789370343844));
#44955=CARTESIAN_POINT('Ctrl Pts',(-1.07803733404953,-0.636309800095198,
2.84052147891033));
#44956=CARTESIAN_POINT('Ctrl Pts',(-1.08928731240602,-0.31943490727716,
2.91697449291878));
#44957=CARTESIAN_POINT('Ctrl Pts',(-1.09475033976786,-0.158333333333333,
2.9470431617148));
#44958=CARTESIAN_POINT('Ctrl Pts',(-1.11909912332319,0.158333333333335,
2.95324376931968));
#44959=CARTESIAN_POINT('Ctrl Pts',(-1.13758418362336,0.319434907277168,
2.92928290322638));
#44960=CARTESIAN_POINT('Ctrl Pts',(-1.17674711288214,0.636309800095208,
2.86564911735402));
#44961=CARTESIAN_POINT('Ctrl Pts',(-1.20212657848975,0.794772684000843,
2.80989517576845));
#44962=CARTESIAN_POINT('Ctrl Pts',(-1.24245750708116,1.06847604194606,2.71506152057097));
#44963=CARTESIAN_POINT('Ctrl Pts',(-1.25999884660707,1.18514270861364,2.67024063466379));
#44964=CARTESIAN_POINT('Ctrl Pts',(-1.27762376107978,1.30000000000274,2.62164883825135));
#44965=CARTESIAN_POINT('Ctrl Pts',(-1.05521937382473,-1.30000000000134,
2.58857464166986));
#44966=CARTESIAN_POINT('Ctrl Pts',(-1.05450214504509,-1.18514270861269,
2.64600090835846));
#44967=CARTESIAN_POINT('Ctrl Pts',(-1.0547849652932,-1.06847604194558,2.69868073338192));
#44968=CARTESIAN_POINT('Ctrl Pts',(-1.05774864995755,-0.79477268400085,
2.80941643797989));
#44969=CARTESIAN_POINT('Ctrl Pts',(-1.06047170225705,-0.636309800095197,
2.87155013435134));
#44970=CARTESIAN_POINT('Ctrl Pts',(-1.07184295676916,-0.319434907277159,
2.94821501020616));
#44971=CARTESIAN_POINT('Ctrl Pts',(-1.07789632591925,-0.158333333333333,
2.97692628369926));
#44972=CARTESIAN_POINT('Ctrl Pts',(-1.10146318465323,0.158333333333335,
2.9828505963045));
#44973=CARTESIAN_POINT('Ctrl Pts',(-1.11825852721492,0.319434907277168,
2.95986988768039));
#44974=CARTESIAN_POINT('Ctrl Pts',(-1.15635408084972,0.636309800095208,
2.89566706022621));
#44975=CARTESIAN_POINT('Ctrl Pts',(-1.1806416071217,0.79477268400084,2.84040087167772));
#44976=CARTESIAN_POINT('Ctrl Pts',(-1.22293951039675,1.06847604194605,2.74103002569047));
#44977=CARTESIAN_POINT('Ctrl Pts',(-1.24208305449305,1.18514270861364,2.69320736685689));
#44978=CARTESIAN_POINT('Ctrl Pts',(-1.26206094764959,1.30000000000275,2.64057600636506));
#44979=CARTESIAN_POINT('Ctrl Pts',(-1.03796310307453,-1.30000000000135,
2.61321937129804));
#44980=CARTESIAN_POINT('Ctrl Pts',(-1.03433234523134,-1.18514270861269,
2.67561294783302));
#44981=CARTESIAN_POINT('Ctrl Pts',(-1.03271434407037,-1.06847604194558,
2.73201023194115));
#44982=CARTESIAN_POINT('Ctrl Pts',(-1.033626308295,-0.794772684000851,2.84844660540857));
#44983=CARTESIAN_POINT('Ctrl Pts',(-1.03850907849285,-0.6363098000952,2.91024159152785));
#44984=CARTESIAN_POINT('Ctrl Pts',(-1.05131116122678,-0.319434907277162,
2.98762987114524));
#44985=CARTESIAN_POINT('Ctrl Pts',(-1.05962760847544,-0.158333333333333,
3.01518593090444));
#44986=CARTESIAN_POINT('Ctrl Pts',(-1.08233494867452,0.158333333333335,
3.02082749843731));
#44987=CARTESIAN_POINT('Ctrl Pts',(-1.09569345115491,0.319434907277167,
2.99864727175407));
#44988=CARTESIAN_POINT('Ctrl Pts',(-1.13124749047663,0.636309800095208,
2.93329174095001));
#44989=CARTESIAN_POINT('Ctrl Pts',(-1.15328508084511,0.794772684000849,
2.8782315917722));
#44990=CARTESIAN_POINT('Ctrl Pts',(-1.19758716438919,1.06847604194606,2.77303275852799));
#44991=CARTESIAN_POINT('Ctrl Pts',(-1.21872779041347,1.18514270861363,2.7214776851753));
#44992=CARTESIAN_POINT('Ctrl Pts',(-1.24183231204969,1.30000000000274,2.66390421538058));
#44993=CARTESIAN_POINT('Ctrl Pts',(-1.02154978498825,-1.30000000000134,
2.63823699667444));
#44994=CARTESIAN_POINT('Ctrl Pts',(-1.01574801095058,-1.18514270861269,
2.70592424384903));
#44995=CARTESIAN_POINT('Ctrl Pts',(-1.01274478987735,-1.06847604194558,
2.76626480042087));
#44996=CARTESIAN_POINT('Ctrl Pts',(-1.01227196560235,-0.794772684000852,
2.88869123219581));
#44997=CARTESIAN_POINT('Ctrl Pts',(-1.01930980404299,-0.636309800095198,
2.95010834994269));
#44998=CARTESIAN_POINT('Ctrl Pts',(-1.03274236210258,-0.319434907277159,
3.02792458695197));
#44999=CARTESIAN_POINT('Ctrl Pts',(-1.04142778207386,-0.158333333333333,
3.05362693099543));
#45000=CARTESIAN_POINT('Ctrl Pts',(-1.06328150122981,0.158333333333335,
3.05901061254694));
#45001=CARTESIAN_POINT('Ctrl Pts',(-1.07529158151554,0.319434907277169,
3.03843229550797));
#45002=CARTESIAN_POINT('Ctrl Pts',(-1.10873268435927,0.636309800095208,
2.97211112779765));
#45003=CARTESIAN_POINT('Ctrl Pts',(-1.12729379095584,0.794772684000842,
2.91684284841793));
#45004=CARTESIAN_POINT('Ctrl Pts',(-1.17336497585264,1.06847604194605,2.80568738725448));
#45005=CARTESIAN_POINT('Ctrl Pts',(-1.19654495568478,1.18514270861363,2.75037781389277));
#45006=CARTESIAN_POINT('Ctrl Pts',(-1.22296240651279,1.30000000000274,2.68787374759144));
#45007=CARTESIAN_POINT('Ctrl Pts',(-1.00569178470089,-1.30000000000134,
2.66339442293999));
#45008=CARTESIAN_POINT('Ctrl Pts',(-0.997606978305174,-1.18514270861269,
2.73622462125294));
#45009=CARTESIAN_POINT('Ctrl Pts',(-0.993275950842555,-1.06847604194558,
2.8004366432757));
#45010=CARTESIAN_POINT('Ctrl Pts',(-0.991942391261186,-0.794772684000851,
2.92886954842842));
#45011=CARTESIAN_POINT('Ctrl Pts',(-1.00208124996111,-0.6363098000952,2.99016914190514));
#45012=CARTESIAN_POINT('Ctrl Pts',(-1.01716774717545,-0.319434907277161,
3.06873680081757));
#45013=CARTESIAN_POINT('Ctrl Pts',(-1.02709000963087,-0.158333333333333,
3.09295577357895));
#45014=CARTESIAN_POINT('Ctrl Pts',(-1.04799004253004,0.158333333333335,
3.0980870815083));
#45015=CARTESIAN_POINT('Ctrl Pts',(-1.05741527487675,0.319434907277167,
3.07866838013204));
#45016=CARTESIAN_POINT('Ctrl Pts',(-1.0880630481429,0.636309800095208,3.01122712361042));
#45017=CARTESIAN_POINT('Ctrl Pts',(-1.10367721439058,0.794772684000846,
2.95603375362214));
#45018=CARTESIAN_POINT('Ctrl Pts',(-1.15053474805594,1.06847604194606,2.83869111901186));
#45019=CARTESIAN_POINT('Ctrl Pts',(-1.17507666076872,1.18514270861364,2.77943677977267));
#45020=CARTESIAN_POINT('Ctrl Pts',(-1.20387759611321,1.30000000000274,2.71172137984417));
#45021=CARTESIAN_POINT('Ctrl Pts',(-0.996652854808941,-1.30000000000134,
2.67874859209622));
#45022=CARTESIAN_POINT('Ctrl Pts',(-0.987235389768998,-1.18514270861269,
2.75484304608189));
#45023=CARTESIAN_POINT('Ctrl Pts',(-0.982190625604162,-1.06847604194558,
2.821528134996));
#45024=CARTESIAN_POINT('Ctrl Pts',(-0.980638024959095,-0.794772684000851,
2.95384651504136));
#45025=CARTESIAN_POINT('Ctrl Pts',(-0.993843850297619,-0.636309800095197,
3.01544607135719));
#45026=CARTESIAN_POINT('Ctrl Pts',(-1.00867880744322,-0.319434907277159,
3.09407798413982));
#45027=CARTESIAN_POINT('Ctrl Pts',(-1.01591199130173,-0.158333333333333,
3.11624435624655));
#45028=CARTESIAN_POINT('Ctrl Pts',(-1.03574610618998,0.158333333333335,
3.12107189416699));
#45029=CARTESIAN_POINT('Ctrl Pts',(-1.04619476393307,0.319434907277169,
3.10325045211595));
#45030=CARTESIAN_POINT('Ctrl Pts',(-1.07614449642726,0.636309800095208,
3.0354349239545));
#45031=CARTESIAN_POINT('Ctrl Pts',(-1.08941717942122,0.794772684000842,
2.98008553500352));
#45032=CARTESIAN_POINT('Ctrl Pts',(-1.13692092038242,1.06847604194605,2.85890915084214));
#45033=CARTESIAN_POINT('Ctrl Pts',(-1.16240855078136,1.18514270861363,2.79721822163055));
#45034=CARTESIAN_POINT('Ctrl Pts',(-1.19282120230414,1.30000000000274,2.7262891298835));
#45035=CARTESIAN_POINT('Ctrl Pts',(-0.988985336877648,-1.30000000000134,
2.69137107011124));
#45036=CARTESIAN_POINT('Ctrl Pts',(-0.979333756628179,-1.18514270861269,
2.77022516793836));
#45037=CARTESIAN_POINT('Ctrl Pts',(-0.973943685309453,-1.06847604194558,
2.83886483367411));
#45038=CARTESIAN_POINT('Ctrl Pts',(-0.971336480425084,-0.794772684000853,
2.97383881132026));
#45039=CARTESIAN_POINT('Ctrl Pts',(-0.983182267165968,-0.636309800095197,
3.03441947199261));
#45040=CARTESIAN_POINT('Ctrl Pts',(-0.997214190673696,-0.319434907277159,
3.11282563491179));
#45041=CARTESIAN_POINT('Ctrl Pts',(-1.00444416170132,-0.158333333333332,
3.13400485249189));
#45042=CARTESIAN_POINT('Ctrl Pts',(-1.02482927490377,0.158333333333335,
3.13902963959976));
#45043=CARTESIAN_POINT('Ctrl Pts',(-1.03666257867743,0.319434907277168,
3.12266994496896));
#45044=CARTESIAN_POINT('Ctrl Pts',(-1.0668461526339,0.636309800095207,3.0549170199033));
#45045=CARTESIAN_POINT('Ctrl Pts',(-1.07844903019705,0.794772684000841,
2.99962093111457));
#45046=CARTESIAN_POINT('Ctrl Pts',(-1.12660470913759,1.06847604194605,2.87562122050712));
#45047=CARTESIAN_POINT('Ctrl Pts',(-1.15281925740509,1.18514270861363,2.8120697940746));
#45048=CARTESIAN_POINT('Ctrl Pts',(-1.18440354487041,1.30000000000274,2.73864182128965));
#45049=CARTESIAN_POINT('Ctrl Pts',(-0.98053380401763,-1.30000000000134,
2.70691834098162));
#45050=CARTESIAN_POINT('Ctrl Pts',(-0.970516247771153,-1.18514270861269,
2.78946589370654));
#45051=CARTESIAN_POINT('Ctrl Pts',(-0.964456204955913,-1.06847604194558,
2.86069494939743));
#45052=CARTESIAN_POINT('Ctrl Pts',(-0.959598941469317,-0.794772684000851,
2.99910032496074));
#45053=CARTESIAN_POINT('Ctrl Pts',(-0.968405938412429,-0.636309800095197,
3.05813977615298));
#45054=CARTESIAN_POINT('Ctrl Pts',(-0.980318422822977,-0.319434907277159,
3.13605005232135));
#45055=CARTESIAN_POINT('Ctrl Pts',(-0.987526841201364,-0.158333333333332,
3.15590188031775));
#45056=CARTESIAN_POINT('Ctrl Pts',(-1.00780526691801,0.158333333333334,
3.16091545903217));
#45057=CARTESIAN_POINT('Ctrl Pts',(-1.01986572741626,0.319434907277167,
3.14599156573793));
#45058=CARTESIAN_POINT('Ctrl Pts',(-1.05131531031871,0.636309800095207,
3.07846803910757));
#45059=CARTESIAN_POINT('Ctrl Pts',(-1.06417222310146,0.794772684000841,
3.02411831903424));
#45060=CARTESIAN_POINT('Ctrl Pts',(-1.11441663505319,1.06847604194605,2.89657730305442));
#45061=CARTESIAN_POINT('Ctrl Pts',(-1.14162671491763,1.18514270861363,2.83050655264808));
#45062=CARTESIAN_POINT('Ctrl Pts',(-1.17429793045148,1.30000000000274,2.75357283179291));
#45063=CARTESIAN_POINT('Ctrl Pts',(-0.974665092423499,-1.30000000000134,
2.71746251872114));
#45064=CARTESIAN_POINT('Ctrl Pts',(-0.965682205213172,-1.18514270861269,
2.80294609442062));
#45065=CARTESIAN_POINT('Ctrl Pts',(-0.959681817346756,-1.06847604194558,
2.87601139807284));
#45066=CARTESIAN_POINT('Ctrl Pts',(-0.952709891133253,-0.794772684000851,
3.01611817347715));
#45067=CARTESIAN_POINT('Ctrl Pts',(-0.955698270378832,-0.636309800095196,
3.07217548853748));
#45068=CARTESIAN_POINT('Ctrl Pts',(-0.964465402259397,-0.319434907277159,
3.14860911293493));
#45069=CARTESIAN_POINT('Ctrl Pts',(-0.972209900210543,-0.158333333333332,
3.16753349812413));
#45070=CARTESIAN_POINT('Ctrl Pts',(-0.992336747193892,0.158333333333334,
3.17245788736581));
#45071=CARTESIAN_POINT('Ctrl Pts',(-1.00385002392357,0.319434907277167,
3.15835068493109));
#45072=CARTESIAN_POINT('Ctrl Pts',(-1.03785006787198,0.636309800095206,
3.09216605874643));
#45073=CARTESIAN_POINT('Ctrl Pts',(-1.05542731230797,0.79477268400084,3.04072080217647));
#45074=CARTESIAN_POINT('Ctrl Pts',(-1.10785601153169,1.06847604194605,2.9114906887883));
#45075=CARTESIAN_POINT('Ctrl Pts',(-1.1353239790356,1.18514270861363,2.84362042448228));
#45076=CARTESIAN_POINT('Ctrl Pts',(-1.16756547282413,1.30000000000274,2.76381882350857));
#45077=CARTESIAN_POINT('Ctrl Pts',(-0.968408877628683,-1.30000000000134,
2.72336636313462));
#45078=CARTESIAN_POINT('Ctrl Pts',(-0.959587680307202,-1.18514270861269,
2.80865755213462));
#45079=CARTESIAN_POINT('Ctrl Pts',(-0.953418388257857,-1.06847604194558,
2.88142219435957));
#45080=CARTESIAN_POINT('Ctrl Pts',(-0.945292521151705,-0.794772684000851,
3.02058424543828));
#45081=CARTESIAN_POINT('Ctrl Pts',(-0.94601257756158,-0.636309800095196,
3.07544248806072));
#45082=CARTESIAN_POINT('Ctrl Pts',(-0.953320013133083,-0.319434907277159,
3.151031219842));
#45083=CARTESIAN_POINT('Ctrl Pts',(-0.961064002623635,-0.158333333333332,
3.17000794893273));
#45084=CARTESIAN_POINT('Ctrl Pts',(-0.98099760953902,0.158333333333334,
3.17479542438189));
#45085=CARTESIAN_POINT('Ctrl Pts',(-0.992074216468526,0.319434907277167,
3.16036137717658));
#45086=CARTESIAN_POINT('Ctrl Pts',(-1.0276372251559,0.636309800095206,3.09502301503918));
#45087=CARTESIAN_POINT('Ctrl Pts',(-1.04845566442809,0.79477268400084,3.04525442796451));
#45088=CARTESIAN_POINT('Ctrl Pts',(-1.10189571121762,1.06847604194605,2.91691192436669));
#45089=CARTESIAN_POINT('Ctrl Pts',(-1.12924033300979,1.18514270861363,2.84921214392821));
#45090=CARTESIAN_POINT('Ctrl Pts',(-1.16079736048773,1.30000000000274,2.76936729730053));
#45091=CARTESIAN_POINT('Ctrl Pts',(-0.96840887762858,-1.3,2.72336636313561));
#45092=CARTESIAN_POINT('Ctrl Pts',(-0.959587680307154,-1.18514270861178,
2.80865755213519));
#45093=CARTESIAN_POINT('Ctrl Pts',(-0.953418388257844,-1.06847604194512,
2.88142219435981));
#45094=CARTESIAN_POINT('Ctrl Pts',(-0.945292521151705,-0.794772684000851,
3.02058424543828));
#45095=CARTESIAN_POINT('Ctrl Pts',(-0.94601257756158,-0.636309800095197,
3.07544248806072));
#45096=CARTESIAN_POINT('Ctrl Pts',(-0.953320013133083,-0.319434907277159,
3.151031219842));
#45097=CARTESIAN_POINT('Ctrl Pts',(-0.961064002623635,-0.158333333333332,
3.17000794893273));
#45098=CARTESIAN_POINT('Ctrl Pts',(-0.98099760953902,0.158333333333334,
3.17479542438189));
#45099=CARTESIAN_POINT('Ctrl Pts',(-0.992074216468526,0.319434907277167,
3.16036137717658));
#45100=CARTESIAN_POINT('Ctrl Pts',(-1.0276372251559,0.636309800095206,3.09502301503918));
#45101=CARTESIAN_POINT('Ctrl Pts',(-1.04845566442809,0.79477268400084,3.04525442796451));
#45102=CARTESIAN_POINT('Ctrl Pts',(-1.10189571121744,1.06847604194511,2.91691192436713));
#45103=CARTESIAN_POINT('Ctrl Pts',(-1.12924033300935,1.18514270861178,2.84921214392929));
#45104=CARTESIAN_POINT('Ctrl Pts',(-1.16079736048697,1.3,2.76936729730244));
#45105=CARTESIAN_POINT('',(-1.23744115436766,-1.2,2.40716791557672));
#45106=CARTESIAN_POINT('Ctrl Pts',(-1.23744115436766,-1.2,2.40716791557672));
#45107=CARTESIAN_POINT('Ctrl Pts',(-1.21281665208152,-1.22396325414416,
2.42555928291992));
#45108=CARTESIAN_POINT('Ctrl Pts',(-1.18823777366837,-1.2466437811891,2.44279487554561));
#45109=CARTESIAN_POINT('Ctrl Pts',(-1.16766532598256,-1.26666346483997,
2.45830035953809));
#45110=CARTESIAN_POINT('Ctrl Pts',(-1.15334387624282,-1.28037911840962,
2.46890623939148));
#45111=CARTESIAN_POINT('Ctrl Pts',(-1.13360931448736,-1.30000000000135,
2.48434204780559));
#45112=CARTESIAN_POINT('',(-1.38832545990542,-0.653834841419392,2.44867887665694));
#45113=CARTESIAN_POINT('Ctrl Pts',(-1.38832545991004,-0.653834841418722,
2.44867887663172));
#45114=CARTESIAN_POINT('Ctrl Pts',(-1.37270162777471,-0.717985758094171,
2.44411362764694));
#45115=CARTESIAN_POINT('Ctrl Pts',(-1.35994621619342,-0.764036487774388,
2.44044932934856));
#45116=CARTESIAN_POINT('Ctrl Pts',(-1.31012606770028,-0.949550441354697,
2.42639500235851));
#45117=CARTESIAN_POINT('Ctrl Pts',(-1.28369169731409,-1.04640534543883,
2.41910914870269));
#45118=CARTESIAN_POINT('Ctrl Pts',(-1.23744115436766,-1.2,2.40716791557672));
#45119=CARTESIAN_POINT('',(-1.52166805320867,0.653834841531101,2.48968935888044));
#45120=CARTESIAN_POINT('Ctrl Pts',(-1.52166805320867,0.653834841531103,
2.48968935888044));
#45121=CARTESIAN_POINT('Ctrl Pts',(-1.49343059891966,0.57602138259582,2.52017174762599));
#45122=CARTESIAN_POINT('Ctrl Pts',(-1.4690466730557,0.493680047789112,2.54546585877262));
#45123=CARTESIAN_POINT('Ctrl Pts',(-1.43213691154417,0.338203658968698,
2.58010273751869));
#45124=CARTESIAN_POINT('Ctrl Pts',(-1.41824662923231,0.265719696696191,
2.59141317455489));
#45125=CARTESIAN_POINT('Ctrl Pts',(-1.39691207797798,0.129748505774919,
2.60327111496509));
#45126=CARTESIAN_POINT('Ctrl Pts',(-1.38884650422918,0.0666446497396744,
2.60515759811574));
#45127=CARTESIAN_POINT('Ctrl Pts',(-1.37599030069352,-0.0595546290449114,
2.6015928052966));
#45128=CARTESIAN_POINT('Ctrl Pts',(-1.37109828489627,-0.122804233593781,
2.59613105082614));
#45129=CARTESIAN_POINT('Ctrl Pts',(-1.36475418668873,-0.260164762898064,
2.57638174285244));
#45130=CARTESIAN_POINT('Ctrl Pts',(-1.3640889993582,-0.333966755798492,
2.56066651484078));
#45131=CARTESIAN_POINT('Ctrl Pts',(-1.36961752260919,-0.491159093464661,
2.51618010434666));
#45132=CARTESIAN_POINT('Ctrl Pts',(-1.37686721292842,-0.574266001747902,
2.48547919212961));
#45133=CARTESIAN_POINT('Ctrl Pts',(-1.38832545986823,-0.653834841430835,
2.4486788766701));
#45134=CARTESIAN_POINT('',(-1.45284569372596,1.2,2.46800894017942));
#45135=CARTESIAN_POINT('Ctrl Pts',(-1.45284569372596,1.2,2.46800894017942));
#45136=CARTESIAN_POINT('Ctrl Pts',(-1.46404686295214,1.1381078493845,2.47144799369182));
#45137=CARTESIAN_POINT('Ctrl Pts',(-1.48005000616772,1.04094628811002,2.47640896356757));
#45138=CARTESIAN_POINT('Ctrl Pts',(-1.510530945921,0.796143969855592,2.48608811667857));
#45139=CARTESIAN_POINT('Ctrl Pts',(-1.51543685031566,0.741398697530247,
2.48767636587472));
#45140=CARTESIAN_POINT('Ctrl Pts',(-1.52166805320867,0.653834841531101,
2.48968935888044));
#45141=CARTESIAN_POINT('Ctrl Pts',(-1.35239702227521,1.30000000000275,2.54236945495733));
#45142=CARTESIAN_POINT('Ctrl Pts',(-1.35320800708816,1.29919411843786,2.54176576771413));
#45143=CARTESIAN_POINT('Ctrl Pts',(-1.35401460134667,1.29838796377945,2.54116064183015));
#45144=CARTESIAN_POINT('Ctrl Pts',(-1.37051248407318,1.28165666458978,2.52853345157028));
#45145=CARTESIAN_POINT('Ctrl Pts',(-1.38637763270161,1.26578864929006,2.51666625640002));
#45146=CARTESIAN_POINT('Ctrl Pts',(-1.41410479224254,1.23782621524452,2.49576387472157));
#45147=CARTESIAN_POINT('Ctrl Pts',(-1.43176600496645,1.21970424320237,2.48214896452996));
#45148=CARTESIAN_POINT('Ctrl Pts',(-1.45284569372596,1.2,2.46800894017942));
#45149=CARTESIAN_POINT('Ctrl Pts',(-0.96840887762858,-1.3,2.72336636313561));
#45150=CARTESIAN_POINT('Ctrl Pts',(-0.959587680307154,-1.18514270861178,
2.80865755213519));
#45151=CARTESIAN_POINT('Ctrl Pts',(-0.953418388257843,-1.06847604194512,
2.88142219435981));
#45152=CARTESIAN_POINT('Ctrl Pts',(-0.945292521151706,-0.794772684000851,
3.02058424543828));
#45153=CARTESIAN_POINT('Ctrl Pts',(-0.946012577561581,-0.636309800095197,
3.07544248806072));
#45154=CARTESIAN_POINT('Ctrl Pts',(-0.953320013133084,-0.319434907277159,
3.151031219842));
#45155=CARTESIAN_POINT('Ctrl Pts',(-0.961064002623636,-0.158333333333332,
3.17000794893273));
#45156=CARTESIAN_POINT('Ctrl Pts',(-0.98099760953902,0.158333333333334,
3.17479542438189));
#45157=CARTESIAN_POINT('Ctrl Pts',(-0.992074216468526,0.319434907277167,
3.16036137717658));
#45158=CARTESIAN_POINT('Ctrl Pts',(-1.0276372251559,0.636309800095206,3.09502301503918));
#45159=CARTESIAN_POINT('Ctrl Pts',(-1.04845566442809,0.79477268400084,3.04525442796451));
#45160=CARTESIAN_POINT('Ctrl Pts',(-1.10189571121744,1.06847604194511,2.91691192436713));
#45161=CARTESIAN_POINT('Ctrl Pts',(-1.12924033300935,1.18514270861178,2.84921214392929));
#45162=CARTESIAN_POINT('Ctrl Pts',(-1.16079736048698,1.3,2.76936729730244));
#45163=CARTESIAN_POINT('Ctrl Pts',(-0.892825757179276,-1.3,2.70900317484779));
#45164=CARTESIAN_POINT('Ctrl Pts',(-0.885729277039984,-1.18514270861178,
2.79445639963879));
#45165=CARTESIAN_POINT('Ctrl Pts',(-0.880764606872678,-1.06847604194512,
2.86728912331394));
#45166=CARTESIAN_POINT('Ctrl Pts',(-0.874220133109745,-0.794772684000851,
3.00639140283985));
#45167=CARTESIAN_POINT('Ctrl Pts',(-0.874292131581308,-0.636309800095197,
3.06094139417448));
#45168=CARTESIAN_POINT('Ctrl Pts',(-0.881134728284516,-0.319434907277159,
3.13605199626587));
#45169=CARTESIAN_POINT('Ctrl Pts',(-0.88771343062497,-0.158333333333332,
3.15460028905268));
#45170=CARTESIAN_POINT('Ctrl Pts',(-0.907721667816887,0.158333333333334,
3.15903665665579));
#45171=CARTESIAN_POINT('Ctrl Pts',(-0.92003707827324,0.319434907277167,
3.1446851783948));
#45172=CARTESIAN_POINT('Ctrl Pts',(-0.956219211262303,0.636309800095206,
3.07909909005189));
#45173=CARTESIAN_POINT('Ctrl Pts',(-0.97775505801435,0.79477268400084,3.02931249032378));
#45174=CARTESIAN_POINT('Ctrl Pts',(-1.02977474137891,1.06847604194511,2.90027217207626));
#45175=CARTESIAN_POINT('Ctrl Pts',(-1.0559911951017,1.18514270861178,2.83214462327784));
#45176=CARTESIAN_POINT('Ctrl Pts',(-1.08590670913801,1.3,2.75174629803529));
#45177=CARTESIAN_POINT('Ctrl Pts',(-0.817242636729971,-1.3,2.69463998655998));
#45178=CARTESIAN_POINT('Ctrl Pts',(-0.811870873772814,-1.18514270861178,
2.78025524714239));
#45179=CARTESIAN_POINT('Ctrl Pts',(-0.808110825487513,-1.06847604194512,
2.85315605226807));
#45180=CARTESIAN_POINT('Ctrl Pts',(-0.803147745067785,-0.794772684000851,
2.99219856024141));
#45181=CARTESIAN_POINT('Ctrl Pts',(-0.802571685601036,-0.636309800095197,
3.04644030028823));
#45182=CARTESIAN_POINT('Ctrl Pts',(-0.808949443435948,-0.319434907277159,
3.12107277268973));
#45183=CARTESIAN_POINT('Ctrl Pts',(-0.814362858626304,-0.158333333333332,
3.13919262917263));
#45184=CARTESIAN_POINT('Ctrl Pts',(-0.834445726094753,0.158333333333334,
3.14327788892968));
#45185=CARTESIAN_POINT('Ctrl Pts',(-0.847999940077955,0.319434907277167,
3.12900897961301));
#45186=CARTESIAN_POINT('Ctrl Pts',(-0.884801197368704,0.636309800095206,
3.06317516506461));
#45187=CARTESIAN_POINT('Ctrl Pts',(-0.907054451600613,0.79477268400084,
3.01337055268305));
#45188=CARTESIAN_POINT('Ctrl Pts',(-0.957653771540386,1.06847604194511,
2.88363241978539));
#45189=CARTESIAN_POINT('Ctrl Pts',(-0.98274205719405,1.18514270861178,2.81507710262639));
#45190=CARTESIAN_POINT('Ctrl Pts',(-1.01101605778904,1.3,2.73412529876815));
#45191=CARTESIAN_POINT('Ctrl Pts',(-0.741659516280667,-1.3,2.68027679827216));
#45192=CARTESIAN_POINT('Ctrl Pts',(-0.738012470505644,-1.18514270861178,
2.76605409464598));
#45193=CARTESIAN_POINT('Ctrl Pts',(-0.735457044102347,-1.06847604194512,
2.8390229812222));
#45194=CARTESIAN_POINT('Ctrl Pts',(-0.732075357025824,-0.794772684000851,
2.97800571764298));
#45195=CARTESIAN_POINT('Ctrl Pts',(-0.730851239620764,-0.636309800095197,
3.03193920640198));
#45196=CARTESIAN_POINT('Ctrl Pts',(-0.73676415858738,-0.319434907277159,
3.1060935491136));
#45197=CARTESIAN_POINT('Ctrl Pts',(-0.741012286627638,-0.158333333333332,
3.12378496929258));
#45198=CARTESIAN_POINT('Ctrl Pts',(-0.761169784372619,0.158333333333334,
3.12751912120358));
#45199=CARTESIAN_POINT('Ctrl Pts',(-0.775962801882669,0.319434907277167,
3.11333278083123));
#45200=CARTESIAN_POINT('Ctrl Pts',(-0.813383183475105,0.636309800095206,
3.04725124007732));
#45201=CARTESIAN_POINT('Ctrl Pts',(-0.836353845186877,0.79477268400084,
2.99742861504232));
#45202=CARTESIAN_POINT('Ctrl Pts',(-0.885532801701862,1.06847604194511,
2.86699266749452));
#45203=CARTESIAN_POINT('Ctrl Pts',(-0.909492919286398,1.18514270861178,
2.79800958197493));
#45204=CARTESIAN_POINT('Ctrl Pts',(-0.936125406440072,1.3,2.71650429950101));
#45205=CARTESIAN_POINT('Ctrl Pts',(-0.741659516280667,-1.3,2.68027679827216));
#45206=CARTESIAN_POINT('Ctrl Pts',(-0.738012470505644,-1.18514270861178,
2.76605409464599));
#45207=CARTESIAN_POINT('Ctrl Pts',(-0.735457044102347,-1.06847604194512,
2.8390229812222));
#45208=CARTESIAN_POINT('Ctrl Pts',(-0.732075357025824,-0.794772684000851,
2.97800571764298));
#45209=CARTESIAN_POINT('Ctrl Pts',(-0.730851239620763,-0.636309800095197,
3.03193920640198));
#45210=CARTESIAN_POINT('Ctrl Pts',(-0.736764158587379,-0.319434907277159,
3.1060935491136));
#45211=CARTESIAN_POINT('Ctrl Pts',(-0.741012286627637,-0.158333333333332,
3.12378496929258));
#45212=CARTESIAN_POINT('Ctrl Pts',(-0.761169784372619,0.158333333333334,
3.12751912120358));
#45213=CARTESIAN_POINT('Ctrl Pts',(-0.775962801882668,0.319434907277167,
3.11333278083123));
#45214=CARTESIAN_POINT('Ctrl Pts',(-0.813383183475106,0.636309800095206,
3.04725124007732));
#45215=CARTESIAN_POINT('Ctrl Pts',(-0.836353845186877,0.79477268400084,
2.99742861504232));
#45216=CARTESIAN_POINT('Ctrl Pts',(-0.885532801701861,1.06847604194511,
2.86699266749452));
#45217=CARTESIAN_POINT('Ctrl Pts',(-0.909492919286397,1.18514270861178,
2.79800958197494));
#45218=CARTESIAN_POINT('Ctrl Pts',(-0.936125406440072,1.3,2.71650429950101));
#45219=CARTESIAN_POINT('Ctrl Pts',(-0.74165951628067,-1.3000000000001,2.68027679827209));
#45220=CARTESIAN_POINT('Ctrl Pts',(-0.738012470505646,-1.18514270861185,
2.76605409464595));
#45221=CARTESIAN_POINT('Ctrl Pts',(-0.735457044102347,-1.06847604194515,
2.83902298122219));
#45222=CARTESIAN_POINT('Ctrl Pts',(-0.732075357025824,-0.794772684000851,
2.97800571764297));
#45223=CARTESIAN_POINT('Ctrl Pts',(-0.730851239620763,-0.636309800095196,
3.03193920640198));
#45224=CARTESIAN_POINT('Ctrl Pts',(-0.73676415858738,-0.319434907277159,
3.1060935491136));
#45225=CARTESIAN_POINT('Ctrl Pts',(-0.741012286627637,-0.158333333333332,
3.12378496929258));
#45226=CARTESIAN_POINT('Ctrl Pts',(-0.761169784372619,0.158333333333334,
3.12751912120358));
#45227=CARTESIAN_POINT('Ctrl Pts',(-0.775962801882669,0.319434907277167,
3.11333278083123));
#45228=CARTESIAN_POINT('Ctrl Pts',(-0.813383183475106,0.636309800095206,
3.04725124007732));
#45229=CARTESIAN_POINT('Ctrl Pts',(-0.836353845186877,0.79477268400084,
2.99742861504232));
#45230=CARTESIAN_POINT('Ctrl Pts',(-0.885532801702163,1.06847604194679,
2.86699266749372));
#45231=CARTESIAN_POINT('Ctrl Pts',(-0.909492919287077,1.18514270861508,
2.79800958197298));
#45232=CARTESIAN_POINT('Ctrl Pts',(-0.936125406441205,1.30000000000488,
2.71650429949754));
#45233=CARTESIAN_POINT('Ctrl Pts',(-0.73773330559217,-1.3000000000001,2.67245517600946));
#45234=CARTESIAN_POINT('Ctrl Pts',(-0.734729140499245,-1.18514270861185,
2.75847136303451));
#45235=CARTESIAN_POINT('Ctrl Pts',(-0.732217053975366,-1.06847604194515,
2.83164616358891));
#45236=CARTESIAN_POINT('Ctrl Pts',(-0.727550431498492,-0.794772684000851,
2.97102841978056));
#45237=CARTESIAN_POINT('Ctrl Pts',(-0.7226833723533,-0.636309800095196,
3.02517530962454));
#45238=CARTESIAN_POINT('Ctrl Pts',(-0.726824245379794,-0.319434907277159,
3.09946703800493));
#45239=CARTESIAN_POINT('Ctrl Pts',(-0.731604230865546,-0.158333333333332,
3.11703748029681));
#45240=CARTESIAN_POINT('Ctrl Pts',(-0.751993950054195,0.158333333333334,
3.12072515304754));
#45241=CARTESIAN_POINT('Ctrl Pts',(-0.766766141896399,0.319434907277167,
3.10658683795392));
#45242=CARTESIAN_POINT('Ctrl Pts',(-0.805863671213904,0.636309800095206,
3.04032716133598));
#45243=CARTESIAN_POINT('Ctrl Pts',(-0.831394255645057,0.79477268400084,
2.99033173914693));
#45244=CARTESIAN_POINT('Ctrl Pts',(-0.882011643621234,1.06847604194679,
2.85950209302966));
#45245=CARTESIAN_POINT('Ctrl Pts',(-0.906248352874114,1.18514270861508,
2.79031303915094));
#45246=CARTESIAN_POINT('Ctrl Pts',(-0.932811379683886,1.30000000000488,
2.70856623748196));
#45247=CARTESIAN_POINT('Ctrl Pts',(-0.735709753270855,-1.3000000000001,
2.66035632699752));
#45248=CARTESIAN_POINT('Ctrl Pts',(-0.734276224702703,-1.18514270861185,
2.7439279293322));
#45249=CARTESIAN_POINT('Ctrl Pts',(-0.732270057354958,-1.06847604194515,
2.81535450686582));
#45250=CARTESIAN_POINT('Ctrl Pts',(-0.726312499312411,-0.794772684000851,
2.95230675291205));
#45251=CARTESIAN_POINT('Ctrl Pts',(-0.715957485685984,-0.636309800095198,
3.0071883638833));
#45252=CARTESIAN_POINT('Ctrl Pts',(-0.717231377152474,-0.31943490727716,
3.08166701371969));
#45253=CARTESIAN_POINT('Ctrl Pts',(-0.722183463147362,-0.158333333333333,
3.10020625520556));
#45254=CARTESIAN_POINT('Ctrl Pts',(-0.742739360703625,0.158333333333335,
3.10387421830447));
#45255=CARTESIAN_POINT('Ctrl Pts',(-0.757379057429574,0.319434907277169,
3.08867052408036));
#45256=CARTESIAN_POINT('Ctrl Pts',(-0.799939881712645,0.636309800095209,
3.0223403580999));
#45257=CARTESIAN_POINT('Ctrl Pts',(-0.83200195614442,0.794772684000844,
2.97198639479701));
#45258=CARTESIAN_POINT('Ctrl Pts',(-0.883860679443162,1.06847604194679,
2.84356969105433));
#45259=CARTESIAN_POINT('Ctrl Pts',(-0.907297495995768,1.18514270861508,
2.77603315718813));
#45260=CARTESIAN_POINT('Ctrl Pts',(-0.931723409339857,1.30000000000488,
2.69654692219852));
#45261=CARTESIAN_POINT('Ctrl Pts',(-0.732581199673119,-1.3000000000001,
2.64260536769187));
#45262=CARTESIAN_POINT('Ctrl Pts',(-0.731581621758525,-1.18514270861185,
2.72252964260173));
#45263=CARTESIAN_POINT('Ctrl Pts',(-0.729689019270264,-1.06847604194515,
2.79124774140366));
#45264=CARTESIAN_POINT('Ctrl Pts',(-0.723253663494429,-0.794772684000852,
2.92411178804753));
#45265=CARTESIAN_POINT('Ctrl Pts',(-0.711354667280304,-0.636309800095197,
2.9793476780709));
#45266=CARTESIAN_POINT('Ctrl Pts',(-0.711355798935644,-0.319434907277159,
3.05351896672594));
#45267=CARTESIAN_POINT('Ctrl Pts',(-0.715491493976768,-0.158333333333332,
3.07327585441042));
#45268=CARTESIAN_POINT('Ctrl Pts',(-0.736146419548719,0.158333333333335,
3.07697661143391));
#45269=CARTESIAN_POINT('Ctrl Pts',(-0.7513715082161,0.319434907277168,3.06057021824835));
#45270=CARTESIAN_POINT('Ctrl Pts',(-0.79607904654136,0.636309800095207,
2.99465056472962));
#45271=CARTESIAN_POINT('Ctrl Pts',(-0.83154007459095,0.794772684000841,
2.94412507676054));
#45272=CARTESIAN_POINT('Ctrl Pts',(-0.884051830167423,1.06847604194679,
2.81976101536945));
#45273=CARTESIAN_POINT('Ctrl Pts',(-0.907042942513032,1.18514270861508,
2.75486405369761));
#45274=CARTESIAN_POINT('Ctrl Pts',(-0.930294773967327,1.30000000000488,
2.67890272438792));
#45275=CARTESIAN_POINT('Ctrl Pts',(-0.729771743392393,-1.30000000000009,
2.62789816097744));
#45276=CARTESIAN_POINT('Ctrl Pts',(-0.728734320005336,-1.18514270861185,
2.70507151758026));
#45277=CARTESIAN_POINT('Ctrl Pts',(-0.726954114717163,-1.06847604194515,
2.77180122606182));
#45278=CARTESIAN_POINT('Ctrl Pts',(-0.721125509588046,-0.794772684000851,
2.90183328548194));
#45279=CARTESIAN_POINT('Ctrl Pts',(-0.710774425642683,-0.636309800095197,
2.95779964073951));
#45280=CARTESIAN_POINT('Ctrl Pts',(-0.710606698362087,-0.319434907277159,
3.03193990563363));
#45281=CARTESIAN_POINT('Ctrl Pts',(-0.712952299894917,-0.158333333333332,
3.0524727895937));
#45282=CARTESIAN_POINT('Ctrl Pts',(-0.733016707245456,0.158333333333335,
3.05613067980892));
#45283=CARTESIAN_POINT('Ctrl Pts',(-0.748548602363565,0.319434907277168,
3.03882122131528));
#45284=CARTESIAN_POINT('Ctrl Pts',(-0.794040662364233,0.636309800095207,
2.9730167888235));
#45285=CARTESIAN_POINT('Ctrl Pts',(-0.831171375868185,0.794772684000842,
2.92211107346514));
#45286=CARTESIAN_POINT('Ctrl Pts',(-0.88358594787812,1.06847604194679,2.80059150689011));
#45287=CARTESIAN_POINT('Ctrl Pts',(-0.906111819380047,1.18514270861508,
2.73761477251729));
#45288=CARTESIAN_POINT('Ctrl Pts',(-0.928475236311926,1.30000000000488,
2.66426262139868));
#45289=CARTESIAN_POINT('Ctrl Pts',(-0.726505469227192,-1.3000000000001,
2.61305804659452));
#45290=CARTESIAN_POINT('Ctrl Pts',(-0.725318776084473,-1.18514270861185,
2.68722387894012));
#45291=CARTESIAN_POINT('Ctrl Pts',(-0.723622119673275,-1.06847604194515,
2.75176622967882));
#45292=CARTESIAN_POINT('Ctrl Pts',(-0.718524386780468,-0.794772684000852,
2.87863980385541));
#45293=CARTESIAN_POINT('Ctrl Pts',(-0.709931954095278,-0.636309800095197,
2.93527807660178));
#45294=CARTESIAN_POINT('Ctrl Pts',(-0.710293323618512,-0.319434907277159,
3.00935793161261));
#45295=CARTESIAN_POINT('Ctrl Pts',(-0.711181795360178,-0.158333333333332,
3.03075121606602));
#45296=CARTESIAN_POINT('Ctrl Pts',(-0.732159223967551,0.158333333333334,
3.03453740674467));
#45297=CARTESIAN_POINT('Ctrl Pts',(-0.750600978758044,0.319434907277167,
3.01658351261059));
#45298=CARTESIAN_POINT('Ctrl Pts',(-0.796324352907775,0.636309800095206,
2.95092226275884));
#45299=CARTESIAN_POINT('Ctrl Pts',(-0.830988928451572,0.794772684000842,
2.89920826232716));
#45300=CARTESIAN_POINT('Ctrl Pts',(-0.882215538271197,1.06847604194679,
2.78073762285996));
#45301=CARTESIAN_POINT('Ctrl Pts',(-0.904421541101885,1.18514270861508,
2.7198949897962));
#45302=CARTESIAN_POINT('Ctrl Pts',(-0.926659445505138,1.30000000000488,
2.64949127372461));
#45303=CARTESIAN_POINT('Ctrl Pts',(-0.718203659447294,-1.3000000000001,
2.58347432518368));
#45304=CARTESIAN_POINT('Ctrl Pts',(-0.71702626283155,-1.18514270861185,
2.65187970978938));
#45305=CARTESIAN_POINT('Ctrl Pts',(-0.715782659739986,-1.06847604194515,
2.71224520391757));
#45306=CARTESIAN_POINT('Ctrl Pts',(-0.712756737612827,-0.794772684000853,
2.83312781605184));
#45307=CARTESIAN_POINT('Ctrl Pts',(-0.707269685879409,-0.636309800095198,
2.89107118306634));
#45308=CARTESIAN_POINT('Ctrl Pts',(-0.710636393371801,-0.319434907277159,
2.96525869637214));
#45309=CARTESIAN_POINT('Ctrl Pts',(-0.712800720158232,-0.158333333333333,
2.98871655055816));
#45310=CARTESIAN_POINT('Ctrl Pts',(-0.73485780184828,0.158333333333335,
2.992681317029));
#45311=CARTESIAN_POINT('Ctrl Pts',(-0.753453663406939,0.319434907277168,
2.97294683811374));
#45312=CARTESIAN_POINT('Ctrl Pts',(-0.797657321518849,0.636309800095208,
2.90732696513016));
#45313=CARTESIAN_POINT('Ctrl Pts',(-0.829377614451152,0.794772684000843,
2.85419637011498));
#45314=CARTESIAN_POINT('Ctrl Pts',(-0.878922936927556,1.06847604194679,
2.74158131689578));
#45315=CARTESIAN_POINT('Ctrl Pts',(-0.900752807799096,1.18514270861508,
2.6848340433371));
#45316=CARTESIAN_POINT('Ctrl Pts',(-0.922966215277102,1.30000000000488,
2.62008637995976));
#45317=CARTESIAN_POINT('Ctrl Pts',(-0.711759248151161,-1.3000000000001,
2.55392799989938));
#45318=CARTESIAN_POINT('Ctrl Pts',(-0.709659453060768,-1.18514270861185,
2.61648977582277));
#45319=CARTESIAN_POINT('Ctrl Pts',(-0.708079464161582,-1.06847604194515,
2.67259991171752));
#45320=CARTESIAN_POINT('Ctrl Pts',(-0.705630230017321,-0.794772684000854,
2.78732097131632));
#45321=CARTESIAN_POINT('Ctrl Pts',(-0.702745937711363,-0.636309800095198,
2.84646488276085));
#45322=CARTESIAN_POINT('Ctrl Pts',(-0.708213072692534,-0.319434907277159,
2.92063246419698));
#45323=CARTESIAN_POINT('Ctrl Pts',(-0.711339447678475,-0.158333333333332,
2.94613913648399));
#45324=CARTESIAN_POINT('Ctrl Pts',(-0.734125218490468,0.158333333333334,
2.95019622821214));
#45325=CARTESIAN_POINT('Ctrl Pts',(-0.752687649534627,0.319434907277165,
2.92855294595052));
#45326=CARTESIAN_POINT('Ctrl Pts',(-0.795867927344174,0.636309800095205,
2.86304392466589));
#45327=CARTESIAN_POINT('Ctrl Pts',(-0.825869341580405,0.794772684000843,
2.80872865049762));
#45328=CARTESIAN_POINT('Ctrl Pts',(-0.874075887182553,1.06847604194679,
2.70213915588633));
#45329=CARTESIAN_POINT('Ctrl Pts',(-0.895466313933186,1.18514270861508,
2.64954635264564));
#45330=CARTESIAN_POINT('Ctrl Pts',(-0.917380340071678,1.30000000000488,
2.5904993888518));
#45331=CARTESIAN_POINT('Ctrl Pts',(-0.701409308678934,-1.3000000000001,
2.52143083639184));
#45332=CARTESIAN_POINT('Ctrl Pts',(-0.698426146535951,-1.18514270861184,
2.5776296854358));
#45333=CARTESIAN_POINT('Ctrl Pts',(-0.696567911764466,-1.06847604194514,
2.62909904971683));
#45334=CARTESIAN_POINT('Ctrl Pts',(-0.694873824972859,-0.794772684000843,
2.73707752168452));
#45335=CARTESIAN_POINT('Ctrl Pts',(-0.694381863306111,-0.636309800095195,
2.7974518787628));
#45336=CARTESIAN_POINT('Ctrl Pts',(-0.702953732513364,-0.319434907277159,
2.87160078252508));
#45337=CARTESIAN_POINT('Ctrl Pts',(-0.708896545536722,-0.158333333333332,
2.89942566072425));
#45338=CARTESIAN_POINT('Ctrl Pts',(-0.732779542220326,0.158333333333334,
2.90359846879207));
#45339=CARTESIAN_POINT('Ctrl Pts',(-0.749996430543724,0.319434907277167,
2.87983083089195));
#45340=CARTESIAN_POINT('Ctrl Pts',(-0.791545806470309,0.636309800095206,
2.81441703993551));
#45341=CARTESIAN_POINT('Ctrl Pts',(-0.819313612205697,0.794772684000841,
2.75876072363453));
#45342=CARTESIAN_POINT('Ctrl Pts',(-0.867005692102054,1.06847604194679,
2.65880185706368));
#45343=CARTESIAN_POINT('Ctrl Pts',(-0.888655048864636,1.18514270861508,
2.6107906112134));
#45344=CARTESIAN_POINT('Ctrl Pts',(-0.911309628168231,1.30000000000488,
2.55803660901066));
#45345=CARTESIAN_POINT('Ctrl Pts',(-0.695015042608171,-1.3000000000001,
2.49781259678561));
#45346=CARTESIAN_POINT('Ctrl Pts',(-0.691330264994516,-1.18514270861185,
2.54936798035452));
#45347=CARTESIAN_POINT('Ctrl Pts',(-0.689101790206814,-1.06847604194514,
2.59744566475941));
#45348=CARTESIAN_POINT('Ctrl Pts',(-0.687317918502706,-0.794772684000844,
2.7004805528623));
#45349=CARTESIAN_POINT('Ctrl Pts',(-0.687738816379448,-0.636309800095195,
2.76173681889702));
#45350=CARTESIAN_POINT('Ctrl Pts',(-0.697669729324493,-0.319434907277159,
2.83580174139693));
#45351=CARTESIAN_POINT('Ctrl Pts',(-0.705033470020429,-0.158333333333332,
2.86522201718424));
#45352=CARTESIAN_POINT('Ctrl Pts',(-0.729713908260099,0.158333333333334,
2.86945474364033));
#45353=CARTESIAN_POINT('Ctrl Pts',(-0.746638691550855,0.319434907277167,
2.84418733046913));
#45354=CARTESIAN_POINT('Ctrl Pts',(-0.787778355364049,0.636309800095205,
2.77890684388552));
#45355=CARTESIAN_POINT('Ctrl Pts',(-0.814620216025745,0.794772684000838,
2.72234169851759));
#45356=CARTESIAN_POINT('Ctrl Pts',(-0.862244632919749,1.06847604194679,
2.62725935743987));
#45357=CARTESIAN_POINT('Ctrl Pts',(-0.884070097538701,1.18514270861508,
2.58259634633224));
#45358=CARTESIAN_POINT('Ctrl Pts',(-0.907106181361594,1.30000000000488,
2.53442794642189));
#45359=CARTESIAN_POINT('Ctrl Pts',(-0.684471546903474,-1.3000000000001,
2.46831190594925));
#45360=CARTESIAN_POINT('Ctrl Pts',(-0.679292846719528,-1.18514270861185,
2.51407523067114));
#45361=CARTESIAN_POINT('Ctrl Pts',(-0.67636879885502,-1.06847604194515,
2.55792096534174));
#45362=CARTESIAN_POINT('Ctrl Pts',(-0.674822361233792,-0.794772684000854,
2.65478336710894));
#45363=CARTESIAN_POINT('Ctrl Pts',(-0.678478767580897,-0.636309800095198,
2.71713334559981));
#45364=CARTESIAN_POINT('Ctrl Pts',(-0.690659306413056,-0.319434907277159,
2.79107914598393));
#45365=CARTESIAN_POINT('Ctrl Pts',(-0.698803958562443,-0.158333333333332,
2.82247483191899));
#45366=CARTESIAN_POINT('Ctrl Pts',(-0.724331819242718,0.158333333333335,
2.82677431923026));
#45367=CARTESIAN_POINT('Ctrl Pts',(-0.741369687464005,0.319434907277167,
2.79964707518251));
#45368=CARTESIAN_POINT('Ctrl Pts',(-0.781890996115929,0.636309800095207,
2.73452225817136));
#45369=CARTESIAN_POINT('Ctrl Pts',(-0.807011700062937,0.794772684000841,
2.67680326982785));
#45370=CARTESIAN_POINT('Ctrl Pts',(-0.85439209018396,1.06847604194679,2.58778738955115));
#45371=CARTESIAN_POINT('Ctrl Pts',(-0.876453514898898,1.18514270861508,
2.54729514463003));
#45372=CARTESIAN_POINT('Ctrl Pts',(-0.900067149061703,1.30000000000489,
2.50484233099641));
#45373=CARTESIAN_POINT('Ctrl Pts',(-0.674261209315636,-1.3000000000001,
2.43590191982576));
#45374=CARTESIAN_POINT('Ctrl Pts',(-0.667529038149191,-1.18514270861185,
2.47530503846599));
#45375=CARTESIAN_POINT('Ctrl Pts',(-0.663661339171831,-1.06847604194515,
2.51449844127821));
#45376=CARTESIAN_POINT('Ctrl Pts',(-0.661343684596083,-0.794772684000854,
2.60455855687163));
#45377=CARTESIAN_POINT('Ctrl Pts',(-0.666221899005568,-0.636309800095196,
2.66807322957033));
#45378=CARTESIAN_POINT('Ctrl Pts',(-0.680453091202015,-0.319434907277157,
2.74185202409489));
#45379=CARTESIAN_POINT('Ctrl Pts',(-0.691402120595438,-0.158333333333332,
2.77541503050119));
#45380=CARTESIAN_POINT('Ctrl Pts',(-0.717772629253875,0.158333333333334,
2.77974510248551));
#45381=CARTESIAN_POINT('Ctrl Pts',(-0.733025999216182,0.319434907277166,
2.75050343715987));
#45382=CARTESIAN_POINT('Ctrl Pts',(-0.772852060962675,0.636309800095205,
2.68556247171395));
#45383=CARTESIAN_POINT('Ctrl Pts',(-0.797551059226474,0.794772684000838,
2.62665941880218));
#45384=CARTESIAN_POINT('Ctrl Pts',(-0.845717106904218,1.06847604194679,
2.54438330441938));
#45385=CARTESIAN_POINT('Ctrl Pts',(-0.868442268727925,1.18514270861508,
2.50850465450521));
#45386=CARTESIAN_POINT('Ctrl Pts',(-0.893043295063443,1.30000000000488,
2.47236163596295));
#45387=CARTESIAN_POINT('Ctrl Pts',(-0.665650684226199,-1.3000000000001,
2.41236448965116));
#45388=CARTESIAN_POINT('Ctrl Pts',(-0.657463728678987,-1.18514270861185,
2.4471572740478));
#45389=CARTESIAN_POINT('Ctrl Pts',(-0.652811062767846,-1.06847604194515,
2.48297516049676));
#45390=CARTESIAN_POINT('Ctrl Pts',(-0.65022738984203,-0.794772684000853,
2.56808983434933));
#45391=CARTESIAN_POINT('Ctrl Pts',(-0.657616410684264,-0.636309800095197,
2.63243055732278));
#45392=CARTESIAN_POINT('Ctrl Pts',(-0.673098780547473,-0.319434907277159,
2.70605930776217));
#45393=CARTESIAN_POINT('Ctrl Pts',(-0.684135212950933,-0.158333333333332,
2.74116263102348));
#45394=CARTESIAN_POINT('Ctrl Pts',(-0.710767709561529,0.158333333333335,
2.7455138041351));
#45395=CARTESIAN_POINT('Ctrl Pts',(-0.725987843158548,0.319434907277167,
2.71477983403209));
#45396=CARTESIAN_POINT('Ctrl Pts',(-0.765519694872641,0.636309800095206,
2.64997707848015));
#45397=CARTESIAN_POINT('Ctrl Pts',(-0.789120836171394,0.794772684000841,
2.59018019489115));
#45398=CARTESIAN_POINT('Ctrl Pts',(-0.837961494715776,1.06847604194679,
2.51279473146583));
#45399=CARTESIAN_POINT('Ctrl Pts',(-0.861369519587865,1.18514270861508,
2.48027014456695));
#45400=CARTESIAN_POINT('Ctrl Pts',(-0.887044257972772,1.30000000000488,
2.44871827047225));
#45401=CARTESIAN_POINT('Ctrl Pts',(-0.656870619801096,-1.3000000000001,
2.38886109932766));
#45402=CARTESIAN_POINT('Ctrl Pts',(-0.646955507175138,-1.18514270861185,
2.41906094384512));
#45403=CARTESIAN_POINT('Ctrl Pts',(-0.641172110179515,-1.06847604194515,
2.4515133873216));
#45404=CARTESIAN_POINT('Ctrl Pts',(-0.637356395807979,-0.794772684000853,
2.53168897806758));
#45405=CARTESIAN_POINT('Ctrl Pts',(-0.645440186674182,-0.636309800095197,
2.59683243151389));
#45406=CARTESIAN_POINT('Ctrl Pts',(-0.662856348260645,-0.319434907277158,
2.67029705351756));
#45407=CARTESIAN_POINT('Ctrl Pts',(-0.676859985583006,-0.158333333333332,
2.70693559241231));
#45408=CARTESIAN_POINT('Ctrl Pts',(-0.705025145353065,0.158333333333334,
2.71130040697335));
#45409=CARTESIAN_POINT('Ctrl Pts',(-0.719631034374305,0.319434907277168,
2.67907185952832));
#45410=CARTESIAN_POINT('Ctrl Pts',(-0.758680132565803,0.636309800095207,
2.614406028439));
#45411=CARTESIAN_POINT('Ctrl Pts',(-0.78073808948678,0.79477268400084,2.55371501141879));
#45412=CARTESIAN_POINT('Ctrl Pts',(-0.830246128428462,1.06847604194679,
2.48122741212257));
#45413=CARTESIAN_POINT('Ctrl Pts',(-0.854437405012396,1.18514270861508,
2.45206178512877));
#45414=CARTESIAN_POINT('Ctrl Pts',(-0.881389762575884,1.30000000000488,
2.42510772694649));
#45415=CARTESIAN_POINT('Ctrl Pts',(-0.649882878774368,-1.3000000000001,
2.36830415817458));
#45416=CARTESIAN_POINT('Ctrl Pts',(-0.638160393524729,-1.18514270861185,
2.39450573828197));
#45417=CARTESIAN_POINT('Ctrl Pts',(-0.631282124890061,-1.06847604194515,
2.42402609610759));
#45418=CARTESIAN_POINT('Ctrl Pts',(-0.626583057813851,-0.794772684000853,
2.49989106866049));
#45419=CARTESIAN_POINT('Ctrl Pts',(-0.636782937033632,-0.636309800095198,
2.56571734829579));
#45420=CARTESIAN_POINT('Ctrl Pts',(-0.655281941044772,-0.31943490727716,
2.63902174680975));
#45421=CARTESIAN_POINT('Ctrl Pts',(-0.669906857441273,-0.158333333333332,
2.67698930985721));
#45422=CARTESIAN_POINT('Ctrl Pts',(-0.698002341158252,0.158333333333335,
2.68135526233245));
#45423=CARTESIAN_POINT('Ctrl Pts',(-0.711418408796788,0.319434907277166,
2.64781596256982));
#45424=CARTESIAN_POINT('Ctrl Pts',(-0.750258894103182,0.636309800095206,
2.58327777225634));
#45425=CARTESIAN_POINT('Ctrl Pts',(-0.772698526102032,0.794772684000843,
2.52184053753016));
#45426=CARTESIAN_POINT('Ctrl Pts',(-0.823092540885076,1.06847604194679,
2.4536193870615));
#45427=CARTESIAN_POINT('Ctrl Pts',(-0.847808970160495,1.18514270861508,
2.4273725281449));
#45428=CARTESIAN_POINT('Ctrl Pts',(-0.875428126993862,1.30000000000488,
2.40440921850705));
#45429=CARTESIAN_POINT('Ctrl Pts',(-0.639601120729089,-1.3000000000001,
2.34486673133637));
#45430=CARTESIAN_POINT('Ctrl Pts',(-0.626738549432459,-1.18514270861185,
2.36648103949476));
#45431=CARTESIAN_POINT('Ctrl Pts',(-0.61911233014439,-1.06847604194515,
2.39264026996296));
#45432=CARTESIAN_POINT('Ctrl Pts',(-0.613591258637418,-0.794772684000853,
2.46357300522486));
#45433=CARTESIAN_POINT('Ctrl Pts',(-0.624299890124151,-0.636309800095198,
2.53021390656471));
#45434=CARTESIAN_POINT('Ctrl Pts',(-0.643934931957813,-0.319434907277159,
2.60333239070418));
#45435=CARTESIAN_POINT('Ctrl Pts',(-0.660036159520178,-0.158333333333332,
2.6427910421422));
#45436=CARTESIAN_POINT('Ctrl Pts',(-0.6894821708808,0.158333333333334,2.64714550972695));
#45437=CARTESIAN_POINT('Ctrl Pts',(-0.703672527292407,0.319434907277166,
2.61211559607771));
#45438=CARTESIAN_POINT('Ctrl Pts',(-0.742294519887011,0.636309800095206,
2.54771556581829));
#45439=CARTESIAN_POINT('Ctrl Pts',(-0.762328448713979,0.794772684000843,
2.48540404651612));
#45440=CARTESIAN_POINT('Ctrl Pts',(-0.813417169094425,1.06847604194679,
2.42206658400128));
#45441=CARTESIAN_POINT('Ctrl Pts',(-0.839076057957825,1.18514270861508,
2.39916544992552));
#45442=CARTESIAN_POINT('Ctrl Pts',(-0.868279421655417,1.30000000000488,
2.38077962241262));
#45443=CARTESIAN_POINT('Ctrl Pts',(-0.633197595098763,-1.3000000000001,
2.32729565509898));
#45444=CARTESIAN_POINT('Ctrl Pts',(-0.618269500330944,-1.18514270861185,
2.34551265657001));
#45445=CARTESIAN_POINT('Ctrl Pts',(-0.609375408590763,-1.06847604194515,
2.36917541648807));
#45446=CARTESIAN_POINT('Ctrl Pts',(-0.602768031506001,-0.794772684000852,
2.43642191705059));
#45447=CARTESIAN_POINT('Ctrl Pts',(-0.615898378255201,-0.636309800095197,
2.5036017450308));
#45448=CARTESIAN_POINT('Ctrl Pts',(-0.636425089780797,-0.319434907277159,
2.57656123962056));
#45449=CARTESIAN_POINT('Ctrl Pts',(-0.652741211014589,-0.158333333333332,
2.61715813013545));
#45450=CARTESIAN_POINT('Ctrl Pts',(-0.681838466694604,0.158333333333334,
2.62150905457092));
#45451=CARTESIAN_POINT('Ctrl Pts',(-0.694678941004356,0.319434907277166,
2.58535909389188));
#45452=CARTESIAN_POINT('Ctrl Pts',(-0.733300373197626,0.636309800095205,
2.52106656301223));
#45453=CARTESIAN_POINT('Ctrl Pts',(-0.754186571802129,0.794772684000841,
2.45811045351102));
#45454=CARTESIAN_POINT('Ctrl Pts',(-0.806660287751361,1.06847604194679,
2.39842947905507));
#45455=CARTESIAN_POINT('Ctrl Pts',(-0.833058301122932,1.18514270861508,
2.37803099503305));
#45456=CARTESIAN_POINT('Ctrl Pts',(-0.863140400574275,1.30000000000488,
2.36306770943312));
#45457=CARTESIAN_POINT('Ctrl Pts',(-0.626079773935383,-1.3000000000001,
2.30973009617971));
#45458=CARTESIAN_POINT('Ctrl Pts',(-0.610331537002746,-1.18514270861185,
2.32451224692394));
#45459=CARTESIAN_POINT('Ctrl Pts',(-0.600796482538009,-1.06847604194515,
2.34566182435764));
#45460=CARTESIAN_POINT('Ctrl Pts',(-0.593122293687099,-0.794772684000854,
2.40923160863995));
#45461=CARTESIAN_POINT('Ctrl Pts',(-0.605662884950393,-0.636309800095198,
2.47705840291504));
#45462=CARTESIAN_POINT('Ctrl Pts',(-0.626783724957263,-0.31943490727716,
2.54987862947416));
#45463=CARTESIAN_POINT('Ctrl Pts',(-0.64475703726334,-0.158333333333332,
2.5915580150273));
#45464=CARTESIAN_POINT('Ctrl Pts',(-0.675054189961014,0.158333333333335,
2.59588195696333));
#45465=CARTESIAN_POINT('Ctrl Pts',(-0.68829025443637,0.319434907277166,
2.55861394244903));
#45466=CARTESIAN_POINT('Ctrl Pts',(-0.727024398230972,0.636309800095206,
2.49442318749211));
#45467=CARTESIAN_POINT('Ctrl Pts',(-0.746734440543491,0.794772684000843,
2.43082141158967));
#45468=CARTESIAN_POINT('Ctrl Pts',(-0.799806743999464,1.06847604194679,
2.37479633394177));
#45469=CARTESIAN_POINT('Ctrl Pts',(-0.826812948308842,1.18514270861509,
2.3569008885581));
#45470=CARTESIAN_POINT('Ctrl Pts',(-0.857852323283982,1.30000000000489,
2.34536117797102));
#45471=CARTESIAN_POINT('Ctrl Pts',(-0.618516064350732,-1.3000000000001,
2.29220914266115));
#45472=CARTESIAN_POINT('Ctrl Pts',(-0.601165595952986,-1.18514270861185,
2.30359702422762));
#45473=CARTESIAN_POINT('Ctrl Pts',(-0.590600175185821,-1.06847604194515,
2.32225479356599));
#45474=CARTESIAN_POINT('Ctrl Pts',(-0.581866756979261,-0.794772684000851,
2.38215286830075));
#45475=CARTESIAN_POINT('Ctrl Pts',(-0.595610486910496,-0.636309800095198,
2.45054905609851));
#45476=CARTESIAN_POINT('Ctrl Pts',(-0.617792955535238,-0.31943490727716,
2.52319924712737));
#45477=CARTESIAN_POINT('Ctrl Pts',(-0.637167225744727,-0.158333333333332,
2.56596826351255));
#45478=CARTESIAN_POINT('Ctrl Pts',(-0.667637211820594,0.158333333333335,
2.57027127447384));
#45479=CARTESIAN_POINT('Ctrl Pts',(-0.679575339066228,0.319434907277167,
2.53190020337716));
#45480=CARTESIAN_POINT('Ctrl Pts',(-0.717742106842312,0.636309800095206,
2.46782156146033));
#45481=CARTESIAN_POINT('Ctrl Pts',(-0.736793863492731,0.794772684000843,
2.40358152724018));
#45482=CARTESIAN_POINT('Ctrl Pts',(-0.791249042953884,1.06847604194679,
2.35120291465679));
#45483=CARTESIAN_POINT('Ctrl Pts',(-0.819342336142497,1.18514270861508,
2.33580188756883));
#45484=CARTESIAN_POINT('Ctrl Pts',(-0.851957293094066,1.30000000000488,
2.32767259396157));
#45485=CARTESIAN_POINT('Ctrl Pts',(-0.612246541381865,-1.3000000000001,
2.27761837040574));
#45486=CARTESIAN_POINT('Ctrl Pts',(-0.593692384082968,-1.18514270861185,
2.28617858275121));
#45487=CARTESIAN_POINT('Ctrl Pts',(-0.582327596914736,-1.06847604194515,
2.30276101850632));
#45488=CARTESIAN_POINT('Ctrl Pts',(-0.572681548268638,-0.794772684000852,
2.3596027033221));
#45489=CARTESIAN_POINT('Ctrl Pts',(-0.587073082306584,-0.636309800095197,
2.42847805994353));
#45490=CARTESIAN_POINT('Ctrl Pts',(-0.610039797410067,-0.319434907277159,
2.50098775770488));
#45491=CARTESIAN_POINT('Ctrl Pts',(-0.630550292877451,-0.158333333333332,
2.54466283821605));
#45492=CARTESIAN_POINT('Ctrl Pts',(-0.661530881486414,0.158333333333334,
2.54894472302388));
#45493=CARTESIAN_POINT('Ctrl Pts',(-0.673037100073311,0.319434907277167,
2.50965063494088));
#45494=CARTESIAN_POINT('Ctrl Pts',(-0.711065100361274,0.636309800095206,
2.44566095314052));
#45495=CARTESIAN_POINT('Ctrl Pts',(-0.729521903519784,0.794772684000841,
2.38088662487286));
#45496=CARTESIAN_POINT('Ctrl Pts',(-0.78485352271252,1.06847604194679,2.33154535248203));
#45497=CARTESIAN_POINT('Ctrl Pts',(-0.813648477505016,1.18514270861508,
2.31822301554134));
#45498=CARTESIAN_POINT('Ctrl Pts',(-0.847287379379839,1.30000000000488,
2.31293635020378));
#45499=CARTESIAN_POINT('Ctrl Pts',(-0.607479816432377,-1.3000000000001,
2.26743691577883));
#45500=CARTESIAN_POINT('Ctrl Pts',(-0.587695759547648,-1.18514270861185,
2.27404585769401));
#45501=CARTESIAN_POINT('Ctrl Pts',(-0.575576671451465,-1.06847604194515,
2.28919013743464));
#45502=CARTESIAN_POINT('Ctrl Pts',(-0.565286764807315,-0.794772684000852,
2.34389479110354));
#45503=CARTESIAN_POINT('Ctrl Pts',(-0.581103229889194,-0.636309800095198,
2.41304642683953));
#45504=CARTESIAN_POINT('Ctrl Pts',(-0.604647533643777,-0.31943490727716,
2.48544261369419));
#45505=CARTESIAN_POINT('Ctrl Pts',(-0.625160380145147,-0.158333333333333,
2.52977641297451));
#45506=CARTESIAN_POINT('Ctrl Pts',(-0.656393070713214,0.158333333333335,
2.53404348737667));
#45507=CARTESIAN_POINT('Ctrl Pts',(-0.667950777501656,0.319434907277167,
2.49409069825917));
#45508=CARTESIAN_POINT('Ctrl Pts',(-0.706318549569805,0.636309800095207,
2.43015415578138));
#45509=CARTESIAN_POINT('Ctrl Pts',(-0.724906926658951,0.794772684000843,
2.36500191170995));
#45510=CARTESIAN_POINT('Ctrl Pts',(-0.780912404472189,1.06847604194679,
2.3177841641865));
#45511=CARTESIAN_POINT('Ctrl Pts',(-0.810088331584231,1.18514270861508,
2.30591686559178));
#45512=CARTESIAN_POINT('Ctrl Pts',(-0.844197489670253,1.30000000000488,
2.30262108171541));
#45513=CARTESIAN_POINT('Ctrl Pts',(-0.604931245382851,-1.3000000000001,
2.26160847477855));
#45514=CARTESIAN_POINT('Ctrl Pts',(-0.584616688670195,-1.18514270861185,
2.26709078669192));
#45515=CARTESIAN_POINT('Ctrl Pts',(-0.572137619939733,-1.06847604194515,
2.28140838306454));
#45516=CARTESIAN_POINT('Ctrl Pts',(-0.561410019466087,-0.794772684000852,
2.33489616950412));
#45517=CARTESIAN_POINT('Ctrl Pts',(-0.577462100406279,-0.636309800095198,
2.40424226993325));
#45518=CARTESIAN_POINT('Ctrl Pts',(-0.601293345077049,-0.31943490727716,
2.47657944903449));
#45519=CARTESIAN_POINT('Ctrl Pts',(-0.622290560639905,-0.158333333333332,
2.52126599426556));
#45520=CARTESIAN_POINT('Ctrl Pts',(-0.653684869393672,0.158333333333335,
2.52552193202855));
#45521=CARTESIAN_POINT('Ctrl Pts',(-0.664974269052977,0.319434907277167,
2.48520499120061));
#45522=CARTESIAN_POINT('Ctrl Pts',(-0.703273406820467,0.636309800095207,
2.42130532012318));
#45523=CARTESIAN_POINT('Ctrl Pts',(-0.721648145326729,0.794772684000843,
2.35593985539621));
#45524=CARTESIAN_POINT('Ctrl Pts',(-0.778134816358336,1.06847604194679,
2.30993383769245));
#45525=CARTESIAN_POINT('Ctrl Pts',(-0.807673287107374,1.18514270861508,
2.29889569734431));
#45526=CARTESIAN_POINT('Ctrl Pts',(-0.84229924175312,1.30000000000488,2.29673371702119));
#45527=CARTESIAN_POINT('Ctrl Pts',(-0.598705350401753,-1.3000000000001,
2.24702934100177));
#45528=CARTESIAN_POINT('Ctrl Pts',(-0.577243519645577,-1.18514270861185,
2.24968477596089));
#45529=CARTESIAN_POINT('Ctrl Pts',(-0.563936836727194,-1.06847604194515,
2.26193184984053));
#45530=CARTESIAN_POINT('Ctrl Pts',(-0.552035760129972,-0.794772684000849,
2.31238364522845));
#45531=CARTESIAN_POINT('Ctrl Pts',(-0.568119224396592,-0.636309800095196,
2.38225132653745));
#45532=CARTESIAN_POINT('Ctrl Pts',(-0.592507924008144,-0.319434907277159,
2.45445080627896));
#45533=CARTESIAN_POINT('Ctrl Pts',(-0.61496683549521,-0.158333333333332,
2.50000379678372));
#45534=CARTESIAN_POINT('Ctrl Pts',(-0.646767713304497,0.158333333333334,
2.50422821446524));
#45535=CARTESIAN_POINT('Ctrl Pts',(-0.657324107698235,0.319434907277167,
2.46300235975121));
#45536=CARTESIAN_POINT('Ctrl Pts',(-0.69523780390506,0.636309800095206,
2.3991984852663));
#45537=CARTESIAN_POINT('Ctrl Pts',(-0.712645846447726,0.794772684000841,
2.33331004648075));
#45538=CARTESIAN_POINT('Ctrl Pts',(-0.770431871534126,1.06847604194679,
2.29032952319989));
#45539=CARTESIAN_POINT('Ctrl Pts',(-0.801044784423362,1.18514270861508,
2.28135946244387));
#45540=CARTESIAN_POINT('Ctrl Pts',(-0.837257181124994,1.30000000000488,
2.28202401687493));
#45541=CARTESIAN_POINT('Ctrl Pts',(-0.587042649530746,-1.30000000000009,
2.22234384363184));
#45542=CARTESIAN_POINT('Ctrl Pts',(-0.562820500195641,-1.18514270861185,
2.22026829704167));
#45543=CARTESIAN_POINT('Ctrl Pts',(-0.547696655758405,-1.06847604194515,
2.2290358717163));
#45544=CARTESIAN_POINT('Ctrl Pts',(-0.533776454017415,-0.794772684000855,
2.27434050244266));
#45545=CARTESIAN_POINT('Ctrl Pts',(-0.551744662673875,-0.636309800095196,
2.34495835777017));
#45546=CARTESIAN_POINT('Ctrl Pts',(-0.57747337456279,-0.319434907277158,
2.41687595758322));
#45547=CARTESIAN_POINT('Ctrl Pts',(-0.601466469856508,-0.158333333333333,
2.46393265375855));
#45548=CARTESIAN_POINT('Ctrl Pts',(-0.633992379378982,0.158333333333335,
2.46809677024522));
#45549=CARTESIAN_POINT('Ctrl Pts',(-0.643460099385473,0.31943490727717,
2.42532591810735));
#45550=CARTESIAN_POINT('Ctrl Pts',(-0.682079987496844,0.636309800095208,
2.36164237349499));
#45551=CARTESIAN_POINT('Ctrl Pts',(-0.700867297629238,0.79477268400084,
2.29479462409256));
#45552=CARTESIAN_POINT('Ctrl Pts',(-0.760180383338873,1.06847604194679,
2.25693188947481));
#45553=CARTESIAN_POINT('Ctrl Pts',(-0.791453011033393,1.18514270861508,
2.25147872126339));
#45554=CARTESIAN_POINT('Ctrl Pts',(-0.828323829384959,1.30000000000488,
2.25696175970412));
#45555=CARTESIAN_POINT('Ctrl Pts',(-0.576486148454196,-1.3000000000001,
2.19912562163394));
#45556=CARTESIAN_POINT('Ctrl Pts',(-0.549805595338174,-1.18514270861185,
2.19260415017178));
#45557=CARTESIAN_POINT('Ctrl Pts',(-0.5330126429192,-1.06847604194515,2.19810476899683));
#45558=CARTESIAN_POINT('Ctrl Pts',(-0.517059899030671,-0.794772684000851,
2.23858573245206));
#45559=CARTESIAN_POINT('Ctrl Pts',(-0.536361982215063,-0.636309800095196,
2.30992895987017));
#45560=CARTESIAN_POINT('Ctrl Pts',(-0.562926419576893,-0.319434907277159,
2.38160063251548));
#45561=CARTESIAN_POINT('Ctrl Pts',(-0.588041432013228,-0.158333333333332,
2.43008246775003));
#45562=CARTESIAN_POINT('Ctrl Pts',(-0.621210414474164,0.158333333333334,
2.43418697459444));
#45563=CARTESIAN_POINT('Ctrl Pts',(-0.630650969299707,0.319434907277167,
2.38992172995728));
#45564=CARTESIAN_POINT('Ctrl Pts',(-0.668824987562712,0.636309800095206,
2.32638233568519));
#45565=CARTESIAN_POINT('Ctrl Pts',(-0.685020236270646,0.79477268400084,
2.25874033545448));
#45566=CARTESIAN_POINT('Ctrl Pts',(-0.746715246697685,1.06847604194679,
2.22569485762038));
#45567=CARTESIAN_POINT('Ctrl Pts',(-0.780090946625215,1.18514270861508,
2.22352789394532));
#45568=CARTESIAN_POINT('Ctrl Pts',(-0.820136862491639,1.30000000000488,
2.23349812949406));
#45569=CARTESIAN_POINT('Ctrl Pts',(-0.570670255377225,-1.3000000000001,
2.18755391703729));
#45570=CARTESIAN_POINT('Ctrl Pts',(-0.542940786613338,-1.18514270861185,
2.17880571545946));
#45571=CARTESIAN_POINT('Ctrl Pts',(-0.52540477270343,-1.06847604194515,
2.18267301919227));
#45572=CARTESIAN_POINT('Ctrl Pts',(-0.508441992410327,-0.794772684000851,
2.22075160545733));
#45573=CARTESIAN_POINT('Ctrl Pts',(-0.527915117224749,-0.636309800095196,
2.29249271205802));
#45574=CARTESIAN_POINT('Ctrl Pts',(-0.554987172141783,-0.319434907277159,
2.36403312099634));
#45575=CARTESIAN_POINT('Ctrl Pts',(-0.581221077759064,-0.158333333333332,
2.41318126918772));
#45576=CARTESIAN_POINT('Ctrl Pts',(-0.614857791973616,0.158333333333334,
2.41724102817915));
#45577=CARTESIAN_POINT('Ctrl Pts',(-0.623796233999666,0.319434907277167,
2.37225523561236));
#45578=CARTESIAN_POINT('Ctrl Pts',(-0.662111769288737,0.636309800095206,
2.30877528147271));
#45579=CARTESIAN_POINT('Ctrl Pts',(-0.678359592024735,0.79477268400084,
2.24069668195692));
#45580=CARTESIAN_POINT('Ctrl Pts',(-0.740987950519493,1.06847604194679,
2.21004687505626));
#45581=CARTESIAN_POINT('Ctrl Pts',(-0.774949037062878,1.18514270861508,
2.20952346492048));
#45582=CARTESIAN_POINT('Ctrl Pts',(-0.815761714366448,1.30000000000488,
2.22174381036905));
#45583=CARTESIAN_POINT('',(-0.819024792214424,1.2,2.31822794574162));
#45584=CARTESIAN_POINT('Ctrl Pts',(-0.819024792214424,1.2,2.31822794574162));
#45585=CARTESIAN_POINT('Ctrl Pts',(-0.82521597710165,1.20975290671087,2.32915586731225));
#45586=CARTESIAN_POINT('Ctrl Pts',(-0.831493530093656,1.21883993984152,
2.3394451037281));
#45587=CARTESIAN_POINT('Ctrl Pts',(-0.842725049707713,1.23553583411338,
2.35832248138883));
#45588=CARTESIAN_POINT('Ctrl Pts',(-0.843308014052171,1.23658026496901,
2.35947858996007));
#45589=CARTESIAN_POINT('Ctrl Pts',(-0.875337102299465,1.28817247228299,
2.41752300234903));
#45590=CARTESIAN_POINT('Ctrl Pts',(-0.877248816045502,1.29056256453409,
2.4203953723537));
#45591=CARTESIAN_POINT('Ctrl Pts',(-0.882736269392908,1.3,2.43100884057243));
#45592=CARTESIAN_POINT('',(-0.66423798661977,0.653834841417894,2.2947693329594));
#45593=CARTESIAN_POINT('Ctrl Pts',(-0.664237986625888,0.653834841417215,
2.29476933293416));
#45594=CARTESIAN_POINT('Ctrl Pts',(-0.680345878045539,0.717897660535232,
2.29695057049292));
#45595=CARTESIAN_POINT('Ctrl Pts',(-0.693505101313191,0.763966491903729,
2.29879280474844));
#45596=CARTESIAN_POINT('Ctrl Pts',(-0.727140785785948,0.885509443554027,
2.30366845023472));
#45597=CARTESIAN_POINT('Ctrl Pts',(-0.742080840142877,0.941055977840171,
2.30590657583669));
#45598=CARTESIAN_POINT('Ctrl Pts',(-0.770642745110105,1.03925891219064,
2.31034536042647));
#45599=CARTESIAN_POINT('Ctrl Pts',(-0.774973594025891,1.05301679619701,
2.31101997894399));
#45600=CARTESIAN_POINT('Ctrl Pts',(-0.799728192199698,1.13603289794848,
2.31501821430012));
#45601=CARTESIAN_POINT('Ctrl Pts',(-0.80800938904033,1.16420864772285,2.31637986922441));
#45602=CARTESIAN_POINT('Ctrl Pts',(-0.819024792214424,1.2,2.31822794574162));
#45603=CARTESIAN_POINT('',(-0.525742999963516,-0.653834841531101,2.27799895388173));
#45604=CARTESIAN_POINT('Ctrl Pts',(-0.525742999963516,-0.6538348415311,
2.27799895388173));
#45605=CARTESIAN_POINT('Ctrl Pts',(-0.539178158222297,-0.575804953766913,
2.31744060698703));
#45606=CARTESIAN_POINT('Ctrl Pts',(-0.5510914907315,-0.493927017715952,
2.35028134650557));
#45607=CARTESIAN_POINT('Ctrl Pts',(-0.570750430336647,-0.338205126032318,
2.39701000106415));
#45608=CARTESIAN_POINT('Ctrl Pts',(-0.578839025687772,-0.265719484524536,
2.41299248805411));
#45609=CARTESIAN_POINT('Ctrl Pts',(-0.593508015655536,-0.129748059605274,
2.43250299417119));
#45610=CARTESIAN_POINT('Ctrl Pts',(-0.60011071216539,-0.0666443969732617,
2.437507137828));
#45611=CARTESIAN_POINT('Ctrl Pts',(-0.613307700163344,0.0595551213823079,
2.43947987121095));
#45612=CARTESIAN_POINT('Ctrl Pts',(-0.619999920040576,0.122805235566241,
2.43648017139236));
#45613=CARTESIAN_POINT('Ctrl Pts',(-0.633837592454916,0.260158152186141,
2.42102084156086));
#45614=CARTESIAN_POINT('Ctrl Pts',(-0.640847266187103,0.333958596470524,
2.40693706705951));
#45615=CARTESIAN_POINT('Ctrl Pts',(-0.653889343793582,0.491154615715495,
2.36404811576026));
#45616=CARTESIAN_POINT('Ctrl Pts',(-0.659737685747932,0.574266546697417,
2.33304833098193));
#45617=CARTESIAN_POINT('Ctrl Pts',(-0.664237986648776,0.653834841429492,
2.29476933298692));
#45618=CARTESIAN_POINT('',(-0.597420188040714,-1.2,2.28618385377298));
#45619=CARTESIAN_POINT('Ctrl Pts',(-0.597420188040713,-1.2,2.28618385377298));
#45620=CARTESIAN_POINT('Ctrl Pts',(-0.58621931009426,-1.14022516977112,
2.28482205463156));
#45621=CARTESIAN_POINT('Ctrl Pts',(-0.570806616189584,-1.05518532565983,
2.28297763515456));
#45622=CARTESIAN_POINT('Ctrl Pts',(-0.538203119733082,-0.802969263789967,
2.27933097932797));
#45623=CARTESIAN_POINT('Ctrl Pts',(-0.531961053416311,-0.737455827809028,
2.27866313457685));
#45624=CARTESIAN_POINT('Ctrl Pts',(-0.525742999963516,-0.653834841531101,
2.27799895388173));
#45625=CARTESIAN_POINT('Ctrl Pts',(-0.65920976572758,-1.3,2.39500858640003));
#45626=CARTESIAN_POINT('Ctrl Pts',(-0.654919428780615,-1.29256895464929,
2.38691933116128));
#45627=CARTESIAN_POINT('Ctrl Pts',(-0.65006515276088,-1.28383644853562,
2.37744823415876));
#45628=CARTESIAN_POINT('Ctrl Pts',(-0.63921127668408,-1.26647251687147,
2.35848214642921));
#45629=CARTESIAN_POINT('Ctrl Pts',(-0.633575792945078,-1.25767778206492,
2.34887219755028));
#45630=CARTESIAN_POINT('Ctrl Pts',(-0.619746849269057,-1.23454545991039,
2.3237601019017));
#45631=CARTESIAN_POINT('Ctrl Pts',(-0.611419467297158,-1.22071295756083,
2.30875136315305));
#45632=CARTESIAN_POINT('Ctrl Pts',(-0.597420188040713,-1.2,2.28618385377298));
#45633=CARTESIAN_POINT('Origin',(0.,1.25,7.2));
#45634=CARTESIAN_POINT('Origin',(0.,1.2,7.2));
#45635=CARTESIAN_POINT('Origin',(0.,0.92691742076555,7.2));
#45636=CARTESIAN_POINT('Origin',(0.,0.653834841531101,7.2));
#45637=CARTESIAN_POINT('Origin',(0.,0.,7.2));
#45638=CARTESIAN_POINT('Origin',(0.,-0.653834841531101,7.2));
#45639=CARTESIAN_POINT('Origin',(0.,-0.926917420765551,7.2));
#45640=CARTESIAN_POINT('Origin',(0.,-1.2,7.2));
#45641=CARTESIAN_POINT('Origin',(0.,-1.25,7.2));
#45642=CARTESIAN_POINT('Ctrl Pts',(-0.23710229803321,-1.30000000000054,
2.16092425493151));
#45643=CARTESIAN_POINT('Ctrl Pts',(-0.279563873100975,-1.18514270861215,
2.1574563860945));
#45644=CARTESIAN_POINT('Ctrl Pts',(-0.312674005334788,-1.0684760419453,
2.16502926538751));
#45645=CARTESIAN_POINT('Ctrl Pts',(-0.367561330757957,-0.794772684000851,
2.20803046837806));
#45646=CARTESIAN_POINT('Ctrl Pts',(-0.36929976285042,-0.636309800095197,
2.27799949945684));
#45647=CARTESIAN_POINT('Ctrl Pts',(-0.393579787165995,-0.319434907277159,
2.34805851202106));
#45648=CARTESIAN_POINT('Ctrl Pts',(-0.392969830592777,-0.158333333333332,
2.39391966368106));
#45649=CARTESIAN_POINT('Ctrl Pts',(-0.426715573254503,0.158333333333334,
2.39694208628984));
#45650=CARTESIAN_POINT('Ctrl Pts',(-0.462594679682927,0.319434907277167,
2.35432227872907));
#45651=CARTESIAN_POINT('Ctrl Pts',(-0.503949232631023,0.636309800095206,
2.28997379608409));
#45652=CARTESIAN_POINT('Ctrl Pts',(-0.53791263772129,0.79477268400084,2.22384909509907));
#45653=CARTESIAN_POINT('Ctrl Pts',(-0.529237518130278,1.0684760419452,2.18307585697225));
#45654=CARTESIAN_POINT('Ctrl Pts',(-0.512888765856002,1.18514270861195,
2.17564712080097));
#45655=CARTESIAN_POINT('Ctrl Pts',(-0.483946399133539,1.30000000000025,
2.17843887244616));
#45656=CARTESIAN_POINT('Ctrl Pts',(-0.23037889702897,-1.30000000000054,
2.17151206948771));
#45657=CARTESIAN_POINT('Ctrl Pts',(-0.271622642083524,-1.18514270861215,
2.1700857215593));
#45658=CARTESIAN_POINT('Ctrl Pts',(-0.303818465808622,-1.0684760419453,
2.17914453006921));
#45659=CARTESIAN_POINT('Ctrl Pts',(-0.35729475106453,-0.794772684000851,
2.22429499885636));
#45660=CARTESIAN_POINT('Ctrl Pts',(-0.359072532092263,-0.636309800095197,
2.2938260406824));
#45661=CARTESIAN_POINT('Ctrl Pts',(-0.38320177356942,-0.319434907277159,
2.36391377144098));
#45662=CARTESIAN_POINT('Ctrl Pts',(-0.383232767764446,-0.158333333333332,
2.40917451598342));
#45663=CARTESIAN_POINT('Ctrl Pts',(-0.416530303335427,0.158333333333334,
2.41205592168762));
#45664=CARTESIAN_POINT('Ctrl Pts',(-0.451176432830852,0.319434907277167,
2.36985523556718));
#45665=CARTESIAN_POINT('Ctrl Pts',(-0.492061752143939,0.636309800095206,
2.30527281803725));
#45666=CARTESIAN_POINT('Ctrl Pts',(-0.525775129538417,0.79477268400084,
2.23950174011295));
#45667=CARTESIAN_POINT('Ctrl Pts',(-0.518587456936803,1.0684760419452,2.19658862087751));
#45668=CARTESIAN_POINT('Ctrl Pts',(-0.503305113780034,1.18514270861195,
2.18771675262694));
#45669=CARTESIAN_POINT('Ctrl Pts',(-0.475851704606216,1.30000000000025,
2.18854851535506));
#45670=CARTESIAN_POINT('Ctrl Pts',(-0.217486849125369,-1.30000000000053,
2.19275902390419));
#45671=CARTESIAN_POINT('Ctrl Pts',(-0.254683144397209,-1.18514270861214,
2.19506054551115));
#45672=CARTESIAN_POINT('Ctrl Pts',(-0.284135067288816,-1.06847604194529,
2.20689629477346));
#45673=CARTESIAN_POINT('Ctrl Pts',(-0.334283851550653,-0.794772684000841,
2.25626521650244));
#45674=CARTESIAN_POINT('Ctrl Pts',(-0.338793322038421,-0.636309800095192,
2.32556525340573));
#45675=CARTESIAN_POINT('Ctrl Pts',(-0.363329433692974,-0.319434907277158,
2.39588620577184));
#45676=CARTESIAN_POINT('Ctrl Pts',(-0.363675064915224,-0.158333333333331,
2.43968426685622));
#45677=CARTESIAN_POINT('Ctrl Pts',(-0.396341931007945,0.158333333333333,
2.44237024832289));
#45678=CARTESIAN_POINT('Ctrl Pts',(-0.429593854357203,0.319434907277163,
2.40133130890081));
#45679=CARTESIAN_POINT('Ctrl Pts',(-0.469702051421616,0.6363098000952,2.33633252607298));
#45680=CARTESIAN_POINT('Ctrl Pts',(-0.501938131550647,0.794772684000836,
2.2709886809046));
#45681=CARTESIAN_POINT('Ctrl Pts',(-0.497754652750861,1.06847604194519,
2.22378244535553));
#45682=CARTESIAN_POINT('Ctrl Pts',(-0.484798075460762,1.18514270861194,
2.21206487283401));
#45683=CARTESIAN_POINT('Ctrl Pts',(-0.460695793839825,1.30000000000024,
2.20906355799674));
#45684=CARTESIAN_POINT('Ctrl Pts',(-0.203987185474402,-1.30000000000052,
2.214758458624));
#45685=CARTESIAN_POINT('Ctrl Pts',(-0.23961805702658,-1.18514270861213,
2.22151036131582));
#45686=CARTESIAN_POINT('Ctrl Pts',(-0.267751852323117,-1.06847604194529,
2.23655683376414));
#45687=CARTESIAN_POINT('Ctrl Pts',(-0.315426801669056,-0.794772684000844,
2.29047931061677));
#45688=CARTESIAN_POINT('Ctrl Pts',(-0.318775093621048,-0.636309800095191,
2.35857908568481));
#45689=CARTESIAN_POINT('Ctrl Pts',(-0.342581858116448,-0.319434907277156,
2.42886303170086));
#45690=CARTESIAN_POINT('Ctrl Pts',(-0.344246402265609,-0.158333333333331,
2.47140640159224));
#45691=CARTESIAN_POINT('Ctrl Pts',(-0.37623154697275,0.158333333333332,
2.47388795006401));
#45692=CARTESIAN_POINT('Ctrl Pts',(-0.407774234211117,0.319434907277162,
2.43398194626325));
#45693=CARTESIAN_POINT('Ctrl Pts',(-0.446629603902531,0.636309800095197,
2.36843534653642));
#45694=CARTESIAN_POINT('Ctrl Pts',(-0.476792671236336,0.794772684000832,
2.30338734799053));
#45695=CARTESIAN_POINT('Ctrl Pts',(-0.475569911788654,1.06847604194519,
2.25170214312543));
#45696=CARTESIAN_POINT('Ctrl Pts',(-0.465073405724185,1.18514270861194,
2.23705598928701));
#45697=CARTESIAN_POINT('Ctrl Pts',(-0.444609680852444,1.30000000000024,
2.23013629167068));
#45698=CARTESIAN_POINT('Ctrl Pts',(-0.196765310466802,-1.30000000000052,
2.22675804947393));
#45699=CARTESIAN_POINT('Ctrl Pts',(-0.230479558059957,-1.18514270861213,
2.23570308762627));
#45700=CARTESIAN_POINT('Ctrl Pts',(-0.257286379630178,-1.06847604194529,
2.25237013581518));
#45701=CARTESIAN_POINT('Ctrl Pts',(-0.303257964204822,-0.794772684000841,
2.30871373933043));
#45702=CARTESIAN_POINT('Ctrl Pts',(-0.307547430038605,-0.636309800095188,
2.37653176265635));
#45703=CARTESIAN_POINT('Ctrl Pts',(-0.331675110731546,-0.319434907277154,
2.44697160924118));
#45704=CARTESIAN_POINT('Ctrl Pts',(-0.334160629348225,-0.15833333333333,
2.48885337959328));
#45705=CARTESIAN_POINT('Ctrl Pts',(-0.365788030374307,0.158333333333332,
2.49122950080718));
#45706=CARTESIAN_POINT('Ctrl Pts',(-0.395864725591021,0.319434907277162,
2.4518083484711));
#45707=CARTESIAN_POINT('Ctrl Pts',(-0.434255637160026,0.636309800095196,
2.38603637581062));
#45708=CARTESIAN_POINT('Ctrl Pts',(-0.464309478206796,0.794772684000828,
2.32144581257927));
#45709=CARTESIAN_POINT('Ctrl Pts',(-0.464699374822084,1.06847604194518,
2.26731063655238));
#45710=CARTESIAN_POINT('Ctrl Pts',(-0.455323241083783,1.18514270861193,
2.25099782135537));
#45711=CARTESIAN_POINT('Ctrl Pts',(-0.436402201809517,1.30000000000024,
2.24180530275743));
#45712=CARTESIAN_POINT('Ctrl Pts',(-0.195199715251824,-1.30000000000052,
2.22943365900812));
#45713=CARTESIAN_POINT('Ctrl Pts',(-0.228511605709378,-1.18514270861213,
2.23887200063285));
#45714=CARTESIAN_POINT('Ctrl Pts',(-0.255035966884731,-1.06847604194529,
2.25590238609696));
#45715=CARTESIAN_POINT('Ctrl Pts',(-0.300631996897572,-0.794772684000841,
2.31278512348812));
#45716=CARTESIAN_POINT('Ctrl Pts',(-0.3050843378607,-0.636309800095188,
2.38052940242937));
#45717=CARTESIAN_POINT('Ctrl Pts',(-0.329268192136499,-0.319434907277154,
2.45100060187918));
#45718=CARTESIAN_POINT('Ctrl Pts',(-0.331946826089393,-0.15833333333333,
2.49273820395524));
#45719=CARTESIAN_POINT('Ctrl Pts',(-0.363497908369338,0.158333333333332,
2.49509203294361));
#45720=CARTESIAN_POINT('Ctrl Pts',(-0.393261813609874,0.319434907277162,
2.4557823768547));
#45721=CARTESIAN_POINT('Ctrl Pts',(-0.431529408639268,0.636309800095196,
2.38995478658298));
#45722=CARTESIAN_POINT('Ctrl Pts',(-0.461506431291599,0.794772684000829,
2.32545116428567));
#45723=CARTESIAN_POINT('Ctrl Pts',(-0.462246199763164,1.06847604194518,
2.27076906174921));
#45724=CARTESIAN_POINT('Ctrl Pts',(-0.453125679257506,1.18514270861193,
2.25408765585355));
#45725=CARTESIAN_POINT('Ctrl Pts',(-0.434564419885971,1.30000000000024,
2.24439470007868));
#45726=CARTESIAN_POINT('Ctrl Pts',(-0.192498978829482,-1.30000000000052,
2.23412609993294));
#45727=CARTESIAN_POINT('Ctrl Pts',(-0.225164896758017,-1.18514270861213,
2.24444120170032));
#45728=CARTESIAN_POINT('Ctrl Pts',(-0.251230206622433,-1.06847604194529,
2.26211564508765));
#45729=CARTESIAN_POINT('Ctrl Pts',(-0.296197561681345,-0.794772684000842,
2.31994869644595));
#45730=CARTESIAN_POINT('Ctrl Pts',(-0.300879303052548,-0.636309800095188,
2.38755164020039));
#45731=CARTESIAN_POINT('Ctrl Pts',(-0.325102701053619,-0.319434907277154,
2.45806382649142));
#45732=CARTESIAN_POINT('Ctrl Pts',(-0.328044816463848,-0.15833333333333,
2.49953034053383));
#45733=CARTESIAN_POINT('Ctrl Pts',(-0.35945797715739,0.158333333333332,
2.50184484158941));
#45734=CARTESIAN_POINT('Ctrl Pts',(-0.388773823191552,0.319434907277163,
2.46275680073802));
#45735=CARTESIAN_POINT('Ctrl Pts',(-0.426815973398791,0.636309800095197,
2.39682877981381));
#45736=CARTESIAN_POINT('Ctrl Pts',(-0.456543389710484,0.794772684000829,
2.33244524985028));
#45737=CARTESIAN_POINT('Ctrl Pts',(-0.457879092298719,1.06847604194518,
2.27680127571584));
#45738=CARTESIAN_POINT('Ctrl Pts',(-0.449218539438891,1.18514270861193,
2.25947826437128));
#45739=CARTESIAN_POINT('Ctrl Pts',(-0.431319257561445,1.30000000000024,
2.24891845627251));
#45740=CARTESIAN_POINT('Ctrl Pts',(-0.188774259644139,-1.30000000000052,
2.24086591573252));
#45741=CARTESIAN_POINT('Ctrl Pts',(-0.220761800809493,-1.18514270861213,
2.25249001056503));
#45742=CARTESIAN_POINT('Ctrl Pts',(-0.246313953205146,-1.06847604194529,
2.27111754735347));
#45743=CARTESIAN_POINT('Ctrl Pts',(-0.290477501476522,-0.794772684000842,
2.3303302357127));
#45744=CARTESIAN_POINT('Ctrl Pts',(-0.295187700097743,-0.636309800095188,
2.39766367135058));
#45745=CARTESIAN_POINT('Ctrl Pts',(-0.319235607269039,-0.319434907277154,
2.46817891569942));
#45746=CARTESIAN_POINT('Ctrl Pts',(-0.322322740325068,-0.15833333333333,
2.5091980855775));
#45747=CARTESIAN_POINT('Ctrl Pts',(-0.353563922818734,0.158333333333332,
2.51146496858702));
#45748=CARTESIAN_POINT('Ctrl Pts',(-0.382669103484203,0.319434907277162,
2.47280848790605));
#45749=CARTESIAN_POINT('Ctrl Pts',(-0.420319849785342,0.636309800095197,
2.40671557072077));
#45750=CARTESIAN_POINT('Ctrl Pts',(-0.449113853348591,0.794772684000829,
2.34234273613684));
#45751=CARTESIAN_POINT('Ctrl Pts',(-0.451226557067176,1.06847604194518,
2.28530388129556));
#45752=CARTESIAN_POINT('Ctrl Pts',(-0.443293415857577,1.18514270861193,
2.26708407448722));
#45753=CARTESIAN_POINT('Ctrl Pts',(-0.42651262228199,1.30000000000024,2.25533446763348));
#45754=CARTESIAN_POINT('Ctrl Pts',(-0.184328545390968,-1.30000000000052,
2.24896206272598));
#45755=CARTESIAN_POINT('Ctrl Pts',(-0.215531490467412,-1.18514270861213,
2.26216516228258));
#45756=CARTESIAN_POINT('Ctrl Pts',(-0.24050201101214,-1.06847604194529,
2.28194518505679));
#45757=CARTESIAN_POINT('Ctrl Pts',(-0.283790761345431,-0.794772684000842,
2.34283500298682));
#45758=CARTESIAN_POINT('Ctrl Pts',(-0.288643793743644,-0.636309800095188,
2.40986833321706));
#45759=CARTESIAN_POINT('Ctrl Pts',(-0.312515191936046,-0.319434907277154,
2.48039519284905));
#45760=CARTESIAN_POINT('Ctrl Pts',(-0.315731313772672,-0.15833333333333,
2.52086741844874));
#45761=CARTESIAN_POINT('Ctrl Pts',(-0.34669078838051,0.158333333333332,
2.52306197531978));
#45762=CARTESIAN_POINT('Ctrl Pts',(-0.375413617338691,0.319434907277163,
2.48489524842215));
#45763=CARTESIAN_POINT('Ctrl Pts',(-0.41260931729808,0.636309800095197,
2.41861256260139));
#45764=CARTESIAN_POINT('Ctrl Pts',(-0.44050809088814,0.794772684000828,
2.35431264723303));
#45765=CARTESIAN_POINT('Ctrl Pts',(-0.443527260501794,1.06847604194518,
2.29559133893406));
#45766=CARTESIAN_POINT('Ctrl Pts',(-0.436404963162388,1.18514270861193,
2.27627729439076));
#45767=CARTESIAN_POINT('Ctrl Pts',(-0.420853481829084,1.30000000000024,
2.26306748382789));
#45768=CARTESIAN_POINT('Ctrl Pts',(-0.174910013499284,-1.30000000000052,
2.26503509219293));
#45769=CARTESIAN_POINT('Ctrl Pts',(-0.203859450038737,-1.18514270861213,
2.28124294331675));
#45770=CARTESIAN_POINT('Ctrl Pts',(-0.22727026814655,-1.06847604194529,
2.303239677686));
#45771=CARTESIAN_POINT('Ctrl Pts',(-0.268558624719782,-0.794772684000844,
2.36743001286962));
#45772=CARTESIAN_POINT('Ctrl Pts',(-0.274445600499521,-0.63630980009519,
2.43403204898114));
#45773=CARTESIAN_POINT('Ctrl Pts',(-0.298847530016446,-0.319434907277155,
2.50478811328702));
#45774=CARTESIAN_POINT('Ctrl Pts',(-0.303369005641152,-0.158333333333331,
2.54441508328069));
#45775=CARTESIAN_POINT('Ctrl Pts',(-0.33395136203271,0.158333333333332,
2.54650477121987));
#45776=CARTESIAN_POINT('Ctrl Pts',(-0.360815451669037,0.319434907277163,
2.50904263688917));
#45777=CARTESIAN_POINT('Ctrl Pts',(-0.397071501484818,0.636309800095199,
2.44239004595036));
#45778=CARTESIAN_POINT('Ctrl Pts',(-0.42418690064276,0.794772684000832,
2.37852820842571));
#45779=CARTESIAN_POINT('Ctrl Pts',(-0.429032737882111,1.06847604194518,
2.31644541810441));
#45780=CARTESIAN_POINT('Ctrl Pts',(-0.423348465701274,1.18514270861193,
2.29488743588331));
#45781=CARTESIAN_POINT('Ctrl Pts',(-0.409882337954649,1.30000000000024,
2.2786448109771));
#45782=CARTESIAN_POINT('Ctrl Pts',(-0.161385254501694,-1.30000000000053,
2.2892981725789));
#45783=CARTESIAN_POINT('Ctrl Pts',(-0.187539772745063,-1.18514270861214,
2.31015635569105));
#45784=CARTESIAN_POINT('Ctrl Pts',(-0.209011612456179,-1.06847604194529,
2.33557535851787));
#45785=CARTESIAN_POINT('Ctrl Pts',(-0.247797933439514,-0.794772684000842,
2.40483474603162));
#45786=CARTESIAN_POINT('Ctrl Pts',(-0.255171667431664,-0.636309800095193,
2.47076334358962));
#45787=CARTESIAN_POINT('Ctrl Pts',(-0.279737090842208,-0.319434907277158,
2.54171341616012));
#45788=CARTESIAN_POINT('Ctrl Pts',(-0.285111694857768,-0.158333333333332,
2.5798145786153));
#45789=CARTESIAN_POINT('Ctrl Pts',(-0.314492438641538,0.158333333333333,
2.58160947030076));
#45790=CARTESIAN_POINT('Ctrl Pts',(-0.338654340348441,0.319434907277165,
2.54524103218855));
#45791=CARTESIAN_POINT('Ctrl Pts',(-0.373618100687796,0.636309800095203,
2.47807365514528));
#45792=CARTESIAN_POINT('Ctrl Pts',(-0.399938319148561,0.794772684000837,
2.4149649714314));
#45793=CARTESIAN_POINT('Ctrl Pts',(-0.407722780808801,1.06847604194519,
2.3478777040346));
#45794=CARTESIAN_POINT('Ctrl Pts',(-0.404239921251716,1.18514270861194,
2.32295585827381));
#45795=CARTESIAN_POINT('Ctrl Pts',(-0.393904597127559,1.30000000000024,
2.30215175898006));
#45796=CARTESIAN_POINT('Ctrl Pts',(-0.146809047088256,-1.30000000000053,
2.31639257663108));
#45797=CARTESIAN_POINT('Ctrl Pts',(-0.17035904517932,-1.18514270861214,
2.34253335301815));
#45798=CARTESIAN_POINT('Ctrl Pts',(-0.189882529958076,-1.0684760419453,
2.37180591564467));
#45799=CARTESIAN_POINT('Ctrl Pts',(-0.225683634204065,-0.79477268400085,
2.44666644399284));
#45800=CARTESIAN_POINT('Ctrl Pts',(-0.233149339068538,-0.636309800095195,
2.51151894746034));
#45801=CARTESIAN_POINT('Ctrl Pts',(-0.257520567695809,-0.319434907277158,
2.58260649354533));
#45802=CARTESIAN_POINT('Ctrl Pts',(-0.264089158815809,-0.158333333333332,
2.61904131619651));
#45803=CARTESIAN_POINT('Ctrl Pts',(-0.293310913161025,0.158333333333334,
2.62079205167843));
#45804=CARTESIAN_POINT('Ctrl Pts',(-0.316494245938754,0.319434907277166,
2.58614460955811));
#45805=CARTESIAN_POINT('Ctrl Pts',(-0.350565709671562,0.636309800095204,
2.51854854226647));
#45806=CARTESIAN_POINT('Ctrl Pts',(-0.374729044259226,0.794772684000838,
2.45598692227775));
#45807=CARTESIAN_POINT('Ctrl Pts',(-0.385059698318788,1.06847604194519,
2.38314652081434));
#45808=CARTESIAN_POINT('Ctrl Pts',(-0.383746823487437,1.18514270861194,
2.35440335971755));
#45809=CARTESIAN_POINT('Ctrl Pts',(-0.376649316470808,1.30000000000025,
2.32844694831461));
#45810=CARTESIAN_POINT('Ctrl Pts',(-0.13654826093367,-1.30000000000053,
2.33535361499277));
#45811=CARTESIAN_POINT('Ctrl Pts',(-0.15790384335973,-1.18514270861214,
2.36512816857481));
#45812=CARTESIAN_POINT('Ctrl Pts',(-0.176036468676417,-1.0684760419453,
2.3971009256881));
#45813=CARTESIAN_POINT('Ctrl Pts',(-0.210480784904201,-0.794772684000849,
2.47604268065416));
#45814=CARTESIAN_POINT('Ctrl Pts',(-0.220295824447027,-0.636309800095195,
2.54059970789379));
#45815=CARTESIAN_POINT('Ctrl Pts',(-0.245157968739213,-0.319434907277158,
2.61191683972681));
#45816=CARTESIAN_POINT('Ctrl Pts',(-0.251778225887239,-0.158333333333332,
2.64703880121469));
#45817=CARTESIAN_POINT('Ctrl Pts',(-0.279851723982855,0.158333333333334,
2.64854512769776));
#45818=CARTESIAN_POINT('Ctrl Pts',(-0.30128193470898,0.319434907277167,
2.61487674221445));
#45819=CARTESIAN_POINT('Ctrl Pts',(-0.333650395581517,0.636309800095205,
2.54673533789483));
#45820=CARTESIAN_POINT('Ctrl Pts',(-0.355724212092589,0.794772684000839,
2.48439750673184));
#45821=CARTESIAN_POINT('Ctrl Pts',(-0.367923974421454,1.06847604194519,
2.40754388914988));
#45822=CARTESIAN_POINT('Ctrl Pts',(-0.368405927183787,1.18514270861194,
2.37619008452405));
#45823=CARTESIAN_POINT('Ctrl Pts',(-0.364089007642033,1.30000000000025,
2.34674955861646));
#45824=CARTESIAN_POINT('Ctrl Pts',(-0.131007506657736,-1.30000000000053,
2.34626587470766));
#45825=CARTESIAN_POINT('Ctrl Pts',(-0.151677974919239,-1.18514270861214,
2.37822797434374));
#45826=CARTESIAN_POINT('Ctrl Pts',(-0.169230547683712,-1.0684760419453,
2.41178482509803));
#45827=CARTESIAN_POINT('Ctrl Pts',(-0.202577539818775,-0.794772684000848,
2.49299205747734));
#45828=CARTESIAN_POINT('Ctrl Pts',(-0.211744813925583,-0.636309800095194,
2.55698483279202));
#45829=CARTESIAN_POINT('Ctrl Pts',(-0.236497253167826,-0.319434907277158,
2.62835347341668));
#45830=CARTESIAN_POINT('Ctrl Pts',(-0.244001971332526,-0.158333333333332,
2.66288630110204));
#45831=CARTESIAN_POINT('Ctrl Pts',(-0.27224584620091,0.158333333333334,
2.66442924486541));
#45832=CARTESIAN_POINT('Ctrl Pts',(-0.293250336416526,0.319434907277167,
2.6314482563698));
#45833=CARTESIAN_POINT('Ctrl Pts',(-0.325488171395546,0.636309800095204,
2.56320436175243));
#45834=CARTESIAN_POINT('Ctrl Pts',(-0.347152213240066,0.794772684000837,
2.50122002778829));
#45835=CARTESIAN_POINT('Ctrl Pts',(-0.360242452059197,1.06847604194519,
2.42203040362271));
#45836=CARTESIAN_POINT('Ctrl Pts',(-0.361398471314416,1.18514270861194,
2.38909240542061));
#45837=CARTESIAN_POINT('Ctrl Pts',(-0.358044230481204,1.30000000000025,
2.35749466305292));
#45838=CARTESIAN_POINT('Ctrl Pts',(-0.117086432067252,-1.30000000000053,
2.37352320141344));
#45839=CARTESIAN_POINT('Ctrl Pts',(-0.135464168151512,-1.18514270861214,
2.41084675042037));
#45840=CARTESIAN_POINT('Ctrl Pts',(-0.151415182366122,-1.0684760419453,
2.44833956525444));
#45841=CARTESIAN_POINT('Ctrl Pts',(-0.182659003208377,-0.794772684000852,
2.53534650585518));
#45842=CARTESIAN_POINT('Ctrl Pts',(-0.192742903268561,-0.636309800095196,
2.59843213671961));
#45843=CARTESIAN_POINT('Ctrl Pts',(-0.218000695569017,-0.319434907277158,
2.67008470161751));
#45844=CARTESIAN_POINT('Ctrl Pts',(-0.227426550264204,-0.158333333333332,
2.70309560096028));
#45845=CARTESIAN_POINT('Ctrl Pts',(-0.254291257836203,0.158333333333334,
2.7043467724717));
#45846=CARTESIAN_POINT('Ctrl Pts',(-0.271370755899094,0.319434907277166,
2.67248169616074));
#45847=CARTESIAN_POINT('Ctrl Pts',(-0.301566418481218,0.636309800095204,
2.60359226481184));
#45848=CARTESIAN_POINT('Ctrl Pts',(-0.322608338668808,0.794772684000839,
2.54251943597892));
#45849=CARTESIAN_POINT('Ctrl Pts',(-0.338076543906821,1.06847604194519,
2.45752302061236));
#45850=CARTESIAN_POINT('Ctrl Pts',(-0.341108322545931,1.18514270861194,
2.42067933094224));
#45851=CARTESIAN_POINT('Ctrl Pts',(-0.340476266930105,1.30000000000025,
2.38378375038661));
#45852=CARTESIAN_POINT('Ctrl Pts',(-0.102459815942602,-1.30000000000054,
2.40364627470184));
#45853=CARTESIAN_POINT('Ctrl Pts',(-0.117674774015024,-1.18514270861215,
2.44677221732563));
#45854=CARTESIAN_POINT('Ctrl Pts',(-0.131530737499575,-1.0684760419453,
2.4885471284722));
#45855=CARTESIAN_POINT('Ctrl Pts',(-0.16040123566095,-0.794772684000851,
2.58193437727779));
#45856=CARTESIAN_POINT('Ctrl Pts',(-0.172912540708817,-0.6363098000952,
2.64425616831593));
#45857=CARTESIAN_POINT('Ctrl Pts',(-0.1989153384542,-0.319434907277161,
2.71624566671582));
#45858=CARTESIAN_POINT('Ctrl Pts',(-0.208972852561719,-0.158333333333333,
2.74727571056124));
#45859=CARTESIAN_POINT('Ctrl Pts',(-0.235436629275575,0.158333333333335,
2.74847840266072));
#45860=CARTESIAN_POINT('Ctrl Pts',(-0.251633688396625,0.319434907277168,
2.71862485889545));
#45861=CARTESIAN_POINT('Ctrl Pts',(-0.27996183079859,0.636309800095209,
2.64913850896298));
#45862=CARTESIAN_POINT('Ctrl Pts',(-0.297052837237228,0.794772684000849,
2.58836982198733));
#45863=CARTESIAN_POINT('Ctrl Pts',(-0.314711528711115,1.0684760419452,2.49688671813418));
#45864=CARTESIAN_POINT('Ctrl Pts',(-0.320125739500395,1.18514270861194,
2.4558064169721));
#45865=CARTESIAN_POINT('Ctrl Pts',(-0.323310367858915,1.30000000000024,
2.41324546052289));
#45866=CARTESIAN_POINT('Ctrl Pts',(-0.0865550189114888,-1.30000000000053,
2.43952180316623));
#45867=CARTESIAN_POINT('Ctrl Pts',(-0.0998021354031824,-1.18514270861214,
2.48981119458842));
#45868=CARTESIAN_POINT('Ctrl Pts',(-0.112284312155286,-1.0684760419453,
2.53683713334547));
#45869=CARTESIAN_POINT('Ctrl Pts',(-0.139353473679405,-0.794772684000851,
2.63793723087301));
#45870=CARTESIAN_POINT('Ctrl Pts',(-0.152637834139488,-0.636309800095197,
2.69899428288379));
#45871=CARTESIAN_POINT('Ctrl Pts',(-0.179118060090335,-0.319434907277159,
2.77130691967836));
#45872=CARTESIAN_POINT('Ctrl Pts',(-0.190776149896774,-0.158333333333333,
2.80013566926875));
#45873=CARTESIAN_POINT('Ctrl Pts',(-0.216342800555802,0.158333333333334,
2.80120353145493));
#45874=CARTESIAN_POINT('Ctrl Pts',(-0.230069884093391,0.319434907277167,
2.7734491731441));
#45875=CARTESIAN_POINT('Ctrl Pts',(-0.256036740898905,0.636309800095206,
2.70329839544103));
#45876=CARTESIAN_POINT('Ctrl Pts',(-0.270614438129939,0.794772684000843,
2.64345562366289));
#45877=CARTESIAN_POINT('Ctrl Pts',(-0.289603342540349,1.0684760419452,2.54405830878662));
#45878=CARTESIAN_POINT('Ctrl Pts',(-0.296607782659313,1.18514270861194,
2.49769499621475));
#45879=CARTESIAN_POINT('Ctrl Pts',(-0.302397069786226,1.30000000000025,
2.44799378564747));
#45880=CARTESIAN_POINT('Ctrl Pts',(-0.0768451818344205,-1.30000000000054,
2.46162868799514));
#45881=CARTESIAN_POINT('Ctrl Pts',(-0.0886298667164653,-1.18514270861215,
2.51630195144563));
#45882=CARTESIAN_POINT('Ctrl Pts',(-0.100195850955182,-1.0684760419453,
2.56655815518386));
#45883=CARTESIAN_POINT('Ctrl Pts',(-0.12641034607682,-0.794772684000849,
2.67245574797313));
#45884=CARTESIAN_POINT('Ctrl Pts',(-0.141376457236268,-0.636309800095196,
2.73290525740483));
#45885=CARTESIAN_POINT('Ctrl Pts',(-0.168174688062727,-0.319434907277159,
2.80543061378637));
#45886=CARTESIAN_POINT('Ctrl Pts',(-0.179809506090771,-0.158333333333332,
2.83277077134714));
#45887=CARTESIAN_POINT('Ctrl Pts',(-0.204422827610632,0.158333333333334,
2.83370548581378));
#45888=CARTESIAN_POINT('Ctrl Pts',(-0.216900306221677,0.319434907277168,
2.80728899553676));
#45889=CARTESIAN_POINT('Ctrl Pts',(-0.241258190720355,0.636309800095206,
2.7366900875382));
#45890=CARTESIAN_POINT('Ctrl Pts',(-0.253585277081685,0.79477268400084,
2.67725991227328));
#45891=CARTESIAN_POINT('Ctrl Pts',(-0.273931795003457,1.06847604194519,
2.57308619511324));
#45892=CARTESIAN_POINT('Ctrl Pts',(-0.282418983421977,1.18514270861194,
2.52356751859579));
#45893=CARTESIAN_POINT('Ctrl Pts',(-0.29058610656347,1.30000000000025,2.46962310770284));
#45894=CARTESIAN_POINT('Ctrl Pts',(-0.0646419694895159,-1.30000000000053,
2.49219986215409));
#45895=CARTESIAN_POINT('Ctrl Pts',(-0.0746299031266144,-1.18514270861214,
2.55291253567633));
#45896=CARTESIAN_POINT('Ctrl Pts',(-0.085042776570219,-1.0684760419453,
2.60760959069788));
#45897=CARTESIAN_POINT('Ctrl Pts',(-0.11008029327507,-0.794772684000852,
2.72007344774905));
#45898=CARTESIAN_POINT('Ctrl Pts',(-0.12639262512847,-0.636309800095197,
2.77954489993001));
#45899=CARTESIAN_POINT('Ctrl Pts',(-0.154435156546678,-0.319434907277159,
2.8524506143583));
#45900=CARTESIAN_POINT('Ctrl Pts',(-0.168270150482634,-0.158333333333332,
2.8780204502782));
#45901=CARTESIAN_POINT('Ctrl Pts',(-0.192020606839366,0.158333333333334,
2.87885542318024));
#45902=CARTESIAN_POINT('Ctrl Pts',(-0.201146304914863,0.319434907277166,
2.85409248168455));
#45903=CARTESIAN_POINT('Ctrl Pts',(-0.223090436112119,0.636309800095205,
2.78294474077531));
#45904=CARTESIAN_POINT('Ctrl Pts',(-0.234079952238902,0.794772684000841,
2.72448047421197));
#45905=CARTESIAN_POINT('Ctrl Pts',(-0.255131024103306,1.06847604194519,
2.61355633361972));
#45906=CARTESIAN_POINT('Ctrl Pts',(-0.264576696026548,1.18514270861194,
2.55949554128694));
#45907=CARTESIAN_POINT('Ctrl Pts',(-0.274355810882019,1.30000000000025,
2.4993889069393));
#45908=CARTESIAN_POINT('Ctrl Pts',(-0.0519913323925298,-1.30000000000053,
2.52275042090885));
#45909=CARTESIAN_POINT('Ctrl Pts',(-0.0603550360115123,-1.18514270861215,
2.58957328418298));
#45910=CARTESIAN_POINT('Ctrl Pts',(-0.0699500144714583,-1.0684760419453,
2.64878750700434));
#45911=CARTESIAN_POINT('Ctrl Pts',(-0.0949608253810958,-0.794772684000853,
2.76800672593707));
#45912=CARTESIAN_POINT('Ctrl Pts',(-0.114769504529623,-0.636309800095196,
2.82673663023976));
#45913=CARTESIAN_POINT('Ctrl Pts',(-0.144041513703257,-0.319434907277158,
2.90003545779939));
#45914=CARTESIAN_POINT('Ctrl Pts',(-0.157655646790745,-0.158333333333332,
2.92354881563667));
#45915=CARTESIAN_POINT('Ctrl Pts',(-0.180115264216867,0.158333333333334,
2.92426615222108));
#45916=CARTESIAN_POINT('Ctrl Pts',(-0.187731724656436,0.319434907277168,
2.90145517946238));
#45917=CARTESIAN_POINT('Ctrl Pts',(-0.20671177222343,0.636309800095206,
2.82964797001604));
#45918=CARTESIAN_POINT('Ctrl Pts',(-0.213393728431101,0.79477268400084,
2.77160923968283));
#45919=CARTESIAN_POINT('Ctrl Pts',(-0.235286231852892,1.06847604194519,
2.65393411759689));
#45920=CARTESIAN_POINT('Ctrl Pts',(-0.246410895641012,1.18514270861195,
2.59544671058704));
#45921=CARTESIAN_POINT('Ctrl Pts',(-0.259183769683156,1.30000000000025,
2.52940909662534));
#45922=CARTESIAN_POINT('Ctrl Pts',(-0.0414484880036898,-1.30000000000054,
2.55063756703304));
#45923=CARTESIAN_POINT('Ctrl Pts',(-0.0488098275549564,-1.18514270861215,
2.62300797498182));
#45924=CARTESIAN_POINT('Ctrl Pts',(-0.0579766463248268,-1.0684760419453,
2.68631168921085));
#45925=CARTESIAN_POINT('Ctrl Pts',(-0.0833248496788771,-0.794772684000855,
2.81161005666598));
#45926=CARTESIAN_POINT('Ctrl Pts',(-0.105626363343272,-0.636309800095197,
2.86953587407838));
#45927=CARTESIAN_POINT('Ctrl Pts',(-0.136562091200086,-0.319434907277158,
2.94320934801511));
#45928=CARTESIAN_POINT('Ctrl Pts',(-0.151314127698468,-0.158333333333332,
2.9650077768798));
#45929=CARTESIAN_POINT('Ctrl Pts',(-0.172923006523827,0.158333333333334,
2.96568282352302));
#45930=CARTESIAN_POINT('Ctrl Pts',(-0.178177065531442,0.319434907277166,
2.94454480196698));
#45931=CARTESIAN_POINT('Ctrl Pts',(-0.194521822168287,0.636309800095205,
2.87227616870795));
#45932=CARTESIAN_POINT('Ctrl Pts',(-0.198901964219526,0.794772684000839,
2.81502334955911));
#45933=CARTESIAN_POINT('Ctrl Pts',(-0.220501886149653,1.06847604194519,
2.69114356802193));
#45934=CARTESIAN_POINT('Ctrl Pts',(-0.232142923985034,1.18514270861195,
2.62849680372957));
#45935=CARTESIAN_POINT('Ctrl Pts',(-0.246075193808231,1.30000000000025,
2.55682624237401));
#45936=CARTESIAN_POINT('Ctrl Pts',(-0.0349002835201406,-1.30000000000054,
2.57033915626948));
#45937=CARTESIAN_POINT('Ctrl Pts',(-0.0414916171038198,-1.18514270861215,
2.64672432756028));
#45938=CARTESIAN_POINT('Ctrl Pts',(-0.0504134225591142,-1.06847604194531,
2.71299807230647));
#45939=CARTESIAN_POINT('Ctrl Pts',(-0.0764084341946251,-0.794772684000856,
2.84274426258533));
#45940=CARTESIAN_POINT('Ctrl Pts',(-0.102183974764143,-0.636309800095198,
2.90025606522728));
#45941=CARTESIAN_POINT('Ctrl Pts',(-0.133047562883809,-0.319434907277158,
2.974084380369));
#45942=CARTESIAN_POINT('Ctrl Pts',(-0.144704112048905,-0.158333333333333,
2.99426031153481));
#45943=CARTESIAN_POINT('Ctrl Pts',(-0.165081364601521,0.158333333333334,
2.99485565250151));
#45944=CARTESIAN_POINT('Ctrl Pts',(-0.171572628444762,0.319434907277168,
2.97524810931612));
#45945=CARTESIAN_POINT('Ctrl Pts',(-0.186757244390619,0.636309800095207,
2.90268736214996));
#45946=CARTESIAN_POINT('Ctrl Pts',(-0.188248554710682,0.79477268400084,
2.84579042814529));
#45947=CARTESIAN_POINT('Ctrl Pts',(-0.209521808555664,1.0684760419452,2.71738892262339));
#45948=CARTESIAN_POINT('Ctrl Pts',(-0.221625126237946,1.18514270861195,
2.65174871878311));
#45949=CARTESIAN_POINT('Ctrl Pts',(-0.23662335826476,1.30000000000025,2.57604856509829));
#45950=CARTESIAN_POINT('Ctrl Pts',(-0.029992213072004,-1.30000000000054,
2.58428069475767));
#45951=CARTESIAN_POINT('Ctrl Pts',(-0.0369470821443265,-1.18514270861215,
2.66342490778013));
#45952=CARTESIAN_POINT('Ctrl Pts',(-0.0459491733771234,-1.0684760419453,
2.73169045003337));
#45953=CARTESIAN_POINT('Ctrl Pts',(-0.0714752977231339,-0.794772684000853,
2.86426560336564));
#45954=CARTESIAN_POINT('Ctrl Pts',(-0.0957112928916897,-0.636309800095197,
2.92106492372564));
#45955=CARTESIAN_POINT('Ctrl Pts',(-0.125688940043713,-0.319434907277158,
2.99483448775138));
#45956=CARTESIAN_POINT('Ctrl Pts',(-0.137027468646895,-0.158333333333333,
3.01402881780954));
#45957=CARTESIAN_POINT('Ctrl Pts',(-0.157981527487602,0.158333333333334,
3.01470166475779));
#45958=CARTESIAN_POINT('Ctrl Pts',(-0.166223436350055,0.319434907277168,
2.99624892902451));
#45959=CARTESIAN_POINT('Ctrl Pts',(-0.181725666151248,0.636309800095206,
2.92370987232953));
#45960=CARTESIAN_POINT('Ctrl Pts',(-0.18163490289444,0.79477268400084,2.86722018173556));
#45961=CARTESIAN_POINT('Ctrl Pts',(-0.202993381777807,1.0684760419452,2.73591708451799));
#45962=CARTESIAN_POINT('Ctrl Pts',(-0.215428171523888,1.18514270861195,
2.66830058285085));
#45963=CARTESIAN_POINT('Ctrl Pts',(-0.231052456917079,1.30000000000025,
2.58990382504281));
#45964=CARTESIAN_POINT('Ctrl Pts',(-0.0249600309789205,-1.30000000000054,
2.60124271611029));
#45965=CARTESIAN_POINT('Ctrl Pts',(-0.0323202509065839,-1.18514270861215,
2.68407081700083));
#45966=CARTESIAN_POINT('Ctrl Pts',(-0.0412013170981547,-1.0684760419453,
2.7550046780852));
#45967=CARTESIAN_POINT('Ctrl Pts',(-0.065231815765751,-0.794772684000853,
2.89139801407353));
#45968=CARTESIAN_POINT('Ctrl Pts',(-0.0861519254167174,-0.636309800095197,
2.94731896886899));
#45969=CARTESIAN_POINT('Ctrl Pts',(-0.113985772631395,-0.319434907277158,
3.02104763479761));
#45970=CARTESIAN_POINT('Ctrl Pts',(-0.125109046164334,-0.158333333333332,
3.03895956505397));
#45971=CARTESIAN_POINT('Ctrl Pts',(-0.145969402090865,0.158333333333334,
3.0396453906214));
#45972=CARTESIAN_POINT('Ctrl Pts',(-0.154682023316671,0.319434907277167,
3.02254296395726));
#45973=CARTESIAN_POINT('Ctrl Pts',(-0.171425972763991,0.636309800095205,
2.94995935209706));
#45974=CARTESIAN_POINT('Ctrl Pts',(-0.172726418166373,0.794772684000839,
2.8941285969512));
#45975=CARTESIAN_POINT('Ctrl Pts',(-0.195368882082855,1.0684760419452,2.75892839454814));
#45976=CARTESIAN_POINT('Ctrl Pts',(-0.208249374524988,1.18514270861195,
2.68864308439401));
#45977=CARTESIAN_POINT('Ctrl Pts',(-0.224209275765781,1.30000000000026,
2.60659562204482));
#45978=CARTESIAN_POINT('Ctrl Pts',(-0.0213943747864332,-1.30000000000054,
2.6127724501415));
#45979=CARTESIAN_POINT('Ctrl Pts',(-0.0303808199747979,-1.18514270861215,
2.69825565188215));
#45980=CARTESIAN_POINT('Ctrl Pts',(-0.0397026858022174,-1.0684760419453,
2.77097185413313));
#45981=CARTESIAN_POINT('Ctrl Pts',(-0.0620129494732966,-0.794772684000851,
2.90946650530856));
#45982=CARTESIAN_POINT('Ctrl Pts',(-0.076590996619337,-0.636309800095197,
2.96367751455667));
#45983=CARTESIAN_POINT('Ctrl Pts',(-0.101057989717431,-0.319434907277159,
3.03661809166351));
#45984=CARTESIAN_POINT('Ctrl Pts',(-0.112567852729613,-0.158333333333332,
3.05351876196813));
#45985=CARTESIAN_POINT('Ctrl Pts',(-0.133278717910193,0.158333333333334,
3.05415093470282));
#45986=CARTESIAN_POINT('Ctrl Pts',(-0.141607349608986,0.319434907277167,
3.0379582636565));
#45987=CARTESIAN_POINT('Ctrl Pts',(-0.161103853485778,0.636309800095206,
2.96615092372332));
#45988=CARTESIAN_POINT('Ctrl Pts',(-0.167600922680341,0.79477268400084,
2.91217535482969));
#45989=CARTESIAN_POINT('Ctrl Pts',(-0.192015477656447,1.0684760419452,2.77486868997395));
#45990=CARTESIAN_POINT('Ctrl Pts',(-0.204772182759206,1.18514270861195,
2.70277064221539));
#45991=CARTESIAN_POINT('Ctrl Pts',(-0.219717436763986,1.30000000000025,
2.61800951420097));
#45992=CARTESIAN_POINT('Ctrl Pts',(-0.0165023515695407,-1.30000000000054,
2.61984802158576));
#45993=CARTESIAN_POINT('Ctrl Pts',(-0.0256069538907616,-1.18514270861215,
2.70510942351974));
#45994=CARTESIAN_POINT('Ctrl Pts',(-0.0347010954711869,-1.0684760419453,
2.77756665167126));
#45995=CARTESIAN_POINT('Ctrl Pts',(-0.0556862153948436,-0.794772684000851,
2.91537714081635));
#45996=CARTESIAN_POINT('Ctrl Pts',(-0.0677962068234773,-0.636309800095197,
2.9688868910723));
#45997=CARTESIAN_POINT('Ctrl Pts',(-0.090659738426676,-0.319434907277159,
3.04130452642146));
#45998=CARTESIAN_POINT('Ctrl Pts',(-0.102179986998412,-0.158333333333332,
3.05825650250268));
#45999=CARTESIAN_POINT('Ctrl Pts',(-0.122673368892049,0.158333333333334,
3.05879493020897));
#46000=CARTESIAN_POINT('Ctrl Pts',(-0.130506918224617,0.319434907277167,
3.04237334549098));
#46001=CARTESIAN_POINT('Ctrl Pts',(-0.151708180499798,0.636309800095206,
2.97106881806364));
#46002=CARTESIAN_POINT('Ctrl Pts',(-0.161724215836604,0.79477268400084,
2.91805939711538));
#46003=CARTESIAN_POINT('Ctrl Pts',(-0.187312562460002,1.0684760419452,2.78141067466404));
#46004=CARTESIAN_POINT('Ctrl Pts',(-0.199984062839926,1.18514270861195,
2.70950503030696));
#46005=CARTESIAN_POINT('Ctrl Pts',(-0.214250816488192,1.30000000000025,
2.62484391020782));
#46006=CARTESIAN_POINT('Ctrl Pts',(-0.0165023515695832,-1.3,2.61984802158616));
#46007=CARTESIAN_POINT('Ctrl Pts',(-0.0256069538907899,-1.18514270861178,
2.70510942351996));
#46008=CARTESIAN_POINT('Ctrl Pts',(-0.0347010954712011,-1.06847604194512,
2.77756665167135));
#46009=CARTESIAN_POINT('Ctrl Pts',(-0.0556862153948436,-0.794772684000851,
2.91537714081636));
#46010=CARTESIAN_POINT('Ctrl Pts',(-0.0677962068234773,-0.636309800095197,
2.9688868910723));
#46011=CARTESIAN_POINT('Ctrl Pts',(-0.0906597384266761,-0.319434907277159,
3.04130452642146));
#46012=CARTESIAN_POINT('Ctrl Pts',(-0.102179986998412,-0.158333333333332,
3.05825650250268));
#46013=CARTESIAN_POINT('Ctrl Pts',(-0.122673368892049,0.158333333333334,
3.05879493020897));
#46014=CARTESIAN_POINT('Ctrl Pts',(-0.130506918224617,0.319434907277167,
3.04237334549098));
#46015=CARTESIAN_POINT('Ctrl Pts',(-0.151708180499798,0.636309800095206,
2.97106881806364));
#46016=CARTESIAN_POINT('Ctrl Pts',(-0.161724215836604,0.79477268400084,
2.91805939711539));
#46017=CARTESIAN_POINT('Ctrl Pts',(-0.187312562459994,1.06847604194511,
2.78141067466408));
#46018=CARTESIAN_POINT('Ctrl Pts',(-0.199984062839908,1.18514270861178,
2.70950503030707));
#46019=CARTESIAN_POINT('Ctrl Pts',(-0.214250816488161,1.3,2.624843910208));
#46020=CARTESIAN_POINT('',(-0.213845469209945,-1.2,2.25462133752143));
#46021=CARTESIAN_POINT('Ctrl Pts',(-0.213845469209944,-1.2,2.25462133752143));
#46022=CARTESIAN_POINT('Ctrl Pts',(-0.204548853415621,-1.21101439883804,
2.2652440296684));
#46023=CARTESIAN_POINT('Ctrl Pts',(-0.194573317233004,-1.22173223319652,
2.27556637829925));
#46024=CARTESIAN_POINT('Ctrl Pts',(-0.176328391038453,-1.24278214089401,
2.29594391828212));
#46025=CARTESIAN_POINT('Ctrl Pts',(-0.167981216328268,-1.25266380271579,
2.30553832043326));
#46026=CARTESIAN_POINT('Ctrl Pts',(-0.146537790562717,-1.27799030514101,
2.33017925706331));
#46027=CARTESIAN_POINT('Ctrl Pts',(-0.143784999781138,-1.28105852037737,
2.33315876593495));
#46028=CARTESIAN_POINT('Ctrl Pts',(-0.128236474659343,-1.30000000000053,
2.35169561531438));
#46029=CARTESIAN_POINT('',(-0.370132009002969,-0.653834841418298,2.26385754909195));
#46030=CARTESIAN_POINT('Ctrl Pts',(-0.370132009002236,-0.653834841417621,
2.26385754906608));
#46031=CARTESIAN_POINT('Ctrl Pts',(-0.353920813038246,-0.717904873026858,
2.26264196775129));
#46032=CARTESIAN_POINT('Ctrl Pts',(-0.340646889995177,-0.76404242422158,
2.26170713554667));
#46033=CARTESIAN_POINT('Ctrl Pts',(-0.288948198313244,-0.949534604808305,
2.2583154474792));
#46034=CARTESIAN_POINT('Ctrl Pts',(-0.26137863609437,-1.04690484158362,
2.25667674178249));
#46035=CARTESIAN_POINT('Ctrl Pts',(-0.213845469209944,-1.2,2.25462133752143));
#46036=CARTESIAN_POINT('',(-0.509087305687289,0.653834841531101,2.27624836987201));
#46037=CARTESIAN_POINT('Ctrl Pts',(-0.509087305687289,0.6538348415311,2.27624836987201));
#46038=CARTESIAN_POINT('Ctrl Pts',(-0.487804298623256,0.576020454349171,
2.31193596787054));
#46039=CARTESIAN_POINT('Ctrl Pts',(-0.469211503005726,0.493680567759374,
2.34174637720171));
#46040=CARTESIAN_POINT('Ctrl Pts',(-0.440310963817089,0.338203591218837,
2.38330062796864));
#46041=CARTESIAN_POINT('Ctrl Pts',(-0.429076774576499,0.265718926343639,
2.39725207328199));
#46042=CARTESIAN_POINT('Ctrl Pts',(-0.410674103030229,0.129747729877892,
2.41328650637845));
#46043=CARTESIAN_POINT('Ctrl Pts',(-0.403176730549767,0.0666442716359389,
2.41680861876812));
#46044=CARTESIAN_POINT('Ctrl Pts',(-0.389859613444735,-0.0595545240722367,
2.41599461060225));
#46045=CARTESIAN_POINT('Ctrl Pts',(-0.383938144316827,-0.122803979681452,
2.41166924346832));
#46046=CARTESIAN_POINT('Ctrl Pts',(-0.373622084086818,-0.260161739957788,
2.39367060768024));
#46047=CARTESIAN_POINT('Ctrl Pts',(-0.369699318789559,-0.333963904502371,
2.37843693440692));
#46048=CARTESIAN_POINT('Ctrl Pts',(-0.365858759811961,-0.491156549484106,
2.33377361115453));
#46049=CARTESIAN_POINT('Ctrl Pts',(-0.366575240625937,-0.574264393662825,
2.30223676434492));
#46050=CARTESIAN_POINT('Ctrl Pts',(-0.370132008968997,-0.653834841429853,
2.26385754911276));
#46051=CARTESIAN_POINT('',(-0.437217345759296,1.2,2.26934679859076));
#46052=CARTESIAN_POINT('Ctrl Pts',(-0.437217345759296,1.2,2.26934679859076));
#46053=CARTESIAN_POINT('Ctrl Pts',(-0.451341357509953,1.12497957419401,
2.27059922148015));
#46054=CARTESIAN_POINT('Ctrl Pts',(-0.467276251271234,1.02797670902483,
2.27207424792545));
#46055=CARTESIAN_POINT('Ctrl Pts',(-0.497443621872752,0.796118559781083,
2.27504120190078));
#46056=CARTESIAN_POINT('Ctrl Pts',(-0.50257497511006,0.741382157389922,
2.27557503273473));
#46057=CARTESIAN_POINT('Ctrl Pts',(-0.50908730568729,0.653834841531101,
2.27624836987201));
#46058=CARTESIAN_POINT('Ctrl Pts',(-0.354392897366409,1.3,2.36296519815122));
#46059=CARTESIAN_POINT('Ctrl Pts',(-0.362135051021157,1.29069343462501,
2.35420092839924));
#46060=CARTESIAN_POINT('Ctrl Pts',(-0.367601211902519,1.28348293012651,
2.34732209545957));
#46061=CARTESIAN_POINT('Ctrl Pts',(-0.414027929604089,1.22697811672721,
2.29438949053698));
#46062=CARTESIAN_POINT('Ctrl Pts',(-0.426468674120977,1.21202615146349,
2.28046701772206));
#46063=CARTESIAN_POINT('Ctrl Pts',(-0.437217345759296,1.2,2.26934679859076));
#46064=CARTESIAN_POINT('Ctrl Pts',(-0.0165023515695832,-1.3,2.61984802158616));
#46065=CARTESIAN_POINT('Ctrl Pts',(-0.0256069538907899,-1.18514270861178,
2.70510942351996));
#46066=CARTESIAN_POINT('Ctrl Pts',(-0.0347010954712011,-1.06847604194512,
2.77756665167135));
#46067=CARTESIAN_POINT('Ctrl Pts',(-0.0556862153948436,-0.794772684000851,
2.91537714081635));
#46068=CARTESIAN_POINT('Ctrl Pts',(-0.0677962068234773,-0.636309800095196,
2.9688868910723));
#46069=CARTESIAN_POINT('Ctrl Pts',(-0.090659738426676,-0.319434907277159,
3.04130452642146));
#46070=CARTESIAN_POINT('Ctrl Pts',(-0.102179986998412,-0.158333333333332,
3.05825650250268));
#46071=CARTESIAN_POINT('Ctrl Pts',(-0.122673368892049,0.158333333333334,
3.05879493020897));
#46072=CARTESIAN_POINT('Ctrl Pts',(-0.130506918224617,0.319434907277167,
3.04237334549098));
#46073=CARTESIAN_POINT('Ctrl Pts',(-0.151708180499798,0.636309800095206,
2.97106881806364));
#46074=CARTESIAN_POINT('Ctrl Pts',(-0.161724215836604,0.79477268400084,
2.91805939711539));
#46075=CARTESIAN_POINT('Ctrl Pts',(-0.187312562459994,1.06847604194511,
2.78141067466408));
#46076=CARTESIAN_POINT('Ctrl Pts',(-0.199984062839908,1.18514270861178,
2.70950503030707));
#46077=CARTESIAN_POINT('Ctrl Pts',(-0.214250816488161,1.3,2.624843910208));
#46078=CARTESIAN_POINT('Ctrl Pts',(0.0604153711163316,-1.3,2.62151331779344));
#46079=CARTESIAN_POINT('Ctrl Pts',(0.0495900516861096,-1.18514270861178,
2.70657462578233));
#46080=CARTESIAN_POINT('Ctrl Pts',(0.039303457172531,-1.06847604194512,
2.77884799266893));
#46081=CARTESIAN_POINT('Ctrl Pts',(0.0167839283489731,-0.794772684000851,
2.91627122624936));
#46082=CARTESIAN_POINT('Ctrl Pts',(0.00537192228428135,-0.636309800095196,
2.96961420006941));
#46083=CARTESIAN_POINT('Ctrl Pts',(-0.0169375195429115,-0.319434907277159,
3.04166079944464));
#46084=CARTESIAN_POINT('Ctrl Pts',(-0.0272288683682577,-0.158333333333332,
3.05843597840478));
#46085=CARTESIAN_POINT('Ctrl Pts',(-0.0477222502618953,0.158333333333334,
3.05861545430687));
#46086=CARTESIAN_POINT('Ctrl Pts',(-0.0567846993408529,0.319434907277167,
3.04201707246781));
#46087=CARTESIAN_POINT('Ctrl Pts',(-0.0785400513920393,0.636309800095206,
2.97034150906653));
#46088=CARTESIAN_POINT('Ctrl Pts',(-0.0892540720927878,0.79477268400084,
2.91716531168238));
#46089=CARTESIAN_POINT('Ctrl Pts',(-0.113308009816262,1.06847604194511,
2.78012933366651));
#46090=CARTESIAN_POINT('Ctrl Pts',(-0.124787057263008,1.18514270861178,
2.7080398280447));
#46091=CARTESIAN_POINT('Ctrl Pts',(-0.137333093802246,1.3,2.62317861400072));
#46092=CARTESIAN_POINT('Ctrl Pts',(0.137333093802246,-1.3,2.62317861400072));
#46093=CARTESIAN_POINT('Ctrl Pts',(0.124787057263009,-1.18514270861178,
2.7080398280447));
#46094=CARTESIAN_POINT('Ctrl Pts',(0.113308009816263,-1.06847604194512,
2.7801293336665));
#46095=CARTESIAN_POINT('Ctrl Pts',(0.0892540720927901,-0.794772684000851,
2.91716531168237));
#46096=CARTESIAN_POINT('Ctrl Pts',(0.0785400513920396,-0.636309800095196,
2.97034150906653));
#46097=CARTESIAN_POINT('Ctrl Pts',(0.0567846993408532,-0.319434907277159,
3.04201707246781));
#46098=CARTESIAN_POINT('Ctrl Pts',(0.0477222502618961,-0.158333333333332,
3.05861545430687));
#46099=CARTESIAN_POINT('Ctrl Pts',(0.0272288683682586,0.158333333333334,
3.05843597840478));
#46100=CARTESIAN_POINT('Ctrl Pts',(0.0169375195429118,0.319434907277167,
3.04166079944463));
#46101=CARTESIAN_POINT('Ctrl Pts',(-0.00537192228428079,0.636309800095206,
2.96961420006942));
#46102=CARTESIAN_POINT('Ctrl Pts',(-0.016783928348971,0.79477268400084,
2.91627122624937));
#46103=CARTESIAN_POINT('Ctrl Pts',(-0.0393034571725295,1.06847604194511,
2.77884799266893));
#46104=CARTESIAN_POINT('Ctrl Pts',(-0.0495900516861082,1.18514270861178,
2.70657462578233));
#46105=CARTESIAN_POINT('Ctrl Pts',(-0.0604153711163307,1.3,2.62151331779344));
#46106=CARTESIAN_POINT('Ctrl Pts',(0.214250816488161,-1.3,2.62484391020801));
#46107=CARTESIAN_POINT('Ctrl Pts',(0.199984062839909,-1.18514270861178,
2.70950503030707));
#46108=CARTESIAN_POINT('Ctrl Pts',(0.187312562459995,-1.06847604194512,
2.78141067466408));
#46109=CARTESIAN_POINT('Ctrl Pts',(0.161724215836607,-0.794772684000851,
2.91805939711538));
#46110=CARTESIAN_POINT('Ctrl Pts',(0.151708180499798,-0.636309800095196,
2.97106881806364));
#46111=CARTESIAN_POINT('Ctrl Pts',(0.130506918224618,-0.319434907277159,
3.04237334549099));
#46112=CARTESIAN_POINT('Ctrl Pts',(0.12267336889205,-0.158333333333332,
3.05879493020897));
#46113=CARTESIAN_POINT('Ctrl Pts',(0.102179986998412,0.158333333333334,
3.05825650250268));
#46114=CARTESIAN_POINT('Ctrl Pts',(0.0906597384266764,0.319434907277167,
3.04130452642146));
#46115=CARTESIAN_POINT('Ctrl Pts',(0.0677962068234778,0.636309800095206,
2.9688868910723));
#46116=CARTESIAN_POINT('Ctrl Pts',(0.0556862153948456,0.79477268400084,
2.91537714081636));
#46117=CARTESIAN_POINT('Ctrl Pts',(0.0347010954712027,1.06847604194511,
2.77756665167135));
#46118=CARTESIAN_POINT('Ctrl Pts',(0.0256069538907915,1.18514270861178,
2.70510942351996));
#46119=CARTESIAN_POINT('Ctrl Pts',(0.0165023515695843,1.3,2.61984802158616));
#46120=CARTESIAN_POINT('Ctrl Pts',(0.214250816488161,-1.3,2.62484391020801));
#46121=CARTESIAN_POINT('Ctrl Pts',(0.199984062839909,-1.18514270861178,
2.70950503030707));
#46122=CARTESIAN_POINT('Ctrl Pts',(0.187312562459995,-1.06847604194512,
2.78141067466408));
#46123=CARTESIAN_POINT('Ctrl Pts',(0.161724215836607,-0.794772684000851,
2.91805939711538));
#46124=CARTESIAN_POINT('Ctrl Pts',(0.151708180499798,-0.636309800095197,
2.97106881806364));
#46125=CARTESIAN_POINT('Ctrl Pts',(0.130506918224618,-0.319434907277159,
3.04237334549099));
#46126=CARTESIAN_POINT('Ctrl Pts',(0.12267336889205,-0.158333333333332,
3.05879493020897));
#46127=CARTESIAN_POINT('Ctrl Pts',(0.102179986998412,0.158333333333334,
3.05825650250268));
#46128=CARTESIAN_POINT('Ctrl Pts',(0.0906597384266764,0.319434907277167,
3.04130452642146));
#46129=CARTESIAN_POINT('Ctrl Pts',(0.0677962068234777,0.636309800095206,
2.9688868910723));
#46130=CARTESIAN_POINT('Ctrl Pts',(0.0556862153948455,0.79477268400084,
2.91537714081636));
#46131=CARTESIAN_POINT('Ctrl Pts',(0.0347010954712026,1.06847604194511,
2.77756665167135));
#46132=CARTESIAN_POINT('Ctrl Pts',(0.0256069538907915,1.18514270861178,
2.70510942351996));
#46133=CARTESIAN_POINT('Ctrl Pts',(0.0165023515695843,1.3,2.61984802158616));
#46134=CARTESIAN_POINT('Ctrl Pts',(0.214250816488492,-1.30000000000266,
2.62484391020604));
#46135=CARTESIAN_POINT('Ctrl Pts',(0.199984062840105,-1.18514270861359,
2.70950503030596));
#46136=CARTESIAN_POINT('Ctrl Pts',(0.18731256246008,-1.06847604194603,2.78141067466363));
#46137=CARTESIAN_POINT('Ctrl Pts',(0.161724215836607,-0.794772684000851,
2.91805939711538));
#46138=CARTESIAN_POINT('Ctrl Pts',(0.151708180499798,-0.636309800095197,
2.97106881806364));
#46139=CARTESIAN_POINT('Ctrl Pts',(0.130506918224618,-0.319434907277159,
3.04237334549099));
#46140=CARTESIAN_POINT('Ctrl Pts',(0.12267336889205,-0.158333333333332,
3.05879493020897));
#46141=CARTESIAN_POINT('Ctrl Pts',(0.102179986998412,0.158333333333334,
3.05825650250268));
#46142=CARTESIAN_POINT('Ctrl Pts',(0.0906597384266765,0.319434907277167,
3.04130452642146));
#46143=CARTESIAN_POINT('Ctrl Pts',(0.0677962068234777,0.636309800095206,
2.9688868910723));
#46144=CARTESIAN_POINT('Ctrl Pts',(0.0556862153948455,0.79477268400084,
2.91537714081636));
#46145=CARTESIAN_POINT('Ctrl Pts',(0.0347010954711178,1.06847604194622,
2.7775666516708));
#46146=CARTESIAN_POINT('Ctrl Pts',(0.0256069538906217,1.18514270861395,
2.70510942351861));
#46147=CARTESIAN_POINT('Ctrl Pts',(0.0165023515693293,1.30000000000322,
2.61984802158377));
#46148=CARTESIAN_POINT('Ctrl Pts',(0.219717436762999,-1.30000000000266,
2.61800951425875));
#46149=CARTESIAN_POINT('Ctrl Pts',(0.204772182758639,-1.18514270861359,
2.70277064226634));
#46150=CARTESIAN_POINT('Ctrl Pts',(0.19201547765618,-1.06847604194603,2.7748686900201));
#46151=CARTESIAN_POINT('Ctrl Pts',(0.167600922680589,-0.794772684000851,
2.91217535486884));
#46152=CARTESIAN_POINT('Ctrl Pts',(0.1611038534861,-0.636309800095197,2.96615092375314));
#46153=CARTESIAN_POINT('Ctrl Pts',(0.141607349608946,-0.319434907277159,
3.0379582637104));
#46154=CARTESIAN_POINT('Ctrl Pts',(0.133278717909188,-0.158333333333332,
3.05415093481762));
#46155=CARTESIAN_POINT('Ctrl Pts',(0.112567852728384,0.158333333333334,
3.05351876207922));
#46156=CARTESIAN_POINT('Ctrl Pts',(0.10105798971678,0.319434907277167,3.03661809170896));
#46157=CARTESIAN_POINT('Ctrl Pts',(0.0765909966189229,0.636309800095206,
2.96367751457251));
#46158=CARTESIAN_POINT('Ctrl Pts',(0.0620129494727478,0.79477268400084,
2.90946650533395));
#46159=CARTESIAN_POINT('Ctrl Pts',(0.0397026858018158,1.06847604194622,
2.77097185416088));
#46160=CARTESIAN_POINT('Ctrl Pts',(0.0303808199744749,1.18514270861395,
2.69825565191217));
#46161=CARTESIAN_POINT('Ctrl Pts',(0.0213943747862455,1.30000000000322,
2.61277245017529));
#46162=CARTESIAN_POINT('Ctrl Pts',(0.224226242429926,-1.30000000000266,
2.60660085909856));
#46163=CARTESIAN_POINT('Ctrl Pts',(0.208257853828071,-1.18514270861359,
2.68864946051841));
#46164=CARTESIAN_POINT('Ctrl Pts',(0.195371213482085,-1.06847604194603,
2.7589356667499));
#46165=CARTESIAN_POINT('Ctrl Pts',(0.172719951292067,-0.794772684000849,
2.89413737790722));
#46166=CARTESIAN_POINT('Ctrl Pts',(0.171421999099358,-0.636309800095195,
2.94996853204855));
#46167=CARTESIAN_POINT('Ctrl Pts',(0.154677214871352,-0.319434907277157,
3.0225522636603));
#46168=CARTESIAN_POINT('Ctrl Pts',(0.145966428273531,-0.158333333333332,
3.03965369608755));
#46169=CARTESIAN_POINT('Ctrl Pts',(0.125103826804356,0.158333333333334,
3.03896798715647));
#46170=CARTESIAN_POINT('Ctrl Pts',(0.113974062136087,0.319434907277168,
3.02105717623826));
#46171=CARTESIAN_POINT('Ctrl Pts',(0.0861413866549122,0.636309800095206,
2.94732861089557));
#46172=CARTESIAN_POINT('Ctrl Pts',(0.0652329202269298,0.794772684000838,
2.89140877704261));
#46173=CARTESIAN_POINT('Ctrl Pts',(0.0412006114249792,1.06847604194621,
2.75501159968778));
#46174=CARTESIAN_POINT('Ctrl Pts',(0.0323159863042974,1.18514270861395,
2.68407500213889));
#46175=CARTESIAN_POINT('Ctrl Pts',(0.0249494320585472,1.30000000000321,
2.60124309110478));
#46176=CARTESIAN_POINT('Ctrl Pts',(0.230949458773703,-1.30000000000266,
2.58988253450759));
#46177=CARTESIAN_POINT('Ctrl Pts',(0.215310207632889,-1.18514270861359,
2.6682714894817));
#46178=CARTESIAN_POINT('Ctrl Pts',(0.202874571394742,-1.06847604194603,
2.73588386953428));
#46179=CARTESIAN_POINT('Ctrl Pts',(0.181546755250328,-0.79477268400085,
2.86718594935033));
#46180=CARTESIAN_POINT('Ctrl Pts',(0.181706589644006,-0.636309800095197,
2.92368822085034));
#46181=CARTESIAN_POINT('Ctrl Pts',(0.166279833913429,-0.319434907277159,
2.99623753732807));
#46182=CARTESIAN_POINT('Ctrl Pts',(0.158104188468809,-0.158333333333332,
3.01469934874809));
#46183=CARTESIAN_POINT('Ctrl Pts',(0.137147922657862,0.158333333333334,
3.0140255997615));
#46184=CARTESIAN_POINT('Ctrl Pts',(0.12572094355746,0.319434907277166,2.99481719140083));
#46185=CARTESIAN_POINT('Ctrl Pts',(0.0957040249390647,0.636309800095205,
2.92104388278613));
#46186=CARTESIAN_POINT('Ctrl Pts',(0.0714764819578855,0.79477268400084,
2.86424787169668));
#46187=CARTESIAN_POINT('Ctrl Pts',(0.0459616329290023,1.06847604194622,
2.73168073618549));
#46188=CARTESIAN_POINT('Ctrl Pts',(0.036969146524305,1.18514270861395,2.66342015805726));
#46189=CARTESIAN_POINT('Ctrl Pts',(0.0300286064412367,1.30000000000322,
2.5842824026674));
#46190=CARTESIAN_POINT('Ctrl Pts',(0.236845399224923,-1.30000000000266,
2.57610161912796));
#46191=CARTESIAN_POINT('Ctrl Pts',(0.221834012227604,-1.18514270861359,
2.65181796325388));
#46192=CARTESIAN_POINT('Ctrl Pts',(0.20970644697097,-1.06847604194603,2.71746793573469));
#46193=CARTESIAN_POINT('Ctrl Pts',(0.188351550244662,-0.794772684000849,
2.84587717312589));
#46194=CARTESIAN_POINT('Ctrl Pts',(0.186768855990391,-0.636309800095196,
2.90275724229796));
#46195=CARTESIAN_POINT('Ctrl Pts',(0.171469624012701,-0.319434907277159,
2.97530338117715));
#46196=CARTESIAN_POINT('Ctrl Pts',(0.164888391661675,-0.158333333333332,
2.99489344943572));
#46197=CARTESIAN_POINT('Ctrl Pts',(0.144505048078426,0.158333333333334,
2.99429991964275));
#46198=CARTESIAN_POINT('Ctrl Pts',(0.132951781539408,0.319434907277167,
2.97414934804337));
#46199=CARTESIAN_POINT('Ctrl Pts',(0.102150875569596,0.636309800095206,
2.90032695920638));
#46200=CARTESIAN_POINT('Ctrl Pts',(0.0764112209685388,0.79477268400084,
2.84281492452855));
#46201=CARTESIAN_POINT('Ctrl Pts',(0.0503921073465047,1.06847604194621,
2.71304101877748));
#46202=CARTESIAN_POINT('Ctrl Pts',(0.0414413960540642,1.18514270861395,
2.64674863185993));
#46203=CARTESIAN_POINT('Ctrl Pts',(0.0348026836530411,1.30000000000322,
2.57033817322763));
#46204=CARTESIAN_POINT('Ctrl Pts',(0.242960861231862,-1.30000000000267,
2.56222898063554));
#46205=CARTESIAN_POINT('Ctrl Pts',(0.2286894017545,-1.18514270861359,2.63502014154845));
#46206=CARTESIAN_POINT('Ctrl Pts',(0.216927525128715,-1.06847604194603,
2.6985053181899));
#46207=CARTESIAN_POINT('Ctrl Pts',(0.195552875595353,-0.79477268400085,
2.82367009107433));
#46208=CARTESIAN_POINT('Ctrl Pts',(0.192243349954664,-0.636309800095197,
2.88086591715262));
#46209=CARTESIAN_POINT('Ctrl Pts',(0.17650634197705,-0.31943490727716,2.95325496211296));
#46210=CARTESIAN_POINT('Ctrl Pts',(0.17113522051647,-0.158333333333332,
2.9739908358149));
#46211=CARTESIAN_POINT('Ctrl Pts',(0.149875803896344,0.158333333333334,
2.97333502370939));
#46212=CARTESIAN_POINT('Ctrl Pts',(0.135702605371645,0.319434907277167,
2.95194658007296));
#46213=CARTESIAN_POINT('Ctrl Pts',(0.104642184068728,0.636309800095206,
2.87821508900477));
#46214=CARTESIAN_POINT('Ctrl Pts',(0.0813510654142378,0.794772684000842,
2.82041706127865));
#46215=CARTESIAN_POINT('Ctrl Pts',(0.0558631364763465,1.06847604194622,
2.69388570487083));
#46216=CARTESIAN_POINT('Ctrl Pts',(0.0468095477267672,1.18514270861395,
2.62975762692213));
#46217=CARTESIAN_POINT('Ctrl Pts',(0.0397351502440323,1.30000000000322,
2.55627220676513));
#46218=CARTESIAN_POINT('Ctrl Pts',(0.250471543072162,-1.30000000000267,
2.54870591804654));
#46219=CARTESIAN_POINT('Ctrl Pts',(0.236868078466005,-1.18514270861359,
2.61871399047799));
#46220=CARTESIAN_POINT('Ctrl Pts',(0.225336052648485,-1.06847604194603,
2.68012857764004));
#46221=CARTESIAN_POINT('Ctrl Pts',(0.203480204027908,-0.79477268400085,
2.80215588983677));
#46222=CARTESIAN_POINT('Ctrl Pts',(0.1982073532554,-0.636309800095196,2.85960963436872));
#46223=CARTESIAN_POINT('Ctrl Pts',(0.180822474756462,-0.319434907277159,
2.93170916824689));
#46224=CARTESIAN_POINT('Ctrl Pts',(0.174664464262972,-0.158333333333332,
2.95331583529123));
#46225=CARTESIAN_POINT('Ctrl Pts',(0.152781665023936,0.158333333333334,
2.95263166308528));
#46226=CARTESIAN_POINT('Ctrl Pts',(0.138586582843348,0.319434907277166,
2.93036861580522));
#46227=CARTESIAN_POINT('Ctrl Pts',(0.108281872775913,0.636309800095205,
2.85681886216328));
#46228=CARTESIAN_POINT('Ctrl Pts',(0.0868071607438343,0.79477268400084,
2.79864821362611));
#46229=CARTESIAN_POINT('Ctrl Pts',(0.0615122998097732,1.06847604194621,
2.67512345987812));
#46230=CARTESIAN_POINT('Ctrl Pts',(0.0521573957606204,1.18514270861395,
2.61301343223756));
#46231=CARTESIAN_POINT('Ctrl Pts',(0.0443967956937546,1.30000000000321,
2.542262665811));
#46232=CARTESIAN_POINT('Ctrl Pts',(0.260324786692414,-1.30000000000267,
2.52661415542551));
#46233=CARTESIAN_POINT('Ctrl Pts',(0.247738100352481,-1.18514270861359,
2.59205864113441));
#46234=CARTESIAN_POINT('Ctrl Pts',(0.236730363824326,-1.06847604194603,
2.65010915080776));
#46235=CARTESIAN_POINT('Ctrl Pts',(0.214947980287267,-0.794772684000848,
2.76713587731543));
#46236=CARTESIAN_POINT('Ctrl Pts',(0.208042015085297,-0.636309800095196,
2.82525416350595));
#46237=CARTESIAN_POINT('Ctrl Pts',(0.189046709496585,-0.319434907277159,
2.89704085517984));
#46238=CARTESIAN_POINT('Ctrl Pts',(0.181568024952914,-0.158333333333332,
2.9200833086852));
#46239=CARTESIAN_POINT('Ctrl Pts',(0.159074504936224,0.158333333333334,
2.91935988914436));
#46240=CARTESIAN_POINT('Ctrl Pts',(0.145313591975273,0.319434907277168,
2.89560943657395));
#46241=CARTESIAN_POINT('Ctrl Pts',(0.115937067005509,0.636309800095207,
2.82231778098446));
#46242=CARTESIAN_POINT('Ctrl Pts',(0.0960962109841885,0.79477268400084,
2.76348818055815));
#46243=CARTESIAN_POINT('Ctrl Pts',(0.0710703651477984,1.06847604194621,
2.6449262435517));
#46244=CARTESIAN_POINT('Ctrl Pts',(0.0614821466118171,1.18514270861395,
2.5861599519411));
#46245=CARTESIAN_POINT('Ctrl Pts',(0.0531384709035037,1.30000000000322,
2.51994843809752));
#46246=CARTESIAN_POINT('Ctrl Pts',(0.276326377533243,-1.30000000000266,
2.49679480815817));
#46247=CARTESIAN_POINT('Ctrl Pts',(0.266773624550892,-1.18514270861358,
2.55639301755284));
#46248=CARTESIAN_POINT('Ctrl Pts',(0.257408085958808,-1.06847604194603,
2.61006830635916));
#46249=CARTESIAN_POINT('Ctrl Pts',(0.236204320935233,-0.79477268400085,
2.72038582977072));
#46250=CARTESIAN_POINT('Ctrl Pts',(0.224618722165695,-0.636309800095196,
2.77885015273103));
#46251=CARTESIAN_POINT('Ctrl Pts',(0.202026006127601,-0.319434907277159,
2.84988966203324));
#46252=CARTESIAN_POINT('Ctrl Pts',(0.192312128337127,-0.158333333333332,
2.87476074147654));
#46253=CARTESIAN_POINT('Ctrl Pts',(0.168505927894078,0.158333333333334,
2.87393181360536));
#46254=CARTESIAN_POINT('Ctrl Pts',(0.155246296971355,0.319434907277164,
2.84828171591575));
#46255=CARTESIAN_POINT('Ctrl Pts',(0.12765136371236,0.636309800095203,2.77545207791248));
#46256=CARTESIAN_POINT('Ctrl Pts',(0.111705856094525,0.79477268400084,2.715907240678));
#46257=CARTESIAN_POINT('Ctrl Pts',(0.0866203030801193,1.06847604194621,
2.60399740450606));
#46258=CARTESIAN_POINT('Ctrl Pts',(0.0760605815387644,1.18514270861395,
2.54966891900018));
#46259=CARTESIAN_POINT('Ctrl Pts',(0.0657997448446978,1.30000000000321,
2.48945356939939));
#46260=CARTESIAN_POINT('Ctrl Pts',(0.292202396494802,-1.30000000000266,
2.46694851625233));
#46261=CARTESIAN_POINT('Ctrl Pts',(0.283999061631066,-1.18514270861358,
2.52029688424042));
#46262=CARTESIAN_POINT('Ctrl Pts',(0.275487483908816,-1.06847604194603,
2.56938158427808));
#46263=CARTESIAN_POINT('Ctrl Pts',(0.255111933968273,-0.79477268400085,
2.6729271348159));
#46264=CARTESIAN_POINT('Ctrl Pts',(0.242813019657568,-0.636309800095196,
2.73248470123121));
#46265=CARTESIAN_POINT('Ctrl Pts',(0.218454706196389,-0.319434907277158,
2.8030732316513));
#46266=CARTESIAN_POINT('Ctrl Pts',(0.206026250815626,-0.158333333333332,
2.82968936167192));
#46267=CARTESIAN_POINT('Ctrl Pts',(0.181291452230541,0.158333333333334,
2.82874104483902));
#46268=CARTESIAN_POINT('Ctrl Pts',(0.169446802573742,0.319434907277166,
2.80118316000646));
#46269=CARTESIAN_POINT('Ctrl Pts',(0.142481675768436,0.636309800095204,
2.72864961011461));
#46270=CARTESIAN_POINT('Ctrl Pts',(0.127566010709557,0.794772684000839,
2.66809682197219));
#46271=CARTESIAN_POINT('Ctrl Pts',(0.101165243211556,1.06847604194621,2.56277705064535));
#46272=CARTESIAN_POINT('Ctrl Pts',(0.0894843035980192,1.18514270861395,
2.5129190957758));
#46273=CARTESIAN_POINT('Ctrl Pts',(0.07755033837604,1.30000000000322,2.45879221256219));
#46274=CARTESIAN_POINT('Ctrl Pts',(0.304272576971275,-1.30000000000266,
2.44537989334799));
#46275=CARTESIAN_POINT('Ctrl Pts',(0.298784633296944,-1.18514270861358,
2.49456792282061));
#46276=CARTESIAN_POINT('Ctrl Pts',(0.291942104826949,-1.06847604194603,
2.54054519967646));
#46277=CARTESIAN_POINT('Ctrl Pts',(0.273005133356464,-0.794772684000849,
2.63934442608221));
#46278=CARTESIAN_POINT('Ctrl Pts',(0.257978411602134,-0.636309800095195,
2.69920763652856));
#46279=CARTESIAN_POINT('Ctrl Pts',(0.231598787365596,-0.319434907277158,
2.76927187817773));
#46280=CARTESIAN_POINT('Ctrl Pts',(0.217472370399731,-0.158333333333332,
2.79715497595911));
#46281=CARTESIAN_POINT('Ctrl Pts',(0.191892554756733,0.158333333333334,
2.79608873751453));
#46282=CARTESIAN_POINT('Ctrl Pts',(0.180681897540819,0.319434907277165,
2.76714927918927));
#46283=CARTESIAN_POINT('Ctrl Pts',(0.154462832241876,0.636309800095203,
2.69489306602771));
#46284=CARTESIAN_POINT('Ctrl Pts',(0.141318825871087,0.794772684000838,
2.63374630787981));
#46285=CARTESIAN_POINT('Ctrl Pts',(0.114121379298996,1.06847604194621,2.53321905935691));
#46286=CARTESIAN_POINT('Ctrl Pts',(0.101502347942526,1.18514270861395,2.48657909896014));
#46287=CARTESIAN_POINT('Ctrl Pts',(0.0880370520859876,1.30000000000321,
2.43681369915072));
#46288=CARTESIAN_POINT('Ctrl Pts',(0.31391933706681,-1.30000000000266,2.4293389678366));
#46289=CARTESIAN_POINT('Ctrl Pts',(0.309400934569747,-1.18514270861358,
2.4751753199178));
#46290=CARTESIAN_POINT('Ctrl Pts',(0.303131998752341,-1.06847604194602,
2.5186753955374));
#46291=CARTESIAN_POINT('Ctrl Pts',(0.28460542075491,-0.794772684000844,
2.61377200638179));
#46292=CARTESIAN_POINT('Ctrl Pts',(0.268426823455187,-0.636309800095196,
2.67406955453933));
#46293=CARTESIAN_POINT('Ctrl Pts',(0.241218797163057,-0.31943490727716,
2.74387709408424));
#46294=CARTESIAN_POINT('Ctrl Pts',(0.226503729694203,-0.158333333333332,
2.77283473837323));
#46295=CARTESIAN_POINT('Ctrl Pts',(0.200615266855469,0.158333333333334,
2.77172723585368));
#46296=CARTESIAN_POINT('Ctrl Pts',(0.189810095540242,0.319434907277164,
2.74170569891167));
#46297=CARTESIAN_POINT('Ctrl Pts',(0.163535141174737,0.636309800095204,
2.66955342631916));
#46298=CARTESIAN_POINT('Ctrl Pts',(0.15047246735778,0.79477268400084,2.60778317810354));
#46299=CARTESIAN_POINT('Ctrl Pts',(0.122451069898524,1.06847604194622,2.51082597321505));
#46300=CARTESIAN_POINT('Ctrl Pts',(0.109283634712029,1.18514270861396,2.46662845922663));
#46301=CARTESIAN_POINT('Ctrl Pts',(0.0950781890041065,1.30000000000322,
2.42020261262772));
#46302=CARTESIAN_POINT('Ctrl Pts',(0.329357357760276,-1.30000000000267,
2.40248830162943));
#46303=CARTESIAN_POINT('Ctrl Pts',(0.327729674566757,-1.18514270861359,
2.4430275075526));
#46304=CARTESIAN_POINT('Ctrl Pts',(0.323315370461579,-1.06847604194603,
2.48259745426958));
#46305=CARTESIAN_POINT('Ctrl Pts',(0.306679793132641,-0.794772684000852,
2.57177276446023));
#46306=CARTESIAN_POINT('Ctrl Pts',(0.28829840342903,-0.636309800095199,
2.63268060877138));
#46307=CARTESIAN_POINT('Ctrl Pts',(0.259149536142379,-0.319434907277161,
2.70192493970066));
#46308=CARTESIAN_POINT('Ctrl Pts',(0.242095782310558,-0.158333333333333,
2.7324073631622));
#46309=CARTESIAN_POINT('Ctrl Pts',(0.215500324796916,0.158333333333335,
2.73118901208806));
#46310=CARTESIAN_POINT('Ctrl Pts',(0.206124614958519,0.319434907277165,
2.69952637433431));
#46311=CARTESIAN_POINT('Ctrl Pts',(0.180762332719264,0.636309800095206,
2.62772266811228));
#46312=CARTESIAN_POINT('Ctrl Pts',(0.169392553392926,0.794772684000845,
2.56516167402763));
#46313=CARTESIAN_POINT('Ctrl Pts',(0.139683659528629,1.06847604194622,2.47408974758264));
#46314=CARTESIAN_POINT('Ctrl Pts',(0.124995150673325,1.18514270861396,2.43385509284417));
#46315=CARTESIAN_POINT('Ctrl Pts',(0.108478012293625,1.30000000000322,2.39280744577801));
#46316=CARTESIAN_POINT('Ctrl Pts',(0.349313927641765,-1.30000000000266,
2.37063062041402));
#46317=CARTESIAN_POINT('Ctrl Pts',(0.350990972581243,-1.18514270861358,
2.40479535651899));
#46318=CARTESIAN_POINT('Ctrl Pts',(0.348696152747529,-1.06847604194603,
2.43963560104537));
#46319=CARTESIAN_POINT('Ctrl Pts',(0.334218857659674,-0.794772684000849,
2.52168409525648));
#46320=CARTESIAN_POINT('Ctrl Pts',(0.313241814432491,-0.636309800095198,
2.58331600960798));
#46321=CARTESIAN_POINT('Ctrl Pts',(0.28201046580892,-0.319434907277161,
2.65189738093111));
#46322=CARTESIAN_POINT('Ctrl Pts',(0.26266427967697,-0.158333333333332,
2.68426798688803));
#46323=CARTESIAN_POINT('Ctrl Pts',(0.235171728445277,0.158333333333334,
2.68288728323856));
#46324=CARTESIAN_POINT('Ctrl Pts',(0.227136327014149,0.319434907277165,
2.64919350404502));
#46325=CARTESIAN_POINT('Ctrl Pts',(0.20214130330482,0.636309800095205,2.57768255349322));
#46326=CARTESIAN_POINT('Ctrl Pts',(0.192061826528855,0.794772684000843,
2.5140529536976));
#46327=CARTESIAN_POINT('Ctrl Pts',(0.159730108434817,1.06847604194622,2.42994044625363));
#46328=CARTESIAN_POINT('Ctrl Pts',(0.143041737765,1.18514270861396,2.39442966052077));
#46329=CARTESIAN_POINT('Ctrl Pts',(0.123660199180121,1.30000000000322,2.35981727685218));
#46330=CARTESIAN_POINT('Ctrl Pts',(0.372656470855065,-1.30000000000266,
2.33357102415659));
#46331=CARTESIAN_POINT('Ctrl Pts',(0.378860083512457,-1.18514270861359,
2.36049270100928));
#46332=CARTESIAN_POINT('Ctrl Pts',(0.379623704547688,-1.06847604194603,
2.38996946461138));
#46333=CARTESIAN_POINT('Ctrl Pts',(0.368820352987192,-0.794772684000852,
2.46396944687276));
#46334=CARTESIAN_POINT('Ctrl Pts',(0.345641686475895,-0.636309800095197,
2.52656684485733));
#46335=CARTESIAN_POINT('Ctrl Pts',(0.312069213115202,-0.319434907277159,
2.59433277240725));
#46336=CARTESIAN_POINT('Ctrl Pts',(0.289014967455505,-0.158333333333332,
2.62862603375246));
#46337=CARTESIAN_POINT('Ctrl Pts',(0.260127011611611,0.158333333333334,
2.6269490852742));
#46338=CARTESIAN_POINT('Ctrl Pts',(0.25389123708121,0.319434907277168,2.59095897495413));
#46339=CARTESIAN_POINT('Ctrl Pts',(0.229440000513363,0.636309800095207,
2.51981775997691));
#46340=CARTESIAN_POINT('Ctrl Pts',(0.221050650127639,0.794772684000841,
2.45499750537546));
#46341=CARTESIAN_POINT('Ctrl Pts',(0.185638193159351,1.06847604194621,2.37897079950157));
#46342=CARTESIAN_POINT('Ctrl Pts',(0.166555801923257,1.18514270861395,2.3489356310057));
#46343=CARTESIAN_POINT('Ctrl Pts',(0.143719759911867,1.30000000000321,2.32177443791985));
#46344=CARTESIAN_POINT('Ctrl Pts',(0.39394052481098,-1.30000000000266,2.30216095517147));
#46345=CARTESIAN_POINT('Ctrl Pts',(0.404452058674696,-1.18514270861358,
2.3230082546088));
#46346=CARTESIAN_POINT('Ctrl Pts',(0.408035072497374,-1.06847604194603,
2.3479548710559));
#46347=CARTESIAN_POINT('Ctrl Pts',(0.400306283866768,-0.79477268400085,
2.41505678796012));
#46348=CARTESIAN_POINT('Ctrl Pts',(0.373759972065985,-0.636309800095195,
2.47811072112627));
#46349=CARTESIAN_POINT('Ctrl Pts',(0.338594991347445,-0.319434907277158,
2.54523185207478));
#46350=CARTESIAN_POINT('Ctrl Pts',(0.314328019102381,-0.158333333333332,
2.58157499811901));
#46351=CARTESIAN_POINT('Ctrl Pts',(0.284743021097901,0.158333333333334,
2.57973868058722));
#46352=CARTESIAN_POINT('Ctrl Pts',(0.279090057296803,0.319434907277166,
2.54158652617387));
#46353=CARTESIAN_POINT('Ctrl Pts',(0.254674771945333,0.636309800095204,
2.47066932183429));
#46354=CARTESIAN_POINT('Ctrl Pts',(0.247976474935861,0.794772684000839,
2.4048763179591));
#46355=CARTESIAN_POINT('Ctrl Pts',(0.209269561084131,1.06847604194621,2.33563397887084));
#46356=CARTESIAN_POINT('Ctrl Pts',(0.187703586226661,1.18514270861395,2.31019653209487));
#46357=CARTESIAN_POINT('Ctrl Pts',(0.161326425285709,1.30000000000321,2.28929408145285));
#46358=CARTESIAN_POINT('Ctrl Pts',(0.40889487947129,-1.30000000000266,2.27992493321004));
#46359=CARTESIAN_POINT('Ctrl Pts',(0.422184967800618,-1.18514270861358,
2.29642013808564));
#46360=CARTESIAN_POINT('Ctrl Pts',(0.427747944200723,-1.06847604194603,
2.31816505247727));
#46361=CARTESIAN_POINT('Ctrl Pts',(0.422748358194651,-0.79477268400085,
2.38052803395972));
#46362=CARTESIAN_POINT('Ctrl Pts',(0.395708521594285,-0.636309800095194,
2.44435535746079));
#46363=CARTESIAN_POINT('Ctrl Pts',(0.359515267236892,-0.319434907277157,
2.5110359405381));
#46364=CARTESIAN_POINT('Ctrl Pts',(0.332737872407183,-0.158333333333332,
2.54842435869403));
#46365=CARTESIAN_POINT('Ctrl Pts',(0.302246003276087,0.158333333333334,
2.54635870301532));
#46366=CARTESIAN_POINT('Ctrl Pts',(0.297763549222328,0.319434907277168,
2.50683793103993));
#46367=CARTESIAN_POINT('Ctrl Pts',(0.273411381106316,0.636309800095205,
2.43608561538753));
#46368=CARTESIAN_POINT('Ctrl Pts',(0.267494466492831,0.794772684000836,
2.36953155090904));
#46369=CARTESIAN_POINT('Ctrl Pts',(0.226281106273681,1.06847604194621,2.30504621887655));
#46370=CARTESIAN_POINT('Ctrl Pts',(0.202920164067203,1.18514270861395,2.28284713173985));
#46371=CARTESIAN_POINT('Ctrl Pts',(0.174038016187705,1.30000000000321,2.2663622682864));
#46372=CARTESIAN_POINT('Ctrl Pts',(0.418074677884182,-1.30000000000266,
2.26695241764461));
#46373=CARTESIAN_POINT('Ctrl Pts',(0.433173626250395,-1.18514270861358,
2.28093773627827));
#46374=CARTESIAN_POINT('Ctrl Pts',(0.439971210966554,-1.06847604194603,
2.30082141255031));
#46375=CARTESIAN_POINT('Ctrl Pts',(0.436497180799323,-0.79477268400085,
2.36038306856137));
#46376=CARTESIAN_POINT('Ctrl Pts',(0.40865778436878,-0.636309800095193,
2.42453753966287));
#46377=CARTESIAN_POINT('Ctrl Pts',(0.371625020041766,-0.319434907277156,
2.49089564224033));
#46378=CARTESIAN_POINT('Ctrl Pts',(0.343321720849447,-0.158333333333332,
2.52887802547803));
#46379=CARTESIAN_POINT('Ctrl Pts',(0.312521115164033,0.158333333333334,
2.52672711617914));
#46380=CARTESIAN_POINT('Ctrl Pts',(0.30912604342682,0.319434907277167,2.48650290222469));
#46381=CARTESIAN_POINT('Ctrl Pts',(0.285248874850876,0.636309800095204,
2.41594875265761));
#46382=CARTESIAN_POINT('Ctrl Pts',(0.280261066055348,0.794772684000835,
2.3490480138972));
#46383=CARTESIAN_POINT('Ctrl Pts',(0.23737752714204,1.06847604194621,2.28731304006279));
#46384=CARTESIAN_POINT('Ctrl Pts',(0.212698397801464,1.18514270861395,2.26695798367019));
#46385=CARTESIAN_POINT('Ctrl Pts',(0.181902834124258,1.30000000000321,2.25297065355183));
#46386=CARTESIAN_POINT('Ctrl Pts',(0.421712459977973,-1.30000000000266,
2.26175696623065));
#46387=CARTESIAN_POINT('Ctrl Pts',(0.43750869095182,-1.18514270861358,2.27473287610592));
#46388=CARTESIAN_POINT('Ctrl Pts',(0.444789040576102,-1.06847604194603,
2.29386986012942));
#46389=CARTESIAN_POINT('Ctrl Pts',(0.441934715123433,-0.79477268400085,
2.35231343536506));
#46390=CARTESIAN_POINT('Ctrl Pts',(0.413838630891733,-0.636309800095194,
2.41661236431494));
#46391=CARTESIAN_POINT('Ctrl Pts',(0.376520763295964,-0.319434907277157,
2.4828531706063));
#46392=CARTESIAN_POINT('Ctrl Pts',(0.347670115184739,-0.158333333333332,
2.52108833834578));
#46393=CARTESIAN_POINT('Ctrl Pts',(0.31668812795415,0.158333333333334,2.51889016933317));
#46394=CARTESIAN_POINT('Ctrl Pts',(0.313584493009362,0.319434907277167,
2.47835102502749));
#46395=CARTESIAN_POINT('Ctrl Pts',(0.289774779982301,0.636309800095205,
2.4078482290991));
#46396=CARTESIAN_POINT('Ctrl Pts',(0.285062270626377,0.794772684000836,
2.34078811305393));
#46397=CARTESIAN_POINT('Ctrl Pts',(0.241559388623895,1.06847604194621,2.2801638124301));
#46398=CARTESIAN_POINT('Ctrl Pts',(0.216415631024418,1.18514270861395,2.26056002576535));
#46399=CARTESIAN_POINT('Ctrl Pts',(0.184958901503789,1.30000000000321,2.24759446582433));
#46400=CARTESIAN_POINT('Ctrl Pts',(0.426467295636889,-1.30000000000266,
2.25532274225131));
#46401=CARTESIAN_POINT('Ctrl Pts',(0.443311053594282,-1.18514270861358,
2.26708819267389));
#46402=CARTESIAN_POINT('Ctrl Pts',(0.451276277723858,-1.06847604194603,
2.2853159470878));
#46403=CARTESIAN_POINT('Ctrl Pts',(0.449166349613946,-0.794772684000851,
2.3423549212329));
#46404=CARTESIAN_POINT('Ctrl Pts',(0.420250688541158,-0.636309800095194,
2.40669534522819));
#46405=CARTESIAN_POINT('Ctrl Pts',(0.38253270170118,-0.319434907277156,
2.47277231690775));
#46406=CARTESIAN_POINT('Ctrl Pts',(0.353379877388863,-0.158333333333332,
2.51141997753213));
#46407=CARTESIAN_POINT('Ctrl Pts',(0.322197963808489,0.158333333333334,
2.5091693846688));
#46408=CARTESIAN_POINT('Ctrl Pts',(0.31925281525967,0.319434907277167,2.46818579243708));
#46409=CARTESIAN_POINT('Ctrl Pts',(0.295321436105165,0.636309800095204,
2.39769835401992));
#46410=CARTESIAN_POINT('Ctrl Pts',(0.290720125827061,0.794772684000836,
2.33038642787854));
#46411=CARTESIAN_POINT('Ctrl Pts',(0.246465322535933,1.06847604194621,2.27115459859657));
#46412=CARTESIAN_POINT('Ctrl Pts',(0.22082090736561,1.18514270861395,2.25250763524956));
#46413=CARTESIAN_POINT('Ctrl Pts',(0.188688341567717,1.30000000000321,2.24085297269625));
#46414=CARTESIAN_POINT('Ctrl Pts',(0.431244061790658,-1.30000000000266,
2.24889883901266));
#46415=CARTESIAN_POINT('Ctrl Pts',(0.44918891043392,-1.18514270861358,2.25946966602348));
#46416=CARTESIAN_POINT('Ctrl Pts',(0.457874292427998,-1.06847604194603,
2.27679853992569));
#46417=CARTESIAN_POINT('Ctrl Pts',(0.456548042029465,-0.79477268400085,
2.33244414553066));
#46418=CARTESIAN_POINT('Ctrl Pts',(0.42675065332855,-0.636309800095194,
2.39680886442213));
#46419=CARTESIAN_POINT('Ctrl Pts',(0.388657227913405,-0.319434907277157,
2.46272530928844));
#46420=CARTESIAN_POINT('Ctrl Pts',(0.359280563081143,-0.158333333333332,
2.5018011697518));
#46421=CARTESIAN_POINT('Ctrl Pts',(0.327911426643574,0.158333333333334,
2.49949964338542));
#46422=CARTESIAN_POINT('Ctrl Pts',(0.325087837645621,0.319434907277167,
2.45806354810334));
#46423=CARTESIAN_POINT('Ctrl Pts',(0.300977517076595,0.636309800095205,
2.38757864463434));
#46424=CARTESIAN_POINT('Ctrl Pts',(0.29642792391652,0.794772684000837,2.32000272570592));
#46425=CARTESIAN_POINT('Ctrl Pts',(0.251374607794543,1.06847604194621,2.2621518191359));
#46426=CARTESIAN_POINT('Ctrl Pts',(0.225216317221286,1.18514270861395,2.24445776965328));
#46427=CARTESIAN_POINT('Ctrl Pts',(0.192401647234186,1.30000000000321,2.23411118455496));
#46428=CARTESIAN_POINT('Ctrl Pts',(0.434968111342912,-1.30000000000266,
2.24373301200879));
#46429=CARTESIAN_POINT('Ctrl Pts',(0.45367912391193,-1.18514270861358,2.25331589338534));
#46430=CARTESIAN_POINT('Ctrl Pts',(0.462894100371637,-1.06847604194603,
2.26991264920826));
#46431=CARTESIAN_POINT('Ctrl Pts',(0.462244796355266,-0.79477268400085,
2.3244579284205));
#46432=CARTESIAN_POINT('Ctrl Pts',(0.432134940692004,-0.636309800095194,
2.3889523875418));
#46433=CARTESIAN_POINT('Ctrl Pts',(0.393770443913773,-0.319434907277157,
2.45475031567949));
#46434=CARTESIAN_POINT('Ctrl Pts',(0.363881237815788,-0.158333333333332,
2.49407930368688));
#46435=CARTESIAN_POINT('Ctrl Pts',(0.332358601705216,0.158333333333334,
2.4917337701187));
#46436=CARTESIAN_POINT('Ctrl Pts',(0.32985431461743,0.319434907277167,2.44999237980584));
#46437=CARTESIAN_POINT('Ctrl Pts',(0.305783344501939,0.636309800095205,
2.37955297547693));
#46438=CARTESIAN_POINT('Ctrl Pts',(0.301461610194176,0.794772684000836,
2.31180726361137));
#46439=CARTESIAN_POINT('Ctrl Pts',(0.255690569076344,1.06847604194621,2.25504263684815));
#46440=CARTESIAN_POINT('Ctrl Pts',(0.229015385646448,1.18514270861395,2.23808652659971));
#46441=CARTESIAN_POINT('Ctrl Pts',(0.195477606502444,1.30000000000321,2.22874560969204));
#46442=CARTESIAN_POINT('Ctrl Pts',(0.444046225881081,-1.30000000000266,
2.23075538235043));
#46443=CARTESIAN_POINT('Ctrl Pts',(0.464468729347459,-1.18514270861358,
2.23781146152863));
#46444=CARTESIAN_POINT('Ctrl Pts',(0.474925864707435,-1.06847604194603,
2.25255510224292));
#46445=CARTESIAN_POINT('Ctrl Pts',(0.476061945440884,-0.79477268400085,
2.30437566678773));
#46446=CARTESIAN_POINT('Ctrl Pts',(0.4458294729986,-0.636309800095193,2.36937781124614));
#46447=CARTESIAN_POINT('Ctrl Pts',(0.40693603065916,-0.319434907277156,
2.43492261629408));
#46448=CARTESIAN_POINT('Ctrl Pts',(0.375388524791862,-0.158333333333332,
2.47478419915548));
#46449=CARTESIAN_POINT('Ctrl Pts',(0.343486689041014,0.158333333333334,
2.47232706794512));
#46450=CARTESIAN_POINT('Ctrl Pts',(0.34194369713619,0.319434907277167,2.42986309442985));
#46451=CARTESIAN_POINT('Ctrl Pts',(0.318276616010384,0.636309800095204,
2.35960917305316));
#46452=CARTESIAN_POINT('Ctrl Pts',(0.315058623268968,0.794772684000835,
2.29156351277918));
#46453=CARTESIAN_POINT('Ctrl Pts',(0.267355287317446,1.06847604194621,2.23748173841521));
#46454=CARTESIAN_POINT('Ctrl Pts',(0.23916384314239,1.18514270861395,2.22231775032448));
#46455=CARTESIAN_POINT('Ctrl Pts',(0.203429961342996,1.30000000000321,2.21539977033806));
#46456=CARTESIAN_POINT('Ctrl Pts',(0.456822167741165,-1.30000000000266,
2.21417858708722));
#46457=CARTESIAN_POINT('Ctrl Pts',(0.48001599689858,-1.18514270861358,2.21812257914067));
#46458=CARTESIAN_POINT('Ctrl Pts',(0.492364054998585,-1.06847604194603,
2.23054701527269));
#46459=CARTESIAN_POINT('Ctrl Pts',(0.495834638598456,-0.794772684000848,
2.2788414705659));
#46460=CARTESIAN_POINT('Ctrl Pts',(0.464178241790207,-0.636309800095195,
2.3441367559944));
#46461=CARTESIAN_POINT('Ctrl Pts',(0.424377110318727,-0.319434907277159,
2.40927007814988));
#46462=CARTESIAN_POINT('Ctrl Pts',(0.391483932513137,-0.158333333333332,
2.45001856419996));
#46463=CARTESIAN_POINT('Ctrl Pts',(0.358957885118911,0.158333333333334,
2.44737481851414));
#46464=CARTESIAN_POINT('Ctrl Pts',(0.358295891275019,0.319434907277166,
2.40388130228096));
#46465=CARTESIAN_POINT('Ctrl Pts',(0.333940058166144,0.636309800095204,
2.3335691697477));
#46466=CARTESIAN_POINT('Ctrl Pts',(0.329719331263256,0.794772684000838,
2.26456161591243));
#46467=CARTESIAN_POINT('Ctrl Pts',(0.280186944664852,1.06847604194621,2.21409181215293));
#46468=CARTESIAN_POINT('Ctrl Pts',(0.251063712196728,1.18514270861395,2.2014793933697));
#46469=CARTESIAN_POINT('Ctrl Pts',(0.214257982063227,1.30000000000322,2.19810106376029));
#46470=CARTESIAN_POINT('Ctrl Pts',(0.471738537321603,-1.30000000000266,
2.19359139467269));
#46471=CARTESIAN_POINT('Ctrl Pts',(0.498459191387175,-1.18514270861358,
2.1937443110641));
#46472=CARTESIAN_POINT('Ctrl Pts',(0.513214193008901,-1.06847604194603,
2.20334023080082));
#46473=CARTESIAN_POINT('Ctrl Pts',(0.519658147617168,-0.794772684000851,
2.24732395184364));
#46474=CARTESIAN_POINT('Ctrl Pts',(0.486124807402051,-0.636309800095196,
2.31292961454153));
#46475=CARTESIAN_POINT('Ctrl Pts',(0.445306741773112,-0.319434907277158,
2.3775858381244));
#46476=CARTESIAN_POINT('Ctrl Pts',(0.410835379031462,-0.158333333333332,
2.41946437558252));
#46477=CARTESIAN_POINT('Ctrl Pts',(0.377897425156198,0.158333333333334,
2.41669026139795));
#46478=CARTESIAN_POINT('Ctrl Pts',(0.378244631154653,0.319434907277167,
2.3719123868402));
#46479=CARTESIAN_POINT('Ctrl Pts',(0.354386666183597,0.636309800095206,
2.30186056246783));
#46480=CARTESIAN_POINT('Ctrl Pts',(0.352291225354584,0.794772684000839,
2.23246446357083));
#46481=CARTESIAN_POINT('Ctrl Pts',(0.29930915091305,1.06847604194621,2.18619019140374));
#46482=CARTESIAN_POINT('Ctrl Pts',(0.26747097145162,1.18514270861395,2.17636765664866));
#46483=CARTESIAN_POINT('Ctrl Pts',(0.226728589375274,1.30000000000321,2.17675300492898));
#46484=CARTESIAN_POINT('Ctrl Pts',(0.479899051869771,-1.30000000000266,
2.18349369390981));
#46485=CARTESIAN_POINT('Ctrl Pts',(0.508096939819008,-1.18514270861359,
2.18168193670886));
#46486=CARTESIAN_POINT('Ctrl Pts',(0.523912487535125,-1.06847604194603,
2.18983223891249));
#46487=CARTESIAN_POINT('Ctrl Pts',(0.531843883631617,-0.794772684000851,
2.23167541759282));
#46488=CARTESIAN_POINT('Ctrl Pts',(0.498005492387928,-0.636309800095197,
2.29762330707595));
#46489=CARTESIAN_POINT('Ctrl Pts',(0.456885556256962,-0.319434907277159,
2.3620887571749));
#46490=CARTESIAN_POINT('Ctrl Pts',(0.421622938295452,-0.158333333333332,
2.40449900401168));
#46491=CARTESIAN_POINT('Ctrl Pts',(0.388101299179105,0.158333333333334,
2.40154708985519));
#46492=CARTESIAN_POINT('Ctrl Pts',(0.388390780368124,0.319434907277167,
2.35598614174768));
#46493=CARTESIAN_POINT('Ctrl Pts',(0.364186147471471,0.636309800095206,
2.28591277009536));
#46494=CARTESIAN_POINT('Ctrl Pts',(0.362428040910858,0.79477268400084,2.21616273366966));
#46495=CARTESIAN_POINT('Ctrl Pts',(0.308246235571133,1.06847604194622,2.17208689777873));
#46496=CARTESIAN_POINT('Ctrl Pts',(0.275593257591481,1.18514270861395,2.16377105386994));
#46497=CARTESIAN_POINT('Ctrl Pts',(0.233740597530111,1.30000000000322,2.16621816223897));
#46498=CARTESIAN_POINT('Ctrl Pts',(0.483946399133603,-1.30000000000266,
2.17843887244765));
#46499=CARTESIAN_POINT('Ctrl Pts',(0.512888765856687,-1.18514270861359,
2.17564712079955));
#46500=CARTESIAN_POINT('Ctrl Pts',(0.529237518131318,-1.06847604194603,
2.18307585696931));
#46501=CARTESIAN_POINT('Ctrl Pts',(0.537912637722501,-0.794772684000851,
2.22384909509565));
#46502=CARTESIAN_POINT('Ctrl Pts',(0.503949232631998,-0.636309800095197,
2.28997379608543));
#46503=CARTESIAN_POINT('Ctrl Pts',(0.462594679683807,-0.319434907277159,
2.35432227873226));
#46504=CARTESIAN_POINT('Ctrl Pts',(0.426715573255356,-0.158333333333332,
2.39694208629252));
#46505=CARTESIAN_POINT('Ctrl Pts',(0.392969830593601,0.158333333333334,
2.39391966368364));
#46506=CARTESIAN_POINT('Ctrl Pts',(0.393579787166861,0.319434907277167,
2.34805851202242));
#46507=CARTESIAN_POINT('Ctrl Pts',(0.369299762851234,0.636309800095206,
2.27799949945949));
#46508=CARTESIAN_POINT('Ctrl Pts',(0.367561330758701,0.79477268400084,2.20803046838465));
#46509=CARTESIAN_POINT('Ctrl Pts',(0.312674005335227,1.06847604194622,2.16502926539412));
#46510=CARTESIAN_POINT('Ctrl Pts',(0.279563873101028,1.18514270861395,2.15745638610035));
#46511=CARTESIAN_POINT('Ctrl Pts',(0.237102298032725,1.30000000000322,2.1609242549359));
#46512=CARTESIAN_POINT('',(0.213860511246102,1.2,2.25462198798418));
#46513=CARTESIAN_POINT('Ctrl Pts',(0.213860511246104,1.2,2.25462198798418));
#46514=CARTESIAN_POINT('Ctrl Pts',(0.195886995792624,1.22118111428885,2.27504564220851));
#46515=CARTESIAN_POINT('Ctrl Pts',(0.176998222640389,1.24193578764922,2.29509804001042));
#46516=CARTESIAN_POINT('Ctrl Pts',(0.151092207988087,1.27245710963303,2.32479181701016));
#46517=CARTESIAN_POINT('Ctrl Pts',(0.137742735792041,1.2882450460087,2.34018786318843));
#46518=CARTESIAN_POINT('Ctrl Pts',(0.128170675826792,1.30000000000322,2.35169387540072));
#46519=CARTESIAN_POINT('',(0.370132030376144,0.653834841391769,2.26385755069956));
#46520=CARTESIAN_POINT('Ctrl Pts',(0.370132030358563,0.653834841386714,
2.26385755066746));
#46521=CARTESIAN_POINT('Ctrl Pts',(0.355372633079986,0.712189636236907,
2.26275083105034));
#46522=CARTESIAN_POINT('Ctrl Pts',(0.340070501696384,0.767445165592266,
2.26166968552551));
#46523=CARTESIAN_POINT('Ctrl Pts',(0.30758726046148,0.882924976234983,2.25953788508247));
#46524=CARTESIAN_POINT('Ctrl Pts',(0.292298074915713,0.939652190622242,
2.25860205979761));
#46525=CARTESIAN_POINT('Ctrl Pts',(0.263959382956805,1.03591237463789,2.25703347013213));
#46526=CARTESIAN_POINT('Ctrl Pts',(0.253916623229151,1.0684334822601,2.25650694870429));
#46527=CARTESIAN_POINT('Ctrl Pts',(0.235165173386919,1.13047486660148,2.25558124511564));
#46528=CARTESIAN_POINT('Ctrl Pts',(0.224576556021974,1.16564206843845,2.25508539822476));
#46529=CARTESIAN_POINT('Ctrl Pts',(0.213860511246104,1.2,2.25462198798418));
#46530=CARTESIAN_POINT('',(0.509087305688322,-0.653834841531101,2.27624836987211));
#46531=CARTESIAN_POINT('Ctrl Pts',(0.509087305688321,-0.653834841531104,
2.27624836987211));
#46532=CARTESIAN_POINT('Ctrl Pts',(0.487739282837231,-0.575782745252652,
2.31204498712868));
#46533=CARTESIAN_POINT('Ctrl Pts',(0.468923233250106,-0.493709515665895,
2.34172379348987));
#46534=CARTESIAN_POINT('Ctrl Pts',(0.439956689959719,-0.338081440925158,
2.38329158654632));
#46535=CARTESIAN_POINT('Ctrl Pts',(0.428678359570631,-0.265625141639599,
2.39723212646428));
#46536=CARTESIAN_POINT('Ctrl Pts',(0.410247542056258,-0.12969433266082,
2.4132538570188));
#46537=CARTESIAN_POINT('Ctrl Pts',(0.402792651297061,-0.0666403947625616,
2.41677473360006));
#46538=CARTESIAN_POINT('Ctrl Pts',(0.389535713993002,0.059482301318641,
2.41596967380273));
#46539=CARTESIAN_POINT('Ctrl Pts',(0.383648853857911,0.122682321790056,
2.41165594399881));
#46540=CARTESIAN_POINT('Ctrl Pts',(0.373499427988676,0.26006074221674,2.39368024622825));
#46541=CARTESIAN_POINT('Ctrl Pts',(0.369686868827108,0.333931391400696,
2.37844650643877));
#46542=CARTESIAN_POINT('Ctrl Pts',(0.366022638034873,0.491495423102932,
2.3336888357912));
#46543=CARTESIAN_POINT('Ctrl Pts',(0.366607600922235,0.574890353678907,
2.3019351734762));
#46544=CARTESIAN_POINT('Ctrl Pts',(0.370132030316485,0.653834841406594,
2.26385755072478));
#46545=CARTESIAN_POINT('',(0.437191572703802,-1.2,2.26934451327648));
#46546=CARTESIAN_POINT('Ctrl Pts',(0.437191572703802,-1.2,2.26934451327648));
#46547=CARTESIAN_POINT('Ctrl Pts',(0.450657019484388,-1.12876701747688,
2.2705384680906));
#46548=CARTESIAN_POINT('Ctrl Pts',(0.467003073169165,-1.03051724707754,
2.27204751542371));
#46549=CARTESIAN_POINT('Ctrl Pts',(0.49993829496903,-0.776505233457344,
2.27528643342527));
#46550=CARTESIAN_POINT('Ctrl Pts',(0.504034558319737,-0.721760519705801,
2.27572594515669));
#46551=CARTESIAN_POINT('Ctrl Pts',(0.509087305688321,-0.653834841531101,
2.27624836987212));
#46552=CARTESIAN_POINT('Ctrl Pts',(0.35416429646195,-1.3,2.36294845478037));
#46553=CARTESIAN_POINT('Ctrl Pts',(0.368383275106154,-1.28213859625167,
2.34608033732313));
#46554=CARTESIAN_POINT('Ctrl Pts',(0.383008753255496,-1.26440354740105,
2.32942146191478));
#46555=CARTESIAN_POINT('Ctrl Pts',(0.416069593475857,-1.22469302390907,
2.29227038705738));
#46556=CARTESIAN_POINT('Ctrl Pts',(0.423498885283735,-1.21525386319095,
2.28344411837659));
#46557=CARTESIAN_POINT('Ctrl Pts',(0.437191572703802,-1.2,2.26934451327648));
#46558=CARTESIAN_POINT('Origin',(0.,1.25,7.2));
#46559=CARTESIAN_POINT('Origin',(0.,1.2,7.2));
#46560=CARTESIAN_POINT('Origin',(0.,0.92691742076555,7.2));
#46561=CARTESIAN_POINT('Origin',(0.,0.653834841531101,7.2));
#46562=CARTESIAN_POINT('Origin',(0.,0.,7.2));
#46563=CARTESIAN_POINT('Origin',(0.,-0.653834841531101,7.2));
#46564=CARTESIAN_POINT('Origin',(0.,-0.926917420765551,7.2));
#46565=CARTESIAN_POINT('Origin',(0.,-1.2,7.2));
#46566=CARTESIAN_POINT('Origin',(0.,-1.25,7.2));
#46567=CARTESIAN_POINT('Ctrl Pts',(0.815761714367341,-1.30000000000348,
2.2217438103648));
#46568=CARTESIAN_POINT('Ctrl Pts',(0.774949037064399,-1.18514270861414,
2.20952346491477));
#46569=CARTESIAN_POINT('Ctrl Pts',(0.7409879505214,-1.06847604194631,2.21004687504984));
#46570=CARTESIAN_POINT('Ctrl Pts',(0.678359592026837,-0.794772684000851,
2.24069668195063));
#46571=CARTESIAN_POINT('Ctrl Pts',(0.662111769290086,-0.636309800095197,
2.30877528147029));
#46572=CARTESIAN_POINT('Ctrl Pts',(0.623796234000798,-0.319434907277159,
2.37225523561121));
#46573=CARTESIAN_POINT('Ctrl Pts',(0.614857791974963,-0.158333333333332,
2.4172410281768));
#46574=CARTESIAN_POINT('Ctrl Pts',(0.581221077760459,0.158333333333334,
2.41318126918527));
#46575=CARTESIAN_POINT('Ctrl Pts',(0.554987172143311,0.319434907277167,
2.36403312099341));
#46576=CARTESIAN_POINT('Ctrl Pts',(0.527915117225985,0.636309800095206,
2.29249271205691));
#46577=CARTESIAN_POINT('Ctrl Pts',(0.508441992410805,0.79477268400084,2.22075160546092));
#46578=CARTESIAN_POINT('Ctrl Pts',(0.525404772703901,1.06847604194528,2.18267301919523));
#46579=CARTESIAN_POINT('Ctrl Pts',(0.542940786614004,1.18514270861212,2.17880571546092));
#46580=CARTESIAN_POINT('Ctrl Pts',(0.570670255378281,1.30000000000051,2.18755391703607));
#46581=CARTESIAN_POINT('Ctrl Pts',(0.817949288434644,-1.30000000000348,
2.22762096990277));
#46582=CARTESIAN_POINT('Ctrl Pts',(0.777519991852497,-1.18514270861414,
2.21652567939064));
#46583=CARTESIAN_POINT('Ctrl Pts',(0.743851598618606,-1.06847604194631,
2.21787086628889));
#46584=CARTESIAN_POINT('Ctrl Pts',(0.681689914158223,-0.794772684000851,
2.24971850865432));
#46585=CARTESIAN_POINT('Ctrl Pts',(0.665468378431205,-0.636309800095197,
2.3175788085538));
#46586=CARTESIAN_POINT('Ctrl Pts',(0.627223601653558,-0.319434907277159,
2.38108848276862));
#46587=CARTESIAN_POINT('Ctrl Pts',(0.618034103229147,-0.158333333333332,
2.42571400136448));
#46588=CARTESIAN_POINT('Ctrl Pts',(0.584631254891397,0.158333333333334,
2.42163186844655));
#46589=CARTESIAN_POINT('Ctrl Pts',(0.558956795864976,0.319434907277167,
2.37281687672975));
#46590=CARTESIAN_POINT('Ctrl Pts',(0.532138549723521,0.636309800095206,
2.30121083594925));
#46591=CARTESIAN_POINT('Ctrl Pts',(0.512750945719485,0.79477268400084,2.22966866896796));
#46592=CARTESIAN_POINT('Ctrl Pts',(0.529208707810351,1.06847604194528,2.19038889410686));
#46593=CARTESIAN_POINT('Ctrl Pts',(0.546373190975948,1.18514270861212,2.18570493282075));
#46594=CARTESIAN_POINT('Ctrl Pts',(0.573578201918189,1.30000000000051,2.1933397693268));
#46595=CARTESIAN_POINT('Ctrl Pts',(0.822480438837854,-1.30000000000349,
2.23938366296825));
#46596=CARTESIAN_POINT('Ctrl Pts',(0.782697976355179,-1.18514270861414,
2.23053940047333));
#46597=CARTESIAN_POINT('Ctrl Pts',(0.749515793345079,-1.06847604194632,
2.23352974476871));
#46598=CARTESIAN_POINT('Ctrl Pts',(0.688106278482148,-0.794772684000857,
2.26777834749776));
#46599=CARTESIAN_POINT('Ctrl Pts',(0.67177948580503,-0.636309800095199,
2.33521414055764));
#46600=CARTESIAN_POINT('Ctrl Pts',(0.633792497448733,-0.319434907277159,
2.39877822350881));
#46601=CARTESIAN_POINT('Ctrl Pts',(0.624484670435901,-0.158333333333333,
2.44266448378591));
#46602=CARTESIAN_POINT('Ctrl Pts',(0.591715216368591,0.158333333333335,
2.43852754202018));
#46603=CARTESIAN_POINT('Ctrl Pts',(0.567079234854538,0.319434907277167,
2.39037832109855));
#46604=CARTESIAN_POINT('Ctrl Pts',(0.540709280232551,0.636309800095207,
2.3186442770227));
#46605=CARTESIAN_POINT('Ctrl Pts',(0.521366831150013,0.794772684000843,
2.24751275404973));
#46606=CARTESIAN_POINT('Ctrl Pts',(0.536815007810077,1.06847604194529,2.20583058195238));
#46607=CARTESIAN_POINT('Ctrl Pts',(0.553267033024608,1.18514270861212,2.19951049152181));
#46608=CARTESIAN_POINT('Ctrl Pts',(0.579484140188884,1.30000000000051,2.20491297848492));
#46609=CARTESIAN_POINT('Ctrl Pts',(0.827534611873413,-1.30000000000348,
2.25405439187517));
#46610=CARTESIAN_POINT('Ctrl Pts',(0.789705377274445,-1.18514270861414,
2.24801726208739));
#46611=CARTESIAN_POINT('Ctrl Pts',(0.757829796105519,-1.06847604194632,
2.25306288479746));
#46612=CARTESIAN_POINT('Ctrl Pts',(0.697944957365153,-0.794772684000858,
2.29032265799794));
#46613=CARTESIAN_POINT('Ctrl Pts',(0.680137957616897,-0.636309800095199,
2.35725623009178));
#46614=CARTESIAN_POINT('Ctrl Pts',(0.641914390341109,-0.319434907277159,
2.42091020322842));
#46615=CARTESIAN_POINT('Ctrl Pts',(0.632611912435405,-0.158333333333333,
2.46386008262676));
#46616=CARTESIAN_POINT('Ctrl Pts',(0.600064040384407,0.158333333333335,
2.45970027866479));
#46617=CARTESIAN_POINT('Ctrl Pts',(0.575717151510573,0.31943490727717,2.41247332235234));
#46618=CARTESIAN_POINT('Ctrl Pts',(0.549886712394817,0.636309800095209,
2.34058500462056));
#46619=CARTESIAN_POINT('Ctrl Pts',(0.53195046354595,0.794772684000843,2.26986813875903));
#46620=CARTESIAN_POINT('Ctrl Pts',(0.546133892069255,1.06847604194529,2.22516386723107));
#46621=CARTESIAN_POINT('Ctrl Pts',(0.561433503866172,1.18514270861212,2.21680472792377));
#46622=CARTESIAN_POINT('Ctrl Pts',(0.585893246800085,1.30000000000051,2.21943727199712));
#46623=CARTESIAN_POINT('Ctrl Pts',(0.833274616578554,-1.30000000000348,
2.27170676121989));
#46624=CARTESIAN_POINT('Ctrl Pts',(0.796691660229516,-1.18514270861414,
2.26906812379398));
#46625=CARTESIAN_POINT('Ctrl Pts',(0.765764921284813,-1.06847604194632,
2.27659600561126));
#46626=CARTESIAN_POINT('Ctrl Pts',(0.707384961176366,-0.794772684000854,
2.31747361181352));
#46627=CARTESIAN_POINT('Ctrl Pts',(0.689805300234883,-0.636309800095199,
2.38373849431988));
#46628=CARTESIAN_POINT('Ctrl Pts',(0.651479287123272,-0.31943490727716,
2.44749818966568));
#46629=CARTESIAN_POINT('Ctrl Pts',(0.640702068838736,-0.158333333333333,
2.48938875417485));
#46630=CARTESIAN_POINT('Ctrl Pts',(0.608698086977467,0.158333333333335,
2.48518269228587));
#46631=CARTESIAN_POINT('Ctrl Pts',(0.586397462498248,0.319434907277168,
2.43897134670432));
#46632=CARTESIAN_POINT('Ctrl Pts',(0.561721046259436,0.636309800095208,
2.36687788085369));
#46633=CARTESIAN_POINT('Ctrl Pts',(0.544514136142152,0.794772684000843,
2.29672597466129));
#46634=CARTESIAN_POINT('Ctrl Pts',(0.557236461195469,1.06847604194529,2.24839375600363));
#46635=CARTESIAN_POINT('Ctrl Pts',(0.571326105454448,1.18514270861212,2.23757572236879));
#46636=CARTESIAN_POINT('Ctrl Pts',(0.593998370865426,1.30000000000051,2.23686088167082));
#46637=CARTESIAN_POINT('Ctrl Pts',(0.838472051594579,-1.30000000000349,
2.28497244552649));
#46638=CARTESIAN_POINT('Ctrl Pts',(0.802393619181787,-1.18514270861415,
2.28487318828213));
#46639=CARTESIAN_POINT('Ctrl Pts',(0.771873709768992,-1.06847604194632,
2.29425687379296));
#46640=CARTESIAN_POINT('Ctrl Pts',(0.714207913647501,-0.794772684000862,
2.33784255934328));
#46641=CARTESIAN_POINT('Ctrl Pts',(0.696654586576742,-0.636309800095204,
2.40363091935228));
#46642=CARTESIAN_POINT('Ctrl Pts',(0.658879800371154,-0.319434907277162,
2.46744541131595));
#46643=CARTESIAN_POINT('Ctrl Pts',(0.64860187246558,-0.158333333333334,
2.50847000637261));
#46644=CARTESIAN_POINT('Ctrl Pts',(0.616923322998412,0.158333333333336,
2.50423682079874));
#46645=CARTESIAN_POINT('Ctrl Pts',(0.594328865496985,0.31943490727717,2.45887586832793));
#46646=CARTESIAN_POINT('Ctrl Pts',(0.570008485219607,0.636309800095213,
2.38664883575975));
#46647=CARTESIAN_POINT('Ctrl Pts',(0.554294603428068,0.794772684000849,
2.3168668138778));
#46648=CARTESIAN_POINT('Ctrl Pts',(0.565934859131679,1.06847604194529,2.26580745919462));
#46649=CARTESIAN_POINT('Ctrl Pts',(0.578992677077282,1.18514270861213,2.25314966902608));
#46650=CARTESIAN_POINT('Ctrl Pts',(0.600069677588373,1.30000000000052,2.2499357913958));
#46651=CARTESIAN_POINT('Ctrl Pts',(0.842426321676452,-1.30000000000349,
2.29673831794152));
#46652=CARTESIAN_POINT('Ctrl Pts',(0.807669532123175,-1.18514270861415,
2.29890154496789));
#46653=CARTESIAN_POINT('Ctrl Pts',(0.778044811919046,-1.06847604194632,
2.3099405040634));
#46654=CARTESIAN_POINT('Ctrl Pts',(0.721461888706337,-0.794772684000861,
2.35594742457385));
#46655=CARTESIAN_POINT('Ctrl Pts',(0.703138929641752,-0.636309800095203,
2.42131458953646));
#46656=CARTESIAN_POINT('Ctrl Pts',(0.664974654116365,-0.319434907277162,
2.48520860293727));
#46657=CARTESIAN_POINT('Ctrl Pts',(0.653927425302214,-0.158333333333334,
2.5255137757051));
#46658=CARTESIAN_POINT('Ctrl Pts',(0.62257423698162,0.158333333333336,2.52125543432605));
#46659=CARTESIAN_POINT('Ctrl Pts',(0.601347319644754,0.319434907277171,
2.47657922652961));
#46660=CARTESIAN_POINT('Ctrl Pts',(0.577523332854969,0.636309800095213,
2.40424082720034));
#46661=CARTESIAN_POINT('Ctrl Pts',(0.561729528529115,0.794772684000849,
2.33488259506381));
#46662=CARTESIAN_POINT('Ctrl Pts',(0.572424770514813,1.06847604194529,2.28139441775701));
#46663=CARTESIAN_POINT('Ctrl Pts',(0.584831835923992,1.18514270861213,2.26707904245198));
#46664=CARTESIAN_POINT('Ctrl Pts',(0.60501639278451,1.30000000000052,2.26160134186575));
#46665=CARTESIAN_POINT('Ctrl Pts',(0.8438497664825,-1.30000000000349,2.30115438810863));
#46666=CARTESIAN_POINT('Ctrl Pts',(0.809459220322253,-1.18514270861415,
2.30416804614865));
#46667=CARTESIAN_POINT('Ctrl Pts',(0.780093900817013,-1.06847604194632,
2.31582890677064));
#46668=CARTESIAN_POINT('Ctrl Pts',(0.723863417114391,-0.794772684000862,
2.36274459538565));
#46669=CARTESIAN_POINT('Ctrl Pts',(0.705401126882505,-0.636309800095203,
2.42795199955603));
#46670=CARTESIAN_POINT('Ctrl Pts',(0.667214983652006,-0.319434907277162,
2.49187283705493));
#46671=CARTESIAN_POINT('Ctrl Pts',(0.656010235704721,-0.158333333333334,
2.53190307843187));
#46672=CARTESIAN_POINT('Ctrl Pts',(0.624775101141794,0.158333333333336,
2.52763656325065));
#46673=CARTESIAN_POINT('Ctrl Pts',(0.603848368774456,0.319434907277171,
2.48322770226953));
#46674=CARTESIAN_POINT('Ctrl Pts',(0.580236583661767,0.636309800095213,
2.41084462918358));
#46675=CARTESIAN_POINT('Ctrl Pts',(0.564680105060892,0.794772684000849,
2.34162841200642));
#46676=CARTESIAN_POINT('Ctrl Pts',(0.57505182445287,1.06847604194529,2.28722736164216));
#46677=CARTESIAN_POINT('Ctrl Pts',(0.587180532214312,1.18514270861213,2.27229261411699));
#46678=CARTESIAN_POINT('Ctrl Pts',(0.606948414722484,1.30000000000052,2.26597131801177));
#46679=CARTESIAN_POINT('Ctrl Pts',(0.845225075246657,-1.30000000000349,
2.30557234964075));
#46680=CARTESIAN_POINT('Ctrl Pts',(0.81114213914197,-1.18514270861415,2.3094377763209));
#46681=CARTESIAN_POINT('Ctrl Pts',(0.782001214760848,-1.06847604194632,
2.32172138880894));
#46682=CARTESIAN_POINT('Ctrl Pts',(0.726096885546306,-0.794772684000862,
2.36954668425287));
#46683=CARTESIAN_POINT('Ctrl Pts',(0.707561471282311,-0.636309800095204,
2.43459335551303));
#46684=CARTESIAN_POINT('Ctrl Pts',(0.66940386339763,-0.319434907277162,
2.49853986597122));
#46685=CARTESIAN_POINT('Ctrl Pts',(0.658091989424287,-0.158333333333334,
2.53829296608385));
#46686=CARTESIAN_POINT('Ctrl Pts',(0.626973132394117,0.158333333333336,
2.53401917970609));
#46687=CARTESIAN_POINT('Ctrl Pts',(0.606257617298661,0.319434907277171,
2.48988288844787));
#46688=CARTESIAN_POINT('Ctrl Pts',(0.582878968391157,0.636309800095214,
2.41745383249566));
#46689=CARTESIAN_POINT('Ctrl Pts',(0.567689353837315,0.794772684000849,
2.34837164734979));
#46690=CARTESIAN_POINT('Ctrl Pts',(0.577756049883937,1.06847604194529,2.29305625514846));
#46691=CARTESIAN_POINT('Ctrl Pts',(0.589591259077048,1.18514270861213,2.2775028556469));
#46692=CARTESIAN_POINT('Ctrl Pts',(0.608904177752535,1.30000000000052,2.27034004029047));
#46693=CARTESIAN_POINT('Ctrl Pts',(0.84787373850355,-1.30000000000349,2.31441471133581));
#46694=CARTESIAN_POINT('Ctrl Pts',(0.814200412838562,-1.18514270861415,
2.319987142917));
#46695=CARTESIAN_POINT('Ctrl Pts',(0.7853851804585,-1.06847604194632,2.33351833085404));
#46696=CARTESIAN_POINT('Ctrl Pts',(0.730039396539782,-0.794772684000861,
2.38316440121895));
#46697=CARTESIAN_POINT('Ctrl Pts',(0.711571769008138,-0.636309800095203,
2.44788687284398));
#46698=CARTESIAN_POINT('Ctrl Pts',(0.673676578636946,-0.319434907277162,
2.51187945678191));
#46699=CARTESIAN_POINT('Ctrl Pts',(0.662395363999465,-0.158333333333334,
2.55106875502679));
#46700=CARTESIAN_POINT('Ctrl Pts',(0.631512165133043,0.158333333333336,
2.54678256436095));
#46701=CARTESIAN_POINT('Ctrl Pts',(0.610861968467718,0.31943490727717,2.50320992785811));
#46702=CARTESIAN_POINT('Ctrl Pts',(0.587985439671236,0.636309800095212,
2.43068456480014));
#46703=CARTESIAN_POINT('Ctrl Pts',(0.573946563231074,0.794772684000848,
2.3618426182233));
#46704=CARTESIAN_POINT('Ctrl Pts',(0.583473112734683,1.06847604194529,2.30469460083018));
#46705=CARTESIAN_POINT('Ctrl Pts',(0.594682459314614,1.18514270861213,2.28790715539512));
#46706=CARTESIAN_POINT('Ctrl Pts',(0.612977462187809,1.30000000000052,2.27906952371177));
#46707=CARTESIAN_POINT('Ctrl Pts',(0.852103938572023,-1.30000000000349,
2.32767411969882));
#46708=CARTESIAN_POINT('Ctrl Pts',(0.8194522968669,-1.18514270861415,2.33580350301075));
#46709=CARTESIAN_POINT('Ctrl Pts',(0.791333461953259,-1.06847604194632,
2.35120472677436));
#46710=CARTESIAN_POINT('Ctrl Pts',(0.736845018622613,-0.794772684000859,
2.40358404084236));
#46711=CARTESIAN_POINT('Ctrl Pts',(0.717802411277297,-0.636309800095203,
2.46782682103428));
#46712=CARTESIAN_POINT('Ctrl Pts',(0.679656280419845,-0.319434907277162,
2.53190271397085));
#46713=CARTESIAN_POINT('Ctrl Pts',(0.667771211845641,-0.158333333333334,
2.57026656208597));
#46714=CARTESIAN_POINT('Ctrl Pts',(0.637292788680856,0.158333333333336,
2.56596154500988));
#46715=CARTESIAN_POINT('Ctrl Pts',(0.617824840813535,0.31943490727717,2.52319718370858));
#46716=CARTESIAN_POINT('Ctrl Pts',(0.595670101735524,0.636309800095212,
2.45054679965987));
#46717=CARTESIAN_POINT('Ctrl Pts',(0.582135679870625,0.794772684000848,
2.38214575462174));
#46718=CARTESIAN_POINT('Ctrl Pts',(0.590787034920216,1.06847604194529,2.32224861478318));
#46719=CARTESIAN_POINT('Ctrl Pts',(0.601255474529726,1.18514270861213,2.30359241829711));
#46720=CARTESIAN_POINT('Ctrl Pts',(0.618447502712073,1.30000000000052,2.29220727775335));
#46721=CARTESIAN_POINT('Ctrl Pts',(0.857969453717047,-1.30000000000349,
2.34536437000766));
#46722=CARTESIAN_POINT('Ctrl Pts',(0.826874392876982,-1.18514270861415,
2.35690645245089));
#46723=CARTESIAN_POINT('Ctrl Pts',(0.799812377387329,-1.06847604194632,
2.37480354034066));
#46724=CARTESIAN_POINT('Ctrl Pts',(0.746610849436285,-0.794772684000859,
2.43083072756189));
#46725=CARTESIAN_POINT('Ctrl Pts',(0.726719229771669,-0.636309800095202,
2.49443343321409));
#46726=CARTESIAN_POINT('Ctrl Pts',(0.688052574451537,-0.319434907277161,
2.55861968388106));
#46727=CARTESIAN_POINT('Ctrl Pts',(0.675108317438119,-0.158333333333334,
2.59587838761032));
#46728=CARTESIAN_POINT('Ctrl Pts',(0.644961961098522,0.158333333333336,
2.59155173687621));
#46729=CARTESIAN_POINT('Ctrl Pts',(0.626942933423789,0.31943490727717,2.54987878732425));
#46730=CARTESIAN_POINT('Ctrl Pts',(0.605867655715064,0.636309800095211,
2.47705788552953));
#46731=CARTESIAN_POINT('Ctrl Pts',(0.593407148634716,0.794772684000847,
2.40922488538287));
#46732=CARTESIAN_POINT('Ctrl Pts',(0.601050462974228,1.06847604194529,2.34565394034333));
#46733=CARTESIAN_POINT('Ctrl Pts',(0.610545298265256,1.18514270861213,2.3245048766012));
#46734=CARTESIAN_POINT('Ctrl Pts',(0.626226461282443,1.30000000000052,2.3097242556889));
#46735=CARTESIAN_POINT('Ctrl Pts',(0.864892167006608,-1.30000000000349,
2.36896827823977));
#46736=CARTESIAN_POINT('Ctrl Pts',(0.835076211528464,-1.18514270861415,
2.38507496762836));
#46737=CARTESIAN_POINT('Ctrl Pts',(0.808890045383593,-1.06847604194632,
2.40630938309406));
#46738=CARTESIAN_POINT('Ctrl Pts',(0.756780302561369,-0.794772684000858,
2.46721120378601));
#46739=CARTESIAN_POINT('Ctrl Pts',(0.736004391759345,-0.636309800095201,
2.52995196405356));
#46740=CARTESIAN_POINT('Ctrl Pts',(0.697428015081395,-0.31943490727716,
2.59427726117001));
#46741=CARTESIAN_POINT('Ctrl Pts',(0.68434036320485,-0.158333333333333,
2.63004974172785));
#46742=CARTESIAN_POINT('Ctrl Pts',(0.655322158131372,0.158333333333335,
2.62569284382494));
#46743=CARTESIAN_POINT('Ctrl Pts',(0.639198686598927,0.319434907277169,
2.58547284172007));
#46744=CARTESIAN_POINT('Ctrl Pts',(0.619060029681164,0.63630980009521,2.5124574511204));
#46745=CARTESIAN_POINT('Ctrl Pts',(0.606808450459504,0.794772684000846,
2.44545422774618));
#46746=CARTESIAN_POINT('Ctrl Pts',(0.612845176618029,1.06847604194529,2.3769830649708));
#46747=CARTESIAN_POINT('Ctrl Pts',(0.621157569349446,1.18514270861213,2.35249169112608));
#46748=CARTESIAN_POINT('Ctrl Pts',(0.635169279741,1.30000000000051,2.33314757269551));
#46749=CARTESIAN_POINT('Ctrl Pts',(0.871983856110559,-1.30000000000349,
2.39259530305307));
#46750=CARTESIAN_POINT('Ctrl Pts',(0.843492504925306,-1.18514270861415,
2.41326700102741));
#46751=CARTESIAN_POINT('Ctrl Pts',(0.818280869489698,-1.06847604194632,
2.43783986036201));
#46752=CARTESIAN_POINT('Ctrl Pts',(0.767613747549898,-0.794772684000856,
2.50362054437507));
#46753=CARTESIAN_POINT('Ctrl Pts',(0.746699420507565,-0.636309800095201,
2.56550661167277));
#46754=CARTESIAN_POINT('Ctrl Pts',(0.708067863075721,-0.319434907277161,
2.62997336311469));
#46755=CARTESIAN_POINT('Ctrl Pts',(0.694162607171851,-0.158333333333333,
2.6642445087104));
#46756=CARTESIAN_POINT('Ctrl Pts',(0.665302359551536,0.158333333333335,
2.65987892344331));
#46757=CARTESIAN_POINT('Ctrl Pts',(0.6498918287039,0.319434907277168,2.62116799218465));
#46758=CARTESIAN_POINT('Ctrl Pts',(0.630665040150285,0.636309800095209,
2.54795999874999));
#46759=CARTESIAN_POINT('Ctrl Pts',(0.619960840132648,0.794772684000845,
2.48173444454022));
#46760=CARTESIAN_POINT('Ctrl Pts',(0.625102222111385,1.06847604194529,2.40833499866515));
#46761=CARTESIAN_POINT('Ctrl Pts',(0.632439243853823,1.18514270861213,2.38049291658993));
#46762=CARTESIAN_POINT('Ctrl Pts',(0.644887773587081,1.30000000000052,2.3565806528413));
#46763=CARTESIAN_POINT('Ctrl Pts',(0.8788002795845,-1.30000000000349,2.41622813084116));
#46764=CARTESIAN_POINT('Ctrl Pts',(0.851801484847447,-1.18514270861415,
2.44148383612387));
#46765=CARTESIAN_POINT('Ctrl Pts',(0.827464580237682,-1.06847604194632,
2.46940614964295));
#46766=CARTESIAN_POINT('Ctrl Pts',(0.77739096071164,-0.794772684000858,
2.54007267819047));
#46767=CARTESIAN_POINT('Ctrl Pts',(0.754165665727303,-0.636309800095201,
2.60107065326827));
#46768=CARTESIAN_POINT('Ctrl Pts',(0.715146022357394,-0.31943490727716,
2.66567920983969));
#46769=CARTESIAN_POINT('Ctrl Pts',(0.701755319112731,-0.158333333333333,
2.69847254135808));
#46770=CARTESIAN_POINT('Ctrl Pts',(0.674041403273267,0.158333333333335,
2.69410734100179));
#46771=CARTESIAN_POINT('Ctrl Pts',(0.659818978446064,0.319434907277168,
2.65690091063574));
#46772=CARTESIAN_POINT('Ctrl Pts',(0.642182073293505,0.636309800095209,
2.58349832102157));
#46773=CARTESIAN_POINT('Ctrl Pts',(0.633514118471711,0.794772684000844,
2.51804753122718));
#46774=CARTESIAN_POINT('Ctrl Pts',(0.637539702821843,1.06847604194529,2.43971769905602));
#46775=CARTESIAN_POINT('Ctrl Pts',(0.643595422408555,1.18514270861213,2.40852429620439));
#46776=CARTESIAN_POINT('Ctrl Pts',(0.653964335279407,1.30000000000051,2.38004357244173));
#46777=CARTESIAN_POINT('Ctrl Pts',(0.883492139156687,-1.30000000000349,
2.43396916719493));
#46778=CARTESIAN_POINT('Ctrl Pts',(0.856681013500535,-1.18514270861415,
2.46264282535752));
#46779=CARTESIAN_POINT('Ctrl Pts',(0.832636437723441,-1.06847604194632,
2.49306744915883));
#46780=CARTESIAN_POINT('Ctrl Pts',(0.783479941244749,-0.794772684000857,
2.56739949746954));
#46781=CARTESIAN_POINT('Ctrl Pts',(0.761811990638407,-0.636309800095201,
2.62778407484409));
#46782=CARTESIAN_POINT('Ctrl Pts',(0.722835384880657,-0.319434907277161,
2.69250196767029));
#46783=CARTESIAN_POINT('Ctrl Pts',(0.707689306788051,-0.158333333333333,
2.72414441130098));
#46784=CARTESIAN_POINT('Ctrl Pts',(0.679787873058307,0.158333333333335,
2.71977688689778));
#46785=CARTESIAN_POINT('Ctrl Pts',(0.666709735021752,0.319434907277167,
2.68371615702853));
#46786=CARTESIAN_POINT('Ctrl Pts',(0.649510613748425,0.636309800095208,
2.61020532966889));
#46787=CARTESIAN_POINT('Ctrl Pts',(0.640923069406501,0.794772684000846,
2.54540094788882));
#46788=CARTESIAN_POINT('Ctrl Pts',(0.644416052402014,1.06847604194529,2.46336564844072));
#46789=CARTESIAN_POINT('Ctrl Pts',(0.650065032644106,1.18514270861213,2.42963732643914));
#46790=CARTESIAN_POINT('Ctrl Pts',(0.659851010217308,1.30000000000052,2.39769072385965));
#46791=CARTESIAN_POINT('Ctrl Pts',(0.889558734078806,-1.30000000000349,
2.45759430808821));
#46792=CARTESIAN_POINT('Ctrl Pts',(0.864447810104551,-1.18514270861414,
2.49087694996875));
#46793=CARTESIAN_POINT('Ctrl Pts',(0.841353620899978,-1.06847604194632,
2.52466490734447));
#46794=CARTESIAN_POINT('Ctrl Pts',(0.79266048462534,-0.794772684000856,
2.60388922802155));
#46795=CARTESIAN_POINT('Ctrl Pts',(0.768013225048203,-0.636309800095199,
2.66334041368903));
#46796=CARTESIAN_POINT('Ctrl Pts',(0.728336186096216,-0.319434907277159,
2.72819115831008));
#46797=CARTESIAN_POINT('Ctrl Pts',(0.713521471386971,-0.158333333333333,
2.75836682748481));
#46798=CARTESIAN_POINT('Ctrl Pts',(0.687308314473149,0.158333333333335,
2.75402055085611));
#46799=CARTESIAN_POINT('Ctrl Pts',(0.676549378221223,0.319434907277169,
2.71949091277189));
#46800=CARTESIAN_POINT('Ctrl Pts',(0.661529476370098,0.636309800095208,
2.64580278422258));
#46801=CARTESIAN_POINT('Ctrl Pts',(0.654713806832131,0.794772684000841,
2.58177408144104));
#46802=CARTESIAN_POINT('Ctrl Pts',(0.657054029412615,1.06847604194529,2.49479983622051));
#46803=CARTESIAN_POINT('Ctrl Pts',(0.661390646011638,1.18514270861212,2.4577127159111));
#46804=CARTESIAN_POINT('Ctrl Pts',(0.669050883568385,1.30000000000051,2.42118640333487));
#46805=CARTESIAN_POINT('Ctrl Pts',(0.894786825006837,-1.30000000000348,
2.48121808219932));
#46806=CARTESIAN_POINT('Ctrl Pts',(0.870089124157715,-1.18514270861414,
2.51907311933544));
#46807=CARTESIAN_POINT('Ctrl Pts',(0.847384183496986,-1.06847604194632,
2.55620783446828));
#46808=CARTESIAN_POINT('Ctrl Pts',(0.799534903148645,-0.794772684000854,
2.64033236727146));
#46809=CARTESIAN_POINT('Ctrl Pts',(0.775766393023481,-0.636309800095198,
2.69895575203986));
#46810=CARTESIAN_POINT('Ctrl Pts',(0.736000855364474,-0.319434907277159,
2.76395207302188));
#46811=CARTESIAN_POINT('Ctrl Pts',(0.719880786059042,-0.158333333333333,
2.79258698076943));
#46812=CARTESIAN_POINT('Ctrl Pts',(0.693412198460061,0.158333333333335,
2.78825422777218));
#46813=CARTESIAN_POINT('Ctrl Pts',(0.68301387996786,0.319434907277168,2.75528325192732));
#46814=CARTESIAN_POINT('Ctrl Pts',(0.668966249908217,0.636309800095208,
2.68146817767856));
#46815=CARTESIAN_POINT('Ctrl Pts',(0.663916868088444,0.794772684000843,
2.61829877751067));
#46816=CARTESIAN_POINT('Ctrl Pts',(0.666256460671176,1.06847604194529,2.52637732519999));
#46817=CARTESIAN_POINT('Ctrl Pts',(0.670153579812955,1.18514270861212,2.48590479535088));
#46818=CARTESIAN_POINT('Ctrl Pts',(0.676935095157896,1.30000000000051,2.4447491263325));
#46819=CARTESIAN_POINT('Ctrl Pts',(0.900920744455079,-1.30000000000348,
2.50489467825102));
#46820=CARTESIAN_POINT('Ctrl Pts',(0.877338716593721,-1.18514270861414,
2.54735202983343));
#46821=CARTESIAN_POINT('Ctrl Pts',(0.855233562772959,-1.06847604194632,
2.58784497109303));
#46822=CARTESIAN_POINT('Ctrl Pts',(0.807578109807804,-0.794772684000853,
2.67685358516273));
#46823=CARTESIAN_POINT('Ctrl Pts',(0.781865791711984,-0.636309800095199,
2.73455216483046));
#46824=CARTESIAN_POINT('Ctrl Pts',(0.741131641213366,-0.31943490727716,
2.79966201910889));
#46825=CARTESIAN_POINT('Ctrl Pts',(0.724343372132867,-0.158333333333333,
2.82678245074128));
#46826=CARTESIAN_POINT('Ctrl Pts',(0.698885888203835,0.158333333333335,
2.8224844959558));
#46827=CARTESIAN_POINT('Ctrl Pts',(0.690689565611929,0.319434907277167,
2.79110176251162));
#46828=CARTESIAN_POINT('Ctrl Pts',(0.678605406869406,0.636309800095207,
2.7171646612579));
#46829=CARTESIAN_POINT('Ctrl Pts',(0.675175735315677,0.794772684000843,
2.65482275704941));
#46830=CARTESIAN_POINT('Ctrl Pts',(0.676706066558325,1.06847604194529,2.5579519195565));
#46831=CARTESIAN_POINT('Ctrl Pts',(0.679566040662273,1.18514270861212,2.51409824761092));
#46832=CARTESIAN_POINT('Ctrl Pts',(0.684623565179587,1.30000000000051,2.46832269985219));
#46833=CARTESIAN_POINT('Ctrl Pts',(0.90391928274594,-1.30000000000348,2.52258106592965));
#46834=CARTESIAN_POINT('Ctrl Pts',(0.880390345489287,-1.18514270861414,
2.5684617029937));
#46835=CARTESIAN_POINT('Ctrl Pts',(0.858348979019847,-1.06847604194631,
2.61145976839938));
#46836=CARTESIAN_POINT('Ctrl Pts',(0.81086559922143,-0.79477268400085,2.70413458403223));
#46837=CARTESIAN_POINT('Ctrl Pts',(0.78527553329063,-0.636309800095198,
2.76119931039013));
#46838=CARTESIAN_POINT('Ctrl Pts',(0.744792849592769,-0.31943490727716,
2.82643472239117));
#46839=CARTESIAN_POINT('Ctrl Pts',(0.728145602864073,-0.158333333333333,
2.85243807310469));
#46840=CARTESIAN_POINT('Ctrl Pts',(0.702967196216689,0.158333333333335,
2.84817008535361));
#46841=CARTESIAN_POINT('Ctrl Pts',(0.694751325057873,0.319434907277168,
2.81794370669857));
#46842=CARTESIAN_POINT('Ctrl Pts',(0.68330518681814,0.636309800095207,2.74392313105902));
#46843=CARTESIAN_POINT('Ctrl Pts',(0.680785537148619,0.794772684000843,
2.68225136282805));
#46844=CARTESIAN_POINT('Ctrl Pts',(0.682816849716337,1.06847604194529,2.58167296327534));
#46845=CARTESIAN_POINT('Ctrl Pts',(0.685764246691761,1.18514270861212,2.53527594870165));
#46846=CARTESIAN_POINT('Ctrl Pts',(0.690779760699591,1.30000000000051,2.48601858192366));
#46847=CARTESIAN_POINT('Ctrl Pts',(0.909809170319496,-1.30000000000348,
2.5462724368549));
#46848=CARTESIAN_POINT('Ctrl Pts',(0.88687330007218,-1.18514270861414,2.59673806151338));
#46849=CARTESIAN_POINT('Ctrl Pts',(0.86507605625583,-1.06847604194631,2.64307989218552));
#46850=CARTESIAN_POINT('Ctrl Pts',(0.817350517353609,-0.794772684000854,
2.74061200261849));
#46851=CARTESIAN_POINT('Ctrl Pts',(0.790156358795621,-0.636309800095199,
2.79673897566274));
#46852=CARTESIAN_POINT('Ctrl Pts',(0.748755125480717,-0.31943490727716,
2.86208266525968));
#46853=CARTESIAN_POINT('Ctrl Pts',(0.731538667378039,-0.158333333333333,
2.8865780598512));
#46854=CARTESIAN_POINT('Ctrl Pts',(0.707194541717449,0.158333333333335,
2.8823638986463));
#46855=CARTESIAN_POINT('Ctrl Pts',(0.700573425945651,0.319434907277167,
2.8537436091181));
#46856=CARTESIAN_POINT('Ctrl Pts',(0.691355618609777,0.636309800095207,
2.77963414761548));
#46857=CARTESIAN_POINT('Ctrl Pts',(0.691549177966722,0.794772684000843,
2.71882567537351));
#46858=CARTESIAN_POINT('Ctrl Pts',(0.693130508207208,1.06847604194529,2.61330408130346));
#46859=CARTESIAN_POINT('Ctrl Pts',(0.695036894474795,1.18514270861212,2.56351974022004));
#46860=CARTESIAN_POINT('Ctrl Pts',(0.698165167742923,1.30000000000051,2.50962744616575));
#46861=CARTESIAN_POINT('Ctrl Pts',(0.915082652483778,-1.30000000000348,
2.57870764115414));
#46862=CARTESIAN_POINT('Ctrl Pts',(0.892766917159951,-1.18514270861414,
2.63548079278448));
#46863=CARTESIAN_POINT('Ctrl Pts',(0.871247728879639,-1.06847604194631,
2.68642481038588));
#46864=CARTESIAN_POINT('Ctrl Pts',(0.823374282072721,-0.794772684000852,
2.79064921663921));
#46865=CARTESIAN_POINT('Ctrl Pts',(0.794677218926977,-0.636309800095197,
2.84550780327277));
#46866=CARTESIAN_POINT('Ctrl Pts',(0.752438118028174,-0.319434907277159,
2.9110027516138));
#46867=CARTESIAN_POINT('Ctrl Pts',(0.734524839113296,-0.158333333333332,
2.93339028932226));
#46868=CARTESIAN_POINT('Ctrl Pts',(0.711293802042359,0.158333333333334,
2.92927477868809));
#46869=CARTESIAN_POINT('Ctrl Pts',(0.70705880736915,0.319434907277168,2.90292244672223));
#46870=CARTESIAN_POINT('Ctrl Pts',(0.69977244719163,0.636309800095207,2.82873750113844));
#46871=CARTESIAN_POINT('Ctrl Pts',(0.700527288995702,0.794772684000841,
2.76912992220276));
#46872=CARTESIAN_POINT('Ctrl Pts',(0.702602766285981,1.06847604194528,2.65682156556838));
#46873=CARTESIAN_POINT('Ctrl Pts',(0.704531974766086,1.18514270861212,2.60237895529294));
#46874=CARTESIAN_POINT('Ctrl Pts',(0.707491994511347,1.30000000000051,2.54210786089436));
#46875=CARTESIAN_POINT('Ctrl Pts',(0.920469044817724,-1.30000000000348,
2.60822457195483));
#46876=CARTESIAN_POINT('Ctrl Pts',(0.898301433057237,-1.18514270861414,
2.6706818179568));
#46877=CARTESIAN_POINT('Ctrl Pts',(0.876625832255922,-1.06847604194631,
2.72576141099587));
#46878=CARTESIAN_POINT('Ctrl Pts',(0.827687501958213,-0.79477268400085,
2.83596243531162));
#46879=CARTESIAN_POINT('Ctrl Pts',(0.796999851289934,-0.636309800095195,
2.88958634448643));
#46880=CARTESIAN_POINT('Ctrl Pts',(0.753217519511882,-0.319434907277158,
2.95515815043732));
#46881=CARTESIAN_POINT('Ctrl Pts',(0.734354418192122,-0.158333333333332,
2.97563582202854));
#46882=CARTESIAN_POINT('Ctrl Pts',(0.711895970281559,0.158333333333334,
2.9716282579602));
#46883=CARTESIAN_POINT('Ctrl Pts',(0.709267921403271,0.319434907277166,
2.94735133204311));
#46884=CARTESIAN_POINT('Ctrl Pts',(0.705333696056776,0.636309800095204,
2.87319209469255));
#46885=CARTESIAN_POINT('Ctrl Pts',(0.710332355477971,0.794772684000837,
2.81480235774102));
#46886=CARTESIAN_POINT('Ctrl Pts',(0.71340381078195,1.06847604194528,2.69640362606351));
#46887=CARTESIAN_POINT('Ctrl Pts',(0.714828087227485,1.18514270861212,2.63774427434602));
#46888=CARTESIAN_POINT('Ctrl Pts',(0.716347120926098,1.30000000000051,2.57167599474888));
#46889=CARTESIAN_POINT('Ctrl Pts',(0.923992559503498,-1.30000000000348,
2.62890061695326));
#46890=CARTESIAN_POINT('Ctrl Pts',(0.901881354947266,-1.18514270861414,
2.69535387068794));
#46891=CARTESIAN_POINT('Ctrl Pts',(0.879974827805498,-1.06847604194631,
2.75333043280351));
#46892=CARTESIAN_POINT('Ctrl Pts',(0.829839213495544,-0.794772684000849,
2.86768503606482));
#46893=CARTESIAN_POINT('Ctrl Pts',(0.796781640694724,-0.636309800095195,
2.92033187439359));
#46894=CARTESIAN_POINT('Ctrl Pts',(0.752080256174901,-0.319434907277158,
2.98595958471202));
#46895=CARTESIAN_POINT('Ctrl Pts',(0.733844807360486,-0.158333333333332,
3.0052046640331));
#46896=CARTESIAN_POINT('Ctrl Pts',(0.712257063199493,0.158333333333334,
3.00131366662896));
#46897=CARTESIAN_POINT('Ctrl Pts',(0.710466878898138,0.319434907277167,
2.97846998365214));
#46898=CARTESIAN_POINT('Ctrl Pts',(0.708013675207788,0.636309800095205,
2.90432100677015));
#46899=CARTESIAN_POINT('Ctrl Pts',(0.714365401162632,0.794772684000839,
2.84677382123667));
#46900=CARTESIAN_POINT('Ctrl Pts',(0.718052883454901,1.06847604194528,2.7240992429047));
#46901=CARTESIAN_POINT('Ctrl Pts',(0.719470360074824,1.18514270861212,2.66248264767173));
#46902=CARTESIAN_POINT('Ctrl Pts',(0.72070913886503,1.3000000000005,2.59235073662463));
#46903=CARTESIAN_POINT('Ctrl Pts',(0.92529189916072,-1.30000000000348,2.63775451220662));
#46904=CARTESIAN_POINT('Ctrl Pts',(0.90286710161616,-1.18514270861414,2.70590656695599));
#46905=CARTESIAN_POINT('Ctrl Pts',(0.880718520683462,-1.06847604194631,
2.76512493099013));
#46906=CARTESIAN_POINT('Ctrl Pts',(0.830188983551121,-0.794772684000851,
2.88129258577059));
#46907=CARTESIAN_POINT('Ctrl Pts',(0.797251592334188,-0.636309800095197,
2.93363499971855));
#46908=CARTESIAN_POINT('Ctrl Pts',(0.752160119240198,-0.319434907277159,
2.99927731465237));
#46909=CARTESIAN_POINT('Ctrl Pts',(0.733263218353926,-0.158333333333332,
3.01787138809224));
#46910=CARTESIAN_POINT('Ctrl Pts',(0.711685603093662,0.158333333333334,
3.01399236569876));
#46911=CARTESIAN_POINT('Ctrl Pts',(0.710356982649902,0.319434907277167,
2.99180138145779));
#46912=CARTESIAN_POINT('Ctrl Pts',(0.708742289116701,0.636309800095206,
2.91768313620638));
#46913=CARTESIAN_POINT('Ctrl Pts',(0.71597300740823,0.794772684000841,2.86052978046723));
#46914=CARTESIAN_POINT('Ctrl Pts',(0.720292134275874,1.06847604194528,2.73602437620757));
#46915=CARTESIAN_POINT('Ctrl Pts',(0.721868578912404,1.18514270861212,2.6731325281192));
#46916=CARTESIAN_POINT('Ctrl Pts',(0.723151878203884,1.30000000000051,2.60124260806661));
#46917=CARTESIAN_POINT('Ctrl Pts',(0.926611318159751,-1.30000000000348,
2.64948665818269));
#46918=CARTESIAN_POINT('Ctrl Pts',(0.90445282821427,-1.18514270861414,2.71989773316588));
#46919=CARTESIAN_POINT('Ctrl Pts',(0.882280853198343,-1.06847604194631,
2.78074250462087));
#46920=CARTESIAN_POINT('Ctrl Pts',(0.831028002213023,-0.794772684000853,
2.89920602375347));
#46921=CARTESIAN_POINT('Ctrl Pts',(0.796094523755093,-0.636309800095197,
2.95088445224024));
#46922=CARTESIAN_POINT('Ctrl Pts',(0.750381762823946,-0.319434907277159,
3.01654690138816));
#46923=CARTESIAN_POINT('Ctrl Pts',(0.732176691888254,-0.158333333333332,
3.0345337535851));
#46924=CARTESIAN_POINT('Ctrl Pts',(0.711294701270189,0.158333333333334,
3.03075995137096));
#46925=CARTESIAN_POINT('Ctrl Pts',(0.710351572107801,0.319434907277166,
3.00935787644432));
#46926=CARTESIAN_POINT('Ctrl Pts',(0.709997615251027,0.636309800095205,
2.93527806331773));
#46927=CARTESIAN_POINT('Ctrl Pts',(0.718617994233884,0.794772684000841,
2.87864263863507));
#46928=CARTESIAN_POINT('Ctrl Pts',(0.723706711382351,1.06847604194528,2.75176911793317));
#46929=CARTESIAN_POINT('Ctrl Pts',(0.725391320126886,1.18514270861212,2.68722624494357));
#46930=CARTESIAN_POINT('Ctrl Pts',(0.726557820517936,1.3000000000005,2.61305934494899));
#46931=CARTESIAN_POINT('Ctrl Pts',(0.928513761894011,-1.30000000000348,
2.66427335298741));
#46932=CARTESIAN_POINT('Ctrl Pts',(0.90608019642325,-1.18514270861414,2.73763274798547));
#46933=CARTESIAN_POINT('Ctrl Pts',(0.883520193103324,-1.06847604194631,
2.80061671768325));
#46934=CARTESIAN_POINT('Ctrl Pts',(0.831109975596004,-0.794772684000851,
2.92215297954406));
#46935=CARTESIAN_POINT('Ctrl Pts',(0.794162608436584,-0.636309800095197,
2.9730779634235));
#46936=CARTESIAN_POINT('Ctrl Pts',(0.748684445248217,-0.31943490727716,
3.03888165819878));
#46937=CARTESIAN_POINT('Ctrl Pts',(0.733032893716133,-0.158333333333333,
3.05616629395804));
#46938=CARTESIAN_POINT('Ctrl Pts',(0.712915773366991,0.158333333333335,
3.05250175010369));
#46939=CARTESIAN_POINT('Ctrl Pts',(0.710588786918305,0.319434907277168,
3.03197974048681));
#46940=CARTESIAN_POINT('Ctrl Pts',(0.710733686134875,0.636309800095207,
2.95784151921007));
#46941=CARTESIAN_POINT('Ctrl Pts',(0.721034800362429,0.794772684000843,
2.90187893722154));
#46942=CARTESIAN_POINT('Ctrl Pts',(0.726882715325336,1.06847604194528,2.77183338838692));
#46943=CARTESIAN_POINT('Ctrl Pts',(0.728687491821999,1.18514270861212,2.70509393505239));
#46944=CARTESIAN_POINT('Ctrl Pts',(0.729765699114486,1.30000000000051,2.62790692781138));
#46945=CARTESIAN_POINT('Ctrl Pts',(0.930286002589785,-1.30000000000348,
2.67890363858943));
#46946=CARTESIAN_POINT('Ctrl Pts',(0.907045931711774,-1.18514270861414,
2.75486940600399));
#46947=CARTESIAN_POINT('Ctrl Pts',(0.884058946872757,-1.06847604194631,
2.8197689238864));
#46948=CARTESIAN_POINT('Ctrl Pts',(0.831539092744121,-0.794772684000853,
2.94413454308327));
#46949=CARTESIAN_POINT('Ctrl Pts',(0.796025953341132,-0.636309800095196,
2.99465196005428));
#46950=CARTESIAN_POINT('Ctrl Pts',(0.751325518317324,-0.319434907277158,
3.0605719012789));
#46951=CARTESIAN_POINT('Ctrl Pts',(0.736156135148362,-0.158333333333332,
3.07698411601015));
#46952=CARTESIAN_POINT('Ctrl Pts',(0.715522674806847,0.158333333333334,
3.07328619511169));
#46953=CARTESIAN_POINT('Ctrl Pts',(0.711372020014341,0.319434907277167,
3.05352879382717));
#46954=CARTESIAN_POINT('Ctrl Pts',(0.711368235162324,0.636309800095206,
2.9793579595281));
#46955=CARTESIAN_POINT('Ctrl Pts',(0.723265628623222,0.794772684000839,
2.92412391234324));
#46956=CARTESIAN_POINT('Ctrl Pts',(0.729702122581364,1.06847604194528,2.79125656303106));
#46957=CARTESIAN_POINT('Ctrl Pts',(0.731596041924747,1.18514270861212,2.72253590444958));
#46958=CARTESIAN_POINT('Ctrl Pts',(0.732597760872638,1.30000000000051,2.64260793958341));
#46959=CARTESIAN_POINT('Ctrl Pts',(0.9317290646797,-1.30000000000348,2.69655002042453));
#46960=CARTESIAN_POINT('Ctrl Pts',(0.907290115516676,-1.18514270861414,
2.77603993473538));
#46961=CARTESIAN_POINT('Ctrl Pts',(0.883846376138303,-1.06847604194631,
2.84357938770473));
#46962=CARTESIAN_POINT('Ctrl Pts',(0.831985781964135,-0.794772684000852,
2.97200107890404));
#46963=CARTESIAN_POINT('Ctrl Pts',(0.799949875653835,-0.636309800095197,
3.022356802163));
#46964=CARTESIAN_POINT('Ctrl Pts',(0.757395319589324,-0.319434907277159,
3.08868693309944));
#46965=CARTESIAN_POINT('Ctrl Pts',(0.742746847031083,-0.158333333333332,
3.10388657941746));
#46966=CARTESIAN_POINT('Ctrl Pts',(0.722185979795504,0.158333333333334,
3.10021804189515));
#46967=CARTESIAN_POINT('Ctrl Pts',(0.717232947701702,0.319434907277167,
3.08168140192397));
#46968=CARTESIAN_POINT('Ctrl Pts',(0.715952345132643,0.636309800095206,
3.00720339320853));
#46969=CARTESIAN_POINT('Ctrl Pts',(0.726294270879949,0.794772684000839,
2.95232337348871));
#46970=CARTESIAN_POINT('Ctrl Pts',(0.732256870087518,1.06847604194528,2.81536627845052));
#46971=CARTESIAN_POINT('Ctrl Pts',(0.734269534690587,1.18514270861212,2.74393616160032));
#46972=CARTESIAN_POINT('Ctrl Pts',(0.735713875635842,1.30000000000051,2.66035957958145));
#46973=CARTESIAN_POINT('Ctrl Pts',(0.932811379691018,-1.30000000000348,
2.70856623744797));
#46974=CARTESIAN_POINT('Ctrl Pts',(0.906248352880216,-1.18514270861414,
2.79031303912099));
#46975=CARTESIAN_POINT('Ctrl Pts',(0.882011643626692,-1.06847604194631,
2.85950209300221));
#46976=CARTESIAN_POINT('Ctrl Pts',(0.8313942556498,-0.794772684000851,2.99033173912196));
#46977=CARTESIAN_POINT('Ctrl Pts',(0.805863671216798,-0.636309800095197,
3.04032716132039));
#46978=CARTESIAN_POINT('Ctrl Pts',(0.76676614190522,-0.319434907277159,
3.10658683790933));
#46979=CARTESIAN_POINT('Ctrl Pts',(0.751993950076098,-0.158333333333332,
3.12072515293865));
#46980=CARTESIAN_POINT('Ctrl Pts',(0.731604230888438,0.158333333333334,
3.11703748018433));
#46981=CARTESIAN_POINT('Ctrl Pts',(0.72682424539096,0.319434907277167,3.0994670379522));
#46982=CARTESIAN_POINT('Ctrl Pts',(0.722683372359811,0.636309800095206,
3.02517530959544));
#46983=CARTESIAN_POINT('Ctrl Pts',(0.727550431506878,0.79477268400084,2.9710284197423));
#46984=CARTESIAN_POINT('Ctrl Pts',(0.732217053984722,1.06847604194528,2.83164616354321));
#46985=CARTESIAN_POINT('Ctrl Pts',(0.734729140509333,1.18514270861212,2.75847136298333));
#46986=CARTESIAN_POINT('Ctrl Pts',(0.7377333056033,1.30000000000051,2.67245517595061));
#46987=CARTESIAN_POINT('Ctrl Pts',(0.936125406440882,-1.30000000000348,
2.71650429949854));
#46988=CARTESIAN_POINT('Ctrl Pts',(0.909492919286885,-1.18514270861414,
2.79800958197354));
#46989=CARTESIAN_POINT('Ctrl Pts',(0.88553280170208,-1.06847604194631,2.86699266749395));
#46990=CARTESIAN_POINT('Ctrl Pts',(0.836353845186883,-0.794772684000851,
2.99742861504232));
#46991=CARTESIAN_POINT('Ctrl Pts',(0.813383183475108,-0.636309800095197,
3.04725124007732));
#46992=CARTESIAN_POINT('Ctrl Pts',(0.77596280188267,-0.319434907277159,
3.11333278083123));
#46993=CARTESIAN_POINT('Ctrl Pts',(0.761169784372622,-0.158333333333332,
3.12751912120358));
#46994=CARTESIAN_POINT('Ctrl Pts',(0.74101228662764,0.158333333333334,3.12378496929258));
#46995=CARTESIAN_POINT('Ctrl Pts',(0.736764158587383,0.319434907277167,
3.10609354911359));
#46996=CARTESIAN_POINT('Ctrl Pts',(0.730851239620766,0.636309800095206,
3.03193920640198));
#46997=CARTESIAN_POINT('Ctrl Pts',(0.732075357025827,0.79477268400084,2.97800571764298));
#46998=CARTESIAN_POINT('Ctrl Pts',(0.735457044102352,1.06847604194528,2.83902298122212));
#46999=CARTESIAN_POINT('Ctrl Pts',(0.738012470505655,1.18514270861212,2.76605409464577));
#47000=CARTESIAN_POINT('Ctrl Pts',(0.741659516280687,1.30000000000051,2.68027679827178));
#47001=CARTESIAN_POINT('Ctrl Pts',(0.936125406440075,-1.3,2.71650429950101));
#47002=CARTESIAN_POINT('Ctrl Pts',(0.909492919286401,-1.18514270861178,
2.79800958197493));
#47003=CARTESIAN_POINT('Ctrl Pts',(0.885532801701865,-1.06847604194512,
2.86699266749452));
#47004=CARTESIAN_POINT('Ctrl Pts',(0.836353845186883,-0.794772684000851,
2.99742861504232));
#47005=CARTESIAN_POINT('Ctrl Pts',(0.813383183475108,-0.636309800095197,
3.04725124007732));
#47006=CARTESIAN_POINT('Ctrl Pts',(0.77596280188267,-0.319434907277159,
3.11333278083123));
#47007=CARTESIAN_POINT('Ctrl Pts',(0.761169784372621,-0.158333333333332,
3.12751912120358));
#47008=CARTESIAN_POINT('Ctrl Pts',(0.74101228662764,0.158333333333334,3.12378496929258));
#47009=CARTESIAN_POINT('Ctrl Pts',(0.736764158587383,0.319434907277167,
3.10609354911359));
#47010=CARTESIAN_POINT('Ctrl Pts',(0.730851239620766,0.636309800095206,
3.03193920640198));
#47011=CARTESIAN_POINT('Ctrl Pts',(0.732075357025827,0.79477268400084,2.97800571764298));
#47012=CARTESIAN_POINT('Ctrl Pts',(0.73545704410235,1.06847604194511,2.8390229812222));
#47013=CARTESIAN_POINT('Ctrl Pts',(0.738012470505647,1.18514270861178,2.76605409464598));
#47014=CARTESIAN_POINT('Ctrl Pts',(0.74165951628067,1.3,2.68027679827216));
#47015=CARTESIAN_POINT('',(0.819062040271282,-1.2,2.31823419506971));
#47016=CARTESIAN_POINT('Ctrl Pts',(0.819062040271282,-1.2,2.31823419506971));
#47017=CARTESIAN_POINT('Ctrl Pts',(0.826817460709897,-1.21221394250375,
2.33192005968323));
#47018=CARTESIAN_POINT('Ctrl Pts',(0.839321576150835,-1.2301813580624,2.35228839172571));
#47019=CARTESIAN_POINT('Ctrl Pts',(0.860218448319171,-1.26364575297284,
2.38993774624693));
#47020=CARTESIAN_POINT('Ctrl Pts',(0.87185017021258,-1.2816915450181,2.41037451072659));
#47021=CARTESIAN_POINT('Ctrl Pts',(0.882693729841481,-1.30000000000349,
2.43100096673687));
#47022=CARTESIAN_POINT('',(0.664237964398142,-0.653834841336346,2.29476932996546));
#47023=CARTESIAN_POINT('Ctrl Pts',(0.664237964461389,-0.653834841321562,
2.29476932993277));
#47024=CARTESIAN_POINT('Ctrl Pts',(0.680825402116955,-0.719831522668225,
2.29701550479488));
#47025=CARTESIAN_POINT('Ctrl Pts',(0.694147737514797,-0.767178700652001,
2.2988870429438));
#47026=CARTESIAN_POINT('Ctrl Pts',(0.744612933014617,-0.949587838682991,
2.30619873464169));
#47027=CARTESIAN_POINT('Ctrl Pts',(0.774822021425007,-1.05662877212074,
2.31081161038503));
#47028=CARTESIAN_POINT('Ctrl Pts',(0.819062040271282,-1.2,2.31823419506971));
#47029=CARTESIAN_POINT('',(0.525742999964552,0.653834841531101,2.27799895388184));
#47030=CARTESIAN_POINT('Ctrl Pts',(0.525742999964552,0.6538348415311,2.27799895388184));
#47031=CARTESIAN_POINT('Ctrl Pts',(0.539185395144359,0.575762922599882,
2.31746185242062));
#47032=CARTESIAN_POINT('Ctrl Pts',(0.551466169169658,0.4937141636101,2.35040598822811));
#47033=CARTESIAN_POINT('Ctrl Pts',(0.571107869262371,0.337918064895967,
2.39711660814527));
#47034=CARTESIAN_POINT('Ctrl Pts',(0.579212684940256,0.265429240963003,
2.41309282046306));
#47035=CARTESIAN_POINT('Ctrl Pts',(0.593808443755668,0.129513007362985,
2.43255632813054));
#47036=CARTESIAN_POINT('Ctrl Pts',(0.600326349577118,0.0665349388579791,
2.43753385439801));
#47037=CARTESIAN_POINT('Ctrl Pts',(0.613439021868735,-0.0594336898450758,
2.4394973403484));
#47038=CARTESIAN_POINT('Ctrl Pts',(0.620111209962176,-0.122553013099034,
2.43651084370931));
#47039=CARTESIAN_POINT('Ctrl Pts',(0.633872071790792,-0.259894286834156,
2.42107710019218));
#47040=CARTESIAN_POINT('Ctrl Pts',(0.64081030202418,-0.333782902442558,
2.40697833921996));
#47041=CARTESIAN_POINT('Ctrl Pts',(0.653754957792595,-0.491517546675328,
2.36393127566722));
#47042=CARTESIAN_POINT('Ctrl Pts',(0.65977017879487,-0.574921333471004,
2.33273270890711));
#47043=CARTESIAN_POINT('Ctrl Pts',(0.664237964504258,-0.653834841358084,
2.29476933002314));
#47044=CARTESIAN_POINT('',(0.59761333344196,1.2,2.28620734018087));
#47045=CARTESIAN_POINT('Ctrl Pts',(0.597613333441959,1.2,2.28620734018087));
#47046=CARTESIAN_POINT('Ctrl Pts',(0.578803584943033,1.09907813786244,2.28391970672137));
#47047=CARTESIAN_POINT('Ctrl Pts',(0.563616863067985,0.997456289320577,
2.28217371941591));
#47048=CARTESIAN_POINT('Ctrl Pts',(0.53349441673388,0.766998566051729,2.27880400694723));
#47049=CARTESIAN_POINT('Ctrl Pts',(0.529155746207933,0.699729784093127,
2.27836348599618));
#47050=CARTESIAN_POINT('Ctrl Pts',(0.525742999964552,0.653834841531101,
2.27799895388184));
#47051=CARTESIAN_POINT('Ctrl Pts',(0.659051978146154,1.3,2.39498694173454));
#47052=CARTESIAN_POINT('Ctrl Pts',(0.649466552315287,1.28312826533509,2.37664251562972));
#47053=CARTESIAN_POINT('Ctrl Pts',(0.639075664739576,1.26651241391695,2.35849331479684));
#47054=CARTESIAN_POINT('Ctrl Pts',(0.622309019792689,1.23888116128521,2.32846173095479));
#47055=CARTESIAN_POINT('Ctrl Pts',(0.620849725903724,1.23596041607477,2.325331181624));
#47056=CARTESIAN_POINT('Ctrl Pts',(0.608663819665247,1.21698970713212,2.30467956529489));
#47057=CARTESIAN_POINT('Ctrl Pts',(0.603301253934286,1.20843659167084,2.29539785940356));
#47058=CARTESIAN_POINT('Ctrl Pts',(0.597613333441959,1.2,2.28620734018087));
#47059=CARTESIAN_POINT('Ctrl Pts',(0.936125406440075,-1.3,2.71650429950101));
#47060=CARTESIAN_POINT('Ctrl Pts',(0.909492919286401,-1.18514270861178,
2.79800958197493));
#47061=CARTESIAN_POINT('Ctrl Pts',(0.885532801701865,-1.06847604194512,
2.86699266749452));
#47062=CARTESIAN_POINT('Ctrl Pts',(0.836353845186883,-0.794772684000851,
2.99742861504232));
#47063=CARTESIAN_POINT('Ctrl Pts',(0.813383183475108,-0.636309800095197,
3.04725124007732));
#47064=CARTESIAN_POINT('Ctrl Pts',(0.77596280188267,-0.319434907277159,
3.11333278083123));
#47065=CARTESIAN_POINT('Ctrl Pts',(0.761169784372622,-0.158333333333332,
3.12751912120358));
#47066=CARTESIAN_POINT('Ctrl Pts',(0.74101228662764,0.158333333333335,3.12378496929258));
#47067=CARTESIAN_POINT('Ctrl Pts',(0.736764158587383,0.319434907277167,
3.10609354911359));
#47068=CARTESIAN_POINT('Ctrl Pts',(0.730851239620766,0.636309800095206,
3.03193920640198));
#47069=CARTESIAN_POINT('Ctrl Pts',(0.732075357025826,0.79477268400084,2.97800571764298));
#47070=CARTESIAN_POINT('Ctrl Pts',(0.73545704410235,1.06847604194511,2.83902298122221));
#47071=CARTESIAN_POINT('Ctrl Pts',(0.738012470505647,1.18514270861178,2.76605409464599));
#47072=CARTESIAN_POINT('Ctrl Pts',(0.74165951628067,1.3,2.68027679827216));
#47073=CARTESIAN_POINT('Ctrl Pts',(1.01101605778904,-1.3,2.73412529876815));
#47074=CARTESIAN_POINT('Ctrl Pts',(0.982742057194053,-1.18514270861178,
2.81507710262639));
#47075=CARTESIAN_POINT('Ctrl Pts',(0.95765377154039,-1.06847604194512,2.88363241978539));
#47076=CARTESIAN_POINT('Ctrl Pts',(0.90705445160062,-0.794772684000851,
3.01337055268305));
#47077=CARTESIAN_POINT('Ctrl Pts',(0.884801197368707,-0.636309800095197,
3.06317516506461));
#47078=CARTESIAN_POINT('Ctrl Pts',(0.847999940077956,-0.319434907277159,
3.12900897961302));
#47079=CARTESIAN_POINT('Ctrl Pts',(0.834445726094755,-0.158333333333332,
3.14327788892968));
#47080=CARTESIAN_POINT('Ctrl Pts',(0.814362858626306,0.158333333333335,
3.13919262917263));
#47081=CARTESIAN_POINT('Ctrl Pts',(0.808949443435951,0.319434907277167,
3.12107277268973));
#47082=CARTESIAN_POINT('Ctrl Pts',(0.802571685601039,0.636309800095206,
3.04644030028823));
#47083=CARTESIAN_POINT('Ctrl Pts',(0.803147745067787,0.79477268400084,2.99219856024142));
#47084=CARTESIAN_POINT('Ctrl Pts',(0.808110825487516,1.06847604194511,2.85315605226807));
#47085=CARTESIAN_POINT('Ctrl Pts',(0.811870873772817,1.18514270861178,2.78025524714239));
#47086=CARTESIAN_POINT('Ctrl Pts',(0.817242636729975,1.3,2.69463998655998));
#47087=CARTESIAN_POINT('Ctrl Pts',(1.08590670913801,-1.3,2.7517462980353));
#47088=CARTESIAN_POINT('Ctrl Pts',(1.05599119510171,-1.18514270861178,2.83214462327784));
#47089=CARTESIAN_POINT('Ctrl Pts',(1.02977474137891,-1.06847604194512,2.90027217207626));
#47090=CARTESIAN_POINT('Ctrl Pts',(0.977755058014356,-0.794772684000851,
3.02931249032378));
#47091=CARTESIAN_POINT('Ctrl Pts',(0.956219211262305,-0.636309800095197,
3.07909909005189));
#47092=CARTESIAN_POINT('Ctrl Pts',(0.920037078273242,-0.319434907277159,
3.1446851783948));
#47093=CARTESIAN_POINT('Ctrl Pts',(0.907721667816889,-0.158333333333332,
3.15903665665579));
#47094=CARTESIAN_POINT('Ctrl Pts',(0.887713430624972,0.158333333333335,
3.15460028905268));
#47095=CARTESIAN_POINT('Ctrl Pts',(0.881134728284519,0.319434907277167,
3.13605199626586));
#47096=CARTESIAN_POINT('Ctrl Pts',(0.874292131581311,0.636309800095206,
3.06094139417447));
#47097=CARTESIAN_POINT('Ctrl Pts',(0.874220133109747,0.79477268400084,3.00639140283986));
#47098=CARTESIAN_POINT('Ctrl Pts',(0.880764606872681,1.06847604194511,2.86728912331394));
#47099=CARTESIAN_POINT('Ctrl Pts',(0.885729277039987,1.18514270861178,2.79445639963879));
#47100=CARTESIAN_POINT('Ctrl Pts',(0.892825757179279,1.3,2.70900317484779));
#47101=CARTESIAN_POINT('Ctrl Pts',(1.16079736048698,-1.3,2.76936729730244));
#47102=CARTESIAN_POINT('Ctrl Pts',(1.12924033300936,-1.18514270861178,2.84921214392929));
#47103=CARTESIAN_POINT('Ctrl Pts',(1.10189571121744,-1.06847604194512,2.91691192436713));
#47104=CARTESIAN_POINT('Ctrl Pts',(1.04845566442809,-0.794772684000851,
3.04525442796451));
#47105=CARTESIAN_POINT('Ctrl Pts',(1.0276372251559,-0.636309800095197,3.09502301503918));
#47106=CARTESIAN_POINT('Ctrl Pts',(0.992074216468528,-0.319434907277159,
3.16036137717659));
#47107=CARTESIAN_POINT('Ctrl Pts',(0.980997609539022,-0.158333333333332,
3.17479542438189));
#47108=CARTESIAN_POINT('Ctrl Pts',(0.961064002623638,0.158333333333335,
3.17000794893274));
#47109=CARTESIAN_POINT('Ctrl Pts',(0.953320013133087,0.319434907277167,
3.151031219842));
#47110=CARTESIAN_POINT('Ctrl Pts',(0.946012577561583,0.636309800095206,
3.07544248806072));
#47111=CARTESIAN_POINT('Ctrl Pts',(0.945292521151707,0.79477268400084,3.02058424543829));
#47112=CARTESIAN_POINT('Ctrl Pts',(0.953418388257846,1.06847604194511,2.88142219435981));
#47113=CARTESIAN_POINT('Ctrl Pts',(0.959587680307157,1.18514270861178,2.80865755213519));
#47114=CARTESIAN_POINT('Ctrl Pts',(0.968408877628583,1.3,2.72336636313561));
#47115=CARTESIAN_POINT('Ctrl Pts',(1.16079736048698,-1.3,2.76936729730244));
#47116=CARTESIAN_POINT('Ctrl Pts',(1.12924033300936,-1.18514270861178,2.84921214392929));
#47117=CARTESIAN_POINT('Ctrl Pts',(1.10189571121744,-1.06847604194512,2.91691192436713));
#47118=CARTESIAN_POINT('Ctrl Pts',(1.04845566442809,-0.794772684000851,
3.0452544279645));
#47119=CARTESIAN_POINT('Ctrl Pts',(1.0276372251559,-0.636309800095197,3.09502301503918));
#47120=CARTESIAN_POINT('Ctrl Pts',(0.992074216468527,-0.319434907277159,
3.16036137717659));
#47121=CARTESIAN_POINT('Ctrl Pts',(0.980997609539022,-0.158333333333332,
3.17479542438189));
#47122=CARTESIAN_POINT('Ctrl Pts',(0.961064002623638,0.158333333333334,
3.17000794893273));
#47123=CARTESIAN_POINT('Ctrl Pts',(0.953320013133086,0.319434907277167,
3.151031219842));
#47124=CARTESIAN_POINT('Ctrl Pts',(0.946012577561583,0.636309800095206,
3.07544248806072));
#47125=CARTESIAN_POINT('Ctrl Pts',(0.945292521151707,0.79477268400084,3.02058424543829));
#47126=CARTESIAN_POINT('Ctrl Pts',(0.953418388257846,1.06847604194511,2.88142219435981));
#47127=CARTESIAN_POINT('Ctrl Pts',(0.959587680307157,1.18514270861178,2.80865755213519));
#47128=CARTESIAN_POINT('Ctrl Pts',(0.968408877628583,1.3,2.72336636313561));
#47129=CARTESIAN_POINT('Ctrl Pts',(1.16079736048841,-1.30000000000522,2.76936729729881));
#47130=CARTESIAN_POINT('Ctrl Pts',(1.12924033301019,-1.18514270861532,2.84921214392724));
#47131=CARTESIAN_POINT('Ctrl Pts',(1.10189571121779,-1.06847604194691,2.91691192436629));
#47132=CARTESIAN_POINT('Ctrl Pts',(1.04845566442809,-0.794772684000851,
3.04525442796451));
#47133=CARTESIAN_POINT('Ctrl Pts',(1.0276372251559,-0.636309800095197,3.09502301503918));
#47134=CARTESIAN_POINT('Ctrl Pts',(0.992074216468527,-0.319434907277159,
3.16036137717659));
#47135=CARTESIAN_POINT('Ctrl Pts',(0.980997609539023,-0.158333333333332,
3.17479542438189));
#47136=CARTESIAN_POINT('Ctrl Pts',(0.961064002623638,0.158333333333334,
3.17000794893273));
#47137=CARTESIAN_POINT('Ctrl Pts',(0.953320013133086,0.319434907277167,
3.151031219842));
#47138=CARTESIAN_POINT('Ctrl Pts',(0.946012577561583,0.636309800095206,
3.07544248806072));
#47139=CARTESIAN_POINT('Ctrl Pts',(0.945292521151708,0.79477268400084,3.02058424543829));
#47140=CARTESIAN_POINT('Ctrl Pts',(0.953418388257849,1.06847604194517,2.88142219435978));
#47141=CARTESIAN_POINT('Ctrl Pts',(0.959587680307164,1.1851427086119,2.80865755213511));
#47142=CARTESIAN_POINT('Ctrl Pts',(0.968408877628597,1.30000000000018,2.72336636313548));
#47143=CARTESIAN_POINT('Ctrl Pts',(1.16756547281118,-1.30000000000522,2.76381882356482));
#47144=CARTESIAN_POINT('Ctrl Pts',(1.13532397902447,-1.18514270861532,2.84362042453195));
#47145=CARTESIAN_POINT('Ctrl Pts',(1.10785601152185,-1.06847604194691,2.91149068883335));
#47146=CARTESIAN_POINT('Ctrl Pts',(1.05542731230007,-0.794772684000851,
3.04072080221479));
#47147=CARTESIAN_POINT('Ctrl Pts',(1.03785006786609,-0.636309800095197,
3.09216605877564));
#47148=CARTESIAN_POINT('Ctrl Pts',(1.00385002391232,-0.319434907277159,
3.15835068498378));
#47149=CARTESIAN_POINT('Ctrl Pts',(0.992336747169056,-0.158333333333332,
3.17245788747789));
#47150=CARTESIAN_POINT('Ctrl Pts',(0.972209900186261,0.158333333333334,
3.16753349823253));
#47151=CARTESIAN_POINT('Ctrl Pts',(0.964465402249313,0.319434907277167,
3.14860911297925));
#47152=CARTESIAN_POINT('Ctrl Pts',(0.955698270375131,0.636309800095206,
3.07217548855289));
#47153=CARTESIAN_POINT('Ctrl Pts',(0.952709891127438,0.79477268400084,3.01611817350183));
#47154=CARTESIAN_POINT('Ctrl Pts',(0.959681817340558,1.06847604194517,2.87601139810055));
#47155=CARTESIAN_POINT('Ctrl Pts',(0.965682205206479,1.1851427086119,2.80294609445152));
#47156=CARTESIAN_POINT('Ctrl Pts',(0.974665092415987,1.30000000000018,2.717462518757));
#47157=CARTESIAN_POINT('Ctrl Pts',(1.17429750653259,-1.30000000000522,2.75357268161649));
#47158=CARTESIAN_POINT('Ctrl Pts',(1.14162650151079,-1.18514270861532,2.8305066317218));
#47159=CARTESIAN_POINT('Ctrl Pts',(1.11441651150372,-1.06847604194691,2.89657751787525));
#47160=CARTESIAN_POINT('Ctrl Pts',(1.0641720284043,-0.794772684000852,3.02411863144687));
#47161=CARTESIAN_POINT('Ctrl Pts',(1.05131458055589,-0.636309800095196,
3.07846805658878));
#47162=CARTESIAN_POINT('Ctrl Pts',(1.0198646696171,-0.319434907277158,3.14599143412024));
#47163=CARTESIAN_POINT('Ctrl Pts',(1.00780392282228,-0.158333333333332,
3.16091515929002));
#47164=CARTESIAN_POINT('Ctrl Pts',(0.987525874605585,0.158333333333335,
3.15590178731436));
#47165=CARTESIAN_POINT('Ctrl Pts',(0.980318225717366,0.319434907277168,
3.13605041188448));
#47166=CARTESIAN_POINT('Ctrl Pts',(0.968406622993036,0.636309800095207,
3.0581405476509));
#47167=CARTESIAN_POINT('Ctrl Pts',(0.959600753467649,0.794772684000839,
2.99910157701068));
#47168=CARTESIAN_POINT('Ctrl Pts',(0.964457436413564,1.06847604194517,2.86069580646051));
#47169=CARTESIAN_POINT('Ctrl Pts',(0.970516793992365,1.18514270861189,2.78946635876449));
#47170=CARTESIAN_POINT('Ctrl Pts',(0.980533231060517,1.30000000000018,2.70691819300439));
#47171=CARTESIAN_POINT('Ctrl Pts',(1.18440293491058,-1.30000000000522,2.73864158445463));
#47172=CARTESIAN_POINT('Ctrl Pts',(1.15281893584074,-1.18514270861532,2.8120698416044));
#47173=CARTESIAN_POINT('Ctrl Pts',(1.12660451412146,-1.06847604194691,2.87562143340008));
#47174=CARTESIAN_POINT('Ctrl Pts',(1.07844875363333,-0.794772684000853,
2.99962125111139));
#47175=CARTESIAN_POINT('Ctrl Pts',(1.06684517117874,-0.636309800095195,
3.05491694960946));
#47176=CARTESIAN_POINT('Ctrl Pts',(1.03666116289866,-0.319434907277157,
3.12266967613995));
#47177=CARTESIAN_POINT('Ctrl Pts',(1.02482746060559,-0.158333333333332,
3.13902915190023));
#47178=CARTESIAN_POINT('Ctrl Pts',(1.00444286620191,0.158333333333334,3.13400464966217));
#47179=CARTESIAN_POINT('Ctrl Pts',(0.997213961942221,0.319434907277168,
3.11282604408903));
#47180=CARTESIAN_POINT('Ctrl Pts',(0.983183225095408,0.636309800095206,
3.03442043943294));
#47181=CARTESIAN_POINT('Ctrl Pts',(0.97133893520286,0.794772684000838,2.97384041811216));
#47182=CARTESIAN_POINT('Ctrl Pts',(0.973945325811959,1.06847604194517,2.83886592421529));
#47183=CARTESIAN_POINT('Ctrl Pts',(0.979334457355884,1.18514270861189,2.77022574197491));
#47184=CARTESIAN_POINT('Ctrl Pts',(0.988984510525345,1.30000000000018,2.69137083460419));
#47185=CARTESIAN_POINT('Ctrl Pts',(1.19282025714432,-1.30000000000522,2.72628875413115));
#47186=CARTESIAN_POINT('Ctrl Pts',(1.16240804411813,-1.18514270861532,2.79721826438278));
#47187=CARTESIAN_POINT('Ctrl Pts',(1.13692060833745,-1.06847604194691,2.85890943556789));
#47188=CARTESIAN_POINT('Ctrl Pts',(1.08941675357591,-0.794772684000851,
2.98008597091395));
#47189=CARTESIAN_POINT('Ctrl Pts',(1.0761430165978,-0.636309800095196,3.03543477422358));
#47190=CARTESIAN_POINT('Ctrl Pts',(1.04619263381479,-0.319434907277158,
3.10325000382581));
#47191=CARTESIAN_POINT('Ctrl Pts',(1.03574336889857,-0.158333333333332,
3.12107111876852));
#47192=CARTESIAN_POINT('Ctrl Pts',(1.0159100403865,0.158333333333334,3.11624401321292));
#47193=CARTESIAN_POINT('Ctrl Pts',(1.00867847609951,0.319434907277168,3.09407856463005));
#47194=CARTESIAN_POINT('Ctrl Pts',(0.993845310643403,0.636309800095207,
3.01544749694316));
#47195=CARTESIAN_POINT('Ctrl Pts',(0.980641741294821,0.794772684000839,
2.95384890499302));
#47196=CARTESIAN_POINT('Ctrl Pts',(0.982193099836836,1.06847604194517,2.82152975406996));
#47197=CARTESIAN_POINT('Ctrl Pts',(0.987236437588956,1.18514270861189,2.7548438908858));
#47198=CARTESIAN_POINT('Ctrl Pts',(0.996651587463857,1.30000000000018,2.67874822204431));
#47199=CARTESIAN_POINT('Ctrl Pts',(1.20387629867497,-1.30000000000522,2.71172082726954));
#47200=CARTESIAN_POINT('Ctrl Pts',(1.17507593415048,-1.18514270861532,2.77943672157987));
#47201=CARTESIAN_POINT('Ctrl Pts',(1.15053427987609,-1.06847604194691,2.83869134085797));
#47202=CARTESIAN_POINT('Ctrl Pts',(1.10367662159133,-0.794772684000853,
2.95603412723863));
#47203=CARTESIAN_POINT('Ctrl Pts',(1.08806112252454,-0.636309800095197,
3.01122675713547));
#47204=CARTESIAN_POINT('Ctrl Pts',(1.05741252960008,-0.319434907277159,
3.07866763728465));
#47205=CARTESIAN_POINT('Ctrl Pts',(1.0479864980603,-0.158333333333333,3.09808593381759));
#47206=CARTESIAN_POINT('Ctrl Pts',(1.02708751229622,0.158333333333335,3.09295520022724));
#47207=CARTESIAN_POINT('Ctrl Pts',(1.0171674141675,0.319434907277168,3.06873742908771));
#47208=CARTESIAN_POINT('Ctrl Pts',(1.00208322181011,0.636309800095208,2.99017086334158));
#47209=CARTESIAN_POINT('Ctrl Pts',(0.991947200773414,0.794772684000841,
2.92887248736516));
#47210=CARTESIAN_POINT('Ctrl Pts',(0.993279089156325,1.06847604194517,2.80043861029839));
#47211=CARTESIAN_POINT('Ctrl Pts',(0.997608246281604,1.1851427086119,2.73622560903023));
#47212=CARTESIAN_POINT('Ctrl Pts',(1.00569003540253,1.30000000000018,2.66339387293194));
#47213=CARTESIAN_POINT('Ctrl Pts',(1.22295971290336,-1.30000000000522,2.68787251266138));
#47214=CARTESIAN_POINT('Ctrl Pts',(1.19654332358173,-1.18514270861532,2.75037736984417));
#47215=CARTESIAN_POINT('Ctrl Pts',(1.17336384415623,-1.06847604194692,2.80568737756851));
#47216=CARTESIAN_POINT('Ctrl Pts',(1.12729251904644,-0.794772684000856,
2.91684301856624));
#47217=CARTESIAN_POINT('Ctrl Pts',(1.10872908000617,-0.6363098000952,2.97210999709675));
#47218=CARTESIAN_POINT('Ctrl Pts',(1.07528657029111,-0.319434907277161,
3.03843051421032));
#47219=CARTESIAN_POINT('Ctrl Pts',(1.06327501252726,-0.158333333333333,
3.05900814238434));
#47220=CARTESIAN_POINT('Ctrl Pts',(1.04142330771059,0.158333333333335,3.05362555883336));
#47221=CARTESIAN_POINT('Ctrl Pts',(1.03274202089434,0.319434907277169,3.02792543173402));
#47222=CARTESIAN_POINT('Ctrl Pts',(1.01931366641166,0.63630980009521,2.95011120583023));
#47223=CARTESIAN_POINT('Ctrl Pts',(1.01228085109468,0.794772684000845,2.88869625988921));
#47224=CARTESIAN_POINT('Ctrl Pts',(1.01275044424827,1.06847604194518,2.7662681088466));
#47225=CARTESIAN_POINT('Ctrl Pts',(1.01575016411372,1.1851427086119,2.70592580887601));
#47226=CARTESIAN_POINT('Ctrl Pts',(1.02154633436856,1.30000000000019,2.63823581911109));
#47227=CARTESIAN_POINT('Ctrl Pts',(1.24182813440133,-1.30000000000522,2.66390221260576));
#47228=CARTESIAN_POINT('Ctrl Pts',(1.218725159562,-1.18514270861532,2.72147669928059));
#47229=CARTESIAN_POINT('Ctrl Pts',(1.19758527856108,-1.06847604194691,2.77303231271835));
#47230=CARTESIAN_POINT('Ctrl Pts',(1.15328306391294,-0.794772684000849,
2.87823129217475));
#47231=CARTESIAN_POINT('Ctrl Pts',(1.13124218605865,-0.636309800095196,
2.93328961063753));
#47232=CARTESIAN_POINT('Ctrl Pts',(1.09568620149555,-0.319434907277159,
2.99864424003564));
#47233=CARTESIAN_POINT('Ctrl Pts',(1.08232555204351,-0.158333333333332,
3.02082353147524));
#47234=CARTESIAN_POINT('Ctrl Pts',(1.05962125523247,0.158333333333334,3.01518360825578));
#47235=CARTESIAN_POINT('Ctrl Pts',(1.05131103637489,0.319434907277167,2.98763078916219));
#47236=CARTESIAN_POINT('Ctrl Pts',(1.03851498364947,0.636309800095206,2.91024541366821));
#47237=CARTESIAN_POINT('Ctrl Pts',(1.03363914893915,0.794772684000838,2.84845345753121));
#47238=CARTESIAN_POINT('Ctrl Pts',(1.03272231259024,1.06847604194517,2.73201465841564));
#47239=CARTESIAN_POINT('Ctrl Pts',(1.0343351888939,1.1851427086119,2.67561491464539));
#47240=CARTESIAN_POINT('Ctrl Pts',(1.03795780598451,1.30000000000018,2.6132174687593));
#47241=CARTESIAN_POINT('Ctrl Pts',(1.26205481118799,-1.30000000000522,2.6405729968505));
#47242=CARTESIAN_POINT('Ctrl Pts',(1.24207905433544,-1.18514270861532,2.69320565243503));
#47243=CARTESIAN_POINT('Ctrl Pts',(1.22293655530526,-1.06847604194691,2.74102898310266));
#47244=CARTESIAN_POINT('Ctrl Pts',(1.18063854536445,-0.794772684000849,
2.84039994130838));
#47245=CARTESIAN_POINT('Ctrl Pts',(1.15634659093339,-0.636309800095197,
2.89566365798084));
#47246=CARTESIAN_POINT('Ctrl Pts',(1.11824845891302,-0.319434907277159,
2.959865286098));
#47247=CARTESIAN_POINT('Ctrl Pts',(1.10145016334698,-0.158333333333332,
2.98284476091643));
#47248=CARTESIAN_POINT('Ctrl Pts',(1.07788761365085,0.158333333333334,2.9769227689399));
#47249=CARTESIAN_POINT('Ctrl Pts',(1.07184303038958,0.319434907277167,2.94821599520184));
#47250=CARTESIAN_POINT('Ctrl Pts',(1.06048002749707,0.636309800095206,2.87155512008751));
#47251=CARTESIAN_POINT('Ctrl Pts',(1.05776628174413,0.794772684000839,2.80942552455464));
#47252=CARTESIAN_POINT('Ctrl Pts',(1.05479561954693,1.06847604194517,2.69868648796352));
#47253=CARTESIAN_POINT('Ctrl Pts',(1.05450561934856,1.1851427086119,2.64600329499075));
#47254=CARTESIAN_POINT('Ctrl Pts',(1.05521150854311,1.30000000000018,2.58857173469979));
#47255=CARTESIAN_POINT('Ctrl Pts',(1.2776175603506,-1.30000000000522,2.62164579396498));
#47256=CARTESIAN_POINT('Ctrl Pts',(1.25999481688344,-1.18514270861532,2.67023889873838));
#47257=CARTESIAN_POINT('Ctrl Pts',(1.24245454125395,-1.06847604194691,2.71506046278283));
#47258=CARTESIAN_POINT('Ctrl Pts',(1.20212351283273,-0.794772684000848,
2.80989422866985));
#47259=CARTESIAN_POINT('Ctrl Pts',(1.17673956294012,-0.636309800095195,
2.86564566881686));
#47260=CARTESIAN_POINT('Ctrl Pts',(1.13757402022123,-0.319434907277158,
2.92927823955686));
#47261=CARTESIAN_POINT('Ctrl Pts',(1.11908596269311,-0.158333333333332,
2.9532378566013));
#47262=CARTESIAN_POINT('Ctrl Pts',(1.09474153850865,0.158333333333334,2.94703959578193));
#47263=CARTESIAN_POINT('Ctrl Pts',(1.08928741242003,0.319434907277168,2.91697547995212));
#47264=CARTESIAN_POINT('Ctrl Pts',(1.07804578085774,0.636309800095207,2.84052651170049));
#47265=CARTESIAN_POINT('Ctrl Pts',(1.07646188707476,0.794772684000837,2.77790287505706));
#47266=CARTESIAN_POINT('Ctrl Pts',(1.07156457759862,1.06847604194517,2.67164506778811));
#47267=CARTESIAN_POINT('Ctrl Pts',(1.06978486191151,1.1851427086119,2.62196362218695));
#47268=CARTESIAN_POINT('Ctrl Pts',(1.0683452943463,1.30000000000018,2.56859579851158));
#47269=CARTESIAN_POINT('Ctrl Pts',(1.29897751391511,-1.30000000000523,2.59886823472693));
#47270=CARTESIAN_POINT('Ctrl Pts',(1.28556771443465,-1.18514270861533,2.6430095662816));
#47271=CARTESIAN_POINT('Ctrl Pts',(1.27070247446087,-1.06847604194692,2.68439718474942));
#47272=CARTESIAN_POINT('Ctrl Pts',(1.23299843764119,-0.79477268400086,2.77364923486504));
#47273=CARTESIAN_POINT('Ctrl Pts',(1.2038834720301,-0.636309800095201,2.82891455501619));
#47274=CARTESIAN_POINT('Ctrl Pts',(1.16234242040859,-0.31943490727716,2.89136182815192));
#47275=CARTESIAN_POINT('Ctrl Pts',(1.14182485146547,-0.158333333333333,
2.91660410511155));
#47276=CARTESIAN_POINT('Ctrl Pts',(1.11654454161528,0.158333333333335,2.91006068713333));
#47277=CARTESIAN_POINT('Ctrl Pts',(1.11201924982408,0.319434907277169,2.87835454662367));
#47278=CARTESIAN_POINT('Ctrl Pts',(1.10158246377129,0.63630980009521,2.80241675556593));
#47279=CARTESIAN_POINT('Ctrl Pts',(1.10242798139847,0.794772684000843,2.73959979850215));
#47280=CARTESIAN_POINT('Ctrl Pts',(1.09531632657767,1.06847604194518,2.63899234578077));
#47281=CARTESIAN_POINT('Ctrl Pts',(1.09153908597683,1.18514270861191,2.59298824503687));
#47282=CARTESIAN_POINT('Ctrl Pts',(1.08706297663432,1.30000000000019,2.54452928195864));
#47283=CARTESIAN_POINT('Ctrl Pts',(1.32380250697462,-1.30000000000523,2.57121941147693));
#47284=CARTESIAN_POINT('Ctrl Pts',(1.31451069985451,-1.18514270861532,2.60959592800393));
#47285=CARTESIAN_POINT('Ctrl Pts',(1.30247132551968,-1.06847604194691,2.64668422653664));
#47286=CARTESIAN_POINT('Ctrl Pts',(1.26831053242304,-0.794772684000854,
2.72938957436126));
#47287=CARTESIAN_POINT('Ctrl Pts',(1.23745046376972,-0.636309800095198,
2.78527587837556));
#47288=CARTESIAN_POINT('Ctrl Pts',(1.19416076340524,-0.319434907277159,
2.84674169288415));
#47289=CARTESIAN_POINT('Ctrl Pts',(1.17034498851464,-0.158333333333333,
2.87309146320457));
#47290=CARTESIAN_POINT('Ctrl Pts',(1.14442378353678,0.158333333333335,2.86629821921497));
#47291=CARTESIAN_POINT('Ctrl Pts',(1.14248695695105,0.31943490727717,2.83323019655854));
#47292=CARTESIAN_POINT('Ctrl Pts',(1.13263359597151,0.63630980009521,2.75777428057413));
#47293=CARTESIAN_POINT('Ctrl Pts',(1.13439789288439,0.794772684000841,2.69394937050413));
#47294=CARTESIAN_POINT('Ctrl Pts',(1.12349975140898,1.06847604194517,2.59970003508306));
#47295=CARTESIAN_POINT('Ctrl Pts',(1.11701341685411,1.1851427086119,2.55799661174547));
#47296=CARTESIAN_POINT('Ctrl Pts',(1.10875814937315,1.30000000000018,2.515386810092));
#47297=CARTESIAN_POINT('Ctrl Pts',(1.34353479425786,-1.30000000000523,2.55103104359542));
#47298=CARTESIAN_POINT('Ctrl Pts',(1.33804312545896,-1.18514270861533,2.58543063651654));
#47299=CARTESIAN_POINT('Ctrl Pts',(1.32849265660278,-1.06847604194692,2.61947456860717));
#47300=CARTESIAN_POINT('Ctrl Pts',(1.29705252288802,-0.794772684000856,
2.69730121453301));
#47301=CARTESIAN_POINT('Ctrl Pts',(1.26322137201649,-0.636309800095202,
2.75286490573782));
#47302=CARTESIAN_POINT('Ctrl Pts',(1.21856519239577,-0.319434907277162,
2.81352802858837));
#47303=CARTESIAN_POINT('Ctrl Pts',(1.19370551790263,-0.158333333333333,
2.84130728407494));
#47304=CARTESIAN_POINT('Ctrl Pts',(1.1672572311677,0.158333333333336,2.83430539053762));
#47305=CARTESIAN_POINT('Ctrl Pts',(1.16583639205031,0.319434907277169,2.79963733920804));
#47306=CARTESIAN_POINT('Ctrl Pts',(1.15627757415748,0.63630980009521,2.72448149151503));
#47307=CARTESIAN_POINT('Ctrl Pts',(1.16001923508657,0.794772684000848,2.66042492911123));
#47308=CARTESIAN_POINT('Ctrl Pts',(1.14623297406581,1.06847604194518,2.57091255294235));
#47309=CARTESIAN_POINT('Ctrl Pts',(1.13744728375627,1.1851427086119,2.53231823294277));
#47310=CARTESIAN_POINT('Ctrl Pts',(1.12584346470176,1.30000000000018,2.4938761838267));
#47311=CARTESIAN_POINT('Ctrl Pts',(1.35705527879887,-1.30000000000523,2.53776290116183));
#47312=CARTESIAN_POINT('Ctrl Pts',(1.35380115355581,-1.18514270861533,2.56938305660187));
#47313=CARTESIAN_POINT('Ctrl Pts',(1.34584081416615,-1.06847604194692,2.60136950328211));
#47314=CARTESIAN_POINT('Ctrl Pts',(1.31657854156224,-0.794772684000857,
2.6761108000208));
#47315=CARTESIAN_POINT('Ctrl Pts',(1.28246012884012,-0.636309800095202,
2.73221828163434));
#47316=CARTESIAN_POINT('Ctrl Pts',(1.2366713883074,-0.319434907277162,2.7922420731235));
#47317=CARTESIAN_POINT('Ctrl Pts',(1.20915115452519,-0.158333333333333,
2.82009033602051));
#47318=CARTESIAN_POINT('Ctrl Pts',(1.18189193316008,0.158333333333336,2.81272748580012));
#47319=CARTESIAN_POINT('Ctrl Pts',(1.18192670079688,0.319434907277169,2.77746487924114));
#47320=CARTESIAN_POINT('Ctrl Pts',(1.17265121446526,0.636309800095211,2.70254838042864));
#47321=CARTESIAN_POINT('Ctrl Pts',(1.17696692154763,0.794772684000848,2.63804206835142));
#47322=CARTESIAN_POINT('Ctrl Pts',(1.16121360887195,1.06847604194518,2.55166730436085));
#47323=CARTESIAN_POINT('Ctrl Pts',(1.15100373070832,1.1851427086119,2.51518588101529));
#47324=CARTESIAN_POINT('Ctrl Pts',(1.13740299972059,1.30000000000018,2.47961146915524));
#47325=CARTESIAN_POINT('Ctrl Pts',(1.36521872532696,-1.30000000000523,2.52851742886439));
#47326=CARTESIAN_POINT('Ctrl Pts',(1.36336594929023,-1.18514270861533,2.55823334895911));
#47327=CARTESIAN_POINT('Ctrl Pts',(1.35639680598846,-1.06847604194692,2.58881179127426));
#47328=CARTESIAN_POINT('Ctrl Pts',(1.32847685888128,-0.794772684000858,
2.66144670909424));
#47329=CARTESIAN_POINT('Ctrl Pts',(1.29382137562031,-0.636309800095202,
2.71778507964574));
#47330=CARTESIAN_POINT('Ctrl Pts',(1.24792930699923,-0.319434907277162,
2.77768202334506));
#47331=CARTESIAN_POINT('Ctrl Pts',(1.21991426953575,-0.158333333333334,
2.80614264216758));
#47332=CARTESIAN_POINT('Ctrl Pts',(1.1928290090653,0.158333333333336,2.79885835339839));
#47333=CARTESIAN_POINT('Ctrl Pts',(1.19381822041475,0.319434907277169,2.76319030999829));
#47334=CARTESIAN_POINT('Ctrl Pts',(1.18441850015633,0.636309800095211,2.68829922773841));
#47335=CARTESIAN_POINT('Ctrl Pts',(1.18823577795932,0.794772684000848,2.62311338878884));
#47336=CARTESIAN_POINT('Ctrl Pts',(1.17093262167389,1.06847604194518,2.53872392163905));
#47337=CARTESIAN_POINT('Ctrl Pts',(1.15981958146128,1.1851427086119,2.50366856483175));
#47338=CARTESIAN_POINT('Ctrl Pts',(1.1450833962469,1.30000000000018,2.47008692460837));
#47339=CARTESIAN_POINT('Ctrl Pts',(1.38122654843761,-1.30000000000523,2.51318553227769));
#47340=CARTESIAN_POINT('Ctrl Pts',(1.38278099200282,-1.18514270861533,2.54005217521767));
#47341=CARTESIAN_POINT('Ctrl Pts',(1.37809806873369,-1.06847604194692,2.56844338335525));
#47342=CARTESIAN_POINT('Ctrl Pts',(1.35287001399835,-0.794772684000859,
2.63755480438889));
#47343=CARTESIAN_POINT('Ctrl Pts',(1.31627260802992,-0.636309800095202,
2.69375117495694));
#47344=CARTESIAN_POINT('Ctrl Pts',(1.26885276023804,-0.319434907277161,
2.75277362407299));
#47345=CARTESIAN_POINT('Ctrl Pts',(1.23884504163408,-0.158333333333334,
2.7817914624677));
#47346=CARTESIAN_POINT('Ctrl Pts',(1.21062406304607,0.158333333333336,2.77400047963829));
#47347=CARTESIAN_POINT('Ctrl Pts',(1.21188528420357,0.319434907277169,2.73703651047564));
#47348=CARTESIAN_POINT('Ctrl Pts',(1.20289147466563,0.636309800095211,2.6624604154852));
#47349=CARTESIAN_POINT('Ctrl Pts',(1.20908308624123,0.794772684000847,2.59748057087056));
#47350=CARTESIAN_POINT('Ctrl Pts',(1.18963859489542,1.06847604194518,2.51681692708733));
#47351=CARTESIAN_POINT('Ctrl Pts',(1.17662584357406,1.1851427086119,2.48412382801717));
#47352=CARTESIAN_POINT('Ctrl Pts',(1.15901714074552,1.30000000000018,2.45365393238805));
#47353=CARTESIAN_POINT('Ctrl Pts',(1.39929231839369,-1.30000000000524,2.49557601088206));
#47354=CARTESIAN_POINT('Ctrl Pts',(1.4043825297588,-1.18514270861533,2.51902603264737));
#47355=CARTESIAN_POINT('Ctrl Pts',(1.40209251391536,-1.06847604194692,2.54482000595124));
#47356=CARTESIAN_POINT('Ctrl Pts',(1.37975231793992,-0.794772684000858,
2.60982424130932));
#47357=CARTESIAN_POINT('Ctrl Pts',(1.34090487750289,-0.636309800095206,
2.66585079183438));
#47358=CARTESIAN_POINT('Ctrl Pts',(1.29277799309058,-0.319434907277165,
2.72434458679463));
#47359=CARTESIAN_POINT('Ctrl Pts',(1.26193437457079,-0.158333333333334,
2.75465054837699));
#47360=CARTESIAN_POINT('Ctrl Pts',(1.2337965541703,0.158333333333336,2.74689265505336));
#47361=CARTESIAN_POINT('Ctrl Pts',(1.23645399959435,0.319434907277168,2.70891052034103));
#47362=CARTESIAN_POINT('Ctrl Pts',(1.22736466079988,0.636309800095212,2.63444799711698));
#47363=CARTESIAN_POINT('Ctrl Pts',(1.23374892176809,0.794772684000854,2.56861469097783));
#47364=CARTESIAN_POINT('Ctrl Pts',(1.21088952787038,1.06847604194519,2.49177015120832));
#47365=CARTESIAN_POINT('Ctrl Pts',(1.19561848422943,1.18514270861191,2.46172586752891));
#47366=CARTESIAN_POINT('Ctrl Pts',(1.17497138154185,1.30000000000019,2.43490045406549));
#47367=CARTESIAN_POINT('Ctrl Pts',(1.41702750924289,-1.30000000000524,2.47782989780478));
#47368=CARTESIAN_POINT('Ctrl Pts',(1.42540170270334,-1.18514270861534,2.49774146295186));
#47369=CARTESIAN_POINT('Ctrl Pts',(1.42550258089223,-1.06847604194693,2.52093867861861));
#47370=CARTESIAN_POINT('Ctrl Pts',(1.40662261634099,-0.794772684000863,
2.58211939738794));
#47371=CARTESIAN_POINT('Ctrl Pts',(1.3674919546006,-0.636309800095208,2.63893967676586));
#47372=CARTESIAN_POINT('Ctrl Pts',(1.31859656767163,-0.319434907277165,
2.6968814494316));
#47373=CARTESIAN_POINT('Ctrl Pts',(1.28526603322289,-0.158333333333335,
2.72766636464627));
#47374=CARTESIAN_POINT('Ctrl Pts',(1.25601404650177,0.158333333333337,2.71937822426703));
#47375=CARTESIAN_POINT('Ctrl Pts',(1.25935949790364,0.31943490727717,2.68007583722304));
#47376=CARTESIAN_POINT('Ctrl Pts',(1.25016395852549,0.636309800095215,2.6057188510221));
#47377=CARTESIAN_POINT('Ctrl Pts',(1.25785622378767,0.794772684000856,2.53952562511162));
#47378=CARTESIAN_POINT('Ctrl Pts',(1.23205394370523,1.06847604194519,2.46670730026971));
#47379=CARTESIAN_POINT('Ctrl Pts',(1.21461736482249,1.18514270861192,2.43935205790224));
#47380=CARTESIAN_POINT('Ctrl Pts',(1.190913058036,1.3000000000002,2.41616192780651));
#47381=CARTESIAN_POINT('Ctrl Pts',(1.42889034239943,-1.30000000000524,2.4671347108158));
#47382=CARTESIAN_POINT('Ctrl Pts',(1.43959238218228,-1.18514270861534,2.48498799650351));
#47383=CARTESIAN_POINT('Ctrl Pts',(1.44129116148517,-1.06847604194693,2.50662397310923));
#47384=CARTESIAN_POINT('Ctrl Pts',(1.42441634870989,-0.794772684000864,
2.56534618007554));
#47385=CARTESIAN_POINT('Ctrl Pts',(1.38418283888682,-0.636309800095209,
2.62218715507073));
#47386=CARTESIAN_POINT('Ctrl Pts',(1.33453728210758,-0.319434907277165,
2.679638563251));
#47387=CARTESIAN_POINT('Ctrl Pts',(1.29984363043981,-0.158333333333335,
2.71081619697965));
#47388=CARTESIAN_POINT('Ctrl Pts',(1.27036017180119,0.158333333333337,2.70240606017764));
#47389=CARTESIAN_POINT('Ctrl Pts',(1.27482324691011,0.31943490727717,2.66259157303672));
#47390=CARTESIAN_POINT('Ctrl Pts',(1.2659349467312,0.636309800095216,2.58847112715167));
#47391=CARTESIAN_POINT('Ctrl Pts',(1.27444322061751,0.794772684000857,2.5220568277252));
#47392=CARTESIAN_POINT('Ctrl Pts',(1.24642615280947,1.06847604194519,2.45157978994058));
#47393=CARTESIAN_POINT('Ctrl Pts',(1.22735423829508,1.18514270861192,2.4257732250998));
#47394=CARTESIAN_POINT('Ctrl Pts',(1.20133795978574,1.3000000000002,2.40466699364358));
#47395=CARTESIAN_POINT('Ctrl Pts',(1.43805424294559,-1.30000000000524,2.45842477476555));
#47396=CARTESIAN_POINT('Ctrl Pts',(1.45052579669823,-1.18514270861534,2.47458154256932));
#47397=CARTESIAN_POINT('Ctrl Pts',(1.4534793455906,-1.06847604194693,2.4949549554672));
#47398=CARTESIAN_POINT('Ctrl Pts',(1.43831413908994,-0.794772684000866,
2.55176290865245));
#47399=CARTESIAN_POINT('Ctrl Pts',(1.39764596953041,-0.636309800095209,
2.60885128227389));
#47400=CARTESIAN_POINT('Ctrl Pts',(1.34745618703037,-0.319434907277166,
2.66594148200833));
#47401=CARTESIAN_POINT('Ctrl Pts',(1.31136635177083,-0.158333333333335,
2.69727833926731));
#47402=CARTESIAN_POINT('Ctrl Pts',(1.28158088407649,0.158333333333337,2.68871558444311));
#47403=CARTESIAN_POINT('Ctrl Pts',(1.286959737645,0.319434907277171,2.6485089972729));
#47404=CARTESIAN_POINT('Ctrl Pts',(1.27836387244858,0.636309800095217,2.57460236864966));
#47405=CARTESIAN_POINT('Ctrl Pts',(1.28763311239507,0.794772684000857,2.50806146259966));
#47406=CARTESIAN_POINT('Ctrl Pts',(1.25789371311807,1.06847604194519,2.4394775747014));
#47407=CARTESIAN_POINT('Ctrl Pts',(1.23752024547041,1.18514270861192,2.41491090455382));
#47408=CARTESIAN_POINT('Ctrl Pts',(1.20964639416876,1.3000000000002,2.39546498804632));
#47409=CARTESIAN_POINT('Ctrl Pts',(1.44524658952179,-1.30000000000524,2.45206126832144));
#47410=CARTESIAN_POINT('Ctrl Pts',(1.45922916135726,-1.18514270861534,2.46704874305171));
#47411=CARTESIAN_POINT('Ctrl Pts',(1.46320189478081,-1.06847604194693,2.486520269857));
#47412=CARTESIAN_POINT('Ctrl Pts',(1.44925497453907,-0.794772684000865,
2.54186244936722));
#47413=CARTESIAN_POINT('Ctrl Pts',(1.40764544713522,-0.636309800095209,
2.59880991679825));
#47414=CARTESIAN_POINT('Ctrl Pts',(1.35704382757086,-0.319434907277166,
2.65561612297188));
#47415=CARTESIAN_POINT('Ctrl Pts',(1.32050975053321,-0.158333333333335,
2.68736805486952));
#47416=CARTESIAN_POINT('Ctrl Pts',(1.29048989222242,0.158333333333337,2.67868800789844));
#47417=CARTESIAN_POINT('Ctrl Pts',(1.29612786258562,0.319434907277171,2.6379816075213));
#47418=CARTESIAN_POINT('Ctrl Pts',(1.28736604709719,0.636309800095217,2.56405374750536));
#47419=CARTESIAN_POINT('Ctrl Pts',(1.29683125017996,0.794772684000857,2.49724645076415));
#47420=CARTESIAN_POINT('Ctrl Pts',(1.26587042318278,1.06847604194519,2.43011340484364));
#47421=CARTESIAN_POINT('Ctrl Pts',(1.24467757393584,1.18514270861192,2.40654812886309));
#47422=CARTESIAN_POINT('Ctrl Pts',(1.21569367023734,1.3000000000002,2.38847698495646));
#47423=CARTESIAN_POINT('Ctrl Pts',(1.45125471048104,-1.30000000000525,2.44677151525934));
#47424=CARTESIAN_POINT('Ctrl Pts',(1.46657802915925,-1.18514270861534,2.46082699799967));
#47425=CARTESIAN_POINT('Ctrl Pts',(1.47145035971793,-1.06847604194693,2.47957310579907));
#47426=CARTESIAN_POINT('Ctrl Pts',(1.45856254474585,-0.794772684000865,
2.53371664720401));
#47427=CARTESIAN_POINT('Ctrl Pts',(1.41605853233152,-0.63630980009521,2.5904910869508));
#47428=CARTESIAN_POINT('Ctrl Pts',(1.36511105480377,-0.319434907277166,
2.64705620006073));
#47429=CARTESIAN_POINT('Ctrl Pts',(1.32826769120673,-0.158333333333335,
2.67917980570048));
#47430=CARTESIAN_POINT('Ctrl Pts',(1.2980787856736,0.158333333333337,2.67041270033892));
#47431=CARTESIAN_POINT('Ctrl Pts',(1.30394353688909,0.319434907277171,2.62929574596627));
#47432=CARTESIAN_POINT('Ctrl Pts',(1.29500696350862,0.636309800095217,2.55533351194471));
#47433=CARTESIAN_POINT('Ctrl Pts',(1.30456279045928,0.794772684000857,2.48827139801315));
#47434=CARTESIAN_POINT('Ctrl Pts',(1.27253343099669,1.06847604194519,2.42232284467321));
#47435=CARTESIAN_POINT('Ctrl Pts',(1.25064238382091,1.18514270861192,2.39958405766975));
#47436=CARTESIAN_POINT('Ctrl Pts',(1.22072461237596,1.3000000000002,2.38265316876895));
#47437=CARTESIAN_POINT('Ctrl Pts',(1.45537244101042,-1.30000000000525,2.44302273583353));
#47438=CARTESIAN_POINT('Ctrl Pts',(1.47152458935058,-1.18514270861534,2.45636857978332));
#47439=CARTESIAN_POINT('Ctrl Pts',(1.47698039860248,-1.06847604194693,2.47458286929736));
#47440=CARTESIAN_POINT('Ctrl Pts',(1.46487372631624,-0.794772684000864,
2.52790860501314));
#47441=CARTESIAN_POINT('Ctrl Pts',(1.42209453125328,-0.636309800095209,
2.58474542793579));
#47442=CARTESIAN_POINT('Ctrl Pts',(1.37094607013501,-0.319434907277166,
2.64116469303645));
#47443=CARTESIAN_POINT('Ctrl Pts',(1.33362045532777,-0.158333333333335,
2.67341299515971));
#47444=CARTESIAN_POINT('Ctrl Pts',(1.30330856590516,0.158333333333337,2.66458056519826));
#47445=CARTESIAN_POINT('Ctrl Pts',(1.30949201144557,0.319434907277171,2.62325544072632));
#47446=CARTESIAN_POINT('Ctrl Pts',(1.30058855659897,0.636309800095217,2.54934296144613));
#47447=CARTESIAN_POINT('Ctrl Pts',(1.31039949309279,0.794772684000857,2.4821908922298));
#47448=CARTESIAN_POINT('Ctrl Pts',(1.27755379562326,1.06847604194519,2.41703947810683));
#47449=CARTESIAN_POINT('Ctrl Pts',(1.25507677437302,1.18514270861192,2.39483386454386));
#47450=CARTESIAN_POINT('Ctrl Pts',(1.22434041725408,1.3000000000002,2.37862427049395));
#47451=CARTESIAN_POINT('Ctrl Pts',(1.45770889761886,-1.30000000000525,2.44087227806979));
#47452=CARTESIAN_POINT('Ctrl Pts',(1.47431661684261,-1.18514270861534,2.4538032152612));
#47453=CARTESIAN_POINT('Ctrl Pts',(1.48009896655861,-1.06847604194693,2.47171005037934));
#47454=CARTESIAN_POINT('Ctrl Pts',(1.4684485819871,-0.794772684000865,2.52457374138764));
#47455=CARTESIAN_POINT('Ctrl Pts',(1.42557749616056,-0.636309800095209,
2.58148035505117));
#47456=CARTESIAN_POINT('Ctrl Pts',(1.37432090710934,-0.319434907277166,
2.63782004259088));
#47457=CARTESIAN_POINT('Ctrl Pts',(1.33666723192535,-0.158333333333335,
2.6701128498047));
#47458=CARTESIAN_POINT('Ctrl Pts',(1.30628393068094,0.158333333333337,2.66124204030451));
#47459=CARTESIAN_POINT('Ctrl Pts',(1.31268294514712,0.319434907277172,2.61981443073772));
#47460=CARTESIAN_POINT('Ctrl Pts',(1.3038258337411,0.636309800095217,2.5459432773986));
#47461=CARTESIAN_POINT('Ctrl Pts',(1.31381025086918,0.794772684000857,2.47875244019008));
#47462=CARTESIAN_POINT('Ctrl Pts',(1.28048713217962,1.06847604194519,2.41405118048533));
#47463=CARTESIAN_POINT('Ctrl Pts',(1.25766003214743,1.18514270861192,2.39214301276931));
#47464=CARTESIAN_POINT('Ctrl Pts',(1.22643017542054,1.3000000000002,2.37633345524551));
#47465=CARTESIAN_POINT('Ctrl Pts',(1.46814055446569,-1.30000000000524,2.43115338734429));
#47466=CARTESIAN_POINT('Ctrl Pts',(1.48673518636836,-1.18514270861534,2.44218454247932));
#47467=CARTESIAN_POINT('Ctrl Pts',(1.49396285394707,-1.06847604194693,2.45869541848749));
#47468=CARTESIAN_POINT('Ctrl Pts',(1.48440025040216,-0.794772684000863,
2.5094980964867));
#47469=CARTESIAN_POINT('Ctrl Pts',(1.44132034195163,-0.636309800095208,
2.56682530190243));
#47470=CARTESIAN_POINT('Ctrl Pts',(1.38964689881658,-0.319434907277165,
2.62284337703136));
#47471=CARTESIAN_POINT('Ctrl Pts',(1.35044030854968,-0.158333333333335,
2.65529734648699));
#47472=CARTESIAN_POINT('Ctrl Pts',(1.3197407819702,0.158333333333337,2.64625545093226));
#47473=CARTESIAN_POINT('Ctrl Pts',(1.3271147927352,0.31943490727717,2.60436881916562));
#47474=CARTESIAN_POINT('Ctrl Pts',(1.31856345788762,0.636309800095216,2.53072901757618));
#47475=CARTESIAN_POINT('Ctrl Pts',(1.32954725468782,0.794772684000856,2.46346697110161));
#47476=CARTESIAN_POINT('Ctrl Pts',(1.29403141650394,1.06847604194519,2.40076968330603));
#47477=CARTESIAN_POINT('Ctrl Pts',(1.26954793162237,1.18514270861192,2.38016129957916));
#47478=CARTESIAN_POINT('Ctrl Pts',(1.23595445221752,1.3000000000002,2.36608386484867));
#47479=CARTESIAN_POINT('Ctrl Pts',(1.48346539173413,-1.30000000000523,2.41811719874013));
#47480=CARTESIAN_POINT('Ctrl Pts',(1.50537195826871,-1.18514270861532,2.42681832126565));
#47481=CARTESIAN_POINT('Ctrl Pts',(1.51488511192707,-1.06847604194692,2.44154812472289));
#47482=CARTESIAN_POINT('Ctrl Pts',(1.50823113694001,-0.794772684000855,
2.48950437638155));
#47483=CARTESIAN_POINT('Ctrl Pts',(1.46354339745113,-0.6363098000952,2.54671340487404));
#47484=CARTESIAN_POINT('Ctrl Pts',(1.411125321792,-0.319434907277161,2.60217481893685));
#47485=CARTESIAN_POINT('Ctrl Pts',(1.37071656390568,-0.158333333333333,
2.63531459468677));
#47486=CARTESIAN_POINT('Ctrl Pts',(1.33947123938326,0.158333333333335,2.62597631962764));
#47487=CARTESIAN_POINT('Ctrl Pts',(1.3476753188231,0.31943490727717,2.58319881968591));
#47488=CARTESIAN_POINT('Ctrl Pts',(1.33840305303561,0.636309800095211,2.509325968028));
#47489=CARTESIAN_POINT('Ctrl Pts',(1.34865735229928,0.794772684000845,2.44096986906576));
#47490=CARTESIAN_POINT('Ctrl Pts',(1.31073523642226,1.06847604194518,2.3813193857751));
#47491=CARTESIAN_POINT('Ctrl Pts',(1.28489309106389,1.1851427086119,2.36293639782752));
#47492=CARTESIAN_POINT('Ctrl Pts',(1.24962387915744,1.30000000000019,2.35199090588064));
#47493=CARTESIAN_POINT('Ctrl Pts',(1.50232800365894,-1.30000000000523,2.40107596869255));
#47494=CARTESIAN_POINT('Ctrl Pts',(1.52841317350604,-1.18514270861532,2.40677102458424));
#47495=CARTESIAN_POINT('Ctrl Pts',(1.54083972280061,-1.06847604194691,2.41921947995603));
#47496=CARTESIAN_POINT('Ctrl Pts',(1.53799339171977,-0.794772684000854,
2.46357960598144));
#47497=CARTESIAN_POINT('Ctrl Pts',(1.49159331440414,-0.636309800095201,
2.52080060706813));
#47498=CARTESIAN_POINT('Ctrl Pts',(1.43822367291136,-0.319434907277162,
2.57555728417339));
#47499=CARTESIAN_POINT('Ctrl Pts',(1.39576077015877,-0.158333333333333,
2.6093349919864));
#47500=CARTESIAN_POINT('Ctrl Pts',(1.36412134633887,0.158333333333335,2.59977366191929));
#47501=CARTESIAN_POINT('Ctrl Pts',(1.37380619390945,0.319434907277167,2.55606276684382));
#47502=CARTESIAN_POINT('Ctrl Pts',(1.36504791729566,0.636309800095209,2.48258779516276));
#47503=CARTESIAN_POINT('Ctrl Pts',(1.37741843250096,0.794772684000847,2.41426910879833));
#47504=CARTESIAN_POINT('Ctrl Pts',(1.335210658048,1.06847604194518,2.35798863023809));
#47505=CARTESIAN_POINT('Ctrl Pts',(1.30610774767455,1.1851427086119,2.34176005044349));
#47506=CARTESIAN_POINT('Ctrl Pts',(1.26617210853617,1.30000000000018,2.33366462462575));
#47507=CARTESIAN_POINT('Ctrl Pts',(1.51240241427739,-1.30000000000522,2.39289301592785));
#47508=CARTESIAN_POINT('Ctrl Pts',(1.54036079622412,-1.18514270861532,2.39698352052958));
#47509=CARTESIAN_POINT('Ctrl Pts',(1.5541361931653,-1.06847604194691,2.40824395634222));
#47510=CARTESIAN_POINT('Ctrl Pts',(1.55319458319893,-0.794772684000851,
2.45082179114856));
#47511=CARTESIAN_POINT('Ctrl Pts',(1.50638430478293,-0.636309800095197,
2.50829316388192));
#47512=CARTESIAN_POINT('Ctrl Pts',(1.45275981718469,-0.319434907277159,
2.56280057377912));
#47513=CARTESIAN_POINT('Ctrl Pts',(1.40945018590222,-0.158333333333332,
2.596952544446));
#47514=CARTESIAN_POINT('Ctrl Pts',(1.37727481249132,0.158333333333334,2.5870955960286));
#47515=CARTESIAN_POINT('Ctrl Pts',(1.38703062157811,0.319434907277167,2.54259045047355));
#47516=CARTESIAN_POINT('Ctrl Pts',(1.37792399116514,0.636309800095206,2.46901592396535));
#47517=CARTESIAN_POINT('Ctrl Pts',(1.39070615145891,0.79477268400084,2.4004245622768));
#47518=CARTESIAN_POINT('Ctrl Pts',(1.34687223012689,1.06847604194517,2.34604685839021));
#47519=CARTESIAN_POINT('Ctrl Pts',(1.3166617592273,1.1851427086119,2.33112379976082));
#47520=CARTESIAN_POINT('Ctrl Pts',(1.27521489776589,1.30000000000018,2.32481577562205));
#47521=CARTESIAN_POINT('Ctrl Pts',(1.5174122737698,-1.30000000000522,2.38879014525548));
#47522=CARTESIAN_POINT('Ctrl Pts',(1.54630261814547,-1.18514270861532,2.39207685648064));
#47523=CARTESIAN_POINT('Ctrl Pts',(1.56074958986041,-1.06847604194691,2.40274235366977));
#47524=CARTESIAN_POINT('Ctrl Pts',(1.56075790439564,-0.794772684000851,
2.44442825749958));
#47525=CARTESIAN_POINT('Ctrl Pts',(1.51378858280601,-0.636309800095197,
2.50204658614368));
#47526=CARTESIAN_POINT('Ctrl Pts',(1.45995892423166,-0.319434907277159,
2.55639080502906));
#47527=CARTESIAN_POINT('Ctrl Pts',(1.41600270611002,-0.158333333333332,
2.5906195818553));
#47528=CARTESIAN_POINT('Ctrl Pts',(1.38362278588542,0.158333333333334,2.58064707201732));
#47529=CARTESIAN_POINT('Ctrl Pts',(1.39375448302884,0.319434907277167,2.53591491365547));
#47530=CARTESIAN_POINT('Ctrl Pts',(1.38457112325773,0.636309800095206,2.4623387576987));
#47531=CARTESIAN_POINT('Ctrl Pts',(1.39741805963303,0.79477268400084,2.39353727747146));
#47532=CARTESIAN_POINT('Ctrl Pts',(1.3526706067805,1.06847604194517,2.34006403730454));
#47533=CARTESIAN_POINT('Ctrl Pts',(1.32185850051434,1.1851427086119,2.32577266001673));
#47534=CARTESIAN_POINT('Ctrl Pts',(1.27960380226534,1.30000000000018,2.32033648973054));
#47535=CARTESIAN_POINT('',(1.23744427200895,1.2,2.40716872050849));
#47536=CARTESIAN_POINT('Ctrl Pts',(1.23744427200895,1.2,2.40716872050849));
#47537=CARTESIAN_POINT('Ctrl Pts',(1.21265992951091,1.22410027197493,2.42566031732214));
#47538=CARTESIAN_POINT('Ctrl Pts',(1.18821929348464,1.24663669298873,2.44278295325562));
#47539=CARTESIAN_POINT('Ctrl Pts',(1.16764034544656,1.26665794013823,2.45828850243014));
#47540=CARTESIAN_POINT('Ctrl Pts',(1.15325920879695,1.28043540591626,2.46894367010376));
#47541=CARTESIAN_POINT('Ctrl Pts',(1.13357773502981,1.30000000000018,2.48433445644807));
#47542=CARTESIAN_POINT('',(1.38832548123549,0.653834841342252,2.44867888290427));
#47543=CARTESIAN_POINT('Ctrl Pts',(1.38832548119236,0.653834841327917,2.44867888285037));
#47544=CARTESIAN_POINT('Ctrl Pts',(1.37454923404638,0.710422285467849,2.44465349402137));
#47545=CARTESIAN_POINT('Ctrl Pts',(1.35937799661829,0.767445708967689,2.44028939546552));
#47546=CARTESIAN_POINT('Ctrl Pts',(1.32837715554167,0.881873342563316,2.43154329000569));
#47547=CARTESIAN_POINT('Ctrl Pts',(1.31343556545719,0.939380857891816,2.42739657917695));
#47548=CARTESIAN_POINT('Ctrl Pts',(1.28543018260622,1.03763475213985,2.41980418590468));
#47549=CARTESIAN_POINT('Ctrl Pts',(1.28390944537373,1.04222967121286,2.41937301107199));
#47550=CARTESIAN_POINT('Ctrl Pts',(1.25550432481215,1.13919581836279,2.41185397080366));
#47551=CARTESIAN_POINT('Ctrl Pts',(1.24774191689618,1.16589029126337,2.40982743326882));
#47552=CARTESIAN_POINT('Ctrl Pts',(1.23744427200895,1.2,2.40716872050849));
#47553=CARTESIAN_POINT('',(1.52166805320966,-0.653834841531101,2.48968935888076));
#47554=CARTESIAN_POINT('Ctrl Pts',(1.52166805320965,-0.653834841531103,
2.48968935888076));
#47555=CARTESIAN_POINT('Ctrl Pts',(1.49334294437536,-0.575779834472804,
2.5202663708974));
#47556=CARTESIAN_POINT('Ctrl Pts',(1.46876645094377,-0.493711163709688,
2.54538047219522));
#47557=CARTESIAN_POINT('Ctrl Pts',(1.43180311244362,-0.338122820387436,
2.58001286451235));
#47558=CARTESIAN_POINT('Ctrl Pts',(1.41789173110139,-0.265674896964429,
2.59130979717286));
#47559=CARTESIAN_POINT('Ctrl Pts',(1.39652617980709,-0.129743851517951,
2.60315463078574));
#47560=CARTESIAN_POINT('Ctrl Pts',(1.38848883722884,-0.066666048842503,
2.60504789056344));
#47561=CARTESIAN_POINT('Ctrl Pts',(1.37568467463284,0.0595072959430674,
2.60150288534975));
#47562=CARTESIAN_POINT('Ctrl Pts',(1.3708331957342,0.122731095105783,2.59605943341458));
#47563=CARTESIAN_POINT('Ctrl Pts',(1.36465986011061,0.260115581078158,2.57636314119223));
#47564=CARTESIAN_POINT('Ctrl Pts',(1.36408862584207,0.333988073947148,2.5606638868716));
#47565=CARTESIAN_POINT('Ctrl Pts',(1.36979927568344,0.491535585046963,2.51611859105072));
#47566=CARTESIAN_POINT('Ctrl Pts',(1.37696799146085,0.574935557742433,2.48517079865281));
#47567=CARTESIAN_POINT('Ctrl Pts',(1.38832548111874,0.653834841363331,2.44867888291351));
#47568=CARTESIAN_POINT('',(1.45278841576471,-1.2,2.46799135471839));
#47569=CARTESIAN_POINT('Ctrl Pts',(1.45278841576471,-1.2,2.46799135471839));
#47570=CARTESIAN_POINT('Ctrl Pts',(1.46425358638865,-1.13668704506502,2.47151131174211));
#47571=CARTESIAN_POINT('Ctrl Pts',(1.48060714938815,-1.03615749185349,2.47658610316088));
#47572=CARTESIAN_POINT('Ctrl Pts',(1.51314428743919,-0.775105528038972,
2.48691778855522));
#47573=CARTESIAN_POINT('Ctrl Pts',(1.51686893334905,-0.721274379078139,
2.48813900096771));
#47574=CARTESIAN_POINT('Ctrl Pts',(1.52166805320965,-0.653834841531101,
2.48968935888076));
#47575=CARTESIAN_POINT('Ctrl Pts',(1.3523706033532,-1.30000000000523,2.54236178400089));
#47576=CARTESIAN_POINT('Ctrl Pts',(1.35337714919034,-1.2989997171284,2.54161244521808));
#47577=CARTESIAN_POINT('Ctrl Pts',(1.35437680901242,-1.29799915645057,2.54086100403259));
#47578=CARTESIAN_POINT('Ctrl Pts',(1.37100486089963,-1.2810069371636,2.52800100315971));
#47579=CARTESIAN_POINT('Ctrl Pts',(1.38698908584542,-1.26515051009269,2.5161817713799));
#47580=CARTESIAN_POINT('Ctrl Pts',(1.41422895348329,-1.23763938663058,2.49560680488971));
#47581=CARTESIAN_POINT('Ctrl Pts',(1.43177461776686,-1.21964479809685,2.48208962741353));
#47582=CARTESIAN_POINT('Ctrl Pts',(1.45278841576471,-1.2,2.4679913547184));
#47583=CARTESIAN_POINT('Origin',(0.,1.25,7.2));
#47584=CARTESIAN_POINT('Origin',(0.,1.2,7.2));
#47585=CARTESIAN_POINT('Origin',(0.,0.92691742076555,7.2));
#47586=CARTESIAN_POINT('Origin',(0.,0.653834841531101,7.2));
#47587=CARTESIAN_POINT('Origin',(0.,0.,7.2));
#47588=CARTESIAN_POINT('Origin',(0.,-0.653834841531101,7.2));
#47589=CARTESIAN_POINT('Origin',(0.,-0.926917420765551,7.2));
#47590=CARTESIAN_POINT('Origin',(0.,-1.2,7.2));
#47591=CARTESIAN_POINT('Origin',(0.,-1.25,7.2));
#47592=CARTESIAN_POINT('Ctrl Pts',(1.83297302538932,-1.30000000000158,2.50013704960828));
#47593=CARTESIAN_POINT('Ctrl Pts',(1.79559295569107,-1.18514270861285,2.47969831528161));
#47594=CARTESIAN_POINT('Ctrl Pts',(1.76226517728476,-1.06847604194566,2.47314938072437));
#47595=CARTESIAN_POINT('Ctrl Pts',(1.69463294550958,-0.794772684000851,
2.49010824789955));
#47596=CARTESIAN_POINT('Ctrl Pts',(1.66458583994784,-0.636309800095196,
2.55332105438372));
#47597=CARTESIAN_POINT('Ctrl Pts',(1.61390936643532,-0.319434907277159,
2.60744757149477));
#47598=CARTESIAN_POINT('Ctrl Pts',(1.59581317861836,-0.158333333333332,
2.64959190996504));
#47599=CARTESIAN_POINT('Ctrl Pts',(1.56375557866912,0.158333333333334,2.63862740032203));
#47600=CARTESIAN_POINT('Ctrl Pts',(1.54831342142296,0.319434907277167,2.58509892141403));
#47601=CARTESIAN_POINT('Ctrl Pts',(1.53670704324243,0.636309800095206,2.50949324534551));
#47602=CARTESIAN_POINT('Ctrl Pts',(1.53257526769918,0.79477268400084,2.43527116374883));
#47603=CARTESIAN_POINT('Ctrl Pts',(1.55708435379909,1.06847604194523,2.40155144628542));
#47604=CARTESIAN_POINT('Ctrl Pts',(1.57504122138999,1.18514270861202,2.40141459471864));
#47605=CARTESIAN_POINT('Ctrl Pts',(1.60034588135027,1.30000000000036,2.41573690783635));
#47606=CARTESIAN_POINT('Ctrl Pts',(1.83480870568655,-1.30000000000158,2.51254415305696));
#47607=CARTESIAN_POINT('Ctrl Pts',(1.79771081770392,-1.18514270861285,2.49446577697444));
#47608=CARTESIAN_POINT('Ctrl Pts',(1.7646139198211,-1.06847604194566,2.48964618907725));
#47609=CARTESIAN_POINT('Ctrl Pts',(1.69739655222609,-0.794772684000851,
2.50914242999906));
#47610=CARTESIAN_POINT('Ctrl Pts',(1.66749164590163,-0.636309800095196,
2.57193910873708));
#47611=CARTESIAN_POINT('Ctrl Pts',(1.61694123862426,-0.319434907277159,
2.62615319012968));
#47612=CARTESIAN_POINT('Ctrl Pts',(1.59850372071989,-0.158333333333332,
2.66748833124109));
#47613=CARTESIAN_POINT('Ctrl Pts',(1.56691293506486,0.158333333333334,2.65657729849294));
#47614=CARTESIAN_POINT('Ctrl Pts',(1.55242668624754,0.319434907277167,2.60393320297167));
#47615=CARTESIAN_POINT('Ctrl Pts',(1.54134412421265,0.636309800095206,2.52830467126513));
#47616=CARTESIAN_POINT('Ctrl Pts',(1.53729692887853,0.79477268400084,2.45450733583496));
#47617=CARTESIAN_POINT('Ctrl Pts',(1.5613175325965,1.06847604194523,2.41822774050965));
#47618=CARTESIAN_POINT('Ctrl Pts',(1.57888716167955,1.18514270861202,2.41633877452248));
#47619=CARTESIAN_POINT('Ctrl Pts',(1.60362879054724,1.30000000000036,2.42826493507295));
#47620=CARTESIAN_POINT('Ctrl Pts',(1.83708905662232,-1.30000000000159,2.53102448418581));
#47621=CARTESIAN_POINT('Ctrl Pts',(1.80136229993117,-1.18514270861286,2.51667909267183));
#47622=CARTESIAN_POINT('Ctrl Pts',(1.76913700894575,-1.06847604194566,2.51456415552258));
#47623=CARTESIAN_POINT('Ctrl Pts',(1.70277922636828,-0.79477268400085,2.53793302389257));
#47624=CARTESIAN_POINT('Ctrl Pts',(1.67135187920676,-0.636309800095195,
2.59978957685925));
#47625=CARTESIAN_POINT('Ctrl Pts',(1.62065406220172,-0.319434907277157,
2.65407625952769));
#47626=CARTESIAN_POINT('Ctrl Pts',(1.60262224066089,-0.158333333333332,
2.69434883567948));
#47627=CARTESIAN_POINT('Ctrl Pts',(1.57157649537649,0.158333333333334,2.68350638536189));
#47628=CARTESIAN_POINT('Ctrl Pts',(1.55748072036052,0.319434907277169,2.63204434634934));
#47629=CARTESIAN_POINT('Ctrl Pts',(1.54714424273508,0.636309800095207,2.55637921263097));
#47630=CARTESIAN_POINT('Ctrl Pts',(1.54431044423645,0.794772684000837,2.48337485439851));
#47631=CARTESIAN_POINT('Ctrl Pts',(1.56766279786463,1.06847604194523,2.44325716475985));
#47632=CARTESIAN_POINT('Ctrl Pts',(1.58448661498275,1.18514270861202,2.4387111168812));
#47633=CARTESIAN_POINT('Ctrl Pts',(1.60802588062332,1.30000000000036,2.44698448246157));
#47634=CARTESIAN_POINT('Ctrl Pts',(1.84208384966657,-1.30000000000158,2.56820316470835));
#47635=CARTESIAN_POINT('Ctrl Pts',(1.80706459881987,-1.18514270861285,2.5609412208685));
#47636=CARTESIAN_POINT('Ctrl Pts',(1.77543875409267,-1.06847604194566,2.5640181209671));
#47637=CARTESIAN_POINT('Ctrl Pts',(1.71021617302907,-0.794772684000848,
2.59501117350305));
#47638=CARTESIAN_POINT('Ctrl Pts',(1.67940607667781,-0.636309800095195,
2.65565089492229));
#47639=CARTESIAN_POINT('Ctrl Pts',(1.62893197543394,-0.319434907277158,
2.71017957772096));
#47640=CARTESIAN_POINT('Ctrl Pts',(1.60964708250435,-0.158333333333332,
2.74796538391066));
#47641=CARTESIAN_POINT('Ctrl Pts',(1.57962478506506,0.158333333333334,2.73725048261268));
#47642=CARTESIAN_POINT('Ctrl Pts',(1.56789372642441,0.319434907277167,2.68842722179615));
#47643=CARTESIAN_POINT('Ctrl Pts',(1.55923857138086,0.636309800095206,2.61273007445824));
#47644=CARTESIAN_POINT('Ctrl Pts',(1.55766344329217,0.794772684000837,2.54114139165139));
#47645=CARTESIAN_POINT('Ctrl Pts',(1.57949120126525,1.06847604194523,2.49328676282195));
#47646=CARTESIAN_POINT('Ctrl Pts',(1.5949086741531,1.18514270861202,2.4834158670341));
#47647=CARTESIAN_POINT('Ctrl Pts',(1.61629519230038,1.30000000000036,2.48438857108989));
#47648=CARTESIAN_POINT('Ctrl Pts',(1.84604424837343,-1.30000000000159,2.60515943272698));
#47649=CARTESIAN_POINT('Ctrl Pts',(1.81265507118371,-1.18514270861286,2.60519420663172));
#47650=CARTESIAN_POINT('Ctrl Pts',(1.7820979101349,-1.06847604194566,2.61358217824961));
#47651=CARTESIAN_POINT('Ctrl Pts',(1.71804727900156,-0.794772684000849,
2.65225762846366));
#47652=CARTESIAN_POINT('Ctrl Pts',(1.68577242078289,-0.636309800095195,
2.71129624843233));
#47653=CARTESIAN_POINT('Ctrl Pts',(1.63510774945675,-0.319434907277157,
2.76600019642908));
#47654=CARTESIAN_POINT('Ctrl Pts',(1.61578764048504,-0.158333333333332,
2.80150232629752));
#47655=CARTESIAN_POINT('Ctrl Pts',(1.58658890630827,0.158333333333334,2.79090471741053));
#47656=CARTESIAN_POINT('Ctrl Pts',(1.5757909659052,0.319434907277168,2.74451319525997));
#47657=CARTESIAN_POINT('Ctrl Pts',(1.56885249695731,0.636309800095206,2.66881702278035));
#47658=CARTESIAN_POINT('Ctrl Pts',(1.56982933223661,0.794772684000836,2.59888504417254));
#47659=CARTESIAN_POINT('Ctrl Pts',(1.59088502566213,1.06847604194523,2.54339135656419));
#47660=CARTESIAN_POINT('Ctrl Pts',(1.60513301753012,1.18514270861202,2.52820947633891));
#47661=CARTESIAN_POINT('Ctrl Pts',(1.62451477177252,1.30000000000036,2.52186687701023));
#47662=CARTESIAN_POINT('Ctrl Pts',(1.84998087442497,-1.30000000000158,2.64821750022589));
#47663=CARTESIAN_POINT('Ctrl Pts',(1.81753200576564,-1.18514270861285,2.65660597517614));
#47664=CARTESIAN_POINT('Ctrl Pts',(1.78756580934509,-1.06847604194566,2.67108144134482));
#47665=CARTESIAN_POINT('Ctrl Pts',(1.72407337042516,-0.794772684000847,
2.71858483141443));
#47666=CARTESIAN_POINT('Ctrl Pts',(1.69097357813135,-0.636309800095194,
2.77590746151336));
#47667=CARTESIAN_POINT('Ctrl Pts',(1.6396390517662,-0.319434907277157,2.8307265598103));
#47668=CARTESIAN_POINT('Ctrl Pts',(1.61879549410128,-0.158333333333332,
2.8632678771389));
#47669=CARTESIAN_POINT('Ctrl Pts',(1.59100525666869,0.158333333333334,2.85291518025025));
#47670=CARTESIAN_POINT('Ctrl Pts',(1.58380273704812,0.319434907277168,2.80987293931332));
#47671=CARTESIAN_POINT('Ctrl Pts',(1.57905167808586,0.636309800095206,2.7342680700284));
#47672=CARTESIAN_POINT('Ctrl Pts',(1.58039437267368,0.794772684000836,2.66585860404003));
#47673=CARTESIAN_POINT('Ctrl Pts',(1.60065206700527,1.06847604194523,2.60143225534537));
#47674=CARTESIAN_POINT('Ctrl Pts',(1.61409160529326,1.18514270861202,2.58011164689002));
#47675=CARTESIAN_POINT('Ctrl Pts',(1.63220187661463,1.30000000000036,2.56535820909775));
#47676=CARTESIAN_POINT('Ctrl Pts',(1.85283044901602,-1.30000000000159,2.68504538799601));
#47677=CARTESIAN_POINT('Ctrl Pts',(1.82102164246291,-1.18514270861286,2.70057949214545));
#47678=CARTESIAN_POINT('Ctrl Pts',(1.79142664860177,-1.06847604194566,2.72025750609338));
#47679=CARTESIAN_POINT('Ctrl Pts',(1.72817064251467,-0.794772684000851,
2.77529091550702));
#47680=CARTESIAN_POINT('Ctrl Pts',(1.69393483689088,-0.636309800095194,
2.83103592248963));
#47681=CARTESIAN_POINT('Ctrl Pts',(1.64263881365639,-0.319434907277156,
2.88607524331724));
#47682=CARTESIAN_POINT('Ctrl Pts',(1.62241952480379,-0.158333333333332,
2.91646130213644));
#47683=CARTESIAN_POINT('Ctrl Pts',(1.59539294034557,0.158333333333334,2.90625956285633));
#47684=CARTESIAN_POINT('Ctrl Pts',(1.58827489522903,0.319434907277167,2.86554585249684));
#47685=CARTESIAN_POINT('Ctrl Pts',(1.58515268627984,0.636309800095205,2.7899827975132));
#47686=CARTESIAN_POINT('Ctrl Pts',(1.58941187234875,0.794772684000835,2.7233635989376));
#47687=CARTESIAN_POINT('Ctrl Pts',(1.60959927129965,1.06847604194523,2.65137578211948));
#47688=CARTESIAN_POINT('Ctrl Pts',(1.62226556377947,1.18514270861202,2.62476489268611));
#47689=CARTESIAN_POINT('Ctrl Pts',(1.63885977175013,1.30000000000036,2.60270397230846));
#47690=CARTESIAN_POINT('Ctrl Pts',(1.85568448251895,-1.30000000000158,2.72795645097212));
#47691=CARTESIAN_POINT('Ctrl Pts',(1.82400623592181,-1.18514270861285,2.75170204140675));
#47692=CARTESIAN_POINT('Ctrl Pts',(1.79437245874033,-1.06847604194566,2.7773548944478));
#47693=CARTESIAN_POINT('Ctrl Pts',(1.73063563857937,-0.794772684000848,
2.84102427497556));
#47694=CARTESIAN_POINT('Ctrl Pts',(1.69534203274488,-0.636309800095195,
2.89499257118523));
#47695=CARTESIAN_POINT('Ctrl Pts',(1.64333947637977,-0.319434907277158,
2.95013761791124));
#47696=CARTESIAN_POINT('Ctrl Pts',(1.62231051404587,-0.158333333333332,
2.97767872212522));
#47697=CARTESIAN_POINT('Ctrl Pts',(1.59665261097123,0.158333333333334,2.96776928219619));
#47698=CARTESIAN_POINT('Ctrl Pts',(1.59219559290535,0.319434907277166,2.9303281940625));
#47699=CARTESIAN_POINT('Ctrl Pts',(1.59158465402795,0.636309800095205,2.85497907049425));
#47700=CARTESIAN_POINT('Ctrl Pts',(1.59748032345738,0.794772684000837,2.79013949145928));
#47701=CARTESIAN_POINT('Ctrl Pts',(1.6176228019188,1.06847604194523,2.70931450316173));
#47702=CARTESIAN_POINT('Ctrl Pts',(1.62969374557501,1.18514270861202,2.67656520456593));
#47703=CARTESIAN_POINT('Ctrl Pts',(1.64511670031386,1.30000000000037,2.64605274994738));
#47704=CARTESIAN_POINT('Ctrl Pts',(1.85622336316529,-1.30000000000159,2.76429054728891));
#47705=CARTESIAN_POINT('Ctrl Pts',(1.82459438932158,-1.18514270861286,2.79509037064409));
#47706=CARTESIAN_POINT('Ctrl Pts',(1.79488348319445,-1.06847604194566,2.82587338111097));
#47707=CARTESIAN_POINT('Ctrl Pts',(1.73067646652796,-0.794772684000851,
2.89694945227406));
#47708=CARTESIAN_POINT('Ctrl Pts',(1.6944354202499,-0.636309800095195,2.94935338210611));
#47709=CARTESIAN_POINT('Ctrl Pts',(1.64196761075382,-0.319434907277157,
3.00461008517178));
#47710=CARTESIAN_POINT('Ctrl Pts',(1.62068829545789,-0.158333333333332,
3.02979545220595));
#47711=CARTESIAN_POINT('Ctrl Pts',(1.59599470275176,0.158333333333334,3.02012457153028));
#47712=CARTESIAN_POINT('Ctrl Pts',(1.59284709103715,0.319434907277166,2.9853361056183));
#47713=CARTESIAN_POINT('Ctrl Pts',(1.59447265136719,0.636309800095204,2.91024244830098));
#47714=CARTESIAN_POINT('Ctrl Pts',(1.60259838285294,0.794772684000836,2.84714880964597));
#47715=CARTESIAN_POINT('Ctrl Pts',(1.62359037912186,1.06847604194523,2.75892429854575));
#47716=CARTESIAN_POINT('Ctrl Pts',(1.63556204596999,1.18514270861202,2.72097797593921));
#47717=CARTESIAN_POINT('Ctrl Pts',(1.65041872231155,1.30000000000036,2.6832744525411));
#47718=CARTESIAN_POINT('Ctrl Pts',(1.857207086575,-1.30000000000158,2.79473457766695));
#47719=CARTESIAN_POINT('Ctrl Pts',(1.82542798871702,-1.18514270861285,2.8313660125812));
#47720=CARTESIAN_POINT('Ctrl Pts',(1.79546058671256,-1.06847604194566,2.86637726826988));
#47721=CARTESIAN_POINT('Ctrl Pts',(1.73041527297429,-0.79477268400085,2.94351733476144));
#47722=CARTESIAN_POINT('Ctrl Pts',(1.69314276881944,-0.636309800095195,
2.99456124033277));
#47723=CARTESIAN_POINT('Ctrl Pts',(1.6397571931075,-0.319434907277157,3.04978086545143));
#47724=CARTESIAN_POINT('Ctrl Pts',(1.61779302863138,-0.158333333333332,
3.0728752244211));
#47725=CARTESIAN_POINT('Ctrl Pts',(1.59373174494822,0.158333333333334,3.06337604168251));
#47726=CARTESIAN_POINT('Ctrl Pts',(1.5920538524928,0.319434907277168,3.0309169560778));
#47727=CARTESIAN_POINT('Ctrl Pts',(1.59557439110431,0.636309800095206,2.95607430228268));
#47728=CARTESIAN_POINT('Ctrl Pts',(1.60528194200455,0.794772684000837,2.89439692122911));
#47729=CARTESIAN_POINT('Ctrl Pts',(1.6270284050152,1.06847604194523,2.80001408481769));
#47730=CARTESIAN_POINT('Ctrl Pts',(1.63899835050215,1.18514270861202,2.75774584268978));
#47731=CARTESIAN_POINT('Ctrl Pts',(1.65352500342459,1.30000000000036,2.7140641910877));
#47732=CARTESIAN_POINT('Ctrl Pts',(1.85717700294372,-1.30000000000158,2.82191251964817));
#47733=CARTESIAN_POINT('Ctrl Pts',(1.82467587459935,-1.18514270861285,2.86364814232314));
#47734=CARTESIAN_POINT('Ctrl Pts',(1.79409818749479,-1.06847604194566,2.90237027513821));
#47735=CARTESIAN_POINT('Ctrl Pts',(1.72790114728519,-0.794772684000848,
2.984864383854));
#47736=CARTESIAN_POINT('Ctrl Pts',(1.69002123908542,-0.636309800095195,
3.03475059042299));
#47737=CARTESIAN_POINT('Ctrl Pts',(1.63639307143117,-0.319434907277158,
3.09007880359328));
#47738=CARTESIAN_POINT('Ctrl Pts',(1.61478134544028,-0.158333333333332,
3.11153331731544));
#47739=CARTESIAN_POINT('Ctrl Pts',(1.59142418067489,0.158333333333334,3.10223802430183));
#47740=CARTESIAN_POINT('Ctrl Pts',(1.59008685968969,0.319434907277168,3.07165441116577));
#47741=CARTESIAN_POINT('Ctrl Pts',(1.59530685793716,0.636309800095207,2.99705383101375));
#47742=CARTESIAN_POINT('Ctrl Pts',(1.60699177532695,0.794772684000838,2.93680522299654));
#47743=CARTESIAN_POINT('Ctrl Pts',(1.63015295398593,1.06847604194523,2.83703937527365));
#47744=CARTESIAN_POINT('Ctrl Pts',(1.64249491695268,1.18514270861202,2.79095403592265));
#47745=CARTESIAN_POINT('Ctrl Pts',(1.65715322685094,1.30000000000036,2.74196829601092));
#47746=CARTESIAN_POINT('Ctrl Pts',(1.85685021732899,-1.30000000000159,2.8459911937542));
#47747=CARTESIAN_POINT('Ctrl Pts',(1.82383248374052,-1.18514270861286,2.89229117867176));
#47748=CARTESIAN_POINT('Ctrl Pts',(1.79276864095702,-1.06847604194566,2.93432330112572));
#47749=CARTESIAN_POINT('Ctrl Pts',(1.7255188284608,-0.794772684000849,3.02156629641757));
#47750=CARTESIAN_POINT('Ctrl Pts',(1.68687937034418,-0.636309800095198,
3.07036965871352));
#47751=CARTESIAN_POINT('Ctrl Pts',(1.63270555281764,-0.31943490727716,3.12571658143093));
#47752=CARTESIAN_POINT('Ctrl Pts',(1.61095676665338,-0.158333333333332,
3.14560901566983));
#47753=CARTESIAN_POINT('Ctrl Pts',(1.58829227266957,0.158333333333335,3.13651452669914));
#47754=CARTESIAN_POINT('Ctrl Pts',(1.58800405119919,0.319434907277168,3.10777322024674));
#47755=CARTESIAN_POINT('Ctrl Pts',(1.59473378186573,0.636309800095208,3.03340117467158));
#47756=CARTESIAN_POINT('Ctrl Pts',(1.60757909381203,0.794772684000842,2.97429514916649));
#47757=CARTESIAN_POINT('Ctrl Pts',(1.63156930313847,1.06847604194524,2.86966720804095));
#47758=CARTESIAN_POINT('Ctrl Pts',(1.64407815725073,1.18514270861202,2.82016190187009));
#47759=CARTESIAN_POINT('Ctrl Pts',(1.65871139278271,1.30000000000037,2.76644084839432));
#47760=CARTESIAN_POINT('Ctrl Pts',(1.85632123702933,-1.30000000000158,2.87004577464627));
#47761=CARTESIAN_POINT('Ctrl Pts',(1.82289752895431,-1.18514270861285,2.92096474537703));
#47762=CARTESIAN_POINT('Ctrl Pts',(1.79130358243341,-1.06847604194566,2.96630756421251));
#47763=CARTESIAN_POINT('Ctrl Pts',(1.7225423608555,-0.79477268400085,3.05817652013863));
#47764=CARTESIAN_POINT('Ctrl Pts',(1.68217109548419,-0.636309800095197,
3.10558863656927));
#47765=CARTESIAN_POINT('Ctrl Pts',(1.62677583236554,-0.319434907277159,
3.16074074995168));
#47766=CARTESIAN_POINT('Ctrl Pts',(1.60463331238041,-0.158333333333332,
3.17896989237942));
#47767=CARTESIAN_POINT('Ctrl Pts',(1.58286022960558,0.158333333333334,3.17015830327284));
#47768=CARTESIAN_POINT('Ctrl Pts',(1.58429600192276,0.319434907277167,3.14352493427863));
#47769=CARTESIAN_POINT('Ctrl Pts',(1.59316901530902,0.636309800095206,3.0695944801784));
#47770=CARTESIAN_POINT('Ctrl Pts',(1.60733848366096,0.794772684000841,3.0116791930089));
#47771=CARTESIAN_POINT('Ctrl Pts',(1.63271777493486,1.06847604194523,2.90230191173186));
#47772=CARTESIAN_POINT('Ctrl Pts',(1.64566487291264,1.18514270861202,2.84941986813064));
#47773=CARTESIAN_POINT('Ctrl Pts',(1.66057331407115,1.30000000000036,2.79100115316534));
#47774=CARTESIAN_POINT('Ctrl Pts',(1.85516825338194,-1.30000000000158,2.89087649958971));
#47775=CARTESIAN_POINT('Ctrl Pts',(1.82087595531089,-1.18514270861286,2.94566041516319));
#47776=CARTESIAN_POINT('Ctrl Pts',(1.78858547647656,-1.06847604194566,2.99381213551726));
#47777=CARTESIAN_POINT('Ctrl Pts',(1.71861261358064,-0.794772684000852,
3.08973054453065));
#47778=CARTESIAN_POINT('Ctrl Pts',(1.67807038790798,-0.636309800095199,
3.13632039877109));
#47779=CARTESIAN_POINT('Ctrl Pts',(1.62205182879722,-0.31943490727716,3.19142725953791));
#47780=CARTESIAN_POINT('Ctrl Pts',(1.59928535208654,-0.158333333333333,
3.20812244832611));
#47781=CARTESIAN_POINT('Ctrl Pts',(1.57795197742068,0.158333333333335,3.19946181817398));
#47782=CARTESIAN_POINT('Ctrl Pts',(1.58027056397191,0.319434907277167,3.17449190967688));
#47783=CARTESIAN_POINT('Ctrl Pts',(1.59103090675974,0.636309800095207,3.10095789708986));
#47784=CARTESIAN_POINT('Ctrl Pts',(1.60701735092504,0.794772684000845,3.04427403233974));
#47785=CARTESIAN_POINT('Ctrl Pts',(1.63400377214994,1.06847604194524,2.93087831801372));
#47786=CARTESIAN_POINT('Ctrl Pts',(1.64746113010348,1.18514270861202,2.87509346701162));
#47787=CARTESIAN_POINT('Ctrl Pts',(1.66269442420776,1.30000000000036,2.81260856801387));
#47788=CARTESIAN_POINT('Ctrl Pts',(1.85462998338906,-1.30000000000158,2.91496806145136));
#47789=CARTESIAN_POINT('Ctrl Pts',(1.81953039247779,-1.18514270861285,2.97428674730439));
#47790=CARTESIAN_POINT('Ctrl Pts',(1.78634444060864,-1.06847604194566,3.02566290057692));
#47791=CARTESIAN_POINT('Ctrl Pts',(1.71409914197363,-0.794772684000847,
3.1260032532413));
#47792=CARTESIAN_POINT('Ctrl Pts',(1.67107866881396,-0.636309800095196,
3.17094188573005));
#47793=CARTESIAN_POINT('Ctrl Pts',(1.61397295051063,-0.319434907277159,
3.22588933174316));
#47794=CARTESIAN_POINT('Ctrl Pts',(1.592195308861,-0.158333333333332,3.2413322754696));
#47795=CARTESIAN_POINT('Ctrl Pts',(1.57169749085167,0.158333333333334,3.23296778748139));
#47796=CARTESIAN_POINT('Ctrl Pts',(1.57436968834082,0.319434907277168,3.20974009366222));
#47797=CARTESIAN_POINT('Ctrl Pts',(1.5868866619752,0.636309800095207,3.13657390352965));
#47798=CARTESIAN_POINT('Ctrl Pts',(1.60481301503526,0.79477268400084,3.08129510338653));
#47799=CARTESIAN_POINT('Ctrl Pts',(1.63333994150167,1.06847604194523,2.96318319881582));
#47800=CARTESIAN_POINT('Ctrl Pts',(1.64725309423382,1.18514270861202,2.90400893539306));
#47801=CARTESIAN_POINT('Ctrl Pts',(1.66273115025762,1.30000000000036,2.83678667555881));
#47802=CARTESIAN_POINT('Ctrl Pts',(1.85283789437504,-1.30000000000158,2.93865027657442));
#47803=CARTESIAN_POINT('Ctrl Pts',(1.81651535992032,-1.18514270861285,3.00230228436277));
#47804=CARTESIAN_POINT('Ctrl Pts',(1.78225631473781,-1.06847604194566,3.05678785253886));
#47805=CARTESIAN_POINT('Ctrl Pts',(1.7078781398863,-0.794772684000851,3.16148410558165));
#47806=CARTESIAN_POINT('Ctrl Pts',(1.66383344619413,-0.636309800095199,
3.20518100870501));
#47807=CARTESIAN_POINT('Ctrl Pts',(1.60550325438214,-0.319434907277161,
3.25989184272619));
#47808=CARTESIAN_POINT('Ctrl Pts',(1.58317021770743,-0.158333333333333,
3.27362635495152));
#47809=CARTESIAN_POINT('Ctrl Pts',(1.56321488157999,0.158333333333335,3.2654805698432));
#47810=CARTESIAN_POINT('Ctrl Pts',(1.56698735291969,0.319434907277167,3.24422596096697));
#47811=CARTESIAN_POINT('Ctrl Pts',(1.5818289141946,0.636309800095207,3.17164826685943));
#47812=CARTESIAN_POINT('Ctrl Pts',(1.60165137239488,0.794772684000844,3.11781961864775));
#47813=CARTESIAN_POINT('Ctrl Pts',(1.63273513266472,1.06847604194524,2.99535467018597));
#47814=CARTESIAN_POINT('Ctrl Pts',(1.64772022370997,1.18514270861202,2.93299760235517));
#47815=CARTESIAN_POINT('Ctrl Pts',(1.66423539774648,1.30000000000037,2.86129400510915));
#47816=CARTESIAN_POINT('Ctrl Pts',(1.85121289296214,-1.30000000000158,2.95640735550508));
#47817=CARTESIAN_POINT('Ctrl Pts',(1.81413477572799,-1.18514270861286,3.0235044952298));
#47818=CARTESIAN_POINT('Ctrl Pts',(1.77903315218445,-1.06847604194566,3.08041661645333));
#47819=CARTESIAN_POINT('Ctrl Pts',(1.70250747556487,-0.794772684000852,
3.18836557146659));
#47820=CARTESIAN_POINT('Ctrl Pts',(1.6555293296576,-0.636309800095198,3.23041432047932));
#47821=CARTESIAN_POINT('Ctrl Pts',(1.59729653296459,-0.31943490727716,3.28530599267342));
#47822=CARTESIAN_POINT('Ctrl Pts',(1.57846605784173,-0.158333333333333,
3.29900685886699));
#47823=CARTESIAN_POINT('Ctrl Pts',(1.55960322480628,0.158333333333335,3.29126031404149));
#47824=CARTESIAN_POINT('Ctrl Pts',(1.56162134457333,0.319434907277168,3.27069541427598));
#47825=CARTESIAN_POINT('Ctrl Pts',(1.577255233148,0.636309800095208,3.19822697616151));
#47826=CARTESIAN_POINT('Ctrl Pts',(1.59906096221992,0.794772684000844,3.14564581967966));
#47827=CARTESIAN_POINT('Ctrl Pts',(1.63183545096121,1.06847604194524,3.01969470358375));
#47828=CARTESIAN_POINT('Ctrl Pts',(1.6474613512956,1.18514270861202,2.95480772724551));
#47829=CARTESIAN_POINT('Ctrl Pts',(1.66452629020275,1.30000000000036,2.87955334577817));
#47830=CARTESIAN_POINT('Ctrl Pts',(1.84997378187141,-1.30000000000158,2.971121535271));
#47831=CARTESIAN_POINT('Ctrl Pts',(1.81142637195795,-1.18514270861286,3.04058194767826));
#47832=CARTESIAN_POINT('Ctrl Pts',(1.77544026524582,-1.06847604194566,3.09927690703692));
#47833=CARTESIAN_POINT('Ctrl Pts',(1.69822228252699,-0.794772684000854,
3.21000365487782));
#47834=CARTESIAN_POINT('Ctrl Pts',(1.6530599183159,-0.636309800095197,3.25206334932354));
#47835=CARTESIAN_POINT('Ctrl Pts',(1.5956337929535,-0.319434907277159,3.30725099401256));
#47836=CARTESIAN_POINT('Ctrl Pts',(1.57732859396373,-0.158333333333332,
3.32013355742912));
#47837=CARTESIAN_POINT('Ctrl Pts',(1.55787980380818,0.158333333333335,3.31221462904587));
#47838=CARTESIAN_POINT('Ctrl Pts',(1.55791689148717,0.319434907277168,3.2920206154993));
#47839=CARTESIAN_POINT('Ctrl Pts',(1.57332227386698,0.636309800095207,3.21946529441339));
#47840=CARTESIAN_POINT('Ctrl Pts',(1.59644561705645,0.794772684000841,3.16791019272484));
#47841=CARTESIAN_POINT('Ctrl Pts',(1.63037248672539,1.06847604194523,3.03929244319824));
#47842=CARTESIAN_POINT('Ctrl Pts',(1.64651775933953,1.18514270861202,2.97247319594244));
#47843=CARTESIAN_POINT('Ctrl Pts',(1.66412261980254,1.30000000000036,2.89450855944361));
#47844=CARTESIAN_POINT('Ctrl Pts',(1.84769026538624,-1.30000000000158,2.98867205329444));
#47845=CARTESIAN_POINT('Ctrl Pts',(1.80728079128909,-1.18514270861285,3.06133928403981));
#47846=CARTESIAN_POINT('Ctrl Pts',(1.77031963716493,-1.06847604194566,3.12252412237443));
#47847=CARTESIAN_POINT('Ctrl Pts',(1.6928982860564,-0.794772684000852,3.23734671539853));
#47848=CARTESIAN_POINT('Ctrl Pts',(1.65105800544677,-0.636309800095197,
3.27993182337879));
#47849=CARTESIAN_POINT('Ctrl Pts',(1.59562625196975,-0.319434907277159,
3.3359607193907));
#47850=CARTESIAN_POINT('Ctrl Pts',(1.57813532525437,-0.158333333333332,
3.34778863471165));
#47851=CARTESIAN_POINT('Ctrl Pts',(1.55878655683849,0.158333333333335,3.33992605458163));
#47852=CARTESIAN_POINT('Ctrl Pts',(1.55779869358718,0.319434907277167,3.32076037305399));
#47853=CARTESIAN_POINT('Ctrl Pts',(1.57204631549811,0.636309800095207,3.24764695926783));
#47854=CARTESIAN_POINT('Ctrl Pts',(1.59359769213642,0.794772684000841,3.19612014661867));
#47855=CARTESIAN_POINT('Ctrl Pts',(1.62791108705985,1.06847604194523,3.06340873206302));
#47856=CARTESIAN_POINT('Ctrl Pts',(1.64472849376649,1.18514270861202,2.99396552178466));
#47857=CARTESIAN_POINT('Ctrl Pts',(1.66351030995401,1.30000000000036,2.91252495514655));
#47858=CARTESIAN_POINT('Ctrl Pts',(1.84624880074941,-1.30000000000158,3.00065723247174));
#47859=CARTESIAN_POINT('Ctrl Pts',(1.80327012405171,-1.18514270861285,3.07509490657786));
#47860=CARTESIAN_POINT('Ctrl Pts',(1.76517783186741,-1.06847604194566,3.13773291842763));
#47861=CARTESIAN_POINT('Ctrl Pts',(1.68846554232873,-0.794772684000851,
3.2551796761652));
#47862=CARTESIAN_POINT('Ctrl Pts',(1.65309822965784,-0.636309800095196,
3.29877447145925));
#47863=CARTESIAN_POINT('Ctrl Pts',(1.60107891377445,-0.319434907277159,
3.35545738171415));
#47864=CARTESIAN_POINT('Ctrl Pts',(1.58369000879615,-0.158333333333332,
3.3662154292582));
#47865=CARTESIAN_POINT('Ctrl Pts',(1.56451256417064,0.158333333333334,3.35836908000967));
#47866=CARTESIAN_POINT('Ctrl Pts',(1.56349013317765,0.319434907277167,3.34018877922963));
#47867=CARTESIAN_POINT('Ctrl Pts',(1.57488586701371,0.636309800095206,3.26665956746972));
#47868=CARTESIAN_POINT('Ctrl Pts',(1.59090434066293,0.79477268400084,3.21470783556925));
#47869=CARTESIAN_POINT('Ctrl Pts',(1.6244481867995,1.06847604194523,3.07934166145306));
#47870=CARTESIAN_POINT('Ctrl Pts',(1.64211927471603,1.18514270861202,3.00828819800809));
#47871=CARTESIAN_POINT('Ctrl Pts',(1.66294156247856,1.30000000000036,2.924776272082));
#47872=CARTESIAN_POINT('Ctrl Pts',(1.84783999216081,-1.30000000000158,3.00911085372598));
#47873=CARTESIAN_POINT('Ctrl Pts',(1.80484358765989,-1.18514270861285,3.08329784479062));
#47874=CARTESIAN_POINT('Ctrl Pts',(1.76706466618288,-1.06847604194566,3.14579189582396));
#47875=CARTESIAN_POINT('Ctrl Pts',(1.69184122946293,-0.794772684000851,
3.26315262496583));
#47876=CARTESIAN_POINT('Ctrl Pts',(1.65901382561028,-0.636309800095196,
3.30711063699039));
#47877=CARTESIAN_POINT('Ctrl Pts',(1.6086720442671,-0.319434907277159,3.36396800272369));
#47878=CARTESIAN_POINT('Ctrl Pts',(1.59125278366871,-0.158333333333332,
3.37476869623928));
#47879=CARTESIAN_POINT('Ctrl Pts',(1.57231214945024,0.158333333333334,3.36692516506795));
#47880=CARTESIAN_POINT('Ctrl Pts',(1.57183510628243,0.319434907277167,3.34873710938264));
#47881=CARTESIAN_POINT('Ctrl Pts',(1.58146895355656,0.636309800095206,3.27497385199526));
#47882=CARTESIAN_POINT('Ctrl Pts',(1.59387972389892,0.79477268400084,3.22247344768589));
#47883=CARTESIAN_POINT('Ctrl Pts',(1.62608364872299,1.06847604194523,3.08723090979032));
#47884=CARTESIAN_POINT('Ctrl Pts',(1.6437543175134,1.18514270861202,3.01638787148176));
#47885=CARTESIAN_POINT('Ctrl Pts',(1.66515576931089,1.30000000000036,2.93324327828973));
#47886=CARTESIAN_POINT('Ctrl Pts',(1.84783999216022,-1.3,3.009110853727));
#47887=CARTESIAN_POINT('Ctrl Pts',(1.80484358765954,-1.18514270861178,3.08329784479119));
#47888=CARTESIAN_POINT('Ctrl Pts',(1.76706466618273,-1.06847604194512,3.1457918958242));
#47889=CARTESIAN_POINT('Ctrl Pts',(1.69184122946293,-0.794772684000851,
3.26315262496584));
#47890=CARTESIAN_POINT('Ctrl Pts',(1.65901382561028,-0.636309800095197,
3.30711063699039));
#47891=CARTESIAN_POINT('Ctrl Pts',(1.6086720442671,-0.319434907277159,3.36396800272368));
#47892=CARTESIAN_POINT('Ctrl Pts',(1.59125278366871,-0.158333333333332,
3.37476869623928));
#47893=CARTESIAN_POINT('Ctrl Pts',(1.57231214945024,0.158333333333334,3.36692516506795));
#47894=CARTESIAN_POINT('Ctrl Pts',(1.57183510628243,0.319434907277167,3.34873710938264));
#47895=CARTESIAN_POINT('Ctrl Pts',(1.58146895355656,0.636309800095206,3.27497385199526));
#47896=CARTESIAN_POINT('Ctrl Pts',(1.59387972389891,0.79477268400084,3.22247344768589));
#47897=CARTESIAN_POINT('Ctrl Pts',(1.62608364872297,1.06847604194511,3.08723090979038));
#47898=CARTESIAN_POINT('Ctrl Pts',(1.64375431751336,1.18514270861178,3.01638787148191));
#47899=CARTESIAN_POINT('Ctrl Pts',(1.66515576931082,1.3,2.93324327828999));
#47900=CARTESIAN_POINT('',(1.8162121882396,-1.2,2.59523363379966));
#47901=CARTESIAN_POINT('Ctrl Pts',(1.8162121882396,-1.2,2.59523363379966));
#47902=CARTESIAN_POINT('Ctrl Pts',(1.82366382114832,-1.21762172383529,2.6171155864293));
#47903=CARTESIAN_POINT('Ctrl Pts',(1.83047749029892,-1.23476275836489,2.63830479398897));
#47904=CARTESIAN_POINT('Ctrl Pts',(1.84184377598764,-1.26421553765088,2.67466690339845));
#47905=CARTESIAN_POINT('Ctrl Pts',(1.84966377084331,-1.28493282003519,2.70024848455808));
#47906=CARTESIAN_POINT('Ctrl Pts',(1.85487686289296,-1.30000000000158,2.71871315094771));
#47907=CARTESIAN_POINT('',(1.66957758855468,-0.653834841386366,2.54006323267476));
#47908=CARTESIAN_POINT('Ctrl Pts',(1.66957758857006,-0.653834841385217,
2.54006323264526));
#47909=CARTESIAN_POINT('Ctrl Pts',(1.6873947828161,-0.728434665160969,2.54644683604794));
#47910=CARTESIAN_POINT('Ctrl Pts',(1.6996738894343,-0.774162846424616,2.55093543968267));
#47911=CARTESIAN_POINT('Ctrl Pts',(1.73768103151109,-0.918719140441923,
2.56495158387815));
#47912=CARTESIAN_POINT('Ctrl Pts',(1.7680361736811,-1.0361514204072,2.57623204764662));
#47913=CARTESIAN_POINT('Ctrl Pts',(1.8162121882396,-1.2,2.59523363379966));
#47914=CARTESIAN_POINT('',(1.53759581372313,0.653834841531101,2.49486460198847));
#47915=CARTESIAN_POINT('Ctrl Pts',(1.53759581372313,0.653834841531102,2.49486460198847));
#47916=CARTESIAN_POINT('Ctrl Pts',(1.54253080068449,0.575902863726212,2.53618577289924));
#47917=CARTESIAN_POINT('Ctrl Pts',(1.54736388103037,0.493640201102665,2.57092573760444));
#47918=CARTESIAN_POINT('Ctrl Pts',(1.55686464232257,0.338190864746863,2.62063165073203));
#47919=CARTESIAN_POINT('Ctrl Pts',(1.56146483259355,0.265716392874933,2.63794716225927));
#47920=CARTESIAN_POINT('Ctrl Pts',(1.57177149979286,0.12975615835201,2.66008608934449));
#47921=CARTESIAN_POINT('Ctrl Pts',(1.57719261268522,0.066649891557159,2.6663551854814));
#47922=CARTESIAN_POINT('Ctrl Pts',(1.58968313431103,-0.0595495593502237,
2.67102603384143));
#47923=CARTESIAN_POINT('Ctrl Pts',(1.59684415233489,-0.122807792517795,
2.66948042211137));
#47924=CARTESIAN_POINT('Ctrl Pts',(1.61355162359461,-0.260168353259011,
2.65721880712717));
#47925=CARTESIAN_POINT('Ctrl Pts',(1.62329765128691,-0.333963506589111,
2.64488766435628));
#47926=CARTESIAN_POINT('Ctrl Pts',(1.6449620096927,-0.49120546185675,2.60562844753539));
#47927=CARTESIAN_POINT('Ctrl Pts',(1.65723414657175,-0.574385269905671,
2.57651514903598));
#47928=CARTESIAN_POINT('Ctrl Pts',(1.66957758858473,-0.65383484140123,2.54006323271733));
#47929=CARTESIAN_POINT('',(1.60611193089494,1.2,2.51780986445051));
#47930=CARTESIAN_POINT('Ctrl Pts',(1.60611193089494,1.2,2.51780986445051));
#47931=CARTESIAN_POINT('Ctrl Pts',(1.58805485708337,1.09750097238566,2.5116158225927));
#47932=CARTESIAN_POINT('Ctrl Pts',(1.57349326241228,0.998393154633832,2.50672903384865));
#47933=CARTESIAN_POINT('Ctrl Pts',(1.55103395914313,0.813752614838904,2.49926560256432));
#47934=CARTESIAN_POINT('Ctrl Pts',(1.5447079032333,0.753887267506067,2.49718876869838));
#47935=CARTESIAN_POINT('Ctrl Pts',(1.53759581372313,0.653834841531101,2.49486460198847));
#47936=CARTESIAN_POINT('Ctrl Pts',(1.6438117816117,1.3,2.63706423159009));
#47937=CARTESIAN_POINT('Ctrl Pts',(1.63803607995104,1.28318156972391,2.61710700275808));
#47938=CARTESIAN_POINT('Ctrl Pts',(1.63190962613203,1.26645607930026,2.59717136778684));
#47939=CARTESIAN_POINT('Ctrl Pts',(1.61573517002289,1.22418846120041,2.54667912684929));
#47940=CARTESIAN_POINT('Ctrl Pts',(1.61410323990346,1.2192547094459,2.54090712136841));
#47941=CARTESIAN_POINT('Ctrl Pts',(1.60611193089494,1.2,2.51780986445051));
#47942=CARTESIAN_POINT('Ctrl Pts',(1.84783999216022,-1.3,3.009110853727));
#47943=CARTESIAN_POINT('Ctrl Pts',(1.80484358765954,-1.18514270861178,3.08329784479119));
#47944=CARTESIAN_POINT('Ctrl Pts',(1.76706466618273,-1.06847604194512,3.1457918958242));
#47945=CARTESIAN_POINT('Ctrl Pts',(1.69184122946293,-0.794772684000851,
3.26315262496583));
#47946=CARTESIAN_POINT('Ctrl Pts',(1.65901382561028,-0.636309800095197,
3.30711063699039));
#47947=CARTESIAN_POINT('Ctrl Pts',(1.6086720442671,-0.319434907277159,3.36396800272369));
#47948=CARTESIAN_POINT('Ctrl Pts',(1.59125278366871,-0.158333333333332,
3.37476869623928));
#47949=CARTESIAN_POINT('Ctrl Pts',(1.57231214945024,0.158333333333334,3.36692516506795));
#47950=CARTESIAN_POINT('Ctrl Pts',(1.57183510628243,0.319434907277167,3.34873710938264));
#47951=CARTESIAN_POINT('Ctrl Pts',(1.58146895355656,0.636309800095206,3.27497385199526));
#47952=CARTESIAN_POINT('Ctrl Pts',(1.59387972389891,0.79477268400084,3.22247344768589));
#47953=CARTESIAN_POINT('Ctrl Pts',(1.62608364872297,1.06847604194511,3.08723090979038));
#47954=CARTESIAN_POINT('Ctrl Pts',(1.64375431751336,1.18514270861178,3.01638787148191));
#47955=CARTESIAN_POINT('Ctrl Pts',(1.66515576931082,1.3,2.93324327828999));
#47956=CARTESIAN_POINT('Ctrl Pts',(1.91743049134307,-1.3,3.04191743383109));
#47957=CARTESIAN_POINT('Ctrl Pts',(1.87294351908302,-1.18514270861178,3.11522175128021));
#47958=CARTESIAN_POINT('Ctrl Pts',(1.83415002075929,-1.06847604194512,3.17706282238686));
#47959=CARTESIAN_POINT('Ctrl Pts',(1.75768234278715,-0.794772684000851,
3.29344567564148));
#47960=CARTESIAN_POINT('Ctrl Pts',(1.72556041438091,-0.636309800095197,
3.33753522603443));
#47961=CARTESIAN_POINT('Ctrl Pts',(1.67587573316224,-0.319434907277159,
3.39427900215457));
#47962=CARTESIAN_POINT('Ctrl Pts',(1.65965103821258,-0.158333333333332,
3.40541802202081));
#47963=CARTESIAN_POINT('Ctrl Pts',(1.64085640284598,0.158333333333334,3.39724657205924));
#47964=CARTESIAN_POINT('Ctrl Pts',(1.6393286137645,0.319434907277167,3.37839716560952));
#47965=CARTESIAN_POINT('Ctrl Pts',(1.64860718876712,0.636309800095206,3.30406958137807));
#47966=CARTESIAN_POINT('Ctrl Pts',(1.66044815183843,0.79477268400084,3.25113292298941));
#47967=CARTESIAN_POINT('Ctrl Pts',(1.69421133997152,1.06847604194511,3.116160709857));
#47968=CARTESIAN_POINT('Ctrl Pts',(1.71304615183609,1.18514270861178,3.0456347202283));
#47969=CARTESIAN_POINT('Ctrl Pts',(1.73610094247183,1.3,2.96300721082251));
#47970=CARTESIAN_POINT('Ctrl Pts',(1.98702099052592,-1.3,3.07472401393519));
#47971=CARTESIAN_POINT('Ctrl Pts',(1.9410434505065,-1.18514270861178,3.14714565776922));
#47972=CARTESIAN_POINT('Ctrl Pts',(1.90123537533586,-1.06847604194512,3.20833374894953));
#47973=CARTESIAN_POINT('Ctrl Pts',(1.82352345611138,-0.794772684000851,
3.32373872631713));
#47974=CARTESIAN_POINT('Ctrl Pts',(1.79210700315155,-0.636309800095197,
3.36795981507847));
#47975=CARTESIAN_POINT('Ctrl Pts',(1.74307942205737,-0.319434907277159,
3.42459000158545));
#47976=CARTESIAN_POINT('Ctrl Pts',(1.72804929275646,-0.158333333333332,
3.43606734780233));
#47977=CARTESIAN_POINT('Ctrl Pts',(1.70940065624172,0.158333333333334,3.42756797905052));
#47978=CARTESIAN_POINT('Ctrl Pts',(1.70682212124656,0.319434907277167,3.4080572218364));
#47979=CARTESIAN_POINT('Ctrl Pts',(1.71574542397769,0.636309800095206,3.33316531076089));
#47980=CARTESIAN_POINT('Ctrl Pts',(1.72701657977794,0.79477268400084,3.27979239829292));
#47981=CARTESIAN_POINT('Ctrl Pts',(1.76233903122006,1.06847604194511,3.14509050992361));
#47982=CARTESIAN_POINT('Ctrl Pts',(1.78233798615881,1.18514270861178,3.07488156897468));
#47983=CARTESIAN_POINT('Ctrl Pts',(1.80704611563284,1.3,2.99277114335502));
#47984=CARTESIAN_POINT('Ctrl Pts',(2.05661148970878,-1.3,3.10753059403929));
#47985=CARTESIAN_POINT('Ctrl Pts',(2.00914338192998,-1.18514270861178,3.17906956425824));
#47986=CARTESIAN_POINT('Ctrl Pts',(1.96832072991242,-1.06847604194512,3.23960467551219));
#47987=CARTESIAN_POINT('Ctrl Pts',(1.8893645694356,-0.794772684000851,3.35403177699278));
#47988=CARTESIAN_POINT('Ctrl Pts',(1.85865359192219,-0.636309800095197,
3.39838440412252));
#47989=CARTESIAN_POINT('Ctrl Pts',(1.8102831109525,-0.319434907277159,3.45490100101634));
#47990=CARTESIAN_POINT('Ctrl Pts',(1.79644754730034,-0.158333333333332,
3.46671667358385));
#47991=CARTESIAN_POINT('Ctrl Pts',(1.77794490963746,0.158333333333334,3.45788938604181));
#47992=CARTESIAN_POINT('Ctrl Pts',(1.77431562872862,0.319434907277167,3.43771727806328));
#47993=CARTESIAN_POINT('Ctrl Pts',(1.78288365918825,0.636309800095206,3.3622610401437));
#47994=CARTESIAN_POINT('Ctrl Pts',(1.79358500771746,0.79477268400084,3.30845187359643));
#47995=CARTESIAN_POINT('Ctrl Pts',(1.8304667224686,1.06847604194511,3.17402030999022));
#47996=CARTESIAN_POINT('Ctrl Pts',(1.85162982048153,1.18514270861178,3.10412841772107));
#47997=CARTESIAN_POINT('Ctrl Pts',(1.87799128879385,1.3,3.02253507588753));
#47998=CARTESIAN_POINT('Ctrl Pts',(2.05661148970878,-1.3,3.10753059403928));
#47999=CARTESIAN_POINT('Ctrl Pts',(2.00914338192998,-1.18514270861178,3.17906956425824));
#48000=CARTESIAN_POINT('Ctrl Pts',(1.96832072991242,-1.06847604194512,3.23960467551219));
#48001=CARTESIAN_POINT('Ctrl Pts',(1.8893645694356,-0.794772684000851,3.35403177699278));
#48002=CARTESIAN_POINT('Ctrl Pts',(1.85865359192218,-0.636309800095197,
3.39838440412251));
#48003=CARTESIAN_POINT('Ctrl Pts',(1.8102831109525,-0.319434907277159,3.45490100101634));
#48004=CARTESIAN_POINT('Ctrl Pts',(1.79644754730033,-0.158333333333332,
3.46671667358385));
#48005=CARTESIAN_POINT('Ctrl Pts',(1.77794490963746,0.158333333333334,3.45788938604181));
#48006=CARTESIAN_POINT('Ctrl Pts',(1.77431562872862,0.319434907277167,3.43771727806327));
#48007=CARTESIAN_POINT('Ctrl Pts',(1.78288365918825,0.636309800095206,3.36226104014369));
#48008=CARTESIAN_POINT('Ctrl Pts',(1.79358500771746,0.79477268400084,3.30845187359643));
#48009=CARTESIAN_POINT('Ctrl Pts',(1.8304667224686,1.06847604194511,3.17402030999022));
#48010=CARTESIAN_POINT('Ctrl Pts',(1.85162982048153,1.18514270861178,3.10412841772107));
#48011=CARTESIAN_POINT('Ctrl Pts',(1.87799128879385,1.3,3.02253507588753));
#48012=CARTESIAN_POINT('Ctrl Pts',(2.05661148970879,-1.30000000000002,3.10753059403927));
#48013=CARTESIAN_POINT('Ctrl Pts',(2.00914338192999,-1.18514270861179,3.17906956425823));
#48014=CARTESIAN_POINT('Ctrl Pts',(1.96832072991242,-1.06847604194512,3.23960467551219));
#48015=CARTESIAN_POINT('Ctrl Pts',(1.8893645694356,-0.794772684000851,3.35403177699278));
#48016=CARTESIAN_POINT('Ctrl Pts',(1.85865359192218,-0.636309800095197,
3.39838440412251));
#48017=CARTESIAN_POINT('Ctrl Pts',(1.8102831109525,-0.319434907277159,3.45490100101634));
#48018=CARTESIAN_POINT('Ctrl Pts',(1.79644754730034,-0.158333333333332,
3.46671667358385));
#48019=CARTESIAN_POINT('Ctrl Pts',(1.77794490963746,0.158333333333334,3.45788938604181));
#48020=CARTESIAN_POINT('Ctrl Pts',(1.77431562872862,0.319434907277167,3.43771727806328));
#48021=CARTESIAN_POINT('Ctrl Pts',(1.78288365918825,0.636309800095206,3.36226104014369));
#48022=CARTESIAN_POINT('Ctrl Pts',(1.79358500771746,0.79477268400084,3.30845187359643));
#48023=CARTESIAN_POINT('Ctrl Pts',(1.83046672246867,1.06847604194558,3.17402030998999));
#48024=CARTESIAN_POINT('Ctrl Pts',(1.8516298204817,1.1851427086127,3.10412841772051));
#48025=CARTESIAN_POINT('Ctrl Pts',(1.87799128879416,1.30000000000137,3.02253507588656));
#48026=CARTESIAN_POINT('Ctrl Pts',(2.06438529509424,-1.30000000000002,3.10351053744534));
#48027=CARTESIAN_POINT('Ctrl Pts',(2.0162566695166,-1.18514270861179,3.17486489847698));
#48028=CARTESIAN_POINT('Ctrl Pts',(1.97527792160046,-1.06847604194512,3.23554112309669));
#48029=CARTESIAN_POINT('Ctrl Pts',(1.89712646386989,-0.794772684000851,
3.35104670893996));
#48030=CARTESIAN_POINT('Ctrl Pts',(1.86923725412317,-0.636309800095197,
3.39771324860388));
#48031=CARTESIAN_POINT('Ctrl Pts',(1.82221963516387,-0.319434907277159,
3.45538257530852));
#48032=CARTESIAN_POINT('Ctrl Pts',(1.80802489881759,-0.158333333333332,
3.46678775674664));
#48033=CARTESIAN_POINT('Ctrl Pts',(1.78936170982528,0.158333333333334,3.45778637043419));
#48034=CARTESIAN_POINT('Ctrl Pts',(1.78572104868507,0.319434907277167,3.43766535674272));
#48035=CARTESIAN_POINT('Ctrl Pts',(1.79303694376684,0.636309800095206,3.36107920118311));
#48036=CARTESIAN_POINT('Ctrl Pts',(1.80176883893061,0.79477268400084,3.30562555398019));
#48037=CARTESIAN_POINT('Ctrl Pts',(1.83771824839722,1.06847604194558,3.17002999274191));
#48038=CARTESIAN_POINT('Ctrl Pts',(1.85877864421361,1.1851427086127,3.0998088920672));
#48039=CARTESIAN_POINT('Ctrl Pts',(1.88533826854518,1.30000000000137,3.01806098486724));
#48040=CARTESIAN_POINT('Ctrl Pts',(2.07311117400897,-1.30000000000002,3.09489607890757));
#48041=CARTESIAN_POINT('Ctrl Pts',(2.02516501665969,-1.1851427086118,3.16336132721032));
#48042=CARTESIAN_POINT('Ctrl Pts',(1.98481640679923,-1.06847604194512,3.22233412436262));
#48043=CARTESIAN_POINT('Ctrl Pts',(1.90915490089316,-0.794772684000852,
3.33664362213621));
#48044=CARTESIAN_POINT('Ctrl Pts',(1.88527241428737,-0.636309800095199,
3.38712679647839));
#48045=CARTESIAN_POINT('Ctrl Pts',(1.8404608163555,-0.31943490727716,3.44662850647972));
#48046=CARTESIAN_POINT('Ctrl Pts',(1.82554655027699,-0.158333333333333,
3.45870878172653));
#48047=CARTESIAN_POINT('Ctrl Pts',(1.8067527003081,0.158333333333335,3.44958823116425));
#48048=CARTESIAN_POINT('Ctrl Pts',(1.80384120716332,0.319434907277167,3.4286804811146));
#48049=CARTESIAN_POINT('Ctrl Pts',(1.80839915476674,0.636309800095207,3.35000389209952));
#48050=CARTESIAN_POINT('Ctrl Pts',(1.81207064732138,0.794772684000844,3.29043038686903));
#48051=CARTESIAN_POINT('Ctrl Pts',(1.84559920552924,1.06847604194558,3.15605953551499));
#48052=CARTESIAN_POINT('Ctrl Pts',(1.86633375488223,1.18514270861271,3.08764494368963));
#48053=CARTESIAN_POINT('Ctrl Pts',(1.89328958309553,1.30000000000137,3.00897992265948));
#48054=CARTESIAN_POINT('Ctrl Pts',(2.08606699867076,-1.30000000000002,3.0823702408846));
#48055=CARTESIAN_POINT('Ctrl Pts',(2.0399225376305,-1.1851427086118,3.14764008196292));
#48056=CARTESIAN_POINT('Ctrl Pts',(2.00108022081302,-1.06847604194512,3.20436220961664));
#48057=CARTESIAN_POINT('Ctrl Pts',(1.92821611252933,-0.794772684000853,
3.31565474374453));
#48058=CARTESIAN_POINT('Ctrl Pts',(1.90537613625137,-0.636309800095198,
3.36733137652309));
#48059=CARTESIAN_POINT('Ctrl Pts',(1.861761274782,-0.319434907277159,3.42732370528723));
#48060=CARTESIAN_POINT('Ctrl Pts',(1.84676876171031,-0.158333333333332,
3.44085260987035));
#48061=CARTESIAN_POINT('Ctrl Pts',(1.82785767731739,0.158333333333335,3.43169011688178));
#48062=CARTESIAN_POINT('Ctrl Pts',(1.82516531181488,0.319434907277167,3.40946043194975));
#48063=CARTESIAN_POINT('Ctrl Pts',(1.82776196305616,0.636309800095207,3.32986428928672));
#48064=CARTESIAN_POINT('Ctrl Pts',(1.82884049859466,0.794772684000843,3.26818649332466));
#48065=CARTESIAN_POINT('Ctrl Pts',(1.8594648678336,1.06847604194558,3.13670945384053));
#48066=CARTESIAN_POINT('Ctrl Pts',(1.87900001879695,1.1851427086127,3.07068436435281));
#48067=CARTESIAN_POINT('Ctrl Pts',(1.90481416602479,1.30000000000137,2.99554572406571));
#48068=CARTESIAN_POINT('Ctrl Pts',(2.09696957937698,-1.30000000000002,3.07210722196282));
#48069=CARTESIAN_POINT('Ctrl Pts',(2.05247729144278,-1.1851427086118,3.13516734031299));
#48070=CARTESIAN_POINT('Ctrl Pts',(2.01471700122407,-1.06847604194512,3.19021030643424));
#48071=CARTESIAN_POINT('Ctrl Pts',(1.94303543835297,-0.794772684000852,
3.29884934400734));
#48072=CARTESIAN_POINT('Ctrl Pts',(1.91850752763247,-0.636309800095198,
3.350202946425));
#48073=CARTESIAN_POINT('Ctrl Pts',(1.87507551772266,-0.31943490727716,3.41028477353073));
#48074=CARTESIAN_POINT('Ctrl Pts',(1.86111460420306,-0.158333333333332,
3.42552196248209));
#48075=CARTESIAN_POINT('Ctrl Pts',(1.84273788650679,0.158333333333335,3.4166882437844));
#48076=CARTESIAN_POINT('Ctrl Pts',(1.84035616299712,0.319434907277167,3.39355506649829));
#48077=CARTESIAN_POINT('Ctrl Pts',(1.84221284626722,0.636309800095207,3.31356950122377));
#48078=CARTESIAN_POINT('Ctrl Pts',(1.84204629899775,0.794772684000843,3.25053778242636));
#48079=CARTESIAN_POINT('Ctrl Pts',(1.87106471889265,1.06847604194558,3.12142528052509));
#48080=CARTESIAN_POINT('Ctrl Pts',(1.88986591440082,1.18514270861271,3.05724590643982));
#48081=CARTESIAN_POINT('Ctrl Pts',(1.91490730668305,1.30000000000137,2.98477517625274));
#48082=CARTESIAN_POINT('Ctrl Pts',(2.11058813200125,-1.30000000000002,3.06000397880413));
#48083=CARTESIAN_POINT('Ctrl Pts',(2.06838975835484,-1.1851427086118,3.12029349547214));
#48084=CARTESIAN_POINT('Ctrl Pts',(2.03210944478524,-1.06847604194513,3.17318478598011));
#48085=CARTESIAN_POINT('Ctrl Pts',(1.96196656526888,-0.794772684000854,
3.27828286548025));
#48086=CARTESIAN_POINT('Ctrl Pts',(1.93527184700814,-0.636309800095199,
3.32905154023907));
#48087=CARTESIAN_POINT('Ctrl Pts',(1.89129063602831,-0.31943490727716,3.38865386231255));
#48088=CARTESIAN_POINT('Ctrl Pts',(1.87801052102755,-0.158333333333333,
3.40566442232698));
#48089=CARTESIAN_POINT('Ctrl Pts',(1.85856089011937,0.158333333333335,3.39625770136831));
#48090=CARTESIAN_POINT('Ctrl Pts',(1.85373294313904,0.319434907277168,3.37042335719926));
#48091=CARTESIAN_POINT('Ctrl Pts',(1.85536397707056,0.636309800095208,3.29047282154238));
#48092=CARTESIAN_POINT('Ctrl Pts',(1.85848213792874,0.794772684000844,3.22857764871937));
#48093=CARTESIAN_POINT('Ctrl Pts',(1.88653846927129,1.06847604194558,3.10325347243792));
#48094=CARTESIAN_POINT('Ctrl Pts',(1.90409579177865,1.18514270861271,3.04132415698621));
#48095=CARTESIAN_POINT('Ctrl Pts',(1.92706589054469,1.30000000000137,2.97171371827676));
#48096=CARTESIAN_POINT('Ctrl Pts',(2.12535537170441,-1.30000000000002,3.0487948012942));
#48097=CARTESIAN_POINT('Ctrl Pts',(2.08510457409783,-1.1851427086118,3.10624984240559));
#48098=CARTESIAN_POINT('Ctrl Pts',(2.05000694414467,-1.06847604194513,3.15692071284892));
#48099=CARTESIAN_POINT('Ctrl Pts',(1.98082924586306,-0.794772684000853,
3.25830776883402));
#48100=CARTESIAN_POINT('Ctrl Pts',(1.9521414637683,-0.636309800095201,3.30859414238913));
#48101=CARTESIAN_POINT('Ctrl Pts',(1.9064880593285,-0.319434907277162,3.36708715701643));
#48102=CARTESIAN_POINT('Ctrl Pts',(1.89147447751587,-0.158333333333333,
3.38442963319047));
#48103=CARTESIAN_POINT('Ctrl Pts',(1.87173028908309,0.158333333333335,3.37489183848399));
#48104=CARTESIAN_POINT('Ctrl Pts',(1.86845863131722,0.319434907277168,3.34870687052084));
#48105=CARTESIAN_POINT('Ctrl Pts',(1.8709227717798,0.636309800095209,3.26936977284123));
#48106=CARTESIAN_POINT('Ctrl Pts',(1.87504632164862,0.794772684000847,3.20730369839696));
#48107=CARTESIAN_POINT('Ctrl Pts',(1.90170503351283,1.06847604194559,3.08531301579748));
#48108=CARTESIAN_POINT('Ctrl Pts',(1.91807197012133,1.18514270861271,3.02553340502337));
#48109=CARTESIAN_POINT('Ctrl Pts',(1.93926627477494,1.30000000000138,2.95877942977227));
#48110=CARTESIAN_POINT('Ctrl Pts',(2.14303983420993,-1.30000000000002,3.03242748668085));
#48111=CARTESIAN_POINT('Ctrl Pts',(2.10599477948638,-1.1851427086118,3.0864351878073));
#48112=CARTESIAN_POINT('Ctrl Pts',(2.07304606191122,-1.06847604194513,3.13446164902164));
#48113=CARTESIAN_POINT('Ctrl Pts',(2.00639129122644,-0.794772684000854,
3.23159452134748));
#48114=CARTESIAN_POINT('Ctrl Pts',(1.97578443836247,-0.6363098000952,3.28167480323916));
#48115=CARTESIAN_POINT('Ctrl Pts',(1.92883104153055,-0.319434907277161,
3.33921641080584));
#48116=CARTESIAN_POINT('Ctrl Pts',(1.91222223148185,-0.158333333333333,
3.35741115879828));
#48117=CARTESIAN_POINT('Ctrl Pts',(1.89156185596208,0.158333333333336,3.34736990639073));
#48118=CARTESIAN_POINT('Ctrl Pts',(1.88832568148489,0.319434907277169,3.31948156388352));
#48119=CARTESIAN_POINT('Ctrl Pts',(1.89153448823503,0.63630980009521,3.24077849406139));
#48120=CARTESIAN_POINT('Ctrl Pts',(1.89861717655721,0.794772684000847,3.17947682954823));
#48121=CARTESIAN_POINT('Ctrl Pts',(1.92358245481021,1.06847604194559,3.06216339058198));
#48122=CARTESIAN_POINT('Ctrl Pts',(1.93819516873417,1.18514270861271,3.00522745510929));
#48123=CARTESIAN_POINT('Ctrl Pts',(1.95661405268106,1.30000000000137,2.94213622500118));
#48124=CARTESIAN_POINT('Ctrl Pts',(2.16828207977002,-1.30000000000003,3.01421432900304));
#48125=CARTESIAN_POINT('Ctrl Pts',(2.13543077770946,-1.18514270861181,3.06412297603415));
#48126=CARTESIAN_POINT('Ctrl Pts',(2.10509779364543,-1.06847604194513,3.10885397352754));
#48127=CARTESIAN_POINT('Ctrl Pts',(2.04084035072463,-0.794772684000861,
3.20023011992529));
#48128=CARTESIAN_POINT('Ctrl Pts',(2.0062449787379,-0.636309800095203,3.24892252893296));
#48129=CARTESIAN_POINT('Ctrl Pts',(1.95650440827287,-0.319434907277161,
3.30449298344116));
#48130=CARTESIAN_POINT('Ctrl Pts',(1.93721902666464,-0.158333333333334,
3.32334251722877));
#48131=CARTESIAN_POINT('Ctrl Pts',(1.91605012504035,0.158333333333336,3.31304233970309));
#48132=CARTESIAN_POINT('Ctrl Pts',(1.9152582443003,0.319434907277173,3.28448329445562));
#48133=CARTESIAN_POINT('Ctrl Pts',(1.91965569576352,0.636309800095215,3.20672897571828));
#48134=CARTESIAN_POINT('Ctrl Pts',(1.92845845189327,0.794772684000848,3.14523263031291));
#48135=CARTESIAN_POINT('Ctrl Pts',(1.95058534406668,1.06847604194559,3.03324878049766));
#48136=CARTESIAN_POINT('Ctrl Pts',(1.96289276371449,1.18514270861272,2.9797377029536));
#48137=CARTESIAN_POINT('Ctrl Pts',(1.97792969127037,1.30000000000138,2.92118920704003));
#48138=CARTESIAN_POINT('Ctrl Pts',(2.19672991623476,-1.30000000000003,2.99108833318567));
#48139=CARTESIAN_POINT('Ctrl Pts',(2.16869424276217,-1.18514270861181,3.03588762958137));
#48140=CARTESIAN_POINT('Ctrl Pts',(2.14173379281298,-1.06847604194513,3.07677957866654));
#48141=CARTESIAN_POINT('Ctrl Pts',(2.08193374144757,-0.794772684000858,
3.16222140751015));
#48142=CARTESIAN_POINT('Ctrl Pts',(2.04588339614435,-0.636309800095203,
3.21145553758907));
#48143=CARTESIAN_POINT('Ctrl Pts',(1.99433386989076,-0.319434907277162,
3.26559008542051));
#48144=CARTESIAN_POINT('Ctrl Pts',(1.97120200673784,-0.158333333333334,
3.28468906039049));
#48145=CARTESIAN_POINT('Ctrl Pts',(1.94875210217719,0.158333333333337,3.27360352254155));
#48146=CARTESIAN_POINT('Ctrl Pts',(1.94973138469771,0.319434907277174,3.24353820867032));
#48147=CARTESIAN_POINT('Ctrl Pts',(1.95494644437421,0.636309800095217,3.16658041875194));
#48148=CARTESIAN_POINT('Ctrl Pts',(1.96652411484811,0.794772684000849,3.10532686289807));
#48149=CARTESIAN_POINT('Ctrl Pts',(1.98460432652983,1.06847604194559,2.99942775676767));
#48150=CARTESIAN_POINT('Ctrl Pts',(1.99364914302969,1.18514270861272,2.94976483985142));
#48151=CARTESIAN_POINT('Ctrl Pts',(2.00391252233024,1.30000000000138,2.89627880511424));
#48152=CARTESIAN_POINT('Ctrl Pts',(2.22228736155764,-1.30000000000004,2.97318805622785));
#48153=CARTESIAN_POINT('Ctrl Pts',(2.19878628984836,-1.18514270861181,3.01411939305874));
#48154=CARTESIAN_POINT('Ctrl Pts',(2.17483352473068,-1.06847604194514,3.05196497398288));
#48155=CARTESIAN_POINT('Ctrl Pts',(2.11845434344017,-0.794772684000864,
3.13226712345224));
#48156=CARTESIAN_POINT('Ctrl Pts',(2.07921732493002,-0.636309800095207,
3.18056046380941));
#48157=CARTESIAN_POINT('Ctrl Pts',(2.02610306617644,-0.319434907277164,
3.23340259317279));
#48158=CARTESIAN_POINT('Ctrl Pts',(2.00139690559124,-0.158333333333335,
3.25376618423287));
#48159=CARTESIAN_POINT('Ctrl Pts',(1.97837829254599,0.158333333333337,3.24233776287423));
#48160=CARTESIAN_POINT('Ctrl Pts',(1.98052143462657,0.319434907277174,3.21081772473499));
#48161=CARTESIAN_POINT('Ctrl Pts',(1.98582042272674,0.636309800095218,3.13414273191321));
#48162=CARTESIAN_POINT('Ctrl Pts',(1.99860964659895,0.794772684000852,3.07240526593313));
#48163=CARTESIAN_POINT('Ctrl Pts',(2.01319306797143,1.0684760419456,2.97147652148233));
#48164=CARTESIAN_POINT('Ctrl Pts',(2.01971052024537,1.18514270861273,2.92512583728176));
#48165=CARTESIAN_POINT('Ctrl Pts',(2.02643280205011,1.3000000000014,2.87611278257491));
#48166=CARTESIAN_POINT('Ctrl Pts',(2.24737536599506,-1.30000000000005,2.95499905098216));
#48167=CARTESIAN_POINT('Ctrl Pts',(2.2286045590397,-1.18514270861182,2.99223335401397));
#48168=CARTESIAN_POINT('Ctrl Pts',(2.20792711755062,-1.06847604194515,3.02723798283389));
#48169=CARTESIAN_POINT('Ctrl Pts',(2.15575338400896,-0.79477268400087,3.10295468458563));
#48170=CARTESIAN_POINT('Ctrl Pts',(2.11462868360512,-0.636309800095211,
3.15115911964104));
#48171=CARTESIAN_POINT('Ctrl Pts',(2.05987426195789,-0.319434907277165,
3.20261922855258));
#48172=CARTESIAN_POINT('Ctrl Pts',(2.03202581413481,-0.158333333333336,
3.22314257767777));
#48173=CARTESIAN_POINT('Ctrl Pts',(2.00803959240179,0.158333333333338,3.21106609562426));
#48174=CARTESIAN_POINT('Ctrl Pts',(2.01188908814568,0.319434907277175,3.17845166474377));
#48175=CARTESIAN_POINT('Ctrl Pts',(2.01781123398656,0.636309800095221,3.10242236996614));
#48176=CARTESIAN_POINT('Ctrl Pts',(2.03278417415428,0.794772684000857,3.04086896994047));
#48177=CARTESIAN_POINT('Ctrl Pts',(2.04347808426441,1.0684760419456,2.94466595306606));
#48178=CARTESIAN_POINT('Ctrl Pts',(2.04696960309575,1.18514270861273,2.90130214713938));
#48179=CARTESIAN_POINT('Ctrl Pts',(2.04932364332018,1.3000000000014,2.85621725661796));
#48180=CARTESIAN_POINT('Ctrl Pts',(2.26798132103125,-1.30000000000005,2.9408473417646));
#48181=CARTESIAN_POINT('Ctrl Pts',(2.25255110305297,-1.18514270861183,2.97478060009054));
#48182=CARTESIAN_POINT('Ctrl Pts',(2.23415159110123,-1.06847604194515,3.00725190803789));
#48183=CARTESIAN_POINT('Ctrl Pts',(2.18478537459899,-0.794772684000873,
3.07888972742241));
#48184=CARTESIAN_POINT('Ctrl Pts',(2.14170408572716,-0.636309800095214,
3.1267431070186));
#48185=CARTESIAN_POINT('Ctrl Pts',(2.08629851241369,-0.319434907277168,
3.17757100674675));
#48186=CARTESIAN_POINT('Ctrl Pts',(2.05739580921471,-0.158333333333336,
3.19924659455908));
#48187=CARTESIAN_POINT('Ctrl Pts',(2.03368395533952,0.158333333333339,3.18738275794237));
#48188=CARTESIAN_POINT('Ctrl Pts',(2.03937689580979,0.319434907277175,3.15421146313419));
#48189=CARTESIAN_POINT('Ctrl Pts',(2.04546040657606,0.636309800095223,3.07846792891086));
#48190=CARTESIAN_POINT('Ctrl Pts',(2.06060576749126,0.794772684000864,3.01599273531813));
#48191=CARTESIAN_POINT('Ctrl Pts',(2.0678307030203,1.06847604194561,2.9233141761816));
#48192=CARTESIAN_POINT('Ctrl Pts',(2.06900714824849,1.18514270861274,2.88240299534151));
#48193=CARTESIAN_POINT('Ctrl Pts',(2.0682326318246,1.3000000000014,2.84069774783254));
#48194=CARTESIAN_POINT('Ctrl Pts',(2.28890432978042,-1.30000000000006,2.92700191529698));
#48195=CARTESIAN_POINT('Ctrl Pts',(2.27802478124005,-1.18514270861183,2.95858349693434));
#48196=CARTESIAN_POINT('Ctrl Pts',(2.26275140213339,-1.06847604194516,2.98917562005717));
#48197=CARTESIAN_POINT('Ctrl Pts',(2.21731621337705,-0.794772684000877,
3.05756369729516));
#48198=CARTESIAN_POINT('Ctrl Pts',(2.17220848809185,-0.636309800095215,
3.10489338359369));
#48199=CARTESIAN_POINT('Ctrl Pts',(2.11513145228693,-0.319434907277167,
3.1542889853963));
#48200=CARTESIAN_POINT('Ctrl Pts',(2.08349683499688,-0.158333333333337,
3.17588196355153));
#48201=CARTESIAN_POINT('Ctrl Pts',(2.05842347363757,0.158333333333339,3.16306052982064));
#48202=CARTESIAN_POINT('Ctrl Pts',(2.06475605343639,0.319434907277179,3.12853903953918));
#48203=CARTESIAN_POINT('Ctrl Pts',(2.07122625430981,0.636309800095227,3.05324521138199));
#48204=CARTESIAN_POINT('Ctrl Pts',(2.08909517719549,0.794772684000863,2.99160015978278));
#48205=CARTESIAN_POINT('Ctrl Pts',(2.09300977471158,1.06847604194561,2.90256984400533));
#48206=CARTESIAN_POINT('Ctrl Pts',(2.09145710151166,1.18514270861274,2.86383573850736));
#48207=CARTESIAN_POINT('Ctrl Pts',(2.08665727089726,1.30000000000141,2.82490545231324));
#48208=CARTESIAN_POINT('Ctrl Pts',(2.30431755283692,-1.30000000000007,2.91638984227385));
#48209=CARTESIAN_POINT('Ctrl Pts',(2.29571829012651,-1.18514270861184,2.94533448550776));
#48210=CARTESIAN_POINT('Ctrl Pts',(2.28213591612243,-1.06847604194516,2.9740169693766));
#48211=CARTESIAN_POINT('Ctrl Pts',(2.23924593107205,-0.79477268400088,3.03967360444674));
#48212=CARTESIAN_POINT('Ctrl Pts',(2.19413283193249,-0.63630980009522,3.087819634541));
#48213=CARTESIAN_POINT('Ctrl Pts',(2.13677609077595,-0.319434907277171,
3.13688315664733));
#48214=CARTESIAN_POINT('Ctrl Pts',(2.10328576819757,-0.158333333333338,
3.15853623876091));
#48215=CARTESIAN_POINT('Ctrl Pts',(2.07816984202021,0.15833333333334,3.14567657626547));
#48216=CARTESIAN_POINT('Ctrl Pts',(2.08643904656091,0.319434907277178,3.11113745708857));
#48217=CARTESIAN_POINT('Ctrl Pts',(2.09285072274629,0.636309800095229,3.0359334515012));
#48218=CARTESIAN_POINT('Ctrl Pts',(2.11011916058644,0.79477268400087,2.97309367718847));
#48219=CARTESIAN_POINT('Ctrl Pts',(2.11124730556027,1.06847604194562,2.88656806265442));
#48220=CARTESIAN_POINT('Ctrl Pts',(2.10799714327054,1.18514270861275,2.84969292888836));
#48221=CARTESIAN_POINT('Ctrl Pts',(2.1010084865338,1.30000000000142,2.81339639379812));
#48222=CARTESIAN_POINT('Ctrl Pts',(2.31848178810538,-1.30000000000007,2.90674308074662));
#48223=CARTESIAN_POINT('Ctrl Pts',(2.31330948407002,-1.18514270861184,2.93431605064516));
#48224=CARTESIAN_POINT('Ctrl Pts',(2.30203462419369,-1.06847604194517,2.96183803201959));
#48225=CARTESIAN_POINT('Ctrl Pts',(2.26188931754665,-0.794772684000884,
3.02530152105712));
#48226=CARTESIAN_POINT('Ctrl Pts',(2.21458477884655,-0.636309800095223,
3.07247131282959));
#48227=CARTESIAN_POINT('Ctrl Pts',(2.15632375272408,-0.319434907277172,
3.1207021557373));
#48228=CARTESIAN_POINT('Ctrl Pts',(2.12186104592459,-0.158333333333339,
3.14294161679127));
#48229=CARTESIAN_POINT('Ctrl Pts',(2.09638240425404,0.158333333333341,3.12982658281625));
#48230=CARTESIAN_POINT('Ctrl Pts',(2.10526842822162,0.319434907277182,3.0944851345404));
#48231=CARTESIAN_POINT('Ctrl Pts',(2.11183099857077,0.636309800095233,3.01951333644257));
#48232=CARTESIAN_POINT('Ctrl Pts',(2.13034374854833,0.794772684000874,2.95681777120825));
#48233=CARTESIAN_POINT('Ctrl Pts',(2.12900406616482,1.06847604194562,2.87265018646151));
#48234=CARTESIAN_POINT('Ctrl Pts',(2.12388559097138,1.18514270861275,2.83726416304824));
#48235=CARTESIAN_POINT('Ctrl Pts',(2.1142285394482,1.30000000000142,2.80292514494225));
#48236=CARTESIAN_POINT('Ctrl Pts',(2.33500443641727,-1.30000000000007,2.89700892416184));
#48237=CARTESIAN_POINT('Ctrl Pts',(2.33230791385509,-1.18514270861185,2.92211467057017));
#48238=CARTESIAN_POINT('Ctrl Pts',(2.32283266395042,-1.06847604194517,2.94782140171622));
#48239=CARTESIAN_POINT('Ctrl Pts',(2.28528272491246,-0.794772684000888,
3.00859748824829));
#48240=CARTESIAN_POINT('Ctrl Pts',(2.23767755759602,-0.636309800095224,
3.05633197853381));
#48241=CARTESIAN_POINT('Ctrl Pts',(2.17894957675327,-0.319434907277171,
3.10406117509063));
#48242=CARTESIAN_POINT('Ctrl Pts',(2.14287631687027,-0.158333333333339,
3.12650800835465));
#48243=CARTESIAN_POINT('Ctrl Pts',(2.1166387623548,0.158333333333341,3.11282772068504));
#48244=CARTESIAN_POINT('Ctrl Pts',(2.12582711643291,0.319434907277181,3.07631724695481));
#48245=CARTESIAN_POINT('Ctrl Pts',(2.13242969586,0.636309800095233,3.00150315147276));
#48246=CARTESIAN_POINT('Ctrl Pts',(2.15256245994101,0.794772684000874,2.93918498086401));
#48247=CARTESIAN_POINT('Ctrl Pts',(2.14865882357122,1.06847604194562,2.85768077878978));
#48248=CARTESIAN_POINT('Ctrl Pts',(2.14154726099493,1.18514270861275,2.82394538145764));
#48249=CARTESIAN_POINT('Ctrl Pts',(2.12901387538286,1.30000000000142,2.79175473584303));
#48250=CARTESIAN_POINT('Ctrl Pts',(2.35046299219406,-1.30000000000009,2.88651938390127));
#48251=CARTESIAN_POINT('Ctrl Pts',(2.35145434254997,-1.18514270861186,2.91010471870674));
#48252=CARTESIAN_POINT('Ctrl Pts',(2.3444785009304,-1.06847604194518,2.93454070194135));
#48253=CARTESIAN_POINT('Ctrl Pts',(2.30995710398222,-0.794772684000892,
2.99295787965795));
#48254=CARTESIAN_POINT('Ctrl Pts',(2.25996266540508,-0.636309800095232,
3.0396171500443));
#48255=CARTESIAN_POINT('Ctrl Pts',(2.20065327861454,-0.319434907277177,
3.08672816750844));
#48256=CARTESIAN_POINT('Ctrl Pts',(2.16393187965731,-0.158333333333341,
3.11011708054026));
#48257=CARTESIAN_POINT('Ctrl Pts',(2.13799717022496,0.158333333333343,3.09665644543285));
#48258=CARTESIAN_POINT('Ctrl Pts',(2.1487758192993,0.319434907277185,3.05991842617207));
#48259=CARTESIAN_POINT('Ctrl Pts',(2.15527444815603,0.636309800095241,2.98516188789695));
#48260=CARTESIAN_POINT('Ctrl Pts',(2.17518339819993,0.794772684000885,2.9218796799385));
#48261=CARTESIAN_POINT('Ctrl Pts',(2.16799220827574,1.06847604194564,2.84250895998002));
#48262=CARTESIAN_POINT('Ctrl Pts',(2.15878722815583,1.18514270861277,2.81034848034886));
#48263=CARTESIAN_POINT('Ctrl Pts',(2.14349006757434,1.30000000000144,2.78038416478162));
#48264=CARTESIAN_POINT('Ctrl Pts',(2.36783505325599,-1.3000000000001,2.87561679699127));
#48265=CARTESIAN_POINT('Ctrl Pts',(2.37177397284949,-1.18514270861187,2.89674501502257));
#48266=CARTESIAN_POINT('Ctrl Pts',(2.36698852169671,-1.06847604194519,2.9194078754243));
#48267=CARTESIAN_POINT('Ctrl Pts',(2.3357781304793,-0.794772684000901,2.97530894752189));
#48268=CARTESIAN_POINT('Ctrl Pts',(2.28588906471611,-0.636309800095238,
3.02291294353573));
#48269=CARTESIAN_POINT('Ctrl Pts',(2.22609023343301,-0.319434907277179,
3.06948140221203));
#48270=CARTESIAN_POINT('Ctrl Pts',(2.18708241423167,-0.158333333333342,
3.09265489349129));
#48271=CARTESIAN_POINT('Ctrl Pts',(2.16014363050186,0.158333333333345,3.07842918311708));
#48272=CARTESIAN_POINT('Ctrl Pts',(2.17147580504844,0.319434907277187,3.04060014268787));
#48273=CARTESIAN_POINT('Ctrl Pts',(2.17790320617912,0.636309800095247,2.96593048690121));
#48274=CARTESIAN_POINT('Ctrl Pts',(2.19924803217963,0.794772684000892,2.90282809369987));
#48275=CARTESIAN_POINT('Ctrl Pts',(2.18916697066081,1.06847604194565,2.82625170081662));
#48276=CARTESIAN_POINT('Ctrl Pts',(2.17780279283653,1.18514270861278,2.79587273566341));
#48277=CARTESIAN_POINT('Ctrl Pts',(2.15943815517932,1.30000000000145,2.76826188840121));
#48278=CARTESIAN_POINT('Ctrl Pts',(2.38159818278248,-1.30000000000011,2.86757732560228));
#48279=CARTESIAN_POINT('Ctrl Pts',(2.38835803633944,-1.18514270861188,2.88726709648415));
#48280=CARTESIAN_POINT('Ctrl Pts',(2.3855241128328,-1.0684760419452,2.90878487398856));
#48281=CARTESIAN_POINT('Ctrl Pts',(2.35681363836256,-0.794772684000908,
2.96271830562995));
#48282=CARTESIAN_POINT('Ctrl Pts',(2.30561969519472,-0.636309800095244,
3.00993767690273));
#48283=CARTESIAN_POINT('Ctrl Pts',(2.2451591336905,-0.319434907277183,3.0558452560672));
#48284=CARTESIAN_POINT('Ctrl Pts',(2.20483064420271,-0.158333333333344,
3.07919353570339));
#48285=CARTESIAN_POINT('Ctrl Pts',(2.17777050754538,0.158333333333346,3.06486001802799));
#48286=CARTESIAN_POINT('Ctrl Pts',(2.19038774253737,0.31943490727719,3.02682434733364));
#48287=CARTESIAN_POINT('Ctrl Pts',(2.19705503421999,0.636309800095253,2.95244123931286));
#48288=CARTESIAN_POINT('Ctrl Pts',(2.21911081285458,0.7947726840009,2.88919402976588));
#48289=CARTESIAN_POINT('Ctrl Pts',(2.20633210372423,1.06847604194566,2.81441474453547));
#48290=CARTESIAN_POINT('Ctrl Pts',(2.19304428398507,1.18514270861279,2.78520929392479));
#48291=CARTESIAN_POINT('Ctrl Pts',(2.17200007419145,1.30000000000147,2.75916757443416));
#48292=CARTESIAN_POINT('Ctrl Pts',(2.39241281507888,-1.30000000000012,2.86099299160901));
#48293=CARTESIAN_POINT('Ctrl Pts',(2.40123064389783,-1.18514270861188,2.87937186881187));
#48294=CARTESIAN_POINT('Ctrl Pts',(2.39987122314209,-1.0684760419452,2.89990398789257));
#48295=CARTESIAN_POINT('Ctrl Pts',(2.3732192067758,-0.794772684000911,2.95231170989772));
#48296=CARTESIAN_POINT('Ctrl Pts',(2.32158734929061,-0.636309800095245,
2.99971220851892));
#48297=CARTESIAN_POINT('Ctrl Pts',(2.26067097336819,-0.319434907277183,
3.0451546597403));
#48298=CARTESIAN_POINT('Ctrl Pts',(2.21892702187026,-0.158333333333344,
3.06835588462233));
#48299=CARTESIAN_POINT('Ctrl Pts',(2.19158252580981,0.158333333333347,3.05379481700059));
#48300=CARTESIAN_POINT('Ctrl Pts',(2.20515161001715,0.319434907277191,3.01554709154152));
#48301=CARTESIAN_POINT('Ctrl Pts',(2.21206062274055,0.636309800095254,2.94143358598389));
#48302=CARTESIAN_POINT('Ctrl Pts',(2.23491733512154,0.794772684000901,2.87824270878038));
#48303=CARTESIAN_POINT('Ctrl Pts',(2.22007525929973,1.06847604194566,2.80496768584344));
#48304=CARTESIAN_POINT('Ctrl Pts',(2.20526040309828,1.18514270861279,2.7767071039221));
#48305=CARTESIAN_POINT('Ctrl Pts',(2.18205527536554,1.30000000000147,2.75190398240171));
#48306=CARTESIAN_POINT('Ctrl Pts',(2.40075906139621,-1.30000000000012,2.85625494698041));
#48307=CARTESIAN_POINT('Ctrl Pts',(2.41130761398963,-1.18514270861189,2.87381149743691));
#48308=CARTESIAN_POINT('Ctrl Pts',(2.41113847876893,-1.0684760419452,2.89367775466536));
#48309=CARTESIAN_POINT('Ctrl Pts',(2.38598773965703,-0.794772684000912,
2.94490866779268));
#48310=CARTESIAN_POINT('Ctrl Pts',(2.33345265229072,-0.636309800095246,
2.99196672747374));
#48311=CARTESIAN_POINT('Ctrl Pts',(2.27218838688196,-0.319434907277184,
3.03704260315317));
#48312=CARTESIAN_POINT('Ctrl Pts',(2.22992098264959,-0.158333333333345,
3.06055543823259));
#48313=CARTESIAN_POINT('Ctrl Pts',(2.20237774376518,0.158333333333347,3.04583547575045));
#48314=CARTESIAN_POINT('Ctrl Pts',(2.21631914337816,0.319434907277191,3.00716395179031));
#48315=CARTESIAN_POINT('Ctrl Pts',(2.22307425179954,0.636309800095255,2.93299822649179));
#48316=CARTESIAN_POINT('Ctrl Pts',(2.24616935156192,0.794772684000903,2.86958107124942));
#48317=CARTESIAN_POINT('Ctrl Pts',(2.22982669049922,1.06847604194566,2.79746816906829));
#48318=CARTESIAN_POINT('Ctrl Pts',(2.21400070184457,1.1851427086128,2.77001568706186));
#48319=CARTESIAN_POINT('Ctrl Pts',(2.18942285695403,1.30000000000147,2.74632572635692));
#48320=CARTESIAN_POINT('Ctrl Pts',(2.40704602554912,-1.30000000000012,2.85272853528918));
#48321=CARTESIAN_POINT('Ctrl Pts',(2.41894744732919,-1.18514270861189,2.86971428113638));
#48322=CARTESIAN_POINT('Ctrl Pts',(2.41970481574944,-1.06847604194521,2.88910946594559));
#48323=CARTESIAN_POINT('Ctrl Pts',(2.39570949568987,-0.794772684000916,
2.93948250885712));
#48324=CARTESIAN_POINT('Ctrl Pts',(2.34242210867447,-0.636309800095249,
2.98622271392694));
#48325=CARTESIAN_POINT('Ctrl Pts',(2.2808968417526,-0.319434907277185,3.03102043769811));
#48326=CARTESIAN_POINT('Ctrl Pts',(2.23828433805704,-0.158333333333345,
3.05480036444708));
#48327=CARTESIAN_POINT('Ctrl Pts',(2.21060493512933,0.158333333333347,3.03996945789718));
#48328=CARTESIAN_POINT('Ctrl Pts',(2.22481883476239,0.319434907277193,3.00097592096811));
#48329=CARTESIAN_POINT('Ctrl Pts',(2.23142811183105,0.636309800095258,2.92674824815461));
#48330=CARTESIAN_POINT('Ctrl Pts',(2.25465858662683,0.794772684000906,2.86312947009923));
#48331=CARTESIAN_POINT('Ctrl Pts',(2.23715641304854,1.06847604194567,2.791861217171));
#48332=CARTESIAN_POINT('Ctrl Pts',(2.2205612568082,1.1851427086128,2.76500566347436));
#48333=CARTESIAN_POINT('Ctrl Pts',(2.19494698675012,1.30000000000148,2.74214394202474));
#48334=CARTESIAN_POINT('Ctrl Pts',(2.41117858829815,-1.30000000000012,2.85032932948442));
#48335=CARTESIAN_POINT('Ctrl Pts',(2.42391523248741,-1.18514270861189,2.86687924818083));
#48336=CARTESIAN_POINT('Ctrl Pts',(2.42526239159974,-1.06847604194521,2.88593731788189));
#48337=CARTESIAN_POINT('Ctrl Pts',(2.40206260966107,-0.794772684000917,
2.93575960201975));
#48338=CARTESIAN_POINT('Ctrl Pts',(2.34848943910999,-0.63630980009525,2.98246672345806));
#48339=CARTESIAN_POINT('Ctrl Pts',(2.28681527120289,-0.319434907277185,
3.02710086613297));
#48340=CARTESIAN_POINT('Ctrl Pts',(2.24380722851281,-0.158333333333345,
3.05092454534281));
#48341=CARTESIAN_POINT('Ctrl Pts',(2.21603686091174,0.158333333333348,3.03601765840459));
#48342=CARTESIAN_POINT('Ctrl Pts',(2.23053779170613,0.319434907277193,2.99689268376164));
#48343=CARTESIAN_POINT('Ctrl Pts',(2.23714641542351,0.636309800095258,2.92269766743079));
#48344=CARTESIAN_POINT('Ctrl Pts',(2.26057947518346,0.794772684000906,2.85902842483262));
#48345=CARTESIAN_POINT('Ctrl Pts',(2.24225976029705,1.06847604194567,2.78828978216868));
#48346=CARTESIAN_POINT('Ctrl Pts',(2.22509138163621,1.1851427086128,2.76178669639393));
#48347=CARTESIAN_POINT('Ctrl Pts',(2.19868455007652,1.30000000000148,2.73940066212868));
#48348=CARTESIAN_POINT('Ctrl Pts',(2.41323520827443,-1.30000000000012,2.84912189739511));
#48349=CARTESIAN_POINT('Ctrl Pts',(2.42637973947482,-1.18514270861189,2.86544585475509));
#48350=CARTESIAN_POINT('Ctrl Pts',(2.42801799749355,-1.06847604194521,2.88433223279753));
#48351=CARTESIAN_POINT('Ctrl Pts',(2.40522090837747,-0.794772684000917,
2.93388324866955));
#48352=CARTESIAN_POINT('Ctrl Pts',(2.35153877693122,-0.63630980009525,2.98060189844466));
#48353=CARTESIAN_POINT('Ctrl Pts',(2.28979444325212,-0.319434907277186,
3.02515797836937));
#48354=CARTESIAN_POINT('Ctrl Pts',(2.24656293042211,-0.158333333333345,
3.04898273817961));
#48355=CARTESIAN_POINT('Ctrl Pts',(2.21874670178875,0.158333333333348,3.03403728268168));
#48356=CARTESIAN_POINT('Ctrl Pts',(2.23340643548609,0.319434907277193,2.99485864798279));
#48357=CARTESIAN_POINT('Ctrl Pts',(2.24003011623958,0.636309800095259,2.92069167220904));
#48358=CARTESIAN_POINT('Ctrl Pts',(2.26358389234128,0.794772684000907,2.85701171734795));
#48359=CARTESIAN_POINT('Ctrl Pts',(2.2448487877729,1.06847604194567,2.78653279237346));
#48360=CARTESIAN_POINT('Ctrl Pts',(2.22738418251441,1.1851427086128,2.76019864061975));
#48361=CARTESIAN_POINT('Ctrl Pts',(2.20056470456104,1.30000000000148,2.73803805223228));
#48362=CARTESIAN_POINT('Ctrl Pts',(2.4149416938484,-1.30000000000013,2.84810972283032));
#48363=CARTESIAN_POINT('Ctrl Pts',(2.42841761794733,-1.18514270861189,2.86423837624598));
#48364=CARTESIAN_POINT('Ctrl Pts',(2.43029499764378,-1.06847604194521,2.8829788474371));
#48365=CARTESIAN_POINT('Ctrl Pts',(2.40783716246048,-0.794772684000917,
2.93230690646064));
#48366=CARTESIAN_POINT('Ctrl Pts',(2.35409241215596,-0.63630980009525,2.979058445274));
#48367=CARTESIAN_POINT('Ctrl Pts',(2.29229354863594,-0.319434907277186,
3.02355285427215));
#48368=CARTESIAN_POINT('Ctrl Pts',(2.24885541735091,-0.158333333333345,
3.04736198846237));
#48369=CARTESIAN_POINT('Ctrl Pts',(2.22100066370134,0.158333333333348,3.03238391154703));
#48370=CARTESIAN_POINT('Ctrl Pts',(2.23580464062873,0.319434907277193,2.99316995187068));
#48371=CARTESIAN_POINT('Ctrl Pts',(2.24245295969698,0.636309800095259,2.91903553476513));
#48372=CARTESIAN_POINT('Ctrl Pts',(2.26612261002616,0.794772684000907,2.8553580721882));
#48373=CARTESIAN_POINT('Ctrl Pts',(2.24703633876835,1.06847604194567,2.78509170502467));
#48374=CARTESIAN_POINT('Ctrl Pts',(2.22931744509398,1.1851427086128,2.75889267576204));
#48375=CARTESIAN_POINT('Ctrl Pts',(2.20214139735672,1.30000000000148,2.73691032395644));
#48376=CARTESIAN_POINT('Ctrl Pts',(2.41613364838208,-1.30000000000013,2.84739916316315));
#48377=CARTESIAN_POINT('Ctrl Pts',(2.42983902368031,-1.18514270861189,2.86338905532675));
#48378=CARTESIAN_POINT('Ctrl Pts',(2.43188288087058,-1.06847604194521,2.88202666611246));
#48379=CARTESIAN_POINT('Ctrl Pts',(2.40966416014421,-0.794772684000917,
2.93120003516014));
#48380=CARTESIAN_POINT('Ctrl Pts',(2.35588459500443,-0.63630980009525,2.9779820160423));
#48381=CARTESIAN_POINT('Ctrl Pts',(2.29404984138118,-0.319434907277186,
3.02243513731673));
#48382=CARTESIAN_POINT('Ctrl Pts',(2.25046223374693,-0.158333333333345,
3.04622938508356));
#48383=CARTESIAN_POINT('Ctrl Pts',(2.22258049616417,0.158333333333348,3.03122837281821));
#48384=CARTESIAN_POINT('Ctrl Pts',(2.23748735745911,0.319434907277193,2.99199117955593));
#48385=CARTESIAN_POINT('Ctrl Pts',(2.24415654248457,0.636309800095259,2.91788226257516));
#48386=CARTESIAN_POINT('Ctrl Pts',(2.26791354297215,0.794772684000907,2.85421125792459));
#48387=CARTESIAN_POINT('Ctrl Pts',(2.24858007637575,1.06847604194567,2.78409253961979));
#48388=CARTESIAN_POINT('Ctrl Pts',(2.23068071130597,1.1851427086128,2.75798616747606));
#48389=CARTESIAN_POINT('Ctrl Pts',(2.20325072248047,1.30000000000148,2.73612521818825));
#48390=CARTESIAN_POINT('Ctrl Pts',(2.41681457200604,-1.30000000000013,2.84699299207084));
#48391=CARTESIAN_POINT('Ctrl Pts',(2.43065041876023,-1.18514270861189,2.86290307521796));
#48392=CARTESIAN_POINT('Ctrl Pts',(2.43278914516079,-1.06847604194521,2.88148170329692));
#48393=CARTESIAN_POINT('Ctrl Pts',(2.41070734297901,-0.794772684000917,
2.93056692343428));
#48394=CARTESIAN_POINT('Ctrl Pts',(2.35691009009076,-0.63630980009525,2.97736811556787));
#48395=CARTESIAN_POINT('Ctrl Pts',(2.29505499304316,-0.319434907277186,
3.02179777530637));
#48396=CARTESIAN_POINT('Ctrl Pts',(2.25138012750943,-0.158333333333345,
3.04558200006546));
#48397=CARTESIAN_POINT('Ctrl Pts',(2.22348289215596,0.158333333333348,3.03056778556771));
#48398=CARTESIAN_POINT('Ctrl Pts',(2.2384498897554,0.319434907277193,2.99131837933657));
#48399=CARTESIAN_POINT('Ctrl Pts',(2.2451315272552,0.636309800095259,2.91722443298138));
#48400=CARTESIAN_POINT('Ctrl Pts',(2.26893823935086,0.794772684000907,2.85355694387179));
#48401=CARTESIAN_POINT('Ctrl Pts',(2.24946333436203,1.06847604194567,2.78352243917053));
#48402=CARTESIAN_POINT('Ctrl Pts',(2.23146070973882,1.1851427086128,2.75746890576994));
#48403=CARTESIAN_POINT('Ctrl Pts',(2.20388542524573,1.30000000000148,2.73567718101984));
#48404=CARTESIAN_POINT('Ctrl Pts',(2.42803368628124,-1.30000000000011,2.84027846919267));
#48405=CARTESIAN_POINT('Ctrl Pts',(2.44402065915128,-1.18514270861188,2.85487052201608));
#48406=CARTESIAN_POINT('Ctrl Pts',(2.44772572745999,-1.0684760419452,2.872476855943));
#48407=CARTESIAN_POINT('Ctrl Pts',(2.42791151992621,-0.794772684000911,
2.92011460180321));
#48408=CARTESIAN_POINT('Ctrl Pts',(2.37383452031449,-0.636309800095245,
2.9672424416972));
#48409=CARTESIAN_POINT('Ctrl Pts',(2.31166562520256,-0.319434907277183,
3.01130282976078));
#48410=CARTESIAN_POINT('Ctrl Pts',(2.26657616089764,-0.158333333333344,
3.03494229696348));
#48411=CARTESIAN_POINT('Ctrl Pts',(2.23842584648046,0.158333333333346,3.01971249569558));
#48412=CARTESIAN_POINT('Ctrl Pts',(2.25434823525271,0.31943490727719,2.98023224163553));
#48413=CARTESIAN_POINT('Ctrl Pts',(2.26124803596978,0.636309800095253,2.90639437862457));
#48414=CARTESIAN_POINT('Ctrl Pts',(2.28594188468099,0.7947726840009,2.84283632170469));
#48415=CARTESIAN_POINT('Ctrl Pts',(2.26412910545058,1.06847604194566,2.77418730483049));
#48416=CARTESIAN_POINT('Ctrl Pts',(2.24440574900138,1.18514270861279,2.74899209209798));
#48417=CARTESIAN_POINT('Ctrl Pts',(2.21440097998873,1.30000000000147,2.72831728234109));
#48418=CARTESIAN_POINT('Ctrl Pts',(2.44524045743472,-1.30000000000006,2.8310296558097));
#48419=CARTESIAN_POINT('Ctrl Pts',(2.46485368041197,-1.18514270861183,2.84409064111044));
#48420=CARTESIAN_POINT('Ctrl Pts',(2.47109329270799,-1.06847604194516,2.86047382708478));
#48421=CARTESIAN_POINT('Ctrl Pts',(2.45461232928673,-0.794772684000878,
2.90599721229061));
#48422=CARTESIAN_POINT('Ctrl Pts',(2.39901041965485,-0.636309800095217,
2.95266860365645));
#48423=CARTESIAN_POINT('Ctrl Pts',(2.33621994369784,-0.319434907277169,
2.99602953340761));
#48424=CARTESIAN_POINT('Ctrl Pts',(2.28982481036253,-0.158333333333337,
3.02005838856858));
#48425=CARTESIAN_POINT('Ctrl Pts',(2.26120820172365,0.158333333333339,3.00443113808546));
#48426=CARTESIAN_POINT('Ctrl Pts',(2.27811655282629,0.319434907277176,2.96428675721951));
#48427=CARTESIAN_POINT('Ctrl Pts',(2.28438953840607,0.636309800095226,2.89008882490359));
#48428=CARTESIAN_POINT('Ctrl Pts',(2.3086092844839,0.794772684000866,2.8253422315068));
#48429=CARTESIAN_POINT('Ctrl Pts',(2.28391313972469,1.06847604194561,2.75910807960274));
#48430=CARTESIAN_POINT('Ctrl Pts',(2.26246063338278,1.18514270861274,2.73575643566054));
#48431=CARTESIAN_POINT('Ctrl Pts',(2.23024566668289,1.30000000000141,2.71772345791827));
#48432=CARTESIAN_POINT('Ctrl Pts',(2.46723566498124,-1.30000000000004,2.81828368411535));
#48433=CARTESIAN_POINT('Ctrl Pts',(2.49156132565254,-1.18514270861182,2.82927316502905));
#48434=CARTESIAN_POINT('Ctrl Pts',(2.50112533947257,-1.06847604194514,2.84403085533445));
#48435=CARTESIAN_POINT('Ctrl Pts',(2.48911776738753,-0.794772684000865,
2.88682938972833));
#48436=CARTESIAN_POINT('Ctrl Pts',(2.4318418165874,-0.636309800095211,2.93315911961345));
#48437=CARTESIAN_POINT('Ctrl Pts',(2.36826535756389,-0.319434907277168,
2.97563179632322));
#48438=CARTESIAN_POINT('Ctrl Pts',(2.31972158902228,-0.158333333333336,
2.99985276530071));
#48439=CARTESIAN_POINT('Ctrl Pts',(2.29076505790789,0.158333333333338,2.98392483559399));
#48440=CARTESIAN_POINT('Ctrl Pts',(2.30931783037278,0.319434907277172,2.94317659647188));
#48441=CARTESIAN_POINT('Ctrl Pts',(2.31601905110005,0.636309800095219,2.86948068711656));
#48442=CARTESIAN_POINT('Ctrl Pts',(2.34231658966155,0.794772684000861,2.80522231166917));
#48443=CARTESIAN_POINT('Ctrl Pts',(2.31272733666762,1.06847604194561,2.74139292904049));
#48444=CARTESIAN_POINT('Ctrl Pts',(2.28763326817312,1.18514270861273,2.71946745101114));
#48445=CARTESIAN_POINT('Ctrl Pts',(2.25025322241536,1.3000000000014,2.70324586958073));
#48446=CARTESIAN_POINT('Ctrl Pts',(2.47880653387094,-1.30000000000002,2.81238598020883));
#48447=CARTESIAN_POINT('Ctrl Pts',(2.50530349436362,-1.18514270861179,2.82219997193384));
#48448=CARTESIAN_POINT('Ctrl Pts',(2.51643668958125,-1.06847604194512,2.83607840627677));
#48449=CARTESIAN_POINT('Ctrl Pts',(2.50666322642594,-0.794772684000851,
2.87753004151657));
#48450=CARTESIAN_POINT('Ctrl Pts',(2.44892689462503,-0.636309800095197,
2.92401312273345));
#48451=CARTESIAN_POINT('Ctrl Pts',(2.38514150298642,-0.319434907277159,
2.96618025706083));
#48452=CARTESIAN_POINT('Ctrl Pts',(2.33567769709269,-0.158333333333332,
2.99058134656035));
#48453=CARTESIAN_POINT('Ctrl Pts',(2.30625480759988,0.158333333333334,2.97425015982675));
#48454=CARTESIAN_POINT('Ctrl Pts',(2.32505056891378,0.319434907277167,2.93274590524431));
#48455=CARTESIAN_POINT('Ctrl Pts',(2.33143994443199,0.636309800095206,2.85888578373837));
#48456=CARTESIAN_POINT('Ctrl Pts',(2.35820372983969,0.79477268400084,2.79445086843063));
#48457=CARTESIAN_POINT('Ctrl Pts',(2.32663344521582,1.06847604194558,2.73214786314114));
#48458=CARTESIAN_POINT('Ctrl Pts',(2.30018582394002,1.1851427086127,2.71126979906201));
#48459=CARTESIAN_POINT('Ctrl Pts',(2.26095618780779,1.30000000000137,2.69648233333975));
#48460=CARTESIAN_POINT('Ctrl Pts',(2.48455995069221,-1.30000000000002,2.80941437546233));
#48461=CARTESIAN_POINT('Ctrl Pts',(2.5121356260387,-1.18514270861179,2.81863590450896));
#48462=CARTESIAN_POINT('Ctrl Pts',(2.52404941520512,-1.06847604194512,2.83207202931145));
#48463=CARTESIAN_POINT('Ctrl Pts',(2.51539056129934,-0.794772684000851,
2.87284872481581));
#48464=CARTESIAN_POINT('Ctrl Pts',(2.45746810794786,-0.636309800095197,
2.91944248366907));
#48465=CARTESIAN_POINT('Ctrl Pts',(2.39351595813041,-0.319434907277159,
2.96140733565522));
#48466=CARTESIAN_POINT('Ctrl Pts',(2.34340372597283,-0.158333333333332,
2.98574911995223));
#48467=CARTESIAN_POINT('Ctrl Pts',(2.3138047860753,0.158333333333334,2.96926236941848));
#48468=CARTESIAN_POINT('Ctrl Pts',(2.33301542000643,0.319434907277167,2.92761421432513));
#48469=CARTESIAN_POINT('Ctrl Pts',(2.33933008166849,0.636309800095206,2.85373654604741));
#48470=CARTESIAN_POINT('Ctrl Pts',(2.36620091374558,0.79477268400084,2.78910957149981));
#48471=CARTESIAN_POINT('Ctrl Pts',(2.33354901187549,1.06847604194558,2.72750133134463));
#48472=CARTESIAN_POINT('Ctrl Pts',(2.30638156847357,1.1851427086127,2.70711605782787));
#48473=CARTESIAN_POINT('Ctrl Pts',(2.26618048011713,1.30000000000137,2.6930134351473));
#48474=CARTESIAN_POINT('',(2.20678870418117,1.2,2.7691328596878));
#48475=CARTESIAN_POINT('Ctrl Pts',(2.20678870418117,1.2,2.7691328596878));
#48476=CARTESIAN_POINT('Ctrl Pts',(2.18719042940982,1.21681100185863,2.77815258574768));
#48477=CARTESIAN_POINT('Ctrl Pts',(2.16682870549213,1.23316343936831,2.78634864439441));
#48478=CARTESIAN_POINT('Ctrl Pts',(2.13772436433275,1.25820872625497,2.80002267851674));
#48479=CARTESIAN_POINT('Ctrl Pts',(2.128098436078,1.26641397694272,2.80447330095078));
#48480=CARTESIAN_POINT('Ctrl Pts',(2.10695042735038,1.28440270834969,2.81424329862363));
#48481=CARTESIAN_POINT('Ctrl Pts',(2.09638038403599,1.29362818749432,2.81941082472892));
#48482=CARTESIAN_POINT('Ctrl Pts',(2.08911835446463,1.30000000000141,2.82300508327628));
#48483=CARTESIAN_POINT('',(2.34584244529745,0.653834841330817,2.8411557470558));
#48484=CARTESIAN_POINT('Ctrl Pts',(2.34584244526459,0.653834841315613,2.84115574699037));
#48485=CARTESIAN_POINT('Ctrl Pts',(2.33291982688079,0.711695067402296,2.83420105328051));
#48486=CARTESIAN_POINT('Ctrl Pts',(2.3192544465607,0.767440337243871,2.82692182047546));
#48487=CARTESIAN_POINT('Ctrl Pts',(2.2907904144071,0.881611845231268,2.81194318081469));
#48488=CARTESIAN_POINT('Ctrl Pts',(2.27698326702507,0.939285575122016,2.80475197710374));
#48489=CARTESIAN_POINT('Ctrl Pts',(2.25126333376498,1.03699756658839,2.79155206652874));
#48490=CARTESIAN_POINT('Ctrl Pts',(2.24987672470583,1.04154831766055,2.79081882997294));
#48491=CARTESIAN_POINT('Ctrl Pts',(2.22388678607746,1.13769836768628,2.77767579297531));
#48492=CARTESIAN_POINT('Ctrl Pts',(2.21630665873191,1.16589155301464,2.77387326690931));
#48493=CARTESIAN_POINT('Ctrl Pts',(2.20678870418117,1.2,2.7691328596878));
#48494=CARTESIAN_POINT('',(2.46774460503229,-0.653834841531101,2.90899352548449));
#48495=CARTESIAN_POINT('Ctrl Pts',(2.46774460503229,-0.653834841531101,
2.90899352548449));
#48496=CARTESIAN_POINT('Ctrl Pts',(2.43367040187115,-0.575755206684555,
2.93302081381537));
#48497=CARTESIAN_POINT('Ctrl Pts',(2.40440703109882,-0.49371053352102,2.95246212356931));
#48498=CARTESIAN_POINT('Ctrl Pts',(2.36105525320677,-0.338116463230631,
2.9786559138965));
#48499=CARTESIAN_POINT('Ctrl Pts',(2.34510580758702,-0.265668632538642,
2.98681711169481));
#48500=CARTESIAN_POINT('Ctrl Pts',(2.32175237490573,-0.129739525092484,
2.99396435195135));
#48501=CARTESIAN_POINT('Ctrl Pts',(2.31349848432192,-0.0666632460451577,
2.99414569446904));
#48502=CARTESIAN_POINT('Ctrl Pts',(2.30171267766772,0.0595076176857795,
2.9880167192894));
#48503=CARTESIAN_POINT('Ctrl Pts',(2.29809985009213,0.122729100378534,2.98168411333372));
#48504=CARTESIAN_POINT('Ctrl Pts',(2.29615407501564,0.260112555578735,2.96113399532689));
#48505=CARTESIAN_POINT('Ctrl Pts',(2.29885574957816,0.333987313117584,2.94565663983887));
#48506=CARTESIAN_POINT('Ctrl Pts',(2.31369679496233,0.49152811065413,2.90327079369133));
#48507=CARTESIAN_POINT('Ctrl Pts',(2.32714321918519,0.5749238686812,2.8744937786279));
#48508=CARTESIAN_POINT('Ctrl Pts',(2.3458424451743,0.653834841353173,2.84115574703964));
#48509=CARTESIAN_POINT('',(2.40480387199025,-1.2,2.87340568838946));
#48510=CARTESIAN_POINT('Ctrl Pts',(2.40480387199025,-1.2,2.87340568838946));
#48511=CARTESIAN_POINT('Ctrl Pts',(2.41517135482326,-1.13733527587012,2.87916813364408));
#48512=CARTESIAN_POINT('Ctrl Pts',(2.43005872934456,-1.03725368999983,2.88749973076383));
#48513=CARTESIAN_POINT('Ctrl Pts',(2.4603247499497,-0.771923993714115,2.90470411541019));
#48514=CARTESIAN_POINT('Ctrl Pts',(2.46348281431209,-0.719575717376282,
2.90654258276977));
#48515=CARTESIAN_POINT('Ctrl Pts',(2.46774460503229,-0.653834841531101,
2.90899352548449));
#48516=CARTESIAN_POINT('Ctrl Pts',(2.2912494730135,-1.30000000000006,2.92534494345862));
#48517=CARTESIAN_POINT('Ctrl Pts',(2.30303220569663,-1.289337655596,2.91956314586749));
#48518=CARTESIAN_POINT('Ctrl Pts',(2.3078497420404,-1.28460982232617,2.91678630959235));
#48519=CARTESIAN_POINT('Ctrl Pts',(2.32967167705473,-1.26566188389439,2.90704899985406));
#48520=CARTESIAN_POINT('Ctrl Pts',(2.3390344571774,-1.25743246251566,2.90277167327097));
#48521=CARTESIAN_POINT('Ctrl Pts',(2.35866194984038,-1.23987895240838,2.8934877174126));
#48522=CARTESIAN_POINT('Ctrl Pts',(2.38088284032858,-1.22001152618653,2.8830048470048));
#48523=CARTESIAN_POINT('Ctrl Pts',(2.40480387199025,-1.2,2.87340568838946));
#48524=CARTESIAN_POINT('Origin',(0.,1.25,7.2));
#48525=CARTESIAN_POINT('Origin',(0.,1.2,7.2));
#48526=CARTESIAN_POINT('Origin',(0.,0.92691742076555,7.2));
#48527=CARTESIAN_POINT('Origin',(0.,0.653834841531101,7.2));
#48528=CARTESIAN_POINT('Origin',(0.,0.,7.2));
#48529=CARTESIAN_POINT('Origin',(0.,-0.653834841531101,7.2));
#48530=CARTESIAN_POINT('Origin',(0.,-0.926917420765551,7.2));
#48531=CARTESIAN_POINT('Origin',(0.,-1.2,7.2));
#48532=CARTESIAN_POINT('Origin',(0.,-1.25,7.2));
#48533=CARTESIAN_POINT('Ctrl Pts',(2.77007461962236,-1.30000000000274,2.98393685222895));
#48534=CARTESIAN_POINT('Ctrl Pts',(2.73776084594367,-1.18514270861364,2.95617299979124));
#48535=CARTESIAN_POINT('Ctrl Pts',(2.70652295951449,-1.06847604194606,2.94283794040697));
#48536=CARTESIAN_POINT('Ctrl Pts',(2.63684270752248,-0.794772684000851,
2.94536468398338));
#48537=CARTESIAN_POINT('Ctrl Pts',(2.59430952183081,-0.636309800095197,
3.00094899446));
#48538=CARTESIAN_POINT('Ctrl Pts',(2.53348691516025,-0.319434907277159,
3.04335648601559));
#48539=CARTESIAN_POINT('Ctrl Pts',(2.50702387179492,-0.158333333333332,
3.08081746056841));
#48540=CARTESIAN_POINT('Ctrl Pts',(2.47794645705815,0.158333333333334,3.06342740195888));
#48541=CARTESIAN_POINT('Ctrl Pts',(2.47397094455433,0.319434907277167,3.00785804372116));
#48542=CARTESIAN_POINT('Ctrl Pts',(2.47833749753066,0.636309800095206,2.93149143136109));
#48543=CARTESIAN_POINT('Ctrl Pts',(2.48972764967703,0.79477268400084,2.85803223588656));
#48544=CARTESIAN_POINT('Ctrl Pts',(2.52071187691362,1.0684760419458,2.83014510068367));
#48545=CARTESIAN_POINT('Ctrl Pts',(2.5383047969051,1.18514270861315,2.83374468235468));
#48546=CARTESIAN_POINT('Ctrl Pts',(2.56007871299605,1.30000000000202,2.85301515320588));
#48547=CARTESIAN_POINT('Ctrl Pts',(2.76929060404465,-1.30000000000274,2.99645449009369));
#48548=CARTESIAN_POINT('Ctrl Pts',(2.73676209966059,-1.18514270861363,2.971058085287));
#48549=CARTESIAN_POINT('Ctrl Pts',(2.70539049707342,-1.06847604194605,2.95946258494912));
#48550=CARTESIAN_POINT('Ctrl Pts',(2.63558849381797,-0.794772684000847,
2.96455750968112));
#48551=CARTESIAN_POINT('Ctrl Pts',(2.59328091779236,-0.636309800095194,
3.01976435068509));
#48552=CARTESIAN_POINT('Ctrl Pts',(2.53256341686942,-0.319434907277157,
3.06228370367669));
#48553=CARTESIAN_POINT('Ctrl Pts',(2.50593474388911,-0.158333333333332,
3.09888219725884));
#48554=CARTESIAN_POINT('Ctrl Pts',(2.47730282396258,0.158333333333334,3.08164150309493));
#48555=CARTESIAN_POINT('Ctrl Pts',(2.47407845734968,0.319434907277168,3.02713594688277));
#48556=CARTESIAN_POINT('Ctrl Pts',(2.47896213178644,0.636309800095205,2.95085588583574));
#48557=CARTESIAN_POINT('Ctrl Pts',(2.49034670616782,0.794772684000836,2.87782974001919));
#48558=CARTESIAN_POINT('Ctrl Pts',(2.52138535406906,1.0684760419458,2.84733710522955));
#48559=CARTESIAN_POINT('Ctrl Pts',(2.53896378271483,1.18514270861314,2.8491423489711));
#48560=CARTESIAN_POINT('Ctrl Pts',(2.56068515942512,1.30000000000202,2.8659519681912));
#48561=CARTESIAN_POINT('Ctrl Pts',(2.76721848791142,-1.30000000000265,3.02121331325036));
#48562=CARTESIAN_POINT('Ctrl Pts',(2.73578637353955,-1.18514270861355,3.00121583992818));
#48563=CARTESIAN_POINT('Ctrl Pts',(2.70501257943525,-1.06847604194598,2.99348304482396));
#48564=CARTESIAN_POINT('Ctrl Pts',(2.63543981029279,-0.794772684000797,
3.00395260141672));
#48565=CARTESIAN_POINT('Ctrl Pts',(2.59106724941863,-0.636309800095158,
3.05737222262203));
#48566=CARTESIAN_POINT('Ctrl Pts',(2.5298731250399,-0.319434907277142,3.09983687965061));
#48567=CARTESIAN_POINT('Ctrl Pts',(2.50382283511936,-0.158333333333323,
3.13505529858875));
#48568=CARTESIAN_POINT('Ctrl Pts',(2.47579477399916,0.158333333333325,3.11801831865943));
#48569=CARTESIAN_POINT('Ctrl Pts',(2.47299997278668,0.319434907277146,3.06526604657375));
#48570=CARTESIAN_POINT('Ctrl Pts',(2.47876718605892,0.636309800095166,2.98911038310189));
#48571=CARTESIAN_POINT('Ctrl Pts',(2.49114624673536,0.794772684000794,2.91731837360279));
#48572=CARTESIAN_POINT('Ctrl Pts',(2.52227539906165,1.06847604194574,2.88158743177373));
#48573=CARTESIAN_POINT('Ctrl Pts',(2.53963249089368,1.18514270861308,2.87971951368484));
#48574=CARTESIAN_POINT('Ctrl Pts',(2.56087201796442,1.30000000000195,2.89145027826303));
#48575=CARTESIAN_POINT('Ctrl Pts',(2.7652185811479,-1.30000000000256,3.04654629607291));
#48576=CARTESIAN_POINT('Ctrl Pts',(2.73243126387775,-1.18514270861348,3.03098812080502));
#48577=CARTESIAN_POINT('Ctrl Pts',(2.70083628138072,-1.06847604194591,3.02656997753292));
#48578=CARTESIAN_POINT('Ctrl Pts',(2.63060008310996,-0.794772684000746,
3.04209888519379));
#48579=CARTESIAN_POINT('Ctrl Pts',(2.58791270220426,-0.636309800095112,
3.09526306562633));
#48580=CARTESIAN_POINT('Ctrl Pts',(2.52733228412459,-0.319434907277116,
3.13812521055095));
#48581=CARTESIAN_POINT('Ctrl Pts',(2.50092370254775,-0.158333333333311,
3.17156613975076));
#48582=CARTESIAN_POINT('Ctrl Pts',(2.47354491525794,0.158333333333314,3.15475538318367));
#48583=CARTESIAN_POINT('Ctrl Pts',(2.47144943768543,0.319434907277126,3.10389195667189));
#48584=CARTESIAN_POINT('Ctrl Pts',(2.4785533351495,0.636309800095123,3.02803358288528));
#48585=CARTESIAN_POINT('Ctrl Pts',(2.49247060842304,0.794772684000734,2.95770033352747));
#48586=CARTESIAN_POINT('Ctrl Pts',(2.52383408752185,1.06847604194566,2.91668889036367));
#48587=CARTESIAN_POINT('Ctrl Pts',(2.54091340125602,1.18514270861299,2.91105954495111));
#48588=CARTESIAN_POINT('Ctrl Pts',(2.56149594075389,1.30000000000185,2.91755318824791));
#48589=CARTESIAN_POINT('Ctrl Pts',(2.76408253126439,-1.30000000000255,3.05972730575715));
#48590=CARTESIAN_POINT('Ctrl Pts',(2.73152836524454,-1.18514270861346,3.04690234069982));
#48591=CARTESIAN_POINT('Ctrl Pts',(2.70004026601005,-1.0684760419459,3.0444554800774));
#48592=CARTESIAN_POINT('Ctrl Pts',(2.62975928514619,-0.794772684000735,
3.06277823992411));
#48593=CARTESIAN_POINT('Ctrl Pts',(2.58653525785172,-0.636309800095103,
3.11521585093284));
#48594=CARTESIAN_POINT('Ctrl Pts',(2.52563186823559,-0.319434907277112,
3.15802247013646));
#48595=CARTESIAN_POINT('Ctrl Pts',(2.49895903018375,-0.158333333333309,
3.19050025120487));
#48596=CARTESIAN_POINT('Ctrl Pts',(2.47190832759045,0.158333333333311,3.17380577933224));
#48597=CARTESIAN_POINT('Ctrl Pts',(2.47065441609167,0.319434907277121,3.12412270606223));
#48598=CARTESIAN_POINT('Ctrl Pts',(2.47824191681505,0.636309800095114,3.04835115392578));
#48599=CARTESIAN_POINT('Ctrl Pts',(2.49200957451927,0.794772684000723,2.97843587612576));
#48600=CARTESIAN_POINT('Ctrl Pts',(2.52349875362235,1.06847604194565,2.93465689948966));
#48601=CARTESIAN_POINT('Ctrl Pts',(2.54064141214415,1.18514270861297,2.92713029039323));
#48602=CARTESIAN_POINT('Ctrl Pts',(2.56129623034307,1.30000000000184,2.93102736901523));
#48603=CARTESIAN_POINT('Ctrl Pts',(2.76393671495793,-1.30000000000255,3.06127271886912));
#48604=CARTESIAN_POINT('Ctrl Pts',(2.73140696766947,-1.18514270861346,3.0487683078493));
#48605=CARTESIAN_POINT('Ctrl Pts',(2.6999301212694,-1.0684760419459,3.04655299023555));
#48606=CARTESIAN_POINT('Ctrl Pts',(2.62964472084827,-0.794772684000736,
3.06520502746905));
#48607=CARTESIAN_POINT('Ctrl Pts',(2.58636702198853,-0.636309800095104,
3.11756090521599));
#48608=CARTESIAN_POINT('Ctrl Pts',(2.52542602591945,-0.319434907277112,
3.16036129461213));
#48609=CARTESIAN_POINT('Ctrl Pts',(2.49871387963128,-0.158333333333309,
3.19272260274774));
#48610=CARTESIAN_POINT('Ctrl Pts',(2.4717012207635,0.158333333333311,3.17604171343888));
#48611=CARTESIAN_POINT('Ctrl Pts',(2.47055032595736,0.319434907277121,3.12649920803476));
#48612=CARTESIAN_POINT('Ctrl Pts',(2.47820064825465,0.636309800095114,3.05074013947077));
#48613=CARTESIAN_POINT('Ctrl Pts',(2.49195786235389,0.794772684000724,2.98087660648409));
#48614=CARTESIAN_POINT('Ctrl Pts',(2.52346380679981,1.06847604194565,2.93677266582891));
#48615=CARTESIAN_POINT('Ctrl Pts',(2.54061323305724,1.18514270861297,2.92902253581192));
#48616=CARTESIAN_POINT('Ctrl Pts',(2.56127432963171,1.30000000000184,2.93261323747555));
#48617=CARTESIAN_POINT('Ctrl Pts',(2.76367479421307,-1.30000000000255,3.06397452733984));
#48618=CARTESIAN_POINT('Ctrl Pts',(2.73117783714647,-1.18514270861346,3.0520268287371));
#48619=CARTESIAN_POINT('Ctrl Pts',(2.69971468392264,-1.0684760419459,3.0502141552986));
#48620=CARTESIAN_POINT('Ctrl Pts',(2.62941679948215,-0.794772684000736,
3.06944045266576));
#48621=CARTESIAN_POINT('Ctrl Pts',(2.58605487221752,-0.636309800095104,
3.12165763870706));
#48622=CARTESIAN_POINT('Ctrl Pts',(2.5250583247634,-0.319434907277112,3.16445140478554));
#48623=CARTESIAN_POINT('Ctrl Pts',(2.49829077627368,-0.158333333333309,
3.19661413676455));
#48624=CARTESIAN_POINT('Ctrl Pts',(2.47134447132379,0.158333333333311,3.17995702806293));
#48625=CARTESIAN_POINT('Ctrl Pts',(2.47035394045193,0.319434907277122,3.13065281472957));
#48626=CARTESIAN_POINT('Ctrl Pts',(2.47811633094835,0.636309800095115,3.05491634979516));
#48627=CARTESIAN_POINT('Ctrl Pts',(2.49187936704538,0.794772684000724,2.9851525184675));
#48628=CARTESIAN_POINT('Ctrl Pts',(2.52341791795381,1.06847604194565,2.94048112062575));
#48629=CARTESIAN_POINT('Ctrl Pts',(2.54057643155836,1.18514270861297,2.93233878096298));
#48630=CARTESIAN_POINT('Ctrl Pts',(2.56124158869765,1.30000000000184,2.93539069452477));
#48631=CARTESIAN_POINT('Ctrl Pts',(2.76309866457954,-1.30000000000255,3.0693569772583));
#48632=CARTESIAN_POINT('Ctrl Pts',(2.73060852771944,-1.18514270861347,3.05849815921093));
#48633=CARTESIAN_POINT('Ctrl Pts',(2.69913847631771,-1.0684760419459,3.05747652440161));
#48634=CARTESIAN_POINT('Ctrl Pts',(2.62879296349401,-0.794772684000738,
3.07784220481634));
#48635=CARTESIAN_POINT('Ctrl Pts',(2.58533532606946,-0.636309800095105,
3.1298130289063));
#48636=CARTESIAN_POINT('Ctrl Pts',(2.52428188718962,-0.319434907277113,
3.17261639434202));
#48637=CARTESIAN_POINT('Ctrl Pts',(2.4974530801566,-0.15833333333331,3.20440186989524));
#48638=CARTESIAN_POINT('Ctrl Pts',(2.47063810417917,0.158333333333312,3.1877925966685));
#48639=CARTESIAN_POINT('Ctrl Pts',(2.46987895907201,0.319434907277122,3.13893071555855));
#48640=CARTESIAN_POINT('Ctrl Pts',(2.47788671941555,0.636309800095115,3.06324697138882));
#48641=CARTESIAN_POINT('Ctrl Pts',(2.49179054834725,0.794772684000726,2.99373052952472));
#48642=CARTESIAN_POINT('Ctrl Pts',(2.52341492440155,1.06847604194565,2.94793175812201));
#48643=CARTESIAN_POINT('Ctrl Pts',(2.54057789787682,1.18514270861298,2.93899986355282));
#48644=CARTESIAN_POINT('Ctrl Pts',(2.56121482423204,1.30000000000184,2.94096066554301));
#48645=CARTESIAN_POINT('Ctrl Pts',(2.7621442995113,-1.30000000000256,3.07699590637945));
#48646=CARTESIAN_POINT('Ctrl Pts',(2.72942903075446,-1.18514270861347,3.06759261633828));
#48647=CARTESIAN_POINT('Ctrl Pts',(2.69781041332261,-1.06847604194591,3.06764199419852));
#48648=CARTESIAN_POINT('Ctrl Pts',(2.62729856571769,-0.794772684000742,
3.0895936207856));
#48649=CARTESIAN_POINT('Ctrl Pts',(2.58397375681921,-0.636309800095108,
3.14132870240152));
#48650=CARTESIAN_POINT('Ctrl Pts',(2.52306333846313,-0.319434907277114,
3.18423899962697));
#48651=CARTESIAN_POINT('Ctrl Pts',(2.49638657956733,-0.15833333333331,3.21558026331581));
#48652=CARTESIAN_POINT('Ctrl Pts',(2.4697476139746,0.158333333333313,3.19903735811405));
#48653=CARTESIAN_POINT('Ctrl Pts',(2.46891703047776,0.319434907277124,3.15065303364791));
#48654=CARTESIAN_POINT('Ctrl Pts',(2.47733461500681,0.636309800095119,3.07506481055014));
#48655=CARTESIAN_POINT('Ctrl Pts',(2.49196724242051,0.79477268400073,3.00609836528132));
#48656=CARTESIAN_POINT('Ctrl Pts',(2.52377377005411,1.06847604194566,2.9587108102807));
#48657=CARTESIAN_POINT('Ctrl Pts',(2.5408736807323,1.18514270861298,2.94862501569126));
#48658=CARTESIAN_POINT('Ctrl Pts',(2.56130563482408,1.30000000000184,2.94896574319025));
#48659=CARTESIAN_POINT('Ctrl Pts',(2.76100115701359,-1.30000000000257,3.08616759468416));
#48660=CARTESIAN_POINT('Ctrl Pts',(2.72800130695223,-1.18514270861348,3.07850646772044));
#48661=CARTESIAN_POINT('Ctrl Pts',(2.69618309389375,-1.06847604194592,3.07983308091253));
#48662=CARTESIAN_POINT('Ctrl Pts',(2.6254064743796,-0.794772684000749,3.10366130052537));
#48663=CARTESIAN_POINT('Ctrl Pts',(2.58215216274572,-0.636309800095113,
3.15507420908088));
#48664=CARTESIAN_POINT('Ctrl Pts',(2.52137305231519,-0.319434907277116,
3.19809534748637));
#48665=CARTESIAN_POINT('Ctrl Pts',(2.49490004610859,-0.158333333333311,
3.22891175502433));
#48666=CARTESIAN_POINT('Ctrl Pts',(2.46850828493044,0.158333333333314,3.21246574523192));
#48667=CARTESIAN_POINT('Ctrl Pts',(2.46766473902188,0.319434907277126,3.16468858611461));
#48668=CARTESIAN_POINT('Ctrl Pts',(2.47656946475392,0.636309800095123,3.08921660187131));
#48669=CARTESIAN_POINT('Ctrl Pts',(2.49193592041559,0.794772684000735,3.02085499815659));
#48670=CARTESIAN_POINT('Ctrl Pts',(2.52402010645754,1.06847604194566,2.97158305391625));
#48671=CARTESIAN_POINT('Ctrl Pts',(2.54111071189665,1.18514270861299,2.96013759686987));
#48672=CARTESIAN_POINT('Ctrl Pts',(2.56140386747354,1.30000000000185,2.95857468173336));
#48673=CARTESIAN_POINT('Ctrl Pts',(2.75973043404253,-1.30000000000257,3.09850296312576));
#48674=CARTESIAN_POINT('Ctrl Pts',(2.72673344694344,-1.18514270861349,3.09332988253571));
#48675=CARTESIAN_POINT('Ctrl Pts',(2.69486206402682,-1.06847604194592,3.09645179355735));
#48676=CARTESIAN_POINT('Ctrl Pts',(2.62383316447927,-0.794772684000754,
3.12282712258378));
#48677=CARTESIAN_POINT('Ctrl Pts',(2.58018454086766,-0.636309800095117,
3.17359946802657));
#48678=CARTESIAN_POINT('Ctrl Pts',(2.5190510459393,-0.319434907277118,3.21654618894011));
#48679=CARTESIAN_POINT('Ctrl Pts',(2.49224201902599,-0.158333333333313,
3.2464126972753));
#48680=CARTESIAN_POINT('Ctrl Pts',(2.46615483373219,0.158333333333315,3.2300839140066));
#48681=CARTESIAN_POINT('Ctrl Pts',(2.46611897094408,0.319434907277128,3.18344725658337));
#48682=CARTESIAN_POINT('Ctrl Pts',(2.47565813709047,0.636309800095127,3.10813901025747));
#48683=CARTESIAN_POINT('Ctrl Pts',(2.4911520371447,0.79477268400074,3.04027505419037));
#48684=CARTESIAN_POINT('Ctrl Pts',(2.52351148979463,1.06847604194567,2.98845100941886));
#48685=CARTESIAN_POINT('Ctrl Pts',(2.54069441470553,1.185142708613,2.97522591670852));
#48686=CARTESIAN_POINT('Ctrl Pts',(2.56105305651101,1.30000000000186,2.97120843999939));
#48687=CARTESIAN_POINT('Ctrl Pts',(2.75818571536233,-1.30000000000258,3.11395382493746));
#48688=CARTESIAN_POINT('Ctrl Pts',(2.72516881337955,-1.1851427086135,3.11188529650836));
#48689=CARTESIAN_POINT('Ctrl Pts',(2.69322800104665,-1.06847604194593,3.11725314803314));
#48690=CARTESIAN_POINT('Ctrl Pts',(2.62192431718254,-0.79477268400076,3.14683348422645));
#48691=CARTESIAN_POINT('Ctrl Pts',(2.57789912794509,-0.636309800095122,
3.1968538353808));
#48692=CARTESIAN_POINT('Ctrl Pts',(2.51639218605445,-0.31943490727712,3.23973300172921));
#48693=CARTESIAN_POINT('Ctrl Pts',(2.4892276348165,-0.158333333333314,3.26842989090202));
#48694=CARTESIAN_POINT('Ctrl Pts',(2.46340122882819,0.158333333333316,3.25219748804885));
#48695=CARTESIAN_POINT('Ctrl Pts',(2.46399403849527,0.319434907277131,3.20684119605487));
#48696=CARTESIAN_POINT('Ctrl Pts',(2.47441264586635,0.636309800095132,3.13176756205614));
#48697=CARTESIAN_POINT('Ctrl Pts',(2.49063108383278,0.794772684000745,3.0647364067299));
#48698=CARTESIAN_POINT('Ctrl Pts',(2.52348977741813,1.06847604194568,3.00978306948002));
#48699=CARTESIAN_POINT('Ctrl Pts',(2.54077114129557,1.18514270861301,2.99432928211294));
#48700=CARTESIAN_POINT('Ctrl Pts',(2.5611105581319,1.30000000000187,2.98720897085252));
#48701=CARTESIAN_POINT('Ctrl Pts',(2.7549023177279,-1.30000000000261,3.13832627815554));
#48702=CARTESIAN_POINT('Ctrl Pts',(2.72120577726823,-1.18514270861352,3.14095019256061));
#48703=CARTESIAN_POINT('Ctrl Pts',(2.68871288765401,-1.06847604194595,3.14972442523763));
#48704=CARTESIAN_POINT('Ctrl Pts',(2.61642848670769,-0.794772684000774,
3.18420312357576));
#48705=CARTESIAN_POINT('Ctrl Pts',(2.57194172056141,-0.636309800095132,
3.23307614933181));
#48706=CARTESIAN_POINT('Ctrl Pts',(2.51044675909465,-0.319434907277125,
3.27611316803085));
#48707=CARTESIAN_POINT('Ctrl Pts',(2.48372887214136,-0.158333333333316,
3.30338169611771));
#48708=CARTESIAN_POINT('Ctrl Pts',(2.45894850607955,0.158333333333319,3.28758166575951));
#48709=CARTESIAN_POINT('Ctrl Pts',(2.46072295196821,0.319434907277137,3.2443405872588));
#48710=CARTESIAN_POINT('Ctrl Pts',(2.47207426405154,0.636309800095144,3.16947145529152));
#48711=CARTESIAN_POINT('Ctrl Pts',(2.48810766360199,0.794772684000758,3.10327100058628));
#48712=CARTESIAN_POINT('Ctrl Pts',(2.52147144464212,1.0684760419457,3.04318070445959));
#48713=CARTESIAN_POINT('Ctrl Pts',(2.53902642198244,1.18514270861303,3.02419036799466));
#48714=CARTESIAN_POINT('Ctrl Pts',(2.55969443210068,1.3000000000019,3.0122205576932));
#48715=CARTESIAN_POINT('Ctrl Pts',(2.75184888476579,-1.30000000000264,3.16283396361858));
#48716=CARTESIAN_POINT('Ctrl Pts',(2.71746663127512,-1.18514270861355,3.17014743557151));
#48717=CARTESIAN_POINT('Ctrl Pts',(2.68448012602566,-1.06847604194598,3.18235462632914));
#48718=CARTESIAN_POINT('Ctrl Pts',(2.61149915762758,-0.794772684000793,
3.2218611484432));
#48719=CARTESIAN_POINT('Ctrl Pts',(2.56724671660987,-0.636309800095148,
3.26990395622154));
#48720=CARTESIAN_POINT('Ctrl Pts',(2.50568271389788,-0.319434907277134,
3.31306241579418));
#48721=CARTESIAN_POINT('Ctrl Pts',(2.47891175269111,-0.15833333333332,3.33865996146269));
#48722=CARTESIAN_POINT('Ctrl Pts',(2.4542701656467,0.158333333333322,3.32291066839621));
#48723=CARTESIAN_POINT('Ctrl Pts',(2.45598525678049,0.319434907277142,3.28129641508887));
#48724=CARTESIAN_POINT('Ctrl Pts',(2.46819998563599,0.636309800095157,3.20660248375591));
#48725=CARTESIAN_POINT('Ctrl Pts',(2.48531425849309,0.794772684000779,3.1417362377766));
#48726=CARTESIAN_POINT('Ctrl Pts',(2.51991043860404,1.06847604194572,3.07680171724122));
#48727=CARTESIAN_POINT('Ctrl Pts',(2.53797508303648,1.18514270861305,3.0543711466414));
#48728=CARTESIAN_POINT('Ctrl Pts',(2.55912896744609,1.30000000000192,3.03761775332049));
#48729=CARTESIAN_POINT('Ctrl Pts',(2.7483447845198,-1.30000000000265,3.18713448216638));
#48730=CARTESIAN_POINT('Ctrl Pts',(2.71346030506721,-1.18514270861355,3.19924195415874));
#48731=CARTESIAN_POINT('Ctrl Pts',(2.67991284763775,-1.06847604194598,3.21486580077584));
#48732=CARTESIAN_POINT('Ctrl Pts',(2.60550029817392,-0.794772684000795,
3.25908354083241));
#48733=CARTESIAN_POINT('Ctrl Pts',(2.55953575074245,-0.63630980009515,3.30539306082358));
#48734=CARTESIAN_POINT('Ctrl Pts',(2.49755111095438,-0.319434907277134,
3.34851999863704));
#48735=CARTESIAN_POINT('Ctrl Pts',(2.47177474429291,-0.158333333333321,
3.37294177377652));
#48736=CARTESIAN_POINT('Ctrl Pts',(2.44821621172272,0.158333333333323,3.35767651489293));
#48737=CARTESIAN_POINT('Ctrl Pts',(2.45050291347272,0.319434907277145,3.31796779184588));
#48738=CARTESIAN_POINT('Ctrl Pts',(2.46436024022379,0.636309800095161,3.24379079980185));
#48739=CARTESIAN_POINT('Ctrl Pts',(2.48315961503444,0.79477268400078,3.18051374342521));
#48740=CARTESIAN_POINT('Ctrl Pts',(2.51868068943466,1.06847604194573,3.1105959175308));
#48741=CARTESIAN_POINT('Ctrl Pts',(2.53685981385929,1.18514270861306,3.08455098390633));
#48742=CARTESIAN_POINT('Ctrl Pts',(2.55784230578616,1.30000000000193,3.06272595277639));
#48743=CARTESIAN_POINT('Ctrl Pts',(2.74574091063359,-1.30000000000266,3.20541339922365));
#48744=CARTESIAN_POINT('Ctrl Pts',(2.70964371406839,-1.18514270861356,3.22071934176333));
#48745=CARTESIAN_POINT('Ctrl Pts',(2.67533364623634,-1.06847604194599,3.23874024204124));
#48746=CARTESIAN_POINT('Ctrl Pts',(2.60019915072659,-0.794772684000802,
3.28664422225255));
#48747=CARTESIAN_POINT('Ctrl Pts',(2.55576917040971,-0.636309800095156,
3.332964495603));
#48748=CARTESIAN_POINT('Ctrl Pts',(2.49371487414238,-0.319434907277137,
3.37617641007381));
#48749=CARTESIAN_POINT('Ctrl Pts',(2.46683846697507,-0.158333333333322,
3.39884683891698));
#48750=CARTESIAN_POINT('Ctrl Pts',(2.44311848446409,0.158333333333324,3.3835033720173));
#48751=CARTESIAN_POINT('Ctrl Pts',(2.44600440432415,0.319434907277148,3.34531201998123));
#48752=CARTESIAN_POINT('Ctrl Pts',(2.46029380290506,0.636309800095166,3.27120803389401));
#48753=CARTESIAN_POINT('Ctrl Pts',(2.47879230060294,0.794772684000788,3.2085085373939));
#48754=CARTESIAN_POINT('Ctrl Pts',(2.51544085880915,1.06847604194574,3.13503668909042));
#48755=CARTESIAN_POINT('Ctrl Pts',(2.53437207462858,1.18514270861307,3.10655120032261));
#48756=CARTESIAN_POINT('Ctrl Pts',(2.55637070338285,1.30000000000194,3.08138346351737));
#48757=CARTESIAN_POINT('Ctrl Pts',(2.74195814600123,-1.30000000000267,3.22308002651805));
#48758=CARTESIAN_POINT('Ctrl Pts',(2.70557844442503,-1.18514270861357,3.24204765563099));
#48759=CARTESIAN_POINT('Ctrl Pts',(2.67088384859235,-1.068476041946,3.2626624023393));
#48760=CARTESIAN_POINT('Ctrl Pts',(2.59462532296085,-0.794772684000805,
3.31409176235129));
#48761=CARTESIAN_POINT('Ctrl Pts',(2.54860492617569,-0.63630980009516,3.35894703121784));
#48762=CARTESIAN_POINT('Ctrl Pts',(2.48613821236498,-0.319434907277141,
3.40208923138921));
#48763=CARTESIAN_POINT('Ctrl Pts',(2.45985076920911,-0.158333333333323,
3.42381119065622));
#48764=CARTESIAN_POINT('Ctrl Pts',(2.4375060132358,0.158333333333325,3.40910176479674));
#48765=CARTESIAN_POINT('Ctrl Pts',(2.4419033528333,0.31943490727715,3.37285105163994));
#48766=CARTESIAN_POINT('Ctrl Pts',(2.457929313369,0.636309800095171,3.29937879431315));
#48767=CARTESIAN_POINT('Ctrl Pts',(2.47738511628924,0.794772684000794,3.23773539497539));
#48768=CARTESIAN_POINT('Ctrl Pts',(2.51452673106549,1.06847604194574,3.16043120584603));
#48769=CARTESIAN_POINT('Ctrl Pts',(2.53342242175017,1.18514270861308,3.12917523589806));
#48770=CARTESIAN_POINT('Ctrl Pts',(2.55513657431532,1.30000000000195,3.1001254150738));
#48771=CARTESIAN_POINT('Ctrl Pts',(2.7396711808232,-1.30000000000267,3.2415292971106));
#48772=CARTESIAN_POINT('Ctrl Pts',(2.70247389906199,-1.18514270861358,3.26389070858423));
#48773=CARTESIAN_POINT('Ctrl Pts',(2.66713585044611,-1.06847604194601,3.28696483524763));
#48774=CARTESIAN_POINT('Ctrl Pts',(2.58979308929543,-0.794772684000814,
3.34191719846965));
#48775=CARTESIAN_POINT('Ctrl Pts',(2.54362204572139,-0.636309800095166,
3.38598362134397));
#48776=CARTESIAN_POINT('Ctrl Pts',(2.4807969499755,-0.319434907277143,3.4290724767243));
#48777=CARTESIAN_POINT('Ctrl Pts',(2.45461066784083,-0.158333333333325,
3.44959903115181));
#48778=CARTESIAN_POINT('Ctrl Pts',(2.43210511511045,0.158333333333327,3.43482545787348));
#48779=CARTESIAN_POINT('Ctrl Pts',(2.43594690083246,0.319434907277153,3.39958946421165));
#48780=CARTESIAN_POINT('Ctrl Pts',(2.45260174599739,0.636309800095177,3.32627726736606));
#48781=CARTESIAN_POINT('Ctrl Pts',(2.47315200888497,0.794772684000802,3.26581631617366));
#48782=CARTESIAN_POINT('Ctrl Pts',(2.51186915916835,1.06847604194575,3.18514950803714));
#48783=CARTESIAN_POINT('Ctrl Pts',(2.531519170011,1.18514270861309,3.15145192925572));
#48784=CARTESIAN_POINT('Ctrl Pts',(2.55405997195039,1.30000000000196,3.11897444393546));
#48785=CARTESIAN_POINT('Ctrl Pts',(2.73578893667187,-1.30000000000268,3.25590696673737));
#48786=CARTESIAN_POINT('Ctrl Pts',(2.69783422254653,-1.18514270861358,3.28107360162963));
#48787=CARTESIAN_POINT('Ctrl Pts',(2.66195064570056,-1.06847604194601,3.30620396777811));
#48788=CARTESIAN_POINT('Ctrl Pts',(2.58383714614665,-0.794772684000814,
3.3641763528397));
#48789=CARTESIAN_POINT('Ctrl Pts',(2.5379334691619,-0.636309800095167,3.4077814403611));
#48790=CARTESIAN_POINT('Ctrl Pts',(2.47500953345229,-0.319434907277144,
3.45092863049741));
#48791=CARTESIAN_POINT('Ctrl Pts',(2.44858806405404,-0.158333333333325,
3.47030416649335));
#48792=CARTESIAN_POINT('Ctrl Pts',(2.42648735108728,0.158333333333327,3.45572989129672));
#48793=CARTESIAN_POINT('Ctrl Pts',(2.4309471764933,0.319434907277153,3.42184459057));
#48794=CARTESIAN_POINT('Ctrl Pts',(2.44857027770594,0.636309800095178,3.34887924806674));
#48795=CARTESIAN_POINT('Ctrl Pts',(2.46970583260632,0.794772684000805,3.2892548202756));
#48796=CARTESIAN_POINT('Ctrl Pts',(2.50937611640074,1.06847604194575,3.2056317008609));
#48797=CARTESIAN_POINT('Ctrl Pts',(2.52943926998928,1.18514270861309,3.16980658619545));
#48798=CARTESIAN_POINT('Ctrl Pts',(2.55239378124058,1.30000000000196,3.13435370671735));
#48799=CARTESIAN_POINT('Ctrl Pts',(2.73421818102398,-1.30000000000268,3.2681977674749));
#48800=CARTESIAN_POINT('Ctrl Pts',(2.69571278637597,-1.18514270861358,3.29563003990244));
#48801=CARTESIAN_POINT('Ctrl Pts',(2.65934320270405,-1.06847604194601,3.322376510302));
#48802=CARTESIAN_POINT('Ctrl Pts',(2.58025633933426,-0.794772684000817,
3.38258186765897));
#48803=CARTESIAN_POINT('Ctrl Pts',(2.53384358370785,-0.636309800095168,
3.42546239955407));
#48804=CARTESIAN_POINT('Ctrl Pts',(2.47040513289856,-0.319434907277144,
3.46843740070974));
#48805=CARTESIAN_POINT('Ctrl Pts',(2.44383015879977,-0.158333333333325,
3.48690345475855));
#48806=CARTESIAN_POINT('Ctrl Pts',(2.42202544186461,0.158333333333327,3.4724760370481));
#48807=CARTESIAN_POINT('Ctrl Pts',(2.42704753007698,0.319434907277154,3.4397164682609));
#48808=CARTESIAN_POINT('Ctrl Pts',(2.44555838076725,0.636309800095179,3.36708110532485));
#48809=CARTESIAN_POINT('Ctrl Pts',(2.46742269085271,0.794772684000805,3.30823367937151));
#48810=CARTESIAN_POINT('Ctrl Pts',(2.50770768141108,1.06847604194576,3.22217370120946));
#48811=CARTESIAN_POINT('Ctrl Pts',(2.52794304634436,1.18514270861309,3.18457353925629));
#48812=CARTESIAN_POINT('Ctrl Pts',(2.55097589650418,1.30000000000196,3.14662539105996));
#48813=CARTESIAN_POINT('Ctrl Pts',(2.72948351347113,-1.30000000000268,3.29195966295096));
#48814=CARTESIAN_POINT('Ctrl Pts',(2.68991926187795,-1.18514270861358,3.32394588125519));
#48815=CARTESIAN_POINT('Ctrl Pts',(2.65266915533746,-1.06847604194601,3.35397123658253));
#48816=CARTESIAN_POINT('Ctrl Pts',(2.57196009538581,-0.794772684000816,
3.41880582819428));
#48817=CARTESIAN_POINT('Ctrl Pts',(2.52487679177749,-0.63630980009517,3.46040937964688));
#48818=CARTESIAN_POINT('Ctrl Pts',(2.46094514261025,-0.319434907277145,
3.50330855480773));
#48819=CARTESIAN_POINT('Ctrl Pts',(2.43467027355434,-0.158333333333326,
3.52025618121959));
#48820=CARTESIAN_POINT('Ctrl Pts',(2.41332137892381,0.158333333333328,3.50606492220678));
#48821=CARTESIAN_POINT('Ctrl Pts',(2.41857837798631,0.319434907277154,3.47512095010223));
#48822=CARTESIAN_POINT('Ctrl Pts',(2.43834959261132,0.63630980009518,3.402918177738));
#48823=CARTESIAN_POINT('Ctrl Pts',(2.46111398918522,0.794772684000808,3.34541583863585));
#48824=CARTESIAN_POINT('Ctrl Pts',(2.50354324361101,1.06847604194576,3.25490000136031));
#48825=CARTESIAN_POINT('Ctrl Pts',(2.52487969584024,1.18514270861309,3.2140856974905));
#48826=CARTESIAN_POINT('Ctrl Pts',(2.54918654821652,1.30000000000196,3.17163804176526));
#48827=CARTESIAN_POINT('Ctrl Pts',(2.72369170179333,-1.3000000000027,3.31849454912433));
#48828=CARTESIAN_POINT('Ctrl Pts',(2.68211479421324,-1.18514270861361,3.35520246504919));
#48829=CARTESIAN_POINT('Ctrl Pts',(2.64332497335363,-1.06847604194603,3.38864640930431));
#48830=CARTESIAN_POINT('Ctrl Pts',(2.56015145517037,-0.794772684000832,
3.45836818345907));
#48831=CARTESIAN_POINT('Ctrl Pts',(2.5128150583507,-0.636309800095181,3.49875698222628));
#48832=CARTESIAN_POINT('Ctrl Pts',(2.44867383136127,-0.319434907277151,
3.54174909975053));
#48833=CARTESIAN_POINT('Ctrl Pts',(2.42314097812259,-0.158333333333328,
3.55722010290175));
#48834=CARTESIAN_POINT('Ctrl Pts',(2.40257018414566,0.15833333333333,3.54344456141889));
#48835=CARTESIAN_POINT('Ctrl Pts',(2.4078959153891,0.319434907277158,3.51444953593751));
#48836=CARTESIAN_POINT('Ctrl Pts',(2.42939514255243,0.636309800095189,3.44288530588052));
#48837=CARTESIAN_POINT('Ctrl Pts',(2.45410708551317,0.794772684000823,3.38732971658239));
#48838=CARTESIAN_POINT('Ctrl Pts',(2.49855328806516,1.06847604194578,3.29162722367303));
#48839=CARTESIAN_POINT('Ctrl Pts',(2.5206580533214,1.18514270861311,3.24698429416533));
#48840=CARTESIAN_POINT('Ctrl Pts',(2.54562846964318,1.30000000000198,3.19912449820366));
#48841=CARTESIAN_POINT('Ctrl Pts',(2.71438902447655,-1.30000000000271,3.35633531279331));
#48842=CARTESIAN_POINT('Ctrl Pts',(2.67060459789709,-1.18514270861361,3.40019886347495));
#48843=CARTESIAN_POINT('Ctrl Pts',(2.62994469888926,-1.06847604194604,3.43874235686978));
#48844=CARTESIAN_POINT('Ctrl Pts',(2.54323048194666,-0.794772684000838,
3.51549514060459));
#48845=CARTESIAN_POINT('Ctrl Pts',(2.49451201224887,-0.636309800095185,
3.5536067747533));
#48846=CARTESIAN_POINT('Ctrl Pts',(2.42861015874721,-0.319434907277153,
3.59593822555784));
#48847=CARTESIAN_POINT('Ctrl Pts',(2.40230917701206,-0.158333333333329,
3.60824880302406));
#48848=CARTESIAN_POINT('Ctrl Pts',(2.38278887602257,0.158333333333331,3.59506410414001));
#48849=CARTESIAN_POINT('Ctrl Pts',(2.39033055985627,0.31943490727716,3.57007363504647));
#48850=CARTESIAN_POINT('Ctrl Pts',(2.41492085725434,0.636309800095193,3.49985764591031));
#48851=CARTESIAN_POINT('Ctrl Pts',(2.44086394794052,0.794772684000828,3.44643060171251));
#48852=CARTESIAN_POINT('Ctrl Pts',(2.48924552311111,1.06847604194578,3.34375288445897));
#48853=CARTESIAN_POINT('Ctrl Pts',(2.51337592653575,1.18514270861312,3.29400773222963));
#48854=CARTESIAN_POINT('Ctrl Pts',(2.54069414220766,1.30000000000199,3.23896280698576));
#48855=CARTESIAN_POINT('Ctrl Pts',(2.70713559815903,-1.30000000000272,3.38544760191281));
#48856=CARTESIAN_POINT('Ctrl Pts',(2.66108666670748,-1.18514270861363,3.43457778468442));
#48857=CARTESIAN_POINT('Ctrl Pts',(2.61851679459819,-1.06847604194605,3.47683322532625));
#48858=CARTESIAN_POINT('Ctrl Pts',(2.52820919701641,-0.794772684000844,
3.55856971677326));
#48859=CARTESIAN_POINT('Ctrl Pts',(2.47766951391152,-0.63630980009519,3.5944422383161));
#48860=CARTESIAN_POINT('Ctrl Pts',(2.41092519018967,-0.319434907277155,
3.63654891312596));
#48861=CARTESIAN_POINT('Ctrl Pts',(2.38612507388147,-0.158333333333331,
3.64759825207347));
#48862=CARTESIAN_POINT('Ctrl Pts',(2.36753152447389,0.158333333333333,3.63497645717648));
#48863=CARTESIAN_POINT('Ctrl Pts',(2.37474937021344,0.319434907277166,3.61201925378152));
#48864=CARTESIAN_POINT('Ctrl Pts',(2.40156007039164,0.636309800095202,3.54274866664481));
#48865=CARTESIAN_POINT('Ctrl Pts',(2.43021686726533,0.794772684000834,3.49184456180963));
#48866=CARTESIAN_POINT('Ctrl Pts',(2.48166834545503,1.06847604194579,3.38378694257873));
#48867=CARTESIAN_POINT('Ctrl Pts',(2.50705731805605,1.18514270861313,3.32994473516944));
#48868=CARTESIAN_POINT('Ctrl Pts',(2.53556382481485,1.300000000002,3.26903445978667));
#48869=CARTESIAN_POINT('Ctrl Pts',(2.69935280611515,-1.30000000000273,3.4142463597142));
#48870=CARTESIAN_POINT('Ctrl Pts',(2.65091913730647,-1.18514270861363,3.46848708019251));
#48871=CARTESIAN_POINT('Ctrl Pts',(2.60632467787954,-1.06847604194605,3.51431952016311));
#48872=CARTESIAN_POINT('Ctrl Pts',(2.51217189721573,-0.794772684000848,
3.6007768151995));
#48873=CARTESIAN_POINT('Ctrl Pts',(2.45996887884519,-0.636309800095194,
3.63447452807947));
#48874=CARTESIAN_POINT('Ctrl Pts',(2.39156773297291,-0.319434907277157,
3.67585824322938));
#48875=CARTESIAN_POINT('Ctrl Pts',(2.36677677594353,-0.158333333333331,
3.68480618023814));
#48876=CARTESIAN_POINT('Ctrl Pts',(2.34892395383732,0.158333333333334,3.67266358137842));
#48877=CARTESIAN_POINT('Ctrl Pts',(2.35719358301814,0.319434907277165,3.65251724971171));
#48878=CARTESIAN_POINT('Ctrl Pts',(2.38651765777384,0.636309800095202,3.58447665900661));
#48879=CARTESIAN_POINT('Ctrl Pts',(2.41666791960658,0.794772684000837,3.53559913548754));
#48880=CARTESIAN_POINT('Ctrl Pts',(2.47198053053757,1.0684760419458,3.42268260092749));
#48881=CARTESIAN_POINT('Ctrl Pts',(2.49935282260984,1.18514270861314,3.36515185339334));
#48882=CARTESIAN_POINT('Ctrl Pts',(2.53015462701651,1.30000000000201,3.29896774216626));
#48883=CARTESIAN_POINT('Ctrl Pts',(2.69303318688899,-1.30000000000273,3.43401667925717));
#48884=CARTESIAN_POINT('Ctrl Pts',(2.64282935584548,-1.18514270861363,3.49194305826096));
#48885=CARTESIAN_POINT('Ctrl Pts',(2.59667057889062,-1.06847604194605,3.54031522326202));
#48886=CARTESIAN_POINT('Ctrl Pts',(2.49937945424869,-0.79477268400085,3.62999245557226));
#48887=CARTESIAN_POINT('Ctrl Pts',(2.44467031211378,-0.636309800095196,
3.66134362032266));
#48888=CARTESIAN_POINT('Ctrl Pts',(2.37628184723862,-0.319434907277159,
3.70291872218279));
#48889=CARTESIAN_POINT('Ctrl Pts',(2.35498741875346,-0.158333333333332,
3.71239366789374));
#48890=CARTESIAN_POINT('Ctrl Pts',(2.33816277204694,0.158333333333334,3.70090332782829));
#48891=CARTESIAN_POINT('Ctrl Pts',(2.34446568277421,0.319434907277166,3.68123393892042));
#48892=CARTESIAN_POINT('Ctrl Pts',(2.37484960204422,0.636309800095205,3.61361419306542));
#48893=CARTESIAN_POINT('Ctrl Pts',(2.4070943212819,0.794772684000841,3.56670915350597));
#48894=CARTESIAN_POINT('Ctrl Pts',(2.46534344402644,1.0684760419458,3.45033103710803));
#48895=CARTESIAN_POINT('Ctrl Pts',(2.49412215195454,1.18514270861314,3.39011485922067));
#48896=CARTESIAN_POINT('Ctrl Pts',(2.52646568091726,1.30000000000202,3.32005827780055));
#48897=CARTESIAN_POINT('Ctrl Pts',(2.68881095174143,-1.30000000000273,3.44818305017374));
#48898=CARTESIAN_POINT('Ctrl Pts',(2.63669007242356,-1.18514270861363,3.50812985442003));
#48899=CARTESIAN_POINT('Ctrl Pts',(2.58929489284264,-1.06847604194606,3.55806783061209));
#48900=CARTESIAN_POINT('Ctrl Pts',(2.49071985840326,-0.794772684000852,
3.65031215060882));
#48901=CARTESIAN_POINT('Ctrl Pts',(2.43767831743658,-0.636309800095195,
3.68199369795424));
#48902=CARTESIAN_POINT('Ctrl Pts',(2.37003893525433,-0.319434907277157,
3.72404063399689));
#48903=CARTESIAN_POINT('Ctrl Pts',(2.34957190091252,-0.158333333333332,
3.73290265012859));
#48904=CARTESIAN_POINT('Ctrl Pts',(2.33223463491217,0.158333333333334,3.72113567254182));
#48905=CARTESIAN_POINT('Ctrl Pts',(2.33644686910212,0.319434907277166,3.70137589803932));
#48906=CARTESIAN_POINT('Ctrl Pts',(2.36656658377296,0.636309800095204,3.63358993894587));
#48907=CARTESIAN_POINT('Ctrl Pts',(2.39985803922327,0.794772684000837,3.5879471723796));
#48908=CARTESIAN_POINT('Ctrl Pts',(2.45974497985535,1.0684760419458,3.46916916360371));
#48909=CARTESIAN_POINT('Ctrl Pts',(2.48941623434979,1.18514270861314,3.40715690064001));
#48910=CARTESIAN_POINT('Ctrl Pts',(2.52283590576881,1.30000000000202,3.33454697355289));
#48911=CARTESIAN_POINT('Ctrl Pts',(2.6829039520614,-1.30000000000273,3.4648600390468));
#48912=CARTESIAN_POINT('Ctrl Pts',(2.6282815105453,-1.18514270861363,3.52754575513347));
#48913=CARTESIAN_POINT('Ctrl Pts',(2.5794116548837,-1.06847604194606,3.57971224017919));
#48914=CARTESIAN_POINT('Ctrl Pts',(2.47980213604945,-0.794772684000851,
3.67592572843441));
#48915=CARTESIAN_POINT('Ctrl Pts',(2.42997521426678,-0.636309800095196,
3.70885360105528));
#48916=CARTESIAN_POINT('Ctrl Pts',(2.36410441800568,-0.319434907277158,
3.75213277591685));
#48917=CARTESIAN_POINT('Ctrl Pts',(2.34457233682742,-0.158333333333332,
3.76008693715092));
#48918=CARTESIAN_POINT('Ctrl Pts',(2.32729940694406,0.158333333333334,3.74838365192667));
#48919=CARTESIAN_POINT('Ctrl Pts',(2.33032257384052,0.319434907277166,3.72943266456022));
#48920=CARTESIAN_POINT('Ctrl Pts',(2.35945341085199,0.636309800095205,3.66087573405795));
#48921=CARTESIAN_POINT('Ctrl Pts',(2.3912258713284,0.794772684000838,3.61494599460186));
#48922=CARTESIAN_POINT('Ctrl Pts',(2.45236846246531,1.0684760419458,3.49226103554975));
#48923=CARTESIAN_POINT('Ctrl Pts',(2.48325251042926,1.18514270861314,3.42782901639173));
#48924=CARTESIAN_POINT('Ctrl Pts',(2.5185542442102,1.30000000000202,3.35207075092373));
#48925=CARTESIAN_POINT('Ctrl Pts',(2.67899628993141,-1.30000000000274,3.47627965711681));
#48926=CARTESIAN_POINT('Ctrl Pts',(2.62148033775266,-1.18514270861364,3.54015492010688));
#48927=CARTESIAN_POINT('Ctrl Pts',(2.57119727859278,-1.06847604194606,3.59350430823753));
#48928=CARTESIAN_POINT('Ctrl Pts',(2.47174278265131,-0.794772684000851,
3.69243519070814));
#48929=CARTESIAN_POINT('Ctrl Pts',(2.42808446301743,-0.636309800095197,
3.72772405735239));
#48930=CARTESIAN_POINT('Ctrl Pts',(2.36541685428271,-0.319434907277159,
3.77235288610033));
#48931=CARTESIAN_POINT('Ctrl Pts',(2.346171214744,-0.158333333333332,3.77926048785863));
#48932=CARTESIAN_POINT('Ctrl Pts',(2.32904419103436,0.158333333333334,3.76759838522902));
#48933=CARTESIAN_POINT('Ctrl Pts',(2.33182399968641,0.319434907277167,3.74960279228391));
#48934=CARTESIAN_POINT('Ctrl Pts',(2.35825829213827,0.636309800095206,3.68004967650707));
#48935=CARTESIAN_POINT('Ctrl Pts',(2.38472809612599,0.79477268400084,3.63256364253536));
#48936=CARTESIAN_POINT('Ctrl Pts',(2.44568313888403,1.0684760419458,3.5071297018696));
#48937=CARTESIAN_POINT('Ctrl Pts',(2.47774091685542,1.18514270861315,3.44130295284402));
#48938=CARTESIAN_POINT('Ctrl Pts',(2.51547129339511,1.30000000000202,3.36394515992168));
#48939=CARTESIAN_POINT('Ctrl Pts',(2.67879510330428,-1.30000000000274,3.4848793737609));
#48940=CARTESIAN_POINT('Ctrl Pts',(2.62131393065235,-1.18514270861364,3.54850574591786));
#48941=CARTESIAN_POINT('Ctrl Pts',(2.57136732543471,-1.06847604194606,3.60177947255492));
#48942=CARTESIAN_POINT('Ctrl Pts',(2.4733870336565,-0.794772684000851,3.70093575626798));
#48943=CARTESIAN_POINT('Ctrl Pts',(2.4321376027347,-0.636309800095197,3.73710797922267));
#48944=CARTESIAN_POINT('Ctrl Pts',(2.37107459905216,-0.319434907277159,
3.7822562302209));
#48945=CARTESIAN_POINT('Ctrl Pts',(2.35179040064045,-0.158333333333332,
3.78919923474563));
#48946=CARTESIAN_POINT('Ctrl Pts',(2.33489442655109,0.158333333333334,3.77758912426359));
#48947=CARTESIAN_POINT('Ctrl Pts',(2.33820931733128,0.319434907277167,3.75969933838138));
#48948=CARTESIAN_POINT('Ctrl Pts',(2.36296888549193,0.636309800095206,3.68955097462145));
#48949=CARTESIAN_POINT('Ctrl Pts',(2.38602389855414,0.79477268400084,3.64077817435492));
#48950=CARTESIAN_POINT('Ctrl Pts',(2.4456425950795,1.0684760419458,3.5151865828561));
#48951=CARTESIAN_POINT('Ctrl Pts',(2.47765621323778,1.18514270861315,3.44956557353161));
#48952=CARTESIAN_POINT('Ctrl Pts',(2.51587672491888,1.30000000000202,3.37268750121553));
#48953=CARTESIAN_POINT('Ctrl Pts',(2.67879510330291,-1.3,3.48487937376242));
#48954=CARTESIAN_POINT('Ctrl Pts',(2.62131393065155,-1.18514270861178,3.54850574591871));
#48955=CARTESIAN_POINT('Ctrl Pts',(2.57136732543437,-1.06847604194512,3.60177947255526));
#48956=CARTESIAN_POINT('Ctrl Pts',(2.4733870336565,-0.794772684000851,3.70093575626798));
#48957=CARTESIAN_POINT('Ctrl Pts',(2.4321376027347,-0.636309800095197,3.73710797922267));
#48958=CARTESIAN_POINT('Ctrl Pts',(2.37107459905216,-0.319434907277159,
3.7822562302209));
#48959=CARTESIAN_POINT('Ctrl Pts',(2.35179040064045,-0.158333333333332,
3.78919923474563));
#48960=CARTESIAN_POINT('Ctrl Pts',(2.33489442655109,0.158333333333334,3.77758912426359));
#48961=CARTESIAN_POINT('Ctrl Pts',(2.33820931733128,0.319434907277167,3.75969933838138));
#48962=CARTESIAN_POINT('Ctrl Pts',(2.36296888549193,0.636309800095206,3.68955097462145));
#48963=CARTESIAN_POINT('Ctrl Pts',(2.38602389855414,0.79477268400084,3.64077817435492));
#48964=CARTESIAN_POINT('Ctrl Pts',(2.44564259507935,1.06847604194511,3.51518658285641));
#48965=CARTESIAN_POINT('Ctrl Pts',(2.47765621323741,1.18514270861178,3.44956557353238));
#48966=CARTESIAN_POINT('Ctrl Pts',(2.5158767249182,1.3,3.37268750121688));
#48967=CARTESIAN_POINT('',(2.73378250710872,-1.2,3.07338719967255));
#48968=CARTESIAN_POINT('Ctrl Pts',(2.73378250710872,-1.2,3.07338719967255));
#48969=CARTESIAN_POINT('Ctrl Pts',(2.7357577738517,-1.2168297082725,3.09488352363361));
#48970=CARTESIAN_POINT('Ctrl Pts',(2.73868491450415,-1.23325632720283,3.1165994859212));
#48971=CARTESIAN_POINT('Ctrl Pts',(2.7416199046039,-1.25866340409469,3.14922928548443));
#48972=CARTESIAN_POINT('Ctrl Pts',(2.74261161481058,-1.26676846238795,3.15969392154395));
#48973=CARTESIAN_POINT('Ctrl Pts',(2.74425212505128,-1.28145222431456,3.17857382838032));
#48974=CARTESIAN_POINT('Ctrl Pts',(2.74535078767749,-1.29188212206828,3.19196062087639));
#48975=CARTESIAN_POINT('Ctrl Pts',(2.74593693625412,-1.29845800981103,3.20033871480917));
#48976=CARTESIAN_POINT('Ctrl Pts',(2.74600242614502,-1.29922960688975,3.20131966196731));
#48977=CARTESIAN_POINT('Ctrl Pts',(2.74606318243978,-1.30000000000266,3.20229603421878));
#48978=CARTESIAN_POINT('',(2.60194865074806,-0.653834841416699,2.98901873447389));
#48979=CARTESIAN_POINT('Ctrl Pts',(2.60194865076408,-0.653834841416013,
2.9890187344531));
#48980=CARTESIAN_POINT('Ctrl Pts',(2.61576784735542,-0.717856062975954,
2.99755756131031));
#48981=CARTESIAN_POINT('Ctrl Pts',(2.62702784454639,-0.763802346224156,
3.00458546056376));
#48982=CARTESIAN_POINT('Ctrl Pts',(2.6708664756529,-0.949540328209464,3.03224190415644));
#48983=CARTESIAN_POINT('Ctrl Pts',(2.69381959728105,-1.04583430085205,3.04691272554419));
#48984=CARTESIAN_POINT('Ctrl Pts',(2.73378250710872,-1.2,3.07338719967255));
#48985=CARTESIAN_POINT('',(2.48224831221869,0.653834841531101,2.91736724473281));
#48986=CARTESIAN_POINT('Ctrl Pts',(2.48224831221869,0.6538348415311,2.91736724473281));
#48987=CARTESIAN_POINT('Ctrl Pts',(2.47847890444284,0.57579108168247,2.95887093612136));
#48988=CARTESIAN_POINT('Ctrl Pts',(2.47600131421347,0.493921151117629,2.99371026845236));
#48989=CARTESIAN_POINT('Ctrl Pts',(2.47494821893025,0.338203801397658,3.04438967831501));
#48990=CARTESIAN_POINT('Ctrl Pts',(2.47583991291864,0.265715671510878,3.06228273998636));
#48991=CARTESIAN_POINT('Ctrl Pts',(2.48131031772334,0.129742783470322,3.08607547669105));
#48992=CARTESIAN_POINT('Ctrl Pts',(2.48530809277579,0.0666420753572764,
3.09333289107435));
#48993=CARTESIAN_POINT('Ctrl Pts',(2.49656212049516,-0.0595517108187469,
3.10050296874366));
#48994=CARTESIAN_POINT('Ctrl Pts',(2.5038959934916,-0.122800467221057,3.10048501116942));
#48995=CARTESIAN_POINT('Ctrl Pts',(2.52282604869386,-0.260148767886255,
3.0919924718622));
#48996=CARTESIAN_POINT('Ctrl Pts',(2.53495894889212,-0.333947398986749,
3.08197900091245));
#48997=CARTESIAN_POINT('Ctrl Pts',(2.56433428307125,-0.491233239064203,
3.04808483264696));
#48998=CARTESIAN_POINT('Ctrl Pts',(2.58224468806056,-0.574172289671449,
3.02219719078165));
#48999=CARTESIAN_POINT('Ctrl Pts',(2.60194865076353,-0.653834841428418,
2.98901873451122));
#49000=CARTESIAN_POINT('',(2.54446987687431,1.2,2.95404038576917));
#49001=CARTESIAN_POINT('Ctrl Pts',(2.54446987687431,1.2,2.95404038576917));
#49002=CARTESIAN_POINT('Ctrl Pts',(2.53342410082955,1.13191853104164,2.94742100005518));
#49003=CARTESIAN_POINT('Ctrl Pts',(2.51940373078794,1.03495910820303,2.93908009495677));
#49004=CARTESIAN_POINT('Ctrl Pts',(2.49230898042137,0.795381693602028,2.9231940999664));
#49005=CARTESIAN_POINT('Ctrl Pts',(2.48794042596448,0.741811055998074,2.92066643953794));
#49006=CARTESIAN_POINT('Ctrl Pts',(2.48224831221869,0.653834841531101,2.91736724473281));
#49007=CARTESIAN_POINT('Ctrl Pts',(2.55661739137893,1.29999999999998,3.07856729836589));
#49008=CARTESIAN_POINT('Ctrl Pts',(2.55522672776558,1.28313639696102,3.05785996776105));
#49009=CARTESIAN_POINT('Ctrl Pts',(2.55298386248016,1.26654349104865,3.03699927317881));
#49010=CARTESIAN_POINT('Ctrl Pts',(2.54970999277994,1.23742205883468,3.0008947194452));
#49011=CARTESIAN_POINT('Ctrl Pts',(2.54814390762507,1.2200626218235,2.97963140604976));
#49012=CARTESIAN_POINT('Ctrl Pts',(2.54446987687431,1.2,2.95404038576917));
#49013=CARTESIAN_POINT('Ctrl Pts',(2.67879510330291,-1.3,3.48487937376242));
#49014=CARTESIAN_POINT('Ctrl Pts',(2.62131393065155,-1.18514270861178,3.54850574591871));
#49015=CARTESIAN_POINT('Ctrl Pts',(2.57136732543437,-1.06847604194512,3.60177947255526));
#49016=CARTESIAN_POINT('Ctrl Pts',(2.4733870336565,-0.794772684000851,3.70093575626798));
#49017=CARTESIAN_POINT('Ctrl Pts',(2.43213760273471,-0.636309800095197,
3.73710797922267));
#49018=CARTESIAN_POINT('Ctrl Pts',(2.37107459905216,-0.319434907277159,
3.7822562302209));
#49019=CARTESIAN_POINT('Ctrl Pts',(2.35179040064045,-0.158333333333332,
3.78919923474564));
#49020=CARTESIAN_POINT('Ctrl Pts',(2.33489442655109,0.158333333333334,3.77758912426359));
#49021=CARTESIAN_POINT('Ctrl Pts',(2.33820931733128,0.319434907277167,3.75969933838138));
#49022=CARTESIAN_POINT('Ctrl Pts',(2.36296888549193,0.636309800095206,3.68955097462145));
#49023=CARTESIAN_POINT('Ctrl Pts',(2.38602389855414,0.79477268400084,3.64077817435492));
#49024=CARTESIAN_POINT('Ctrl Pts',(2.44564259507935,1.06847604194511,3.51518658285641));
#49025=CARTESIAN_POINT('Ctrl Pts',(2.47765621323741,1.18514270861178,3.44956557353238));
#49026=CARTESIAN_POINT('Ctrl Pts',(2.5158767249182,1.3,3.37268750121688));
#49027=CARTESIAN_POINT('Ctrl Pts',(2.74004401157309,-1.3,3.53143772972948));
#49028=CARTESIAN_POINT('Ctrl Pts',(2.68128836180793,-1.18514270861178,3.59389081034382));
#49029=CARTESIAN_POINT('Ctrl Pts',(2.63048511284273,-1.06847604194512,3.64631488384437));
#49030=CARTESIAN_POINT('Ctrl Pts',(2.53149108129824,-0.794772684000851,
3.74425596830184));
#49031=CARTESIAN_POINT('Ctrl Pts',(2.49090436112714,-0.636309800095197,
3.78070353178887));
#49032=CARTESIAN_POINT('Ctrl Pts',(2.43050771496334,-0.319434907277159,
3.82587729417744));
#49033=CARTESIAN_POINT('Ctrl Pts',(2.41232163607126,-0.158333333333332,
3.83339959597414));
#49034=CARTESIAN_POINT('Ctrl Pts',(2.3956366485587,0.158333333333334,3.82149908738234));
#49035=CARTESIAN_POINT('Ctrl Pts',(2.39806125730008,0.319434907277167,3.80274394047715));
#49036=CARTESIAN_POINT('Ctrl Pts',(2.42259064688909,0.636309800095206,3.73196971651));
#49037=CARTESIAN_POINT('Ctrl Pts',(2.4451790066595,0.79477268400084,3.68265172576932));
#49038=CARTESIAN_POINT('Ctrl Pts',(2.50626668917078,1.06847604194511,3.55764874086027));
#49039=CARTESIAN_POINT('Ctrl Pts',(2.53935309295667,1.18514270861178,3.49257989089658));
#49040=CARTESIAN_POINT('Ctrl Pts',(2.57908330629107,1.3,3.41655135131922));
#49041=CARTESIAN_POINT('Ctrl Pts',(2.80129291984328,-1.3,3.57799608569655));
#49042=CARTESIAN_POINT('Ctrl Pts',(2.7412627929643,-1.18514270861178,3.63927587476892));
#49043=CARTESIAN_POINT('Ctrl Pts',(2.68960290025109,-1.06847604194512,3.69085029513349));
#49044=CARTESIAN_POINT('Ctrl Pts',(2.58959512893997,-0.794772684000851,
3.7875761803357));
#49045=CARTESIAN_POINT('Ctrl Pts',(2.54967111951957,-0.636309800095197,
3.82429908435506));
#49046=CARTESIAN_POINT('Ctrl Pts',(2.48994083087453,-0.319434907277159,
3.86949835813398));
#49047=CARTESIAN_POINT('Ctrl Pts',(2.47285287150207,-0.158333333333332,
3.87759995720265));
#49048=CARTESIAN_POINT('Ctrl Pts',(2.4563788705663,0.158333333333334,3.86540905050109));
#49049=CARTESIAN_POINT('Ctrl Pts',(2.45791319726889,0.319434907277167,3.84578854257292));
#49050=CARTESIAN_POINT('Ctrl Pts',(2.48221240828625,0.636309800095206,3.77438845839854));
#49051=CARTESIAN_POINT('Ctrl Pts',(2.50433411476485,0.79477268400084,3.72452527718373));
#49052=CARTESIAN_POINT('Ctrl Pts',(2.5668907832622,1.06847604194511,3.60011089886413));
#49053=CARTESIAN_POINT('Ctrl Pts',(2.60104997267594,1.18514270861178,3.53559420826078));
#49054=CARTESIAN_POINT('Ctrl Pts',(2.64228988766393,1.3,3.46041520142157));
#49055=CARTESIAN_POINT('Ctrl Pts',(2.86254182811346,-1.3,3.62455444166361));
#49056=CARTESIAN_POINT('Ctrl Pts',(2.80123722412067,-1.18514270861178,3.68466093919403));
#49057=CARTESIAN_POINT('Ctrl Pts',(2.74872068765945,-1.06847604194512,3.73538570642261));
#49058=CARTESIAN_POINT('Ctrl Pts',(2.6476991765817,-0.794772684000851,3.83089639236955));
#49059=CARTESIAN_POINT('Ctrl Pts',(2.60843787791201,-0.636309800095197,
3.86789463692126));
#49060=CARTESIAN_POINT('Ctrl Pts',(2.54937394678571,-0.319434907277159,
3.91311942209052));
#49061=CARTESIAN_POINT('Ctrl Pts',(2.53338410693289,-0.158333333333332,
3.92180031843115));
#49062=CARTESIAN_POINT('Ctrl Pts',(2.5171210925739,0.158333333333334,3.90931901361984));
#49063=CARTESIAN_POINT('Ctrl Pts',(2.5177651372377,0.319434907277167,3.88883314466868));
#49064=CARTESIAN_POINT('Ctrl Pts',(2.54183416968341,0.636309800095206,3.81680720028709));
#49065=CARTESIAN_POINT('Ctrl Pts',(2.56348922287021,0.79477268400084,3.76639882859814));
#49066=CARTESIAN_POINT('Ctrl Pts',(2.62751487735363,1.06847604194511,3.64257305686799));
#49067=CARTESIAN_POINT('Ctrl Pts',(2.6627468523952,1.18514270861178,3.57860852562499));
#49068=CARTESIAN_POINT('Ctrl Pts',(2.70549646903679,1.3,3.50427905152391));
#49069=CARTESIAN_POINT('Ctrl Pts',(2.86254182811346,-1.3,3.62455444166361));
#49070=CARTESIAN_POINT('Ctrl Pts',(2.80123722412067,-1.18514270861178,3.68466093919403));
#49071=CARTESIAN_POINT('Ctrl Pts',(2.74872068765946,-1.06847604194512,3.73538570642261));
#49072=CARTESIAN_POINT('Ctrl Pts',(2.6476991765817,-0.794772684000851,3.83089639236955));
#49073=CARTESIAN_POINT('Ctrl Pts',(2.60843787791201,-0.636309800095197,
3.86789463692126));
#49074=CARTESIAN_POINT('Ctrl Pts',(2.54937394678571,-0.319434907277159,
3.91311942209052));
#49075=CARTESIAN_POINT('Ctrl Pts',(2.53338410693288,-0.158333333333332,
3.92180031843115));
#49076=CARTESIAN_POINT('Ctrl Pts',(2.5171210925739,0.158333333333334,3.90931901361984));
#49077=CARTESIAN_POINT('Ctrl Pts',(2.5177651372377,0.319434907277167,3.88883314466868));
#49078=CARTESIAN_POINT('Ctrl Pts',(2.54183416968341,0.636309800095206,3.81680720028709));
#49079=CARTESIAN_POINT('Ctrl Pts',(2.5634892228702,0.79477268400084,3.76639882859813));
#49080=CARTESIAN_POINT('Ctrl Pts',(2.62751487735363,1.06847604194511,3.64257305686799));
#49081=CARTESIAN_POINT('Ctrl Pts',(2.6627468523952,1.18514270861178,3.57860852562499));
#49082=CARTESIAN_POINT('Ctrl Pts',(2.70549646903679,1.3,3.50427905152391));
#49083=CARTESIAN_POINT('Ctrl Pts',(2.86254182811642,-1.30000000000554,3.62455444166071));
#49084=CARTESIAN_POINT('Ctrl Pts',(2.80123722412236,-1.18514270861553,3.6846609391924));
#49085=CARTESIAN_POINT('Ctrl Pts',(2.74872068766016,-1.06847604194702,3.73538570642194));
#49086=CARTESIAN_POINT('Ctrl Pts',(2.6476991765817,-0.794772684000851,3.83089639236955));
#49087=CARTESIAN_POINT('Ctrl Pts',(2.60843787791201,-0.636309800095197,
3.86789463692126));
#49088=CARTESIAN_POINT('Ctrl Pts',(2.54937394678571,-0.319434907277159,
3.91311942209052));
#49089=CARTESIAN_POINT('Ctrl Pts',(2.53338410693289,-0.158333333333332,
3.92180031843115));
#49090=CARTESIAN_POINT('Ctrl Pts',(2.5171210925739,0.158333333333334,3.90931901361984));
#49091=CARTESIAN_POINT('Ctrl Pts',(2.5177651372377,0.319434907277167,3.88883314466868));
#49092=CARTESIAN_POINT('Ctrl Pts',(2.54183416968341,0.636309800095206,3.81680720028709));
#49093=CARTESIAN_POINT('Ctrl Pts',(2.56348922287021,0.79477268400084,3.76639882859813));
#49094=CARTESIAN_POINT('Ctrl Pts',(2.62751487735364,1.06847604194517,3.64257305686796));
#49095=CARTESIAN_POINT('Ctrl Pts',(2.66274685239524,1.18514270861189,3.57860852562492));
#49096=CARTESIAN_POINT('Ctrl Pts',(2.70549646903686,1.30000000000017,3.5042790515238));
#49097=CARTESIAN_POINT('Ctrl Pts',(2.87098157396645,-1.30000000000554,3.62223849797031));
#49098=CARTESIAN_POINT('Ctrl Pts',(2.80906926848047,-1.18514270861553,3.68202709109595));
#49099=CARTESIAN_POINT('Ctrl Pts',(2.7563707080711,-1.06847604194702,3.73285743386342));
#49100=CARTESIAN_POINT('Ctrl Pts',(2.65591208554583,-0.794772684000851,
3.8295903438114));
#49101=CARTESIAN_POINT('Ctrl Pts',(2.61892980277957,-0.636309800095197,
3.86943861486421));
#49102=CARTESIAN_POINT('Ctrl Pts',(2.56094950437883,-0.319434907277159,
3.91607221576025));
#49103=CARTESIAN_POINT('Ctrl Pts',(2.54469368652178,-0.158333333333332,
3.92427691498543));
#49104=CARTESIAN_POINT('Ctrl Pts',(2.52830982643484,0.158333333333334,3.91159193538119));
#49105=CARTESIAN_POINT('Ctrl Pts',(2.52893211645302,0.319434907277167,3.89115367810119));
#49106=CARTESIAN_POINT('Ctrl Pts',(2.55201129877011,0.636309800095206,3.81776217390742));
#49107=CARTESIAN_POINT('Ctrl Pts',(2.57208184262637,0.79477268400084,3.76533578503149));
#49108=CARTESIAN_POINT('Ctrl Pts',(2.63543757364827,1.06847604194517,3.64017761464239));
#49109=CARTESIAN_POINT('Ctrl Pts',(2.67063753705879,1.18514270861189,3.57586971600027));
#49110=CARTESIAN_POINT('Ctrl Pts',(2.71361311548166,1.30000000000017,3.5014302531102));
#49111=CARTESIAN_POINT('Ctrl Pts',(2.88130082125157,-1.30000000000553,3.61561587076792));
#49112=CARTESIAN_POINT('Ctrl Pts',(2.82016066715714,-1.18514270861553,3.67260438117326));
#49113=CARTESIAN_POINT('Ctrl Pts',(2.76842861614806,-1.06847604194701,3.72189205592847));
#49114=CARTESIAN_POINT('Ctrl Pts',(2.6706518295684,-0.794772684000848,3.817965973679));
#49115=CARTESIAN_POINT('Ctrl Pts',(2.63680341206716,-0.636309800095194,
3.86239125090444));
#49116=CARTESIAN_POINT('Ctrl Pts',(2.58060872343043,-0.319434907277157,
3.91128594284546));
#49117=CARTESIAN_POINT('Ctrl Pts',(2.56351725959355,-0.158333333333332,
3.92001259183717));
#49118=CARTESIAN_POINT('Ctrl Pts',(2.5470343810601,0.158333333333334,3.90718754649781));
#49119=CARTESIAN_POINT('Ctrl Pts',(2.54853327574153,0.319434907277167,3.88612733727331));
#49120=CARTESIAN_POINT('Ctrl Pts',(2.56934003151366,0.636309800095205,3.81010783163589));
#49121=CARTESIAN_POINT('Ctrl Pts',(2.58529810153918,0.794772684000837,3.75258095831877));
#49122=CARTESIAN_POINT('Ctrl Pts',(2.64602744646709,1.06847604194516,3.62811825223073));
#49123=CARTESIAN_POINT('Ctrl Pts',(2.68053526324991,1.18514270861188,3.5655147599639));
#49124=CARTESIAN_POINT('Ctrl Pts',(2.72326341364027,1.30000000000016,3.49418306909796));
#49125=CARTESIAN_POINT('Ctrl Pts',(2.89657701929988,-1.30000000000553,3.60605436272481));
#49126=CARTESIAN_POINT('Ctrl Pts',(2.83785983129768,-1.18514270861553,3.66028459218314));
#49127=CARTESIAN_POINT('Ctrl Pts',(2.78806648256914,-1.06847604194702,3.70767886828241));
#49128=CARTESIAN_POINT('Ctrl Pts',(2.69364973981185,-0.794772684000849,
3.80137670747613));
#49129=CARTESIAN_POINT('Ctrl Pts',(2.66057259609715,-0.636309800095194,
3.84718746245279));
#49130=CARTESIAN_POINT('Ctrl Pts',(2.60545054146012,-0.319434907277157,
3.89681571822015));
#49131=CARTESIAN_POINT('Ctrl Pts',(2.58798683559333,-0.158333333333332,
3.90695072166245));
#49132=CARTESIAN_POINT('Ctrl Pts',(2.57140695597793,0.158333333333334,3.89406819926671));
#49133=CARTESIAN_POINT('Ctrl Pts',(2.57340807017908,0.319434907277166,3.87176905961988));
#49134=CARTESIAN_POINT('Ctrl Pts',(2.59248226872427,0.636309800095204,3.79443673235879));
#49135=CARTESIAN_POINT('Ctrl Pts',(2.60631386943291,0.794772684000837,3.73428739218371));
#49136=CARTESIAN_POINT('Ctrl Pts',(2.66359704128096,1.06847604194516,3.61205146082038));
#49137=CARTESIAN_POINT('Ctrl Pts',(2.69643828805896,1.18514270861188,3.55154131212699));
#49138=CARTESIAN_POINT('Ctrl Pts',(2.73732501907265,1.30000000000016,3.48343242013976));
#49139=CARTESIAN_POINT('Ctrl Pts',(2.90936639791106,-1.30000000000553,3.59827482203786));
#49140=CARTESIAN_POINT('Ctrl Pts',(2.85272180916184,-1.18514270861552,3.65068715009277));
#49141=CARTESIAN_POINT('Ctrl Pts',(2.80433520504782,-1.06847604194701,3.69666533731781));
#49142=CARTESIAN_POINT('Ctrl Pts',(2.71163006634977,-0.794772684000845,
3.78801999524921));
#49143=CARTESIAN_POINT('Ctrl Pts',(2.67698192370522,-0.636309800095192,
3.83317642236382));
#49144=CARTESIAN_POINT('Ctrl Pts',(2.62202362155589,-0.319434907277156,
3.88293393740567));
#49145=CARTESIAN_POINT('Ctrl Pts',(2.60521467878967,-0.158333333333331,
3.894953219045));
#49146=CARTESIAN_POINT('Ctrl Pts',(2.58907353697783,0.158333333333333,3.88248974574418));
#49147=CARTESIAN_POINT('Ctrl Pts',(2.59153304544427,0.319434907277166,3.85934407438143));
#49148=CARTESIAN_POINT('Ctrl Pts',(2.60996342472877,0.636309800095202,3.78147581865173));
#49149=CARTESIAN_POINT('Ctrl Pts',(2.62289827165848,0.794772684000833,3.71977755633891));
#49150=CARTESIAN_POINT('Ctrl Pts',(2.67812342430724,1.06847604194516,3.59952069917244));
#49151=CARTESIAN_POINT('Ctrl Pts',(2.70985831899148,1.18514270861188,3.54065686063037));
#49152=CARTESIAN_POINT('Ctrl Pts',(2.7494231860719,1.30000000000016,3.47498392105788));
#49153=CARTESIAN_POINT('Ctrl Pts',(2.92520978215932,-1.30000000000552,3.58926377761781));
#49154=CARTESIAN_POINT('Ctrl Pts',(2.87137430883562,-1.18514270861552,3.63941583633585));
#49155=CARTESIAN_POINT('Ctrl Pts',(2.82487387978676,-1.06847604194701,3.68357671893372));
#49156=CARTESIAN_POINT('Ctrl Pts',(2.73439400595118,-0.794772684000843,
3.77175637672006));
#49157=CARTESIAN_POINT('Ctrl Pts',(2.6977337833005,-0.636309800095191,3.81588237558861));
#49158=CARTESIAN_POINT('Ctrl Pts',(2.64234943531422,-0.319434907277156,
3.86507084612856));
#49159=CARTESIAN_POINT('Ctrl Pts',(2.62585700317256,-0.158333333333331,
3.87899578028677));
#49160=CARTESIAN_POINT('Ctrl Pts',(2.60883450413301,0.158333333333333,3.86579195045199));
#49161=CARTESIAN_POINT('Ctrl Pts',(2.60954505347175,0.319434907277164,3.83955505545891));
#49162=CARTESIAN_POINT('Ctrl Pts',(2.62772875062843,0.6363098000952,3.7616546613167));
#49163=CARTESIAN_POINT('Ctrl Pts',(2.64349737435505,0.794772684000833,3.70162336321975));
#49164=CARTESIAN_POINT('Ctrl Pts',(2.69697512145966,1.06847604194516,3.58487210094493));
#49165=CARTESIAN_POINT('Ctrl Pts',(2.72704288094852,1.18514270861188,3.52797730830442));
#49166=CARTESIAN_POINT('Ctrl Pts',(2.76402986475048,1.30000000000015,3.46472501840155));
#49167=CARTESIAN_POINT('Ctrl Pts',(2.94195211702088,-1.30000000000551,3.58135635188366));
#49168=CARTESIAN_POINT('Ctrl Pts',(2.89061465528179,-1.18514270861551,3.62917911126257));
#49169=CARTESIAN_POINT('Ctrl Pts',(2.84574056684063,-1.068476041947,3.67144661144475));
#49170=CARTESIAN_POINT('Ctrl Pts',(2.75700413082334,-0.794772684000838,
3.75625923237902));
#49171=CARTESIAN_POINT('Ctrl Pts',(2.71855109018231,-0.636309800095188,
3.79954530516389));
#49172=CARTESIAN_POINT('Ctrl Pts',(2.66175505497251,-0.319434907277155,
3.84729132613465));
#49173=CARTESIAN_POINT('Ctrl Pts',(2.64347546109041,-0.15833333333333,3.86113639964704));
#49174=CARTESIAN_POINT('Ctrl Pts',(2.62607723464659,0.158333333333332,3.84764227098316));
#49175=CARTESIAN_POINT('Ctrl Pts',(2.62816708666822,0.319434907277163,3.82122097164442));
#49176=CARTESIAN_POINT('Ctrl Pts',(2.64706259124335,0.636309800095198,3.74411868020596));
#49177=CARTESIAN_POINT('Ctrl Pts',(2.6641715349787,0.794772684000831,3.68441341960523));
#49178=CARTESIAN_POINT('Ctrl Pts',(2.71563003021196,1.06847604194515,3.57063049673968));
#49179=CARTESIAN_POINT('Ctrl Pts',(2.74404835952103,1.18514270861187,3.51553217123244));
#49180=CARTESIAN_POINT('Ctrl Pts',(2.77861054227786,1.30000000000015,3.45458793145365));
#49181=CARTESIAN_POINT('Ctrl Pts',(2.96275287236147,-1.30000000000551,3.56912187057325));
#49182=CARTESIAN_POINT('Ctrl Pts',(2.9152380089655,-1.18514270861551,3.61419539427489));
#49183=CARTESIAN_POINT('Ctrl Pts',(2.8729820087517,-1.068476041947,3.65428018094039));
#49184=CARTESIAN_POINT('Ctrl Pts',(2.78751122095751,-0.794772684000838,
3.73535907652415));
#49185=CARTESIAN_POINT('Ctrl Pts',(2.74712712559485,-0.636309800095189,
3.7779565913181));
#49186=CARTESIAN_POINT('Ctrl Pts',(2.68921555700873,-0.319434907277157,
3.82446702635131));
#49187=CARTESIAN_POINT('Ctrl Pts',(2.6692019677842,-0.15833333333333,3.83883345347065));
#49188=CARTESIAN_POINT('Ctrl Pts',(2.65111542605734,0.158333333333332,3.82474985461491));
#49189=CARTESIAN_POINT('Ctrl Pts',(2.65381112051842,0.319434907277161,3.79685030737055));
#49190=CARTESIAN_POINT('Ctrl Pts',(2.67331602736107,0.636309800095197,3.72053130998223));
#49191=CARTESIAN_POINT('Ctrl Pts',(2.69291357929012,0.794772684000833,3.66196882305464));
#49192=CARTESIAN_POINT('Ctrl Pts',(2.74171634204975,1.06847604194515,3.55239654305779));
#49193=CARTESIAN_POINT('Ctrl Pts',(2.76785669428666,1.18514270861187,3.49974892305915));
#49194=CARTESIAN_POINT('Ctrl Pts',(2.79901249108243,1.30000000000015,3.44188346301939));
#49195=CARTESIAN_POINT('Ctrl Pts',(2.99103081011791,-1.3000000000055,3.55633083166487));
#49196=CARTESIAN_POINT('Ctrl Pts',(2.94848803293486,-1.1851427086155,3.59827269681306));
#49197=CARTESIAN_POINT('Ctrl Pts',(2.90950880187268,-1.06847604194699,3.63570253211179));
#49198=CARTESIAN_POINT('Ctrl Pts',(2.82769148477546,-0.794772684000828,
3.71174924788332));
#49199=CARTESIAN_POINT('Ctrl Pts',(2.78383232077458,-0.636309800095179,
3.75230485190503));
#49200=CARTESIAN_POINT('Ctrl Pts',(2.72373721633015,-0.31943490727715,3.79643645488893));
#49201=CARTESIAN_POINT('Ctrl Pts',(2.70106719923632,-0.158333333333328,
3.81097609762809));
#49202=CARTESIAN_POINT('Ctrl Pts',(2.68248021019993,0.15833333333333,3.79647629815684));
#49203=CARTESIAN_POINT('Ctrl Pts',(2.68747839337143,0.319434907277157,3.76820790883034));
#49204=CARTESIAN_POINT('Ctrl Pts',(2.70784903438241,0.636309800095187,3.69297067913685));
#49205=CARTESIAN_POINT('Ctrl Pts',(2.72924338216426,0.79477268400082,3.63464523256112));
#49206=CARTESIAN_POINT('Ctrl Pts',(2.77415286444821,1.06847604194513,3.52970451359164));
#49207=CARTESIAN_POINT('Ctrl Pts',(2.7973159748855,1.18514270861185,3.47992887819828));
#49208=CARTESIAN_POINT('Ctrl Pts',(2.82420254493968,1.30000000000012,3.42580255621658));
#49209=CARTESIAN_POINT('Ctrl Pts',(3.02374000248281,-1.30000000000548,3.53970490348622));
#49210=CARTESIAN_POINT('Ctrl Pts',(2.98688227510008,-1.18514270861548,3.57754592275709));
#49211=CARTESIAN_POINT('Ctrl Pts',(2.95194015891161,-1.06847604194698,3.61185076016537));
#49212=CARTESIAN_POINT('Ctrl Pts',(2.87564232544601,-0.79477268400082,3.68293250972372));
#49213=CARTESIAN_POINT('Ctrl Pts',(2.83029179168419,-0.636309800095175,
3.72376888730158));
#49214=CARTESIAN_POINT('Ctrl Pts',(2.76875349594478,-0.31943490727715,3.76615824891994));
#49215=CARTESIAN_POINT('Ctrl Pts',(2.74231322500643,-0.158333333333327,
3.78020127492504));
#49216=CARTESIAN_POINT('Ctrl Pts',(2.72265100687055,0.158333333333329,3.76468932346359));
#49217=CARTESIAN_POINT('Ctrl Pts',(2.7297147732218,0.319434907277155,3.73533386827454));
#49218=CARTESIAN_POINT('Ctrl Pts',(2.7506205684183,0.636309800095184,3.6609413659136));
#49219=CARTESIAN_POINT('Ctrl Pts',(2.77445372491561,0.794772684000816,3.6031922735046));
#49220=CARTESIAN_POINT('Ctrl Pts',(2.81412306654961,1.06847604194513,3.50334462000068));
#49221=CARTESIAN_POINT('Ctrl Pts',(2.83333729156544,1.18514270861185,3.45669992867096));
#49222=CARTESIAN_POINT('Ctrl Pts',(2.8545943534977,1.30000000000012,3.40663089549319));
#49223=CARTESIAN_POINT('Ctrl Pts',(3.05811345181906,-1.30000000000546,3.52497819970161));
#49224=CARTESIAN_POINT('Ctrl Pts',(3.02784713000013,-1.18514270861546,3.55976796518647));
#49225=CARTESIAN_POINT('Ctrl Pts',(2.99739814779495,-1.06847604194695,3.59148490966405));
#49226=CARTESIAN_POINT('Ctrl Pts',(2.92663292557024,-0.7947726840008,3.65765856511712));
#49227=CARTESIAN_POINT('Ctrl Pts',(2.87762423700182,-0.636309800095158,
3.696400314332));
#49228=CARTESIAN_POINT('Ctrl Pts',(2.81437264477428,-0.31943490727714,3.73665586758347));
#49229=CARTESIAN_POINT('Ctrl Pts',(2.7854988204527,-0.158333333333323,3.75149817535916));
#49230=CARTESIAN_POINT('Ctrl Pts',(2.76506258419809,0.158333333333324,3.73523024002701));
#49231=CARTESIAN_POINT('Ctrl Pts',(2.77370832229935,0.319434907277146,3.70430476682064));
#49232=CARTESIAN_POINT('Ctrl Pts',(2.79490878610156,0.636309800095165,3.63053623764237));
#49233=CARTESIAN_POINT('Ctrl Pts',(2.82105731392976,0.794772684000791,3.57332185604792));
#49234=CARTESIAN_POINT('Ctrl Pts',(2.85545611566572,1.0684760419451,3.47850624606086));
#49235=CARTESIAN_POINT('Ctrl Pts',(2.87074934203554,1.18514270861182,3.4349825522203));
#49236=CARTESIAN_POINT('Ctrl Pts',(2.8864458281049,1.30000000000009,3.38897732883797));
#49237=CARTESIAN_POINT('Ctrl Pts',(3.09205625616862,-1.30000000000543,3.50984328348391));
#49238=CARTESIAN_POINT('Ctrl Pts',(3.06800478826141,-1.18514270861544,3.54116922813601));
#49239=CARTESIAN_POINT('Ctrl Pts',(3.04195194514736,-1.06847604194693,3.57018503742081));
#49240=CARTESIAN_POINT('Ctrl Pts',(2.97714108859957,-0.794772684000788,
3.63188048662145));
#49241=CARTESIAN_POINT('Ctrl Pts',(2.92620087283072,-0.636309800095147,
3.67036357934875));
#49242=CARTESIAN_POINT('Ctrl Pts',(2.86161204481792,-0.319434907277135,
3.70886469308564));
#49243=CARTESIAN_POINT('Ctrl Pts',(2.82907770173351,-0.15833333333332,3.72319103898903));
#49244=CARTESIAN_POINT('Ctrl Pts',(2.80811545785615,0.158333333333322,3.7063924783893));
#49245=CARTESIAN_POINT('Ctrl Pts',(2.81978347874688,0.31943490727714,3.67537519627519));
#49246=CARTESIAN_POINT('Ctrl Pts',(2.84147833975011,0.636309800095155,3.60243740100193));
#49247=CARTESIAN_POINT('Ctrl Pts',(2.86909110561065,0.794772684000779,3.54488893058255));
#49248=CARTESIAN_POINT('Ctrl Pts',(2.89748472667741,1.06847604194508,3.45437721046725));
#49249=CARTESIAN_POINT('Ctrl Pts',(2.90852267843929,1.1851427086118,3.41364721031541));
#49250=CARTESIAN_POINT('Ctrl Pts',(2.9183080354906,1.30000000000007,3.37136637985989));
#49251=CARTESIAN_POINT('Ctrl Pts',(3.11687629317787,-1.30000000000541,3.50004924215962));
#49252=CARTESIAN_POINT('Ctrl Pts',(3.09754542267603,-1.18514270861542,3.52930518627741));
#49253=CARTESIAN_POINT('Ctrl Pts',(3.0747546067079,-1.06847604194692,3.55658817309006));
#49254=CARTESIAN_POINT('Ctrl Pts',(3.01411009634812,-0.794772684000775,
3.61505940450598));
#49255=CARTESIAN_POINT('Ctrl Pts',(2.96079261695772,-0.636309800095137,
3.65220373194291));
#49256=CARTESIAN_POINT('Ctrl Pts',(2.89540151624588,-0.319434907277129,
3.68956165600955));
#49257=CARTESIAN_POINT('Ctrl Pts',(2.86150434657455,-0.158333333333317,
3.7048038980158));
#49258=CARTESIAN_POINT('Ctrl Pts',(2.84019968751387,0.158333333333319,3.68765515484666));
#49259=CARTESIAN_POINT('Ctrl Pts',(2.85289391107185,0.319434907277135,3.6554224140808));
#49260=CARTESIAN_POINT('Ctrl Pts',(2.87468177331336,0.636309800095144,3.58281140246088));
#49261=CARTESIAN_POINT('Ctrl Pts',(2.90400762976015,0.794772684000765,3.52574151485857));
#49262=CARTESIAN_POINT('Ctrl Pts',(2.92809977392654,1.06847604194507,3.43821719621443));
#49263=CARTESIAN_POINT('Ctrl Pts',(2.9359865228172,1.18514270861178,3.39931308160935));
#49264=CARTESIAN_POINT('Ctrl Pts',(2.94133142409081,1.30000000000005,3.35939088684461));
#49265=CARTESIAN_POINT('Ctrl Pts',(3.13158353443155,-1.30000000000541,3.49443635111853));
#49266=CARTESIAN_POINT('Ctrl Pts',(3.11498108231661,-1.18514270861541,3.52243016001803));
#49267=CARTESIAN_POINT('Ctrl Pts',(3.09414544753145,-1.06847604194691,3.54873997504398));
#49268=CARTESIAN_POINT('Ctrl Pts',(3.03623146421028,-0.794772684000773,
3.60563054828418));
#49269=CARTESIAN_POINT('Ctrl Pts',(2.98236769368786,-0.636309800095134,
3.64292466044221));
#49270=CARTESIAN_POINT('Ctrl Pts',(2.91631142052615,-0.319434907277128,
3.67938965362454));
#49271=CARTESIAN_POINT('Ctrl Pts',(2.88044270014575,-0.158333333333317,
3.69387287687065));
#49272=CARTESIAN_POINT('Ctrl Pts',(2.85865085934877,0.158333333333318,3.67618650762719));
#49273=CARTESIAN_POINT('Ctrl Pts',(2.87260183512496,0.319434907277134,3.64393871473653));
#49274=CARTESIAN_POINT('Ctrl Pts',(2.89452615463776,0.636309800095142,3.57160714945251));
#49275=CARTESIAN_POINT('Ctrl Pts',(2.92450780919669,0.794772684000762,3.51445504771415));
#49276=CARTESIAN_POINT('Ctrl Pts',(2.94602178220094,1.06847604194506,3.42863571906366));
#49277=CARTESIAN_POINT('Ctrl Pts',(2.95208385538883,1.18514270861177,3.39083350140881));
#49278=CARTESIAN_POINT('Ctrl Pts',(2.95489540002235,1.30000000000004,3.35237707355236));
#49279=CARTESIAN_POINT('Ctrl Pts',(3.13747310944787,-1.30000000000541,3.49219508269092));
#49280=CARTESIAN_POINT('Ctrl Pts',(3.12186406304511,-1.18514270861541,3.51956831209898));
#49281=CARTESIAN_POINT('Ctrl Pts',(3.10174684277267,-1.06847604194691,3.54541437692169));
#49282=CARTESIAN_POINT('Ctrl Pts',(3.04485725601163,-0.794772684000771,
3.60159590144885));
#49283=CARTESIAN_POINT('Ctrl Pts',(2.99082346793244,-0.636309800095134,
3.6390167161116));
#49284=CARTESIAN_POINT('Ctrl Pts',(2.9246017824391,-0.319434907277128,3.67523948609918));
#49285=CARTESIAN_POINT('Ctrl Pts',(2.88807824804091,-0.158333333333317,
3.68956399077605));
#49286=CARTESIAN_POINT('Ctrl Pts',(2.86619353667346,0.158333333333318,3.67177298542));
#49287=CARTESIAN_POINT('Ctrl Pts',(2.880683819517,0.319434907277135,3.63955575270664));
#49288=CARTESIAN_POINT('Ctrl Pts',(2.9026304893724,0.636309800095142,3.5673011875794));
#49289=CARTESIAN_POINT('Ctrl Pts',(2.93271554483,0.794772684000762,3.50994922438559));
#49290=CARTESIAN_POINT('Ctrl Pts',(2.95319450356583,1.06847604194506,3.42480511734035));
#49291=CARTESIAN_POINT('Ctrl Pts',(2.95855830491183,1.18514270861177,3.38747509513212));
#49292=CARTESIAN_POINT('Ctrl Pts',(2.9604213251873,1.30000000000004,3.34967077975544));
#49293=CARTESIAN_POINT('Ctrl Pts',(3.14724612156393,-1.3000000000054,3.48766330278961));
#49294=CARTESIAN_POINT('Ctrl Pts',(3.13348128227247,-1.18514270861541,3.5140676492899));
#49295=CARTESIAN_POINT('Ctrl Pts',(3.11468903259007,-1.06847604194691,3.53917782727463));
#49296=CARTESIAN_POINT('Ctrl Pts',(3.05966085271442,-0.794772684000766,
3.59419757352424));
#49297=CARTESIAN_POINT('Ctrl Pts',(3.00509682848601,-0.63630980009513,3.63158621209596));
#49298=CARTESIAN_POINT('Ctrl Pts',(2.93881145735945,-0.319434907277126,
3.66764063632057));
#49299=CARTESIAN_POINT('Ctrl Pts',(2.90163688889582,-0.158333333333316,
3.68223796966319));
#49300=CARTESIAN_POINT('Ctrl Pts',(2.87983121837161,0.158333333333317,3.66453734208435));
#49301=CARTESIAN_POINT('Ctrl Pts',(2.89521422951983,0.319434907277132,3.63232151937108));
#49302=CARTESIAN_POINT('Ctrl Pts',(2.9170542722588,0.636309800095138,3.56004488163989));
#49303=CARTESIAN_POINT('Ctrl Pts',(2.94702340432198,0.794772684000757,3.50201390974382));
#49304=CARTESIAN_POINT('Ctrl Pts',(2.96554943465532,1.06847604194505,3.41789800082923));
#49305=CARTESIAN_POINT('Ctrl Pts',(2.96967079764774,1.18514270861176,3.38137354255371));
#49306=CARTESIAN_POINT('Ctrl Pts',(2.96989429155835,1.30000000000003,3.34473528617021));
#49307=CARTESIAN_POINT('Ctrl Pts',(3.16813308791021,-1.3000000000054,3.4801976087041));
#49308=CARTESIAN_POINT('Ctrl Pts',(3.15861104087973,-1.1851427086154,3.50535118787714));
#49309=CARTESIAN_POINT('Ctrl Pts',(3.14277726544515,-1.0684760419469,3.52937024792866));
#49310=CARTESIAN_POINT('Ctrl Pts',(3.09161672138539,-0.794772684000766,
3.58223811551322));
#49311=CARTESIAN_POINT('Ctrl Pts',(3.03534693789403,-0.636309800095129,
3.6187218270644));
#49312=CARTESIAN_POINT('Ctrl Pts',(2.96803742254168,-0.319434907277126,
3.65337423047707));
#49313=CARTESIAN_POINT('Ctrl Pts',(2.92883858231923,-0.158333333333316,
3.66769464217141));
#49314=CARTESIAN_POINT('Ctrl Pts',(2.90622356807653,0.158333333333318,3.64909280244314));
#49315=CARTESIAN_POINT('Ctrl Pts',(2.92239523057836,0.319434907277134,3.61581692172046));
#49316=CARTESIAN_POINT('Ctrl Pts',(2.94447913758118,0.636309800095139,3.54399422758025));
#49317=CARTESIAN_POINT('Ctrl Pts',(2.97650667690471,0.794772684000756,3.48708945195852));
#49318=CARTESIAN_POINT('Ctrl Pts',(2.9915670013947,1.06847604194505,3.40551175333258));
#49319=CARTESIAN_POINT('Ctrl Pts',(2.99300105055347,1.18514270861176,3.37038148369381));
#49320=CARTESIAN_POINT('Ctrl Pts',(2.98935009243932,1.30000000000003,3.3354329073998));
#49321=CARTESIAN_POINT('Ctrl Pts',(3.19179194785933,-1.30000000000532,3.47145281285552));
#49322=CARTESIAN_POINT('Ctrl Pts',(3.18689867313708,-1.18514270861533,3.49493494775585));
#49323=CARTESIAN_POINT('Ctrl Pts',(3.17431550602839,-1.06847604194684,3.51756498343844));
#49324=CARTESIAN_POINT('Ctrl Pts',(3.12748068298343,-0.794772684000715,
3.56787637333307));
#49325=CARTESIAN_POINT('Ctrl Pts',(3.06924355582359,-0.636309800095087,
3.60331146965924));
#49326=CARTESIAN_POINT('Ctrl Pts',(3.00149505536153,-0.319434907277103,
3.63718459141884));
#49327=CARTESIAN_POINT('Ctrl Pts',(2.96098140760044,-0.158333333333305,
3.6523108758059));
#49328=CARTESIAN_POINT('Ctrl Pts',(2.93839872540465,0.158333333333307,3.63373857487706));
#49329=CARTESIAN_POINT('Ctrl Pts',(2.95623380536833,0.319434907277111,3.60007094708565));
#49330=CARTESIAN_POINT('Ctrl Pts',(2.97817832027118,0.636309800095095,3.52830432733564));
#49331=CARTESIAN_POINT('Ctrl Pts',(3.01075035598527,0.794772684000702,3.47071903367215));
#49332=CARTESIAN_POINT('Ctrl Pts',(3.02115660837694,1.06847604194498,3.39126100268221));
#49333=CARTESIAN_POINT('Ctrl Pts',(3.01945905835154,1.18514270861168,3.3576417212101));
#49334=CARTESIAN_POINT('Ctrl Pts',(3.01155947723004,1.29999999999994,3.32479759567122));
#49335=CARTESIAN_POINT('Ctrl Pts',(3.21522080882871,-1.30000000000528,3.46246711081863));
#49336=CARTESIAN_POINT('Ctrl Pts',(3.21478036472508,-1.1851427086153,3.48407010925375));
#49337=CARTESIAN_POINT('Ctrl Pts',(3.2054431767628,-1.06847604194681,3.50530808615156));
#49338=CARTESIAN_POINT('Ctrl Pts',(3.16331914657126,-0.794772684000694,
3.55352878865432));
#49339=CARTESIAN_POINT('Ctrl Pts',(3.10445481574066,-0.636309800095072,
3.58951896614683));
#49340=CARTESIAN_POINT('Ctrl Pts',(3.03622583171377,-0.319434907277096,
3.62257076628785));
#49341=CARTESIAN_POINT('Ctrl Pts',(2.99327478607966,-0.158333333333301,
3.63715677864556));
#49342=CARTESIAN_POINT('Ctrl Pts',(2.96991053877903,0.158333333333303,3.61766975016863));
#49343=CARTESIAN_POINT('Ctrl Pts',(2.98892675674291,0.319434907277103,3.58309285692305));
#49344=CARTESIAN_POINT('Ctrl Pts',(3.01072668242984,0.63630980009508,3.51137369396961));
#49345=CARTESIAN_POINT('Ctrl Pts',(3.04460510772446,0.794772684000685,3.45395272792116));
#49346=CARTESIAN_POINT('Ctrl Pts',(3.05068074461062,1.06847604194496,3.3769694383871));
#49347=CARTESIAN_POINT('Ctrl Pts',(3.04591541965882,1.18514270861165,3.34492984949011));
#49348=CARTESIAN_POINT('Ctrl Pts',(3.03375485167175,1.29999999999991,3.31417388522341));
#49349=CARTESIAN_POINT('Ctrl Pts',(3.23043539172048,-1.30000000000525,3.45755404152851));
#49350=CARTESIAN_POINT('Ctrl Pts',(3.2329405320919,-1.18514270861527,3.47820324486245));
#49351=CARTESIAN_POINT('Ctrl Pts',(3.22568713974405,-1.06847604194679,3.4986527219145));
#49352=CARTESIAN_POINT('Ctrl Pts',(3.18638618961544,-0.794772684000677,
3.54543369714194));
#49353=CARTESIAN_POINT('Ctrl Pts',(3.12652860387767,-0.636309800095058,
3.58102011372498));
#49354=CARTESIAN_POINT('Ctrl Pts',(3.05782286067161,-0.319434907277089,
3.6133293068439));
#49355=CARTESIAN_POINT('Ctrl Pts',(3.01347626991863,-0.158333333333298,
3.62773044976816));
#49356=CARTESIAN_POINT('Ctrl Pts',(2.98993339731732,0.158333333333299,3.60801834881184));
#49357=CARTESIAN_POINT('Ctrl Pts',(3.01013999760652,0.319434907277096,3.57338353464544));
#49358=CARTESIAN_POINT('Ctrl Pts',(3.03210689055872,0.636309800095065,3.50198461231473));
#49359=CARTESIAN_POINT('Ctrl Pts',(3.06682651501897,0.794772684000667,3.44469950089005));
#49360=CARTESIAN_POINT('Ctrl Pts',(3.06994197699543,1.06847604194493,3.3689708590629));
#49361=CARTESIAN_POINT('Ctrl Pts',(3.06306346665119,1.18514270861163,3.33769266444407));
#49362=CARTESIAN_POINT('Ctrl Pts',(3.04795787791233,1.29999999999988,3.30791639823066));
#49363=CARTESIAN_POINT('Ctrl Pts',(3.24236037790981,-1.30000000000524,3.45333727526057));
#49364=CARTESIAN_POINT('Ctrl Pts',(3.24716949580118,-1.18514270861526,3.47315376125293));
#49365=CARTESIAN_POINT('Ctrl Pts',(3.24157375609316,-1.06847604194678,3.49295791273523));
#49366=CARTESIAN_POINT('Ctrl Pts',(3.20460917540481,-0.79477268400067,3.53868096928009));
#49367=CARTESIAN_POINT('Ctrl Pts',(3.14425046756847,-0.636309800095053,
3.574312076442));
#49368=CARTESIAN_POINT('Ctrl Pts',(3.0751964674596,-0.319434907277087,3.60607199428668));
#49369=CARTESIAN_POINT('Ctrl Pts',(3.02951884639692,-0.158333333333296,
3.62006145448726));
#49370=CARTESIAN_POINT('Ctrl Pts',(3.00576205606805,0.158333333333298,3.60008675760718));
#49371=CARTESIAN_POINT('Ctrl Pts',(3.02695727830684,0.319434907277093,3.56545728113027));
#49372=CARTESIAN_POINT('Ctrl Pts',(3.04909841932032,0.63630980009506,3.49436555167233));
#49373=CARTESIAN_POINT('Ctrl Pts',(3.08455863757736,0.794772684000662,3.43726743726676));
#49374=CARTESIAN_POINT('Ctrl Pts',(3.08533390700979,1.06847604194492,3.36257119443522));
#49375=CARTESIAN_POINT('Ctrl Pts',(3.07676594735122,1.18514270861162,3.33190059891139));
#49376=CARTESIAN_POINT('Ctrl Pts',(3.05929444262332,1.29999999999987,3.30289264361694));
#49377=CARTESIAN_POINT('Ctrl Pts',(3.25151506053727,-1.30000000000523,3.45044442082133));
#49378=CARTESIAN_POINT('Ctrl Pts',(3.25818052889986,-1.18514270861526,3.46980749709816));
#49379=CARTESIAN_POINT('Ctrl Pts',(3.25388329241467,-1.06847604194677,3.48920286726995));
#49380=CARTESIAN_POINT('Ctrl Pts',(3.21862977519508,-0.794772684000666,
3.53408465775458));
#49381=CARTESIAN_POINT('Ctrl Pts',(3.15747235989514,-0.63630980009505,3.56920933418693));
#49382=CARTESIAN_POINT('Ctrl Pts',(3.08815646817621,-0.319434907277086,
3.60054108442575));
#49383=CARTESIAN_POINT('Ctrl Pts',(3.04189754295722,-0.158333333333296,
3.61472107209399));
#49384=CARTESIAN_POINT('Ctrl Pts',(3.01797372470983,0.158333333333297,3.5945431182307));
#49385=CARTESIAN_POINT('Ctrl Pts',(3.03961372085166,0.319434907277091,3.55956805127921));
#49386=CARTESIAN_POINT('Ctrl Pts',(3.06161440808337,0.636309800095057,3.48839230192767));
#49387=CARTESIAN_POINT('Ctrl Pts',(3.09736224761959,0.794772684000659,3.43113070515455));
#49388=CARTESIAN_POINT('Ctrl Pts',(3.09643186938066,1.06847604194492,3.35726335515356));
#49389=CARTESIAN_POINT('Ctrl Pts',(3.08670795795583,1.18514270861161,3.32717417292955));
#49390=CARTESIAN_POINT('Ctrl Pts',(3.06766286137189,1.29999999999986,3.29897024724187));
#49391=CARTESIAN_POINT('Ctrl Pts',(3.25839374116323,-1.30000000000522,3.44829774143665));
#49392=CARTESIAN_POINT('Ctrl Pts',(3.26650238174667,-1.18514270861524,3.4673851188094));
#49393=CARTESIAN_POINT('Ctrl Pts',(3.26321007457816,-1.06847604194676,3.48651319165782));
#49394=CARTESIAN_POINT('Ctrl Pts',(3.22926571633663,-0.794772684000659,
3.53079688118505));
#49395=CARTESIAN_POINT('Ctrl Pts',(3.16743555483022,-0.636309800095044,
3.56545105153254));
#49396=CARTESIAN_POINT('Ctrl Pts',(3.09792478855041,-0.319434907277083,
3.59645939042958));
#49397=CARTESIAN_POINT('Ctrl Pts',(3.05127922196103,-0.158333333333294,
3.61083604519458));
#49398=CARTESIAN_POINT('Ctrl Pts',(3.02724725143658,0.158333333333296,3.59052331406926));
#49399=CARTESIAN_POINT('Ctrl Pts',(3.04921905371466,0.319434907277089,3.55528782026933));
#49400=CARTESIAN_POINT('Ctrl Pts',(3.07108571412861,0.636309800095052,3.48401629312595));
#49401=CARTESIAN_POINT('Ctrl Pts',(3.10699976074015,0.794772684000652,3.42657662119549));
#49402=CARTESIAN_POINT('Ctrl Pts',(3.10475968117388,1.06847604194491,3.35329452560483));
#49403=CARTESIAN_POINT('Ctrl Pts',(3.09416135764752,1.1851427086116,3.32363162846848));
#49404=CARTESIAN_POINT('Ctrl Pts',(3.07393435803593,1.29999999999985,3.29602693800773));
#49405=CARTESIAN_POINT('Ctrl Pts',(3.2629351555692,-1.30000000000522,3.44681055730694));
#49406=CARTESIAN_POINT('Ctrl Pts',(3.27195063283112,-1.18514270861524,3.46564439602566));
#49407=CARTESIAN_POINT('Ctrl Pts',(3.26930490564037,-1.06847604194676,3.48456486026918));
#49408=CARTESIAN_POINT('Ctrl Pts',(3.23625303145248,-0.794772684000657,
3.52847503998891));
#49409=CARTESIAN_POINT('Ctrl Pts',(3.17415149607227,-0.636309800095043,
3.56303901281693));
#49410=CARTESIAN_POINT('Ctrl Pts',(3.10452955844486,-0.319434907277082,
3.59385694153619));
#49411=CARTESIAN_POINT('Ctrl Pts',(3.05748804064638,-0.158333333333294,
3.60819414683819));
#49412=CARTESIAN_POINT('Ctrl Pts',(3.03338240007983,0.158333333333296,3.58778759734221));
#49413=CARTESIAN_POINT('Ctrl Pts',(3.05566128091489,0.319434907277088,3.5524820616037));
#49414=CARTESIAN_POINT('Ctrl Pts',(3.07752001872709,0.636309800095051,3.48124176820776));
#49415=CARTESIAN_POINT('Ctrl Pts',(3.11364277148084,0.79477268400065,3.42379492402245));
#49416=CARTESIAN_POINT('Ctrl Pts',(3.11049337442213,1.06847604194491,3.35086141207141));
#49417=CARTESIAN_POINT('Ctrl Pts',(3.09926141795675,1.1851427086116,3.32142448566816));
#49418=CARTESIAN_POINT('Ctrl Pts',(3.07816076231604,1.29999999999985,3.2941208477323));
#49419=CARTESIAN_POINT('Ctrl Pts',(3.2651977655983,-1.30000000000522,3.4460570044894));
#49420=CARTESIAN_POINT('Ctrl Pts',(3.27465921485341,-1.18514270861524,3.46475464341014));
#49421=CARTESIAN_POINT('Ctrl Pts',(3.27233393696745,-1.06847604194676,3.48356770879022));
#49422=CARTESIAN_POINT('Ctrl Pts',(3.2397323822584,-0.794772684000657,3.52729631157071));
#49423=CARTESIAN_POINT('Ctrl Pts',(3.17752178562626,-0.636309800095043,
3.56184883363791));
#49424=CARTESIAN_POINT('Ctrl Pts',(3.1078476368185,-0.319434907277082,3.5925760349404));
#49425=CARTESIAN_POINT('Ctrl Pts',(3.06058772743218,-0.158333333333294,
3.60686829725747));
#49426=CARTESIAN_POINT('Ctrl Pts',(3.03644527364713,0.158333333333296,3.58641449742714));
#49427=CARTESIAN_POINT('Ctrl Pts',(3.05889036651009,0.319434907277088,3.5510891556183));
#49428=CARTESIAN_POINT('Ctrl Pts',(3.08075762975828,0.63630980009505,3.47987898774469));
#49429=CARTESIAN_POINT('Ctrl Pts',(3.11700012148815,0.794772684000649,3.42244613527154));
#49430=CARTESIAN_POINT('Ctrl Pts',(3.11339055039977,1.06847604194491,3.34968045295409));
#49431=CARTESIAN_POINT('Ctrl Pts',(3.10183395340449,1.1851427086116,3.32034744392509));
#49432=CARTESIAN_POINT('Ctrl Pts',(3.08028320899029,1.29999999999985,3.29317899350803));
#49433=CARTESIAN_POINT('Ctrl Pts',(3.2670773572165,-1.30000000000522,3.4454216913974));
#49434=CARTESIAN_POINT('Ctrl Pts',(3.27690346099998,-1.18514270861524,3.46399707135251));
#49435=CARTESIAN_POINT('Ctrl Pts',(3.27484235905761,-1.06847604194676,3.48271706772866));
#49436=CARTESIAN_POINT('Ctrl Pts',(3.24261897799492,-0.794772684000656,
3.52629809714264));
#49437=CARTESIAN_POINT('Ctrl Pts',(3.18034046996167,-0.636309800095042,
3.56086999118983));
#49438=CARTESIAN_POINT('Ctrl Pts',(3.11062587849898,-0.319434907277082,
3.59152561799046));
#49439=CARTESIAN_POINT('Ctrl Pts',(3.06316711554304,-0.158333333333294,
3.60575962620988));
#49440=CARTESIAN_POINT('Ctrl Pts',(3.03899373624695,0.158333333333295,3.58526587749418));
#49441=CARTESIAN_POINT('Ctrl Pts',(3.06158720505367,0.319434907277087,3.54993590984734));
#49442=CARTESIAN_POINT('Ctrl Pts',(3.08347174416763,0.63630980009505,3.47876265237086));
#49443=CARTESIAN_POINT('Ctrl Pts',(3.11982701814721,0.794772684000649,3.42135628234749));
#49444=CARTESIAN_POINT('Ctrl Pts',(3.11582977098446,1.06847604194491,3.34872551469281));
#49445=CARTESIAN_POINT('Ctrl Pts',(3.10399636889382,1.1851427086116,3.31947182962008));
#49446=CARTESIAN_POINT('Ctrl Pts',(3.08205982489668,1.29999999999985,3.29240362755716));
#49447=CARTESIAN_POINT('Ctrl Pts',(3.26839113242907,-1.30000000000522,3.4449746547755));
#49448=CARTESIAN_POINT('Ctrl Pts',(3.27847045351117,-1.18514270861524,3.46346192886595));
#49449=CARTESIAN_POINT('Ctrl Pts',(3.27659354100122,-1.06847604194676,3.48211588468545));
#49450=CARTESIAN_POINT('Ctrl Pts',(3.24463620619448,-0.794772684000656,
3.52559532247786));
#49451=CARTESIAN_POINT('Ctrl Pts',(3.18231740566533,-0.636309800095042,
3.56018988379013));
#49452=CARTESIAN_POINT('Ctrl Pts',(3.11257644655851,-0.319434907277082,
3.59079784181469));
#49453=CARTESIAN_POINT('Ctrl Pts',(3.06497484078213,-0.158333333333294,
3.60498650919207));
#49454=CARTESIAN_POINT('Ctrl Pts',(3.04077972177938,0.158333333333295,3.58446456585854));
#49455=CARTESIAN_POINT('Ctrl Pts',(3.06347824714969,0.319434907277088,3.54913277272834));
#49456=CARTESIAN_POINT('Ctrl Pts',(3.0853775573579,0.63630980009505,3.47798839762382));
#49457=CARTESIAN_POINT('Ctrl Pts',(3.12181659359161,0.794772684000649,3.42060613391417));
#49458=CARTESIAN_POINT('Ctrl Pts',(3.11754710088519,1.06847604194491,3.34806866304846));
#49459=CARTESIAN_POINT('Ctrl Pts',(3.10551816588902,1.1851427086116,3.31886837560809));
#49460=CARTESIAN_POINT('Ctrl Pts',(3.083308401089,1.29999999999985,3.29186658408691));
#49461=CARTESIAN_POINT('Ctrl Pts',(3.26914141517851,-1.30000000000522,3.44471866630091));
#49462=CARTESIAN_POINT('Ctrl Pts',(3.27936503375922,-1.18514270861524,3.46315510004237));
#49463=CARTESIAN_POINT('Ctrl Pts',(3.27759322408484,-1.06847604194676,3.48177113502083));
#49464=CARTESIAN_POINT('Ctrl Pts',(3.24578815034159,-0.794772684000656,
3.52519281473233));
#49465=CARTESIAN_POINT('Ctrl Pts',(3.18344794709283,-0.636309800095042,
3.55980233955652));
#49466=CARTESIAN_POINT('Ctrl Pts',(3.11369178556253,-0.319434907277082,
3.59038290776075));
#49467=CARTESIAN_POINT('Ctrl Pts',(3.06600657894605,-0.158333333333294,
3.60454325978532));
#49468=CARTESIAN_POINT('Ctrl Pts',(3.04179920469789,0.158333333333295,3.58400538652966));
#49469=CARTESIAN_POINT('Ctrl Pts',(3.0645596308527,0.319434907277087,3.54867479637399));
#49470=CARTESIAN_POINT('Ctrl Pts',(3.08646841883026,0.636309800095049,3.47754814084337));
#49471=CARTESIAN_POINT('Ctrl Pts',(3.12295571757344,0.794772684000649,3.42018005651234));
#49472=CARTESIAN_POINT('Ctrl Pts',(3.1185300450144,1.06847604194491,3.34769519918457));
#49473=CARTESIAN_POINT('Ctrl Pts',(3.10638879801904,1.1851427086116,3.3185247695525));
#49474=CARTESIAN_POINT('Ctrl Pts',(3.08402201369178,1.29999999999985,3.29155991919689));
#49475=CARTESIAN_POINT('Ctrl Pts',(3.2815192757435,-1.30000000000524,3.44049349245556));
#49476=CARTESIAN_POINT('Ctrl Pts',(3.29411750209666,-1.18514270861526,3.45808378517407));
#49477=CARTESIAN_POINT('Ctrl Pts',(3.29407811160572,-1.06847604194678,3.47607236336675));
#49478=CARTESIAN_POINT('Ctrl Pts',(3.26479168863541,-0.794772684000672,
3.51854969671626));
#49479=CARTESIAN_POINT('Ctrl Pts',(3.20211463122718,-0.636309800095055,
3.55342708072927));
#49480=CARTESIAN_POINT('Ctrl Pts',(3.13213552189026,-0.319434907277088,
3.58358960599319));
#49481=CARTESIAN_POINT('Ctrl Pts',(3.08310955670434,-0.158333333333297,
3.59732839724589));
#49482=CARTESIAN_POINT('Ctrl Pts',(3.05869326203224,0.158333333333299,3.57651899659488));
#49483=CARTESIAN_POINT('Ctrl Pts',(3.08241532664736,0.319434907277094,3.54113626936939));
#49484=CARTESIAN_POINT('Ctrl Pts',(3.10446819107465,0.636309800095062,3.47028638166786));
#49485=CARTESIAN_POINT('Ctrl Pts',(3.14178581750134,0.794772684000664,3.4131936241766));
#49486=CARTESIAN_POINT('Ctrl Pts',(3.13479782110837,1.06847604194493,3.34159159469494));
#49487=CARTESIAN_POINT('Ctrl Pts',(3.12080760531913,1.18514270861162,3.31291693254506));
#49488=CARTESIAN_POINT('Ctrl Pts',(3.09585201844837,1.29999999999987,3.28656147369124));
#49489=CARTESIAN_POINT('Ctrl Pts',(3.30633337300009,-1.30000000000539,3.43306487095043));
#49490=CARTESIAN_POINT('Ctrl Pts',(3.32406547015772,-1.1851427086154,3.44965584374711));
#49491=CARTESIAN_POINT('Ctrl Pts',(3.32765731547434,-1.0684760419469,3.46674748844742));
#49492=CARTESIAN_POINT('Ctrl Pts',(3.30328838620176,-0.794772684000765,
3.50738925913304));
#49493=CARTESIAN_POINT('Ctrl Pts',(3.23879682294951,-0.636309800095127,
3.54130171876271));
#49494=CARTESIAN_POINT('Ctrl Pts',(3.16813786468817,-0.319434907277124,
3.57030559004538));
#49495=CARTESIAN_POINT('Ctrl Pts',(3.11710951207744,-0.158333333333315,
3.58395650927749));
#49496=CARTESIAN_POINT('Ctrl Pts',(3.09226299934626,0.158333333333317,3.56258450769254));
#49497=CARTESIAN_POINT('Ctrl Pts',(3.11774095891631,0.319434907277132,3.52696166627474));
#49498=CARTESIAN_POINT('Ctrl Pts',(3.13922311326188,0.636309800095137,3.45564656166672));
#49499=CARTESIAN_POINT('Ctrl Pts',(3.17628812002097,0.794772684000752,3.3969085309373));
#49500=CARTESIAN_POINT('Ctrl Pts',(3.16473749775489,1.06847604194505,3.32749488900432));
#49501=CARTESIAN_POINT('Ctrl Pts',(3.14787282716488,1.18514270861176,3.3006149624431));
#49502=CARTESIAN_POINT('Ctrl Pts',(3.1191433223711,1.30000000000003,3.27690170288451));
#49503=CARTESIAN_POINT('Ctrl Pts',(3.33062939107151,-1.30000000000554,3.42534919669555));
#49504=CARTESIAN_POINT('Ctrl Pts',(3.35332856352848,-1.18514270861553,3.44081299553099));
#49505=CARTESIAN_POINT('Ctrl Pts',(3.36047748554674,-1.06847604194702,3.45697322363563));
#49506=CARTESIAN_POINT('Ctrl Pts',(3.34106873621573,-0.794772684000851,
3.49591547433162));
#49507=CARTESIAN_POINT('Ctrl Pts',(3.27513477130193,-0.636309800095197,
3.52930916811412));
#49508=CARTESIAN_POINT('Ctrl Pts',(3.20409726056275,-0.319434907277159,
3.55752565372287));
#49509=CARTESIAN_POINT('Ctrl Pts',(3.15126301207831,-0.158333333333332,
3.57130224199688));
#49510=CARTESIAN_POINT('Ctrl Pts',(3.12601838770936,0.158333333333334,3.54939933546828));
#49511=CARTESIAN_POINT('Ctrl Pts',(3.15259691103518,0.319434907277167,3.51276440601536));
#49512=CARTESIAN_POINT('Ctrl Pts',(3.17427247911497,0.636309800095206,3.44187942845857));
#49513=CARTESIAN_POINT('Ctrl Pts',(3.2137035449833,0.79477268400084,3.38458268055424));
#49514=CARTESIAN_POINT('Ctrl Pts',(3.19697910110487,1.06847604194517,3.31662261217747));
#49515=CARTESIAN_POINT('Ctrl Pts',(3.17625676661729,1.18514270861189,3.2903696517621));
#49516=CARTESIAN_POINT('Ctrl Pts',(3.14205148969539,1.30000000000017,3.26728112636297));
#49517=CARTESIAN_POINT('Ctrl Pts',(3.34312043552546,-1.30000000000554,3.42192826582793));
#49518=CARTESIAN_POINT('Ctrl Pts',(3.36817625250915,-1.18514270861553,3.43668158762693));
#49519=CARTESIAN_POINT('Ctrl Pts',(3.37703616937261,-1.06847604194702,3.45230111691552));
#49520=CARTESIAN_POINT('Ctrl Pts',(3.36008858049118,-0.794772684000851,
3.49038646683314));
#49521=CARTESIAN_POINT('Ctrl Pts',(3.29374448453208,-0.636309800095197,
3.523919285052));
#49522=CARTESIAN_POINT('Ctrl Pts',(3.22246485929501,-0.319434907277159,
3.55167070473743));
#49523=CARTESIAN_POINT('Ctrl Pts',(3.16838675811195,-0.158333333333332,
3.56506164372659));
#49524=CARTESIAN_POINT('Ctrl Pts',(3.14286241424647,0.158333333333334,3.5427812026076));
#49525=CARTESIAN_POINT('Ctrl Pts',(3.17031238807969,0.319434907277167,3.50603727501036));
#49526=CARTESIAN_POINT('Ctrl Pts',(3.19184909015917,0.636309800095206,3.43508690301979));
#49527=CARTESIAN_POINT('Ctrl Pts',(3.23156943363573,0.79477268400084,3.3774589430542));
#49528=CARTESIAN_POINT('Ctrl Pts',(3.21244012754109,1.06847604194517,3.31040827863485));
#49529=CARTESIAN_POINT('Ctrl Pts',(3.19010469464422,1.18514270861189,3.28482004316132));
#49530=CARTESIAN_POINT('Ctrl Pts',(3.15371419664818,1.30000000000017,3.26266732036942));
#49531=CARTESIAN_POINT('',(3.07985616677633,1.2,3.32482439211205));
#49532=CARTESIAN_POINT('Ctrl Pts',(3.07985616677633,1.2,3.32482439211205));
#49533=CARTESIAN_POINT('Ctrl Pts',(3.05014647401839,1.22374741355226,3.33154618210707));
#49534=CARTESIAN_POINT('Ctrl Pts',(3.02045877557164,1.24661638075374,3.3373574996142));
#49535=CARTESIAN_POINT('Ctrl Pts',(3.00582299008617,1.2582899439244,3.34073830904269));
#49536=CARTESIAN_POINT('Ctrl Pts',(2.99588832002411,1.26618999194865,3.34301915383334));
#49537=CARTESIAN_POINT('Ctrl Pts',(2.97463599570754,1.28302939977084,3.34785885555862));
#49538=CARTESIAN_POINT('Ctrl Pts',(2.96409046681166,1.29150679485646,3.35043257954748));
#49539=CARTESIAN_POINT('Ctrl Pts',(2.95357407118872,1.30000000000004,3.3530661292399));
#49540=CARTESIAN_POINT('',(3.20083482135393,0.653834841418549,3.42413500689526));
#49541=CARTESIAN_POINT('Ctrl Pts',(3.20083482136852,0.653834841417875,3.42413500687395));
#49542=CARTESIAN_POINT('Ctrl Pts',(3.18838633393975,0.718152197254491,3.41358231176756));
#49543=CARTESIAN_POINT('Ctrl Pts',(3.17833113418676,0.763624982037616,3.40513577897662));
#49544=CARTESIAN_POINT('Ctrl Pts',(3.13840443789891,0.949782885938845,3.37192609991964));
#49545=CARTESIAN_POINT('Ctrl Pts',(3.11710083982675,1.04698696039931,3.35442517607146));
#49546=CARTESIAN_POINT('Ctrl Pts',(3.07985616677634,1.2,3.32482439211205));
#49547=CARTESIAN_POINT('',(3.3059688760626,-0.653834841531101,3.5158352655581));
#49548=CARTESIAN_POINT('Ctrl Pts',(3.3059688760626,-0.6538348415311,3.5158352655581));
#49549=CARTESIAN_POINT('Ctrl Pts',(3.26766469767615,-0.575797940622744,
3.53224408913098));
#49550=CARTESIAN_POINT('Ctrl Pts',(3.23528548386165,-0.49392132436527,3.54536167683063));
#49551=CARTESIAN_POINT('Ctrl Pts',(3.18740430810065,-0.338200813941495,
3.56201786612114));
#49552=CARTESIAN_POINT('Ctrl Pts',(3.17011432354766,-0.265716187090828,
3.566700550714));
#49553=CARTESIAN_POINT('Ctrl Pts',(3.14580106413494,-0.129745742366583,
3.56885504483666));
#49554=CARTESIAN_POINT('Ctrl Pts',(3.1376655006151,-0.066643296824382,3.56729763532479));
#49555=CARTESIAN_POINT('Ctrl Pts',(3.12737068196028,0.059553431415733,3.55881191132792));
#49556=CARTESIAN_POINT('Ctrl Pts',(3.12512315151907,0.12280156340828,3.55183285058316));
#49557=CARTESIAN_POINT('Ctrl Pts',(3.12735984298063,0.260160697362436,3.53121091709078));
#49558=CARTESIAN_POINT('Ctrl Pts',(3.13314355351978,0.333962939326844,3.51658347201579));
#49559=CARTESIAN_POINT('Ctrl Pts',(3.15628677742229,0.491153916066733,3.47819158431581));
#49560=CARTESIAN_POINT('Ctrl Pts',(3.1753971249946,0.574259753110387,3.45309552551028));
#49561=CARTESIAN_POINT('Ctrl Pts',(3.20083482131431,0.65383484143008,3.42413500689214));
#49562=CARTESIAN_POINT('',(3.25193073118135,-1.2,3.46805057381556));
#49563=CARTESIAN_POINT('Ctrl Pts',(3.25193073118135,-1.2,3.46805057381556));
#49564=CARTESIAN_POINT('Ctrl Pts',(3.2611441147676,-1.13542851615971,3.47607889408488));
#49565=CARTESIAN_POINT('Ctrl Pts',(3.27351847074519,-1.03917466802095,3.4869248101128));
#49566=CARTESIAN_POINT('Ctrl Pts',(3.29732029958888,-0.795561890270455,
3.50806949716737));
#49567=CARTESIAN_POINT('Ctrl Pts',(3.30108969495973,-0.741496651508692,
3.51145695404667));
#49568=CARTESIAN_POINT('Ctrl Pts',(3.3059688760626,-0.653834841531101,3.5158352655581));
#49569=CARTESIAN_POINT('Ctrl Pts',(3.12987662697833,-1.30000000000541,3.49508808473909));
#49570=CARTESIAN_POINT('Ctrl Pts',(3.13109823331778,-1.29899972592073,3.49481065515237));
#49571=CARTESIAN_POINT('Ctrl Pts',(3.13232167623714,-1.29800069349213,3.49453663626624));
#49572=CARTESIAN_POINT('Ctrl Pts',(3.15283006555946,-1.28106822770405,3.48970374150241));
#49573=CARTESIAN_POINT('Ctrl Pts',(3.17216112258937,-1.26515575976258,3.48526789140061));
#49574=CARTESIAN_POINT('Ctrl Pts',(3.2036719906995,-1.23909634935026,3.47796888024456));
#49575=CARTESIAN_POINT('Ctrl Pts',(3.22760791802916,-1.21917023077842,3.47228335861269));
#49576=CARTESIAN_POINT('Ctrl Pts',(3.25193073118135,-1.2,3.46805057381556));
#49577=CARTESIAN_POINT('Origin',(0.,1.25,7.2));
#49578=CARTESIAN_POINT('Origin',(0.,1.2,7.2));
#49579=CARTESIAN_POINT('Origin',(0.,0.92691742076555,7.2));
#49580=CARTESIAN_POINT('Origin',(0.,0.653834841531101,7.2));
#49581=CARTESIAN_POINT('Origin',(0.,0.,7.2));
#49582=CARTESIAN_POINT('Origin',(0.,-0.653834841531101,7.2));
#49583=CARTESIAN_POINT('Origin',(0.,-0.926917420765551,7.2));
#49584=CARTESIAN_POINT('Origin',(0.,-1.2,7.2));
#49585=CARTESIAN_POINT('Origin',(0.,-1.25,7.2));
#49586=CARTESIAN_POINT('Ctrl Pts',(3.58611066068443,-1.30000000000134,3.65199884532217));
#49587=CARTESIAN_POINT('Ctrl Pts',(3.56027544999399,-1.18514270861269,3.61812328835111));
#49588=CARTESIAN_POINT('Ctrl Pts',(3.53249270107514,-1.06847604194558,3.59858491022381));
#49589=CARTESIAN_POINT('Ctrl Pts',(3.46380979024152,-0.794772684000851,
3.58656909938251));
#49590=CARTESIAN_POINT('Ctrl Pts',(3.41064942873151,-0.636309800095197,
3.63209561276063));
#49591=CARTESIAN_POINT('Ctrl Pts',(3.34233892867367,-0.319434907277159,
3.66093066788605));
#49592=CARTESIAN_POINT('Ctrl Pts',(3.30866559173879,-0.158333333333332,
3.69207105417578));
#49593=CARTESIAN_POINT('Ctrl Pts',(3.2838391847674,0.158333333333334,3.66901547560771));
#49594=CARTESIAN_POINT('Ctrl Pts',(3.29150406597897,0.319434907277167,3.61383388564663));
#49595=CARTESIAN_POINT('Ctrl Pts',(3.31165271079405,0.636309800095206,3.54004392440282));
#49596=CARTESIAN_POINT('Ctrl Pts',(3.33806698632524,0.79477268400084,3.47055813438899));
#49597=CARTESIAN_POINT('Ctrl Pts',(3.37417869140185,1.06852528713347,3.4497186342675));
#49598=CARTESIAN_POINT('Ctrl Pts',(3.39064595623598,1.18523969452324,3.456907049513));
#49599=CARTESIAN_POINT('Ctrl Pts',(3.407945382661,1.30014322216931,3.48030665351317));
#49600=CARTESIAN_POINT('Ctrl Pts',(3.58274121447463,-1.30000000000134,3.66407993676206));
#49601=CARTESIAN_POINT('Ctrl Pts',(3.55620374542005,-1.18514270861269,3.6324754479871));
#49602=CARTESIAN_POINT('Ctrl Pts',(3.52792852769947,-1.06847604194558,3.61461081421486));
#49603=CARTESIAN_POINT('Ctrl Pts',(3.45859257127325,-0.794772684000851,
3.60508175009811));
#49604=CARTESIAN_POINT('Ctrl Pts',(3.40573136963311,-0.636309800095197,
3.65028594950435));
#49605=CARTESIAN_POINT('Ctrl Pts',(3.33750042120983,-0.319434907277159,
3.67925227433872));
#49606=CARTESIAN_POINT('Ctrl Pts',(3.30384439394135,-0.158333333333332,
3.70951459060301));
#49607=CARTESIAN_POINT('Ctrl Pts',(3.2794226920353,0.158333333333334,3.6866977360883));
#49608=CARTESIAN_POINT('Ctrl Pts',(3.28760112792004,0.319434907277167,3.63271287353839));
#49609=CARTESIAN_POINT('Ctrl Pts',(3.30823759882109,0.636309800095206,3.55911508785096));
#49610=CARTESIAN_POINT('Ctrl Pts',(3.33455638238822,0.794772684000839,3.49005172463855));
#49611=CARTESIAN_POINT('Ctrl Pts',(3.37126313977548,1.06852528713347,3.46667451953378));
#49612=CARTESIAN_POINT('Ctrl Pts',(3.38808948508963,1.18523969452324,3.47210378935024));
#49613=CARTESIAN_POINT('Ctrl Pts',(3.40584943566987,1.30014322216931,3.49308383984994));
#49614=CARTESIAN_POINT('Ctrl Pts',(3.57557006138374,-1.30000000000134,3.68788375928115));
#49615=CARTESIAN_POINT('Ctrl Pts',(3.54871468730387,-1.18514270861269,3.66160123862957));
#49616=CARTESIAN_POINT('Ctrl Pts',(3.52006039654804,-1.06847604194558,3.64752641016531));
#49617=CARTESIAN_POINT('Ctrl Pts',(3.44970739523745,-0.794772684000851,
3.64321295184625));
#49618=CARTESIAN_POINT('Ctrl Pts',(3.39554233222154,-0.636309800095199,
3.68647457548047));
#49619=CARTESIAN_POINT('Ctrl Pts',(3.32698774364401,-0.319434907277161,
3.71537815626217));
#49620=CARTESIAN_POINT('Ctrl Pts',(3.29412717751249,-0.158333333333332,
3.74437727537379));
#49621=CARTESIAN_POINT('Ctrl Pts',(3.27036429293828,0.158333333333334,3.7219560698061));
#49622=CARTESIAN_POINT('Ctrl Pts',(3.27878216535924,0.319434907277165,3.66988801420742));
#49623=CARTESIAN_POINT('Ctrl Pts',(3.30031819130643,0.636309800095206,3.59663343330932));
#49624=CARTESIAN_POINT('Ctrl Pts',(3.32721809087927,0.794772684000843,3.52889942146027));
#49625=CARTESIAN_POINT('Ctrl Pts',(3.36511136767073,1.06852528713347,3.50042325914989));
#49626=CARTESIAN_POINT('Ctrl Pts',(3.38251100926453,1.18523969452324,3.50222876615767));
#49627=CARTESIAN_POINT('Ctrl Pts',(3.40090383106788,1.30014322216931,3.51816896088486));
#49628=CARTESIAN_POINT('Ctrl Pts',(3.56833827722676,-1.30000000000135,3.71222778574955));
#49629=CARTESIAN_POINT('Ctrl Pts',(3.53951368675864,-1.1851427086127,3.69020412855297));
#49630=CARTESIAN_POINT('Ctrl Pts',(3.50953174671455,-1.06847604194559,3.67931834756835));
#49631=CARTESIAN_POINT('Ctrl Pts',(3.43759375829876,-0.79477268400086,3.67990073797496));
#49632=CARTESIAN_POINT('Ctrl Pts',(3.38473957204787,-0.636309800095202,
3.72298966139289));
#49633=CARTESIAN_POINT('Ctrl Pts',(3.31656863253884,-0.31943490727716,3.75231856887475));
#49634=CARTESIAN_POINT('Ctrl Pts',(3.28381112398346,-0.158333333333333,
3.77956240396853));
#49635=CARTESIAN_POINT('Ctrl Pts',(3.26055576646907,0.158333333333335,3.75744897779247));
#49636=CARTESIAN_POINT('Ctrl Pts',(3.26911907660334,0.319434907277167,3.70728528593329));
#49637=CARTESIAN_POINT('Ctrl Pts',(3.2918328786251,0.636309800095209,3.63455556259583));
#49638=CARTESIAN_POINT('Ctrl Pts',(3.32000435343564,0.794772684000844,3.56860834600287));
#49639=CARTESIAN_POINT('Ctrl Pts',(3.35920572172797,1.06852528713348,3.53499777280326));
#49640=CARTESIAN_POINT('Ctrl Pts',(3.37709638055073,1.18523969452325,3.53304948152668));
#49641=CARTESIAN_POINT('Ctrl Pts',(3.39590487901678,1.30014322216932,3.54370509973294));
#49642=CARTESIAN_POINT('Ctrl Pts',(3.56451873103144,-1.30000000000135,3.72490745184346));
#49643=CARTESIAN_POINT('Ctrl Pts',(3.53537269284097,-1.1851427086127,3.70561850550658));
#49644=CARTESIAN_POINT('Ctrl Pts',(3.50509427141749,-1.06847604194559,3.6966891013083));
#49645=CARTESIAN_POINT('Ctrl Pts',(3.43252902895124,-0.794772684000859,
3.69999300604859));
#49646=CARTESIAN_POINT('Ctrl Pts',(3.37924708572632,-0.636309800095202,
3.74222270265255));
#49647=CARTESIAN_POINT('Ctrl Pts',(3.3107713763284,-0.319434907277161,3.77142952113616));
#49648=CARTESIAN_POINT('Ctrl Pts',(3.2780046005121,-0.158333333333333,3.79770928059227));
#49649=CARTESIAN_POINT('Ctrl Pts',(3.25504948205071,0.158333333333335,3.77578028795297));
#49650=CARTESIAN_POINT('Ctrl Pts',(3.26416085675191,0.319434907277167,3.72692636513837));
#49651=CARTESIAN_POINT('Ctrl Pts',(3.28730506801098,0.636309800095209,3.65436593388957));
#49652=CARTESIAN_POINT('Ctrl Pts',(3.31522477600129,0.794772684000845,3.58878455992508));
#49653=CARTESIAN_POINT('Ctrl Pts',(3.35512040885107,1.06852528713348,3.55248950013008));
#49654=CARTESIAN_POINT('Ctrl Pts',(3.37347102058355,1.18523969452325,3.54869942253555));
#49655=CARTESIAN_POINT('Ctrl Pts',(3.39289883263694,1.30014322216932,3.55683375675957));
#49656=CARTESIAN_POINT('Ctrl Pts',(3.56405407843926,-1.30000000000135,3.72638825584007));
#49657=CARTESIAN_POINT('Ctrl Pts',(3.53486512075411,-1.1851427086127,3.70741783545932));
#49658=CARTESIAN_POINT('Ctrl Pts',(3.50454957210363,-1.06847604194559,3.69871726394456));
#49659=CARTESIAN_POINT('Ctrl Pts',(3.43191193961276,-0.79477268400086,3.70234260855873));
#49660=CARTESIAN_POINT('Ctrl Pts',(3.37859610411269,-0.636309800095202,
3.74448229810159));
#49661=CARTESIAN_POINT('Ctrl Pts',(3.3100842727485,-0.319434907277161,3.77367477472895));
#49662=CARTESIAN_POINT('Ctrl Pts',(3.27730053746247,-0.158333333333333,
3.79983058246958));
#49663=CARTESIAN_POINT('Ctrl Pts',(3.25437940413007,0.158333333333335,3.77792249528188));
#49664=CARTESIAN_POINT('Ctrl Pts',(3.26356406444697,0.319434907277167,3.72922864376837));
#49665=CARTESIAN_POINT('Ctrl Pts',(3.28676811589004,0.636309800095209,3.65669414717994));
#49666=CARTESIAN_POINT('Ctrl Pts',(3.31466720209241,0.794772684000845,3.5911614685024));
#49667=CARTESIAN_POINT('Ctrl Pts',(3.35464687355412,1.06852528713348,3.55455203426073));
#49668=CARTESIAN_POINT('Ctrl Pts',(3.37305048040543,1.18523969452325,3.5505445273049));
#49669=CARTESIAN_POINT('Ctrl Pts',(3.39254789692153,1.30014322216932,3.55838011592867));
#49670=CARTESIAN_POINT('Ctrl Pts',(3.56323412079071,-1.30000000000135,3.72897518027144));
#49671=CARTESIAN_POINT('Ctrl Pts',(3.53395858234347,-1.1851427086127,3.71055407799477));
#49672=CARTESIAN_POINT('Ctrl Pts',(3.50357082351767,-1.06847604194559,3.70224886594239));
#49673=CARTESIAN_POINT('Ctrl Pts',(3.43079957000651,-0.794772684000859,
3.70643189474446));
#49674=CARTESIAN_POINT('Ctrl Pts',(3.37743097835824,-0.636309800095202,
3.74841896020542));
#49675=CARTESIAN_POINT('Ctrl Pts',(3.30887043014344,-0.319434907277161,
3.77759635709755));
#49676=CARTESIAN_POINT('Ctrl Pts',(3.27608132292629,-0.158333333333333,
3.80355163191065));
#49677=CARTESIAN_POINT('Ctrl Pts',(3.25322209667042,0.158333333333335,3.78168201958454));
#49678=CARTESIAN_POINT('Ctrl Pts',(3.26250887851396,0.319434907277167,3.73325114933835));
#49679=CARTESIAN_POINT('Ctrl Pts',(3.28581677536265,0.636309800095209,3.66076127075894));
#49680=CARTESIAN_POINT('Ctrl Pts',(3.31370301444247,0.794772684000845,3.59532856098206));
#49681=CARTESIAN_POINT('Ctrl Pts',(3.35383280469244,1.06852528713348,3.55817086313435));
#49682=CARTESIAN_POINT('Ctrl Pts',(3.37232671642551,1.18523969452325,3.55378129974125));
#49683=CARTESIAN_POINT('Ctrl Pts',(3.39193974652874,1.30014322216932,3.56109015442525));
#49684=CARTESIAN_POINT('Ctrl Pts',(3.56156582974602,-1.30000000000135,3.73412995924475));
#49685=CARTESIAN_POINT('Ctrl Pts',(3.53209133194118,-1.1851427086127,3.71678998648117));
#49686=CARTESIAN_POINT('Ctrl Pts',(3.50154526127351,-1.06847604194559,3.70926618595618));
#49687=CARTESIAN_POINT('Ctrl Pts',(3.42850217963027,-0.794772684000859,
3.71456202320195));
#49688=CARTESIAN_POINT('Ctrl Pts',(3.37507654568519,-0.636309800095203,
3.75627781946126));
#49689=CARTESIAN_POINT('Ctrl Pts',(3.30643358005453,-0.319434907277161,
3.78543555203506));
#49690=CARTESIAN_POINT('Ctrl Pts',(3.2736276039743,-0.158333333333333,3.81098472065163));
#49691=CARTESIAN_POINT('Ctrl Pts',(3.25087704757571,0.158333333333335,3.7891821210627));
#49692=CARTESIAN_POINT('Ctrl Pts',(3.26032456276067,0.319434907277167,3.74124947997401));
#49693=CARTESIAN_POINT('Ctrl Pts',(3.28386454079099,0.636309800095209,3.66886461811563));
#49694=CARTESIAN_POINT('Ctrl Pts',(3.31182178754529,0.794772684000846,3.60369418477127));
#49695=CARTESIAN_POINT('Ctrl Pts',(3.35226734248451,1.06852528713348,3.5654497474108));
#49696=CARTESIAN_POINT('Ctrl Pts',(3.37093080265433,1.18523969452325,3.56028878987513));
#49697=CARTESIAN_POINT('Ctrl Pts',(3.39074621458239,1.30014322216932,3.56652537641267));
#49698=CARTESIAN_POINT('Ctrl Pts',(3.55795146928502,-1.30000000000135,3.74425510241154));
#49699=CARTESIAN_POINT('Ctrl Pts',(3.5276397670157,-1.1851427086127,3.72876901708838));
#49700=CARTESIAN_POINT('Ctrl Pts',(3.4965130841671,-1.06847604194559,3.72262266645001));
#49701=CARTESIAN_POINT('Ctrl Pts',(3.422721451741,-0.79477268400086,3.73000002243147));
#49702=CARTESIAN_POINT('Ctrl Pts',(3.36961874311334,-0.636309800095203,
3.77148182779834));
#49703=CARTESIAN_POINT('Ctrl Pts',(3.30126931674964,-0.319434907277161,
3.80091734639357));
#49704=CARTESIAN_POINT('Ctrl Pts',(3.26898601617818,-0.158333333333333,
3.82603122146535));
#49705=CARTESIAN_POINT('Ctrl Pts',(3.2465114457038,0.158333333333335,3.80441018268777));
#49706=CARTESIAN_POINT('Ctrl Pts',(3.25558832361884,0.319434907277168,3.75702201836801));
#49707=CARTESIAN_POINT('Ctrl Pts',(3.27964939834871,0.636309800095209,3.6848766247219));
#49708=CARTESIAN_POINT('Ctrl Pts',(3.30852724093942,0.794772684000846,3.62071968257323));
#49709=CARTESIAN_POINT('Ctrl Pts',(3.34969625632022,1.06852528713348,3.58035913324092));
#49710=CARTESIAN_POINT('Ctrl Pts',(3.36860193479976,1.18523969452325,3.57359493601362));
#49711=CARTESIAN_POINT('Ctrl Pts',(3.38858855032014,1.30014322216932,3.57754124552071));
#49712=CARTESIAN_POINT('Ctrl Pts',(3.55125760872384,-1.30000000000135,3.76488742240349));
#49713=CARTESIAN_POINT('Ctrl Pts',(3.51994370793949,-1.1851427086127,3.75358829971908));
#49714=CARTESIAN_POINT('Ctrl Pts',(3.48803104416294,-1.06847604194559,3.75046543253572));
#49715=CARTESIAN_POINT('Ctrl Pts',(3.41292314443867,-0.794772684000858,
3.76213977047639));
#49716=CARTESIAN_POINT('Ctrl Pts',(3.35964999376592,-0.636309800095202,
3.80257521452938));
#49717=CARTESIAN_POINT('Ctrl Pts',(3.29088986736577,-0.319434907277161,
3.8318703722204));
#49718=CARTESIAN_POINT('Ctrl Pts',(3.25849766059209,-0.158333333333334,
3.85531320792739));
#49719=CARTESIAN_POINT('Ctrl Pts',(3.23636220474763,0.158333333333336,3.83390613421074));
#49720=CARTESIAN_POINT('Ctrl Pts',(3.24588861328513,0.319434907277171,3.78841736816753));
#49721=CARTESIAN_POINT('Ctrl Pts',(3.27104806480137,0.636309800095212,3.71681884761097));
#49722=CARTESIAN_POINT('Ctrl Pts',(3.30067777372572,0.794772684000843,3.65401339492102));
#49723=CARTESIAN_POINT('Ctrl Pts',(3.34336407352903,1.06852528713348,3.60946500285551));
#49724=CARTESIAN_POINT('Ctrl Pts',(3.36300630369808,1.18523969452325,3.59964787807733));
#49725=CARTESIAN_POINT('Ctrl Pts',(3.38380909159561,1.30014322216933,3.59930152167878));
#49726=CARTESIAN_POINT('Ctrl Pts',(3.54143697371732,-1.30000000000136,3.79420796713043));
#49727=CARTESIAN_POINT('Ctrl Pts',(3.50854073084844,-1.1851427086127,3.78880121095158));
#49728=CARTESIAN_POINT('Ctrl Pts',(3.47534451349436,-1.06847604194558,3.78989510533326));
#49729=CARTESIAN_POINT('Ctrl Pts',(3.39796160945554,-0.794772684000852,
3.80744002343325));
#49730=CARTESIAN_POINT('Ctrl Pts',(3.34389786299372,-0.636309800095203,
3.84597495349244));
#49731=CARTESIAN_POINT('Ctrl Pts',(3.27464436116271,-0.319434907277163,
3.87513301512672));
#49732=CARTESIAN_POINT('Ctrl Pts',(3.2426752008845,-0.158333333333334,3.89660192235794));
#49733=CARTESIAN_POINT('Ctrl Pts',(3.22166096247914,0.158333333333336,3.87595595768556));
#49734=CARTESIAN_POINT('Ctrl Pts',(3.23257771150001,0.319434907277168,3.83369951488959));
#49735=CARTESIAN_POINT('Ctrl Pts',(3.25910447812562,0.636309800095211,3.76277547949074));
#49736=CARTESIAN_POINT('Ctrl Pts',(3.28834676493135,0.794772684000847,3.70095602241445));
#49737=CARTESIAN_POINT('Ctrl Pts',(3.3330176648565,1.06852528713348,3.65028482032406));
#49738=CARTESIAN_POINT('Ctrl Pts',(3.35389657654681,1.18523969452325,3.63620894075663));
#49739=CARTESIAN_POINT('Ctrl Pts',(3.37631346515805,1.30014322216933,3.62999603702785));
#49740=CARTESIAN_POINT('Ctrl Pts',(3.5308494554429,-1.30000000000135,3.82301235750127));
#49741=CARTESIAN_POINT('Ctrl Pts',(3.49565379721992,-1.1851427086127,3.82299168397096));
#49742=CARTESIAN_POINT('Ctrl Pts',(3.46082623482376,-1.06847604194559,3.82805987493514));
#49743=CARTESIAN_POINT('Ctrl Pts',(3.38121797345607,-0.79477268400086,3.85152470495659));
#49744=CARTESIAN_POINT('Ctrl Pts',(3.3279576869809,-0.636309800095204,3.88931306817055));
#49745=CARTESIAN_POINT('Ctrl Pts',(3.25892586967109,-0.319434907277163,
3.9188460358497));
#49746=CARTESIAN_POINT('Ctrl Pts',(3.22769302712512,-0.158333333333334,
3.93853026895662));
#49747=CARTESIAN_POINT('Ctrl Pts',(3.20691438908692,0.158333333333336,3.91804349652783));
#49748=CARTESIAN_POINT('Ctrl Pts',(3.21706206652025,0.319434907277172,3.87755908286915));
#49749=CARTESIAN_POINT('Ctrl Pts',(3.24439366783777,0.636309800095215,3.80693442462951));
#49750=CARTESIAN_POINT('Ctrl Pts',(3.27458119135646,0.79477268400085,3.7470230193912));
#49751=CARTESIAN_POINT('Ctrl Pts',(3.32176363692496,1.06852528713348,3.6905707095344));
#49752=CARTESIAN_POINT('Ctrl Pts',(3.34402017306192,1.18523969452325,3.67231724709913));
#49753=CARTESIAN_POINT('Ctrl Pts',(3.36810489928664,1.30014322216932,3.66025219477543));
#49754=CARTESIAN_POINT('Ctrl Pts',(3.52371537962296,-1.30000000000135,3.84339604055803));
#49755=CARTESIAN_POINT('Ctrl Pts',(3.48731301665105,-1.1851427086127,3.84745493965236));
#49756=CARTESIAN_POINT('Ctrl Pts',(3.45142165013046,-1.06847604194559,3.85537158057938));
#49757=CARTESIAN_POINT('Ctrl Pts',(3.36968591745182,-0.79477268400086,3.88257276021143));
#49758=CARTESIAN_POINT('Ctrl Pts',(3.31503821404233,-0.636309800095207,
3.91839227977945));
#49759=CARTESIAN_POINT('Ctrl Pts',(3.24543711991941,-0.319434907277165,
3.94766351942526));
#49760=CARTESIAN_POINT('Ctrl Pts',(3.21504596931657,-0.158333333333335,
3.96635996650926));
#49761=CARTESIAN_POINT('Ctrl Pts',(3.19521296665219,0.158333333333337,3.94655979247265));
#49762=CARTESIAN_POINT('Ctrl Pts',(3.20589244968541,0.31943490727717,3.90809629468899));
#49763=CARTESIAN_POINT('Ctrl Pts',(3.23484799455299,0.636309800095215,3.83842605633801));
#49764=CARTESIAN_POINT('Ctrl Pts',(3.2663336670866,0.794772684000854,3.78025792039953));
#49765=CARTESIAN_POINT('Ctrl Pts',(3.31526112888122,1.06852528713349,3.71973885925459));
#49766=CARTESIAN_POINT('Ctrl Pts',(3.3382448472766,1.18523969452325,3.69839512736118));
#49767=CARTESIAN_POINT('Ctrl Pts',(3.36302840712315,1.30014322216933,3.68191029696368));
#49768=CARTESIAN_POINT('Ctrl Pts',(3.51979390028975,-1.30000000000136,3.85333145849074));
#49769=CARTESIAN_POINT('Ctrl Pts',(3.48238428396745,-1.1851427086127,3.85912832344819));
#49770=CARTESIAN_POINT('Ctrl Pts',(3.44581182126015,-1.06847604194559,3.86835725545699));
#49771=CARTESIAN_POINT('Ctrl Pts',(3.36325610843303,-0.794772684000859,
3.89760669611004));
#49772=CARTESIAN_POINT('Ctrl Pts',(3.30933112338547,-0.636309800095206,
3.93349727704609));
#49773=CARTESIAN_POINT('Ctrl Pts',(3.23978280683933,-0.319434907277165,
3.96288649231997));
#49774=CARTESIAN_POINT('Ctrl Pts',(3.20930922997601,-0.158333333333335,
3.98070348680371));
#49775=CARTESIAN_POINT('Ctrl Pts',(3.1893653703264,0.158333333333337,3.96082437654682));
#49776=CARTESIAN_POINT('Ctrl Pts',(3.19981109945215,0.319434907277172,3.9230136476974));
#49777=CARTESIAN_POINT('Ctrl Pts',(3.22890628758542,0.636309800095216,3.85336559723001));
#49778=CARTESIAN_POINT('Ctrl Pts',(3.26044354591702,0.794772684000854,3.79569967042955));
#49779=CARTESIAN_POINT('Ctrl Pts',(3.31033911162144,1.06852528713349,3.73321313335938));
#49780=CARTESIAN_POINT('Ctrl Pts',(3.33393151120473,1.18523969452325,3.71048413390068));
#49781=CARTESIAN_POINT('Ctrl Pts',(3.35951327834847,1.30014322216933,3.69208061652413));
#49782=CARTESIAN_POINT('Ctrl Pts',(3.5179290077231,-1.30000000000135,3.85837468584765));
#49783=CARTESIAN_POINT('Ctrl Pts',(3.48005403549629,-1.1851427086127,3.86506852730633));
#49784=CARTESIAN_POINT('Ctrl Pts',(3.44314187351344,-1.06847604194559,3.87495403837134));
#49785=CARTESIAN_POINT('Ctrl Pts',(3.36009167935358,-0.794772684000861,
3.90516494180309));
#49786=CARTESIAN_POINT('Ctrl Pts',(3.30629219032297,-0.636309800095207,
3.94091742287119));
#49787=CARTESIAN_POINT('Ctrl Pts',(3.23666675631854,-0.319434907277165,
3.97028826328755));
#49788=CARTESIAN_POINT('Ctrl Pts',(3.20612698068171,-0.158333333333335,
3.98764668534676));
#49789=CARTESIAN_POINT('Ctrl Pts',(3.18630624078372,0.158333333333337,3.96785644620198));
#49790=CARTESIAN_POINT('Ctrl Pts',(3.19698046189018,0.319434907277171,3.9306236218399));
#49791=CARTESIAN_POINT('Ctrl Pts',(3.22632376004245,0.636309800095215,3.86111292352323));
#49792=CARTESIAN_POINT('Ctrl Pts',(3.25777655973932,0.794772684000855,3.80361188830843));
#49793=CARTESIAN_POINT('Ctrl Pts',(3.30817850266376,1.06852528713349,3.74015681273327));
#49794=CARTESIAN_POINT('Ctrl Pts',(3.33209361724937,1.18523969452325,3.71674937395376));
#49795=CARTESIAN_POINT('Ctrl Pts',(3.35810157080076,1.30014322216933,3.69740832117871));
#49796=CARTESIAN_POINT('Ctrl Pts',(3.51685348631722,-1.30000000000135,3.86124902200402));
#49797=CARTESIAN_POINT('Ctrl Pts',(3.47871524848394,-1.1851427086127,3.86845787734754));
#49798=CARTESIAN_POINT('Ctrl Pts',(3.44161058451423,-1.06847604194559,3.87872010796917));
#49799=CARTESIAN_POINT('Ctrl Pts',(3.35827915037236,-0.794772684000861,
3.90948182137531));
#49800=CARTESIAN_POINT('Ctrl Pts',(3.30454936288267,-0.636309800095207,
3.94515362384163));
#49801=CARTESIAN_POINT('Ctrl Pts',(3.23487623129755,-0.319434907277165,
3.97451120451713));
#49802=CARTESIAN_POINT('Ctrl Pts',(3.20429173341362,-0.158333333333335,
3.99160236582141));
#49803=CARTESIAN_POINT('Ctrl Pts',(3.18454347805265,0.158333333333337,3.97186450496687));
#49804=CARTESIAN_POINT('Ctrl Pts',(3.19535519874992,0.319434907277171,3.93496742549603));
#49805=CARTESIAN_POINT('Ctrl Pts',(3.22485250527958,0.636309800095216,3.86554387127726));
#49806=CARTESIAN_POINT('Ctrl Pts',(3.25627421268125,0.794772684000854,3.80814857075943));
#49807=CARTESIAN_POINT('Ctrl Pts',(3.30696480236959,1.06852528713349,3.74413943949904));
#49808=CARTESIAN_POINT('Ctrl Pts',(3.33105931371092,1.18523969452325,3.72034083223412));
#49809=CARTESIAN_POINT('Ctrl Pts',(3.3573010868368,1.30014322216933,3.70045732919041));
#49810=CARTESIAN_POINT('Ctrl Pts',(3.51180487015753,-1.30000000000136,3.87401110494669));
#49811=CARTESIAN_POINT('Ctrl Pts',(3.47264024281404,-1.1851427086127,3.88366306949258));
#49812=CARTESIAN_POINT('Ctrl Pts',(3.43474217778609,-1.06847604194559,3.89567950440077));
#49813=CARTESIAN_POINT('Ctrl Pts',(3.35011607841354,-0.794772684000859,
3.92890227246578));
#49814=CARTESIAN_POINT('Ctrl Pts',(3.2962603770796,-0.636309800095206,3.9638733351931));
#49815=CARTESIAN_POINT('Ctrl Pts',(3.22630686737986,-0.319434907277165,
3.99312184883118));
#49816=CARTESIAN_POINT('Ctrl Pts',(3.19568831864123,-0.158333333333335,
4.00914097268011));
#49817=CARTESIAN_POINT('Ctrl Pts',(3.17652657558406,0.158333333333337,3.98983366734609));
#49818=CARTESIAN_POINT('Ctrl Pts',(3.18823486903591,0.319434907277171,3.95465441538546));
#49819=CARTESIAN_POINT('Ctrl Pts',(3.2186450253389,0.636309800095215,3.88577852154938));
#49820=CARTESIAN_POINT('Ctrl Pts',(3.25004744052039,0.794772684000853,3.82892797482705));
#49821=CARTESIAN_POINT('Ctrl Pts',(3.30185451104873,1.06852528713349,3.76229555265933));
#49822=CARTESIAN_POINT('Ctrl Pts',(3.32659192685424,1.18523969452325,3.73662293940689));
#49823=CARTESIAN_POINT('Ctrl Pts',(3.35363611181697,1.30014322216933,3.71412721745266));
#49824=CARTESIAN_POINT('Ctrl Pts',(3.50259650582532,-1.30000000000136,3.89746406347487));
#49825=CARTESIAN_POINT('Ctrl Pts',(3.46154999817241,-1.1851427086127,3.91159800414215));
#49826=CARTESIAN_POINT('Ctrl Pts',(3.42218167181803,-1.06847604194559,3.92682005562182));
#49827=CARTESIAN_POINT('Ctrl Pts',(3.33510989685151,-0.794772684000861,
3.9644997933532));
#49828=CARTESIAN_POINT('Ctrl Pts',(3.28073758681194,-0.636309800095206,
3.9979602998355));
#49829=CARTESIAN_POINT('Ctrl Pts',(3.21051363500489,-0.319434907277164,
4.02719485174671));
#49830=CARTESIAN_POINT('Ctrl Pts',(3.18100004367731,-0.158333333333335,
4.04212537242215));
#49831=CARTESIAN_POINT('Ctrl Pts',(3.16212607813994,0.158333333333337,4.02304941802012));
#49832=CARTESIAN_POINT('Ctrl Pts',(3.17290244559924,0.31943490727717,3.9891388498205));
#49833=CARTESIAN_POINT('Ctrl Pts',(3.20440295564305,0.636309800095215,3.92085259690198));
#49834=CARTESIAN_POINT('Ctrl Pts',(3.23732532390392,0.794772684000853,3.86615764113347));
#49835=CARTESIAN_POINT('Ctrl Pts',(3.29193397918288,1.06852528713349,3.79525519905378));
#49836=CARTESIAN_POINT('Ctrl Pts',(3.31809858178777,1.18523969452325,3.76631546584324));
#49837=CARTESIAN_POINT('Ctrl Pts',(3.34678415229658,1.30014322216933,3.73913427300855));
#49838=CARTESIAN_POINT('Ctrl Pts',(3.49089583575975,-1.30000000000135,3.92550201961658));
#49839=CARTESIAN_POINT('Ctrl Pts',(3.44736236322143,-1.1851427086127,3.94492906119646));
#49840=CARTESIAN_POINT('Ctrl Pts',(3.40609555172084,-1.06847604194558,3.96395922057786));
#49841=CARTESIAN_POINT('Ctrl Pts',(3.31599740219843,-0.794772684000857,
4.00700581844465));
#49842=CARTESIAN_POINT('Ctrl Pts',(3.26166161224019,-0.636309800095204,
4.03913026138824));
#49843=CARTESIAN_POINT('Ctrl Pts',(3.1905759569815,-0.319434907277163,4.06792484823472));
#49844=CARTESIAN_POINT('Ctrl Pts',(3.16068882050753,-0.158333333333334,
4.08020066157171));
#49845=CARTESIAN_POINT('Ctrl Pts',(3.14236254451807,0.158333333333336,4.06156050213763));
#49846=CARTESIAN_POINT('Ctrl Pts',(3.1541827888424,0.319434907277169,4.03086642678733));
#49847=CARTESIAN_POINT('Ctrl Pts',(3.18741079324074,0.636309800095212,3.96365118824068));
#49848=CARTESIAN_POINT('Ctrl Pts',(3.22079758656425,0.79477268400085,3.91058590082593));
#49849=CARTESIAN_POINT('Ctrl Pts',(3.2784066018515,1.06852528713348,3.83421419732015));
#49850=CARTESIAN_POINT('Ctrl Pts',(3.3062703620255,1.18523969452325,3.80127839118273));
#49851=CARTESIAN_POINT('Ctrl Pts',(3.33705519689666,1.30014322216932,3.76847305109419));
#49852=CARTESIAN_POINT('Ctrl Pts',(3.47625432854937,-1.30000000000135,3.95868777960396));
#49853=CARTESIAN_POINT('Ctrl Pts',(3.42911187370096,-1.1851427086127,3.98396161926474));
#49854=CARTESIAN_POINT('Ctrl Pts',(3.38511464244507,-1.06847604194558,4.00719727209129));
#49855=CARTESIAN_POINT('Ctrl Pts',(3.29073833232675,-0.794772684000857,
4.056167659072));
#49856=CARTESIAN_POINT('Ctrl Pts',(3.23624777135572,-0.636309800095203,
4.08654859182015));
#49857=CARTESIAN_POINT('Ctrl Pts',(3.16482158835148,-0.319434907277162,
4.11536321774138));
#49858=CARTESIAN_POINT('Ctrl Pts',(3.13634639591439,-0.158333333333334,
4.12589756673083));
#49859=CARTESIAN_POINT('Ctrl Pts',(3.11868364739977,0.158333333333336,4.10781157269918));
#49860=CARTESIAN_POINT('Ctrl Pts',(3.12966022013018,0.319434907277171,4.07938414633349));
#49861=CARTESIAN_POINT('Ctrl Pts',(3.16477433760615,0.636309800095214,4.01333669546797));
#49862=CARTESIAN_POINT('Ctrl Pts',(3.20002198057908,0.794772684000849,3.96326008053157));
#49863=CARTESIAN_POINT('Ctrl Pts',(3.26221817393558,1.06852528713348,3.88106524589728));
#49864=CARTESIAN_POINT('Ctrl Pts',(3.29253078212396,1.18523969452325,3.84362847782292));
#49865=CARTESIAN_POINT('Ctrl Pts',(3.32622722561664,1.30014322216932,3.80434242564489));
#49866=CARTESIAN_POINT('Ctrl Pts',(3.46117898356208,-1.30000000000135,3.99157311770267));
#49867=CARTESIAN_POINT('Ctrl Pts',(3.41076491298548,-1.1851427086127,4.023001957923));
#49868=CARTESIAN_POINT('Ctrl Pts',(3.36415720577044,-1.06847604194558,4.05056023207062));
#49869=CARTESIAN_POINT('Ctrl Pts',(3.26527753908959,-0.794772684000856,
4.1052835764333));
#49870=CARTESIAN_POINT('Ctrl Pts',(3.20964019318071,-0.636309800095204,
4.13305481307774));
#49871=CARTESIAN_POINT('Ctrl Pts',(3.13712088711537,-0.319434907277164,
4.16127738694213));
#49872=CARTESIAN_POINT('Ctrl Pts',(3.10939958819912,-0.158333333333334,
4.16957122426424));
#49873=CARTESIAN_POINT('Ctrl Pts',(3.09289608996282,0.158333333333336,4.15246771284705));
#49874=CARTESIAN_POINT('Ctrl Pts',(3.10494510744031,0.31943490727717,4.12785984948249));
#49875=CARTESIAN_POINT('Ctrl Pts',(3.14215484712265,0.636309800095213,4.06319052949148));
#49876=CARTESIAN_POINT('Ctrl Pts',(3.1777260399402,0.794772684000852,4.01491400155314));
#49877=CARTESIAN_POINT('Ctrl Pts',(3.24388341852259,1.06852528713348,3.92641073195946));
#49878=CARTESIAN_POINT('Ctrl Pts',(3.27651390845349,1.18523969452325,3.88436610441899));
#49879=CARTESIAN_POINT('Ctrl Pts',(3.31313106099549,1.30014322216932,3.83859566465085));
#49880=CARTESIAN_POINT('Ctrl Pts',(3.44485221849218,-1.30000000000135,4.02343367468143));
#49881=CARTESIAN_POINT('Ctrl Pts',(3.3904531107521,-1.1851427086127,4.06041041072846));
#49882=CARTESIAN_POINT('Ctrl Pts',(3.34077120931611,-1.06847604194558,4.09188873350675));
#49883=CARTESIAN_POINT('Ctrl Pts',(3.23689376840521,-0.794772684000859,
4.15190752173675));
#49884=CARTESIAN_POINT('Ctrl Pts',(3.18091387827706,-0.636309800095201,
4.1776973988966));
#49885=CARTESIAN_POINT('Ctrl Pts',(3.10714605361911,-0.319434907277161,
4.20514333036985));
#49886=CARTESIAN_POINT('Ctrl Pts',(3.07968331606346,-0.158333333333333,
4.21070967621743));
#49887=CARTESIAN_POINT('Ctrl Pts',(3.06375590315938,0.158333333333335,4.19416442293091));
#49888=CARTESIAN_POINT('Ctrl Pts',(3.07589901910471,0.319434907277169,4.17273488913912));
#49889=CARTESIAN_POINT('Ctrl Pts',(3.11598582338588,0.63630980009521,4.11019815002703));
#49890=CARTESIAN_POINT('Ctrl Pts',(3.15393758156696,0.794772684000845,4.06545604734486));
#49891=CARTESIAN_POINT('Ctrl Pts',(3.22569455534372,1.06852528713348,3.97196316158908));
#49892=CARTESIAN_POINT('Ctrl Pts',(3.26123632842328,1.18523969452324,3.92576064732784));
#49893=CARTESIAN_POINT('Ctrl Pts',(3.30125161870687,1.30014322216932,3.87383476312156));
#49894=CARTESIAN_POINT('Ctrl Pts',(3.43445482759663,-1.30000000000135,4.04512352187352));
#49895=CARTESIAN_POINT('Ctrl Pts',(3.37739310683949,-1.1851427086127,4.08582511462002));
#49896=CARTESIAN_POINT('Ctrl Pts',(3.32553252350525,-1.06847604194558,4.11982694886549));
#49897=CARTESIAN_POINT('Ctrl Pts',(3.2177398692601,-0.794772684000855,4.18290020559656));
#49898=CARTESIAN_POINT('Ctrl Pts',(3.1602717043156,-0.636309800095199,4.2062596545617));
#49899=CARTESIAN_POINT('Ctrl Pts',(3.08559934474851,-0.31943490727716,4.23313249169756));
#49900=CARTESIAN_POINT('Ctrl Pts',(3.05951170294829,-0.158333333333333,
4.23793047763546));
#49901=CARTESIAN_POINT('Ctrl Pts',(3.04424337809605,0.158333333333335,4.22200977856802));
#49902=CARTESIAN_POINT('Ctrl Pts',(3.05606999883945,0.31943490727717,4.20236614100586));
#49903=CARTESIAN_POINT('Ctrl Pts',(3.09759007473543,0.63630980009521,4.14087419196223));
#49904=CARTESIAN_POINT('Ctrl Pts',(3.13660284781725,0.794772684000843,4.09810486373787));
#49905=CARTESIAN_POINT('Ctrl Pts',(3.21170591764102,1.06852528713347,4.0009754697502));
#49906=CARTESIAN_POINT('Ctrl Pts',(3.24908590504518,1.18523969452324,3.95191024741244));
#49907=CARTESIAN_POINT('Ctrl Pts',(3.29132888160908,1.30014322216931,3.89583342772439));
#49908=CARTESIAN_POINT('Ctrl Pts',(3.42583540128219,-1.30000000000135,4.06067213536237));
#49909=CARTESIAN_POINT('Ctrl Pts',(3.36661288013924,-1.1851427086127,4.10398359613909));
#49910=CARTESIAN_POINT('Ctrl Pts',(3.31307522218595,-1.06847604194558,4.13980302109888));
#49911=CARTESIAN_POINT('Ctrl Pts',(3.20252569336342,-0.794772684000855,
4.2052449568935));
#49912=CARTESIAN_POINT('Ctrl Pts',(3.1448199300957,-0.636309800095199,4.22749548355176));
#49913=CARTESIAN_POINT('Ctrl Pts',(3.06936510190686,-0.319434907277159,
4.25380950454983));
#49914=CARTESIAN_POINT('Ctrl Pts',(3.04329844177634,-0.158333333333333,
4.25715800894188));
#49915=CARTESIAN_POINT('Ctrl Pts',(3.02831998681033,0.158333333333335,4.241544528057));
#49916=CARTESIAN_POINT('Ctrl Pts',(3.04035721885161,0.319434907277168,4.22365522892132));
#49917=CARTESIAN_POINT('Ctrl Pts',(3.08336891334343,0.636309800095208,4.16335268713494));
#49918=CARTESIAN_POINT('Ctrl Pts',(3.12328012705945,0.794772684000842,4.12220188537788));
#49919=CARTESIAN_POINT('Ctrl Pts',(3.20157995038045,1.06852528713347,4.02295034772459));
#49920=CARTESIAN_POINT('Ctrl Pts',(3.24072639992362,1.18523969452324,3.97206638214448));
#49921=CARTESIAN_POINT('Ctrl Pts',(3.28511821848901,1.30014322216931,3.91327088983663));
#49922=CARTESIAN_POINT('Ctrl Pts',(3.41867497750123,-1.30000000000135,4.07366642162037));
#49923=CARTESIAN_POINT('Ctrl Pts',(3.35786428909695,-1.1851427086127,4.11939666182868));
#49924=CARTESIAN_POINT('Ctrl Pts',(3.30294497738628,-1.06847604194559,4.15678994545929));
#49925=CARTESIAN_POINT('Ctrl Pts',(3.1896806394923,-0.794772684000859,4.22391587364973));
#49926=CARTESIAN_POINT('Ctrl Pts',(3.12999634180018,-0.6363098000952,4.24366964123252));
#49927=CARTESIAN_POINT('Ctrl Pts',(3.05446827144717,-0.319434907277159,
4.27009294864879));
#49928=CARTESIAN_POINT('Ctrl Pts',(3.03115588594621,-0.158333333333333,
4.27472361324213));
#49929=CARTESIAN_POINT('Ctrl Pts',(3.01693050365394,0.158333333333335,4.25983509121364));
#49930=CARTESIAN_POINT('Ctrl Pts',(3.02744853280611,0.31943490727717,4.2418711520045));
#49931=CARTESIAN_POINT('Ctrl Pts',(3.07108562688173,0.63630980009521,4.18195307022728));
#49932=CARTESIAN_POINT('Ctrl Pts',(3.11216848002771,0.794772684000844,4.14246168042456));
#49933=CARTESIAN_POINT('Ctrl Pts',(3.19285610432454,1.06852528713347,4.04114397801849));
#49934=CARTESIAN_POINT('Ctrl Pts',(3.23327308090119,1.18523969452324,3.98854953307814));
#49935=CARTESIAN_POINT('Ctrl Pts',(3.27917211935977,1.30014322216931,3.92722765900645));
#49936=CARTESIAN_POINT('Ctrl Pts',(3.41288009340851,-1.30000000000134,4.0840369854531));
#49937=CARTESIAN_POINT('Ctrl Pts',(3.3501085556977,-1.18514270861269,4.13109309512308));
#49938=CARTESIAN_POINT('Ctrl Pts',(3.2938516684092,-1.06847604194558,4.1695359618191));
#49939=CARTESIAN_POINT('Ctrl Pts',(3.17893715034814,-0.794772684000856,
4.2384483600127));
#49940=CARTESIAN_POINT('Ctrl Pts',(3.12033039179534,-0.636309800095199,
4.25855232243253));
#49941=CARTESIAN_POINT('Ctrl Pts',(3.04531401376896,-0.31943490727716,4.28547323290277));
#49942=CARTESIAN_POINT('Ctrl Pts',(3.0229656380322,-0.158333333333333,4.2898835348833));
#49943=CARTESIAN_POINT('Ctrl Pts',(3.00852261298693,0.158333333333335,4.27481928527001));
#49944=CARTESIAN_POINT('Ctrl Pts',(3.0174471831594,0.319434907277169,4.25653778583326));
#49945=CARTESIAN_POINT('Ctrl Pts',(3.06096808240439,0.636309800095209,4.19650192222135));
#49946=CARTESIAN_POINT('Ctrl Pts',(3.1026006996025,0.794772684000843,4.1581458150171));
#49947=CARTESIAN_POINT('Ctrl Pts',(3.18512170256247,1.06852528713347,4.05516397331139));
#49948=CARTESIAN_POINT('Ctrl Pts',(3.22664119150678,1.18523969452324,4.00127326457945));
#49949=CARTESIAN_POINT('Ctrl Pts',(3.27395146596591,1.30014322216931,3.93807937694368));
#49950=CARTESIAN_POINT('Ctrl Pts',(3.4085543132438,-1.30000000000134,4.09168377759149));
#49951=CARTESIAN_POINT('Ctrl Pts',(3.34467845415707,-1.18514270861269,4.13986232556471));
#49952=CARTESIAN_POINT('Ctrl Pts',(3.28766192706407,-1.06847604194558,4.17917206071897));
#49953=CARTESIAN_POINT('Ctrl Pts',(3.1717887724725,-0.794772684000855,4.24949668099906));
#49954=CARTESIAN_POINT('Ctrl Pts',(3.11371826607727,-0.636309800095199,
4.26970423515541));
#49955=CARTESIAN_POINT('Ctrl Pts',(3.03899940900825,-0.319434907277159,
4.29698286659211));
#49956=CARTESIAN_POINT('Ctrl Pts',(3.01725958678558,-0.158333333333333,
4.30125685881936));
#49957=CARTESIAN_POINT('Ctrl Pts',(3.00276096947443,0.158333333333335,4.28616267948842));
#49958=CARTESIAN_POINT('Ctrl Pts',(3.01082965053031,0.319434907277169,4.26783367352206));
#49959=CARTESIAN_POINT('Ctrl Pts',(3.05433035874579,0.636309800095209,4.20769258011705));
#49960=CARTESIAN_POINT('Ctrl Pts',(3.09623103923164,0.794772684000843,4.16992322245467));
#49961=CARTESIAN_POINT('Ctrl Pts',(3.17988110680528,1.06852528713347,4.06564020803105));
#49962=CARTESIAN_POINT('Ctrl Pts',(3.22208818472508,1.18523969452324,4.01079574450038));
#49963=CARTESIAN_POINT('Ctrl Pts',(3.27028479171056,1.30014322216931,3.94625770947172));
#49964=CARTESIAN_POINT('Ctrl Pts',(3.40082388779475,-1.30000000000134,4.10430824537168));
#49965=CARTESIAN_POINT('Ctrl Pts',(3.33423500616368,-1.18514270861269,4.15421179357926));
#49966=CARTESIAN_POINT('Ctrl Pts',(3.27551973015998,-1.06847604194558,4.19505922110236));
#49967=CARTESIAN_POINT('Ctrl Pts',(3.15806530074953,-0.794772684000855,
4.26850349972861));
#49968=CARTESIAN_POINT('Ctrl Pts',(3.10273257509845,-0.636309800095199,
4.29056591942227));
#49969=CARTESIAN_POINT('Ctrl Pts',(3.02937307405698,-0.31943490727716,4.3192570837257));
#49970=CARTESIAN_POINT('Ctrl Pts',(3.00855323477179,-0.158333333333333,
4.32288342726441));
#49971=CARTESIAN_POINT('Ctrl Pts',(2.99403405178878,0.158333333333335,4.30779225194209));
#49972=CARTESIAN_POINT('Ctrl Pts',(3.00087337772276,0.319434907277168,4.28986623407122));
#49973=CARTESIAN_POINT('Ctrl Pts',(3.04356111718931,0.636309800095208,4.22882320170994));
#49974=CARTESIAN_POINT('Ctrl Pts',(3.08413237899026,0.794772684000843,4.1904766533688));
#49975=CARTESIAN_POINT('Ctrl Pts',(3.16950424792553,1.06852528713347,4.08314582629006));
#49976=CARTESIAN_POINT('Ctrl Pts',(3.21317507354939,1.18523969452324,4.02651144248977));
#49977=CARTESIAN_POINT('Ctrl Pts',(3.26355369627107,1.30014322216931,3.95971316303145));
#49978=CARTESIAN_POINT('Ctrl Pts',(3.39464917870745,-1.30000000000134,4.11466263946878));
#49979=CARTESIAN_POINT('Ctrl Pts',(3.32510507657478,-1.18514270861269,4.16518479880478));
#49980=CARTESIAN_POINT('Ctrl Pts',(3.26482642907165,-1.06847604194558,4.2069153131676));
#49981=CARTESIAN_POINT('Ctrl Pts',(3.1469757483796,-0.794772684000851,4.28301069085576));
#49982=CARTESIAN_POINT('Ctrl Pts',(3.09694274384213,-0.636309800095197,
4.30845659929));
#49983=CARTESIAN_POINT('Ctrl Pts',(3.02637005246077,-0.319434907277159,
4.33908386446847));
#49984=CARTESIAN_POINT('Ctrl Pts',(3.00610967573939,-0.158333333333332,
4.34183776787586));
#49985=CARTESIAN_POINT('Ctrl Pts',(2.99178190375838,0.158333333333334,4.32686979332697));
#49986=CARTESIAN_POINT('Ctrl Pts',(2.99824187046467,0.319434907277167,4.30984680666278));
#49987=CARTESIAN_POINT('Ctrl Pts',(3.03855572360122,0.636309800095206,4.24730726381801));
#49988=CARTESIAN_POINT('Ctrl Pts',(3.07431251187027,0.79477268400084,4.20635824741822));
#49989=CARTESIAN_POINT('Ctrl Pts',(3.16003068251616,1.06852528713347,4.09631458963396));
#49990=CARTESIAN_POINT('Ctrl Pts',(3.20509827163572,1.18523969452324,4.03856156651537));
#49991=CARTESIAN_POINT('Ctrl Pts',(3.2581204848396,1.30014322216931,3.97070056908081));
#49992=CARTESIAN_POINT('Ctrl Pts',(3.39266784164081,-1.30000000000134,4.12304256032365));
#49993=CARTESIAN_POINT('Ctrl Pts',(3.32321437844547,-1.18514270861269,4.17332679788356));
#49994=CARTESIAN_POINT('Ctrl Pts',(3.26328407460055,-1.06847604194558,4.21505186785088));
#49995=CARTESIAN_POINT('Ctrl Pts',(3.14683348690377,-0.794772684000851,
4.29167173715239));
#49996=CARTESIAN_POINT('Ctrl Pts',(3.09897158712509,-0.636309800095197,
4.31848151812622));
#49997=CARTESIAN_POINT('Ctrl Pts',(3.02986065695598,-0.319434907277159,
4.3499500784224));
#49998=CARTESIAN_POINT('Ctrl Pts',(3.00955419085523,-0.158333333333332,
4.35273203641936));
#49999=CARTESIAN_POINT('Ctrl Pts',(2.99544198242645,0.158333333333334,4.33786307216675));
#50000=CARTESIAN_POINT('Ctrl Pts',(3.00240549451288,0.319434907277167,4.32105409284838));
#50001=CARTESIAN_POINT('Ctrl Pts',(3.04120395637117,0.636309800095206,4.25758354584163));
#50002=CARTESIAN_POINT('Ctrl Pts',(3.07388603025902,0.79477268400084,4.21466382420666));
#50003=CARTESIAN_POINT('Ctrl Pts',(3.15832509141374,1.06852528713347,4.10419092108222));
#50004=CARTESIAN_POINT('Ctrl Pts',(3.20330442392552,1.18523969452324,4.04663254077152));
#50005=CARTESIAN_POINT('Ctrl Pts',(3.25670393351411,1.30014322216931,3.97934667714784));
#50006=CARTESIAN_POINT('Ctrl Pts',(3.39267401414619,-1.3,4.12301649229108));
#50007=CARTESIAN_POINT('Ctrl Pts',(3.32322027641429,-1.18514270861178,4.17330146776302));
#50008=CARTESIAN_POINT('Ctrl Pts',(3.26328889377514,-1.06847604194512,4.2150265525134));
#50009=CARTESIAN_POINT('Ctrl Pts',(3.1468339558515,-0.794772684000851,4.29164478539433));
#50010=CARTESIAN_POINT('Ctrl Pts',(3.09896529592856,-0.636309800095197,
4.31845031956243));
#50011=CARTESIAN_POINT('Ctrl Pts',(3.02984981618038,-0.319434907277159,
4.34991626061164));
#50012=CARTESIAN_POINT('Ctrl Pts',(3.00954349196179,-0.158333333333332,
4.35269813353154));
#50013=CARTESIAN_POINT('Ctrl Pts',(2.99543061314513,0.158333333333334,4.33782886127835));
#50014=CARTESIAN_POINT('Ctrl Pts',(3.0023925612396,0.319434907277167,4.321019214687));
#50015=CARTESIAN_POINT('Ctrl Pts',(3.04119573834858,0.636309800095206,4.25755156466003));
#50016=CARTESIAN_POINT('Ctrl Pts',(3.0738873794296,0.79477268400084,4.21463797384584));
#50017=CARTESIAN_POINT('Ctrl Pts',(3.15831522453555,1.06847604194511,4.10418628394815));
#50018=CARTESIAN_POINT('Ctrl Pts',(3.2032726433294,1.18514270861178,4.04665525660054));
#50019=CARTESIAN_POINT('Ctrl Pts',(3.25664179513071,1.3,3.97940364582358));
#50020=CARTESIAN_POINT('',(3.5320296967332,-1.2,3.73196507782941));
#50021=CARTESIAN_POINT('Ctrl Pts',(3.5320296967332,-1.2,3.73196507782941));
#50022=CARTESIAN_POINT('Ctrl Pts',(3.53028867930381,-1.21211429492071,3.74748292462223));
#50023=CARTESIAN_POINT('Ctrl Pts',(3.52932228775817,-1.22418007100414,3.76371958287565));
#50024=CARTESIAN_POINT('Ctrl Pts',(3.52404626292729,-1.25801070045455,3.80696300336817));
#50025=CARTESIAN_POINT('Ctrl Pts',(3.52267668202219,-1.26620635932822,3.81736245170488));
#50026=CARTESIAN_POINT('Ctrl Pts',(3.52019027398267,-1.28225243755813,3.83796696657072));
#50027=CARTESIAN_POINT('Ctrl Pts',(3.518816732318,-1.28996988102069,3.84770823323038));
#50028=CARTESIAN_POINT('Ctrl Pts',(3.51736191102066,-1.29864194176201,3.85876656793681));
#50029=CARTESIAN_POINT('Ctrl Pts',(3.51725750255116,-1.2992769549125,3.85957876048008));
#50030=CARTESIAN_POINT('Ctrl Pts',(3.51713261275492,-1.30000000000135,3.86049731482626));
#50031=CARTESIAN_POINT('',(3.42060206186096,-0.653834841369904,3.62201431891782));
#50032=CARTESIAN_POINT('Ctrl Pts',(3.42060206188991,-0.653834841368647,
3.62201431889471));
#50033=CARTESIAN_POINT('Ctrl Pts',(3.43224320734967,-0.717311520958095,
3.63314340931357));
#50034=CARTESIAN_POINT('Ctrl Pts',(3.44190785954811,-0.76493199155208,3.64246729321156));
#50035=CARTESIAN_POINT('Ctrl Pts',(3.47882511314388,-0.949616792156694,
3.67842212036166));
#50036=CARTESIAN_POINT('Ctrl Pts',(3.50217968247802,-1.06344427584388,3.70156424878262));
#50037=CARTESIAN_POINT('Ctrl Pts',(3.5320296967332,-1.2,3.73196507782941));
#50038=CARTESIAN_POINT('',(3.31841464832137,0.653834841531101,3.5270414892343));
#50039=CARTESIAN_POINT('Ctrl Pts',(3.31841464832137,0.653834841531103,3.52704148923431));
#50040=CARTESIAN_POINT('Ctrl Pts',(3.30612895695982,0.575984024643342,3.56675609404422));
#50041=CARTESIAN_POINT('Ctrl Pts',(3.29646327650278,0.493650097853836,3.60055643709482));
#50042=CARTESIAN_POINT('Ctrl Pts',(3.2849183733937,0.338156451488989,3.6498336491464));
#50043=CARTESIAN_POINT('Ctrl Pts',(3.28204499020856,0.265682397105468,3.66749131270142));
#50044=CARTESIAN_POINT('Ctrl Pts',(3.28241779428724,0.129732771186047,3.69186605780633));
#50045=CARTESIAN_POINT('Ctrl Pts',(3.28481237300939,0.0666332289558237,
3.69978892565048));
#50046=CARTESIAN_POINT('Ctrl Pts',(3.29431982878688,-0.0595523952111457,
3.70913249053805));
#50047=CARTESIAN_POINT('Ctrl Pts',(3.30149068665183,-0.122793824757702,
3.7106341531275));
#50048=CARTESIAN_POINT('Ctrl Pts',(3.32176361712298,-0.260152744154284,
3.70625373983926));
#50049=CARTESIAN_POINT('Ctrl Pts',(3.33571246492882,-0.333967683943717,
3.69897587089194));
#50050=CARTESIAN_POINT('Ctrl Pts',(3.37149324193757,-0.491223354642014,
3.6719351756202));
#50051=CARTESIAN_POINT('Ctrl Pts',(3.39449120914342,-0.57435899131098,3.65030401370791));
#50052=CARTESIAN_POINT('Ctrl Pts',(3.42060206187218,-0.653834841386456,
3.62201431897468));
#50053=CARTESIAN_POINT('',(3.37161559917284,1.2,3.57581619513933));
#50054=CARTESIAN_POINT('Ctrl Pts',(3.37161559917284,1.2,3.57581619513933));
#50055=CARTESIAN_POINT('Ctrl Pts',(3.36149720337276,1.12668871690934,3.56640294709369));
#50056=CARTESIAN_POINT('Ctrl Pts',(3.34983325017182,1.03142317896752,3.55563034886084));
#50057=CARTESIAN_POINT('Ctrl Pts',(3.32722135236781,0.796454095927989,3.53499453597592));
#50058=CARTESIAN_POINT('Ctrl Pts',(3.32317714215184,0.739661249859152,3.53134426838176));
#50059=CARTESIAN_POINT('Ctrl Pts',(3.31841464832137,0.653834841531101,3.52704148923431));
#50060=CARTESIAN_POINT('Ctrl Pts',(3.35740616785769,1.30000000000401,3.69995373973539));
#50061=CARTESIAN_POINT('Ctrl Pts',(3.35984187854911,1.28338139784583,3.67926185597637));
#50062=CARTESIAN_POINT('Ctrl Pts',(3.36202234317964,1.27060240530429,3.6636799898001));
#50063=CARTESIAN_POINT('Ctrl Pts',(3.36677577393269,1.23928230445676,3.62508321444296));
#50064=CARTESIAN_POINT('Ctrl Pts',(3.3675752148028,1.23365566836096,3.61811282666168));
#50065=CARTESIAN_POINT('Ctrl Pts',(3.36962079575489,1.21824133508529,3.59889874207068));
#50066=CARTESIAN_POINT('Ctrl Pts',(3.37086515981833,1.20824229626914,3.58637558604191));
#50067=CARTESIAN_POINT('Ctrl Pts',(3.37161559917284,1.2,3.57581619513933));
#50068=CARTESIAN_POINT('Ctrl Pts',(3.39267401414619,-1.3,4.12301649229108));
#50069=CARTESIAN_POINT('Ctrl Pts',(3.32322027641429,-1.18514270861178,4.17330146776302));
#50070=CARTESIAN_POINT('Ctrl Pts',(3.26328889377514,-1.06847604194512,4.2150265525134));
#50071=CARTESIAN_POINT('Ctrl Pts',(3.1468339558515,-0.794772684000851,4.29164478539432));
#50072=CARTESIAN_POINT('Ctrl Pts',(3.09896529592856,-0.636309800095196,
4.31845031956243));
#50073=CARTESIAN_POINT('Ctrl Pts',(3.02984981618038,-0.319434907277159,
4.34991626061163));
#50074=CARTESIAN_POINT('Ctrl Pts',(3.00954349196179,-0.158333333333332,
4.35269813353154));
#50075=CARTESIAN_POINT('Ctrl Pts',(2.99543061314513,0.158333333333334,4.33782886127834));
#50076=CARTESIAN_POINT('Ctrl Pts',(3.0023925612396,0.319434907277167,4.321019214687));
#50077=CARTESIAN_POINT('Ctrl Pts',(3.04119573834857,0.636309800095206,4.25755156466003));
#50078=CARTESIAN_POINT('Ctrl Pts',(3.0738873794296,0.79477268400084,4.21463797384584));
#50079=CARTESIAN_POINT('Ctrl Pts',(3.15831522453555,1.06847604194511,4.10418628394815));
#50080=CARTESIAN_POINT('Ctrl Pts',(3.20327264332939,1.18514270861178,4.04665525660054));
#50081=CARTESIAN_POINT('Ctrl Pts',(3.25664179513071,1.3,3.97940364582358));
#50082=CARTESIAN_POINT('Ctrl Pts',(3.44290446030743,-1.3,4.18129180055357));
#50083=CARTESIAN_POINT('Ctrl Pts',(3.37244803687278,-1.18514270861178,4.23016414502714));
#50084=CARTESIAN_POINT('Ctrl Pts',(3.31185538302694,-1.06847604194512,4.27088003735102));
#50085=CARTESIAN_POINT('Ctrl Pts',(3.19466151211464,-0.794772684000851,
4.34609885764707));
#50086=CARTESIAN_POINT('Ctrl Pts',(3.14738383460685,-0.636309800095196,
4.37331150080897));
#50087=CARTESIAN_POINT('Ctrl Pts',(3.07891484675056,-0.319434907277159,
4.40494093928184));
#50088=CARTESIAN_POINT('Ctrl Pts',(3.05956220283012,-0.158333333333332,
4.40851776232448));
#50089=CARTESIAN_POINT('Ctrl Pts',(3.04571607718934,0.158333333333334,4.39340830443289));
#50090=CARTESIAN_POINT('Ctrl Pts',(3.05198711671704,0.319434907277167,4.37556710698916));
#50091=CARTESIAN_POINT('Ctrl Pts',(3.09069526886232,0.636309800095206,4.31143941648607));
#50092=CARTESIAN_POINT('Ctrl Pts',(3.12304380561888,0.79477268400084,4.26789552624273));
#50093=CARTESIAN_POINT('Ctrl Pts',(3.20878615765139,1.06847604194511,4.15832499982844));
#50094=CARTESIAN_POINT('Ctrl Pts',(3.25467811874699,1.18514270861178,4.10155711050815));
#50095=CARTESIAN_POINT('Ctrl Pts',(3.3093473538106,1.3,4.03545035276417));
#50096=CARTESIAN_POINT('Ctrl Pts',(3.49313490646867,-1.3,4.23956710881606));
#50097=CARTESIAN_POINT('Ctrl Pts',(3.42167579733126,-1.18514270861178,4.28702682229127));
#50098=CARTESIAN_POINT('Ctrl Pts',(3.36042187227873,-1.06847604194512,4.32673352218864));
#50099=CARTESIAN_POINT('Ctrl Pts',(3.24248906837778,-0.794772684000851,
4.40055292989982));
#50100=CARTESIAN_POINT('Ctrl Pts',(3.19580237328514,-0.636309800095196,
4.42817268205552));
#50101=CARTESIAN_POINT('Ctrl Pts',(3.12797987732074,-0.319434907277159,
4.45996561795205));
#50102=CARTESIAN_POINT('Ctrl Pts',(3.10958091369845,-0.158333333333332,
4.46433739111742));
#50103=CARTESIAN_POINT('Ctrl Pts',(3.09600154123355,0.158333333333334,4.44898774758743));
#50104=CARTESIAN_POINT('Ctrl Pts',(3.10158167219449,0.319434907277167,4.43011499929131));
#50105=CARTESIAN_POINT('Ctrl Pts',(3.14019479937607,0.636309800095206,4.36532726831211));
#50106=CARTESIAN_POINT('Ctrl Pts',(3.17220023180817,0.79477268400084,4.32115307863963));
#50107=CARTESIAN_POINT('Ctrl Pts',(3.25925709076723,1.06847604194511,4.21246371570874));
#50108=CARTESIAN_POINT('Ctrl Pts',(3.30608359416459,1.18514270861178,4.15645896441577));
#50109=CARTESIAN_POINT('Ctrl Pts',(3.3620529124905,1.3,4.09149705970477));
#50110=CARTESIAN_POINT('Ctrl Pts',(3.54336535262991,-1.3,4.29784241707855));
#50111=CARTESIAN_POINT('Ctrl Pts',(3.47090355778975,-1.18514270861178,4.34388949955539));
#50112=CARTESIAN_POINT('Ctrl Pts',(3.40898836153053,-1.06847604194512,4.38258700702626));
#50113=CARTESIAN_POINT('Ctrl Pts',(3.29031662464092,-0.794772684000851,
4.45500700215256));
#50114=CARTESIAN_POINT('Ctrl Pts',(3.24422091196343,-0.636309800095196,
4.48303386330206));
#50115=CARTESIAN_POINT('Ctrl Pts',(3.17704490789093,-0.319434907277159,
4.51499029662226));
#50116=CARTESIAN_POINT('Ctrl Pts',(3.15959962456677,-0.158333333333332,
4.52015701991036));
#50117=CARTESIAN_POINT('Ctrl Pts',(3.14628700527777,0.158333333333334,4.50456719074197));
#50118=CARTESIAN_POINT('Ctrl Pts',(3.15117622767193,0.319434907277167,4.48466289159347));
#50119=CARTESIAN_POINT('Ctrl Pts',(3.18969432988981,0.636309800095206,4.41921512013816));
#50120=CARTESIAN_POINT('Ctrl Pts',(3.22135665799746,0.79477268400084,4.37441063103653));
#50121=CARTESIAN_POINT('Ctrl Pts',(3.30972802388306,1.06847604194511,4.26660243158904));
#50122=CARTESIAN_POINT('Ctrl Pts',(3.35748906958219,1.18514270861178,4.21136081832338));
#50123=CARTESIAN_POINT('Ctrl Pts',(3.4147584711704,1.3,4.14754376664537));
#50124=CARTESIAN_POINT('Ctrl Pts',(3.54336535262991,-1.3,4.29784241707854));
#50125=CARTESIAN_POINT('Ctrl Pts',(3.47090355778975,-1.18514270861178,4.34388949955539));
#50126=CARTESIAN_POINT('Ctrl Pts',(3.40898836153053,-1.06847604194512,4.38258700702626));
#50127=CARTESIAN_POINT('Ctrl Pts',(3.29031662464092,-0.794772684000851,
4.45500700215256));
#50128=CARTESIAN_POINT('Ctrl Pts',(3.24422091196343,-0.636309800095197,
4.48303386330206));
#50129=CARTESIAN_POINT('Ctrl Pts',(3.17704490789093,-0.319434907277159,
4.51499029662226));
#50130=CARTESIAN_POINT('Ctrl Pts',(3.15959962456678,-0.158333333333332,
4.52015701991036));
#50131=CARTESIAN_POINT('Ctrl Pts',(3.14628700527777,0.158333333333334,4.50456719074198));
#50132=CARTESIAN_POINT('Ctrl Pts',(3.15117622767193,0.319434907277167,4.48466289159347));
#50133=CARTESIAN_POINT('Ctrl Pts',(3.18969432988981,0.636309800095206,4.41921512013816));
#50134=CARTESIAN_POINT('Ctrl Pts',(3.22135665799746,0.79477268400084,4.37441063103653));
#50135=CARTESIAN_POINT('Ctrl Pts',(3.30972802388306,1.06847604194511,4.26660243158904));
#50136=CARTESIAN_POINT('Ctrl Pts',(3.35748906958219,1.18514270861178,4.21136081832338));
#50137=CARTESIAN_POINT('Ctrl Pts',(3.4147584711704,1.3,4.14754376664537));
#50138=CARTESIAN_POINT('Ctrl Pts',(3.5433653526303,-1.30000000000062,4.2978424170783));
#50139=CARTESIAN_POINT('Ctrl Pts',(3.47090355778997,-1.1851427086122,4.34388949955525));
#50140=CARTESIAN_POINT('Ctrl Pts',(3.40898836153062,-1.06847604194533,4.3825870070262));
#50141=CARTESIAN_POINT('Ctrl Pts',(3.29031662464092,-0.794772684000851,
4.45500700215256));
#50142=CARTESIAN_POINT('Ctrl Pts',(3.24422091196343,-0.636309800095197,
4.48303386330206));
#50143=CARTESIAN_POINT('Ctrl Pts',(3.17704490789093,-0.319434907277159,
4.51499029662226));
#50144=CARTESIAN_POINT('Ctrl Pts',(3.15959962456678,-0.158333333333332,
4.52015701991036));
#50145=CARTESIAN_POINT('Ctrl Pts',(3.14628700527777,0.158333333333334,4.50456719074198));
#50146=CARTESIAN_POINT('Ctrl Pts',(3.15117622767193,0.319434907277167,4.48466289159347));
#50147=CARTESIAN_POINT('Ctrl Pts',(3.18969432988981,0.636309800095206,4.41921512013816));
#50148=CARTESIAN_POINT('Ctrl Pts',(3.22135665799746,0.79477268400084,4.37441063103653));
#50149=CARTESIAN_POINT('Ctrl Pts',(3.30972802388322,1.0684760419456,4.26660243158885));
#50150=CARTESIAN_POINT('Ctrl Pts',(3.35748906958259,1.18514270861274,4.21136081832292));
#50151=CARTESIAN_POINT('Ctrl Pts',(3.41475847117111,1.30000000000142,4.14754376664458));
#50152=CARTESIAN_POINT('Ctrl Pts',(3.5521021815528,-1.30000000000062,4.29733180414384));
#50153=CARTESIAN_POINT('Ctrl Pts',(3.47911206099876,-1.1851427086122,4.34294158094407));
#50154=CARTESIAN_POINT('Ctrl Pts',(3.41699686806362,-1.06847604194533,4.38170451196752));
#50155=CARTESIAN_POINT('Ctrl Pts',(3.29862160460323,-0.794772684000851,
4.45543705367823));
#50156=CARTESIAN_POINT('Ctrl Pts',(3.25416255203503,-0.636309800095197,
4.48672549546171));
#50157=CARTESIAN_POINT('Ctrl Pts',(3.18775359145329,-0.319434907277159,
4.52028525841712));
#50158=CARTESIAN_POINT('Ctrl Pts',(3.17014714932986,-0.158333333333332,
4.52493089070268));
#50159=CARTESIAN_POINT('Ctrl Pts',(3.15675867145257,0.158333333333334,4.50911671228464));
#50160=CARTESIAN_POINT('Ctrl Pts',(3.1616167155693,0.319434907277167,4.48925446133289));
#50161=CARTESIAN_POINT('Ctrl Pts',(3.19945051410824,0.636309800095206,4.42226516940974));
#50162=CARTESIAN_POINT('Ctrl Pts',(3.22998252758132,0.79477268400084,4.37515732362437));
#50163=CARTESIAN_POINT('Ctrl Pts',(3.31797563069851,1.0684760419456,4.26590655670564));
#50164=CARTESIAN_POINT('Ctrl Pts',(3.36577675439426,1.18514270861274,4.2103224238498));
#50165=CARTESIAN_POINT('Ctrl Pts',(3.42329004791205,1.30000000000142,4.14644476699746));
#50166=CARTESIAN_POINT('Ctrl Pts',(3.56358560401321,-1.30000000000062,4.29301250933056));
#50167=CARTESIAN_POINT('Ctrl Pts',(3.49193405704469,-1.1851427086122,4.33603236797316));
#50168=CARTESIAN_POINT('Ctrl Pts',(3.43108544333025,-1.06847604194533,4.37347838998896));
#50169=CARTESIAN_POINT('Ctrl Pts',(3.31546990986285,-0.794772684000853,
4.44710951424628));
#50170=CARTESIAN_POINT('Ctrl Pts',(3.27311970557639,-0.636309800095198,
4.48352197486765));
#50171=CARTESIAN_POINT('Ctrl Pts',(3.20798893278061,-0.319434907277159,
4.51966840504823));
#50172=CARTESIAN_POINT('Ctrl Pts',(3.18945903340722,-0.158333333333333,
4.52466173920179));
#50173=CARTESIAN_POINT('Ctrl Pts',(3.17601420125164,0.158333333333335,4.50870622817952));
#50174=CARTESIAN_POINT('Ctrl Pts',(3.18188067369713,0.319434907277169,4.4884411098495));
#50175=CARTESIAN_POINT('Ctrl Pts',(3.21803362526629,0.636309800095209,4.41840175019651));
#50176=CARTESIAN_POINT('Ctrl Pts',(3.24556941817653,0.794772684000842,4.36540084563633));
#50177=CARTESIAN_POINT('Ctrl Pts',(3.33084078171532,1.0684760419456,4.25628551380435));
#50178=CARTESIAN_POINT('Ctrl Pts',(3.37761225073271,1.18514270861274,4.20223564636569));
#50179=CARTESIAN_POINT('Ctrl Pts',(3.43424437510688,1.30000000000142,4.14136789551703));
#50180=CARTESIAN_POINT('Ctrl Pts',(3.58056423090191,-1.30000000000062,4.28691857619095));
#50181=CARTESIAN_POINT('Ctrl Pts',(3.51184687283633,-1.1851427086122,4.32773477727964));
#50182=CARTESIAN_POINT('Ctrl Pts',(3.45327824423354,-1.06847604194533,4.36372030623571));
#50183=CARTESIAN_POINT('Ctrl Pts',(3.34141859085254,-0.794772684000853,
4.43569425800561));
#50184=CARTESIAN_POINT('Ctrl Pts',(3.29951533377265,-0.636309800095199,
4.47359261889896));
#50185=CARTESIAN_POINT('Ctrl Pts',(3.23525711070835,-0.319434907277161,
4.51064583822628));
#50186=CARTESIAN_POINT('Ctrl Pts',(3.21604851840059,-0.158333333333333,
4.51690915011358));
#50187=CARTESIAN_POINT('Ctrl Pts',(3.20253345039015,0.158333333333335,4.5008959554661));
#50188=CARTESIAN_POINT('Ctrl Pts',(3.20920278516287,0.319434907277168,4.47960149063721));
#50189=CARTESIAN_POINT('Ctrl Pts',(3.24394413212942,0.636309800095208,4.40793019855565));
#50190=CARTESIAN_POINT('Ctrl Pts',(3.26990464364179,0.794772684000844,4.35186295250137));
#50191=CARTESIAN_POINT('Ctrl Pts',(3.35133623487503,1.0684760419456,4.24419300944702));
#50192=CARTESIAN_POINT('Ctrl Pts',(3.39604531243483,1.18514270861274,4.19184388554515));
#50193=CARTESIAN_POINT('Ctrl Pts',(3.4502147490473,1.30000000000142,4.13375196652515));
#50194=CARTESIAN_POINT('Ctrl Pts',(3.59459177663741,-1.30000000000062,4.2817873486779));
#50195=CARTESIAN_POINT('Ctrl Pts',(3.52830294999471,-1.1851427086122,4.32126438957367));
#50196=CARTESIAN_POINT('Ctrl Pts',(3.47142888440619,-1.06847604194533,4.35617370605141));
#50197=CARTESIAN_POINT('Ctrl Pts',(3.36178839673057,-0.794772684000853,
4.42626885352393));
#50198=CARTESIAN_POINT('Ctrl Pts',(3.31852312824454,-0.636309800095198,
4.46326358015796));
#50199=CARTESIAN_POINT('Ctrl Pts',(3.2544599882222,-0.319434907277159,4.50056569204394));
#50200=CARTESIAN_POINT('Ctrl Pts',(3.2355596056058,-0.158333333333333,4.50890029393364));
#50201=CARTESIAN_POINT('Ctrl Pts',(3.22237306826455,0.158333333333335,4.49336746505154));
#50202=CARTESIAN_POINT('Ctrl Pts',(3.22956496962436,0.319434907277169,4.47118278232066));
#50203=CARTESIAN_POINT('Ctrl Pts',(3.2637573887239,0.636309800095208,4.39881377980514));
#50204=CARTESIAN_POINT('Ctrl Pts',(3.28921334598366,0.794772684000841,4.34112021976925));
#50205=CARTESIAN_POINT('Ctrl Pts',(3.36822517239961,1.0684760419456,4.23499892082117));
#50206=CARTESIAN_POINT('Ctrl Pts',(3.41150609894505,1.18514270861274,4.18404600643178));
#50207=CARTESIAN_POINT('Ctrl Pts',(3.46386666005709,1.30000000000143,4.12807615578604));
#50208=CARTESIAN_POINT('Ctrl Pts',(3.61517717129052,-1.30000000000062,4.27590496591519));
#50209=CARTESIAN_POINT('Ctrl Pts',(3.55257603072622,-1.18514270861221,4.31343443912465));
#50210=CARTESIAN_POINT('Ctrl Pts',(3.49822507367094,-1.06847604194533,4.34665935470873));
#50211=CARTESIAN_POINT('Ctrl Pts',(3.39172306435096,-0.794772684000854,
4.413471167091));
#50212=CARTESIAN_POINT('Ctrl Pts',(3.34628580744375,-0.6363098000952,4.44860492003066));
#50213=CARTESIAN_POINT('Ctrl Pts',(3.2817010387109,-0.319434907277161,4.48490921587586));
#50214=CARTESIAN_POINT('Ctrl Pts',(3.26253764798989,-0.158333333333333,
4.49525969638023));
#50215=CARTESIAN_POINT('Ctrl Pts',(3.24859414851813,0.158333333333335,4.47877122196578));
#50216=CARTESIAN_POINT('Ctrl Pts',(3.25488708647475,0.319434907277168,4.45314814577066));
#50217=CARTESIAN_POINT('Ctrl Pts',(3.28888423186795,0.636309800095209,4.38078135733872));
#50218=CARTESIAN_POINT('Ctrl Pts',(3.31693946370155,0.794772684000846,4.32534030247022));
#50219=CARTESIAN_POINT('Ctrl Pts',(3.39307595215939,1.0684760419456,4.22268003510549));
#50220=CARTESIAN_POINT('Ctrl Pts',(3.43399352685011,1.18514270861274,4.17354996578764));
#50221=CARTESIAN_POINT('Ctrl Pts',(3.48287201151301,1.30000000000142,4.11972765295644));
#50222=CARTESIAN_POINT('Ctrl Pts',(3.64437267289813,-1.30000000000062,4.26737943677028));
#50223=CARTESIAN_POINT('Ctrl Pts',(3.58678645305855,-1.18514270861221,4.30208784740518));
#50224=CARTESIAN_POINT('Ctrl Pts',(3.53590367424904,-1.06847604194533,4.33296392790851));
#50225=CARTESIAN_POINT('Ctrl Pts',(3.43384056593238,-0.794772684000854,
4.39544040135096));
#50226=CARTESIAN_POINT('Ctrl Pts',(3.38623061017473,-0.636309800095199,
4.42929823027561));
#50227=CARTESIAN_POINT('Ctrl Pts',(3.32015703785874,-0.31943490727716,4.46322634983303));
#50228=CARTESIAN_POINT('Ctrl Pts',(3.29807995641088,-0.158333333333333,
4.47281316602024));
#50229=CARTESIAN_POINT('Ctrl Pts',(3.28357941163567,0.158333333333335,4.45563258154672));
#50230=CARTESIAN_POINT('Ctrl Pts',(3.29196321705421,0.319434907277169,4.4297810809044));
#50231=CARTESIAN_POINT('Ctrl Pts',(3.32685587542683,0.636309800095209,4.35899172542706));
#50232=CARTESIAN_POINT('Ctrl Pts',(3.35725208631104,0.794772684000844,4.30498495279098));
#50233=CARTESIAN_POINT('Ctrl Pts',(3.42909951824085,1.0684760419456,4.20665305398618));
#50234=CARTESIAN_POINT('Ctrl Pts',(3.46667275064931,1.18514270861274,4.15991547309123));
#50235=CARTESIAN_POINT('Ctrl Pts',(3.51071912439348,1.30000000000142,4.10900454673807));
#50236=CARTESIAN_POINT('Ctrl Pts',(3.6737420698711,-1.30000000000063,4.25912999654594));
#50237=CARTESIAN_POINT('Ctrl Pts',(3.62184231618095,-1.18514270861221,4.29199543832869));
#50238=CARTESIAN_POINT('Ctrl Pts',(3.57489009921585,-1.06847604194534,4.32116332599509));
#50239=CARTESIAN_POINT('Ctrl Pts',(3.47785088485393,-0.794772684000862,
4.38000489181838));
#50240=CARTESIAN_POINT('Ctrl Pts',(3.4274789502663,-0.636309800095207,4.41148412633647));
#50241=CARTESIAN_POINT('Ctrl Pts',(3.36026164960747,-0.319434907277165,
4.44334903460234));
#50242=CARTESIAN_POINT('Ctrl Pts',(3.3362262356368,-0.158333333333335,4.45351730072373));
#50243=CARTESIAN_POINT('Ctrl Pts',(3.32106806187295,0.158333333333337,4.4354738147948));
#50244=CARTESIAN_POINT('Ctrl Pts',(3.33051057601067,0.31943490727717,4.40793856281615));
#50245=CARTESIAN_POINT('Ctrl Pts',(3.3657003458411,0.636309800095214,4.3379423909508));
#50246=CARTESIAN_POINT('Ctrl Pts',(3.3985296934135,0.794772684000856,4.2855346205433));
#50247=CARTESIAN_POINT('Ctrl Pts',(3.46578958001787,1.06847604194561,4.19129389020568));
#50248=CARTESIAN_POINT('Ctrl Pts',(3.49986477922429,1.18514270861275,4.14683941635537));
#50249=CARTESIAN_POINT('Ctrl Pts',(3.53890086495046,1.30000000000143,4.09872378885478));
#50250=CARTESIAN_POINT('Ctrl Pts',(3.71280539583414,-1.30000000000064,4.2499861281838));
#50251=CARTESIAN_POINT('Ctrl Pts',(3.66785373478321,-1.18514270861222,4.27984483444986));
#50252=CARTESIAN_POINT('Ctrl Pts',(3.62579800315821,-1.06847604194535,4.30652049503519));
#50253=CARTESIAN_POINT('Ctrl Pts',(3.53533102618688,-0.794772684000865,
4.36079313514626));
#50254=CARTESIAN_POINT('Ctrl Pts',(3.48270660238735,-0.636309800095211,
4.39125278842555));
#50255=CARTESIAN_POINT('Ctrl Pts',(3.4138032523265,-0.319434907277167,4.42014522530414));
#50256=CARTESIAN_POINT('Ctrl Pts',(3.38550575108799,-0.158333333333335,
4.42845155481182));
#50257=CARTESIAN_POINT('Ctrl Pts',(3.36962435074409,0.158333333333338,4.40938186290787));
#50258=CARTESIAN_POINT('Ctrl Pts',(3.38228202234426,0.319434907277171,4.38226570729989));
#50259=CARTESIAN_POINT('Ctrl Pts',(3.4183440412698,0.636309800095218,4.31400035314523));
#50260=CARTESIAN_POINT('Ctrl Pts',(3.45365007369846,0.794772684000861,4.26283591810305));
#50261=CARTESIAN_POINT('Ctrl Pts',(3.51432257080541,1.06847604194562,4.17291021015486));
#50262=CARTESIAN_POINT('Ctrl Pts',(3.54352829849691,1.18514270861276,4.13086142403693));
#50263=CARTESIAN_POINT('Ctrl Pts',(3.57567687801983,1.30000000000144,4.08568935869604));
#50264=CARTESIAN_POINT('Ctrl Pts',(3.73984169575366,-1.30000000000065,4.24369792702482));
#50265=CARTESIAN_POINT('Ctrl Pts',(3.70009029665069,-1.18514270861223,4.27212598516521));
#50266=CARTESIAN_POINT('Ctrl Pts',(3.66168668719453,-1.06847604194536,4.297501336716));
#50267=CARTESIAN_POINT('Ctrl Pts',(3.57608033044364,-0.794772684000877,
4.34907111220608));
#50268=CARTESIAN_POINT('Ctrl Pts',(3.5213729174716,-0.636309800095216,4.37791105023502));
#50269=CARTESIAN_POINT('Ctrl Pts',(3.45173005884871,-0.319434907277168,
4.40528139275286));
#50270=CARTESIAN_POINT('Ctrl Pts',(3.42160585925665,-0.158333333333336,
4.41391300952443));
#50271=CARTESIAN_POINT('Ctrl Pts',(3.40527212173098,0.158333333333338,4.39418531282052));
#50272=CARTESIAN_POINT('Ctrl Pts',(3.41928392621009,0.319434907277173,4.36612106135141));
#50273=CARTESIAN_POINT('Ctrl Pts',(3.45520527900381,0.636309800095221,4.29796580102719));
#50274=CARTESIAN_POINT('Ctrl Pts',(3.49165555094935,0.794772684000865,4.2467799582519));
#50275=CARTESIAN_POINT('Ctrl Pts',(3.5476576245798,1.06847604194563,4.1597157943461));
#50276=CARTESIAN_POINT('Ctrl Pts',(3.57360474182269,1.18514270861277,4.11952920202481));
#50277=CARTESIAN_POINT('Ctrl Pts',(3.60125775371514,1.30000000000145,4.07684286789193));
#50278=CARTESIAN_POINT('Ctrl Pts',(3.77057621024779,-1.30000000000065,4.2379879271015));
#50279=CARTESIAN_POINT('Ctrl Pts',(3.73643249224655,-1.18514270861224,4.2645649472371));
#50280=CARTESIAN_POINT('Ctrl Pts',(3.70200374773516,-1.06847604194536,4.28836838987465));
#50281=CARTESIAN_POINT('Ctrl Pts',(3.62180799220937,-0.794772684000879,
4.33695158535697));
#50282=CARTESIAN_POINT('Ctrl Pts',(3.56524355524324,-0.636309800095217,
4.3647082579409));
#50283=CARTESIAN_POINT('Ctrl Pts',(3.49478613174268,-0.319434907277169,
4.39037576030595));
#50284=CARTESIAN_POINT('Ctrl Pts',(3.46218066956914,-0.158333333333337,
4.39864161599536));
#50285=CARTESIAN_POINT('Ctrl Pts',(3.44541368781495,0.158333333333339,4.37824223121294));
#50286=CARTESIAN_POINT('Ctrl Pts',(3.46130343379324,0.319434907277174,4.34964902787133));
#50287=CARTESIAN_POINT('Ctrl Pts',(3.49750329847094,0.636309800095223,4.28228271306155));
#50288=CARTESIAN_POINT('Ctrl Pts',(3.5358199278298,0.794772684000867,4.23207070452443));
#50289=CARTESIAN_POINT('Ctrl Pts',(3.58639994847023,1.06847604194563,4.14781392326694));
#50290=CARTESIAN_POINT('Ctrl Pts',(3.60841589789106,1.18514270861277,4.10919379097405));
#50291=CARTESIAN_POINT('Ctrl Pts',(3.63055357997191,1.30000000000145,4.06842516497326));
#50292=CARTESIAN_POINT('Ctrl Pts',(3.79462037248655,-1.30000000000065,4.23248904186284));
#50293=CARTESIAN_POINT('Ctrl Pts',(3.76524282283804,-1.18514270861224,4.25807139147591));
#50294=CARTESIAN_POINT('Ctrl Pts',(3.73418925928466,-1.06847604194536,4.28095407868263));
#50295=CARTESIAN_POINT('Ctrl Pts',(3.65857738782657,-0.794772684000879,
4.32758090357173));
#50296=CARTESIAN_POINT('Ctrl Pts',(3.60040457910877,-0.636309800095218,
4.35423587023406));
#50297=CARTESIAN_POINT('Ctrl Pts',(3.52924851154402,-0.31943490727717,4.3784562060816));
#50298=CARTESIAN_POINT('Ctrl Pts',(3.49447968130587,-0.158333333333337,
4.38614777089569));
#50299=CARTESIAN_POINT('Ctrl Pts',(3.47750044519023,0.158333333333339,4.36542754016807));
#50300=CARTESIAN_POINT('Ctrl Pts',(3.49540412812361,0.319434907277176,4.33723169419255));
#50301=CARTESIAN_POINT('Ctrl Pts',(3.53174232357333,0.636309800095225,4.27036586654147));
#50302=CARTESIAN_POINT('Ctrl Pts',(3.57086134674376,0.794772684000868,4.2198267658269));
#50303=CARTESIAN_POINT('Ctrl Pts',(3.61691542379709,1.06847604194563,4.1375276664807));
#50304=CARTESIAN_POINT('Ctrl Pts',(3.6358059254883,1.18514270861278,4.10020016865909));
#50305=CARTESIAN_POINT('Ctrl Pts',(3.65365182538603,1.30000000000146,4.06116940364073));
#50306=CARTESIAN_POINT('Ctrl Pts',(3.82888894787332,-1.30000000000066,4.22716284196521));
#50307=CARTESIAN_POINT('Ctrl Pts',(3.80593264912406,-1.18514270861225,4.25121972230422));
#50308=CARTESIAN_POINT('Ctrl Pts',(3.77943693726649,-1.06847604194537,4.27273352877866));
#50309=CARTESIAN_POINT('Ctrl Pts',(3.71004979008918,-0.794772684000884,
4.31655971618947));
#50310=CARTESIAN_POINT('Ctrl Pts',(3.64977418033061,-0.636309800095223,
4.34181552019614));
#50311=CARTESIAN_POINT('Ctrl Pts',(3.57776768300628,-0.319434907277173,
4.3641282065308));
#50312=CARTESIAN_POINT('Ctrl Pts',(3.54032260485783,-0.158333333333338,
4.37139895676545));
#50313=CARTESIAN_POINT('Ctrl Pts',(3.52276007360683,0.15833333333334,4.34971852351405));
#50314=CARTESIAN_POINT('Ctrl Pts',(3.54254944263255,0.319434907277177,4.32070154415104));
#50315=CARTESIAN_POINT('Ctrl Pts',(3.57897212495849,0.63630980009523,4.25436139779018));
#50316=CARTESIAN_POINT('Ctrl Pts',(3.62013362735884,0.794772684000875,4.20488495138493));
#50317=CARTESIAN_POINT('Ctrl Pts',(3.6598731686715,1.06847604194564,4.12510137464479));
#50318=CARTESIAN_POINT('Ctrl Pts',(3.67423458806077,1.18514270861279,4.08915849505924));
#50319=CARTESIAN_POINT('Ctrl Pts',(3.68575565190016,1.30000000000147,4.05180808998614));
#50320=CARTESIAN_POINT('Ctrl Pts',(3.86578404397843,-1.30000000000068,4.22059393941875));
#50321=CARTESIAN_POINT('Ctrl Pts',(3.84991983243156,-1.18514270861226,4.24316430874856));
#50322=CARTESIAN_POINT('Ctrl Pts',(3.82853115116094,-1.06847604194538,4.26343685622839));
#50323=CARTESIAN_POINT('Ctrl Pts',(3.76635638840658,-0.794772684000894,
4.30496206826487));
#50324=CARTESIAN_POINT('Ctrl Pts',(3.70443753319059,-0.636309800095231,
4.32981945300887));
#50325=CARTESIAN_POINT('Ctrl Pts',(3.63164779125229,-0.319434907277176,
4.35026891636056));
#50326=CARTESIAN_POINT('Ctrl Pts',(3.59069310496552,-0.15833333333334,4.35601525622158));
#50327=CARTESIAN_POINT('Ctrl Pts',(3.57257645100268,0.158333333333342,4.33336461662472));
#50328=CARTESIAN_POINT('Ctrl Pts',(3.59513035178827,0.319434907277182,4.30460139098978));
#50329=CARTESIAN_POINT('Ctrl Pts',(3.63159652953213,0.636309800095238,4.23876022277154));
#50330=CARTESIAN_POINT('Ctrl Pts',(3.67409806878359,0.794772684000883,4.18905821311206));
#50331=CARTESIAN_POINT('Ctrl Pts',(3.70691792339081,1.06847604194565,4.11193558672093));
#50332=CARTESIAN_POINT('Ctrl Pts',(3.71649547878129,1.1851427086128,4.07772509165791));
#50333=CARTESIAN_POINT('Ctrl Pts',(3.72144409059821,1.30000000000149,4.04268762882171));
#50334=CARTESIAN_POINT('Ctrl Pts',(3.90344079132076,-1.3000000000007,4.21553163691707));
#50335=CARTESIAN_POINT('Ctrl Pts',(3.89499337632463,-1.18514270861227,4.23729060012759));
#50336=CARTESIAN_POINT('Ctrl Pts',(3.87886197620791,-1.0684760419454,4.25664495943046));
#50337=CARTESIAN_POINT('Ctrl Pts',(3.8238436720583,-0.794772684000903,4.29580228518037));
#50338=CARTESIAN_POINT('Ctrl Pts',(3.75921741940078,-0.636309800095236,
4.31824524376349));
#50339=CARTESIAN_POINT('Ctrl Pts',(3.68584534308364,-0.319434907277178,
4.33708131683519));
#50340=CARTESIAN_POINT('Ctrl Pts',(3.64266915085392,-0.158333333333342,
4.34349399923061));
#50341=CARTESIAN_POINT('Ctrl Pts',(3.62423560135531,0.158333333333344,4.32027591932134));
#50342=CARTESIAN_POINT('Ctrl Pts',(3.64873452700158,0.319434907277185,4.29042134256727));
#50343=CARTESIAN_POINT('Ctrl Pts',(3.68505522440327,0.636309800095243,4.22474760639587));
#50344=CARTESIAN_POINT('Ctrl Pts',(3.72945278009421,0.794772684000889,4.17570719036836));
#50345=CARTESIAN_POINT('Ctrl Pts',(3.75501039618448,1.06847604194566,4.10063722479461));
#50346=CARTESIAN_POINT('Ctrl Pts',(3.75949108194612,1.18514270861281,4.06762233632771));
#50347=CARTESIAN_POINT('Ctrl Pts',(3.75738950846692,1.3000000000015,4.0340875658745));
#50348=CARTESIAN_POINT('Ctrl Pts',(3.93147377616527,-1.30000000000071,4.21143726929199));
#50349=CARTESIAN_POINT('Ctrl Pts',(3.92840610329863,-1.18514270861229,4.23227712567801));
#50350=CARTESIAN_POINT('Ctrl Pts',(3.9161925755242,-1.06847604194541,4.2509169327825));
#50351=CARTESIAN_POINT('Ctrl Pts',(3.86684812859849,-0.794772684000911,
4.28889606211575));
#50352=CARTESIAN_POINT('Ctrl Pts',(3.80132675731271,-0.636309800095245,
4.3116279899647));
#50353=CARTESIAN_POINT('Ctrl Pts',(3.72756648851605,-0.319434907277184,
4.32934055793407));
#50354=CARTESIAN_POINT('Ctrl Pts',(3.68172597295035,-0.158333333333344,
4.33440289559836));
#50355=CARTESIAN_POINT('Ctrl Pts',(3.66280311231976,0.158333333333346,4.31025692903056));
#50356=CARTESIAN_POINT('Ctrl Pts',(3.68922480229359,0.319434907277191,4.28037607515652));
#50357=CARTESIAN_POINT('Ctrl Pts',(3.7254508113924,0.636309800095254,4.21484984705132));
#50358=CARTESIAN_POINT('Ctrl Pts',(3.77095851021474,0.794772684000901,4.16582082097937));
#50359=CARTESIAN_POINT('Ctrl Pts',(3.79103094672001,1.06847604194568,4.09219956202305));
#50360=CARTESIAN_POINT('Ctrl Pts',(3.79172296786206,1.18514270861283,4.06011405387389));
#50361=CARTESIAN_POINT('Ctrl Pts',(3.78441839614007,1.30000000000152,4.02781095264135));
#50362=CARTESIAN_POINT('Ctrl Pts',(3.95043864767117,-1.30000000000072,4.20925725898497));
#50363=CARTESIAN_POINT('Ctrl Pts',(3.95104583400332,-1.18514270861229,4.22967037753864));
#50364=CARTESIAN_POINT('Ctrl Pts',(3.94147292066165,-1.06847604194541,4.24790093097384));
#50365=CARTESIAN_POINT('Ctrl Pts',(3.89583950901916,-0.794772684000913,
4.28497499437453));
#50366=CARTESIAN_POINT('Ctrl Pts',(3.8293960455156,-0.636309800095246,4.3072798834843));
#50367=CARTESIAN_POINT('Ctrl Pts',(3.75525310382334,-0.319434907277183,
4.32399157087252));
#50368=CARTESIAN_POINT('Ctrl Pts',(3.70766249886697,-0.158333333333344,
4.32817377141168));
#50369=CARTESIAN_POINT('Ctrl Pts',(3.68856395072071,0.158333333333346,4.30367623710034));
#50370=CARTESIAN_POINT('Ctrl Pts',(3.71646988117644,0.319434907277191,4.27417450090621));
#50371=CARTESIAN_POINT('Ctrl Pts',(3.75290435261723,0.636309800095255,4.20923745755768));
#50372=CARTESIAN_POINT('Ctrl Pts',(3.79949284977158,0.794772684000901,4.16080347453736));
#50373=CARTESIAN_POINT('Ctrl Pts',(3.81577447298326,1.06847604194568,4.08790199358733));
#50374=CARTESIAN_POINT('Ctrl Pts',(3.81376017863368,1.18514270861283,4.05611279774224));
#50375=CARTESIAN_POINT('Ctrl Pts',(3.80268387853975,1.30000000000152,4.0240907558893));
#50376=CARTESIAN_POINT('Ctrl Pts',(3.9599652473406,-1.30000000000072,4.2082758133326));
#50377=CARTESIAN_POINT('Ctrl Pts',(3.96247373018997,-1.1851427086123,4.22861432199262));
#50378=CARTESIAN_POINT('Ctrl Pts',(3.95425317231514,-1.06847604194541,4.24670969468615));
#50379=CARTESIAN_POINT('Ctrl Pts',(3.91047580869722,-0.794772684000916,
4.28333153275462));
#50380=CARTESIAN_POINT('Ctrl Pts',(3.84339133338614,-0.636309800095249,
4.30504330605792));
#50381=CARTESIAN_POINT('Ctrl Pts',(3.76908987076134,-0.319434907277185,
4.32129971957743));
#50382=CARTESIAN_POINT('Ctrl Pts',(3.72087714150373,-0.158333333333345,
4.32552144672611));
#50383=CARTESIAN_POINT('Ctrl Pts',(3.70164568823774,0.158333333333347,4.30076892697359));
#50384=CARTESIAN_POINT('Ctrl Pts',(3.7300511581721,0.319434907277193,4.27100751547332));
#50385=CARTESIAN_POINT('Ctrl Pts',(3.76635241068391,0.636309800095258,4.20593539906908));
#50386=CARTESIAN_POINT('Ctrl Pts',(3.81323744935562,0.794772684000906,4.15736982750891));
#50387=CARTESIAN_POINT('Ctrl Pts',(3.82768797731427,1.06847604194568,4.08494046727559));
#50388=CARTESIAN_POINT('Ctrl Pts',(3.8244333521082,1.18514270861283,4.0534985246992));
#50389=CARTESIAN_POINT('Ctrl Pts',(3.81166900358756,1.30000000000153,4.02196662581921));
#50390=CARTESIAN_POINT('Ctrl Pts',(3.96795660160527,-1.30000000000072,4.20756810680955));
#50391=CARTESIAN_POINT('Ctrl Pts',(3.97209954742154,-1.1851427086123,4.22794665512002));
#50392=CARTESIAN_POINT('Ctrl Pts',(3.96503255625194,-1.06847604194542,4.24598437637122));
#50393=CARTESIAN_POINT('Ctrl Pts',(3.92280919592593,-0.794772684000918,
4.28224734210741));
#50394=CARTESIAN_POINT('Ctrl Pts',(3.85508341517208,-0.63630980009525,4.30325616298306));
#50395=CARTESIAN_POINT('Ctrl Pts',(3.78063937085281,-0.319434907277186,
4.31910554794975));
#50396=CARTESIAN_POINT('Ctrl Pts',(3.73196789195621,-0.158333333333345,
4.32346449797966));
#50397=CARTESIAN_POINT('Ctrl Pts',(3.71265745079205,0.158333333333347,4.29855353410026));
#50398=CARTESIAN_POINT('Ctrl Pts',(3.74149078519913,0.319434907277193,4.26859800790141));
#50399=CARTESIAN_POINT('Ctrl Pts',(3.77767574494274,0.636309800095259,4.20340332602937));
#50400=CARTESIAN_POINT('Ctrl Pts',(3.82478841406823,0.794772684000907,4.1546932186604));
#50401=CARTESIAN_POINT('Ctrl Pts',(3.83767602433403,1.06847604194569,4.08258873535245));
#50402=CARTESIAN_POINT('Ctrl Pts',(3.83336792724296,1.18514270861284,4.05139915651908));
#50403=CARTESIAN_POINT('Ctrl Pts',(3.81917316410977,1.30000000000153,4.02023135794197));
#50404=CARTESIAN_POINT('Ctrl Pts',(3.97348957508239,-1.30000000000072,4.20695237207222));
#50405=CARTESIAN_POINT('Ctrl Pts',(3.97871939465724,-1.1851427086123,4.22724269249007));
#50406=CARTESIAN_POINT('Ctrl Pts',(3.97243672548582,-1.06847604194542,4.24519268843738));
#50407=CARTESIAN_POINT('Ctrl Pts',(3.93132635078679,-0.794772684000919,
4.28125415225274));
#50408=CARTESIAN_POINT('Ctrl Pts',(3.86334433943363,-0.63630980009525,4.30215771288401));
#50409=CARTESIAN_POINT('Ctrl Pts',(3.78882281651341,-0.319434907277186,
4.31776997688037));
#50410=CARTESIAN_POINT('Ctrl Pts',(3.73968442782979,-0.158333333333346,
4.3219397055478));
#50411=CARTESIAN_POINT('Ctrl Pts',(3.7203114251934,0.158333333333348,4.29690084080081));
#50412=CARTESIAN_POINT('Ctrl Pts',(3.74952681995744,0.319434907277194,4.2669676940428));
#50413=CARTESIAN_POINT('Ctrl Pts',(3.78570722405296,0.636309800095259,4.20182892840625));
#50414=CARTESIAN_POINT('Ctrl Pts',(3.8330725899664,0.794772684000907,4.15318429705582));
#50415=CARTESIAN_POINT('Ctrl Pts',(3.84483294238354,1.06847604194569,4.08124764646214));
#50416=CARTESIAN_POINT('Ctrl Pts',(3.83973999715607,1.18514270861284,4.0501494404042));
#50417=CARTESIAN_POINT('Ctrl Pts',(3.82446348590374,1.30000000000153,4.01909173881478));
#50418=CARTESIAN_POINT('Ctrl Pts',(3.9762493453264,-1.30000000000072,4.20663124623647));
#50419=CARTESIAN_POINT('Ctrl Pts',(3.98201445584902,-1.1851427086123,4.22686110722728));
#50420=CARTESIAN_POINT('Ctrl Pts',(3.97612075762044,-1.06847604194542,4.24476089668994));
#50421=CARTESIAN_POINT('Ctrl Pts',(3.93557095513018,-0.794772684000919,
4.28073005983005));
#50422=CARTESIAN_POINT('Ctrl Pts',(3.86748860951078,-0.636309800095251,
4.30163715114415));
#50423=CARTESIAN_POINT('Ctrl Pts',(3.79293299943984,-0.319434907277186,
4.31714054172959));
#50424=CARTESIAN_POINT('Ctrl Pts',(3.74354167200372,-0.158333333333346,
4.32117722132424));
#50425=CARTESIAN_POINT('Ctrl Pts',(3.72413832370986,0.158333333333348,4.29607527301169));
#50426=CARTESIAN_POINT('Ctrl Pts',(3.75355646528761,0.319434907277193,4.26617542786185));
#50427=CARTESIAN_POINT('Ctrl Pts',(3.78974957006065,0.636309800095259,4.20109172067779));
#50428=CARTESIAN_POINT('Ctrl Pts',(3.83726280707289,0.794772684000908,4.15251844840692));
#50429=CARTESIAN_POINT('Ctrl Pts',(3.84845325322281,1.06847604194569,4.08065397088516));
#50430=CARTESIAN_POINT('Ctrl Pts',(3.84295812420178,1.18514270861284,4.04958360320056));
#50431=CARTESIAN_POINT('Ctrl Pts',(3.8271239366683,1.30000000000153,4.01855033730926));
#50432=CARTESIAN_POINT('Ctrl Pts',(3.9778242406541,-1.30000000000072,4.20644374584943));
#50433=CARTESIAN_POINT('Ctrl Pts',(3.98389358920159,-1.1851427086123,4.22663572625));
#50434=CARTESIAN_POINT('Ctrl Pts',(3.97822157650232,-1.06847604194542,4.24450561237847));
#50435=CARTESIAN_POINT('Ctrl Pts',(3.93799319915352,-0.794772684000919,
4.28042412189174));
#50436=CARTESIAN_POINT('Ctrl Pts',(3.869860199366,-0.636309800095251,4.30134643422922));
#50437=CARTESIAN_POINT('Ctrl Pts',(3.79528514884846,-0.319434907277186,
4.31678776143938));
#50438=CARTESIAN_POINT('Ctrl Pts',(3.74574263768344,-0.158333333333346,
4.32073550019824));
#50439=CARTESIAN_POINT('Ctrl Pts',(3.72632180662379,0.158333333333348,4.29559714436483));
#50440=CARTESIAN_POINT('Ctrl Pts',(3.75586079346121,0.319434907277193,4.26572593897617));
#50441=CARTESIAN_POINT('Ctrl Pts',(3.792063913688,0.636309800095259,4.20067880511743));
#50442=CARTESIAN_POINT('Ctrl Pts',(3.83966285207613,0.794772684000908,4.15214815192017));
#50443=CARTESIAN_POINT('Ctrl Pts',(3.85052627487336,1.06847604194569,4.08032247938029));
#50444=CARTESIAN_POINT('Ctrl Pts',(3.84479993025133,1.18514270861284,4.04926556481795));
#50445=CARTESIAN_POINT('Ctrl Pts',(3.82864486780783,1.30000000000153,4.01824240793237));
#50446=CARTESIAN_POINT('Ctrl Pts',(3.99120204265725,-1.30000000000072,4.20483258890774));
#50447=CARTESIAN_POINT('Ctrl Pts',(3.99984014572018,-1.18514270861229,4.22466990353234));
#50448=CARTESIAN_POINT('Ctrl Pts',(3.99604541110411,-1.06847604194541,4.24227305966425));
#50449=CARTESIAN_POINT('Ctrl Pts',(3.95855647278786,-0.794772684000913,
4.27777851876826));
#50450=CARTESIAN_POINT('Ctrl Pts',(3.89003289437388,-0.636309800095247,
4.29891255623496));
#50451=CARTESIAN_POINT('Ctrl Pts',(3.81533376908325,-0.319434907277184,
4.31390722216253));
#50452=CARTESIAN_POINT('Ctrl Pts',(3.76454564771665,-0.158333333333345,
4.31717238002423));
#50453=CARTESIAN_POINT('Ctrl Pts',(3.74497402444854,0.158333333333347,4.29171807813497));
#50454=CARTESIAN_POINT('Ctrl Pts',(3.77547356617403,0.319434907277191,4.26196114100903));
#50455=CARTESIAN_POINT('Ctrl Pts',(3.81176709258041,0.636309800095255,4.19723116161557));
#50456=CARTESIAN_POINT('Ctrl Pts',(3.86017384862098,0.794772684000903,4.14921298844651));
#50457=CARTESIAN_POINT('Ctrl Pts',(3.86826533404931,1.06847604194568,4.07772629020409));
#50458=CARTESIAN_POINT('Ctrl Pts',(3.8605627950136,1.18514270861283,4.0467599012596));
#50459=CARTESIAN_POINT('Ctrl Pts',(3.84165521271933,1.30000000000152,4.01577106619662));
#50460=CARTESIAN_POINT('Ctrl Pts',(4.01714771322487,-1.30000000000067,4.20256713842914));
#50461=CARTESIAN_POINT('Ctrl Pts',(4.0310716095307,-1.18514270861225,4.22252983978109));
#50462=CARTESIAN_POINT('Ctrl Pts',(4.03105144551193,-1.06847604194538,4.24002641390433));
#50463=CARTESIAN_POINT('Ctrl Pts',(3.99879129374527,-0.794772684000891,
4.27474975306124));
#50464=CARTESIAN_POINT('Ctrl Pts',(3.92862047411215,-0.636309800095223,
4.29442790699677));
#50465=CARTESIAN_POINT('Ctrl Pts',(3.85351966006039,-0.31943490727717,4.3081931331775));
#50466=CARTESIAN_POINT('Ctrl Pts',(3.80085515946744,-0.158333333333339,
4.31111896123164));
#50467=CARTESIAN_POINT('Ctrl Pts',(3.78103480159934,0.158333333333341,4.28513383912195));
#50468=CARTESIAN_POINT('Ctrl Pts',(3.81329874038641,0.319434907277181,4.25546850313326));
#50469=CARTESIAN_POINT('Ctrl Pts',(3.84920874621917,0.636309800095233,4.19031008381362));
#50470=CARTESIAN_POINT('Ctrl Pts',(3.89790985350236,0.79477268400087,4.14098496371114));
#50471=CARTESIAN_POINT('Ctrl Pts',(3.90097061500278,1.06847604194564,4.07056556841953));
#50472=CARTESIAN_POINT('Ctrl Pts',(3.8899631846853,1.18514270861279,4.04059238554448));
#50473=CARTESIAN_POINT('Ctrl Pts',(3.8666234338092,1.30000000000148,4.01112796672044));
#50474=CARTESIAN_POINT('Ctrl Pts',(4.04264117857254,-1.30000000000062,4.2003111613257));
#50475=CARTESIAN_POINT('Ctrl Pts',(4.06162921508691,-1.1851427086122,4.22015646238016));
#50476=CARTESIAN_POINT('Ctrl Pts',(4.06526201565741,-1.06847604194533,4.23744989519209));
#50477=CARTESIAN_POINT('Ctrl Pts',(4.03818084487976,-0.794772684000851,
4.27150585838726));
#50478=CARTESIAN_POINT('Ctrl Pts',(3.96674475595548,-0.636309800095197,
4.29046137771269));
#50479=CARTESIAN_POINT('Ctrl Pts',(3.891393048032,-0.319434907277159,4.30329173644276));
#50480=CARTESIAN_POINT('Ctrl Pts',(3.83684904087862,-0.158333333333332,
4.3057824152738));
#50481=CARTESIAN_POINT('Ctrl Pts',(3.81670994245089,0.158333333333334,4.27910948726714));
#50482=CARTESIAN_POINT('Ctrl Pts',(3.85032449139865,0.319434907277167,4.24880110464381));
#50483=CARTESIAN_POINT('Ctrl Pts',(3.88626421184786,0.636309800095206,4.18397173792747));
#50484=CARTESIAN_POINT('Ctrl Pts',(3.93674627805647,0.79477268400084,4.13612524101046));
#50485=CARTESIAN_POINT('Ctrl Pts',(3.93451699612749,1.0684760419456,4.06617305577716));
#50486=CARTESIAN_POINT('Ctrl Pts',(3.91970579175569,1.18514270861274,4.0361853699336));
#50487=CARTESIAN_POINT('Ctrl Pts',(3.89104835655611,1.30000000000142,4.00648970725012));
#50488=CARTESIAN_POINT('Ctrl Pts',(4.0555705152568,-1.30000000000062,4.19956202017773));
#50489=CARTESIAN_POINT('Ctrl Pts',(4.07701141444266,-1.1851427086122,4.21920234377182));
#50490=CARTESIAN_POINT('Ctrl Pts',(4.08243023812087,-1.06847604194533,4.23632262916535));
#50491=CARTESIAN_POINT('Ctrl Pts',(4.05793460522167,-0.794772684000851,
4.27005212095055));
#50492=CARTESIAN_POINT('Ctrl Pts',(3.98606842200265,-0.636309800095197,
4.28905845347054));
#50493=CARTESIAN_POINT('Ctrl Pts',(3.91057658300642,-0.319434907277159,
4.3013835706489));
#50494=CARTESIAN_POINT('Ctrl Pts',(3.85489608531509,-0.158333333333332,
4.30323841603954));
#50495=CARTESIAN_POINT('Ctrl Pts',(3.83456187378799,0.158333333333334,4.27613804652562));
#50496=CARTESIAN_POINT('Ctrl Pts',(3.86905149194718,0.319434907277167,4.24590423237741));
#50497=CARTESIAN_POINT('Ctrl Pts',(3.90486897721866,0.636309800095206,4.18098202838765));
#50498=CARTESIAN_POINT('Ctrl Pts',(3.95570286248539,0.79477268400084,4.13287170138419));
#50499=CARTESIAN_POINT('Ctrl Pts',(3.9509321946351,1.0684760419456,4.06330904848038));
#50500=CARTESIAN_POINT('Ctrl Pts',(3.9344049378379,1.18514270861274,4.03363617972609));
#50501=CARTESIAN_POINT('Ctrl Pts',(3.90341546958523,1.30000000000142,4.00440153710932));
#50502=CARTESIAN_POINT('',(3.81821165418158,1.2,4.04980004382707));
#50503=CARTESIAN_POINT('Ctrl Pts',(3.81821165418158,1.2,4.04980004382707));
#50504=CARTESIAN_POINT('Ctrl Pts',(3.79665007582074,1.21683809744007,4.05012443991704));
#50505=CARTESIAN_POINT('Ctrl Pts',(3.77476695290109,1.23326902184029,4.04951335763234));
#50506=CARTESIAN_POINT('Ctrl Pts',(3.72583131966217,1.27112366990156,4.05009292864458));
#50507=CARTESIAN_POINT('Ctrl Pts',(3.7087188599897,1.28439008066975,4.05044181113104));
#50508=CARTESIAN_POINT('Ctrl Pts',(3.68882920344064,1.30000000000147,4.05118449130007));
#50509=CARTESIAN_POINT('',(3.91593537809339,0.653834841369515,4.17213769893144));
#50510=CARTESIAN_POINT('Ctrl Pts',(3.91593537811947,0.653834841368255,4.172137698905));
#50511=CARTESIAN_POINT('Ctrl Pts',(3.90607125701142,0.717394112008443,4.15938042760931));
#50512=CARTESIAN_POINT('Ctrl Pts',(3.89801101167046,0.763835254644307,4.14905065629189));
#50513=CARTESIAN_POINT('Ctrl Pts',(3.86589991141364,0.949861807330393,4.10830966604798));
#50514=CARTESIAN_POINT('Ctrl Pts',(3.84603384758169,1.05921169948484,4.08352203753005));
#50515=CARTESIAN_POINT('Ctrl Pts',(3.81821165418158,1.2,4.04980004382707));
#50516=CARTESIAN_POINT('',(3.99970644341025,-0.653834841531101,4.28369268311062));
#50517=CARTESIAN_POINT('Ctrl Pts',(3.99970644341025,-0.653834841531099,
4.28369268311062));
#50518=CARTESIAN_POINT('Ctrl Pts',(3.9589217428953,-0.575977434761783,4.29176044842603));
#50519=CARTESIAN_POINT('Ctrl Pts',(3.92429750866062,-0.493637200227944,
4.29784498951834));
#50520=CARTESIAN_POINT('Ctrl Pts',(3.87408537207185,-0.338132850880589,
4.30417904451077));
#50521=CARTESIAN_POINT('Ctrl Pts',(3.85622396295216,-0.265656967148426,
4.30518930057354));
#50522=CARTESIAN_POINT('Ctrl Pts',(3.83202315778412,-0.129714373082854,
4.3022669066107));
#50523=CARTESIAN_POINT('Ctrl Pts',(3.82439467993068,-0.0666240349472378,
4.29905620930053));
#50524=CARTESIAN_POINT('Ctrl Pts',(3.81609664033849,0.0595432864754608,
4.28862474620457));
#50525=CARTESIAN_POINT('Ctrl Pts',(3.81535212458621,0.122776486830215,4.28133711266253));
#50526=CARTESIAN_POINT('Ctrl Pts',(3.82182272809368,0.260125347725809,4.26163282896374));
#50527=CARTESIAN_POINT('Ctrl Pts',(3.83051526302472,0.333941089025903,4.24851874359709));
#50528=CARTESIAN_POINT('Ctrl Pts',(3.86114742698447,0.491208851516981,4.2157592661589));
#50529=CARTESIAN_POINT('Ctrl Pts',(3.88506929628498,0.574353773592851,4.19514993653885));
#50530=CARTESIAN_POINT('Ctrl Pts',(3.91593537803789,0.653834841386106,4.17213769891429));
#50531=CARTESIAN_POINT('',(3.95671284637792,-1.2,4.2256221740828));
#50532=CARTESIAN_POINT('Ctrl Pts',(3.95671284637792,-1.2,4.2256221740828));
#50533=CARTESIAN_POINT('Ctrl Pts',(3.96497406598561,-1.12725969986381,4.23661179129406));
#50534=CARTESIAN_POINT('Ctrl Pts',(3.97450006409837,-1.03199076411307,4.24937898084558));
#50535=CARTESIAN_POINT('Ctrl Pts',(3.99271101970977,-0.796651282571319,
4.27409392899359));
#50536=CARTESIAN_POINT('Ctrl Pts',(3.99591651479174,-0.739855008065579,
4.27849480776061));
#50537=CARTESIAN_POINT('Ctrl Pts',(3.99970644341025,-0.653834841531101,
4.28369268311062));
#50538=CARTESIAN_POINT('Ctrl Pts',(3.83160559603087,-1.30000000000066,4.22656788265504));
#50539=CARTESIAN_POINT('Ctrl Pts',(3.85268755687877,-1.28300366105782,4.22601146009439));
#50540=CARTESIAN_POINT('Ctrl Pts',(3.87378621355538,-1.26602077773898,4.22557624381621));
#50541=CARTESIAN_POINT('Ctrl Pts',(3.92099711546401,-1.2283719856465,4.2253654510458));
#50542=CARTESIAN_POINT('Ctrl Pts',(3.93742292581801,-1.21501533405422,4.22495017710272));
#50543=CARTESIAN_POINT('Ctrl Pts',(3.95671284637792,-1.2,4.2256221740828));
#50544=CARTESIAN_POINT('Origin',(0.,1.25,7.2));
#50545=CARTESIAN_POINT('Origin',(0.,1.2,7.2));
#50546=CARTESIAN_POINT('Origin',(0.,0.92691742076555,7.2));
#50547=CARTESIAN_POINT('Origin',(0.,0.653834841531101,7.2));
#50548=CARTESIAN_POINT('Origin',(0.,0.,7.2));
#50549=CARTESIAN_POINT('Origin',(0.,-0.653834841531101,7.2));
#50550=CARTESIAN_POINT('Origin',(0.,-0.926917420765551,7.2));
#50551=CARTESIAN_POINT('Origin',(0.,-1.2,7.2));
#50552=CARTESIAN_POINT('Origin',(0.,-1.25,7.2));
#50553=CARTESIAN_POINT('Ctrl Pts',(4.24541645780685,-1.30000000000147,4.47512551407364));
#50554=CARTESIAN_POINT('Ctrl Pts',(4.22718893278279,-1.18514270861278,4.43661877696157));
#50555=CARTESIAN_POINT('Ctrl Pts',(4.2040755608183,-1.06847604194562,4.41173100097083));
#50556=CARTESIAN_POINT('Ctrl Pts',(4.13939176392353,-0.794772684000851,
4.38569778430383));
#50557=CARTESIAN_POINT('Ctrl Pts',(4.07792758948489,-0.636309800095197,
4.41917677348839));
#50558=CARTESIAN_POINT('Ctrl Pts',(4.00511469268244,-0.319434907277159,
4.43317916190871));
#50559=CARTESIAN_POINT('Ctrl Pts',(3.96570274858467,-0.158333333333332,
4.45663797562632));
#50560=CARTESIAN_POINT('Ctrl Pts',(3.94621238249364,0.158333333333334,4.42892451651608));
#50561=CARTESIAN_POINT('Ctrl Pts',(3.96518266533146,0.319434907277167,4.3765423951036));
#50562=CARTESIAN_POINT('Ctrl Pts',(4.00023280952294,0.636309800095206,4.3085540603659));
#50563=CARTESIAN_POINT('Ctrl Pts',(4.04051677784848,0.79477268400084,4.2460785382662));
#50564=CARTESIAN_POINT('Ctrl Pts',(4.08016499765644,1.06847604194569,4.23320479314945));
#50565=CARTESIAN_POINT('Ctrl Pts',(4.09477284803596,1.18514270861292,4.24364885985363));
#50566=CARTESIAN_POINT('Ctrl Pts',(4.10682630355144,1.30000000000169,4.27010956050376));
#50567=CARTESIAN_POINT('Ctrl Pts',(4.23960884193275,-1.30000000000147,4.48624205742122));
#50568=CARTESIAN_POINT('Ctrl Pts',(4.22022222294608,-1.18514270861278,4.44981075249239));
#50569=CARTESIAN_POINT('Ctrl Pts',(4.19627915278588,-1.06847604194562,4.42645775550554));
#50570=CARTESIAN_POINT('Ctrl Pts',(4.1304395571954,-0.794772684000851,4.40272116836744));
#50571=CARTESIAN_POINT('Ctrl Pts',(4.06933501810858,-0.636309800095197,
4.43594708574808));
#50572=CARTESIAN_POINT('Ctrl Pts',(3.99657264203947,-0.319434907277159,
4.45009441503412));
#50573=CARTESIAN_POINT('Ctrl Pts',(3.95736019037403,-0.158333333333332,
4.4726979455451));
#50574=CARTESIAN_POINT('Ctrl Pts',(3.9382160520501,0.158333333333334,4.44530213670932));
#50575=CARTESIAN_POINT('Ctrl Pts',(3.95743985353982,0.319434907277165,4.39419736536322));
#50576=CARTESIAN_POINT('Ctrl Pts',(3.992927208102,0.636309800095204,4.32649843143128));
#50577=CARTESIAN_POINT('Ctrl Pts',(4.03302994372149,0.794772684000841,4.26441625119816));
#50578=CARTESIAN_POINT('Ctrl Pts',(4.07378763143588,1.06847604194569,4.24918439864749));
#50579=CARTESIAN_POINT('Ctrl Pts',(4.08911206629833,1.18514270861292,4.25798336192542));
#50580=CARTESIAN_POINT('Ctrl Pts',(4.10211844323279,1.30000000000169,4.28217459305472));
#50581=CARTESIAN_POINT('Ctrl Pts',(4.22767543402957,-1.30000000000147,4.50806909203799));
#50582=CARTESIAN_POINT('Ctrl Pts',(4.20687971577468,-1.18514270861278,4.47678576931432));
#50583=CARTESIAN_POINT('Ctrl Pts',(4.18178147215414,-1.06847604194562,4.45706455756511));
#50584=CARTESIAN_POINT('Ctrl Pts',(4.11385981419251,-0.794772684000849,
4.43821540255297));
#50585=CARTESIAN_POINT('Ctrl Pts',(4.05186292446327,-0.636309800095195,
4.46924991849888));
#50586=CARTESIAN_POINT('Ctrl Pts',(3.97878311668032,-0.319434907277158,
4.48325358835845));
#50587=CARTESIAN_POINT('Ctrl Pts',(3.94060084469131,-0.158333333333332,
4.50477443631655));
#50588=CARTESIAN_POINT('Ctrl Pts',(3.92202810261724,0.158333333333334,4.47791014713781));
#50589=CARTESIAN_POINT('Ctrl Pts',(3.94113066143261,0.319434907277165,4.42877203439641));
#50590=CARTESIAN_POINT('Ctrl Pts',(3.97741179451921,0.636309800095203,4.36158149886323));
#50591=CARTESIAN_POINT('Ctrl Pts',(4.01772483256587,0.794772684000838,4.30084139570613));
#50592=CARTESIAN_POINT('Ctrl Pts',(4.06070253778891,1.06847604194569,4.28086982070652));
#50593=CARTESIAN_POINT('Ctrl Pts',(4.07735759975927,1.18514270861292,4.28626233727591));
#50594=CARTESIAN_POINT('Ctrl Pts',(4.0920642675898,1.30000000000169,4.30569232521228));
#50595=CARTESIAN_POINT('Ctrl Pts',(4.21536537138849,-1.30000000000148,4.53073018436133));
#50596=CARTESIAN_POINT('Ctrl Pts',(4.19171379454328,-1.18514270861278,4.50325264395899));
#50597=CARTESIAN_POINT('Ctrl Pts',(4.16462606938504,-1.06847604194563,4.48641597238428));
#50598=CARTESIAN_POINT('Ctrl Pts',(4.0941098153866,-0.794772684000856,4.47210242857244));
#50599=CARTESIAN_POINT('Ctrl Pts',(4.03346761141163,-0.636309800095198,
4.50326462824729));
#50600=CARTESIAN_POINT('Ctrl Pts',(3.96071008590311,-0.319434907277159,
4.51780391381332));
#50601=CARTESIAN_POINT('Ctrl Pts',(3.92306324501872,-0.158333333333333,
4.53766562651771));
#50602=CARTESIAN_POINT('Ctrl Pts',(3.90488012894027,0.158333333333334,4.51116354761295));
#50603=CARTESIAN_POINT('Ctrl Pts',(3.92354863114418,0.319434907277167,4.46376917352988));
#50604=CARTESIAN_POINT('Ctrl Pts',(3.96088826961113,0.636309800095206,4.39734628374278));
#50605=CARTESIAN_POINT('Ctrl Pts',(4.00230037561805,0.794772684000841,4.33885835941129));
#50606=CARTESIAN_POINT('Ctrl Pts',(4.04766438094242,1.06847604194569,4.31407344698293));
#50607=CARTESIAN_POINT('Ctrl Pts',(4.06555992346895,1.18514270861292,4.31580908798941));
#50608=CARTESIAN_POINT('Ctrl Pts',(4.08171461151912,1.30000000000169,4.33000884022113));
#50609=CARTESIAN_POINT('Ctrl Pts',(4.2085808450133,-1.30000000000148,4.54298047372179));
#50610=CARTESIAN_POINT('Ctrl Pts',(4.18398441102912,-1.18514270861278,4.51825502561577));
#50611=CARTESIAN_POINT('Ctrl Pts',(4.15615495420865,-1.06847604194563,4.50337578034686));
#50612=CARTESIAN_POINT('Ctrl Pts',(4.08439441217396,-0.794772684000854,
4.4917484454727));
#50613=CARTESIAN_POINT('Ctrl Pts',(4.02353939608196,-0.636309800095197,
4.5219690142106));
#50614=CARTESIAN_POINT('Ctrl Pts',(3.9504823383192,-0.319434907277158,4.53630419925681));
#50615=CARTESIAN_POINT('Ctrl Pts',(3.91297617665875,-0.158333333333332,
4.55510202742408));
#50616=CARTESIAN_POINT('Ctrl Pts',(3.89506471881218,0.158333333333334,4.5288581595896));
#50617=CARTESIAN_POINT('Ctrl Pts',(3.91406984960906,0.319434907277167,4.48299886281169));
#50618=CARTESIAN_POINT('Ctrl Pts',(3.95184347519112,0.636309800095206,4.41687220251966));
#50619=CARTESIAN_POINT('Ctrl Pts',(3.99290223892469,0.79477268400084,4.35869637636772));
#50620=CARTESIAN_POINT('Ctrl Pts',(4.03958051780275,1.06847604194569,4.33128930588467));
#50621=CARTESIAN_POINT('Ctrl Pts',(4.05836014539548,1.18514270861292,4.33122248868109));
#50622=CARTESIAN_POINT('Ctrl Pts',(4.07571410325526,1.30000000000169,4.34295235955402));
#50623=CARTESIAN_POINT('Ctrl Pts',(4.20704609201274,-1.30000000000148,4.54567370393651));
#50624=CARTESIAN_POINT('Ctrl Pts',(4.18222266565875,-1.18514270861278,4.52154229127531));
#50625=CARTESIAN_POINT('Ctrl Pts',(4.15421915538174,-1.06847604194563,4.50708863765698));
#50626=CARTESIAN_POINT('Ctrl Pts',(4.08217881452316,-0.794772684000854,
4.49605536577328));
#50627=CARTESIAN_POINT('Ctrl Pts',(4.02130604660735,-0.636309800095197,
4.52609789071604));
#50628=CARTESIAN_POINT('Ctrl Pts',(3.94819597380128,-0.319434907277158,
4.54040245096397));
#50629=CARTESIAN_POINT('Ctrl Pts',(3.91072278825904,-0.158333333333332,
4.55896581463651));
#50630=CARTESIAN_POINT('Ctrl Pts',(3.89286905623125,0.158333333333334,4.53277722495117));
#50631=CARTESIAN_POINT('Ctrl Pts',(3.91192915619521,0.319434907277167,4.48723963284581));
#50632=CARTESIAN_POINT('Ctrl Pts',(3.94981182527956,0.636309800095205,4.4211910906106));
#50633=CARTESIAN_POINT('Ctrl Pts',(3.99083691129868,0.794772684000839,4.36312830796479));
#50634=CARTESIAN_POINT('Ctrl Pts',(4.03781437771274,1.06847604194569,4.33514525823157));
#50635=CARTESIAN_POINT('Ctrl Pts',(4.05678516999129,1.18514270861292,4.33467258717553));
#50636=CARTESIAN_POINT('Ctrl Pts',(4.07439195002436,1.30000000000169,4.34584007041882));
#50637=CARTESIAN_POINT('Ctrl Pts',(4.20433936154425,-1.30000000000147,4.55036564872492));
#50638=CARTESIAN_POINT('Ctrl Pts',(4.17908965394546,-1.18514270861278,4.52724270221372));
#50639=CARTESIAN_POINT('Ctrl Pts',(4.15076399214117,-1.06847604194563,4.51351508747843));
#50640=CARTESIAN_POINT('Ctrl Pts',(4.07821997728699,-0.794772684000854,
4.50350664717199));
#50641=CARTESIAN_POINT('Ctrl Pts',(4.01734734138685,-0.636309800095197,
4.53327162429178));
#50642=CARTESIAN_POINT('Ctrl Pts',(3.94416815826401,-0.319434907277158,
4.54754774675137));
#50643=CARTESIAN_POINT('Ctrl Pts',(3.90677716273327,-0.158333333333332,
4.5657256039145));
#50644=CARTESIAN_POINT('Ctrl Pts',(3.88902354607648,0.158333333333334,4.53963347110758));
#50645=CARTESIAN_POINT('Ctrl Pts',(3.90813695298707,0.319434907277167,4.49461618985308));
#50646=CARTESIAN_POINT('Ctrl Pts',(3.94622059044497,0.636309800095206,4.42871445010138));
#50647=CARTESIAN_POINT('Ctrl Pts',(3.98724992174037,0.794772684000839,4.37091224759782));
#50648=CARTESIAN_POINT('Ctrl Pts',(4.03475881967035,1.06847604194569,4.34192866799764));
#50649=CARTESIAN_POINT('Ctrl Pts',(4.05405600820849,1.18514270861292,4.34073742432239));
#50650=CARTESIAN_POINT('Ctrl Pts',(4.07208554374899,1.30000000000169,4.35090085463336));
#50651=CARTESIAN_POINT('Ctrl Pts',(4.19873267755499,-1.30000000000147,4.55955506317463));
#50652=CARTESIAN_POINT('Ctrl Pts',(4.17231133494234,-1.18514270861278,4.53810655307788));
#50653=CARTESIAN_POINT('Ctrl Pts',(4.14315429278747,-1.06847604194562,4.52563026012046));
#50654=CARTESIAN_POINT('Ctrl Pts',(4.06947567934627,-0.794772684000854,
4.51753514399271));
#50655=CARTESIAN_POINT('Ctrl Pts',(4.00896929670049,-0.636309800095196,
4.54714109090363));
#50656=CARTESIAN_POINT('Ctrl Pts',(3.93598472360625,-0.319434907277158,
4.56171241723378));
#50657=CARTESIAN_POINT('Ctrl Pts',(3.89913110815116,-0.158333333333332,
4.57950311275997));
#50658=CARTESIAN_POINT('Ctrl Pts',(3.88156910106732,0.158333333333334,4.55360146623094));
#50659=CARTESIAN_POINT('Ctrl Pts',(3.90019959247597,0.319434907277167,4.50903198651371));
#50660=CARTESIAN_POINT('Ctrl Pts',(3.93875826929773,0.636309800095205,4.44348753744588));
#50661=CARTESIAN_POINT('Ctrl Pts',(3.98052794628395,0.794772684000839,4.3869195618298));
#50662=CARTESIAN_POINT('Ctrl Pts',(4.02920242948869,1.06847604194569,4.35603670625649));
#50663=CARTESIAN_POINT('Ctrl Pts',(4.04907016256394,1.18514270861292,4.35333003563285));
#50664=CARTESIAN_POINT('Ctrl Pts',(4.06773624850241,1.30000000000169,4.36128473824072));
#50665=CARTESIAN_POINT('Ctrl Pts',(4.19093136889261,-1.30000000000147,4.57290821024422));
#50666=CARTESIAN_POINT('Ctrl Pts',(4.16313154427205,-1.18514270861278,4.55417304171649));
#50667=CARTESIAN_POINT('Ctrl Pts',(4.13293331447271,-1.06847604194562,4.54364432926449));
#50668=CARTESIAN_POINT('Ctrl Pts',(4.05762856673893,-0.79477268400085,4.53827945246952));
#50669=CARTESIAN_POINT('Ctrl Pts',(3.99713251667256,-0.636309800095196,
4.56709991584869));
#50670=CARTESIAN_POINT('Ctrl Pts',(3.92391655521161,-0.319434907277159,
4.58155092634557));
#50671=CARTESIAN_POINT('Ctrl Pts',(3.8873086612351,-0.158333333333332,4.59824238789949));
#50672=CARTESIAN_POINT('Ctrl Pts',(3.87005884656604,0.158333333333334,4.57265595866863));
#50673=CARTESIAN_POINT('Ctrl Pts',(3.88886394919438,0.319434907277168,4.52962487744537));
#50674=CARTESIAN_POINT('Ctrl Pts',(3.92806965388208,0.636309800095206,4.46459034758097));
#50675=CARTESIAN_POINT('Ctrl Pts',(3.96991258425277,0.794772684000838,4.40882972731653));
#50676=CARTESIAN_POINT('Ctrl Pts',(4.02019691836951,1.06847604194569,4.37517252189455));
#50677=CARTESIAN_POINT('Ctrl Pts',(4.04103788752713,1.18514270861292,4.37044670215731));
#50678=CARTESIAN_POINT('Ctrl Pts',(4.0609536008214,1.3000000000017,4.37556401978768));
#50679=CARTESIAN_POINT('Ctrl Pts',(4.18172242510089,-1.30000000000147,4.58911913974467));
#50680=CARTESIAN_POINT('Ctrl Pts',(4.15242075783392,-1.18514270861278,4.57381508171145));
#50681=CARTESIAN_POINT('Ctrl Pts',(4.12106825076219,-1.06847604194562,4.56573360478442));
#50682=CARTESIAN_POINT('Ctrl Pts',(4.04389983716102,-0.794772684000853,
4.56374938361677));
#50683=CARTESIAN_POINT('Ctrl Pts',(3.98329099744489,-0.636309800095197,
4.59148869754783));
#50684=CARTESIAN_POINT('Ctrl Pts',(3.90966015561019,-0.319434907277159,
4.60564290670402));
#50685=CARTESIAN_POINT('Ctrl Pts',(3.87321187328493,-0.158333333333333,
4.6208588406351));
#50686=CARTESIAN_POINT('Ctrl Pts',(3.85621823674316,0.158333333333335,4.59552323915029));
#50687=CARTESIAN_POINT('Ctrl Pts',(3.87517408213286,0.319434907277169,4.55428904304731));
#50688=CARTESIAN_POINT('Ctrl Pts',(3.91520613040173,0.636309800095208,4.48991856855682));
#50689=CARTESIAN_POINT('Ctrl Pts',(3.95728363671029,0.79477268400084,4.43527185629106));
#50690=CARTESIAN_POINT('Ctrl Pts',(4.00964742619141,1.06847604194569,4.39843438524851));
#50691=CARTESIAN_POINT('Ctrl Pts',(4.03171928662598,1.18514270861292,4.39134954378234));
#50692=CARTESIAN_POINT('Ctrl Pts',(4.0531966632983,1.3000000000017,4.39312543710154));
#50693=CARTESIAN_POINT('Ctrl Pts',(4.16880507082559,-1.30000000000147,4.61004578002529));
#50694=CARTESIAN_POINT('Ctrl Pts',(4.13696503396582,-1.18514270861278,4.59874349674725));
#50695=CARTESIAN_POINT('Ctrl Pts',(4.10371802628018,-1.06847604194562,4.59354496739133));
#50696=CARTESIAN_POINT('Ctrl Pts',(4.02366040341415,-0.794772684000849,
4.59563621722879));
#50697=CARTESIAN_POINT('Ctrl Pts',(3.96311397001787,-0.636309800095195,
4.62215678944795));
#50698=CARTESIAN_POINT('Ctrl Pts',(3.88943653601152,-0.319434907277158,
4.63646741409111));
#50699=CARTESIAN_POINT('Ctrl Pts',(3.85397611191893,-0.158333333333332,
4.65056016494006));
#50700=CARTESIAN_POINT('Ctrl Pts',(3.83775883998639,0.158333333333334,4.62604196448687));
#50701=CARTESIAN_POINT('Ctrl Pts',(3.85692018103754,0.319434907277168,4.58720679960908));
#50702=CARTESIAN_POINT('Ctrl Pts',(3.89773084313788,0.636309800095206,4.5234110729215));
#50703=CARTESIAN_POINT('Ctrl Pts',(3.93934209301345,0.794772684000837,4.46948746060851));
#50704=CARTESIAN_POINT('Ctrl Pts',(3.99424963300068,1.06847604194569,4.42815357346725));
#50705=CARTESIAN_POINT('Ctrl Pts',(4.01799642861208,1.18514270861292,4.41793482658671));
#50706=CARTESIAN_POINT('Ctrl Pts',(4.04172258029922,1.30000000000169,4.41538924099766));
#50707=CARTESIAN_POINT('Ctrl Pts',(4.15604312001451,-1.30000000000148,4.63118777585926));
#50708=CARTESIAN_POINT('Ctrl Pts',(4.1216791626411,-1.18514270861278,4.62390281465639));
#50709=CARTESIAN_POINT('Ctrl Pts',(4.08658988648999,-1.06847604194563,4.62164593015606));
#50710=CARTESIAN_POINT('Ctrl Pts',(4.00385100751946,-0.794772684000854,
4.62804793851824));
#50711=CARTESIAN_POINT('Ctrl Pts',(3.94383336495263,-0.636309800095198,
4.65387812734365));
#50712=CARTESIAN_POINT('Ctrl Pts',(3.87003875709904,-0.319434907277159,
4.66826804374778));
#50713=CARTESIAN_POINT('Ctrl Pts',(3.8352167054639,-0.158333333333332,4.68082503182623));
#50714=CARTESIAN_POINT('Ctrl Pts',(3.81911560801986,0.158333333333334,4.65642088163312));
#50715=CARTESIAN_POINT('Ctrl Pts',(3.83758219438638,0.319434907277165,4.6190667059095));
#50716=CARTESIAN_POINT('Ctrl Pts',(3.87909815500753,0.636309800095204,4.5557678817093));
#50717=CARTESIAN_POINT('Ctrl Pts',(3.92109800041264,0.79477268400084,4.50344432729588));
#50718=CARTESIAN_POINT('Ctrl Pts',(3.97910646526714,1.06847604194569,4.45819029969242));
#50719=CARTESIAN_POINT('Ctrl Pts',(4.00473334786608,1.18514270861292,4.44505142981327));
#50720=CARTESIAN_POINT('Ctrl Pts',(4.03087739805383,1.30000000000169,4.43836248177756));
#50721=CARTESIAN_POINT('Ctrl Pts',(4.14297610782065,-1.30000000000148,4.65198541354976));
#50722=CARTESIAN_POINT('Ctrl Pts',(4.10620291401802,-1.18514270861278,4.64887574315513));
#50723=CARTESIAN_POINT('Ctrl Pts',(4.06921033438157,-1.06847604194563,4.64951097508102));
#50724=CARTESIAN_POINT('Ctrl Pts',(3.98324324991729,-0.794772684000855,
4.65962996143306));
#50725=CARTESIAN_POINT('Ctrl Pts',(3.92236141661275,-0.636309800095197,
4.68317313228162));
#50726=CARTESIAN_POINT('Ctrl Pts',(3.84818966802474,-0.319434907277158,
4.69735660219927));
#50727=CARTESIAN_POINT('Ctrl Pts',(3.81474932380975,-0.158333333333332,
4.7092392649545));
#50728=CARTESIAN_POINT('Ctrl Pts',(3.79944294976693,0.158333333333334,4.685720309876));
#50729=CARTESIAN_POINT('Ctrl Pts',(3.81766613437042,0.319434907277167,4.65034974776563));
#50730=CARTESIAN_POINT('Ctrl Pts',(3.86047817775576,0.636309800095206,4.58819660150164));
#50731=CARTESIAN_POINT('Ctrl Pts',(3.9033754919168,0.79477268400084,4.53801363871568));
#50732=CARTESIAN_POINT('Ctrl Pts',(3.96424901291745,1.06847604194569,4.48857485447331));
#50733=CARTESIAN_POINT('Ctrl Pts',(3.9914447211426,1.18514270861292,4.47217394456677));
#50734=CARTESIAN_POINT('Ctrl Pts',(4.01948624593792,1.30000000000169,4.46077234256479));
#50735=CARTESIAN_POINT('Ctrl Pts',(4.1331323253172,-1.30000000000148,4.66758769368662));
#50736=CARTESIAN_POINT('Ctrl Pts',(4.09395398214409,-1.18514270861279,4.66691172061687));
#50737=CARTESIAN_POINT('Ctrl Pts',(4.05529296241795,-1.06847604194563,4.66943087663154));
#50738=CARTESIAN_POINT('Ctrl Pts',(3.96717339339293,-0.794772684000856,
4.68263201834918));
#50739=CARTESIAN_POINT('Ctrl Pts',(3.90768874347606,-0.636309800095198,
4.70680805472394));
#50740=CARTESIAN_POINT('Ctrl Pts',(3.83342912388408,-0.319434907277158,
4.72105415210319));
#50741=CARTESIAN_POINT('Ctrl Pts',(3.79971225905942,-0.158333333333332,
4.73091072894089));
#50742=CARTESIAN_POINT('Ctrl Pts',(3.7842917854581,0.158333333333334,4.70725691348332));
#50743=CARTESIAN_POINT('Ctrl Pts',(3.80243447904911,0.319434907277167,4.67350146574777));
#50744=CARTESIAN_POINT('Ctrl Pts',(3.84559677523662,0.636309800095206,4.61157340969996));
#50745=CARTESIAN_POINT('Ctrl Pts',(3.88795953460117,0.794772684000839,4.56176937733571));
#50746=CARTESIAN_POINT('Ctrl Pts',(3.95131713811071,1.06847604194569,4.50955132448505));
#50747=CARTESIAN_POINT('Ctrl Pts',(3.98020441701305,1.18514270861292,4.49123939964216));
#50748=CARTESIAN_POINT('Ctrl Pts',(4.01055381588896,1.3000000000017,4.47721881016595));
#50749=CARTESIAN_POINT('Ctrl Pts',(4.12254789803899,-1.30000000000148,4.68226017949022));
#50750=CARTESIAN_POINT('Ctrl Pts',(4.08162160927235,-1.18514270861279,4.68481381781336));
#50751=CARTESIAN_POINT('Ctrl Pts',(4.04154893072778,-1.06847604194563,4.6895395859463));
#50752=CARTESIAN_POINT('Ctrl Pts',(3.95094503715524,-0.794772684000856,
4.70547511011371));
#50753=CARTESIAN_POINT('Ctrl Pts',(3.89055896161236,-0.636309800095199,
4.72761125572642));
#50754=CARTESIAN_POINT('Ctrl Pts',(3.81593662704533,-0.319434907277159,
4.7416081001466));
#50755=CARTESIAN_POINT('Ctrl Pts',(3.78316485350851,-0.158333333333333,
4.75086331769791));
#50756=CARTESIAN_POINT('Ctrl Pts',(3.76875250647682,0.158333333333335,4.72836052237739));
#50757=CARTESIAN_POINT('Ctrl Pts',(3.78748461749782,0.319434907277168,4.69699270366139));
#50758=CARTESIAN_POINT('Ctrl Pts',(3.83199090736013,0.636309800095208,4.63636448802781));
#50759=CARTESIAN_POINT('Ctrl Pts',(3.87485052625608,0.794772684000842,4.58796986865435));
#50760=CARTESIAN_POINT('Ctrl Pts',(3.94017354152225,1.06847604194569,4.5324020847612));
#50761=CARTESIAN_POINT('Ctrl Pts',(3.97011512822077,1.18514270861293,4.51150022929617));
#50762=CARTESIAN_POINT('Ctrl Pts',(4.00172238876529,1.3000000000017,4.49374975302422));
#50763=CARTESIAN_POINT('Ctrl Pts',(4.11277136635694,-1.30000000000148,4.69795681868002));
#50764=CARTESIAN_POINT('Ctrl Pts',(4.06972341382925,-1.18514270861279,4.70328683022413));
#50765=CARTESIAN_POINT('Ctrl Pts',(4.02807427462076,-1.06847604194563,4.71001290352959));
#50766=CARTESIAN_POINT('Ctrl Pts',(3.93508796976659,-0.794772684000856,
4.72877666036137));
#50767=CARTESIAN_POINT('Ctrl Pts',(3.87492859356411,-0.636309800095199,
4.75018115722892));
#50768=CARTESIAN_POINT('Ctrl Pts',(3.80006801748132,-0.319434907277159,
4.76406600863756));
#50769=CARTESIAN_POINT('Ctrl Pts',(3.7679477891152,-0.158333333333333,4.77236034151488));
#50770=CARTESIAN_POINT('Ctrl Pts',(3.75340490428175,0.158333333333335,4.7497246578718));
#50771=CARTESIAN_POINT('Ctrl Pts',(3.77112410984858,0.319434907277167,4.71894684138089));
#50772=CARTESIAN_POINT('Ctrl Pts',(3.81607291389888,0.636309800095207,4.65864471171329));
#50773=CARTESIAN_POINT('Ctrl Pts',(3.85938745500052,0.794772684000843,4.61170848166047));
#50774=CARTESIAN_POINT('Ctrl Pts',(3.92757055983804,1.06847604194569,4.55376900664564));
#50775=CARTESIAN_POINT('Ctrl Pts',(3.95924803712011,1.18514270861292,4.53100273925647));
#50776=CARTESIAN_POINT('Ctrl Pts',(3.99308905203305,1.30000000000169,4.51055005634297));
#50777=CARTESIAN_POINT('Ctrl Pts',(4.101856528153,-1.30000000000148,4.7122711116332));
#50778=CARTESIAN_POINT('Ctrl Pts',(4.05659542579174,-1.18514270861279,4.72028838079266));
#50779=CARTESIAN_POINT('Ctrl Pts',(4.01331820273123,-1.06847604194563,4.72896882822391));
#50780=CARTESIAN_POINT('Ctrl Pts',(3.91792231794129,-0.794772684000857,
4.75055447278382));
#50781=CARTESIAN_POINT('Ctrl Pts',(3.85817109968514,-0.6363098000952,4.77144910042573));
#50782=CARTESIAN_POINT('Ctrl Pts',(3.78305855782865,-0.31943490727716,4.78520903031956));
#50783=CARTESIAN_POINT('Ctrl Pts',(3.75116081181364,-0.158333333333333,
4.79202927430626));
#50784=CARTESIAN_POINT('Ctrl Pts',(3.73698370523568,0.158333333333335,4.76983140310512));
#50785=CARTESIAN_POINT('Ctrl Pts',(3.75484510432218,0.319434907277169,4.74098689183149));
#50786=CARTESIAN_POINT('Ctrl Pts',(3.80079318359405,0.636309800095209,4.68165787792731));
#50787=CARTESIAN_POINT('Ctrl Pts',(3.84450273988808,0.794772684000844,4.63609370377142));
#50788=CARTESIAN_POINT('Ctrl Pts',(3.9150270820872,1.0684760419457,4.5752130454864));
#50789=CARTESIAN_POINT('Ctrl Pts',(3.9480581762961,1.18514270861293,4.55016322717855));
#50790=CARTESIAN_POINT('Ctrl Pts',(3.98359299016023,1.3000000000017,4.52641657168378));
#50791=CARTESIAN_POINT('Ctrl Pts',(4.08853169252917,-1.30000000000148,4.73287853781556));
#50792=CARTESIAN_POINT('Ctrl Pts',(4.0404930763511,-1.18514270861278,4.74467643615338));
#50793=CARTESIAN_POINT('Ctrl Pts',(3.99507502628155,-1.06847604194563,4.75599153237031));
#50794=CARTESIAN_POINT('Ctrl Pts',(3.8962042767245,-0.794772684000854,4.78101629872514));
#50795=CARTESIAN_POINT('Ctrl Pts',(3.83610607894287,-0.636309800095199,
4.80017074373498));
#50796=CARTESIAN_POINT('Ctrl Pts',(3.76037354956376,-0.31943490727716,4.8134188260809));
#50797=CARTESIAN_POINT('Ctrl Pts',(3.7292573865684,-0.158333333333333,4.81883751778385));
#50798=CARTESIAN_POINT('Ctrl Pts',(3.71543660868739,0.158333333333335,4.79707715292213));
#50799=CARTESIAN_POINT('Ctrl Pts',(3.73301950557419,0.319434907277167,4.77027969434264));
#50800=CARTESIAN_POINT('Ctrl Pts',(3.78001446475977,0.636309800095207,4.71193002795179));
#50801=CARTESIAN_POINT('Ctrl Pts',(3.82401597092546,0.794772684000843,4.66795096043174));
#50802=CARTESIAN_POINT('Ctrl Pts',(3.89804389930781,1.06847604194569,4.60356088594938));
#50803=CARTESIAN_POINT('Ctrl Pts',(3.93320306627985,1.18514270861293,4.57581440871316));
#50804=CARTESIAN_POINT('Ctrl Pts',(3.97147745303223,1.3000000000017,4.54819353159681));
#50805=CARTESIAN_POINT('Ctrl Pts',(4.07049950580579,-1.30000000000147,4.75697072422884));
#50806=CARTESIAN_POINT('Ctrl Pts',(4.01840400164301,-1.18514270861278,4.77278304834912));
#50807=CARTESIAN_POINT('Ctrl Pts',(3.96997511063938,-1.06847604194562,4.78697882013429));
#50808=CARTESIAN_POINT('Ctrl Pts',(3.86656529415587,-0.794772684000852,
4.81603933352813));
#50809=CARTESIAN_POINT('Ctrl Pts',(3.80682492347781,-0.636309800095199,
4.83392412958058));
#50810=CARTESIAN_POINT('Ctrl Pts',(3.73085791651992,-0.319434907277161,
4.84718915136435));
#50811=CARTESIAN_POINT('Ctrl Pts',(3.70109773297182,-0.158333333333333,
4.85136434419625));
#50812=CARTESIAN_POINT('Ctrl Pts',(3.6877832654516,0.158333333333335,4.83026057386087));
#50813=CARTESIAN_POINT('Ctrl Pts',(3.70441500576368,0.319434907277169,4.80530409557185));
#50814=CARTESIAN_POINT('Ctrl Pts',(3.7528824829836,0.636309800095209,4.74839533465946));
#50815=CARTESIAN_POINT('Ctrl Pts',(3.79805031895221,0.794772684000843,4.70736492996899));
#50816=CARTESIAN_POINT('Ctrl Pts',(3.87672961928093,1.0684760419457,4.63893194866196));
#50817=CARTESIAN_POINT('Ctrl Pts',(3.91455463501092,1.18514270861293,4.60782998161182));
#50818=CARTESIAN_POINT('Ctrl Pts',(3.95614731271391,1.3000000000017,4.57524814942757));
#50819=CARTESIAN_POINT('Ctrl Pts',(4.04694899362265,-1.30000000000148,4.78821554320533));
#50820=CARTESIAN_POINT('Ctrl Pts',(3.98989123950318,-1.18514270861278,4.80967914782147));
#50821=CARTESIAN_POINT('Ctrl Pts',(3.93765915269118,-1.06847604194563,4.82779369545612));
#50822=CARTESIAN_POINT('Ctrl Pts',(3.82814084001427,-0.794772684000855,
4.86190493269116));
#50823=CARTESIAN_POINT('Ctrl Pts',(3.76801298829164,-0.636309800095199,
4.87711372021431));
#50824=CARTESIAN_POINT('Ctrl Pts',(3.69092186684021,-0.319434907277159,
4.88936263478558));
#50825=CARTESIAN_POINT('Ctrl Pts',(3.66216472084552,-0.158333333333333,
4.89086732377457));
#50826=CARTESIAN_POINT('Ctrl Pts',(3.64967259372367,0.158333333333335,4.87083435624963));
#50827=CARTESIAN_POINT('Ctrl Pts',(3.6665543296177,0.319434907277168,4.85020517031915));
#50828=CARTESIAN_POINT('Ctrl Pts',(3.71694367941793,0.636309800095208,4.79530005415465));
#50829=CARTESIAN_POINT('Ctrl Pts',(3.76196030831813,0.794772684000843,4.75620516222934));
#50830=CARTESIAN_POINT('Ctrl Pts',(3.84668046872571,1.06847604194569,4.68246710330853));
#50831=CARTESIAN_POINT('Ctrl Pts',(3.88829024992674,1.18514270861292,4.64732640905243));
#50832=CARTESIAN_POINT('Ctrl Pts',(3.93483759407961,1.30000000000169,4.60896349398276));
#50833=CARTESIAN_POINT('Ctrl Pts',(4.02820350434561,-1.30000000000148,4.81142487691947));
#50834=CARTESIAN_POINT('Ctrl Pts',(3.96711139186663,-1.18514270861278,4.83688576735673));
#50835=CARTESIAN_POINT('Ctrl Pts',(3.91175795323818,-1.06847604194562,4.85769236163318));
#50836=CARTESIAN_POINT('Ctrl Pts',(3.79713792120171,-0.794772684000852,
4.89500740153633));
#50837=CARTESIAN_POINT('Ctrl Pts',(3.73641632741839,-0.636309800095197,
4.90761088418304));
#50838=CARTESIAN_POINT('Ctrl Pts',(3.65836041920465,-0.319434907277159,
4.91891194253082));
#50839=CARTESIAN_POINT('Ctrl Pts',(3.63071576553046,-0.158333333333332,
4.91891982220856));
#50840=CARTESIAN_POINT('Ctrl Pts',(3.6187632745685,0.158333333333334,4.89969039499684));
#50841=CARTESIAN_POINT('Ctrl Pts',(3.63505260823184,0.319434907277167,4.88146360551658));
#50842=CARTESIAN_POINT('Ctrl Pts',(3.68754575873434,0.636309800095206,4.82893523730036));
#50843=CARTESIAN_POINT('Ctrl Pts',(3.73427465223176,0.794772684000839,4.79355980214051));
#50844=CARTESIAN_POINT('Ctrl Pts',(3.82428024392525,1.06847604194569,4.71663817608718));
#50845=CARTESIAN_POINT('Ctrl Pts',(3.8688015764165,1.18514270861292,4.67846105993602));
#50846=CARTESIAN_POINT('Ctrl Pts',(3.91888415579065,1.3000000000017,4.63540334932512));
#50847=CARTESIAN_POINT('Ctrl Pts',(4.01343459618057,-1.30000000000147,4.83038036764169));
#50848=CARTESIAN_POINT('Ctrl Pts',(3.94884952914959,-1.18514270861278,4.85880372193244));
#50849=CARTESIAN_POINT('Ctrl Pts',(3.89078431289497,-1.06847604194562,4.88156901137547));
#50850=CARTESIAN_POINT('Ctrl Pts',(3.77170420702538,-0.794772684000852,
4.92109012247909));
#50851=CARTESIAN_POINT('Ctrl Pts',(3.71031820055588,-0.636309800095198,
4.93138847019967));
#50852=CARTESIAN_POINT('Ctrl Pts',(3.63153238108231,-0.31943490727716,4.94197870250372));
#50853=CARTESIAN_POINT('Ctrl Pts',(3.60521842414231,-0.158333333333333,
4.94125686221945));
#50854=CARTESIAN_POINT('Ctrl Pts',(3.59372977080699,0.158333333333335,4.92270534040838));
#50855=CARTESIAN_POINT('Ctrl Pts',(3.60942918364311,0.319434907277167,4.90630002073989));
#50856=CARTESIAN_POINT('Ctrl Pts',(3.66303294591662,0.636309800095207,4.85502035171266));
#50857=CARTESIAN_POINT('Ctrl Pts',(3.71010928811268,0.794772684000843,4.82148032437692));
#50858=CARTESIAN_POINT('Ctrl Pts',(3.80424215552203,1.06847604194569,4.74179267501399));
#50859=CARTESIAN_POINT('Ctrl Pts',(3.85128182563464,1.18514270861292,4.70132919279899));
#50860=CARTESIAN_POINT('Ctrl Pts',(3.90461453552475,1.30000000000169,4.65489605905986));
#50861=CARTESIAN_POINT('Ctrl Pts',(4.00369573333263,-1.30000000000148,4.84150363158983));
#50862=CARTESIAN_POINT('Ctrl Pts',(3.9369331406498,-1.18514270861279,4.87168016066382));
#50863=CARTESIAN_POINT('Ctrl Pts',(3.87721261864588,-1.06847604194563,4.89563713118229));
#50864=CARTESIAN_POINT('Ctrl Pts',(3.75551485779726,-0.794772684000856,
4.93661410117369));
#50865=CARTESIAN_POINT('Ctrl Pts',(3.69414906548409,-0.636309800095199,
4.9460040068037));
#50866=CARTESIAN_POINT('Ctrl Pts',(3.61477395639173,-0.319434907277159,
4.95594238498443));
#50867=CARTESIAN_POINT('Ctrl Pts',(3.58861414097703,-0.158333333333333,
4.95391588925231));
#50868=CARTESIAN_POINT('Ctrl Pts',(3.57726781607701,0.158333333333335,4.93561307976536));
#50869=CARTESIAN_POINT('Ctrl Pts',(3.59283848397009,0.319434907277167,4.92066300742993));
#50870=CARTESIAN_POINT('Ctrl Pts',(3.64755963040239,0.636309800095207,4.87074166589155));
#50871=CARTESIAN_POINT('Ctrl Pts',(3.69529974618228,0.794772684000843,4.83892431680909));
#50872=CARTESIAN_POINT('Ctrl Pts',(3.79245733604709,1.06847604194569,4.75817145155974));
#50873=CARTESIAN_POINT('Ctrl Pts',(3.84123315554959,1.18514270861292,4.71654348050613));
#50874=CARTESIAN_POINT('Ctrl Pts',(3.89672887394551,1.30000000000169,4.6682424615769));
#50875=CARTESIAN_POINT('Ctrl Pts',(3.99200513405346,-1.30000000000148,4.85500476616359));
#50876=CARTESIAN_POINT('Ctrl Pts',(3.9225817040123,-1.18514270861278,4.88750892319406));
#50877=CARTESIAN_POINT('Ctrl Pts',(3.86073528255479,-1.06847604194562,4.91292369199203));
#50878=CARTESIAN_POINT('Ctrl Pts',(3.73536208225759,-0.794772684000853,
4.95525898707803));
#50879=CARTESIAN_POINT('Ctrl Pts',(3.67258109636451,-0.636309800095199,
4.96158478192644));
#50880=CARTESIAN_POINT('Ctrl Pts',(3.59320814768429,-0.31943490727716,4.97176932104344));
#50881=CARTESIAN_POINT('Ctrl Pts',(3.56997555784675,-0.158333333333333,
4.97186073258582));
#50882=CARTESIAN_POINT('Ctrl Pts',(3.55929280216314,0.158333333333335,4.95453826427217));
#50883=CARTESIAN_POINT('Ctrl Pts',(3.57301586257808,0.319434907277169,4.93908630245288));
#50884=CARTESIAN_POINT('Ctrl Pts',(3.62823902969615,0.636309800095209,4.88962085686202));
#50885=CARTESIAN_POINT('Ctrl Pts',(3.67674433586902,0.794772684000844,4.85984726567696));
#50886=CARTESIAN_POINT('Ctrl Pts',(3.77726226125242,1.06847604194569,4.77718005722317));
#50887=CARTESIAN_POINT('Ctrl Pts',(3.82803455991401,1.18514270861292,4.73385987707036));
#50888=CARTESIAN_POINT('Ctrl Pts',(3.88606867189482,1.30000000000169,4.6830030881825));
#50889=CARTESIAN_POINT('Ctrl Pts',(3.98232662500902,-1.30000000000148,4.86614166803579));
#50890=CARTESIAN_POINT('Ctrl Pts',(3.91032776155344,-1.18514270861278,4.89969217989033));
#50891=CARTESIAN_POINT('Ctrl Pts',(3.8467218346907,-1.06847604194563,4.92603065578664));
#50892=CARTESIAN_POINT('Ctrl Pts',(3.71916878184664,-0.794772684000855,
4.97021655827468));
#50893=CARTESIAN_POINT('Ctrl Pts',(3.65787869457123,-0.636309800095198,
4.97765410576821));
#50894=CARTESIAN_POINT('Ctrl Pts',(3.57897420566855,-0.319434907277158,
4.98853742307923));
#50895=CARTESIAN_POINT('Ctrl Pts',(3.55660206408478,-0.158333333333333,
4.98821755280578));
#50896=CARTESIAN_POINT('Ctrl Pts',(3.54553189689183,0.158333333333334,4.97039301587236));
#50897=CARTESIAN_POINT('Ctrl Pts',(3.55744003194949,0.319434907277168,4.95408557004192));
#50898=CARTESIAN_POINT('Ctrl Pts',(3.61256068172531,0.636309800095207,4.90445630177975));
#50899=CARTESIAN_POINT('Ctrl Pts',(3.661578762114,0.794772684000841,4.87634867301211));
#50900=CARTESIAN_POINT('Ctrl Pts',(3.76462577505384,1.06847604194569,4.79224273511056));
#50901=CARTESIAN_POINT('Ctrl Pts',(3.81696042431411,1.18514270861292,4.74767559603195));
#50902=CARTESIAN_POINT('Ctrl Pts',(3.87702448920102,1.30000000000169,4.69494766196028));
#50903=CARTESIAN_POINT('Ctrl Pts',(3.97017242189175,-1.30000000000147,4.8790119628149));
#50904=CARTESIAN_POINT('Ctrl Pts',(3.89477616791294,-1.18514270861278,4.91405759574364));
#50905=CARTESIAN_POINT('Ctrl Pts',(3.82891412524378,-1.06847604194562,4.9418349037975));
#50906=CARTESIAN_POINT('Ctrl Pts',(3.69878556645952,-0.794772684000853,
4.98921475774886));
#50907=CARTESIAN_POINT('Ctrl Pts',(3.63987925188336,-0.636309800095197,
4.99903821383355));
#50908=CARTESIAN_POINT('Ctrl Pts',(3.56209901489986,-0.319434907277159,
5.01178185899569));
#50909=CARTESIAN_POINT('Ctrl Pts',(3.54101295953038,-0.158333333333333,
5.01109473458552));
#50910=CARTESIAN_POINT('Ctrl Pts',(3.52999041709157,0.158333333333334,4.99337364465456));
#50911=CARTESIAN_POINT('Ctrl Pts',(3.54046028559251,0.319434907277167,4.97729034590911));
#50912=CARTESIAN_POINT('Ctrl Pts',(3.59496068023953,0.636309800095207,4.92651367674735));
#50913=CARTESIAN_POINT('Ctrl Pts',(3.64267540721733,0.79477268400084,4.8974863283316));
#50914=CARTESIAN_POINT('Ctrl Pts',(3.74843407961049,1.06847604194569,4.81028335055866));
#50915=CARTESIAN_POINT('Ctrl Pts',(3.8028541532843,1.18514270861292,4.76398549709187));
#50916=CARTESIAN_POINT('Ctrl Pts',(3.86591529009784,1.3000000000017,4.70913672804752));
#50917=CARTESIAN_POINT('Ctrl Pts',(3.96195840372475,-1.30000000000147,4.88785815300733));
#50918=CARTESIAN_POINT('Ctrl Pts',(3.88343455682606,-1.18514270861278,4.92281726405495));
#50919=CARTESIAN_POINT('Ctrl Pts',(3.81579954549607,-1.06847604194562,4.95110239256332));
#50920=CARTESIAN_POINT('Ctrl Pts',(3.68470452745418,-0.794772684000851,
5.00102846304682));
#50921=CARTESIAN_POINT('Ctrl Pts',(3.63046739270751,-0.636309800095197,
5.01550900850482));
#50922=CARTESIAN_POINT('Ctrl Pts',(3.55506550341723,-0.319434907277159,
5.03079025948107));
#50923=CARTESIAN_POINT('Ctrl Pts',(3.53467416208633,-0.158333333333332,
5.02927276087076));
#50924=CARTESIAN_POINT('Ctrl Pts',(3.52377125184822,0.158333333333334,5.01165271185736));
#50925=CARTESIAN_POINT('Ctrl Pts',(3.53363020048007,0.319434907277167,4.99634356970428));
#50926=CARTESIAN_POINT('Ctrl Pts',(3.58606892910199,0.636309800095206,4.94355543209541));
#50927=CARTESIAN_POINT('Ctrl Pts',(3.62956460835032,0.79477268400084,4.91094102067596));
#50928=CARTESIAN_POINT('Ctrl Pts',(3.73626839073644,1.06847604194569,4.82114406341654));
#50929=CARTESIAN_POINT('Ctrl Pts',(3.79232877910752,1.18514270861292,4.77404740884945));
#50930=CARTESIAN_POINT('Ctrl Pts',(3.85826144221939,1.30000000000169,4.71872387520778));
#50931=CARTESIAN_POINT('Ctrl Pts',(3.95827679071615,-1.30000000000147,4.89563255511119));
#50932=CARTESIAN_POINT('Ctrl Pts',(3.87988594951817,-1.18514270861278,4.93037843917678));
#50933=CARTESIAN_POINT('Ctrl Pts',(3.81258907846072,-1.06847604194562,4.95873129561837));
#50934=CARTESIAN_POINT('Ctrl Pts',(3.68274913399113,-0.794772684000851,
5.00946289323563));
#50935=CARTESIAN_POINT('Ctrl Pts',(3.630353335205,-0.636309800095197,5.0257302081468));
#50936=CARTESIAN_POINT('Ctrl Pts',(3.55620605750903,-0.319434907277159,
5.04213862663278));
#50937=CARTESIAN_POINT('Ctrl Pts',(3.53576509129249,-0.158333333333332,
5.04063778675236));
#50938=CARTESIAN_POINT('Ctrl Pts',(3.52505210827392,0.158333333333334,5.02315921127616));
#50939=CARTESIAN_POINT('Ctrl Pts',(3.53535684314381,0.319434907277167,5.00816436619336));
#50940=CARTESIAN_POINT('Ctrl Pts',(3.58650774416314,0.636309800095206,4.95415127075708));
#50941=CARTESIAN_POINT('Ctrl Pts',(3.62740723167583,0.79477268400084,4.91897241923608));
#50942=CARTESIAN_POINT('Ctrl Pts',(3.73295432340188,1.06847604194569,4.82848789979354));
#50943=CARTESIAN_POINT('Ctrl Pts',(3.78889068790091,1.18514270861292,4.78156123638169));
#50944=CARTESIAN_POINT('Ctrl Pts',(3.85507599179584,1.30000000000169,4.72687530524289));
#50945=CARTESIAN_POINT('Ctrl Pts',(3.95827679071515,-1.3,4.89563255511164));
#50946=CARTESIAN_POINT('Ctrl Pts',(3.8798859495176,-1.18514270861178,4.93037843917702));
#50947=CARTESIAN_POINT('Ctrl Pts',(3.81258907846048,-1.06847604194512,4.95873129561847));
#50948=CARTESIAN_POINT('Ctrl Pts',(3.68274913399113,-0.794772684000851,
5.00946289323563));
#50949=CARTESIAN_POINT('Ctrl Pts',(3.630353335205,-0.636309800095197,5.0257302081468));
#50950=CARTESIAN_POINT('Ctrl Pts',(3.55620605750903,-0.319434907277159,
5.04213862663278));
#50951=CARTESIAN_POINT('Ctrl Pts',(3.53576509129248,-0.158333333333332,
5.04063778675235));
#50952=CARTESIAN_POINT('Ctrl Pts',(3.52505210827392,0.158333333333334,5.02315921127615));
#50953=CARTESIAN_POINT('Ctrl Pts',(3.53535684314381,0.319434907277167,5.00816436619335));
#50954=CARTESIAN_POINT('Ctrl Pts',(3.58650774416314,0.636309800095206,4.95415127075708));
#50955=CARTESIAN_POINT('Ctrl Pts',(3.62740723167583,0.79477268400084,4.91897241923608));
#50956=CARTESIAN_POINT('Ctrl Pts',(3.73295432340165,1.06847604194511,4.82848789979373));
#50957=CARTESIAN_POINT('Ctrl Pts',(3.78889068790036,1.18514270861178,4.78156123638215));
#50958=CARTESIAN_POINT('Ctrl Pts',(3.85507599179487,1.3,4.7268753052437));
#50959=CARTESIAN_POINT('',(4.1759065994826,-1.2,4.54212414277912));
#50960=CARTESIAN_POINT('Ctrl Pts',(4.1759065994826,-1.2,4.54212414277912));
#50961=CARTESIAN_POINT('Ctrl Pts',(4.17214418520691,-1.20924463866719,4.55342996457554));
#50962=CARTESIAN_POINT('Ctrl Pts',(4.16875627541578,-1.21821443520797,4.56484907677502));
#50963=CARTESIAN_POINT('Ctrl Pts',(4.16201532047973,-1.23542515838613,4.58643092051385));
#50964=CARTESIAN_POINT('Ctrl Pts',(4.1614115775334,-1.23665315490756,4.5877694327218));
#50965=CARTESIAN_POINT('Ctrl Pts',(4.15027423165472,-1.26335624147386,4.62034316080045));
#50966=CARTESIAN_POINT('Ctrl Pts',(4.14011740706728,-1.28779025121432,4.65037203783849));
#50967=CARTESIAN_POINT('Ctrl Pts',(4.13470146325513,-1.3,4.66489767272486));
#50968=CARTESIAN_POINT('',(4.08975875278338,-0.653834841367117,4.41138504922928));
#50969=CARTESIAN_POINT('Ctrl Pts',(4.08975875281708,-0.653834841365838,
4.4113850492124));
#50970=CARTESIAN_POINT('Ctrl Pts',(4.09883612367009,-0.717342388655811,
4.42469784339655));
#50971=CARTESIAN_POINT('Ctrl Pts',(4.10644894485254,-0.765483511502256,
4.43597370734929));
#50972=CARTESIAN_POINT('Ctrl Pts',(4.13503526267317,-0.949592603242909,
4.47874631007404));
#50973=CARTESIAN_POINT('Ctrl Pts',(4.15182328757237,-1.05626431331092,4.50428578367362));
#50974=CARTESIAN_POINT('Ctrl Pts',(4.1759065994826,-1.2,4.54212414277912));
#50975=CARTESIAN_POINT('',(4.00955034077224,0.653834841531101,4.29724164546664));
#50976=CARTESIAN_POINT('Ctrl Pts',(4.00955034077224,0.653834841531101,4.29724164546664));
#50977=CARTESIAN_POINT('Ctrl Pts',(3.98927872982994,0.575994542894782,4.33352914862505));
#50978=CARTESIAN_POINT('Ctrl Pts',(3.97279875699981,0.493637872429252,4.36460185351157));
#50979=CARTESIAN_POINT('Ctrl Pts',(3.95126345212767,0.338127837060752,4.41040803616251));
#50980=CARTESIAN_POINT('Ctrl Pts',(3.94478094307397,0.265653872177931,4.42707925918047));
#50981=CARTESIAN_POINT('Ctrl Pts',(3.94007563669224,0.129712215371197,4.45098897808368));
#50982=CARTESIAN_POINT('Ctrl Pts',(3.94076895770888,0.0666227083564181,
4.45923189482429));
#50983=CARTESIAN_POINT('Ctrl Pts',(3.94812442420765,-0.0595436117189309,
4.47034568766396));
#50984=CARTESIAN_POINT('Ctrl Pts',(3.95482572321592,-0.122773201281119,
4.47330664288229));
#50985=CARTESIAN_POINT('Ctrl Pts',(3.97556620162042,-0.260125628448797,
4.47324337421401));
#50986=CARTESIAN_POINT('Ctrl Pts',(3.99072482510553,-0.333944860941934,
4.46902771026615));
#50987=CARTESIAN_POINT('Ctrl Pts',(4.03134314078074,-0.491205254633584,
4.45001447015766));
#50988=CARTESIAN_POINT('Ctrl Pts',(4.05833207591073,-0.574347106328157,
4.4336311917751));
#50989=CARTESIAN_POINT('Ctrl Pts',(4.08975875278252,-0.653834841383954,
4.41138504928823));
#50990=CARTESIAN_POINT('',(4.05150253593681,1.2,4.35608945265544));
#50991=CARTESIAN_POINT('Ctrl Pts',(4.05150253593681,1.2,4.35608945265544));
#50992=CARTESIAN_POINT('Ctrl Pts',(4.04575710139426,1.14657618383835,4.34790437009688));
#50993=CARTESIAN_POINT('Ctrl Pts',(4.03662031939464,1.06003819843532,4.3349237974889));
#50994=CARTESIAN_POINT('Ctrl Pts',(4.0161950566583,0.792700141885613,4.3064105960449));
#50995=CARTESIAN_POINT('Ctrl Pts',(4.01325274808858,0.738260770271576,4.30235574271615));
#50996=CARTESIAN_POINT('Ctrl Pts',(4.00955034077224,0.653834841531101,4.29724164546664));
#50997=CARTESIAN_POINT('Ctrl Pts',(4.01191463394249,1.3,4.47474020138297));
#50998=CARTESIAN_POINT('Ctrl Pts',(4.01997786089997,1.28107343755638,4.45292765725262));
#50999=CARTESIAN_POINT('Ctrl Pts',(4.02551045807113,1.26655089503634,4.43531292137856));
#51000=CARTESIAN_POINT('Ctrl Pts',(4.03894397720598,1.23311712142409,4.39592764313121));
#51001=CARTESIAN_POINT('Ctrl Pts',(4.04577421378828,1.21590150548676,4.37560629030699));
#51002=CARTESIAN_POINT('Ctrl Pts',(4.05150253593681,1.2,4.35608945265544));
#51003=CARTESIAN_POINT('Ctrl Pts',(3.95827679071515,-1.3,4.89563255511164));
#51004=CARTESIAN_POINT('Ctrl Pts',(3.8798859495176,-1.18514270861178,4.93037843917702));
#51005=CARTESIAN_POINT('Ctrl Pts',(3.81258907846048,-1.06847604194512,4.95873129561847));
#51006=CARTESIAN_POINT('Ctrl Pts',(3.68274913399113,-0.794772684000851,
5.00946289323563));
#51007=CARTESIAN_POINT('Ctrl Pts',(3.630353335205,-0.636309800095197,5.0257302081468));
#51008=CARTESIAN_POINT('Ctrl Pts',(3.55620605750904,-0.319434907277159,
5.04213862663278));
#51009=CARTESIAN_POINT('Ctrl Pts',(3.53576509129249,-0.158333333333332,
5.04063778675235));
#51010=CARTESIAN_POINT('Ctrl Pts',(3.52505210827392,0.158333333333334,5.02315921127615));
#51011=CARTESIAN_POINT('Ctrl Pts',(3.53535684314381,0.319434907277167,5.00816436619336));
#51012=CARTESIAN_POINT('Ctrl Pts',(3.58650774416314,0.636309800095206,4.95415127075708));
#51013=CARTESIAN_POINT('Ctrl Pts',(3.62740723167583,0.79477268400084,4.91897241923608));
#51014=CARTESIAN_POINT('Ctrl Pts',(3.73295432340165,1.06847604194511,4.82848789979373));
#51015=CARTESIAN_POINT('Ctrl Pts',(3.78889068790036,1.18514270861178,4.78156123638215));
#51016=CARTESIAN_POINT('Ctrl Pts',(3.85507599179487,1.3,4.7268753052437));
#51017=CARTESIAN_POINT('Ctrl Pts',(3.99529346323777,-1.3,4.96307790506253));
#51018=CARTESIAN_POINT('Ctrl Pts',(3.91621554992515,-1.18514270861178,4.99623355742632));
#51019=CARTESIAN_POINT('Ctrl Pts',(3.84848168092754,-1.06847604194512,5.02346178870243));
#51020=CARTESIAN_POINT('Ctrl Pts',(3.7182099051649,-0.794772684000851,5.07267092145019));
#51021=CARTESIAN_POINT('Ctrl Pts',(3.66630753169098,-0.636309800095197,
5.08945932120005));
#51022=CARTESIAN_POINT('Ctrl Pts',(3.59275862546217,-0.319434907277159,
5.10616207752106));
#51023=CARTESIAN_POINT('Ctrl Pts',(3.57308521991698,-0.158333333333332,
5.10563709747918));
#51024=CARTESIAN_POINT('Ctrl Pts',(3.56268309827958,0.158333333333334,5.08797904610088));
#51025=CARTESIAN_POINT('Ctrl Pts',(3.57252649407444,0.319434907277167,5.07183154405847));
#51026=CARTESIAN_POINT('Ctrl Pts',(3.62372167678492,0.636309800095206,5.01715307481322));
#51027=CARTESIAN_POINT('Ctrl Pts',(3.66441660424588,0.79477268400084,4.98128636201763));
#51028=CARTESIAN_POINT('Ctrl Pts',(3.77106627357833,1.06847604194511,4.89193705188011));
#51029=CARTESIAN_POINT('Ctrl Pts',(3.8277580930697,1.18514270861178,4.84595115236908));
#51030=CARTESIAN_POINT('Ctrl Pts',(3.89497704195816,1.3,4.7926553589873));
#51031=CARTESIAN_POINT('Ctrl Pts',(4.0323101357604,-1.3,5.03052325501342));
#51032=CARTESIAN_POINT('Ctrl Pts',(3.95254515033271,-1.18514270861178,5.06208867567562));
#51033=CARTESIAN_POINT('Ctrl Pts',(3.88437428339459,-1.06847604194512,5.08819228178639));
#51034=CARTESIAN_POINT('Ctrl Pts',(3.75367067633867,-0.794772684000851,
5.13587894966475));
#51035=CARTESIAN_POINT('Ctrl Pts',(3.70226172817696,-0.636309800095197,
5.15318843425331));
#51036=CARTESIAN_POINT('Ctrl Pts',(3.62931119341529,-0.319434907277159,
5.17018552840935));
#51037=CARTESIAN_POINT('Ctrl Pts',(3.61040534854147,-0.158333333333332,
5.170636408206));
#51038=CARTESIAN_POINT('Ctrl Pts',(3.60031408828524,0.158333333333334,5.1527988809256));
#51039=CARTESIAN_POINT('Ctrl Pts',(3.60969614500508,0.319434907277167,5.13549872192358));
#51040=CARTESIAN_POINT('Ctrl Pts',(3.6609356094067,0.636309800095206,5.08015487886937));
#51041=CARTESIAN_POINT('Ctrl Pts',(3.70142597681592,0.79477268400084,5.04360030479918));
#51042=CARTESIAN_POINT('Ctrl Pts',(3.80917822375501,1.06847604194511,4.9553862039665));
#51043=CARTESIAN_POINT('Ctrl Pts',(3.86662549823905,1.18514270861178,4.91034106835601));
#51044=CARTESIAN_POINT('Ctrl Pts',(3.93487809212145,1.3,4.85843541273091));
#51045=CARTESIAN_POINT('Ctrl Pts',(4.06932680828302,-1.3,5.09796860496431));
#51046=CARTESIAN_POINT('Ctrl Pts',(3.98887475074027,-1.18514270861178,5.12794379392492));
#51047=CARTESIAN_POINT('Ctrl Pts',(3.92026688586164,-1.06847604194512,5.15292277487036));
#51048=CARTESIAN_POINT('Ctrl Pts',(3.78913144751244,-0.794772684000851,
5.19908697787931));
#51049=CARTESIAN_POINT('Ctrl Pts',(3.73821592466294,-0.636309800095197,
5.21691754730656));
#51050=CARTESIAN_POINT('Ctrl Pts',(3.66586376136842,-0.319434907277159,
5.23420897929763));
#51051=CARTESIAN_POINT('Ctrl Pts',(3.64772547716597,-0.158333333333332,
5.23563571893282));
#51052=CARTESIAN_POINT('Ctrl Pts',(3.6379450782909,0.158333333333334,5.21761871575033));
#51053=CARTESIAN_POINT('Ctrl Pts',(3.64686579593571,0.319434907277167,5.19916589978869));
#51054=CARTESIAN_POINT('Ctrl Pts',(3.69814954202848,0.636309800095206,5.14315668292551));
#51055=CARTESIAN_POINT('Ctrl Pts',(3.73843534938597,0.79477268400084,5.10591424758073));
#51056=CARTESIAN_POINT('Ctrl Pts',(3.84729017393168,1.06847604194511,5.01883535605289));
#51057=CARTESIAN_POINT('Ctrl Pts',(3.90549290340839,1.18514270861178,4.97473098434294));
#51058=CARTESIAN_POINT('Ctrl Pts',(3.97477914228474,1.3,4.92421546647452));
#51059=CARTESIAN_POINT('Ctrl Pts',(4.06932680828302,-1.3,5.09796860496431));
#51060=CARTESIAN_POINT('Ctrl Pts',(3.98887475074027,-1.18514270861178,5.12794379392492));
#51061=CARTESIAN_POINT('Ctrl Pts',(3.92026688586165,-1.06847604194512,5.15292277487036));
#51062=CARTESIAN_POINT('Ctrl Pts',(3.78913144751244,-0.794772684000851,
5.19908697787931));
#51063=CARTESIAN_POINT('Ctrl Pts',(3.73821592466294,-0.636309800095197,
5.21691754730656));
#51064=CARTESIAN_POINT('Ctrl Pts',(3.66586376136842,-0.319434907277159,
5.23420897929763));
#51065=CARTESIAN_POINT('Ctrl Pts',(3.64772547716596,-0.158333333333332,
5.23563571893282));
#51066=CARTESIAN_POINT('Ctrl Pts',(3.6379450782909,0.158333333333334,5.21761871575033));
#51067=CARTESIAN_POINT('Ctrl Pts',(3.64686579593571,0.319434907277167,5.19916589978868));
#51068=CARTESIAN_POINT('Ctrl Pts',(3.69814954202848,0.636309800095206,5.14315668292551));
#51069=CARTESIAN_POINT('Ctrl Pts',(3.73843534938597,0.79477268400084,5.10591424758073));
#51070=CARTESIAN_POINT('Ctrl Pts',(3.84729017393168,1.06847604194511,5.01883535605289));
#51071=CARTESIAN_POINT('Ctrl Pts',(3.90549290340839,1.18514270861178,4.97473098434294));
#51072=CARTESIAN_POINT('Ctrl Pts',(3.97477914228473,1.3,4.92421546647452));
#51073=CARTESIAN_POINT('Ctrl Pts',(4.0693268082831,-1.30000000000011,5.09796860496428));
#51074=CARTESIAN_POINT('Ctrl Pts',(3.98887475074031,-1.18514270861186,5.1279437939249));
#51075=CARTESIAN_POINT('Ctrl Pts',(3.92026688586166,-1.06847604194515,5.15292277487035));
#51076=CARTESIAN_POINT('Ctrl Pts',(3.78913144751244,-0.794772684000851,
5.19908697787931));
#51077=CARTESIAN_POINT('Ctrl Pts',(3.73821592466294,-0.636309800095197,
5.21691754730656));
#51078=CARTESIAN_POINT('Ctrl Pts',(3.66586376136842,-0.319434907277159,
5.23420897929763));
#51079=CARTESIAN_POINT('Ctrl Pts',(3.64772547716596,-0.158333333333332,
5.23563571893282));
#51080=CARTESIAN_POINT('Ctrl Pts',(3.6379450782909,0.158333333333334,5.21761871575033));
#51081=CARTESIAN_POINT('Ctrl Pts',(3.64686579593571,0.319434907277167,5.19916589978868));
#51082=CARTESIAN_POINT('Ctrl Pts',(3.69814954202848,0.636309800095206,5.14315668292551));
#51083=CARTESIAN_POINT('Ctrl Pts',(3.73843534938597,0.79477268400084,5.10591424758073));
#51084=CARTESIAN_POINT('Ctrl Pts',(3.84729017393193,1.06847604194573,5.01883535605269));
#51085=CARTESIAN_POINT('Ctrl Pts',(3.905492903409,1.18514270861299,4.97473098434248));
#51086=CARTESIAN_POINT('Ctrl Pts',(3.97477914228582,1.3000000000018,4.92421546647373));
#51087=CARTESIAN_POINT('Ctrl Pts',(4.07797887893023,-1.30000000000011,5.09928563902119));
#51088=CARTESIAN_POINT('Ctrl Pts',(3.99710096182082,-1.18514270861186,5.12872323339091));
#51089=CARTESIAN_POINT('Ctrl Pts',(3.92828386835217,-1.06847604194515,5.15372462658026));
#51090=CARTESIAN_POINT('Ctrl Pts',(3.79716553099686,-0.794772684000851,
5.20123433417352));
#51091=CARTESIAN_POINT('Ctrl Pts',(3.74717278256209,-0.636309800095197,
5.2225954916431));
#51092=CARTESIAN_POINT('Ctrl Pts',(3.67523755004235,-0.319434907277159,
5.24161469397914));
#51093=CARTESIAN_POINT('Ctrl Pts',(3.65704996965851,-0.158333333333332,
5.24249822290199));
#51094=CARTESIAN_POINT('Ctrl Pts',(3.64724201471915,0.158333333333334,5.22424600115186));
#51095=CARTESIAN_POINT('Ctrl Pts',(3.65612349309497,0.319434907277167,5.2058278322046));
#51096=CARTESIAN_POINT('Ctrl Pts',(3.7070583893129,0.636309800095206,5.1481685060594));
#51097=CARTESIAN_POINT('Ctrl Pts',(3.7467174769052,0.79477268400084,5.10843804227397));
#51098=CARTESIAN_POINT('Ctrl Pts',(3.85550223127368,1.06847604194573,5.01986946158344));
#51099=CARTESIAN_POINT('Ctrl Pts',(3.91381537677383,1.18514270861299,4.97543838784214));
#51100=CARTESIAN_POINT('Ctrl Pts',(3.98335277848031,1.3000000000018,4.92491429715123));
#51101=CARTESIAN_POINT('Ctrl Pts',(4.09010264837502,-1.30000000000011,5.0974281824879));
#51102=CARTESIAN_POINT('Ctrl Pts',(4.01107193700271,-1.18514270861186,5.12460716309181));
#51103=CARTESIAN_POINT('Ctrl Pts',(3.94376817464231,-1.06847604194516,5.14858398387072));
#51104=CARTESIAN_POINT('Ctrl Pts',(3.81537461770386,-0.794772684000852,
5.19657760663093));
#51105=CARTESIAN_POINT('Ctrl Pts',(3.76638838416209,-0.636309800095198,
5.22341425512017));
#51106=CARTESIAN_POINT('Ctrl Pts',(3.69516960528746,-0.319434907277159,
5.24523969656485));
#51107=CARTESIAN_POINT('Ctrl Pts',(3.67600601086261,-0.158333333333333,
5.24626900813328));
#51108=CARTESIAN_POINT('Ctrl Pts',(3.66616720149152,0.158333333333335,5.22785505234343));
#51109=CARTESIAN_POINT('Ctrl Pts',(3.67610760976984,0.319434907277169,5.20922731970925));
#51110=CARTESIAN_POINT('Ctrl Pts',(3.72603146219124,0.636309800095208,5.14823279065688));
#51111=CARTESIAN_POINT('Ctrl Pts',(3.76399726034961,0.794772684000841,5.10214216240938));
#51112=CARTESIAN_POINT('Ctrl Pts',(3.87009225143811,1.06847604194573,5.01314284055789));
#51113=CARTESIAN_POINT('Ctrl Pts',(3.92707741387766,1.18514270861299,4.96999514155808));
#51114=CARTESIAN_POINT('Ctrl Pts',(3.9951231483213,1.3000000000018,4.92222425223821));
#51115=CARTESIAN_POINT('Ctrl Pts',(4.10794777737404,-1.30000000000012,5.09490870018085));
#51116=CARTESIAN_POINT('Ctrl Pts',(4.03225269306678,-1.18514270861186,5.12055373952318));
#51117=CARTESIAN_POINT('Ctrl Pts',(3.9674904650733,-1.06847604194516,5.14359000792102));
#51118=CARTESIAN_POINT('Ctrl Pts',(3.84313384796426,-0.794772684000854,
5.19078161354514));
#51119=CARTESIAN_POINT('Ctrl Pts',(3.79428998871027,-0.636309800095197,
5.21920069851044));
#51120=CARTESIAN_POINT('Ctrl Pts',(3.72375313872692,-0.319434907277158,
5.24213353045454));
#51121=CARTESIAN_POINT('Ctrl Pts',(3.70367705257536,-0.158333333333332,
5.24429872357439));
#51122=CARTESIAN_POINT('Ctrl Pts',(3.69377031090259,0.158333333333334,5.22578741725238));
#51123=CARTESIAN_POINT('Ctrl Pts',(3.70466740404922,0.319434907277167,5.20622006587942));
#51124=CARTESIAN_POINT('Ctrl Pts',(3.75354256291749,0.636309800095206,5.14332178106065));
#51125=CARTESIAN_POINT('Ctrl Pts',(3.79063989923004,0.79477268400084,5.09398573728429));
#51126=CARTESIAN_POINT('Ctrl Pts',(3.89268207298159,1.06847604194573,5.00562106515799));
#51127=CARTESIAN_POINT('Ctrl Pts',(3.94729257723669,1.18514270861299,4.96370624545236));
#51128=CARTESIAN_POINT('Ctrl Pts',(4.0123433097649,1.3000000000018,4.91812639837089));
#51129=CARTESIAN_POINT('Ctrl Pts',(4.12279848538878,-1.30000000000011,5.09299696544897));
#51130=CARTESIAN_POINT('Ctrl Pts',(4.04973737154303,-1.18514270861186,5.11780304214634));
#51131=CARTESIAN_POINT('Ctrl Pts',(3.98683773167486,-1.06847604194515,5.14010459239705));
#51132=CARTESIAN_POINT('Ctrl Pts',(3.86500201823367,-0.794772684000847,
5.18583967776539));
#51133=CARTESIAN_POINT('Ctrl Pts',(3.81499269883938,-0.636309800095196,
5.21304042894478));
#51134=CARTESIAN_POINT('Ctrl Pts',(3.74455865547157,-0.319434907277159,
5.23617576257593));
#51135=CARTESIAN_POINT('Ctrl Pts',(3.72431438160608,-0.158333333333332,
5.24034022241887));
#51136=CARTESIAN_POINT('Ctrl Pts',(3.71464909220497,0.158333333333334,5.22241426405417));
#51137=CARTESIAN_POINT('Ctrl Pts',(3.72633101530915,0.319434907277168,5.20229432941527));
#51138=CARTESIAN_POINT('Ctrl Pts',(3.77483095349572,0.636309800095206,5.13863137615708));
#51139=CARTESIAN_POINT('Ctrl Pts',(3.81170550975848,0.79477268400084,5.08744014969362));
#51140=CARTESIAN_POINT('Ctrl Pts',(3.91105160620998,1.06847604194572,5.0000431978649));
#51141=CARTESIAN_POINT('Ctrl Pts',(3.96398160966473,1.18514270861299,4.95919623757555));
#51142=CARTESIAN_POINT('Ctrl Pts',(4.02683837255595,1.30000000000179,4.91533321906738));
#51143=CARTESIAN_POINT('Ctrl Pts',(4.14093676471968,-1.30000000000012,5.09122327296693));
#51144=CARTESIAN_POINT('Ctrl Pts',(4.07136124135871,-1.18514270861186,5.11513023307149));
#51145=CARTESIAN_POINT('Ctrl Pts',(4.01092377079359,-1.06847604194515,5.13655462063614));
#51146=CARTESIAN_POINT('Ctrl Pts',(3.89241185333326,-0.794772684000849,
5.18031400264045));
#51147=CARTESIAN_POINT('Ctrl Pts',(3.84098475691061,-0.636309800095196,
5.20574733491462));
#51148=CARTESIAN_POINT('Ctrl Pts',(3.77038842401171,-0.319434907277158,
5.22817448647597));
#51149=CARTESIAN_POINT('Ctrl Pts',(3.74965933386978,-0.158333333333332,
5.23419883041956));
#51150=CARTESIAN_POINT('Ctrl Pts',(3.73946847381987,0.158333333333334,5.21519302180799));
#51151=CARTESIAN_POINT('Ctrl Pts',(3.75076522365139,0.319434907277166,5.19145759520968));
#51152=CARTESIAN_POINT('Ctrl Pts',(3.79905845830081,0.636309800095205,5.12767971641947));
#51153=CARTESIAN_POINT('Ctrl Pts',(3.83790641149878,0.79477268400084,5.07929867273251));
#51154=CARTESIAN_POINT('Ctrl Pts',(3.93424552319471,1.06847604194572,4.99440458049406));
#51155=CARTESIAN_POINT('Ctrl Pts',(3.98484885667692,1.18514270861299,4.95465795765977));
#51156=CARTESIAN_POINT('Ctrl Pts',(4.04435389190397,1.30000000000179,4.91191221888519));
#51157=CARTESIAN_POINT('Ctrl Pts',(4.15945674239667,-1.30000000000011,5.0907785324072));
#51158=CARTESIAN_POINT('Ctrl Pts',(4.09311080137659,-1.18514270861186,5.11348319756018));
#51159=CARTESIAN_POINT('Ctrl Pts',(4.0349310031657,-1.06847604194515,5.13378061450161));
#51160=CARTESIAN_POINT('Ctrl Pts',(3.91938945399031,-0.794772684000846,
5.17511048318358));
#51161=CARTESIAN_POINT('Ctrl Pts',(3.86667281998677,-0.636309800095196,
5.1991035673952));
#51162=CARTESIAN_POINT('Ctrl Pts',(3.79539589942942,-0.31943490727716,5.21970860197993));
#51163=CARTESIAN_POINT('Ctrl Pts',(3.77306755224646,-0.158333333333332,
5.22498077356131));
#51164=CARTESIAN_POINT('Ctrl Pts',(3.76271494571253,0.158333333333334,5.20569233878662));
#51165=CARTESIAN_POINT('Ctrl Pts',(3.77547192320316,0.319434907277168,5.18256501209488));
#51166=CARTESIAN_POINT('Ctrl Pts',(3.82407000646787,0.636309800095207,5.11975133721079));
#51167=CARTESIAN_POINT('Ctrl Pts',(3.86382586108813,0.794772684000841,5.07181087963962));
#51168=CARTESIAN_POINT('Ctrl Pts',(3.95706378536076,1.06847604194573,4.98878077345485));
#51169=CARTESIAN_POINT('Ctrl Pts',(4.00543525417068,1.18514270861299,4.95007068503404));
#51170=CARTESIAN_POINT('Ctrl Pts',(4.06181894917838,1.30000000000179,4.90859116459128));
#51171=CARTESIAN_POINT('Ctrl Pts',(4.18342557961076,-1.30000000000011,5.0880533237051));
#51172=CARTESIAN_POINT('Ctrl Pts',(4.12172043887367,-1.18514270861186,5.10991684623856));
#51173=CARTESIAN_POINT('Ctrl Pts',(4.06683983019807,-1.06847604194515,5.12935875501752));
#51174=CARTESIAN_POINT('Ctrl Pts',(3.95582067963427,-0.794772684000848,
5.16867904142233));
#51175=CARTESIAN_POINT('Ctrl Pts',(3.90159042509488,-0.636309800095196,
5.19114024563324));
#51176=CARTESIAN_POINT('Ctrl Pts',(3.82979124448239,-0.319434907277159,
5.21013150112414));
#51177=CARTESIAN_POINT('Ctrl Pts',(3.80569292631823,-0.158333333333333,
5.21522728291445));
#51178=CARTESIAN_POINT('Ctrl Pts',(3.79491029823192,0.158333333333334,5.19503577853373));
#51179=CARTESIAN_POINT('Ctrl Pts',(3.80871919091485,0.319434907277169,5.17060237547614));
#51180=CARTESIAN_POINT('Ctrl Pts',(3.85755031629569,0.636309800095207,5.10874318097783));
#51181=CARTESIAN_POINT('Ctrl Pts',(3.89921906501687,0.794772684000841,5.06307537622152));
#51182=CARTESIAN_POINT('Ctrl Pts',(3.988349596926,1.06847604194572,4.98286049811985));
#51183=CARTESIAN_POINT('Ctrl Pts',(4.033643981749,1.18514270861299,4.945453426566));
#51184=CARTESIAN_POINT('Ctrl Pts',(4.08565144674312,1.30000000000179,4.90536133193446));
#51185=CARTESIAN_POINT('Ctrl Pts',(4.22679133883142,-1.30000000000012,5.08754453791729));
#51186=CARTESIAN_POINT('Ctrl Pts',(4.17306496523607,-1.18514270861186,5.10773194716304));
#51187=CARTESIAN_POINT('Ctrl Pts',(4.12380529594997,-1.06847604194515,5.12539098632623));
#51188=CARTESIAN_POINT('Ctrl Pts',(4.02032458605148,-0.794772684000849,
5.1603458587825));
#51189=CARTESIAN_POINT('Ctrl Pts',(3.96318443294295,-0.636309800095198,
5.17933184465802));
#51190=CARTESIAN_POINT('Ctrl Pts',(3.89004562735247,-0.31943490727716,5.19434297850385));
#51191=CARTESIAN_POINT('Ctrl Pts',(3.86230316271858,-0.158333333333333,
5.19773408440576));
#51192=CARTESIAN_POINT('Ctrl Pts',(3.85110134256581,0.158333333333335,5.17666779739711));
#51193=CARTESIAN_POINT('Ctrl Pts',(3.86811858072083,0.319434907277172,5.15318648826755));
#51194=CARTESIAN_POINT('Ctrl Pts',(3.91746929822009,0.636309800095212,5.09327663222656));
#51195=CARTESIAN_POINT('Ctrl Pts',(3.9613474480484,0.794772684000842,5.04908300808404));
#51196=CARTESIAN_POINT('Ctrl Pts',(4.0427970212933,1.06847604194573,4.97242114815261));
#51197=CARTESIAN_POINT('Ctrl Pts',(4.08259446846774,1.185142708613,4.93685566114292));
#51198=CARTESIAN_POINT('Ctrl Pts',(4.12693286056292,1.3000000000018,4.89890876568608));
#51199=CARTESIAN_POINT('Ctrl Pts',(4.26662860959375,-1.30000000000012,5.08602638006158));
#51200=CARTESIAN_POINT('Ctrl Pts',(4.22064492887383,-1.18514270861187,5.10567179853889));
#51201=CARTESIAN_POINT('Ctrl Pts',(4.1769425473203,-1.06847604194516,5.1226133871387));
#51202=CARTESIAN_POINT('Ctrl Pts',(4.08125156074687,-0.79477268400086,5.15550545804108));
#51203=CARTESIAN_POINT('Ctrl Pts',(4.02203334074001,-0.636309800095201,
5.17254930925954));
#51204=CARTESIAN_POINT('Ctrl Pts',(3.9482250533704,-0.31943490727716,5.18500429751723));
#51205=CARTESIAN_POINT('Ctrl Pts',(3.91730131763066,-0.158333333333334,
5.18704892685074));
#51206=CARTESIAN_POINT('Ctrl Pts',(3.90552730303133,0.158333333333335,5.16460377015688));
#51207=CARTESIAN_POINT('Ctrl Pts',(3.9249029836412,0.319434907277171,5.14060546316211));
#51208=CARTESIAN_POINT('Ctrl Pts',(3.97426818785949,0.636309800095211,5.0814301994222));
#51209=CARTESIAN_POINT('Ctrl Pts',(4.02015060433034,0.794772684000846,5.03849229416171));
#51210=CARTESIAN_POINT('Ctrl Pts',(4.09419024093476,1.06847604194573,4.96458973189248));
#51211=CARTESIAN_POINT('Ctrl Pts',(4.12875752178953,1.185142708613,4.93050993642205));
#51212=CARTESIAN_POINT('Ctrl Pts',(4.16584306825184,1.3000000000018,4.89434002632783));
#51213=CARTESIAN_POINT('Ctrl Pts',(4.30412671312965,-1.30000000000013,5.08697688034835));
#51214=CARTESIAN_POINT('Ctrl Pts',(4.26520156315833,-1.18514270861187,5.10587992951633));
#51215=CARTESIAN_POINT('Ctrl Pts',(4.22656223259812,-1.06847604194517,5.12197699053405));
#51216=CARTESIAN_POINT('Ctrl Pts',(4.13795794925005,-0.794772684000862,
5.1526820277279));
#51217=CARTESIAN_POINT('Ctrl Pts',(4.07675900440676,-0.636309800095203,
5.16780866837543));
#51218=CARTESIAN_POINT('Ctrl Pts',(4.00244493151388,-0.31943490727716,5.17812328554403));
#51219=CARTESIAN_POINT('Ctrl Pts',(3.96881555197009,-0.158333333333333,
5.17941069446765));
#51220=CARTESIAN_POINT('Ctrl Pts',(3.956710122217,0.158333333333335,5.15609672050486));
#51221=CARTESIAN_POINT('Ctrl Pts',(3.97834621812703,0.319434907277169,5.13176330863161));
#51222=CARTESIAN_POINT('Ctrl Pts',(4.02777396866241,0.63630980009521,5.07341396750342));
#51223=CARTESIAN_POINT('Ctrl Pts',(4.07553836165738,0.794772684000846,5.03190523626189));
#51224=CARTESIAN_POINT('Ctrl Pts',(4.14251703231831,1.06847604194573,4.95996175355017));
#51225=CARTESIAN_POINT('Ctrl Pts',(4.17210106068191,1.185142708613,4.92680230509333));
#51226=CARTESIAN_POINT('Ctrl Pts',(4.20227653268427,1.30000000000181,4.89162507607687));
#51227=CARTESIAN_POINT('Ctrl Pts',(4.32877752354224,-1.30000000000013,5.08656709641375));
#51228=CARTESIAN_POINT('Ctrl Pts',(4.29471764204734,-1.18514270861187,5.10547876627365));
#51229=CARTESIAN_POINT('Ctrl Pts',(4.25957139147602,-1.06847604194517,5.12137741460555));
#51230=CARTESIAN_POINT('Ctrl Pts',(4.17586679177897,-0.794772684000861,
5.15114579028333));
#51231=CARTESIAN_POINT('Ctrl Pts',(4.11335372953131,-0.636309800095201,
5.16493876231558));
#51232=CARTESIAN_POINT('Ctrl Pts',(4.03865680925113,-0.319434907277159,
5.17369177464462));
#51233=CARTESIAN_POINT('Ctrl Pts',(4.00300143242074,-0.158333333333333,
5.17389121757444));
#51234=CARTESIAN_POINT('Ctrl Pts',(3.9907467253463,0.158333333333335,5.15019805216469));
#51235=CARTESIAN_POINT('Ctrl Pts',(4.01427473292349,0.319434907277171,5.12668534350072));
#51236=CARTESIAN_POINT('Ctrl Pts',(4.06375031928799,0.636309800095211,5.06889723091102));
#51237=CARTESIAN_POINT('Ctrl Pts',(4.11240127141197,0.794772684000843,5.02732095624963));
#51238=CARTESIAN_POINT('Ctrl Pts',(4.17454632702921,1.06847604194573,4.95635231974399));
#51239=CARTESIAN_POINT('Ctrl Pts',(4.20079656480992,1.185142708613,4.92378719688524));
#51240=CARTESIAN_POINT('Ctrl Pts',(4.22639674849581,1.3000000000018,4.88937664426398));
#51241=CARTESIAN_POINT('Ctrl Pts',(4.36338436399257,-1.30000000000013,5.0884218903031));
#51242=CARTESIAN_POINT('Ctrl Pts',(4.33592664886913,-1.18514270861187,5.10718352049792));
#51243=CARTESIAN_POINT('Ctrl Pts',(4.30552726312009,-1.06847604194517,5.12269850082007));
#51244=CARTESIAN_POINT('Ctrl Pts',(4.2285027530392,-0.794772684000863,5.15104079842947));
#51245=CARTESIAN_POINT('Ctrl Pts',(4.16422516240804,-0.636309800095203,
5.16303243823351));
#51246=CARTESIAN_POINT('Ctrl Pts',(4.08910985640763,-0.319434907277161,
5.16978297911069));
#51247=CARTESIAN_POINT('Ctrl Pts',(4.0509544209241,-0.158333333333334,5.16908627269049));
#51248=CARTESIAN_POINT('Ctrl Pts',(4.03832107969072,0.158333333333335,5.14431580914702));
#51249=CARTESIAN_POINT('Ctrl Pts',(4.06381919631585,0.319434907277169,5.12028774054229));
#51250=CARTESIAN_POINT('Ctrl Pts',(4.11325013655031,0.636309800095211,5.06298848473702));
#51251=CARTESIAN_POINT('Ctrl Pts',(4.16369137852978,0.794772684000846,5.02290141665623));
#51252=CARTESIAN_POINT('Ctrl Pts',(4.21914030658468,1.06847604194574,4.95309282287407));
#51253=CARTESIAN_POINT('Ctrl Pts',(4.24067397323001,1.185142708613,4.92094784529199));
#51254=CARTESIAN_POINT('Ctrl Pts',(4.25973952015092,1.30000000000181,4.88687544371288));
#51255=CARTESIAN_POINT('Ctrl Pts',(4.40081792825242,-1.30000000000013,5.08960668509033));
#51256=CARTESIAN_POINT('Ctrl Pts',(4.38060481916243,-1.18514270861188,5.10838195576156));
#51257=CARTESIAN_POINT('Ctrl Pts',(4.3554607296501,-1.06847604194517,5.12374749427031));
#51258=CARTESIAN_POINT('Ctrl Pts',(4.28598130160392,-0.794772684000866,
5.15136779868103));
#51259=CARTESIAN_POINT('Ctrl Pts',(4.22020498737131,-0.636309800095208,
5.16269876035965));
#51260=CARTESIAN_POINT('Ctrl Pts',(4.14472081457194,-0.319434907277165,
5.16748862079014));
#51261=CARTESIAN_POINT('Ctrl Pts',(4.10344384562433,-0.158333333333335,
5.16455139316179));
#51262=CARTESIAN_POINT('Ctrl Pts',(4.09045892148647,0.158333333333337,5.13868911700679));
#51263=CARTESIAN_POINT('Ctrl Pts',(4.11858576847778,0.319434907277171,5.11543355955347));
#51264=CARTESIAN_POINT('Ctrl Pts',(4.16795708181541,0.636309800095216,5.05863732762711));
#51265=CARTESIAN_POINT('Ctrl Pts',(4.21978800755112,0.794772684000854,5.01868454107607));
#51266=CARTESIAN_POINT('Ctrl Pts',(4.26791808824448,1.06847604194575,4.95004897516277));
#51267=CARTESIAN_POINT('Ctrl Pts',(4.28440774598148,1.18514270861301,4.9185943220005));
#51268=CARTESIAN_POINT('Ctrl Pts',(4.29655333291852,1.30000000000182,4.88539480896152));
#51269=CARTESIAN_POINT('Ctrl Pts',(4.43869075631515,-1.30000000000014,5.09244705574098));
#51270=CARTESIAN_POINT('Ctrl Pts',(4.4259039117771,-1.18514270861188,5.11197858778474));
#51271=CARTESIAN_POINT('Ctrl Pts',(4.40609614803908,-1.06847604194518,5.12754664347477));
#51272=CARTESIAN_POINT('Ctrl Pts',(4.34411652339266,-0.794772684000867,
5.1543555432298));
#51273=CARTESIAN_POINT('Ctrl Pts',(4.27619860307338,-0.636309800095207,
5.16276898456766));
#51274=CARTESIAN_POINT('Ctrl Pts',(4.20048954849266,-0.319434907277163,
5.16588018400511));
#51275=CARTESIAN_POINT('Ctrl Pts',(4.15691369948975,-0.158333333333335,
5.16316308628125));
#51276=CARTESIAN_POINT('Ctrl Pts',(4.14373089636936,0.158333333333337,5.13666783959865));
#51277=CARTESIAN_POINT('Ctrl Pts',(4.17396099819442,0.319434907277173,5.11269068694486));
#51278=CARTESIAN_POINT('Ctrl Pts',(4.22314953732488,0.636309800095217,5.05601593393405));
#51279=CARTESIAN_POINT('Ctrl Pts',(4.27671605343378,0.794772684000851,5.01714584195804));
#51280=CARTESIAN_POINT('Ctrl Pts',(4.31731758874883,1.06847604194574,4.94901350491504));
#51281=CARTESIAN_POINT('Ctrl Pts',(4.32857128559891,1.18514270861301,4.91766527313274));
#51282=CARTESIAN_POINT('Ctrl Pts',(4.33350377909629,1.30000000000182,4.88446077372224));
#51283=CARTESIAN_POINT('Ctrl Pts',(4.46694355687885,-1.30000000000014,5.09421253927619));
#51284=CARTESIAN_POINT('Ctrl Pts',(4.4596064259396,-1.18514270861189,5.11394876273183));
#51285=CARTESIAN_POINT('Ctrl Pts',(4.44377954862526,-1.06847604194518,5.12962974440685));
#51286=CARTESIAN_POINT('Ctrl Pts',(4.38760328337876,-0.794772684000872,
5.15648752928424));
#51287=CARTESIAN_POINT('Ctrl Pts',(4.3187730302285,-0.636309800095212,5.16507039195884));
#51288=CARTESIAN_POINT('Ctrl Pts',(4.24292776592144,-0.319434907277166,
5.16702937530694));
#51289=CARTESIAN_POINT('Ctrl Pts',(4.19702442005355,-0.158333333333336,
5.16242417342549));
#51290=CARTESIAN_POINT('Ctrl Pts',(4.18354609357958,0.158333333333338,5.13489369752115));
#51291=CARTESIAN_POINT('Ctrl Pts',(4.21564175361208,0.319434907277175,5.11124266511601));
#51292=CARTESIAN_POINT('Ctrl Pts',(4.26470351866793,0.636309800095221,5.05468440217912));
#51293=CARTESIAN_POINT('Ctrl Pts',(4.31937178111756,0.794772684000859,5.01609861444084));
#51294=CARTESIAN_POINT('Ctrl Pts',(4.35431037108749,1.06847604194575,4.94825399957144));
#51295=CARTESIAN_POINT('Ctrl Pts',(4.36166410385363,1.18514270861302,4.91702696257548));
#51296=CARTESIAN_POINT('Ctrl Pts',(4.36124794839026,1.30000000000182,4.88394030846984));
#51297=CARTESIAN_POINT('Ctrl Pts',(4.48436618663496,-1.30000000000014,5.09588490856402));
#51298=CARTESIAN_POINT('Ctrl Pts',(4.4804099567393,-1.18514270861189,5.11595623744478));
#51299=CARTESIAN_POINT('Ctrl Pts',(4.46703110461135,-1.06847604194518,5.1317821487358));
#51300=CARTESIAN_POINT('Ctrl Pts',(4.41435513741988,-0.794772684000872,
5.15853540585559));
#51301=CARTESIAN_POINT('Ctrl Pts',(4.34476889322958,-0.636309800095214,
5.16651743138278));
#51302=CARTESIAN_POINT('Ctrl Pts',(4.26877059680495,-0.319434907277168,
5.16749990384559));
#51303=CARTESIAN_POINT('Ctrl Pts',(4.22147324109189,-0.158333333333337,
5.16179550010107));
#51304=CARTESIAN_POINT('Ctrl Pts',(4.20790626770664,0.158333333333339,5.13392436678544));
#51305=CARTESIAN_POINT('Ctrl Pts',(4.24125663852064,0.319434907277176,5.11088979094392));
#51306=CARTESIAN_POINT('Ctrl Pts',(4.29039404310591,0.636309800095223,5.05490356707114));
#51307=CARTESIAN_POINT('Ctrl Pts',(4.34592397091069,0.794772684000863,5.01707090348525));
#51308=CARTESIAN_POINT('Ctrl Pts',(4.37732508768174,1.06847604194575,4.94914432789985));
#51309=CARTESIAN_POINT('Ctrl Pts',(4.38219364604858,1.18514270861302,4.91766097371381));
#51310=CARTESIAN_POINT('Ctrl Pts',(4.37833838285809,1.30000000000183,4.88409716298504));
#51311=CARTESIAN_POINT('Ctrl Pts',(4.49070400846268,-1.30000000000014,5.09652071259581));
#51312=CARTESIAN_POINT('Ctrl Pts',(4.48798825337379,-1.18514270861189,5.1167655310822));
#51313=CARTESIAN_POINT('Ctrl Pts',(4.47550560194655,-1.06847604194518,5.13267131386532));
#51314=CARTESIAN_POINT('Ctrl Pts',(4.42410469560128,-0.794772684000872,
5.15939281353954));
#51315=CARTESIAN_POINT('Ctrl Pts',(4.35421254555806,-0.636309800095214,
5.1670173368963));
#51316=CARTESIAN_POINT('Ctrl Pts',(4.27817340285055,-0.319434907277168,
5.16768424858849));
#51317=CARTESIAN_POINT('Ctrl Pts',(4.23043444623617,-0.158333333333337,
5.16181148227735));
#51318=CARTESIAN_POINT('Ctrl Pts',(4.21681702784594,0.158333333333338,5.13375826922441));
#51319=CARTESIAN_POINT('Ctrl Pts',(4.25055057292307,0.319434907277175,5.110698391497));
#51320=CARTESIAN_POINT('Ctrl Pts',(4.29964232896039,0.636309800095222,5.05468044231088));
#51321=CARTESIAN_POINT('Ctrl Pts',(4.35540993324731,0.794772684000862,5.0168849790298));
#51322=CARTESIAN_POINT('Ctrl Pts',(4.38554641430621,1.06847604194575,4.94899736917052));
#51323=CARTESIAN_POINT('Ctrl Pts',(4.38954737955112,1.18514270861302,4.9175353766224));
#51324=CARTESIAN_POINT('Ctrl Pts',(4.38450434405719,1.30000000000183,4.88399742235045));
#51325=CARTESIAN_POINT('Ctrl Pts',(4.49706625050769,-1.30000000000014,5.09725490143989));
#51326=CARTESIAN_POINT('Ctrl Pts',(4.49561313210597,-1.18514270861189,5.11776177368923));
#51327=CARTESIAN_POINT('Ctrl Pts',(4.48403718193686,-1.06847604194518,5.13379000112895));
#51328=CARTESIAN_POINT('Ctrl Pts',(4.43390865483705,-0.794772684000871,
5.16047184749054));
#51329=CARTESIAN_POINT('Ctrl Pts',(4.3636497831239,-0.636309800095214,5.16750626028728));
#51330=CARTESIAN_POINT('Ctrl Pts',(4.28756531497726,-0.319434907277168,
5.16783169026165));
#51331=CARTESIAN_POINT('Ctrl Pts',(4.23942987235426,-0.158333333333337,
5.16194741269489));
#51332=CARTESIAN_POINT('Ctrl Pts',(4.22577045208385,0.158333333333338,5.13373942688524));
#51333=CARTESIAN_POINT('Ctrl Pts',(4.25987060472629,0.319434907277175,5.11059656273882));
#51334=CARTESIAN_POINT('Ctrl Pts',(4.30889743682903,0.636309800095223,5.05448205830684));
#51335=CARTESIAN_POINT('Ctrl Pts',(4.36487767719341,0.794772684000863,5.01664278826843));
#51336=CARTESIAN_POINT('Ctrl Pts',(4.39374659513668,1.06847604194575,4.94878339216866));
#51337=CARTESIAN_POINT('Ctrl Pts',(4.39688482303203,1.18514270861302,4.9173578773307));
#51338=CARTESIAN_POINT('Ctrl Pts',(4.39066499394388,1.30000000000183,4.88388066578801));
#51339=CARTESIAN_POINT('Ctrl Pts',(4.50342826126824,-1.30000000000014,5.09799890728752));
#51340=CARTESIAN_POINT('Ctrl Pts',(4.5032420856426,-1.18514270861189,5.11878887146126));
#51341=CARTESIAN_POINT('Ctrl Pts',(4.49257623194904,-1.06847604194518,5.13495548473586));
#51342=CARTESIAN_POINT('Ctrl Pts',(4.44372582343088,-0.794772684000872,
5.16162273004491));
#51343=CARTESIAN_POINT('Ctrl Pts',(4.37309890724761,-0.636309800095214,
5.16806100431414));
#51344=CARTESIAN_POINT('Ctrl Pts',(4.29697528558695,-0.319434907277168,
5.16806105128099));
#51345=CARTESIAN_POINT('Ctrl Pts',(4.24845291887343,-0.158333333333336,
5.16218849036971));
#51346=CARTESIAN_POINT('Ctrl Pts',(4.23475258734916,0.158333333333338,5.13382616185956));
#51347=CARTESIAN_POINT('Ctrl Pts',(4.26921358881558,0.319434907277174,5.11058481137938));
#51348=CARTESIAN_POINT('Ctrl Pts',(4.31816602131599,0.636309800095222,5.05434366360625));
#51349=CARTESIAN_POINT('Ctrl Pts',(4.37434838324022,0.794772684000862,5.01642824211172));
#51350=CARTESIAN_POINT('Ctrl Pts',(4.40194351193221,1.06847604194575,4.94857304605718));
#51351=CARTESIAN_POINT('Ctrl Pts',(4.40421791446416,1.18514270861302,4.91717758007938));
#51352=CARTESIAN_POINT('Ctrl Pts',(4.39682181081755,1.30000000000183,4.88375864821306));
#51353=CARTESIAN_POINT('Ctrl Pts',(4.5089703151262,-1.30000000000014,5.09855433356514));
#51354=CARTESIAN_POINT('Ctrl Pts',(4.50986730449823,-1.18514270861189,5.1194902140667));
#51355=CARTESIAN_POINT('Ctrl Pts',(4.49998765777042,-1.06847604194518,5.13573692231672));
#51356=CARTESIAN_POINT('Ctrl Pts',(4.45226751216336,-0.794772684000871,
5.16243714255034));
#51357=CARTESIAN_POINT('Ctrl Pts',(4.38140730018764,-0.636309800095213,
5.1687021689243));
#51358=CARTESIAN_POINT('Ctrl Pts',(4.30525623160429,-0.319434907277168,
5.1684501436253));
#51359=CARTESIAN_POINT('Ctrl Pts',(4.25631839326472,-0.158333333333336,
5.16230199422985));
#51360=CARTESIAN_POINT('Ctrl Pts',(4.24258473667234,0.158333333333338,5.13380593151017));
#51361=CARTESIAN_POINT('Ctrl Pts',(4.2774154453425,0.319434907277175,5.11066851664683));
#51362=CARTESIAN_POINT('Ctrl Pts',(4.32635278207021,0.636309800095222,5.05448427175959));
#51363=CARTESIAN_POINT('Ctrl Pts',(4.38276986346915,0.794772684000862,5.01668834541608));
#51364=CARTESIAN_POINT('Ctrl Pts',(4.40922659624202,1.06847604194575,4.94876025066249));
#51365=CARTESIAN_POINT('Ctrl Pts',(4.4107134089054,1.18514270861302,4.91728834502899));
#51366=CARTESIAN_POINT('Ctrl Pts',(4.40223489493331,1.30000000000183,4.88374808899692));
#51367=CARTESIAN_POINT('Ctrl Pts',(4.51173593338493,-1.30000000000014,5.0988119602196));
#51368=CARTESIAN_POINT('Ctrl Pts',(4.51316878410743,-1.18514270861189,5.11979885946483));
#51369=CARTESIAN_POINT('Ctrl Pts',(4.50367993561254,-1.06847604194518,5.136076882354));
#51370=CARTESIAN_POINT('Ctrl Pts',(4.4565274872811,-0.794772684000871,5.16280392524531));
#51371=CARTESIAN_POINT('Ctrl Pts',(4.38556942968062,-0.636309800095214,
5.16905517158179));
#51372=CARTESIAN_POINT('Ctrl Pts',(4.30940797613757,-0.319434907277168,
5.16869064712411));
#51373=CARTESIAN_POINT('Ctrl Pts',(4.26025013011133,-0.158333333333336,
5.16235872701826));
#51374=CARTESIAN_POINT('Ctrl Pts',(4.24649955259772,0.158333333333338,5.13379357096223));
#51375=CARTESIAN_POINT('Ctrl Pts',(4.28152116181099,0.319434907277174,5.11072957108493));
#51376=CARTESIAN_POINT('Ctrl Pts',(4.33045923925767,0.636309800095221,5.0546011357185));
#51377=CARTESIAN_POINT('Ctrl Pts',(4.38700624373682,0.794772684000862,5.01690598005947));
#51378=CARTESIAN_POINT('Ctrl Pts',(4.41289071606697,1.06847604194575,4.94893059205468));
#51379=CARTESIAN_POINT('Ctrl Pts',(4.41397847476729,1.18514270861302,4.91740271407581));
#51380=CARTESIAN_POINT('Ctrl Pts',(4.40494956321041,1.30000000000183,4.88377098484906));
#51381=CARTESIAN_POINT('Ctrl Pts',(4.51331549988098,-1.30000000000014,5.09895634230767));
#51382=CARTESIAN_POINT('Ctrl Pts',(4.51505386685927,-1.18514270861189,5.11996963318523));
#51383=CARTESIAN_POINT('Ctrl Pts',(4.50578809552361,-1.06847604194518,5.13626457196588));
#51384=CARTESIAN_POINT('Ctrl Pts',(4.45896054925151,-0.794772684000871,
5.16300880309351));
#51385=CARTESIAN_POINT('Ctrl Pts',(4.38794960734779,-0.636309800095214,
5.16926379970333));
#51386=CARTESIAN_POINT('Ctrl Pts',(4.31178198849649,-0.319434907277168,
5.1688343464384));
#51387=CARTESIAN_POINT('Ctrl Pts',(4.26249479831643,-0.158333333333336,
5.1623841728602));
#51388=CARTESIAN_POINT('Ctrl Pts',(4.24873474873611,0.158333333333338,5.1337799496331));
#51389=CARTESIAN_POINT('Ctrl Pts',(4.28386868929949,0.319434907277174,5.11076930433508));
#51390=CARTESIAN_POINT('Ctrl Pts',(4.33280899807485,0.636309800095221,5.05467883811918));
#51391=CARTESIAN_POINT('Ctrl Pts',(4.38943094971871,0.794772684000862,5.01704314978778));
#51392=CARTESIAN_POINT('Ctrl Pts',(4.41498744433985,1.06847604194575,4.94903762837009));
#51393=CARTESIAN_POINT('Ctrl Pts',(4.41584622184238,1.18514270861302,4.91747476919486));
#51394=CARTESIAN_POINT('Ctrl Pts',(4.40650131728738,1.30000000000183,4.88378612121329));
#51395=CARTESIAN_POINT('Ctrl Pts',(4.52673420369595,-1.30000000000014,5.10015672069679));
#51396=CARTESIAN_POINT('Ctrl Pts',(4.53105886446733,-1.18514270861189,5.12135679964457));
#51397=CARTESIAN_POINT('Ctrl Pts',(4.52368495272715,-1.06847604194518,5.13778140892107));
#51398=CARTESIAN_POINT('Ctrl Pts',(4.47962369866828,-0.79477268400087,5.16469325181154));
#51399=CARTESIAN_POINT('Ctrl Pts',(4.40818825363879,-0.636309800095212,
5.17107852727311));
#51400=CARTESIAN_POINT('Ctrl Pts',(4.33199311210111,-0.319434907277167,
5.17018879965183));
#51401=CARTESIAN_POINT('Ctrl Pts',(4.28162985675607,-0.158333333333336,
5.16281249744401));
#51402=CARTESIAN_POINT('Ctrl Pts',(4.2677871536587,0.158333333333338,5.13386585357558));
#51403=CARTESIAN_POINT('Ctrl Pts',(4.30383451681207,0.319434907277172,5.11116134357201));
#51404=CARTESIAN_POINT('Ctrl Pts',(4.35279692096245,0.636309800095219,5.05539906111259));
#51405=CARTESIAN_POINT('Ctrl Pts',(4.41010452611587,0.79477268400086,5.01843725806858));
#51406=CARTESIAN_POINT('Ctrl Pts',(4.43287946120475,1.06847604194575,4.95018778605438));
#51407=CARTESIAN_POINT('Ctrl Pts',(4.43178623420622,1.18514270861302,4.91830230319173));
#51408=CARTESIAN_POINT('Ctrl Pts',(4.41974135470369,1.30000000000183,4.88407400500928));
#51409=CARTESIAN_POINT('Ctrl Pts',(4.55257517464123,-1.30000000000013,5.1033102584444));
#51410=CARTESIAN_POINT('Ctrl Pts',(4.56204421640626,-1.18514270861187,5.12573190702204));
#51411=CARTESIAN_POINT('Ctrl Pts',(4.55838559416382,-1.06847604194517,5.14283935276507));
#51412=CARTESIAN_POINT('Ctrl Pts',(4.5196059148415,-0.794772684000862,5.17008410311367));
#51413=CARTESIAN_POINT('Ctrl Pts',(4.44686892664056,-0.636309800095204,
5.17472119164269));
#51414=CARTESIAN_POINT('Ctrl Pts',(4.37054149862908,-0.319434907277161,
5.17255733923234));
#51415=CARTESIAN_POINT('Ctrl Pts',(4.31841632073828,-0.158333333333334,
5.16446413815593));
#51416=CARTESIAN_POINT('Ctrl Pts',(4.30443648682053,0.158333333333336,5.13493687844417));
#51417=CARTESIAN_POINT('Ctrl Pts',(4.342177815926,0.319434907277172,5.11266026279369));
#51418=CARTESIAN_POINT('Ctrl Pts',(4.39085227802371,0.636309800095214,5.05639544117813));
#51419=CARTESIAN_POINT('Ctrl Pts',(4.44873093967267,0.794772684000848,5.01824254835966));
#51420=CARTESIAN_POINT('Ctrl Pts',(4.46636449056368,1.06847604194574,4.94999476957805));
#51421=CARTESIAN_POINT('Ctrl Pts',(4.46183091987552,1.185142708613,4.91839135385537));
#51422=CARTESIAN_POINT('Ctrl Pts',(4.44513086770591,1.30000000000181,4.8847264570152));
#51423=CARTESIAN_POINT('Ctrl Pts',(4.57797014782441,-1.30000000000011,5.10637392230933));
#51424=CARTESIAN_POINT('Ctrl Pts',(4.59241718008651,-1.18514270861186,5.12973339069855));
#51425=CARTESIAN_POINT('Ctrl Pts',(4.5923750883925,-1.06847604194515,5.14740422222097));
#51426=CARTESIAN_POINT('Ctrl Pts',(4.55880507328097,-0.794772684000851,
5.17508548890529));
#51427=CARTESIAN_POINT('Ctrl Pts',(4.48498896022061,-0.636309800095197,
5.17877438662047));
#51428=CARTESIAN_POINT('Ctrl Pts',(4.40861628632669,-0.319434907277159,
5.17565787022847));
#51429=CARTESIAN_POINT('Ctrl Pts',(4.35474635534816,-0.158333333333332,
5.16675378500001));
#51430=CARTESIAN_POINT('Ctrl Pts',(4.34059295810105,0.158333333333334,5.1364765704601));
#51431=CARTESIAN_POINT('Ctrl Pts',(4.3797744155812,0.319434907277167,5.11381935642279));
#51432=CARTESIAN_POINT('Ctrl Pts',(4.42840755015826,0.636309800095206,5.05787895495823));
#51433=CARTESIAN_POINT('Ctrl Pts',(4.48773430817404,0.79477268400084,5.02157383053672));
#51434=CARTESIAN_POINT('Ctrl Pts',(4.50009761851211,1.06847604194573,4.95268677460948));
#51435=CARTESIAN_POINT('Ctrl Pts',(4.49184486495928,1.18514270861299,4.92027496910602));
#51436=CARTESIAN_POINT('Ctrl Pts',(4.46998773891406,1.3000000000018,4.88527001209309));
#51437=CARTESIAN_POINT('Ctrl Pts',(4.59077270268395,-1.30000000000011,5.10832931194405));
#51438=CARTESIAN_POINT('Ctrl Pts',(4.60766161389344,-1.18514270861186,5.13199826094758));
#51439=CARTESIAN_POINT('Ctrl Pts',(4.60940251578961,-1.06847604194515,5.14987106382229));
#51440=CARTESIAN_POINT('Ctrl Pts',(4.57842941557334,-0.794772684000851,
5.17777055683221));
#51441=CARTESIAN_POINT('Ctrl Pts',(4.50418204215329,-0.636309800095197,
5.1814197357197));
#51442=CARTESIAN_POINT('Ctrl Pts',(4.42777734501206,-0.319434907277159,
5.17777988362783));
#51443=CARTESIAN_POINT('Ctrl Pts',(4.37292795574625,-0.158333333333332,
5.16801756977584));
#51444=CARTESIAN_POINT('Ctrl Pts',(4.35867257917562,0.158333333333334,5.13728168805675));
#51445=CARTESIAN_POINT('Ctrl Pts',(4.39869447984769,0.319434907277167,5.11487935011378));
#51446=CARTESIAN_POINT('Ctrl Pts',(4.44722735233343,0.636309800095206,5.05882272597048));
#51447=CARTESIAN_POINT('Ctrl Pts',(4.50695309467615,0.79477268400084,5.02233268407818));
#51448=CARTESIAN_POINT('Ctrl Pts',(4.51674956614749,1.06847604194573,4.95329826442052));
#51449=CARTESIAN_POINT('Ctrl Pts',(4.50675280587869,1.18514270861299,4.9208376091363));
#51450=CARTESIAN_POINT('Ctrl Pts',(4.48251875583617,1.3000000000018,4.88579874086039));
#51451=CARTESIAN_POINT('',(4.3897288827106,1.2,4.91247287747308));
#51452=CARTESIAN_POINT('Ctrl Pts',(4.3897288827106,1.2,4.91247287747308));
#51453=CARTESIAN_POINT('Ctrl Pts',(4.36857135610553,1.21681573945508,4.90825963985616));
#51454=CARTESIAN_POINT('Ctrl Pts',(4.3473023706465,1.23325593210168,4.90314947462289));
#51455=CARTESIAN_POINT('Ctrl Pts',(4.2998391327148,1.27069836523098,4.89364883337151));
#51456=CARTESIAN_POINT('Ctrl Pts',(4.28243988954012,1.28442464637428,4.89030656849232));
#51457=CARTESIAN_POINT('Ctrl Pts',(4.26287719563543,1.30000000000181,4.88691158514987));
#51458=CARTESIAN_POINT('',(4.45989076534562,0.653834841370385,5.05247250056665));
#51459=CARTESIAN_POINT('Ctrl Pts',(4.45989076537646,0.653834841369131,5.05247250054632));
#51460=CARTESIAN_POINT('Ctrl Pts',(4.45288492245741,0.717482042443765,5.03792307375374));
#51461=CARTESIAN_POINT('Ctrl Pts',(4.44711302933054,0.764209734534401,5.02607170794616));
#51462=CARTESIAN_POINT('Ctrl Pts',(4.42420943059583,0.949856843367683,4.97961640082602));
#51463=CARTESIAN_POINT('Ctrl Pts',(4.41030972125718,1.0567232552086,4.95196718576286));
#51464=CARTESIAN_POINT('Ctrl Pts',(4.3897288827106,1.2,4.91247287747308));
#51465=CARTESIAN_POINT('',(4.51863764645995,-0.653834841531101,5.17900672440632));
#51466=CARTESIAN_POINT('Ctrl Pts',(4.51863764645995,-0.6538348415311,5.17900672440632));
#51467=CARTESIAN_POINT('Ctrl Pts',(4.47706947811755,-0.575982437876214,
5.17841861144383));
#51468=CARTESIAN_POINT('Ctrl Pts',(4.44193277695744,-0.493637398627582,
5.17716781668147));
#51469=CARTESIAN_POINT('Ctrl Pts',(4.39149855918852,-0.338135451747832,
5.17291766455466));
#51470=CARTESIAN_POINT('Ctrl Pts',(4.37381733731089,-0.265660868320344,
5.17019185540934));
#51471=CARTESIAN_POINT('Ctrl Pts',(4.35075353763555,-0.129717629145974,
5.16230413532239));
#51472=CARTESIAN_POINT('Ctrl Pts',(4.3439598574373,-0.0666258049312309,
5.15757923333407));
#51473=CARTESIAN_POINT('Ctrl Pts',(4.33801233342096,0.0595444162497744,
5.14565140581426));
#51474=CARTESIAN_POINT('Ctrl Pts',(4.33879948700794,0.122777977220077,5.13836852715898));
#51475=CARTESIAN_POINT('Ctrl Pts',(4.34922857416695,0.2601311288836,5.12044478424126));
#51476=CARTESIAN_POINT('Ctrl Pts',(4.36046089628691,0.333946038931111,5.10943059845951));
#51477=CARTESIAN_POINT('Ctrl Pts',(4.39723462068707,0.491209513290317,5.08375691479056));
#51478=CARTESIAN_POINT('Ctrl Pts',(4.42491373516359,0.574351626734296,5.06856490516704));
#51479=CARTESIAN_POINT('Ctrl Pts',(4.45989076529517,0.653834841386886,5.05247250053849));
#51480=CARTESIAN_POINT('',(4.48868816730329,-1.2,5.11333315148022));
#51481=CARTESIAN_POINT('Ctrl Pts',(4.48868816730329,-1.2,5.11333315148022));
#51482=CARTESIAN_POINT('Ctrl Pts',(4.49330354820273,-1.14227030646505,5.12326142807387));
#51483=CARTESIAN_POINT('Ctrl Pts',(4.49957148427282,-1.06120661874143,5.13679379880293));
#51484=CARTESIAN_POINT('Ctrl Pts',(4.51379468897461,-0.796649462481794,
5.16817211105445));
#51485=CARTESIAN_POINT('Ctrl Pts',(4.51601641408078,-0.739685413249303,
5.17314604221026));
#51486=CARTESIAN_POINT('Ctrl Pts',(4.51863764645995,-0.653834841531101,
5.17900672440632));
#51487=CARTESIAN_POINT('Ctrl Pts',(4.36619448174045,-1.30000000000001,5.08840208666064));
#51488=CARTESIAN_POINT('Ctrl Pts',(4.38689833577429,-1.28301364714831,5.09219695776369));
#51489=CARTESIAN_POINT('Ctrl Pts',(4.40759529208872,-1.26604667874466,5.0961307302198));
#51490=CARTESIAN_POINT('Ctrl Pts',(4.45484463189025,-1.22753397446419,5.10588976509139));
#51491=CARTESIAN_POINT('Ctrl Pts',(4.47022545323923,-1.21477226219745,5.10866030766466));
#51492=CARTESIAN_POINT('Ctrl Pts',(4.48868816730329,-1.2,5.11333315148022));
#51493=CARTESIAN_POINT('Origin',(0.,1.25,7.2));
#51494=CARTESIAN_POINT('Origin',(0.,1.2,7.2));
#51495=CARTESIAN_POINT('Origin',(0.,0.92691742076555,7.2));
#51496=CARTESIAN_POINT('Origin',(0.,0.653834841531101,7.2));
#51497=CARTESIAN_POINT('Origin',(0.,0.,7.2));
#51498=CARTESIAN_POINT('Origin',(0.,-0.653834841531101,7.2));
#51499=CARTESIAN_POINT('Origin',(0.,-0.926917420765551,7.2));
#51500=CARTESIAN_POINT('Origin',(0.,-1.2,7.2));
#51501=CARTESIAN_POINT('Origin',(0.,-1.25,7.2));
#51502=CARTESIAN_POINT('Ctrl Pts',(4.7191771839547,-1.30000000000134,5.41734227325848));
#51503=CARTESIAN_POINT('Ctrl Pts',(4.70935397490593,-1.18514270861269,5.37588728519308));
#51504=CARTESIAN_POINT('Ctrl Pts',(4.69192014516093,-1.06847604194558,5.34673782657451));
#51505=CARTESIAN_POINT('Ctrl Pts',(4.63406245451663,-0.794772684000851,
5.3078249805714));
#51506=CARTESIAN_POINT('Ctrl Pts',(4.56698074651016,-0.636309800095197,
5.32779325308501));
#51507=CARTESIAN_POINT('Ctrl Pts',(4.49284772594841,-0.319434907277159,
5.32635100323535));
#51508=CARTESIAN_POINT('Ctrl Pts',(4.44941966576432,-0.158333333333332,
5.34110298165352));
#51509=CARTESIAN_POINT('Ctrl Pts',(4.43611716307696,0.158333333333334,5.30994285314816));
#51510=CARTESIAN_POINT('Ctrl Pts',(4.46556375515151,0.319434907277167,5.26264955034729));
#51511=CARTESIAN_POINT('Ctrl Pts',(4.51398353922898,0.636309800095206,5.20343425858799));
#51512=CARTESIAN_POINT('Ctrl Pts',(4.56637659762912,0.79477268400084,5.15069948450899));
#51513=CARTESIAN_POINT('Ctrl Pts',(4.60783501082194,1.06847604194514,5.14635039002878));
#51514=CARTESIAN_POINT('Ctrl Pts',(4.61995220105504,1.18514270861184,5.15960337168886));
#51515=CARTESIAN_POINT('Ctrl Pts',(4.62624077063569,1.30000000000009,5.18799189685967));
#51516=CARTESIAN_POINT('Ctrl Pts',(4.71118521909801,-1.30000000000134,5.42700842222637));
#51517=CARTESIAN_POINT('Ctrl Pts',(4.69979673845632,-1.18514270861269,5.38734252398592));
#51518=CARTESIAN_POINT('Ctrl Pts',(4.68123224291413,-1.06847604194558,5.35952180181295));
#51519=CARTESIAN_POINT('Ctrl Pts',(4.62176651442015,-0.794772684000851,
5.32261509441226));
#51520=CARTESIAN_POINT('Ctrl Pts',(4.55508919945685,-0.636309800095197,
5.34241059774211));
#51521=CARTESIAN_POINT('Ctrl Pts',(4.48097546072873,-0.319434907277159,
5.34112062530357));
#51522=CARTESIAN_POINT('Ctrl Pts',(4.43792035696629,-0.158333333333332,
5.35507748731411));
#51523=CARTESIAN_POINT('Ctrl Pts',(4.42489047293298,0.158333333333334,5.32430005246305));
#51524=CARTESIAN_POINT('Ctrl Pts',(4.45431946765656,0.319434907277167,5.27830889605651));
#51525=CARTESIAN_POINT('Ctrl Pts',(4.5031067381983,0.636309800095206,5.21946758214842));
#51526=CARTESIAN_POINT('Ctrl Pts',(4.55524074388928,0.79477268400084,5.16707987407414));
#51527=CARTESIAN_POINT('Ctrl Pts',(4.59827465855659,1.06847604194514,5.16065487381351));
#51528=CARTESIAN_POINT('Ctrl Pts',(4.6114348104173,1.18514270861184,5.17244768779572));
#51529=CARTESIAN_POINT('Ctrl Pts',(4.61912732704296,1.30000000000009,5.19881446030323));
#51530=CARTESIAN_POINT('Ctrl Pts',(4.69494687124662,-1.3000000000016,5.445801977467));
#51531=CARTESIAN_POINT('Ctrl Pts',(4.68127539588664,-1.18514270861292,5.41115438741575));
#51532=CARTESIAN_POINT('Ctrl Pts',(4.66092526233145,-1.06847604194579,5.386812218893));
#51533=CARTESIAN_POINT('Ctrl Pts',(4.59848334629683,-0.794772684001002,
5.35438452529471));
#51534=CARTESIAN_POINT('Ctrl Pts',(4.53116973209331,-0.63630980009532,5.37149271969744));
#51535=CARTESIAN_POINT('Ctrl Pts',(4.45670596000581,-0.319434907277221,
5.36988490694989));
#51536=CARTESIAN_POINT('Ctrl Pts',(4.41494753063121,-0.158333333333363,
5.38309622210191));
#51537=CARTESIAN_POINT('Ctrl Pts',(4.40229724694797,0.158333333333365,5.35285740435751));
#51538=CARTESIAN_POINT('Ctrl Pts',(4.43104909968437,0.319434907277229,5.30854619488518));
#51539=CARTESIAN_POINT('Ctrl Pts',(4.48047089785509,0.63630980009533,5.25031366414003));
#51540=CARTESIAN_POINT('Ctrl Pts',(4.53265817182857,0.794772684000994,5.19946768138508));
#51541=CARTESIAN_POINT('Ctrl Pts',(4.57884238347787,1.06847604194535,5.18885484938565));
#51542=CARTESIAN_POINT('Ctrl Pts',(4.59398697743196,1.18514270861207,5.19755297456347));
#51543=CARTESIAN_POINT('Ctrl Pts',(4.60428473141087,1.30000000000035,5.21954312664747));
#51544=CARTESIAN_POINT('Ctrl Pts',(4.67855760031106,-1.30000000000186,5.46495686707269));
#51545=CARTESIAN_POINT('Ctrl Pts',(4.66120377365009,-1.18514270861316,5.43307420647752));
#51546=CARTESIAN_POINT('Ctrl Pts',(4.63825704955113,-1.068476041946,5.41090735290281));
#51547=CARTESIAN_POINT('Ctrl Pts',(4.57232481446913,-0.794772684001165,
5.38214294453913));
#51548=CARTESIAN_POINT('Ctrl Pts',(4.50650585290617,-0.63630980009545,5.40001639808124));
#51549=CARTESIAN_POINT('Ctrl Pts',(4.43231296648443,-0.319434907277286,
5.39910293902452));
#51550=CARTESIAN_POINT('Ctrl Pts',(4.39132670753068,-0.158333333333395,
5.41071813719325));
#51551=CARTESIAN_POINT('Ctrl Pts',(4.37907887492038,0.158333333333397,5.38106212502469));
#51552=CARTESIAN_POINT('Ctrl Pts',(4.40729214896405,0.319434907277294,5.33867722957612));
#51553=CARTESIAN_POINT('Ctrl Pts',(4.45760677965426,0.636309800095459,5.28145202353281));
#51554=CARTESIAN_POINT('Ctrl Pts',(4.51015579493688,0.794772684001156,5.23263852905263));
#51555=CARTESIAN_POINT('Ctrl Pts',(4.55960657769512,1.06847604194556,5.21792091386001));
#51556=CARTESIAN_POINT('Ctrl Pts',(4.57672612162891,1.18514270861231,5.22344389860329));
#51557=CARTESIAN_POINT('Ctrl Pts',(4.58955979797253,1.30000000000061,5.24086057836533));
#51558=CARTESIAN_POINT('Ctrl Pts',(4.67014172218832,-1.30000000000189,5.4746514904811));
#51559=CARTESIAN_POINT('Ctrl Pts',(4.65141061882585,-1.18514270861319,5.4450466677508));
#51560=CARTESIAN_POINT('Ctrl Pts',(4.62742281607529,-1.06847604194603,5.42448826836267));
#51561=CARTESIAN_POINT('Ctrl Pts',(4.5598621657925,-0.794772684001185,5.39789330073363));
#51562=CARTESIAN_POINT('Ctrl Pts',(4.49404072528191,-0.636309800095465,
5.41489649838808));
#51563=CARTESIAN_POINT('Ctrl Pts',(4.41962544439486,-0.319434907277294,
5.41375469060185));
#51564=CARTESIAN_POINT('Ctrl Pts',(4.37897528911165,-0.158333333333399,
5.42445428554484));
#51565=CARTESIAN_POINT('Ctrl Pts',(4.36691981565501,0.158333333333401,5.39507877025299));
#51566=CARTESIAN_POINT('Ctrl Pts',(4.39512779232409,0.319434907277302,5.35411223658114));
#51567=CARTESIAN_POINT('Ctrl Pts',(4.44577463236498,0.636309800095475,5.29723400018175));
#51568=CARTESIAN_POINT('Ctrl Pts',(4.49796376419975,0.794772684001176,5.24865657877164));
#51569=CARTESIAN_POINT('Ctrl Pts',(4.54909160096736,1.06847604194559,5.23183655050129));
#51570=CARTESIAN_POINT('Ctrl Pts',(4.56734349850341,1.18514270861234,5.23590627755165));
#51571=CARTESIAN_POINT('Ctrl Pts',(4.58171594751187,1.30000000000064,5.2513264986471));
#51572=CARTESIAN_POINT('Ctrl Pts',(4.66975770319508,-1.30000000000189,5.47508963792264));
#51573=CARTESIAN_POINT('Ctrl Pts',(4.6509638121167,-1.18514270861319,5.44558817224115));
#51574=CARTESIAN_POINT('Ctrl Pts',(4.62692864703389,-1.06847604194603,5.42510290197827));
#51575=CARTESIAN_POINT('Ctrl Pts',(4.55929421601096,-0.794772684001185,
5.39860704470745));
#51576=CARTESIAN_POINT('Ctrl Pts',(4.49347380603036,-0.636309800095465,
5.41557246512998));
#51577=CARTESIAN_POINT('Ctrl Pts',(4.41904815444869,-0.319434907277294,
5.41441990348809));
#51578=CARTESIAN_POINT('Ctrl Pts',(4.37841168271835,-0.158333333333399,
5.42507538042472));
#51579=CARTESIAN_POINT('Ctrl Pts',(4.36636475283526,0.158333333333401,5.39571233267948));
#51580=CARTESIAN_POINT('Ctrl Pts',(4.3945733925091,0.319434907277302,5.35481174037171));
#51581=CARTESIAN_POINT('Ctrl Pts',(4.44523618562804,0.636309800095475,5.2979505962091));
#51582=CARTESIAN_POINT('Ctrl Pts',(4.49740972306233,0.794772684001175,5.24938503158791));
#51583=CARTESIAN_POINT('Ctrl Pts',(4.54861403658599,1.06847604194559,5.2324697634132));
#51584=CARTESIAN_POINT('Ctrl Pts',(4.56691733345257,1.18514270861234,5.23647329586455));
#51585=CARTESIAN_POINT('Ctrl Pts',(4.58135947716816,1.30000000000064,5.2518023535876));
#51586=CARTESIAN_POINT('Ctrl Pts',(4.66937366746064,-1.30000000000189,5.47552778045089));
#51587=CARTESIAN_POINT('Ctrl Pts',(4.65051669169493,-1.18514270861319,5.44612915188768));
#51588=CARTESIAN_POINT('Ctrl Pts',(4.62643396503698,-1.06847604194603,5.42571666422186));
#51589=CARTESIAN_POINT('Ctrl Pts',(4.55872551875528,-0.794772684001185,
5.399319517354));
#51590=CARTESIAN_POINT('Ctrl Pts',(4.4929061657213,-0.636309800095465,5.41624725734922));
#51591=CARTESIAN_POINT('Ctrl Pts',(4.41847055766395,-0.319434907277293,
5.415084614726));
#51592=CARTESIAN_POINT('Ctrl Pts',(4.37784863172277,-0.158333333333399,
5.42569733153273));
#51593=CARTESIAN_POINT('Ctrl Pts',(4.3658103170721,0.158333333333401,5.39634687308374));
#51594=CARTESIAN_POINT('Ctrl Pts',(4.394018749592,0.319434907277302,5.35551085962946));
#51595=CARTESIAN_POINT('Ctrl Pts',(4.4446973896353,0.636309800095474,5.29866664025922));
#51596=CARTESIAN_POINT('Ctrl Pts',(4.49685595516693,0.794772684001175,5.25011389565956));
#51597=CARTESIAN_POINT('Ctrl Pts',(4.548136841441,1.06847604194559,5.23310354460809));
#51598=CARTESIAN_POINT('Ctrl Pts',(4.56649148995048,1.18514270861234,5.23704081452944));
#51599=CARTESIAN_POINT('Ctrl Pts',(4.58100319144551,1.30000000000064,5.25227850504666));
#51600=CARTESIAN_POINT('Ctrl Pts',(4.66860424610756,-1.30000000000189,5.47640181124463));
#51601=CARTESIAN_POINT('Ctrl Pts',(4.64962043429344,-1.18514270861319,5.4472078224012));
#51602=CARTESIAN_POINT('Ctrl Pts',(4.62544222348014,-1.06847604194603,5.4269403525071));
#51603=CARTESIAN_POINT('Ctrl Pts',(4.557585618843,-0.794772684001185,5.40074048707532));
#51604=CARTESIAN_POINT('Ctrl Pts',(4.49176959485631,-0.636309800095465,
5.41759484605104));
#51605=CARTESIAN_POINT('Ctrl Pts',(4.4173144942221,-0.319434907277294,5.41641276937917));
#51606=CARTESIAN_POINT('Ctrl Pts',(4.37672145967416,-0.158333333333399,
5.42693966204847));
#51607=CARTESIAN_POINT('Ctrl Pts',(4.36470027204301,0.158333333333401,5.39761426227359));
#51608=CARTESIAN_POINT('Ctrl Pts',(4.39290776017728,0.319434907277302,5.3569066287119));
#51609=CARTESIAN_POINT('Ctrl Pts',(4.44361873976636,0.636309800095475,5.30009724581093));
#51610=CARTESIAN_POINT('Ctrl Pts',(4.49574912285305,0.794772684001176,5.25157279731524));
#51611=CARTESIAN_POINT('Ctrl Pts',(4.54718351306965,1.06847604194559,5.23437279429459));
#51612=CARTESIAN_POINT('Ctrl Pts',(4.56564069312157,1.18514270861234,5.23817726141035));
#51613=CARTESIAN_POINT('Ctrl Pts',(4.58029101153264,1.30000000000064,5.25323143962657));
#51614=CARTESIAN_POINT('Ctrl Pts',(4.66693219276478,-1.30000000000189,5.47828738177555));
#51615=CARTESIAN_POINT('Ctrl Pts',(4.64766935794,-1.18514270861319,5.44952990506921));
#51616=CARTESIAN_POINT('Ctrl Pts',(4.62328180500171,-1.06847604194603,5.42957265493046));
#51617=CARTESIAN_POINT('Ctrl Pts',(4.55510255496264,-0.794772684001184,
5.4037976985262));
#51618=CARTESIAN_POINT('Ctrl Pts',(4.48929899212577,-0.636309800095464,
5.42050187043342));
#51619=CARTESIAN_POINT('Ctrl Pts',(4.41480542526063,-0.319434907277293,
5.41928396473858));
#51620=CARTESIAN_POINT('Ctrl Pts',(4.37427829715946,-0.158333333333399,
5.42963015579167));
#51621=CARTESIAN_POINT('Ctrl Pts',(4.36229409858572,0.158333333333401,5.40035906140909));
#51622=CARTESIAN_POINT('Ctrl Pts',(4.39049315721296,0.319434907277301,5.35991979077081));
#51623=CARTESIAN_POINT('Ctrl Pts',(4.44127621473851,0.636309800095473,5.30318890946986));
#51624=CARTESIAN_POINT('Ctrl Pts',(4.49335565797689,0.794772684001174,5.25474111672184));
#51625=CARTESIAN_POINT('Ctrl Pts',(4.5451243536289,1.06847604194559,5.23713274866849));
#51626=CARTESIAN_POINT('Ctrl Pts',(4.56380264041945,1.18514270861233,5.24064786127112));
#51627=CARTESIAN_POINT('Ctrl Pts',(4.57875046387201,1.30000000000064,5.25530009655232));
#51628=CARTESIAN_POINT('Ctrl Pts',(4.66433918992144,-1.30000000000188,5.48115537773742));
#51629=CARTESIAN_POINT('Ctrl Pts',(4.64462219001566,-1.18514270861318,5.45302835129213));
#51630=CARTESIAN_POINT('Ctrl Pts',(4.61989798918264,-1.06847604194602,5.43352436265774));
#51631=CARTESIAN_POINT('Ctrl Pts',(4.55121250337003,-0.794772684001181,
5.40838718952874));
#51632=CARTESIAN_POINT('Ctrl Pts',(4.48545813985766,-0.636309800095462,
5.42491067930126));
#51633=CARTESIAN_POINT('Ctrl Pts',(4.41092879968034,-0.319434907277292,
5.42367627998968));
#51634=CARTESIAN_POINT('Ctrl Pts',(4.37052608002569,-0.158333333333399,
5.43378096763672));
#51635=CARTESIAN_POINT('Ctrl Pts',(4.35859759217659,0.1583333333334,5.4045925269395));
#51636=CARTESIAN_POINT('Ctrl Pts',(4.38674242879302,0.3194349072773,5.36450256247766));
#51637=CARTESIAN_POINT('Ctrl Pts',(4.43764525238439,0.636309800095472,5.30790530752386));
#51638=CARTESIAN_POINT('Ctrl Pts',(4.48970501358236,0.794772684001172,5.25966391154349));
#51639=CARTESIAN_POINT('Ctrl Pts',(4.54199635107428,1.06847604194559,5.24143965836856));
#51640=CARTESIAN_POINT('Ctrl Pts',(4.561007966488,1.18514270861233,5.24449923967641));
#51641=CARTESIAN_POINT('Ctrl Pts',(4.5763962149002,1.30000000000063,5.25850700621639));
#51642=CARTESIAN_POINT('Ctrl Pts',(4.66172094582562,-1.30000000000188,5.48398442088032));
#51643=CARTESIAN_POINT('Ctrl Pts',(4.64150899348046,-1.18514270861318,5.45641999848686));
#51644=CARTESIAN_POINT('Ctrl Pts',(4.61642395834516,-1.06847604194602,5.43732907294139));
#51645=CARTESIAN_POINT('Ctrl Pts',(4.54721471283658,-0.794772684001179,
5.41280068864089));
#51646=CARTESIAN_POINT('Ctrl Pts',(4.48155516606521,-0.63630980009546,5.4292202247029));
#51647=CARTESIAN_POINT('Ctrl Pts',(4.40702933723865,-0.319434907277291,
5.42803369794112));
#51648=CARTESIAN_POINT('Ctrl Pts',(4.36679451875707,-0.158333333333398,
5.43796559955891));
#51649=CARTESIAN_POINT('Ctrl Pts',(4.35491993278884,0.1583333333334,5.40885853892069));
#51650=CARTESIAN_POINT('Ctrl Pts',(4.38293867732819,0.319434907277299,5.36900727587747));
#51651=CARTESIAN_POINT('Ctrl Pts',(4.43397241595115,0.63630980009547,5.31255941411302));
#51652=CARTESIAN_POINT('Ctrl Pts',(4.48610689373479,0.794772684001169,5.26466634500749));
#51653=CARTESIAN_POINT('Ctrl Pts',(4.53893316513018,1.06847604194558,5.24584450419028));
#51654=CARTESIAN_POINT('Ctrl Pts',(4.55826670494919,1.18514270861233,5.24843138609822));
#51655=CARTESIAN_POINT('Ctrl Pts',(4.57406724910643,1.30000000000063,5.26175242738594));
#51656=CARTESIAN_POINT('Ctrl Pts',(4.65961765599959,-1.30000000000188,5.4862348200152));
#51657=CARTESIAN_POINT('Ctrl Pts',(4.63899451884016,-1.18514270861318,5.45909535878768));
#51658=CARTESIAN_POINT('Ctrl Pts',(4.61361138707586,-1.06847604194602,5.44031933916282));
#51659=CARTESIAN_POINT('Ctrl Pts',(4.54397473505142,-0.794772684001178,
5.41626420090247));
#51660=CARTESIAN_POINT('Ctrl Pts',(4.47840478660175,-0.63630980009546,5.43262355317404));
#51661=CARTESIAN_POINT('Ctrl Pts',(4.40389466358109,-0.319434907277291,
5.43149635883522));
#51662=CARTESIAN_POINT('Ctrl Pts',(4.36381059902997,-0.158333333333398,
5.44131593587122));
#51663=CARTESIAN_POINT('Ctrl Pts',(4.35197931163416,0.1583333333334,5.41227511086386));
#51664=CARTESIAN_POINT('Ctrl Pts',(4.37987298285693,0.319434907277299,5.37257818907799));
#51665=CARTESIAN_POINT('Ctrl Pts',(4.43101509826136,0.636309800095469,5.31625524436967));
#51666=CARTESIAN_POINT('Ctrl Pts',(4.48323929908517,0.794772684001169,5.26868557276865));
#51667=CARTESIAN_POINT('Ctrl Pts',(4.53649974833629,1.06847604194558,5.24939489077834));
#51668=CARTESIAN_POINT('Ctrl Pts',(4.55608872115211,1.18514270861233,5.25160041987816));
#51669=CARTESIAN_POINT('Ctrl Pts',(4.57221219179707,1.30000000000063,5.26436169952119));
#51670=CARTESIAN_POINT('Ctrl Pts',(4.65645802341575,-1.30000000000188,5.48960367750286));
#51671=CARTESIAN_POINT('Ctrl Pts',(4.63520906889767,-1.18514270861318,5.46308670277238));
#51672=CARTESIAN_POINT('Ctrl Pts',(4.6093729641242,-1.06847604194601,5.44477340173828));
#51673=CARTESIAN_POINT('Ctrl Pts',(4.53908915885635,-0.794772684001175,
5.42141814016419));
#51674=CARTESIAN_POINT('Ctrl Pts',(4.47366052691697,-0.636309800095458,
5.43769880485434));
#51675=CARTESIAN_POINT('Ctrl Pts',(4.39917939959728,-0.31943490727729,5.43666934906166));
#51676=CARTESIAN_POINT('Ctrl Pts',(4.3593286810474,-0.158333333333397,5.4463314264387));
#51677=CARTESIAN_POINT('Ctrl Pts',(4.3475623901759,0.158333333333399,5.41739068141055));
#51678=CARTESIAN_POINT('Ctrl Pts',(4.37525716574878,0.319434907277298,5.37790894068853));
#51679=CARTESIAN_POINT('Ctrl Pts',(4.42656489904725,0.636309800095467,5.32177847598885));
#51680=CARTESIAN_POINT('Ctrl Pts',(4.47894022941081,0.794772684001166,5.27471890995798));
#51681=CARTESIAN_POINT('Ctrl Pts',(4.53285528563043,1.06847604194558,5.25472980658627));
#51682=CARTESIAN_POINT('Ctrl Pts',(4.55282607501066,1.18514270861232,5.25636110693174));
#51683=CARTESIAN_POINT('Ctrl Pts',(4.56942982368338,1.30000000000062,5.26827624980302));
#51684=CARTESIAN_POINT('Ctrl Pts',(4.65172118736733,-1.30000000000187,5.49466426294768));
#51685=CARTESIAN_POINT('Ctrl Pts',(4.62953530745722,-1.18514270861317,5.46908539104944));
#51686=CARTESIAN_POINT('Ctrl Pts',(4.60301728186944,-1.06847604194601,5.45146296630844));
#51687=CARTESIAN_POINT('Ctrl Pts',(4.53174721469078,-0.794772684001171,
5.42913262441784));
#51688=CARTESIAN_POINT('Ctrl Pts',(4.46649976982099,-0.636309800095454,
5.44524266254511));
#51689=CARTESIAN_POINT('Ctrl Pts',(4.39204489191104,-0.319434907277288,
5.44433103317628));
#51690=CARTESIAN_POINT('Ctrl Pts',(4.35254308403161,-0.158333333333397,
5.45375490248664));
#51691=CARTESIAN_POINT('Ctrl Pts',(4.340883637343,0.158333333333398,5.4249812631589));
#51692=CARTESIAN_POINT('Ctrl Pts',(4.36831059437072,0.319434907277296,5.38587428192443));
#51693=CARTESIAN_POINT('Ctrl Pts',(4.41986216725414,0.636309800095464,5.33002860994802));
#51694=CARTESIAN_POINT('Ctrl Pts',(4.47240823278967,0.794772684001162,5.28364794370393));
#51695=CARTESIAN_POINT('Ctrl Pts',(4.52732036069452,1.06847604194557,5.26263427823024));
#51696=CARTESIAN_POINT('Ctrl Pts',(4.54788509653285,1.18514270861232,5.26343644066977));
#51697=CARTESIAN_POINT('Ctrl Pts',(4.56524514273436,1.30000000000062,5.27413680269932));
#51698=CARTESIAN_POINT('Ctrl Pts',(4.64343731377181,-1.30000000000185,5.50388797998165));
#51699=CARTESIAN_POINT('Ctrl Pts',(4.61978873133986,-1.18514270861316,5.48031998362622));
#51700=CARTESIAN_POINT('Ctrl Pts',(4.59217046718998,-1.068476041946,5.46411584541671));
#51701=CARTESIAN_POINT('Ctrl Pts',(4.51919599308853,-0.794772684001161,
5.4436930299779));
#51702=CARTESIAN_POINT('Ctrl Pts',(4.45400261297904,-0.636309800095446,
5.45904661482441));
#51703=CARTESIAN_POINT('Ctrl Pts',(4.37931066061378,-0.319434907277284,
5.45787638034737));
#51704=CARTESIAN_POINT('Ctrl Pts',(4.34010869977133,-0.158333333333395,
5.46635690222688));
#51705=CARTESIAN_POINT('Ctrl Pts',(4.32863248605252,0.158333333333396,5.43786714965165));
#51706=CARTESIAN_POINT('Ctrl Pts',(4.35603805714203,0.319434907277293,5.40015099671855));
#51707=CARTESIAN_POINT('Ctrl Pts',(4.40800596400493,0.636309800095456,5.34480895728543));
#51708=CARTESIAN_POINT('Ctrl Pts',(4.46036003808239,0.794772684001151,5.29889952382618));
#51709=CARTESIAN_POINT('Ctrl Pts',(4.51699995807158,1.06847604194556,5.27599065917723));
#51710=CARTESIAN_POINT('Ctrl Pts',(4.5386892684419,1.1851427086123,5.27541374926672));
#51711=CARTESIAN_POINT('Ctrl Pts',(4.55755056653508,1.3000000000006,5.28417632809513));
#51712=CARTESIAN_POINT('Ctrl Pts',(4.63309485448232,-1.3000000000018,5.51545665194679));
#51713=CARTESIAN_POINT('Ctrl Pts',(4.60760364164271,-1.18514270861311,5.49438368210212));
#51714=CARTESIAN_POINT('Ctrl Pts',(4.57860822372549,-1.06847604194595,5.47995294952138));
#51715=CARTESIAN_POINT('Ctrl Pts',(4.50352759308024,-0.794772684001128,
5.46195996725641));
#51716=CARTESIAN_POINT('Ctrl Pts',(4.43847086903231,-0.63630980009542,5.47648406203382));
#51717=CARTESIAN_POINT('Ctrl Pts',(4.36352655275373,-0.319434907277271,
5.47505714380749));
#51718=CARTESIAN_POINT('Ctrl Pts',(4.32474324350625,-0.158333333333388,
5.48241472934437));
#51719=CARTESIAN_POINT('Ctrl Pts',(4.31342386194375,0.15833333333339,5.45416031427122));
#51720=CARTESIAN_POINT('Ctrl Pts',(4.34057405669332,0.319434907277279,5.41782832862097));
#51721=CARTESIAN_POINT('Ctrl Pts',(4.39310065915147,0.636309800095429,5.36316959541494));
#51722=CARTESIAN_POINT('Ctrl Pts',(4.44553030973306,0.794772684001119,5.31832839198243));
#51723=CARTESIAN_POINT('Ctrl Pts',(4.50441545219899,1.06847604194552,5.29318734209524));
#51724=CARTESIAN_POINT('Ctrl Pts',(4.52750125039646,1.18514270861225,5.29087758351447));
#51725=CARTESIAN_POINT('Ctrl Pts',(4.54818365052745,1.30000000000055,5.29714069528139));
#51726=CARTESIAN_POINT('Ctrl Pts',(4.6161176146744,-1.30000000000174,5.53325242217053));
#51727=CARTESIAN_POINT('Ctrl Pts',(4.58732595215133,-1.18514270861306,5.51558939620259));
#51728=CARTESIAN_POINT('Ctrl Pts',(4.55588209662729,-1.06847604194591,5.50359082894549));
#51729=CARTESIAN_POINT('Ctrl Pts',(4.47711340364355,-0.794772684001098,
5.48895777106956));
#51730=CARTESIAN_POINT('Ctrl Pts',(4.41230604183178,-0.636309800095395,
5.50219354548612));
#51731=CARTESIAN_POINT('Ctrl Pts',(4.33727355937462,-0.319434907277259,
5.50089227085189));
#51732=CARTESIAN_POINT('Ctrl Pts',(4.29971762482629,-0.158333333333382,
5.50740221834196));
#51733=CARTESIAN_POINT('Ctrl Pts',(4.28903017588411,0.158333333333384,5.48017967903576));
#51734=CARTESIAN_POINT('Ctrl Pts',(4.3159463033878,0.319434907277267,5.44634259540802));
#51735=CARTESIAN_POINT('Ctrl Pts',(4.36911217875662,0.636309800095405,5.39240657377784));
#51736=CARTESIAN_POINT('Ctrl Pts',(4.42082888974231,0.794772684001087,5.34800452472138));
#51737=CARTESIAN_POINT('Ctrl Pts',(4.48315348314286,1.06847604194547,5.31902371701114));
#51738=CARTESIAN_POINT('Ctrl Pts',(4.5085608872895,1.18514270861221,5.31404943712708));
#51739=CARTESIAN_POINT('Ctrl Pts',(4.53239768845348,1.3000000000005,5.31664559517197));
#51740=CARTESIAN_POINT('Ctrl Pts',(4.59914282463979,-1.30000000000162,5.5510909883858));
#51741=CARTESIAN_POINT('Ctrl Pts',(4.56702672616545,-1.18514270861294,5.53679389600347));
#51742=CARTESIAN_POINT('Ctrl Pts',(4.53317405091121,-1.0684760419458,5.52729541184619));
#51743=CARTESIAN_POINT('Ctrl Pts',(4.450955759107,-0.79477268400102,5.51643775823578));
#51744=CARTESIAN_POINT('Ctrl Pts',(4.38699771120582,-0.636309800095331,
5.52943437329957));
#51745=CARTESIAN_POINT('Ctrl Pts',(4.31187329989311,-0.319434907277225,
5.52825583955045));
#51746=CARTESIAN_POINT('Ctrl Pts',(4.27518623909131,-0.158333333333365,
5.53326785410993));
#51747=CARTESIAN_POINT('Ctrl Pts',(4.26446568816465,0.158333333333367,5.50597675500226));
#51748=CARTESIAN_POINT('Ctrl Pts',(4.29019729726968,0.319434907277233,5.47312013259392));
#51749=CARTESIAN_POINT('Ctrl Pts',(4.34396319420537,0.636309800095338,5.41983611993691));
#51750=CARTESIAN_POINT('Ctrl Pts',(4.3960664930059,0.794772684001007,5.37762997047923));
#51751=CARTESIAN_POINT('Ctrl Pts',(4.46218061828739,1.06847604194536,5.34536762855042));
#51752=CARTESIAN_POINT('Ctrl Pts',(4.48992864601964,1.18514270861209,5.33775927694476));
#51753=CARTESIAN_POINT('Ctrl Pts',(4.51680634641956,1.30000000000036,5.33650774611683));
#51754=CARTESIAN_POINT('Ctrl Pts',(4.58425706155024,-1.30000000000161,5.56666693784608));
#51755=CARTESIAN_POINT('Ctrl Pts',(4.54934641908668,-1.18514270861293,5.55555096597518));
#51756=CARTESIAN_POINT('Ctrl Pts',(4.51334321280132,-1.0684760419458,5.54818858475124));
#51757=CARTESIAN_POINT('Ctrl Pts',(4.42764456287057,-0.794772684001015,
5.53985155658237));
#51758=CARTESIAN_POINT('Ctrl Pts',(4.36323699882183,-0.636309800095328,
5.55051525689881));
#51759=CARTESIAN_POINT('Ctrl Pts',(4.28775589540894,-0.319434907277225,
5.54896405460372));
#51760=CARTESIAN_POINT('Ctrl Pts',(4.25232434093199,-0.158333333333365,
5.55356099824275));
#51761=CARTESIAN_POINT('Ctrl Pts',(4.24222446884936,0.158333333333367,5.52734280767035));
#51762=CARTESIAN_POINT('Ctrl Pts',(4.26761085002562,0.319434907277234,5.49652744853665));
#51763=CARTESIAN_POINT('Ctrl Pts',(4.32240782374077,0.636309800095338,5.44467454255857));
#51764=CARTESIAN_POINT('Ctrl Pts',(4.37485911402526,0.794772684001005,5.40439130860367));
#51765=CARTESIAN_POINT('Ctrl Pts',(4.44419613943937,1.06847604194536,5.36908451924072));
#51766=CARTESIAN_POINT('Ctrl Pts',(4.47387959944389,1.18514270861208,5.358972935203));
#51767=CARTESIAN_POINT('Ctrl Pts',(4.50323309034115,1.30000000000036,5.35403276799731));
#51768=CARTESIAN_POINT('Ctrl Pts',(4.57558856625113,-1.3000000000016,5.57530232637884));
#51769=CARTESIAN_POINT('Ctrl Pts',(4.53881326219513,-1.18514270861292,5.56552049733167));
#51770=CARTESIAN_POINT('Ctrl Pts',(4.50148536593342,-1.06847604194579,5.55920339728274));
#51771=CARTESIAN_POINT('Ctrl Pts',(4.41397385960811,-0.794772684001007,
5.5526138495408));
#51772=CARTESIAN_POINT('Ctrl Pts',(4.35029675070984,-0.636309800095322,
5.56370748004289));
#51773=CARTESIAN_POINT('Ctrl Pts',(4.2748039665828,-0.319434907277222,5.56228315938248));
#51774=CARTESIAN_POINT('Ctrl Pts',(4.23967479680681,-0.158333333333364,
5.56588570353577));
#51775=CARTESIAN_POINT('Ctrl Pts',(4.22947881187277,0.158333333333365,5.53950259976342));
#51776=CARTESIAN_POINT('Ctrl Pts',(4.25430888765728,0.31943490727723,5.50924503607498));
#51777=CARTESIAN_POINT('Ctrl Pts',(4.30924321033487,0.636309800095331,5.45748274682784));
#51778=CARTESIAN_POINT('Ctrl Pts',(4.36152013083792,0.794772684000997,5.41775682917475));
#51779=CARTESIAN_POINT('Ctrl Pts',(4.43281265088734,1.06847604194535,5.38089753337119));
#51780=CARTESIAN_POINT('Ctrl Pts',(4.46379355744217,1.18514270861207,5.36965480595422));
#51781=CARTESIAN_POINT('Ctrl Pts',(4.49489548027066,1.30000000000035,5.36312437450212));
#51782=CARTESIAN_POINT('Ctrl Pts',(4.56261230358745,-1.30000000000158,5.58829235114902));
#51783=CARTESIAN_POINT('Ctrl Pts',(4.5231919902109,-1.18514270861291,5.58079144907158));
#51784=CARTESIAN_POINT('Ctrl Pts',(4.48391086259223,-1.06847604194578,5.57610915203169));
#51785=CARTESIAN_POINT('Ctrl Pts',(4.39348514657536,-0.794772684001001,
5.57180365067601));
#51786=CARTESIAN_POINT('Ctrl Pts',(4.33020120361279,-0.636309800095317,
5.58229128160804));
#51787=CARTESIAN_POINT('Ctrl Pts',(4.25444104633124,-0.319434907277219,
5.58061017277558));
#51788=CARTESIAN_POINT('Ctrl Pts',(4.21974659764685,-0.158333333333363,
5.58269369541246));
#51789=CARTESIAN_POINT('Ctrl Pts',(4.20999271078741,0.158333333333364,5.55707577920068));
#51790=CARTESIAN_POINT('Ctrl Pts',(4.23503288483197,0.319434907277228,5.52947251411293));
#51791=CARTESIAN_POINT('Ctrl Pts',(4.29072217396501,0.636309800095328,5.47877179929094));
#51792=CARTESIAN_POINT('Ctrl Pts',(4.34248883596468,0.794772684000991,5.43939020400205));
#51793=CARTESIAN_POINT('Ctrl Pts',(4.41662435868359,1.06847604194534,5.40004809333104));
#51794=CARTESIAN_POINT('Ctrl Pts',(4.4494865285756,1.18514270861206,5.38701200335624));
#51795=CARTESIAN_POINT('Ctrl Pts',(4.48312034756644,1.30000000000033,5.37796956534724));
#51796=CARTESIAN_POINT('Ctrl Pts',(4.54301380784669,-1.30000000000155,5.60754561873799));
#51797=CARTESIAN_POINT('Ctrl Pts',(4.49979258745065,-1.18514270861288,5.60379481597793));
#51798=CARTESIAN_POINT('Ctrl Pts',(4.45765702292381,-1.06847604194574,5.60171611997361));
#51799=CARTESIAN_POINT('Ctrl Pts',(4.36282352191878,-0.794772684000976,
5.60077681747148));
#51800=CARTESIAN_POINT('Ctrl Pts',(4.29958263496403,-0.636309800095297,
5.60931453785102));
#51801=CARTESIAN_POINT('Ctrl Pts',(4.2234914941984,-0.319434907277209,5.60736584564812));
#51802=CARTESIAN_POINT('Ctrl Pts',(4.19031554805787,-0.158333333333357,
5.6087274109245));
#51803=CARTESIAN_POINT('Ctrl Pts',(4.1808176578041,0.158333333333359,5.58359711196709));
#51804=CARTESIAN_POINT('Ctrl Pts',(4.20454998114033,0.319434907277217,5.55719162544147));
#51805=CARTESIAN_POINT('Ctrl Pts',(4.26118406444266,0.636309800095306,5.50777576293752));
#51806=CARTESIAN_POINT('Ctrl Pts',(4.3135833993088,0.794772684000966,5.47132072006254));
#51807=CARTESIAN_POINT('Ctrl Pts',(4.39229505523178,1.06847604194531,5.42878365567674));
#51808=CARTESIAN_POINT('Ctrl Pts',(4.42792972501858,1.18514270861202,5.41296560669806));
#51809=CARTESIAN_POINT('Ctrl Pts',(4.46512770529741,1.3000000000003,5.39974222775972));
#51810=CARTESIAN_POINT('Ctrl Pts',(4.516298972992,-1.3000000000015,5.63216227364944));
#51811=CARTESIAN_POINT('Ctrl Pts',(4.46765342605821,-1.18514270861284,5.6327703562665));
#51812=CARTESIAN_POINT('Ctrl Pts',(4.42152401198595,-1.06847604194572,5.63383083869071));
#51813=CARTESIAN_POINT('Ctrl Pts',(4.32076860758239,-0.794772684000958,
5.63732589929622));
#51814=CARTESIAN_POINT('Ctrl Pts',(4.25845143957159,-0.636309800095281,
5.64488057483907));
#51815=CARTESIAN_POINT('Ctrl Pts',(4.18182204396956,-0.3194349072772,5.64240443057221));
#51816=CARTESIAN_POINT('Ctrl Pts',(4.14971614301137,-0.158333333333353,
5.64102184400878));
#51817=CARTESIAN_POINT('Ctrl Pts',(4.14053077540987,0.158333333333355,5.61649581157307));
#51818=CARTESIAN_POINT('Ctrl Pts',(4.16351040483269,0.319434907277211,5.59349208043877));
#51819=CARTESIAN_POINT('Ctrl Pts',(4.22130949356724,0.636309800095291,5.54572587370549));
#51820=CARTESIAN_POINT('Ctrl Pts',(4.27328072613241,0.794772684000945,5.51108618839217));
#51821=CARTESIAN_POINT('Ctrl Pts',(4.35813807793187,1.06847604194528,5.46435842093235));
#51822=CARTESIAN_POINT('Ctrl Pts',(4.3977545667793,1.18514270861199,5.44528778384203));
#51823=CARTESIAN_POINT('Ctrl Pts',(4.44025594115493,1.30000000000026,5.4273732287603));
#51824=CARTESIAN_POINT('Ctrl Pts',(4.4943385548838,-1.30000000000144,5.65331652551978));
#51825=CARTESIAN_POINT('Ctrl Pts',(4.44111925554601,-1.18514270861278,5.65742385386435));
#51826=CARTESIAN_POINT('Ctrl Pts',(4.39153931856661,-1.06847604194566,5.66084062336221));
#51827=CARTESIAN_POINT('Ctrl Pts',(4.28540740081183,-0.794772684000913,
5.66713871534291));
#51828=CARTESIAN_POINT('Ctrl Pts',(4.22308865148336,-0.636309800095247,
5.67239269145178));
#51829=CARTESIAN_POINT('Ctrl Pts',(4.14584564055604,-0.319434907277184,
5.66911903350957));
#51830=CARTESIAN_POINT('Ctrl Pts',(4.11518564330417,-0.158333333333345,
5.66644082444016));
#51831=CARTESIAN_POINT('Ctrl Pts',(4.10641616714155,0.158333333333347,5.64275210326189));
#51832=CARTESIAN_POINT('Ctrl Pts',(4.12836718487157,0.319434907277194,5.62197732139297));
#51833=CARTESIAN_POINT('Ctrl Pts',(4.18762417697754,0.636309800095258,5.57651859441387));
#51834=CARTESIAN_POINT('Ctrl Pts',(4.24049473217301,0.794772684000904,5.54559351084376));
#51835=CARTESIAN_POINT('Ctrl Pts',(4.33065336907891,1.06847604194522,5.495734264183));
#51836=CARTESIAN_POINT('Ctrl Pts',(4.3734134672318,1.18514270861193,5.47366901455216));
#51837=CARTESIAN_POINT('Ctrl Pts',(4.41990733032775,1.30000000000019,5.45112073570273));
#51838=CARTESIAN_POINT('Ctrl Pts',(4.47582949985432,-1.30000000000144,5.66843433384013));
#51839=CARTESIAN_POINT('Ctrl Pts',(4.41879406299081,-1.18514270861278,5.67510274423551));
#51840=CARTESIAN_POINT('Ctrl Pts',(4.36638556973584,-1.06847604194566,5.68031676220333));
#51841=CARTESIAN_POINT('Ctrl Pts',(4.25600063138655,-0.79477268400091,5.68900224931184));
#51842=CARTESIAN_POINT('Ctrl Pts',(4.19404971549608,-0.636309800095244,
5.6930639368886));
#51843=CARTESIAN_POINT('Ctrl Pts',(4.11659846569157,-0.319434907277182,
5.68972467519604));
#51844=CARTESIAN_POINT('Ctrl Pts',(4.08725497155438,-0.158333333333344,
5.68638447927321));
#51845=CARTESIAN_POINT('Ctrl Pts',(4.07885160595465,0.158333333333346,5.66346590183524));
#51846=CARTESIAN_POINT('Ctrl Pts',(4.09999152136496,0.319434907277193,5.64444220511035));
#51847=CARTESIAN_POINT('Ctrl Pts',(4.15991876903039,0.636309800095255,5.59996812177501));
#51848=CARTESIAN_POINT('Ctrl Pts',(4.2124157915973,0.794772684000898,5.57017371395485));
#51849=CARTESIAN_POINT('Ctrl Pts',(4.30687468477072,1.06847604194522,5.51787148695648));
#51850=CARTESIAN_POINT('Ctrl Pts',(4.35244962590473,1.18514270861193,5.49389380217444));
#51851=CARTESIAN_POINT('Ctrl Pts',(4.40271175336492,1.30000000000019,5.46857812868941));
#51852=CARTESIAN_POINT('Ctrl Pts',(4.45542493556607,-1.30000000000142,5.68625771326939));
#51853=CARTESIAN_POINT('Ctrl Pts',(4.39420635524456,-1.18514270861277,5.69596986392667));
#51854=CARTESIAN_POINT('Ctrl Pts',(4.33864496717878,-1.06847604194565,5.70322160418365));
#51855=CARTESIAN_POINT('Ctrl Pts',(4.22335629155764,-0.794772684000902,
5.71429053465481));
#51856=CARTESIAN_POINT('Ctrl Pts',(4.16157081915296,-0.636309800095236,
5.7165455055085));
#51857=CARTESIAN_POINT('Ctrl Pts',(4.08329064411361,-0.319434907277177,
5.71188878932228));
#51858=CARTESIAN_POINT('Ctrl Pts',(4.05463582269465,-0.158333333333342,
5.70610769473987));
#51859=CARTESIAN_POINT('Ctrl Pts',(4.0465228193423,0.158333333333344,5.68383506722709));
#51860=CARTESIAN_POINT('Ctrl Pts',(4.0673207203027,0.319434907277186,5.66808682426998));
#51861=CARTESIAN_POINT('Ctrl Pts',(4.12855366925288,0.636309800095244,5.6258617737382));
#51862=CARTESIAN_POINT('Ctrl Pts',(4.1810976527764,0.794772684000889,5.5981460706891));
#51863=CARTESIAN_POINT('Ctrl Pts',(4.28062148488611,1.0684760419452,5.54358048255127));
#51864=CARTESIAN_POINT('Ctrl Pts',(4.32936623029481,1.18514270861191,5.51749860208889));
#51865=CARTESIAN_POINT('Ctrl Pts',(4.38377554191335,1.30000000000016,5.48895426241469));
#51866=CARTESIAN_POINT('Ctrl Pts',(4.43225268787918,-1.30000000000137,5.70516072474127));
#51867=CARTESIAN_POINT('Ctrl Pts',(4.36613347470572,-1.18514270861272,5.71785619133634));
#51868=CARTESIAN_POINT('Ctrl Pts',(4.30686656640134,-1.06847604194561,5.72703108182496));
#51869=CARTESIAN_POINT('Ctrl Pts',(4.18577834696053,-0.794772684000878,
5.74009367918948));
#51870=CARTESIAN_POINT('Ctrl Pts',(4.12380303207223,-0.636309800095214,
5.73940093161573));
#51871=CARTESIAN_POINT('Ctrl Pts',(4.04506367699879,-0.319434907277166,
5.73425187114617));
#51872=CARTESIAN_POINT('Ctrl Pts',(4.01851537171127,-0.158333333333337,
5.72864632025602));
#51873=CARTESIAN_POINT('Ctrl Pts',(4.01088922296883,0.158333333333339,5.70750320497276));
#51874=CARTESIAN_POINT('Ctrl Pts',(4.03021207820231,0.319434907277177,5.69314302340603));
#51875=CARTESIAN_POINT('Ctrl Pts',(4.09260132301132,0.636309800095224,5.65282683635549));
#51876=CARTESIAN_POINT('Ctrl Pts',(4.14568293805015,0.794772684000862,5.62844713099643));
#51877=CARTESIAN_POINT('Ctrl Pts',(4.2508220265062,1.06847604194517,5.57127723847806));
#51878=CARTESIAN_POINT('Ctrl Pts',(4.30301548770747,1.18514270861186,5.54265797204684));
#51879=CARTESIAN_POINT('Ctrl Pts',(4.36189159450457,1.30000000000012,5.51016616730232));
#51880=CARTESIAN_POINT('Ctrl Pts',(4.4090851760024,-1.30000000000137,5.72400020051124));
#51881=CARTESIAN_POINT('Ctrl Pts',(4.33802134759834,-1.18514270861272,5.73940830788491));
#51882=CARTESIAN_POINT('Ctrl Pts',(4.27500476704778,-1.0684760419456,5.75027058921371));
#51883=CARTESIAN_POINT('Ctrl Pts',(4.14801461194053,-0.79477268400087,5.7648628645221));
#51884=CARTESIAN_POINT('Ctrl Pts',(4.08597965493875,-0.636309800095212,
5.76144969401772));
#51885=CARTESIAN_POINT('Ctrl Pts',(4.00629549513168,-0.319434907277166,
5.75468117423453));
#51886=CARTESIAN_POINT('Ctrl Pts',(3.98094327595155,-0.158333333333336,
5.74728069400309));
#51887=CARTESIAN_POINT('Ctrl Pts',(3.97361735282597,0.158333333333338,5.72692681989707));
#51888=CARTESIAN_POINT('Ctrl Pts',(3.99214944324806,0.319434907277175,5.71549125834631));
#51889=CARTESIAN_POINT('Ctrl Pts',(4.05588095842403,0.636309800095221,5.67770868694704));
#51890=CARTESIAN_POINT('Ctrl Pts',(4.10903941712925,0.794772684000858,5.65594961861467));
#51891=CARTESIAN_POINT('Ctrl Pts',(4.22016590033604,1.06847604194517,5.5971307493497));
#51892=CARTESIAN_POINT('Ctrl Pts',(4.27612221881426,1.18514270861187,5.56667518822238));
#51893=CARTESIAN_POINT('Ctrl Pts',(4.3399323188325,1.30000000000012,5.53122457501863));
#51894=CARTESIAN_POINT('Ctrl Pts',(4.39231891341342,-1.30000000000136,5.73621537749296));
#51895=CARTESIAN_POINT('Ctrl Pts',(4.31765942975983,-1.18514270861271,5.75357177533912));
#51896=CARTESIAN_POINT('Ctrl Pts',(4.25188676500677,-1.0684760419456,5.76557492280135));
#51897=CARTESIAN_POINT('Ctrl Pts',(4.12046908111323,-0.794772684000867,
5.78093751535959));
#51898=CARTESIAN_POINT('Ctrl Pts',(4.05778038283076,-0.636309800095208,
5.77414225579004));
#51899=CARTESIAN_POINT('Ctrl Pts',(3.97800859932127,-0.319434907277164,
5.76756567149917));
#51900=CARTESIAN_POINT('Ctrl Pts',(3.95520035708981,-0.158333333333335,
5.76269698499336));
#51901=CARTESIAN_POINT('Ctrl Pts',(3.94833518429538,0.158333333333337,5.74349827159986));
#51902=CARTESIAN_POINT('Ctrl Pts',(3.96499427116526,0.319434907277172,5.73128534480092));
#51903=CARTESIAN_POINT('Ctrl Pts',(4.02932371604558,0.636309800095216,5.69444315181794));
#51904=CARTESIAN_POINT('Ctrl Pts',(4.08299019926578,0.794772684000854,5.67546484354474));
#51905=CARTESIAN_POINT('Ctrl Pts',(4.19852158235783,1.06847604194516,5.61556027904465));
#51906=CARTESIAN_POINT('Ctrl Pts',(4.25719705724207,1.18514270861186,5.58376271007258));
#51907=CARTESIAN_POINT('Ctrl Pts',(4.32453875212963,1.30000000000011,5.54609803841764));
#51908=CARTESIAN_POINT('Ctrl Pts',(4.38057663395295,-1.30000000000135,5.74519668890432));
#51909=CARTESIAN_POINT('Ctrl Pts',(4.30317639524159,-1.1851427086127,5.76305837794972));
#51910=CARTESIAN_POINT('Ctrl Pts',(4.23548147494313,-1.06847604194559,5.77559986068481));
#51911=CARTESIAN_POINT('Ctrl Pts',(4.10151389380763,-0.794772684000863,
5.79228245383744));
#51912=CARTESIAN_POINT('Ctrl Pts',(4.03998121252943,-0.636309800095205,
5.7867372046775));
#51913=CARTESIAN_POINT('Ctrl Pts',(3.96053722377183,-0.319434907277163,
5.78098056510057));
#51914=CARTESIAN_POINT('Ctrl Pts',(3.93875704946889,-0.158333333333334,
5.77609714660842));
#51915=CARTESIAN_POINT('Ctrl Pts',(3.93163988064319,0.158333333333336,5.75637324885947));
#51916=CARTESIAN_POINT('Ctrl Pts',(3.9466618734353,0.319434907277171,5.7428622438365));
#51917=CARTESIAN_POINT('Ctrl Pts',(4.01087747043568,0.636309800095214,5.70573468057763));
#51918=CARTESIAN_POINT('Ctrl Pts',(4.06465181025686,0.794772684000851,5.6883983338919));
#51919=CARTESIAN_POINT('Ctrl Pts',(4.18291930551696,1.06847604194515,5.62751390936758));
#51920=CARTESIAN_POINT('Ctrl Pts',(4.24337208879345,1.18514270861185,5.59478575178472));
#51921=CARTESIAN_POINT('Ctrl Pts',(4.31308403889095,1.3000000000001,5.55568404800531));
#51922=CARTESIAN_POINT('Ctrl Pts',(4.36598759938401,-1.30000000000135,5.75520187083884));
#51923=CARTESIAN_POINT('Ctrl Pts',(4.28495371436841,-1.1851427086127,5.77380994737787));
#51924=CARTESIAN_POINT('Ctrl Pts',(4.2147559770505,-1.06847604194558,5.78728839633516));
#51925=CARTESIAN_POINT('Ctrl Pts',(4.07761882978273,-0.794772684000858,
5.80657584388858));
#51926=CARTESIAN_POINT('Ctrl Pts',(4.01795330178055,-0.636309800095201,
5.80392668218628));
#51927=CARTESIAN_POINT('Ctrl Pts',(3.93921907864403,-0.319434907277161,
5.80021298084493));
#51928=CARTESIAN_POINT('Ctrl Pts',(3.91873439854227,-0.158333333333333,
5.7951550993706));
#51929=CARTESIAN_POINT('Ctrl Pts',(3.91163478140379,0.158333333333335,5.77552597077783));
#51930=CARTESIAN_POINT('Ctrl Pts',(3.92521934381218,0.319434907277169,5.76196968775307));
#51931=CARTESIAN_POINT('Ctrl Pts',(3.98908579202181,0.63630980009521,5.72363285871615));
#51932=CARTESIAN_POINT('Ctrl Pts',(4.04179431355421,0.794772684000846,5.70516207961435));
#51933=CARTESIAN_POINT('Ctrl Pts',(4.16337291576826,1.06847604194515,5.64185200560908));
#51934=CARTESIAN_POINT('Ctrl Pts',(4.22622970877727,1.18514270861185,5.60787943748067));
#51935=CARTESIAN_POINT('Ctrl Pts',(4.29931642282803,1.3000000000001,5.56733888639128));
#51936=CARTESIAN_POINT('Ctrl Pts',(4.35610142762914,-1.30000000000134,5.76212147047595));
#51937=CARTESIAN_POINT('Ctrl Pts',(4.27202510729744,-1.18514270861269,5.77999061529273));
#51938=CARTESIAN_POINT('Ctrl Pts',(4.19998727434625,-1.06847604194558,5.79359553631554));
#51939=CARTESIAN_POINT('Ctrl Pts',(4.06137678325034,-0.794772684000851,
5.81517441551416));
#51940=CARTESIAN_POINT('Ctrl Pts',(4.00531418533707,-0.636309800095197,
5.81806199192094));
#51941=CARTESIAN_POINT('Ctrl Pts',(3.92838285750872,-0.319434907277159,
5.81733237660638));
#51942=CARTESIAN_POINT('Ctrl Pts',(3.90875262161207,-0.158333333333332,
5.81160844072743));
#51943=CARTESIAN_POINT('Ctrl Pts',(3.90175138030431,0.158333333333334,5.79210658955772));
#51944=CARTESIAN_POINT('Ctrl Pts',(3.91457783688431,0.319434907277167,5.77918177957112));
#51945=CARTESIAN_POINT('Ctrl Pts',(3.97684592441674,0.636309800095206,5.73844981415392));
#51946=CARTESIAN_POINT('Ctrl Pts',(4.02617203613902,0.79477268400084,5.71559136609044));
#51947=CARTESIAN_POINT('Ctrl Pts',(4.14921392208308,1.06847604194514,5.64994165160661));
#51948=CARTESIAN_POINT('Ctrl Pts',(4.213841201547,1.18514270861184,5.61552978207355));
#51949=CARTESIAN_POINT('Ctrl Pts',(4.28983548720086,1.30000000000009,5.57512337184579));
#51950=CARTESIAN_POINT('Ctrl Pts',(4.35088387761145,-1.30000000000134,5.76896053285544));
#51951=CARTESIAN_POINT('Ctrl Pts',(4.26698198886915,-1.18514270861269,5.78664876365145));
#51952=CARTESIAN_POINT('Ctrl Pts',(4.19526082558516,-1.06847604194558,5.80039023590544));
#51953=CARTESIAN_POINT('Ctrl Pts',(4.05771050318435,-0.794772684000851,
5.82301798400579));
#51954=CARTESIAN_POINT('Ctrl Pts',(4.00307751336492,-0.636309800095197,
5.82803611993916));
#51955=CARTESIAN_POINT('Ctrl Pts',(3.9271390295546,-0.319434907277159,5.82866988923775));
#51956=CARTESIAN_POINT('Ctrl Pts',(3.90745678965039,-0.158333333333332,
5.8229519304616));
#51957=CARTESIAN_POINT('Ctrl Pts',(3.90061191119441,0.158333333333334,5.80362794938222));
#51958=CARTESIAN_POINT('Ctrl Pts',(3.91380906647831,0.319434907277167,5.79110325249133));
#51959=CARTESIAN_POINT('Ctrl Pts',(3.97507215158419,0.636309800095206,5.74890534309992));
#51960=CARTESIAN_POINT('Ctrl Pts',(4.02239198166674,0.79477268400084,5.72299871549042));
#51961=CARTESIAN_POINT('Ctrl Pts',(4.14444540563289,1.06847604194514,5.65643597419594));
#51962=CARTESIAN_POINT('Ctrl Pts',(4.20891602829543,1.18514270861184,5.62216459509058));
#51963=CARTESIAN_POINT('Ctrl Pts',(4.28502486891064,1.30000000000009,5.58243438119359));
#51964=CARTESIAN_POINT('Ctrl Pts',(4.35088387761047,-1.3,5.76896053285564));
#51965=CARTESIAN_POINT('Ctrl Pts',(4.26698198886859,-1.18514270861178,5.78664876365156));
#51966=CARTESIAN_POINT('Ctrl Pts',(4.19526082558493,-1.06847604194512,5.80039023590548));
#51967=CARTESIAN_POINT('Ctrl Pts',(4.05771050318435,-0.794772684000851,
5.8230179840058));
#51968=CARTESIAN_POINT('Ctrl Pts',(4.00307751336492,-0.636309800095197,
5.82803611993916));
#51969=CARTESIAN_POINT('Ctrl Pts',(3.9271390295546,-0.319434907277159,5.82866988923776));
#51970=CARTESIAN_POINT('Ctrl Pts',(3.90745678965039,-0.158333333333332,
5.8229519304616));
#51971=CARTESIAN_POINT('Ctrl Pts',(3.90061191119441,0.158333333333334,5.80362794938222));
#51972=CARTESIAN_POINT('Ctrl Pts',(3.91380906647831,0.319434907277167,5.79110325249133));
#51973=CARTESIAN_POINT('Ctrl Pts',(3.9750721515842,0.636309800095206,5.74890534309992));
#51974=CARTESIAN_POINT('Ctrl Pts',(4.02239198166674,0.79477268400084,5.72299871549042));
#51975=CARTESIAN_POINT('Ctrl Pts',(4.14444540563287,1.06847604194511,5.65643597419595));
#51976=CARTESIAN_POINT('Ctrl Pts',(4.20891602829539,1.18514270861178,5.6221645950906));
#51977=CARTESIAN_POINT('Ctrl Pts',(4.28502486891058,1.3,5.58243438119362));
#51978=CARTESIAN_POINT('',(4.63722129958651,-1.2,5.46833068437959));
#51979=CARTESIAN_POINT('Ctrl Pts',(4.6372212995865,-1.2,5.4683306843796));
#51980=CARTESIAN_POINT('Ctrl Pts',(4.62750586065925,-1.21481068879262,5.48465035288688));
#51981=CARTESIAN_POINT('Ctrl Pts',(4.62725170851186,-1.21549275722123,5.48594687910636));
#51982=CARTESIAN_POINT('Ctrl Pts',(4.6149839274451,-1.23450984640621,5.50765759125053));
#51983=CARTESIAN_POINT('Ctrl Pts',(4.61396625404581,-1.23601256685819,5.50922612580931));
#51984=CARTESIAN_POINT('Ctrl Pts',(4.5936259721994,-1.26668179624999,5.54302123985939));
#51985=CARTESIAN_POINT('Ctrl Pts',(4.58460229424093,-1.28035635399065,5.55832572060974));
#51986=CARTESIAN_POINT('Ctrl Pts',(4.57129987359789,-1.30000000000159,5.57959342582533));
#51987=CARTESIAN_POINT('',(4.58017336234084,-0.65383484141843,5.32263163693194));
#51988=CARTESIAN_POINT('Ctrl Pts',(4.58017336236564,-0.653834841417755,
5.32263163692465));
#51989=CARTESIAN_POINT('Ctrl Pts',(4.58634999591384,-0.718019341709874,
5.33770063084345));
#51990=CARTESIAN_POINT('Ctrl Pts',(4.59130924624133,-0.763830568183498,
5.34995750755485));
#51991=CARTESIAN_POINT('Ctrl Pts',(4.6105027479006,-0.949554209366674,5.39805721041602));
#51992=CARTESIAN_POINT('Ctrl Pts',(4.62071098387629,-1.04816473166287,5.424117862114));
#51993=CARTESIAN_POINT('Ctrl Pts',(4.6372212995865,-1.2,5.46833068437959));
#51994=CARTESIAN_POINT('',(4.52544944337419,0.653834841531101,5.19430627077206));
#51995=CARTESIAN_POINT('Ctrl Pts',(4.52544944337418,0.6538348415311,5.19430627077206));
#51996=CARTESIAN_POINT('Ctrl Pts',(4.49800585333586,0.575794444672551,5.22566650872935));
#51997=CARTESIAN_POINT('Ctrl Pts',(4.47552348374572,0.493916456452013,5.2524053607931));
#51998=CARTESIAN_POINT('Ctrl Pts',(4.44488537421593,0.338192744373412,5.29279369503618));
#51999=CARTESIAN_POINT('Ctrl Pts',(4.43508928797886,0.265707177517069,5.30779049654904));
#52000=CARTESIAN_POINT('Ctrl Pts',(4.42552848990739,0.12973909330966,5.33024832219718));
#52001=CARTESIAN_POINT('Ctrl Pts',(4.42449620873789,0.0666398892825386,
5.33846719753409));
#52002=CARTESIAN_POINT('Ctrl Pts',(4.42938530227431,-0.0595502670510932,
5.35088018140976));
#52003=CARTESIAN_POINT('Ctrl Pts',(4.43532785702372,-0.122795603932536,
5.35517433332143));
#52004=CARTESIAN_POINT('Ctrl Pts',(4.4556310002044,-0.260150559875305,5.35942166735652));
#52005=CARTESIAN_POINT('Ctrl Pts',(4.4713300777237,-0.333952819465554,5.35844333383778));
#52006=CARTESIAN_POINT('Ctrl Pts',(4.51499497518982,-0.491148042392089,
5.34829752130936));
#52007=CARTESIAN_POINT('Ctrl Pts',(4.5447686026171,-0.574257524294844,5.33787546399782));
#52008=CARTESIAN_POINT('Ctrl Pts',(4.58017336233156,-0.653834841429973,
5.32263163697063));
#52009=CARTESIAN_POINT('',(4.55420717418533,1.2,5.26049052216833));
#52010=CARTESIAN_POINT('Ctrl Pts',(4.55420717418533,1.2,5.26049052216833));
#52011=CARTESIAN_POINT('Ctrl Pts',(4.54938384035087,1.13496897291812,5.24916474015826));
#52012=CARTESIAN_POINT('Ctrl Pts',(4.54290377805626,1.03871956312488,5.23407139532195));
#52013=CARTESIAN_POINT('Ctrl Pts',(4.5301510071915,0.795283719863686,5.20490499247069));
#52014=CARTESIAN_POINT('Ctrl Pts',(4.52810469686917,0.741463044907116,5.20029732278355));
#52015=CARTESIAN_POINT('Ctrl Pts',(4.52544944337418,0.653834841531101,5.19430627077206));
#52016=CARTESIAN_POINT('Ctrl Pts',(4.49080284932948,1.30000000000007,5.36828229018401));
#52017=CARTESIAN_POINT('Ctrl Pts',(4.49816830366447,1.2884795594474,5.35583641315607));
#52018=CARTESIAN_POINT('Ctrl Pts',(4.50506668818057,1.27813273296559,5.34541970920166));
#52019=CARTESIAN_POINT('Ctrl Pts',(4.51196371767097,1.26718805828393,5.33343091922482));
#52020=CARTESIAN_POINT('Ctrl Pts',(4.51743270817141,1.25854452828621,5.32405235793424));
#52021=CARTESIAN_POINT('Ctrl Pts',(4.52987929250229,1.23907155243216,5.30329891655241));
#52022=CARTESIAN_POINT('Ctrl Pts',(4.54268753971979,1.21913747525351,5.28228350697248));
#52023=CARTESIAN_POINT('Ctrl Pts',(4.55420717418533,1.2,5.26049052216833));
#52024=CARTESIAN_POINT('Ctrl Pts',(4.35088387761047,-1.3,5.76896053285564));
#52025=CARTESIAN_POINT('Ctrl Pts',(4.26698198886859,-1.18514270861178,5.78664876365156));
#52026=CARTESIAN_POINT('Ctrl Pts',(4.19526082558493,-1.06847604194512,5.80039023590548));
#52027=CARTESIAN_POINT('Ctrl Pts',(4.05771050318435,-0.794772684000851,
5.8230179840058));
#52028=CARTESIAN_POINT('Ctrl Pts',(4.00307751336492,-0.636309800095196,
5.82803611993916));
#52029=CARTESIAN_POINT('Ctrl Pts',(3.9271390295546,-0.319434907277159,5.82866988923776));
#52030=CARTESIAN_POINT('Ctrl Pts',(3.90745678965039,-0.158333333333332,
5.8229519304616));
#52031=CARTESIAN_POINT('Ctrl Pts',(3.90061191119441,0.158333333333335,5.80362794938222));
#52032=CARTESIAN_POINT('Ctrl Pts',(3.91380906647831,0.319434907277167,5.79110325249134));
#52033=CARTESIAN_POINT('Ctrl Pts',(3.9750721515842,0.636309800095206,5.74890534309992));
#52034=CARTESIAN_POINT('Ctrl Pts',(4.02239198166674,0.794772684000841,5.72299871549042));
#52035=CARTESIAN_POINT('Ctrl Pts',(4.14444540563287,1.06847604194511,5.65643597419595));
#52036=CARTESIAN_POINT('Ctrl Pts',(4.20891602829539,1.18514270861178,5.6221645950906));
#52037=CARTESIAN_POINT('Ctrl Pts',(4.28502486891058,1.3,5.58243438119362));
#52038=CARTESIAN_POINT('Ctrl Pts',(4.37306897027954,-1.3,5.84262823906338));
#52039=CARTESIAN_POINT('Ctrl Pts',(4.28882565135864,-1.18514270861178,5.85861813821062));
#52040=CARTESIAN_POINT('Ctrl Pts',(4.21691086230761,-1.06847604194512,5.87116870407665));
#52041=CARTESIAN_POINT('Ctrl Pts',(4.0792546834088,-0.794772684000851,5.89221747404342));
#52042=CARTESIAN_POINT('Ctrl Pts',(4.02499599674477,-0.636309800095196,
5.89784789675249));
#52043=CARTESIAN_POINT('Ctrl Pts',(3.94958161227244,-0.319434907277159,
5.8988939803217));
#52044=CARTESIAN_POINT('Ctrl Pts',(3.93044726732831,-0.158333333333332,
5.89429014134225));
#52045=CARTESIAN_POINT('Ctrl Pts',(3.92394377232475,0.158333333333335,5.87485523805521));
#52046=CARTESIAN_POINT('Ctrl Pts',(3.9369293207567,0.319434907277167,5.86110715473768));
#52047=CARTESIAN_POINT('Ctrl Pts',(3.99837405888618,0.636309800095206,5.81826761823271));
#52048=CARTESIAN_POINT('Ctrl Pts',(4.04563681344556,0.794772684000841,5.7916456303416));
#52049=CARTESIAN_POINT('Ctrl Pts',(4.16853269776624,1.06847604194511,5.72642253007944));
#52050=CARTESIAN_POINT('Ctrl Pts',(4.23354667110408,1.18514270861178,5.69322842485112));
#52051=CARTESIAN_POINT('Ctrl Pts',(4.31037754319865,1.3,5.65507287774392));
#52052=CARTESIAN_POINT('Ctrl Pts',(4.39525406294861,-1.3,5.91629594527112));
#52053=CARTESIAN_POINT('Ctrl Pts',(4.3106693138487,-1.18514270861178,5.93058751276968));
#52054=CARTESIAN_POINT('Ctrl Pts',(4.2385608990303,-1.06847604194512,5.94194717224782));
#52055=CARTESIAN_POINT('Ctrl Pts',(4.10079886363325,-0.794772684000851,
5.96141696408105));
#52056=CARTESIAN_POINT('Ctrl Pts',(4.04691448012462,-0.636309800095196,
5.96765967356582));
#52057=CARTESIAN_POINT('Ctrl Pts',(3.97202419499028,-0.319434907277159,
5.96911807140564));
#52058=CARTESIAN_POINT('Ctrl Pts',(3.95343774500623,-0.158333333333332,
5.9656283522229));
#52059=CARTESIAN_POINT('Ctrl Pts',(3.94727563345509,0.158333333333335,5.9460825267282));
#52060=CARTESIAN_POINT('Ctrl Pts',(3.96004957503508,0.319434907277167,5.93111105698402));
#52061=CARTESIAN_POINT('Ctrl Pts',(4.02167596618816,0.636309800095206,5.8876298933655));
#52062=CARTESIAN_POINT('Ctrl Pts',(4.06888164522438,0.794772684000841,5.86029254519278));
#52063=CARTESIAN_POINT('Ctrl Pts',(4.19261998989962,1.06847604194511,5.79640908596293));
#52064=CARTESIAN_POINT('Ctrl Pts',(4.25817731391276,1.18514270861178,5.76429225461164));
#52065=CARTESIAN_POINT('Ctrl Pts',(4.33573021748671,1.3,5.72771137429423));
#52066=CARTESIAN_POINT('Ctrl Pts',(4.41743915561768,-1.3,5.98996365147886));
#52067=CARTESIAN_POINT('Ctrl Pts',(4.33251297633875,-1.18514270861178,6.00255688732874));
#52068=CARTESIAN_POINT('Ctrl Pts',(4.26021093575299,-1.06847604194512,6.01272564041899));
#52069=CARTESIAN_POINT('Ctrl Pts',(4.12234304385769,-0.794772684000851,
6.03061645411867));
#52070=CARTESIAN_POINT('Ctrl Pts',(4.06883296350447,-0.636309800095196,
6.03747145037915));
#52071=CARTESIAN_POINT('Ctrl Pts',(3.99446677770813,-0.319434907277159,
6.03934216248958));
#52072=CARTESIAN_POINT('Ctrl Pts',(3.97642822268415,-0.158333333333332,
6.03696656310355));
#52073=CARTESIAN_POINT('Ctrl Pts',(3.97060749458543,0.158333333333335,6.01730981540119));
#52074=CARTESIAN_POINT('Ctrl Pts',(3.98316982931346,0.319434907277167,6.00111495923037));
#52075=CARTESIAN_POINT('Ctrl Pts',(4.04497787349015,0.636309800095206,5.95699216849829));
#52076=CARTESIAN_POINT('Ctrl Pts',(4.0921264770032,0.794772684000841,5.92893946004396));
#52077=CARTESIAN_POINT('Ctrl Pts',(4.21670728203299,1.06847604194511,5.86639564184641));
#52078=CARTESIAN_POINT('Ctrl Pts',(4.28280795672145,1.18514270861178,5.83535608437217));
#52079=CARTESIAN_POINT('Ctrl Pts',(4.36108289177478,1.3,5.80034987084453));
#52080=CARTESIAN_POINT('Ctrl Pts',(4.41743915561768,-1.3,5.98996365147886));
#52081=CARTESIAN_POINT('Ctrl Pts',(4.33251297633875,-1.18514270861178,6.00255688732874));
#52082=CARTESIAN_POINT('Ctrl Pts',(4.26021093575299,-1.06847604194512,6.01272564041899));
#52083=CARTESIAN_POINT('Ctrl Pts',(4.12234304385769,-0.794772684000851,
6.03061645411867));
#52084=CARTESIAN_POINT('Ctrl Pts',(4.06883296350448,-0.636309800095197,
6.03747145037915));
#52085=CARTESIAN_POINT('Ctrl Pts',(3.99446677770812,-0.319434907277159,
6.03934216248958));
#52086=CARTESIAN_POINT('Ctrl Pts',(3.97642822268415,-0.158333333333332,
6.03696656310355));
#52087=CARTESIAN_POINT('Ctrl Pts',(3.97060749458543,0.158333333333334,6.01730981540119));
#52088=CARTESIAN_POINT('Ctrl Pts',(3.98316982931346,0.319434907277167,6.00111495923037));
#52089=CARTESIAN_POINT('Ctrl Pts',(4.04497787349014,0.636309800095206,5.95699216849829));
#52090=CARTESIAN_POINT('Ctrl Pts',(4.0921264770032,0.79477268400084,5.92893946004396));
#52091=CARTESIAN_POINT('Ctrl Pts',(4.21670728203298,1.06847604194511,5.86639564184641));
#52092=CARTESIAN_POINT('Ctrl Pts',(4.28280795672145,1.18514270861178,5.83535608437217));
#52093=CARTESIAN_POINT('Ctrl Pts',(4.36108289177478,1.3,5.80034987084453));
#52094=CARTESIAN_POINT('Ctrl Pts',(4.41743915561997,-1.30000000000309,5.98996365147853));
#52095=CARTESIAN_POINT('Ctrl Pts',(4.33251297634005,-1.18514270861388,6.00255688732856));
#52096=CARTESIAN_POINT('Ctrl Pts',(4.26021093575352,-1.06847604194618,6.01272564041892));
#52097=CARTESIAN_POINT('Ctrl Pts',(4.12234304385769,-0.794772684000851,
6.03061645411867));
#52098=CARTESIAN_POINT('Ctrl Pts',(4.06883296350447,-0.636309800095196,
6.03747145037915));
#52099=CARTESIAN_POINT('Ctrl Pts',(3.99446677770812,-0.319434907277159,
6.03934216248958));
#52100=CARTESIAN_POINT('Ctrl Pts',(3.97642822268415,-0.158333333333332,
6.03696656310355));
#52101=CARTESIAN_POINT('Ctrl Pts',(3.97060749458543,0.158333333333334,6.01730981540119));
#52102=CARTESIAN_POINT('Ctrl Pts',(3.98316982931346,0.319434907277167,6.00111495923037));
#52103=CARTESIAN_POINT('Ctrl Pts',(4.04497787349015,0.636309800095206,5.95699216849829));
#52104=CARTESIAN_POINT('Ctrl Pts',(4.0921264770032,0.794772684000841,5.92893946004397));
#52105=CARTESIAN_POINT('Ctrl Pts',(4.21670728203357,1.0684760419464,5.86639564184612));
#52106=CARTESIAN_POINT('Ctrl Pts',(4.28280795672289,1.18514270861431,5.8353560843715));
#52107=CARTESIAN_POINT('Ctrl Pts',(4.36108289177733,1.30000000000375,5.80034987084339));
#52108=CARTESIAN_POINT('Ctrl Pts',(4.42562833098721,-1.30000000000309,5.99305077181872));
#52109=CARTESIAN_POINT('Ctrl Pts',(4.34039737039433,-1.18514270861388,6.00502961962694));
#52110=CARTESIAN_POINT('Ctrl Pts',(4.26788601359697,-1.06847604194618,6.01517679412997));
#52111=CARTESIAN_POINT('Ctrl Pts',(4.12975510286419,-0.794772684000851,
6.03438726540721));
#52112=CARTESIAN_POINT('Ctrl Pts',(4.07641358156132,-0.636309800095196,
6.04488755347926));
#52113=CARTESIAN_POINT('Ctrl Pts',(4.00209599194821,-0.319434907277159,
6.04853496478958));
#52114=CARTESIAN_POINT('Ctrl Pts',(3.98412215784035,-0.158333333333332,
6.04561777589617));
#52115=CARTESIAN_POINT('Ctrl Pts',(3.97832338053354,0.158333333333334,6.0257252204883));
#52116=CARTESIAN_POINT('Ctrl Pts',(3.99084012994539,0.319434907277167,6.0095560959087));
#52117=CARTESIAN_POINT('Ctrl Pts',(4.05265002446484,0.636309800095206,5.96374672477414));
#52118=CARTESIAN_POINT('Ctrl Pts',(4.09970289374315,0.794772684000841,5.93313005490399));
#52119=CARTESIAN_POINT('Ctrl Pts',(4.2245248835901,1.0684760419464,5.86911453241694));
#52120=CARTESIAN_POINT('Ctrl Pts',(4.29080148661917,1.18514270861431,5.8377783689165));
#52121=CARTESIAN_POINT('Ctrl Pts',(4.36932387838279,1.30000000000375,5.80281598959156));
#52122=CARTESIAN_POINT('Ctrl Pts',(4.43787121888944,-1.30000000000308,5.99376524194423));
#52123=CARTESIAN_POINT('Ctrl Pts',(4.35491096318019,-1.18514270861386,6.00391672292321));
#52124=CARTESIAN_POINT('Ctrl Pts',(4.2840885617701,-1.06847604194617,6.01337406538631));
#52125=CARTESIAN_POINT('Ctrl Pts',(4.14851551814112,-0.794772684000842,
6.03361881957726));
#52126=CARTESIAN_POINT('Ctrl Pts',(4.09501955407359,-0.636309800095189,
6.04967670444219));
#52127=CARTESIAN_POINT('Ctrl Pts',(4.02081949266675,-0.319434907277155,
6.0562190775837));
#52128=CARTESIAN_POINT('Ctrl Pts',(4.00186551766012,-0.15833333333333,6.05325499433251));
#52129=CARTESIAN_POINT('Ctrl Pts',(3.99606931639037,0.158333333333333,6.03319499170625));
#52130=CARTESIAN_POINT('Ctrl Pts',(4.00965920221954,0.319434907277164,6.01702438361));
#52131=CARTESIAN_POINT('Ctrl Pts',(4.07117263776139,0.636309800095199,5.9677364370366));
#52132=CARTESIAN_POINT('Ctrl Pts',(4.11789328435415,0.794772684000831,5.93055388199639));
#52133=CARTESIAN_POINT('Ctrl Pts',(4.24018002663975,1.06847604194638,5.86555700416122));
#52134=CARTESIAN_POINT('Ctrl Pts',(4.30489463524463,1.1851427086143,5.83519871970262));
#52135=CARTESIAN_POINT('Ctrl Pts',(4.38139045288901,1.30000000000373,5.80261689082876));
#52136=CARTESIAN_POINT('Ctrl Pts',(4.45585041430731,-1.30000000000307,5.99501197237341));
#52137=CARTESIAN_POINT('Ctrl Pts',(4.37647147135345,-1.18514270861386,6.00435238130437));
#52138=CARTESIAN_POINT('Ctrl Pts',(4.30833031726903,-1.06847604194617,6.01341501487799));
#52139=CARTESIAN_POINT('Ctrl Pts',(4.17687216014389,-0.794772684000842,
6.03370979476238));
#52140=CARTESIAN_POINT('Ctrl Pts',(4.12318598035631,-0.636309800095189,
6.051344155984));
#52141=CARTESIAN_POINT('Ctrl Pts',(4.04942280399533,-0.319434907277155,
6.05911325681098));
#52142=CARTESIAN_POINT('Ctrl Pts',(4.02934019274684,-0.15833333333333,6.05707345537754));
#52143=CARTESIAN_POINT('Ctrl Pts',(4.02349949763675,0.158333333333333,6.03691189730058));
#52144=CARTESIAN_POINT('Ctrl Pts',(4.0382239070047,0.319434907277164,6.02003355142058));
#52145=CARTESIAN_POINT('Ctrl Pts',(4.09910720400251,0.636309800095199,5.96866407027448));
#52146=CARTESIAN_POINT('Ctrl Pts',(4.14564853964763,0.794772684000832,5.92810673121632));
#52147=CARTESIAN_POINT('Ctrl Pts',(4.26383848145775,1.06847604194638,5.86288689468531));
#52148=CARTESIAN_POINT('Ctrl Pts',(4.32597451263342,1.1851427086143,5.83324406605495));
#52149=CARTESIAN_POINT('Ctrl Pts',(4.3990865285438,1.30000000000373,5.80218965939557));
#52150=CARTESIAN_POINT('Ctrl Pts',(4.47077112054955,-1.30000000000307,5.99624136741226));
#52151=CARTESIAN_POINT('Ctrl Pts',(4.3941367061776,-1.18514270861385,6.0053141056848));
#52152=CARTESIAN_POINT('Ctrl Pts',(4.3279655414052,-1.06847604194616,6.0140486726285));
#52153=CARTESIAN_POINT('Ctrl Pts',(4.19926911302636,-0.794772684000836,
6.03344602619192));
#52154=CARTESIAN_POINT('Ctrl Pts',(4.14469678620781,-0.636309800095183,
6.04964010753271));
#52155=CARTESIAN_POINT('Ctrl Pts',(4.07099239599207,-0.319434907277152,
6.05762788567868));
#52156=CARTESIAN_POINT('Ctrl Pts',(4.05033624387987,-0.158333333333329,
6.05752341512769));
#52157=CARTESIAN_POINT('Ctrl Pts',(4.04460429816785,0.158333333333331,6.0379605124523));
#52158=CARTESIAN_POINT('Ctrl Pts',(4.06019377913399,0.319434907277161,6.0206465745952));
#52159=CARTESIAN_POINT('Ctrl Pts',(4.12086749225863,0.636309800095193,5.96844239186139));
#52160=CARTESIAN_POINT('Ctrl Pts',(4.16759019757613,0.794772684000824,5.92608052888347));
#52161=CARTESIAN_POINT('Ctrl Pts',(4.28295080002241,1.06847604194637,5.86124858282267));
#52162=CARTESIAN_POINT('Ctrl Pts',(4.34322444403162,1.18514270861429,5.83229200346367));
#52163=CARTESIAN_POINT('Ctrl Pts',(4.41383640178237,1.30000000000372,5.80244219193521));
#52164=CARTESIAN_POINT('Ctrl Pts',(4.48888549481477,-1.30000000000306,5.99826902796289));
#52165=CARTESIAN_POINT('Ctrl Pts',(4.41585250305352,-1.18514270861385,6.00716604759878));
#52166=CARTESIAN_POINT('Ctrl Pts',(4.35227563785691,-1.06847604194615,6.01553951366496));
#52167=CARTESIAN_POINT('Ctrl Pts',(4.22724590480102,-0.794772684000832,
6.03367438190129));
#52168=CARTESIAN_POINT('Ctrl Pts',(4.17165190374168,-0.636309800095182,
6.04784773027761));
#52169=CARTESIAN_POINT('Ctrl Pts',(4.09793603477848,-0.319434907277151,
6.0551166088243));
#52170=CARTESIAN_POINT('Ctrl Pts',(4.07641255024289,-0.158333333333329,
6.05672669443841));
#52171=CARTESIAN_POINT('Ctrl Pts',(4.07040330877367,0.158333333333331,6.03605204947613));
#52172=CARTESIAN_POINT('Ctrl Pts',(4.08639823387368,0.31943490727716,6.01522745208349));
#52173=CARTESIAN_POINT('Ctrl Pts',(4.14689459595155,0.636309800095192,5.9628716242103));
#52174=CARTESIAN_POINT('Ctrl Pts',(4.19493228340675,0.794772684000823,5.9235372548977));
#52175=CARTESIAN_POINT('Ctrl Pts',(4.3068199206522,1.06847604194637,5.86052220641105));
#52176=CARTESIAN_POINT('Ctrl Pts',(4.36458750470472,1.18514270861428,5.83217938427488));
#52177=CARTESIAN_POINT('Ctrl Pts',(4.43169066049147,1.30000000000371,5.8027706195549));
#52178=CARTESIAN_POINT('Ctrl Pts',(4.5070805240044,-1.30000000000304,6.00172835399182));
#52179=CARTESIAN_POINT('Ctrl Pts',(4.43743267384654,-1.18514270861383,6.01016185167031));
#52180=CARTESIAN_POINT('Ctrl Pts',(4.37628118333525,-1.06847604194614,6.01793101980723));
#52181=CARTESIAN_POINT('Ctrl Pts',(4.25463729741546,-0.79477268400082,6.03434461828046));
#52182=CARTESIAN_POINT('Ctrl Pts',(4.19808657167185,-0.636309800095172,
6.04682497611925));
#52183=CARTESIAN_POINT('Ctrl Pts',(4.12408493576571,-0.319434907277146,
6.05216015227242));
#52184=CARTESIAN_POINT('Ctrl Pts',(4.10118108824753,-0.158333333333326,
6.05275179787127));
#52185=CARTESIAN_POINT('Ctrl Pts',(4.0950379936865,0.158333333333328,6.03161959587353));
#52186=CARTESIAN_POINT('Ctrl Pts',(4.11224098282643,0.319434907277155,6.01137027620302));
#52187=CARTESIAN_POINT('Ctrl Pts',(4.172828774167,0.636309800095181,5.95998681893364));
#52188=CARTESIAN_POINT('Ctrl Pts',(4.22174645187094,0.79477268400081,5.9216197443018));
#52189=CARTESIAN_POINT('Ctrl Pts',(4.33025333204167,1.06847604194635,5.85979788035525));
#52190=CARTESIAN_POINT('Ctrl Pts',(4.38563297633725,1.18514270861426,5.83195039824915));
#52191=CARTESIAN_POINT('Ctrl Pts',(4.44942365707838,1.30000000000369,5.80301582821375));
#52192=CARTESIAN_POINT('Ctrl Pts',(4.53109886254452,-1.30000000000303,6.00406302153179));
#52193=CARTESIAN_POINT('Ctrl Pts',(4.46616480243323,-1.18514270861382,6.01256767400805));
#52194=CARTESIAN_POINT('Ctrl Pts',(4.40841786727856,-1.06847604194613,6.02013682822857));
#52195=CARTESIAN_POINT('Ctrl Pts',(4.29161459126626,-0.794772684000815,
6.03546190056545));
#52196=CARTESIAN_POINT('Ctrl Pts',(4.23390801699434,-0.636309800095169,
6.0461976720324));
#52197=CARTESIAN_POINT('Ctrl Pts',(4.15971786921738,-0.319434907277146,
6.04979125214187));
#52198=CARTESIAN_POINT('Ctrl Pts',(4.13507614674857,-0.158333333333325,
6.04965079389733));
#52199=CARTESIAN_POINT('Ctrl Pts',(4.1287251135606,0.158333333333328,6.02765789882209));
#52200=CARTESIAN_POINT('Ctrl Pts',(4.14731388921087,0.319434907277154,6.00671206620468));
#52201=CARTESIAN_POINT('Ctrl Pts',(4.20796025920192,0.63630980009518,5.95647385486317));
#52202=CARTESIAN_POINT('Ctrl Pts',(4.25823946126208,0.794772684000807,5.92061942086322));
#52203=CARTESIAN_POINT('Ctrl Pts',(4.36212968709833,1.06847604194635,5.86069137778686));
#52204=CARTESIAN_POINT('Ctrl Pts',(4.41422395080956,1.18514270861426,5.83347966904655));
#52205=CARTESIAN_POINT('Ctrl Pts',(4.47344224897951,1.30000000000369,5.80499688086099));
#52206=CARTESIAN_POINT('Ctrl Pts',(4.55542077951101,-1.30000000000301,6.0091065818418));
#52207=CARTESIAN_POINT('Ctrl Pts',(4.49515867257234,-1.1851427086138,6.01776346089841));
#52208=CARTESIAN_POINT('Ctrl Pts',(4.44076843666203,-1.06847604194611,6.02506284513832));
#52209=CARTESIAN_POINT('Ctrl Pts',(4.32868130771967,-0.794772684000799,
6.03878979837678));
#52210=CARTESIAN_POINT('Ctrl Pts',(4.26968336791182,-0.636309800095154,
6.04672131813715));
#52211=CARTESIAN_POINT('Ctrl Pts',(4.19523270114734,-0.319434907277137,
6.04799361755878));
#52212=CARTESIAN_POINT('Ctrl Pts',(4.16886869472472,-0.158333333333322,
6.04709843557643));
#52213=CARTESIAN_POINT('Ctrl Pts',(4.1623841418559,0.158333333333324,6.02456257462145));
#52214=CARTESIAN_POINT('Ctrl Pts',(4.18256377673187,0.319434907277147,6.00407772113189));
#52215=CARTESIAN_POINT('Ctrl Pts',(4.24319442846635,0.636309800095165,5.95454716229398));
#52216=CARTESIAN_POINT('Ctrl Pts',(4.29447370823118,0.794772684000787,5.91935837850987));
#52217=CARTESIAN_POINT('Ctrl Pts',(4.39365357926063,1.06847604194633,5.86048505252226));
#52218=CARTESIAN_POINT('Ctrl Pts',(4.44247879492748,1.18514270861423,5.83376298909323));
#52219=CARTESIAN_POINT('Ctrl Pts',(4.49719793506867,1.30000000000366,5.80580294358365));
#52220=CARTESIAN_POINT('Ctrl Pts',(4.57961335592317,-1.30000000000298,6.01326169023633));
#52221=CARTESIAN_POINT('Ctrl Pts',(4.52404695564334,-1.18514270861378,6.02217753251362));
#52222=CARTESIAN_POINT('Ctrl Pts',(4.47306199948735,-1.06847604194609,6.02944633197147));
#52223=CARTESIAN_POINT('Ctrl Pts',(4.36586060370283,-0.794772684000784,
6.04243371443469));
#52224=CARTESIAN_POINT('Ctrl Pts',(4.30585581723244,-0.636309800095142,
6.04909462591785));
#52225=CARTESIAN_POINT('Ctrl Pts',(4.23121474878952,-0.319434907277131,
6.04828584773161));
#52226=CARTESIAN_POINT('Ctrl Pts',(4.2029207811322,-0.158333333333319,6.04532202205807));
#52227=CARTESIAN_POINT('Ctrl Pts',(4.19628041448162,0.158333333333321,6.02203922050159));
#52228=CARTESIAN_POINT('Ctrl Pts',(4.21813530655345,0.31943490727714,6.00249961225309));
#52229=CARTESIAN_POINT('Ctrl Pts',(4.27884041084526,0.636309800095152,5.95429548433113));
#52230=CARTESIAN_POINT('Ctrl Pts',(4.33126058845234,0.794772684000772,5.92069046234265));
#52231=CARTESIAN_POINT('Ctrl Pts',(4.42567265879968,1.06847604194631,5.86279094197079));
#52232=CARTESIAN_POINT('Ctrl Pts',(4.47115504984018,1.18514270861421,5.83626623457124));
#52233=CARTESIAN_POINT('Ctrl Pts',(4.52125234497956,1.30000000000364,5.8082793767526));
#52234=CARTESIAN_POINT('Ctrl Pts',(4.60381579105714,-1.30000000000298,6.01754841177121));
#52235=CARTESIAN_POINT('Ctrl Pts',(4.55290203223089,-1.18514270861378,6.02632358361635));
#52236=CARTESIAN_POINT('Ctrl Pts',(4.50530124431252,-1.06847604194609,6.03336789866386));
#52237=CARTESIAN_POINT('Ctrl Pts',(4.40298752727133,-0.794772684000784,
6.04564305017475));
#52238=CARTESIAN_POINT('Ctrl Pts',(4.34201232346892,-0.636309800095145,
6.05164736415331));
#52239=CARTESIAN_POINT('Ctrl Pts',(4.26733571815094,-0.319434907277134,
6.04969354682945));
#52240=CARTESIAN_POINT('Ctrl Pts',(4.23737292911869,-0.158333333333319,
6.04591398439182));
#52241=CARTESIAN_POINT('Ctrl Pts',(4.23058205335565,0.158333333333322,6.02181828848998));
#52242=CARTESIAN_POINT('Ctrl Pts',(4.25388869406487,0.319434907277141,6.00196886684759));
#52243=CARTESIAN_POINT('Ctrl Pts',(4.31445834431823,0.636309800095155,5.95389082819043));
#52244=CARTESIAN_POINT('Ctrl Pts',(4.36786778497214,0.794772684000777,5.92103100417116));
#52245=CARTESIAN_POINT('Ctrl Pts',(4.45743057115858,1.06847604194631,5.86363653008099));
#52246=CARTESIAN_POINT('Ctrl Pts',(4.49956711306004,1.18514270861421,5.83728451025261));
#52247=CARTESIAN_POINT('Ctrl Pts',(4.54507178535092,1.30000000000364,5.80942441175477));
#52248=CARTESIAN_POINT('Ctrl Pts',(4.62354611479265,-1.30000000000292,6.02187971789063));
#52249=CARTESIAN_POINT('Ctrl Pts',(4.57654041299366,-1.18514270861372,6.03190893581532));
#52250=CARTESIAN_POINT('Ctrl Pts',(4.53176285751006,-1.06847604194604,6.03955116088897));
#52251=CARTESIAN_POINT('Ctrl Pts',(4.43346521035186,-0.794772684000746,
6.05169179862876));
#52252=CARTESIAN_POINT('Ctrl Pts',(4.37152877982439,-0.636309800095112,
6.05516887015694));
#52253=CARTESIAN_POINT('Ctrl Pts',(4.29671435794294,-0.319434907277116,
6.05124212051647));
#52254=CARTESIAN_POINT('Ctrl Pts',(4.26531192771955,-0.158333333333311,
6.04636116710423));
#52255=CARTESIAN_POINT('Ctrl Pts',(4.25842001866299,0.158333333333313,6.02170035863254));
#52256=CARTESIAN_POINT('Ctrl Pts',(4.28302862982561,0.319434907277126,6.00238960620395));
#52257=CARTESIAN_POINT('Ctrl Pts',(4.34360492693411,0.636309800095123,5.9551285363422));
#52258=CARTESIAN_POINT('Ctrl Pts',(4.39787976032314,0.794772684000733,5.92328230146951));
#52259=CARTESIAN_POINT('Ctrl Pts',(4.48356835798253,1.06847604194626,5.86660248501926));
#52260=CARTESIAN_POINT('Ctrl Pts',(4.52300590752555,1.18514270861416,5.84043964376399));
#52261=CARTESIAN_POINT('Ctrl Pts',(4.56478958776009,1.30000000000358,5.81264855360073));
#52262=CARTESIAN_POINT('Ctrl Pts',(4.63874413860242,-1.30000000000292,6.02548249806497));
#52263=CARTESIAN_POINT('Ctrl Pts',(4.59465672471239,-1.18514270861372,6.03557603946561));
#52264=CARTESIAN_POINT('Ctrl Pts',(4.55200234525745,-1.06847604194603,6.04316523301098));
#52265=CARTESIAN_POINT('Ctrl Pts',(4.45677279196024,-0.794772684000744,
6.05491224377494));
#52266=CARTESIAN_POINT('Ctrl Pts',(4.39422085386997,-0.636309800095109,
6.05770680163088));
#52267=CARTESIAN_POINT('Ctrl Pts',(4.31940808634673,-0.319434907277114,
6.0530565082544));
#52268=CARTESIAN_POINT('Ctrl Pts',(4.28699461990195,-0.158333333333311,
6.04781261330039));
#52269=CARTESIAN_POINT('Ctrl Pts',(4.28003945825534,0.158333333333313,6.0227713625454));
#52270=CARTESIAN_POINT('Ctrl Pts',(4.30556805694205,0.319434907277125,6.00333617711307));
#52271=CARTESIAN_POINT('Ctrl Pts',(4.36607047738981,0.63630980009512,5.95624153076773));
#52272=CARTESIAN_POINT('Ctrl Pts',(4.4209775188318,0.79477268400073,5.92504094672903));
#52273=CARTESIAN_POINT('Ctrl Pts',(4.5035970151742,1.06847604194625,5.86842779829152));
#52274=CARTESIAN_POINT('Ctrl Pts',(4.54091462698009,1.18514270861415,5.84216667581498));
#52275=CARTESIAN_POINT('Ctrl Pts',(4.57978693197907,1.30000000000357,5.81415016509678));
#52276=CARTESIAN_POINT('Ctrl Pts',(4.64482079169386,-1.30000000000291,6.02690740127364));
#52277=CARTESIAN_POINT('Ctrl Pts',(4.60191504159934,-1.18514270861371,6.03716613059751));
#52278=CARTESIAN_POINT('Ctrl Pts',(4.56011944211076,-1.06847604194603,6.04482333556412));
#52279=CARTESIAN_POINT('Ctrl Pts',(4.46612791609618,-0.794772684000742,
6.0565029691571));
#52280=CARTESIAN_POINT('Ctrl Pts',(4.40332274652645,-0.636309800095109,
6.05891824706142));
#52281=CARTESIAN_POINT('Ctrl Pts',(4.32849953478007,-0.319434907277114,
6.0538798088146));
#52282=CARTESIAN_POINT('Ctrl Pts',(4.29565827532708,-0.158333333333311,
6.04833685913728));
#52283=CARTESIAN_POINT('Ctrl Pts',(4.28868341905821,0.158333333333313,6.02317300087302));
#52284=CARTESIAN_POINT('Ctrl Pts',(4.31460773806686,0.319434907277124,6.00386949195305));
#52285=CARTESIAN_POINT('Ctrl Pts',(4.37510569943537,0.63630980009512,5.95700444250547));
#52286=CARTESIAN_POINT('Ctrl Pts',(4.43028166958698,0.794772684000729,5.92617200183776));
#52287=CARTESIAN_POINT('Ctrl Pts',(4.51167910779437,1.06847604194625,5.86961587904899));
#52288=CARTESIAN_POINT('Ctrl Pts',(4.54814679444583,1.18514270861415,5.84329781936374));
#52289=CARTESIAN_POINT('Ctrl Pts',(4.5858482328209,1.30000000000357,5.81514274993776));
#52290=CARTESIAN_POINT('Ctrl Pts',(4.65541484816498,-1.30000000000291,6.02904115986957));
#52291=CARTESIAN_POINT('Ctrl Pts',(4.61460498496626,-1.18514270861371,6.0399105177876));
#52292=CARTESIAN_POINT('Ctrl Pts',(4.5743320538263,-1.06847604194603,6.04790675769232));
#52293=CARTESIAN_POINT('Ctrl Pts',(4.48253394678982,-0.794772684000739,
6.05974219413844));
#52294=CARTESIAN_POINT('Ctrl Pts',(4.41928383318675,-0.636309800095105,
6.06137265385868));
#52295=CARTESIAN_POINT('Ctrl Pts',(4.34442306225996,-0.319434907277113,
6.05547552036877));
#52296=CARTESIAN_POINT('Ctrl Pts',(4.31079257432893,-0.15833333333331,6.04910982007256));
#52297=CARTESIAN_POINT('Ctrl Pts',(4.30376503396204,0.158333333333312,6.02357447304307));
#52298=CARTESIAN_POINT('Ctrl Pts',(4.33039479005563,0.319434907277123,6.00457287561657));
#52299=CARTESIAN_POINT('Ctrl Pts',(4.39088636021054,0.636309800095117,5.95811404147546));
#52300=CARTESIAN_POINT('Ctrl Pts',(4.44652348451578,0.794772684000725,5.92788673225629));
#52301=CARTESIAN_POINT('Ctrl Pts',(4.52579694767258,1.06847604194624,5.87152878984834));
#52302=CARTESIAN_POINT('Ctrl Pts',(4.56078851772166,1.18514270861415,5.84518250637771));
#52303=CARTESIAN_POINT('Ctrl Pts',(4.59645711299034,1.30000000000357,5.81688520443742));
#52304=CARTESIAN_POINT('Ctrl Pts',(4.6766367318432,-1.30000000000289,6.03366080550862));
#52305=CARTESIAN_POINT('Ctrl Pts',(4.63993747158105,-1.18514270861369,6.04487333679941));
#52306=CARTESIAN_POINT('Ctrl Pts',(4.60265480542224,-1.06847604194601,6.05297495110862));
#52307=CARTESIAN_POINT('Ctrl Pts',(4.51517660389278,-0.794772684000726,
6.06450446032101));
#52308=CARTESIAN_POINT('Ctrl Pts',(4.45105908241519,-0.636309800095095,
6.06509936357692));
#52309=CARTESIAN_POINT('Ctrl Pts',(4.37619392540727,-0.319434907277107,
6.05814915506877));
#52310=CARTESIAN_POINT('Ctrl Pts',(4.3410990948752,-0.158333333333307,6.05094393173563));
#52311=CARTESIAN_POINT('Ctrl Pts',(4.3340396043192,0.158333333333309,6.02527429564328));
#52312=CARTESIAN_POINT('Ctrl Pts',(4.36212647356014,0.319434907277117,6.00728440154909));
#52313=CARTESIAN_POINT('Ctrl Pts',(4.42250699520338,0.636309800095105,5.96098084925809));
#52314=CARTESIAN_POINT('Ctrl Pts',(4.47882945207936,0.794772684000713,5.93021983262011));
#52315=CARTESIAN_POINT('Ctrl Pts',(4.55375622132621,1.06847604194623,5.87358000316449));
#52316=CARTESIAN_POINT('Ctrl Pts',(4.58578679647162,1.18514270861412,5.84713790028093));
#52317=CARTESIAN_POINT('Ctrl Pts',(4.61741492466572,1.30000000000354,5.81877097797278));
#52318=CARTESIAN_POINT('Ctrl Pts',(4.70094536200485,-1.30000000000283,6.040011863196));
#52319=CARTESIAN_POINT('Ctrl Pts',(4.66902133675282,-1.18514270861363,6.05279341445746));
#52320=CARTESIAN_POINT('Ctrl Pts',(4.63520845163771,-1.06847604194596,6.0617460142815));
#52321=CARTESIAN_POINT('Ctrl Pts',(4.55273027862888,-0.794772684000688,
6.07358266703692));
#52322=CARTESIAN_POINT('Ctrl Pts',(4.48757147724743,-0.636309800095066,
6.07175891365129));
#52323=CARTESIAN_POINT('Ctrl Pts',(4.41268620746716,-0.319434907277093,
6.0629803630447));
#52324=CARTESIAN_POINT('Ctrl Pts',(4.37595562502286,-0.1583333333333,6.05490103609209));
#52325=CARTESIAN_POINT('Ctrl Pts',(4.36875227568137,0.158333333333302,6.0281015831388));
#52326=CARTESIAN_POINT('Ctrl Pts',(4.39823174652913,0.319434907277102,6.00933141895887));
#52327=CARTESIAN_POINT('Ctrl Pts',(4.45854160063371,0.636309800095077,5.96362333769257));
#52328=CARTESIAN_POINT('Ctrl Pts',(4.51608172583745,0.794772684000676,5.93551344003385));
#52329=CARTESIAN_POINT('Ctrl Pts',(4.58609921371453,1.06847604194618,5.87892679803689));
#52330=CARTESIAN_POINT('Ctrl Pts',(4.61469399881586,1.18514270861407,5.85194577731453));
#52331=CARTESIAN_POINT('Ctrl Pts',(4.64157559291995,1.30000000000348,5.8224779964487));
#52332=CARTESIAN_POINT('Ctrl Pts',(4.72069270328122,-1.3000000000028,6.04521039352825));
#52333=CARTESIAN_POINT('Ctrl Pts',(4.69257203670566,-1.18514270861361,6.05835663747547));
#52334=CARTESIAN_POINT('Ctrl Pts',(4.66154109137681,-1.06847604194594,6.06755884022885));
#52335=CARTESIAN_POINT('Ctrl Pts',(4.58313007382887,-0.794772684000672,
6.07970624532299));
#52336=CARTESIAN_POINT('Ctrl Pts',(4.51731897215768,-0.636309800095054,
6.07820763874449));
#52337=CARTESIAN_POINT('Ctrl Pts',(4.44244429505606,-0.319434907277088,
6.06831849035796));
#52338=CARTESIAN_POINT('Ctrl Pts',(4.40422789755839,-0.158333333333297,
6.05795366283987));
#52339=CARTESIAN_POINT('Ctrl Pts',(4.39695983770024,0.158333333333299,6.03050840572729));
#52340=CARTESIAN_POINT('Ctrl Pts',(4.42783577478779,0.319434907277095,6.01316697049685));
#52341=CARTESIAN_POINT('Ctrl Pts',(4.48805341198737,0.636309800095063,5.96768375595659));
#52342=CARTESIAN_POINT('Ctrl Pts',(4.5462177986737,0.794772684000664,5.93901571765619));
#52343=CARTESIAN_POINT('Ctrl Pts',(4.61221117101888,1.06847604194616,5.88213897831174));
#52344=CARTESIAN_POINT('Ctrl Pts',(4.63806563950542,1.18514270861405,5.85505464187112));
#52345=CARTESIAN_POINT('Ctrl Pts',(4.66120849088553,1.30000000000346,5.82550580196134));
#52346=CARTESIAN_POINT('Ctrl Pts',(4.73277983786844,-1.3000000000028,6.04774757720061));
#52347=CARTESIAN_POINT('Ctrl Pts',(4.70702828209547,-1.18514270861361,6.06144066240088));
#52348=CARTESIAN_POINT('Ctrl Pts',(4.67772380816164,-1.06847604194593,6.07096186531051));
#52349=CARTESIAN_POINT('Ctrl Pts',(4.60181665932455,-0.794772684000669,
6.08331986606822));
#52350=CARTESIAN_POINT('Ctrl Pts',(4.53551006683239,-0.636309800095052,
6.0810430560724));
#52351=CARTESIAN_POINT('Ctrl Pts',(4.46068656840018,-0.319434907277087,
6.0708469211743));
#52352=CARTESIAN_POINT('Ctrl Pts',(4.42170832034993,-0.158333333333296,
6.06048747780477));
#52353=CARTESIAN_POINT('Ctrl Pts',(4.41444165181559,0.158333333333298,6.03307259932769));
#52354=CARTESIAN_POINT('Ctrl Pts',(4.44609545841066,0.319434907277094,6.01595725300538));
#52355=CARTESIAN_POINT('Ctrl Pts',(4.50623495553593,0.636309800095061,5.97043328921319));
#52356=CARTESIAN_POINT('Ctrl Pts',(4.5648121875001,0.794772684000661,5.94159185355148));
#52357=CARTESIAN_POINT('Ctrl Pts',(4.62831581752182,1.06847604194616,5.88441441473242));
#52358=CARTESIAN_POINT('Ctrl Pts',(4.65247175398913,1.18514270861404,5.85717138499989));
#52359=CARTESIAN_POINT('Ctrl Pts',(4.6732952585286,1.30000000000345,5.82743532016684));
#52360=CARTESIAN_POINT('Ctrl Pts',(4.74494445621426,-1.30000000000275,6.05141731309816));
#52361=CARTESIAN_POINT('Ctrl Pts',(4.72159046772432,-1.18514270861356,6.06624105700331));
#52362=CARTESIAN_POINT('Ctrl Pts',(4.69402959774547,-1.0684760419459,6.07641364231617));
#52363=CARTESIAN_POINT('Ctrl Pts',(4.62063973673839,-0.794772684000642,
6.08916924259824));
#52364=CARTESIAN_POINT('Ctrl Pts',(4.55383037099021,-0.63630980009503,6.08549942988976));
#52365=CARTESIAN_POINT('Ctrl Pts',(4.47898769993957,-0.319434907277075,
6.074077080766));
#52366=CARTESIAN_POINT('Ctrl Pts',(4.43914810147163,-0.158333333333291,
6.06277640534756));
#52367=CARTESIAN_POINT('Ctrl Pts',(4.43180983029836,0.158333333333293,6.0346854767056));
#52368=CARTESIAN_POINT('Ctrl Pts',(4.46420681851606,0.319434907277083,6.01758245701524));
#52369=CARTESIAN_POINT('Ctrl Pts',(4.52431449074692,0.636309800095039,5.97242268988233));
#52370=CARTESIAN_POINT('Ctrl Pts',(4.5834589120997,0.794772684000632,5.94471142931503));
#52371=CARTESIAN_POINT('Ctrl Pts',(4.64450497239395,1.06847604194612,5.88749046259075));
#52372=CARTESIAN_POINT('Ctrl Pts',(4.66694884054746,1.185142708614,5.8599635463673));
#52373=CARTESIAN_POINT('Ctrl Pts',(4.68541199933239,1.30000000000341,5.82967855016972));
#52374=CARTESIAN_POINT('Ctrl Pts',(4.76168328182841,-1.30000000000272,6.05637407538914));
#52375=CARTESIAN_POINT('Ctrl Pts',(4.74151822683416,-1.18514270861354,6.07120642815316));
#52376=CARTESIAN_POINT('Ctrl Pts',(4.71629112175755,-1.06847604194587,6.08139554862026));
#52377=CARTESIAN_POINT('Ctrl Pts',(4.64631711401595,-0.794772684000621,
6.09420765974442));
#52378=CARTESIAN_POINT('Ctrl Pts',(4.5789340665717,-0.636309800095014,6.09077707494308));
#52379=CARTESIAN_POINT('Ctrl Pts',(4.50417819467794,-0.319434907277067,
6.07909088955251));
#52380=CARTESIAN_POINT('Ctrl Pts',(4.4632640376533,-0.158333333333287,6.06732493430611));
#52381=CARTESIAN_POINT('Ctrl Pts',(4.45587334963848,0.158333333333289,6.03864220529557));
#52382=CARTESIAN_POINT('Ctrl Pts',(4.48924849400527,0.319434907277077,6.02098088567907));
#52383=CARTESIAN_POINT('Ctrl Pts',(4.54925219317818,0.636309800095025,5.97575900359238));
#52384=CARTESIAN_POINT('Ctrl Pts',(4.60908633115064,0.794772684000613,5.94897774902275));
#52385=CARTESIAN_POINT('Ctrl Pts',(4.66673128287468,1.06847604194609,5.89150927474576));
#52386=CARTESIAN_POINT('Ctrl Pts',(4.68683018214767,1.18514270861397,5.86364625932992));
#52387=CARTESIAN_POINT('Ctrl Pts',(4.70207561704814,1.30000000000337,5.83279620159604));
#52388=CARTESIAN_POINT('Ctrl Pts',(4.7798379970422,-1.30000000000266,6.06110253687931));
#52389=CARTESIAN_POINT('Ctrl Pts',(4.76328097334858,-1.18514270861348,6.07786348671036));
#52390=CARTESIAN_POINT('Ctrl Pts',(4.74067709072031,-1.06847604194582,6.08918028975207));
#52391=CARTESIAN_POINT('Ctrl Pts',(4.67448814614907,-0.794772684000584,
6.10274730051581));
#52392=CARTESIAN_POINT('Ctrl Pts',(4.60630253549995,-0.636309800094985,
6.09662993565042));
#52393=CARTESIAN_POINT('Ctrl Pts',(4.53159424561923,-0.319434907277053,
6.0838013327509));
#52394=CARTESIAN_POINT('Ctrl Pts',(4.48951023736959,-0.15833333333328,6.07183198905575));
#52395=CARTESIAN_POINT('Ctrl Pts',(4.4821426868114,0.158333333333282,6.04335038428183));
#52396=CARTESIAN_POINT('Ctrl Pts',(4.51675951190241,0.319434907277061,6.02682073307529));
#52397=CARTESIAN_POINT('Ctrl Pts',(4.57666357621065,0.636309800094995,5.98166978023208));
#52398=CARTESIAN_POINT('Ctrl Pts',(4.63708456690679,0.794772684000577,5.95424377633781));
#52399=CARTESIAN_POINT('Ctrl Pts',(4.69095441782067,1.06847604194604,5.8958353667492));
#52400=CARTESIAN_POINT('Ctrl Pts',(4.70848363320909,1.18514270861392,5.86747665052283));
#52401=CARTESIAN_POINT('Ctrl Pts',(4.72022380159989,1.30000000000331,5.83604205433626));
#52402=CARTESIAN_POINT('Ctrl Pts',(4.79803929283521,-1.30000000000263,6.06614678322407));
#52403=CARTESIAN_POINT('Ctrl Pts',(4.78497732456114,-1.18514270861345,6.08322755623773));
#52404=CARTESIAN_POINT('Ctrl Pts',(4.76493629506773,-1.0684760419458,6.09485086245138));
#52405=CARTESIAN_POINT('Ctrl Pts',(4.702514480171,-0.794772684000566,6.10909518496873));
#52406=CARTESIAN_POINT('Ctrl Pts',(4.6337583158824,-0.636309800094968,6.10392234455836));
#52407=CARTESIAN_POINT('Ctrl Pts',(4.55913407892579,-0.319434907277044,
6.09061273470484));
#52408=CARTESIAN_POINT('Ctrl Pts',(4.51580190865141,-0.158333333333275,
6.07705069401337));
#52409=CARTESIAN_POINT('Ctrl Pts',(4.5083421663999,0.158333333333278,6.04742756797417));
#52410=CARTESIAN_POINT('Ctrl Pts',(4.544036612003,0.319434907277053,6.03047774157301));
#52411=CARTESIAN_POINT('Ctrl Pts',(4.60382842848645,0.636309800094978,5.98525747815496));
#52412=CARTESIAN_POINT('Ctrl Pts',(4.66500701574621,0.794772684000556,5.95889528869559));
#52413=CARTESIAN_POINT('Ctrl Pts',(4.71517494313533,1.06847604194601,5.90023635608127));
#52414=CARTESIAN_POINT('Ctrl Pts',(4.73015035970638,1.18514270861389,5.87151429963215));
#52415=CARTESIAN_POINT('Ctrl Pts',(4.73838535598652,1.30000000000328,5.83946146513514));
#52416=CARTESIAN_POINT('Ctrl Pts',(4.81094807828055,-1.30000000000258,6.07031856917121));
#52417=CARTESIAN_POINT('Ctrl Pts',(4.80040109501589,-1.18514270861341,6.08840887737886));
#52418=CARTESIAN_POINT('Ctrl Pts',(4.78219419594427,-1.06847604194576,6.10063671605705));
#52419=CARTESIAN_POINT('Ctrl Pts',(4.72243667893648,-0.794772684000535,
6.11534199217825));
#52420=CARTESIAN_POINT('Ctrl Pts',(4.65317658805189,-0.636309800094944,
6.10903162237028));
#52421=CARTESIAN_POINT('Ctrl Pts',(4.57859096384098,-0.319434907277032,
6.09488648935993));
#52422=CARTESIAN_POINT('Ctrl Pts',(4.53439696116877,-0.158333333333269,
6.08059548100309));
#52423=CARTESIAN_POINT('Ctrl Pts',(4.52693655107921,0.158333333333272,6.05083684999365));
#52424=CARTESIAN_POINT('Ctrl Pts',(4.56349429876338,0.319434907277041,6.03460096200745));
#52425=CARTESIAN_POINT('Ctrl Pts',(4.62324178818616,0.636309800094954,5.98969480751174));
#52426=CARTESIAN_POINT('Ctrl Pts',(4.68491393411039,0.794772684000524,5.96367396250213));
#52427=CARTESIAN_POINT('Ctrl Pts',(4.73241342899345,1.06847604194597,5.90433667604155));
#52428=CARTESIAN_POINT('Ctrl Pts',(4.74555459285911,1.18514270861384,5.87507424421135));
#52429=CARTESIAN_POINT('Ctrl Pts',(4.75127614928519,1.30000000000323,5.84223429319674));
#52430=CARTESIAN_POINT('Ctrl Pts',(4.8185298804356,-1.30000000000257,6.07259108813827));
#52431=CARTESIAN_POINT('Ctrl Pts',(4.80945416287109,-1.1851427086134,6.09110994876213));
#52432=CARTESIAN_POINT('Ctrl Pts',(4.79232260434384,-1.06847604194575,6.10361999370318));
#52433=CARTESIAN_POINT('Ctrl Pts',(4.73413467280032,-0.794772684000532,
6.11863913385612));
#52434=CARTESIAN_POINT('Ctrl Pts',(4.66460317470995,-0.636309800094941,
6.11214114341466));
#52435=CARTESIAN_POINT('Ctrl Pts',(4.5900426618142,-0.31943490727703,6.09758341926879));
#52436=CARTESIAN_POINT('Ctrl Pts',(4.54532685018444,-0.158333333333269,
6.08260397486844));
#52437=CARTESIAN_POINT('Ctrl Pts',(4.53785597458308,0.158333333333271,6.05264851354725));
#52438=CARTESIAN_POINT('Ctrl Pts',(4.57491371826594,0.319434907277039,6.03679573423671));
#52439=CARTESIAN_POINT('Ctrl Pts',(4.63463789281222,0.636309800094951,5.99212224239495));
#52440=CARTESIAN_POINT('Ctrl Pts',(4.69661644685499,0.794772684000521,5.96647342222013));
#52441=CARTESIAN_POINT('Ctrl Pts',(4.74255240611472,1.06847604194597,5.90679120314264));
#52442=CARTESIAN_POINT('Ctrl Pts',(4.75461520664285,1.18514270861384,5.87720825205933));
#52443=CARTESIAN_POINT('Ctrl Pts',(4.75885683303048,1.30000000000322,5.84387657108736));
#52444=CARTESIAN_POINT('Ctrl Pts',(4.82156335065102,-1.30000000000257,6.07351992691993));
#52445=CARTESIAN_POINT('Ctrl Pts',(4.81307603159707,-1.1851427086134,6.09221744319849));
#52446=CARTESIAN_POINT('Ctrl Pts',(4.79637446542063,-1.06847604194575,6.10484289962611));
#52447=CARTESIAN_POINT('Ctrl Pts',(4.73881395230902,-0.79477268400053,6.11998255672066));
#52448=CARTESIAN_POINT('Ctrl Pts',(4.669172937198,-0.63630980009494,6.11337925974468));
#52449=CARTESIAN_POINT('Ctrl Pts',(4.59462305158774,-0.31943490727703,6.09865712892641));
#52450=CARTESIAN_POINT('Ctrl Pts',(4.54970080024142,-0.158333333333268,
6.08343482517382));
#52451=CARTESIAN_POINT('Ctrl Pts',(4.54222563209188,0.158333333333271,6.05339961884823));
#52452=CARTESIAN_POINT('Ctrl Pts',(4.57948149923688,0.319434907277039,6.03767582519329));
#52453=CARTESIAN_POINT('Ctrl Pts',(4.63919449888597,0.63630980009495,5.9930738228806));
#52454=CARTESIAN_POINT('Ctrl Pts',(4.70129367065987,0.79477268400052,5.9675537403918));
#52455=CARTESIAN_POINT('Ctrl Pts',(4.7466045404738,1.06847604194597,5.90773699490193));
#52456=CARTESIAN_POINT('Ctrl Pts',(4.758236768349,1.18514270861383,5.87803411752938));
#52457=CARTESIAN_POINT('Ctrl Pts',(4.76188782749003,1.30000000000322,5.84452081547814));
#52458=CARTESIAN_POINT('Ctrl Pts',(4.82687180554659,-1.30000000000256,6.07516303402758));
#52459=CARTESIAN_POINT('Ctrl Pts',(4.81941366164088,-1.1851427086134,6.09418064141752));
#52460=CARTESIAN_POINT('Ctrl Pts',(4.80346422963748,-1.06847604194575,6.10701136017159));
#52461=CARTESIAN_POINT('Ctrl Pts',(4.74700127685497,-0.794772684000528,
6.12235993683822));
#52462=CARTESIAN_POINT('Ctrl Pts',(4.67716837738524,-0.636309800094938,
6.11554555143684));
#52463=CARTESIAN_POINT('Ctrl Pts',(4.60263831817618,-0.319434907277029,
6.10054193746771));
#52464=CARTESIAN_POINT('Ctrl Pts',(4.55735821474082,-0.158333333333268,
6.08493920424772));
#52465=CARTESIAN_POINT('Ctrl Pts',(4.54987431150987,0.15833333333327,6.05475127028888));
#52466=CARTESIAN_POINT('Ctrl Pts',(4.58747219868369,0.319434907277038,6.03919945093894));
#52467=CARTESIAN_POINT('Ctrl Pts',(4.64716203523448,0.636309800094948,5.99468134954926));
#52468=CARTESIAN_POINT('Ctrl Pts',(4.70946959676387,0.794772684000518,5.96935828691381));
#52469=CARTESIAN_POINT('Ctrl Pts',(4.75368817807476,1.06847604194596,5.90931968376478));
#52470=CARTESIAN_POINT('Ctrl Pts',(4.76456883971137,1.18514270861383,5.87942535681887));
#52471=CARTESIAN_POINT('Ctrl Pts',(4.76718957759493,1.30000000000322,5.84562518958093));
#52472=CARTESIAN_POINT('Ctrl Pts',(4.83294183153657,-1.30000000000255,6.07717547848024));
#52473=CARTESIAN_POINT('Ctrl Pts',(4.82666302720955,-1.18514270861339,6.09667934639319));
#52474=CARTESIAN_POINT('Ctrl Pts',(4.81157442383178,-1.06847604194574,6.10980130540581));
#52475=CARTESIAN_POINT('Ctrl Pts',(4.75636433336315,-0.794772684000522,
6.12537216950749));
#52476=CARTESIAN_POINT('Ctrl Pts',(4.68629888445387,-0.636309800094933,
6.11797637025502));
#52477=CARTESIAN_POINT('Ctrl Pts',(4.61179504573014,-0.319434907277026,
6.10263727675094));
#52478=CARTESIAN_POINT('Ctrl Pts',(4.56612601490908,-0.158333333333267,
6.0868969511743));
#52479=CARTESIAN_POINT('Ctrl Pts',(4.55863200153038,0.158333333333269,6.05653705639946));
#52480=CARTESIAN_POINT('Ctrl Pts',(4.59660638914432,0.319434907277035,6.0409884473164));
#52481=CARTESIAN_POINT('Ctrl Pts',(4.65625413071718,0.636309800094943,5.99637900850148));
#52482=CARTESIAN_POINT('Ctrl Pts',(4.71878104658324,0.794772684000511,5.97108276538689));
#52483=CARTESIAN_POINT('Ctrl Pts',(4.76175471078031,1.06847604194595,5.91081980006133));
#52484=CARTESIAN_POINT('Ctrl Pts',(4.77178386433909,1.18514270861382,5.88078275953025));
#52485=CARTESIAN_POINT('Ctrl Pts',(4.77324046455682,1.30000000000321,5.84679428319473));
#52486=CARTESIAN_POINT('Ctrl Pts',(4.8390112966445,-1.30000000000254,6.07922833436859));
#52487=CARTESIAN_POINT('Ctrl Pts',(4.8339135640654,-1.18514270861338,6.09927229604029));
#52488=CARTESIAN_POINT('Ctrl Pts',(4.81968675892488,-1.06847604194573,6.11271650145966));
#52489=CARTESIAN_POINT('Ctrl Pts',(4.76573000910636,-0.794772684000516,
6.12852854826283));
#52490=CARTESIAN_POINT('Ctrl Pts',(4.69542749616083,-0.636309800094927,
6.12045465101031));
#52491=CARTESIAN_POINT('Ctrl Pts',(4.62095209785004,-0.319434907277023,
6.10478117796908));
#52492=CARTESIAN_POINT('Ctrl Pts',(4.57490134636149,-0.158333333333265,
6.08897820923182));
#52493=CARTESIAN_POINT('Ctrl Pts',(4.56739926580259,0.158333333333267,6.05846060622671));
#52494=CARTESIAN_POINT('Ctrl Pts',(4.60574790329659,0.319434907277033,6.04289046439477));
#52495=CARTESIAN_POINT('Ctrl Pts',(4.66534955738218,0.636309800094938,5.99814438476442));
#52496=CARTESIAN_POINT('Ctrl Pts',(4.72808987051969,0.794772684000504,5.97281491664591));
#52497=CARTESIAN_POINT('Ctrl Pts',(4.7698168520734,1.06847604194594,5.91230119986894));
#52498=CARTESIAN_POINT('Ctrl Pts',(4.77899489585878,1.18514270861381,5.88212034815777));
#52499=CARTESIAN_POINT('Ctrl Pts',(4.77928891925188,1.3000000000032,5.84795279047415));
#52500=CARTESIAN_POINT('Ctrl Pts',(4.84356149439792,-1.30000000000254,6.08073619732913));
#52501=CARTESIAN_POINT('Ctrl Pts',(4.8393482645136,-1.18514270861337,6.1011533481644));
#52502=CARTESIAN_POINT('Ctrl Pts',(4.82576733162132,-1.06847604194572,6.11482793676999));
#52503=CARTESIAN_POINT('Ctrl Pts',(4.77275139183321,-0.794772684000512,
6.13084230444543));
#52504=CARTESIAN_POINT('Ctrl Pts',(4.70227599982204,-0.636309800094924,
6.12238275651382));
#52505=CARTESIAN_POINT('Ctrl Pts',(4.6278224045325,-0.319434907277022,6.10647297836777));
#52506=CARTESIAN_POINT('Ctrl Pts',(4.58148079102623,-0.158333333333265,
6.09052479916083));
#52507=CARTESIAN_POINT('Ctrl Pts',(4.57397362820661,0.158333333333267,6.0598899687823));
#52508=CARTESIAN_POINT('Ctrl Pts',(4.61260710790117,0.319434907277032,6.04436986604123));
#52509=CARTESIAN_POINT('Ctrl Pts',(4.67217851650135,0.636309800094935,5.99957638132379));
#52510=CARTESIAN_POINT('Ctrl Pts',(4.7350844771806,0.794772684000501,5.97428347733527));
#52511=CARTESIAN_POINT('Ctrl Pts',(4.77587357611191,1.06847604194594,5.91354819880508));
#52512=CARTESIAN_POINT('Ctrl Pts',(4.78440989833677,1.1851427086138,5.88322022759615));
#52513=CARTESIAN_POINT('Ctrl Pts',(4.78382645324408,1.30000000000319,5.84885433679028));
#52514=CARTESIAN_POINT('Ctrl Pts',(4.84735109619278,-1.30000000000253,6.08194736323051));
#52515=CARTESIAN_POINT('Ctrl Pts',(4.84387297711041,-1.18514270861336,6.10262734294782));
#52516=CARTESIAN_POINT('Ctrl Pts',(4.83082945738997,-1.06847604194572,6.11647464917));
#52517=CARTESIAN_POINT('Ctrl Pts',(4.77859832846308,-0.794772684000508,
6.13267985404193));
#52518=CARTESIAN_POINT('Ctrl Pts',(4.70798563528429,-0.63630980009492,6.12406340049069));
#52519=CARTESIAN_POINT('Ctrl Pts',(4.63355045458484,-0.31943490727702,6.10797546379102));
#52520=CARTESIAN_POINT('Ctrl Pts',(4.58695984285549,-0.158333333333264,
6.09177860752226));
#52521=CARTESIAN_POINT('Ctrl Pts',(4.57944918836609,0.158333333333266,6.06104441523148));
#52522=CARTESIAN_POINT('Ctrl Pts',(4.61832512952634,0.31943490727703,6.04564528896951));
#52523=CARTESIAN_POINT('Ctrl Pts',(4.67787721388067,0.636309800094931,6.000885293576));
#52524=CARTESIAN_POINT('Ctrl Pts',(4.74092911393698,0.794772684000496,5.97570879341499));
#52525=CARTESIAN_POINT('Ctrl Pts',(4.78093385702523,1.06847604194593,5.91475556026459));
#52526=CARTESIAN_POINT('Ctrl Pts',(4.78893147581347,1.1851427086138,5.88425932578742));
#52527=CARTESIAN_POINT('Ctrl Pts',(4.78761014242878,1.30000000000318,5.84965125292416));
#52528=CARTESIAN_POINT('Ctrl Pts',(4.84981335970265,-1.30000000000253,6.08271543673521));
#52529=CARTESIAN_POINT('Ctrl Pts',(4.84681216960126,-1.18514270861336,6.10354542857903));
#52530=CARTESIAN_POINT('Ctrl Pts',(4.83411760053641,-1.06847604194572,6.1174966921877));
#52531=CARTESIAN_POINT('Ctrl Pts',(4.78239696189765,-0.794772684000507,
6.13383566375637));
#52532=CARTESIAN_POINT('Ctrl Pts',(4.71169803130065,-0.63630980009492,6.12518762763234));
#52533=CARTESIAN_POINT('Ctrl Pts',(4.63727503230506,-0.319434907277019,
6.10899387850149));
#52534=CARTESIAN_POINT('Ctrl Pts',(4.59051985296273,-0.158333333333263,
6.09258456230556));
#52535=CARTESIAN_POINT('Ctrl Pts',(4.58300720612642,0.158333333333266,6.06178474597553));
#52536=CARTESIAN_POINT('Ctrl Pts',(4.6220426819302,0.319434907277029,6.04649333922819));
#52537=CARTESIAN_POINT('Ctrl Pts',(4.68158471984265,0.63630980009493,6.00178516205892));
#52538=CARTESIAN_POINT('Ctrl Pts',(4.74473500781343,0.794772684000495,5.97672300320449));
#52539=CARTESIAN_POINT('Ctrl Pts',(4.7842289634859,1.06847604194593,5.91561562779994));
#52540=CARTESIAN_POINT('Ctrl Pts',(4.79187486711119,1.1851427086138,5.88499139560751));
#52541=CARTESIAN_POINT('Ctrl Pts',(4.79007120434632,1.30000000000318,5.85019404978402));
#52542=CARTESIAN_POINT('Ctrl Pts',(4.85094964634893,-1.30000000000253,6.08306779187192));
#52543=CARTESIAN_POINT('Ctrl Pts',(4.84816846260519,-1.18514270861336,6.10396475566952));
#52544=CARTESIAN_POINT('Ctrl Pts',(4.83563490089031,-1.06847604194572,6.11796318511599));
#52545=CARTESIAN_POINT('Ctrl Pts',(4.78414992192894,-0.794772684000507,
6.13436536311531));
#52546=CARTESIAN_POINT('Ctrl Pts',(4.71341155752716,-0.63630980009492,6.1257109881841));
#52547=CARTESIAN_POINT('Ctrl Pts',(4.63899425350069,-0.319434907277019,
6.10947015908353));
#52548=CARTESIAN_POINT('Ctrl Pts',(4.59216286874051,-0.158333333333263,
6.09295777030185));
#52549=CARTESIAN_POINT('Ctrl Pts',(4.58464934874306,0.158333333333266,6.0621275986729));
#52550=CARTESIAN_POINT('Ctrl Pts',(4.62375862448146,0.319434907277029,6.0468883650167));
#52551=CARTESIAN_POINT('Ctrl Pts',(4.68329631008815,0.63630980009493,6.00220728330628));
#52552=CARTESIAN_POINT('Ctrl Pts',(4.74649242772978,0.794772684000495,5.97720262890682));
#52553=CARTESIAN_POINT('Ctrl Pts',(4.78575057188746,1.06847604194593,5.9160228008181));
#52554=CARTESIAN_POINT('Ctrl Pts',(4.79323399432667,1.1851427086138,5.88533740405829));
#52555=CARTESIAN_POINT('Ctrl Pts',(4.79120744325674,1.30000000000318,5.85044909118237));
#52556=CARTESIAN_POINT('Ctrl Pts',(4.85151776293019,-1.30000000000253,6.08324358479667));
#52557=CARTESIAN_POINT('Ctrl Pts',(4.84884655889996,-1.18514270861336,6.10417359305687));
#52558=CARTESIAN_POINT('Ctrl Pts',(4.8363934910204,-1.06847604194572,6.11819544663104));
#52559=CARTESIAN_POINT('Ctrl Pts',(4.78502635064411,-0.794772684000507,
6.13462951415317));
#52560=CARTESIAN_POINT('Ctrl Pts',(4.71426833995495,-0.63630980009492,6.12597354378368));
#52561=CARTESIAN_POINT('Ctrl Pts',(4.63985390202787,-0.319434907277019,
6.10970958088203));
#52562=CARTESIAN_POINT('Ctrl Pts',(4.59298437609572,-0.158333333333263,
6.09314483996833));
#52563=CARTESIAN_POINT('Ctrl Pts',(4.58547042767463,0.158333333333266,6.06229945950021));
#52564=CARTESIAN_POINT('Ctrl Pts',(4.62461662402917,0.319434907277029,6.04708659910565));
#52565=CARTESIAN_POINT('Ctrl Pts',(4.68415218438462,0.63630980009493,6.00241960966407));
#52566=CARTESIAN_POINT('Ctrl Pts',(4.74737129829366,0.794772684000495,5.97744465461301));
#52567=CARTESIAN_POINT('Ctrl Pts',(4.78651153236238,1.06847604194593,5.91622840739023));
#52568=CARTESIAN_POINT('Ctrl Pts',(4.7939136905355,1.1851427086138,5.88551206469203));
#52569=CARTESIAN_POINT('Ctrl Pts',(4.79177564984189,1.30000000000318,5.85057762443301));
#52570=CARTESIAN_POINT('Ctrl Pts',(4.85199117167453,-1.30000000000253,6.08338979720196));
#52571=CARTESIAN_POINT('Ctrl Pts',(4.8494116027254,-1.18514270861336,6.10434707702687));
#52572=CARTESIAN_POINT('Ctrl Pts',(4.83702560731203,-1.06847604194572,6.11838836417142));
#52573=CARTESIAN_POINT('Ctrl Pts',(4.78575667319626,-0.794772684000506,
6.13484921979393));
#52574=CARTESIAN_POINT('Ctrl Pts',(4.71498234069302,-0.636309800094919,
6.12619298053283));
#52575=CARTESIAN_POINT('Ctrl Pts',(4.64057029990235,-0.319434907277019,
6.10990994199582));
#52576=CARTESIAN_POINT('Ctrl Pts',(4.59366895218851,-0.158333333333263,
6.09330085972181));
#52577=CARTESIAN_POINT('Ctrl Pts',(4.58615465430625,0.158333333333266,6.06244281756089));
#52578=CARTESIAN_POINT('Ctrl Pts',(4.62533164690651,0.319434907277029,6.04725236075715));
#52579=CARTESIAN_POINT('Ctrl Pts',(4.68486547541404,0.63630980009493,6.0025975506947));
#52580=CARTESIAN_POINT('Ctrl Pts',(4.74810380440349,0.794772684000494,5.97764789769707));
#52581=CARTESIAN_POINT('Ctrl Pts',(4.78714577026928,1.06847604194593,5.91640110141059));
#52582=CARTESIAN_POINT('Ctrl Pts',(4.79448018794372,1.1851427086138,5.88565868956355));
#52583=CARTESIAN_POINT('Ctrl Pts',(4.79224920291661,1.30000000000318,5.85068533456457));
#52584=CARTESIAN_POINT('Ctrl Pts',(4.85232255024837,-1.30000000000253,6.08349210501827));
#52585=CARTESIAN_POINT('Ctrl Pts',(4.84980711534308,-1.18514270861336,6.10446835008361));
#52586=CARTESIAN_POINT('Ctrl Pts',(4.83746806547677,-1.06847604194572,6.11852320156077));
#52587=CARTESIAN_POINT('Ctrl Pts',(4.78626787610001,-0.794772684000506,
6.13500291632764));
#52588=CARTESIAN_POINT('Ctrl Pts',(4.71548213668488,-0.636309800094919,
6.1263468992948));
#52589=CARTESIAN_POINT('Ctrl Pts',(4.64107179257917,-0.319434907277019,
6.11005080784577));
#52590=CARTESIAN_POINT('Ctrl Pts',(4.59414818736665,-0.158333333333263,
6.0934108481001));
#52591=CARTESIAN_POINT('Ctrl Pts',(4.58663364693649,0.158333333333266,6.06254390033073));
#52592=CARTESIAN_POINT('Ctrl Pts',(4.62583217203044,0.319434907277029,6.04736874073722));
#52593=CARTESIAN_POINT('Ctrl Pts',(4.68536479253069,0.63630980009493,6.00272243929111));
#52594=CARTESIAN_POINT('Ctrl Pts',(4.74861659642694,0.794772684000494,5.97779085964576));
#52595=CARTESIAN_POINT('Ctrl Pts',(4.78758979248769,1.06847604194593,5.91652274959415));
#52596=CARTESIAN_POINT('Ctrl Pts',(4.79487679837593,1.1851427086138,5.88576206683842));
#52597=CARTESIAN_POINT('Ctrl Pts',(4.79258075767685,1.30000000000318,5.85076139596124));
#52598=CARTESIAN_POINT('Ctrl Pts',(4.85251190324314,-1.30000000000253,6.08355044596462));
#52599=CARTESIAN_POINT('Ctrl Pts',(4.85003311963239,-1.18514270861336,6.10453752533249));
#52600=CARTESIAN_POINT('Ctrl Pts',(4.83772089855381,-1.06847604194571,6.11860013226608));
#52601=CARTESIAN_POINT('Ctrl Pts',(4.78655999708807,-0.794772684000506,
6.13509065093837));
#52602=CARTESIAN_POINT('Ctrl Pts',(4.7157677494904,-0.636309800094919,6.12643492366188));
#52603=CARTESIAN_POINT('Ctrl Pts',(4.64135836161881,-0.319434907277019,
6.11013118911448));
#52604=CARTESIAN_POINT('Ctrl Pts',(4.59442199860524,-0.158333333333263,
6.09347303387878));
#52605=CARTESIAN_POINT('Ctrl Pts',(4.58690732254322,0.158333333333266,6.06260105720591));
#52606=CARTESIAN_POINT('Ctrl Pts',(4.62611819457161,0.319434907277029,6.047435271639));
#52607=CARTESIAN_POINT('Ctrl Pts',(4.68565014319882,0.63630980009493,6.00279409494844));
#52608=CARTESIAN_POINT('Ctrl Pts',(4.74890965125886,0.794772684000494,5.97787278285643));
#52609=CARTESIAN_POINT('Ctrl Pts',(4.78784352652163,1.06847604194593,5.91659230348755));
#52610=CARTESIAN_POINT('Ctrl Pts',(4.79510342179896,1.1851427086138,5.88582104180445));
#52611=CARTESIAN_POINT('Ctrl Pts',(4.79277018039452,1.30000000000318,5.85080456729165));
#52612=CARTESIAN_POINT('Ctrl Pts',(4.86472558979003,-1.30000000000256,6.08732701272415));
#52613=CARTESIAN_POINT('Ctrl Pts',(4.8646099437343,-1.18514270861339,6.1090082878518));
#52614=CARTESIAN_POINT('Ctrl Pts',(4.85402760574505,-1.06847604194574,6.12356913043093));
#52615=CARTESIAN_POINT('Ctrl Pts',(4.80540013577967,-0.794772684000528,
6.14075796605051));
#52616=CARTESIAN_POINT('Ctrl Pts',(4.73418764713308,-0.636309800094937,
6.13211774128059));
#52617=CARTESIAN_POINT('Ctrl Pts',(4.65984242997234,-0.319434907277028,
6.11535711134947));
#52618=CARTESIAN_POINT('Ctrl Pts',(4.61208889892998,-0.158333333333268,
6.09760172484103));
#52619=CARTESIAN_POINT('Ctrl Pts',(4.60456520912973,0.15833333333327,6.06639620794663));
#52620=CARTESIAN_POINT('Ctrl Pts',(4.64456604111084,0.319434907277037,6.05173924304811));
#52621=CARTESIAN_POINT('Ctrl Pts',(4.70405251924755,0.636309800094947,6.00739471694425));
#52622=CARTESIAN_POINT('Ctrl Pts',(4.76780941860996,0.794772684000517,5.98315811264259));
#52623=CARTESIAN_POINT('Ctrl Pts',(4.80421088102902,1.06847604194596,5.92110660856591));
#52624=CARTESIAN_POINT('Ctrl Pts',(4.80972472899935,1.18514270861383,5.88966949830968));
#52625=CARTESIAN_POINT('Ctrl Pts',(4.80499558066583,1.30000000000321,5.85365507467733));
#52626=CARTESIAN_POINT('Ctrl Pts',(4.88902711963931,-1.30000000000283,6.09588044237462));
#52627=CARTESIAN_POINT('Ctrl Pts',(4.89362272238644,-1.18514270861364,6.11974191404088));
#52628=CARTESIAN_POINT('Ctrl Pts',(4.88648376275866,-1.06847604194596,6.1356918865946));
#52629=CARTESIAN_POINT('Ctrl Pts',(4.84288215129751,-0.794772684000684,
6.15426236833479));
#52630=CARTESIAN_POINT('Ctrl Pts',(4.77077405342329,-0.636309800095067,
6.14378744785621));
#52631=CARTESIAN_POINT('Ctrl Pts',(4.69656033089538,-0.319434907277095,
6.12570668923954));
#52632=CARTESIAN_POINT('Ctrl Pts',(4.64725062312647,-0.1583333333333,6.10673167683751));
#52633=CARTESIAN_POINT('Ctrl Pts',(4.63971054859242,0.158333333333302,6.07482811089041));
#52634=CARTESIAN_POINT('Ctrl Pts',(4.68126272296262,0.319434907277101,6.06099583291417));
#52635=CARTESIAN_POINT('Ctrl Pts',(4.74056080461783,0.636309800095076,6.01593214642562));
#52636=CARTESIAN_POINT('Ctrl Pts',(4.80507337495969,0.794772684000679,5.99020181338789));
#52637=CARTESIAN_POINT('Ctrl Pts',(4.83652787897588,1.06847604194618,5.92725255822721));
#52638=CARTESIAN_POINT('Ctrl Pts',(4.83868267738028,1.18514270861407,5.89559025311695));
#52639=CARTESIAN_POINT('Ctrl Pts',(4.82937678490462,1.30000000000348,5.85951404295586));
#52640=CARTESIAN_POINT('Ctrl Pts',(4.91321985407802,-1.30000000000309,6.10393818921991));
#52641=CARTESIAN_POINT('Ctrl Pts',(4.92249447745382,-1.18514270861388,6.12979090408451));
#52642=CARTESIAN_POINT('Ctrl Pts',(4.9187793331044,-1.06847604194618,6.14706683418608));
#52643=CARTESIAN_POINT('Ctrl Pts',(4.88018764440598,-0.794772684000851,
6.16716360017606));
#52644=CARTESIAN_POINT('Ctrl Pts',(4.80721762555925,-0.636309800095196,
6.15542465374956));
#52645=CARTESIAN_POINT('Ctrl Pts',(4.73316183802081,-0.319434907277159,
6.13649746895652));
#52646=CARTESIAN_POINT('Ctrl Pts',(4.68232035769752,-0.158333333333332,
6.11658777091958));
#52647=CARTESIAN_POINT('Ctrl Pts',(4.67477123300628,0.158333333333334,6.08402952940802));
#52648=CARTESIAN_POINT('Ctrl Pts',(4.71780718131348,0.319434907277167,6.07001371293154));
#52649=CARTESIAN_POINT('Ctrl Pts',(4.77700822866973,0.636309800095206,6.02540714069458));
#52650=CARTESIAN_POINT('Ctrl Pts',(4.84258681448599,0.794772684000839,6.00223009691712));
#52651=CARTESIAN_POINT('Ctrl Pts',(4.86900238110365,1.0684760419464,5.93741886519659));
#52652=CARTESIAN_POINT('Ctrl Pts',(4.86766876330111,1.18514270861432,5.90399949146263));
#52653=CARTESIAN_POINT('Ctrl Pts',(4.85356720770038,1.30000000000375,5.86521512471389));
#52654=CARTESIAN_POINT('Ctrl Pts',(4.92533609403191,-1.30000000000309,6.10851264972719));
#52655=CARTESIAN_POINT('Ctrl Pts',(4.93693489080362,-1.18514270861388,6.1351757774929));
#52656=CARTESIAN_POINT('Ctrl Pts',(4.93492178515123,-1.06847604194618,6.1530199706002));
#52657=CARTESIAN_POINT('Ctrl Pts',(4.89882489072261,-0.794772684000851,
6.17387012311378));
#52658=CARTESIAN_POINT('Ctrl Pts',(4.82544129359841,-0.636309800095196,
6.16200266174069));
#52659=CARTESIAN_POINT('Ctrl Pts',(4.75146299020767,-0.319434907277159,
6.14255691938095));
#52660=CARTESIAN_POINT('Ctrl Pts',(4.69984189087486,-0.158333333333332,
6.12160410624644));
#52661=CARTESIAN_POINT('Ctrl Pts',(4.69228837762174,0.158333333333334,6.08857601784043));
#52662=CARTESIAN_POINT('Ctrl Pts',(4.73609341170092,0.319434907277167,6.07498424576916));
#52663=CARTESIAN_POINT('Ctrl Pts',(4.79522055198674,0.636309800095206,6.03024314493691));
#52664=CARTESIAN_POINT('Ctrl Pts',(4.86122784986915,0.794772684000841,6.0069681780851));
#52665=CARTESIAN_POINT('Ctrl Pts',(4.88516330785021,1.0684760419464,5.9414791270764));
#52666=CARTESIAN_POINT('Ctrl Pts',(4.88213395050327,1.18514270861431,5.90764937166149));
#52667=CARTESIAN_POINT('Ctrl Pts',(4.86571446294546,1.30000000000375,5.86833764440499));
#52668=CARTESIAN_POINT('',(4.76941883344573,1.2,5.87518152519931));
#52669=CARTESIAN_POINT('Ctrl Pts',(4.76941883344572,1.2,5.87518152519931));
#52670=CARTESIAN_POINT('Ctrl Pts',(4.74961204056679,1.21680461799894,5.86666410782715));
#52671=CARTESIAN_POINT('Ctrl Pts',(4.72990091069275,1.23316973561102,5.85707750905065));
#52672=CARTESIAN_POINT('Ctrl Pts',(4.70474620103762,1.25441876751169,5.84645216075377));
#52673=CARTESIAN_POINT('Ctrl Pts',(4.70038407444622,1.25810278200312,5.84461785213178));
#52674=CARTESIAN_POINT('Ctrl Pts',(4.68036604493196,1.27496667239558,5.83609863719043));
#52675=CARTESIAN_POINT('Ctrl Pts',(4.66554413690735,1.28742980080914,5.82982295251271));
#52676=CARTESIAN_POINT('Ctrl Pts',(4.65067750876737,1.30000000000347,5.82388274140186));
#52677=CARTESIAN_POINT('',(4.80892752422524,0.65383484141801,6.02666455499999));
#52678=CARTESIAN_POINT('Ctrl Pts',(4.80892752424968,0.653834841417331,6.02666455499128));
#52679=CARTESIAN_POINT('Ctrl Pts',(4.80506100115371,0.718122177489598,6.01081756986998));
#52680=CARTESIAN_POINT('Ctrl Pts',(4.80189346001836,0.763538358793002,5.99808354372755));
#52681=CARTESIAN_POINT('Ctrl Pts',(4.78910823433444,0.949783543739865,5.94773239137322));
#52682=CARTESIAN_POINT('Ctrl Pts',(4.78204164843337,1.04839967606025,5.92062434825642));
#52683=CARTESIAN_POINT('Ctrl Pts',(4.76941883344572,1.2,5.87518152519931));
#52684=CARTESIAN_POINT('',(4.84008270153026,-0.653834841531101,6.16264786964716));
#52685=CARTESIAN_POINT('Ctrl Pts',(4.84008270153025,-0.653834841531099,
6.16264786964715));
#52686=CARTESIAN_POINT('Ctrl Pts',(4.79944932185601,-0.575798355642387,
6.15340830475714));
#52687=CARTESIAN_POINT('Ctrl Pts',(4.76554358800515,-0.493918960588331,
6.14499354505786));
#52688=CARTESIAN_POINT('Ctrl Pts',(4.71701549206806,-0.338195044740467,
6.13032179136123));
#52689=CARTESIAN_POINT('Ctrl Pts',(4.70027425207649,-0.265709840048834,
6.12394244996249));
#52690=CARTESIAN_POINT('Ctrl Pts',(4.67933806233096,-0.129740191198744,
6.11139089035258));
#52691=CARTESIAN_POINT('Ctrl Pts',(4.67367217159743,-0.0666411092615673,
6.10534940426575));
#52692=CARTESIAN_POINT('Ctrl Pts',(4.6703311450012,0.059549413910394,6.09243289590055));
#52693=CARTESIAN_POINT('Ctrl Pts',(4.67261431641252,0.122794913999556,6.0854643527866));
#52694=CARTESIAN_POINT('Ctrl Pts',(4.68654341749057,0.260150718519473,6.07009424202348));
#52695=CARTESIAN_POINT('Ctrl Pts',(4.69981969456811,0.333951442794183,6.06166111874082));
#52696=CARTESIAN_POINT('Ctrl Pts',(4.74110964114528,0.491144733190181,6.04420974956465));
#52697=CARTESIAN_POINT('Ctrl Pts',(4.77132339271692,0.574255455836941,6.03514263513348));
#52698=CARTESIAN_POINT('Ctrl Pts',(4.80892752419487,0.653834841429595,6.02666455497405));
#52699=CARTESIAN_POINT('',(4.82444742165433,-1.2,6.09220621246874));
#52700=CARTESIAN_POINT('Ctrl Pts',(4.82444742165433,-1.2,6.09220621246874));
#52701=CARTESIAN_POINT('Ctrl Pts',(4.8272118332668,-1.1348197950149,6.10424523870834));
#52702=CARTESIAN_POINT('Ctrl Pts',(4.83083887049113,-1.03881930443303,6.12025722567746));
#52703=CARTESIAN_POINT('Ctrl Pts',(4.83765685676595,-0.795493170498027,
6.15131114758654));
#52704=CARTESIAN_POINT('Ctrl Pts',(4.83870897311039,-0.741489946887419,
6.15623832079));
#52705=CARTESIAN_POINT('Ctrl Pts',(4.84008270153025,-0.6538348415311,6.16264786964715));
#52706=CARTESIAN_POINT('Ctrl Pts',(4.7098133285389,-1.30000000000282,6.04234788891915));
#52707=CARTESIAN_POINT('Ctrl Pts',(4.72925071810808,-1.28307077053216,6.05050207742009));
#52708=CARTESIAN_POINT('Ctrl Pts',(4.74865938770459,-1.26613268536529,6.05870659013052));
#52709=CARTESIAN_POINT('Ctrl Pts',(4.78083864386518,-1.23799653492038,6.07242372484376));
#52710=CARTESIAN_POINT('Ctrl Pts',(4.8036210251056,-1.21801262437289,6.08199369402584));
#52711=CARTESIAN_POINT('Ctrl Pts',(4.82444742165433,-1.2,6.09220621246874));
#52712=CARTESIAN_POINT('Origin',(0.,1.25,7.2));
#52713=CARTESIAN_POINT('Origin',(0.,1.2,7.2));
#52714=CARTESIAN_POINT('Origin',(0.,0.92691742076555,7.2));
#52715=CARTESIAN_POINT('Origin',(0.,0.653834841531101,7.2));
#52716=CARTESIAN_POINT('Origin',(0.,0.,7.2));
#52717=CARTESIAN_POINT('Origin',(0.,-0.653834841531101,7.2));
#52718=CARTESIAN_POINT('Origin',(0.,-0.926917420765551,7.2));
#52719=CARTESIAN_POINT('Origin',(0.,-1.2,7.2));
#52720=CARTESIAN_POINT('Origin',(0.,-1.25,7.2));
#52721=CARTESIAN_POINT('Ctrl Pts',(4.98668722203916,-1.30000000000008,6.43746972924236));
#52722=CARTESIAN_POINT('Ctrl Pts',(4.98569765033805,-1.18514270861184,6.39487827212538));
#52723=CARTESIAN_POINT('Ctrl Pts',(4.97470530482918,-1.06847604194514,6.36274110209538));
#52724=CARTESIAN_POINT('Ctrl Pts',(4.92620237914858,-0.794772684000851,
6.31264930485112));
#52725=CARTESIAN_POINT('Ctrl Pts',(4.85643493010791,-0.636309800095196,
6.31823415136655));
#52726=CARTESIAN_POINT('Ctrl Pts',(4.7842217545151,-0.319434907277159,6.30141029648602));
#52727=CARTESIAN_POINT('Ctrl Pts',(4.73867559286568,-0.158333333333332,
6.30681070736002));
#52728=CARTESIAN_POINT('Ctrl Pts',(4.73214233678194,0.158333333333334,6.27356575659811));
#52729=CARTESIAN_POINT('Ctrl Pts',(4.77077828071913,0.319434907277167,6.2334282166797));
#52730=CARTESIAN_POINT('Ctrl Pts',(4.83045152777451,0.636309800095206,6.18557396029517));
#52731=CARTESIAN_POINT('Ctrl Pts',(4.89266384818737,0.79477268400084,6.14488469691364));
#52732=CARTESIAN_POINT('Ctrl Pts',(4.93412052316908,1.06847604194527,6.149250329368));
#52733=CARTESIAN_POINT('Ctrl Pts',(4.9432174738979,1.1851427086121,6.16473300709073));
#52734=CARTESIAN_POINT('Ctrl Pts',(4.94346631687715,1.30000000000048,6.19380864200933));
#52735=CARTESIAN_POINT('Ctrl Pts',(4.97686019541382,-1.30000000000008,6.44526302673736));
#52736=CARTESIAN_POINT('Ctrl Pts',(4.97396758436905,-1.18514270861184,6.40409612527667));
#52737=CARTESIAN_POINT('Ctrl Pts',(4.96159302098239,-1.06847604194514,6.37302357697528));
#52738=CARTESIAN_POINT('Ctrl Pts',(4.91110009726839,-0.794772684000851,
6.32455974952348));
#52739=CARTESIAN_POINT('Ctrl Pts',(4.84176412504578,-0.636309800095198,
6.33005968031769));
#52740=CARTESIAN_POINT('Ctrl Pts',(4.76953814967829,-0.319434907277161,
6.31338878414013));
#52741=CARTESIAN_POINT('Ctrl Pts',(4.72452210845459,-0.158333333333333,
6.31808899580793));
#52742=CARTESIAN_POINT('Ctrl Pts',(4.71817594716849,0.158333333333335,6.28527505653109));
#52743=CARTESIAN_POINT('Ctrl Pts',(4.75652394684051,0.319434907277168,6.24640754928909));
#52744=CARTESIAN_POINT('Ctrl Pts',(4.81647889553183,0.636309800095209,6.19899550317458));
#52745=CARTESIAN_POINT('Ctrl Pts',(4.8783656650789,0.794772684000845,6.15859186148608));
#52746=CARTESIAN_POINT('Ctrl Pts',(4.92179501812862,1.06847604194528,6.16125451685743));
#52747=CARTESIAN_POINT('Ctrl Pts',(4.93221572520193,1.1851427086121,6.17552577898485));
#52748=CARTESIAN_POINT('Ctrl Pts',(4.93425818162946,1.30000000000048,6.20291573839054));
#52749=CARTESIAN_POINT('Ctrl Pts',(4.95706874230453,-1.30000000000014,6.46030632993531));
#52750=CARTESIAN_POINT('Ctrl Pts',(4.95079122398016,-1.18514270861189,6.42325134866451));
#52751=CARTESIAN_POINT('Ctrl Pts',(4.93588292679964,-1.06847604194519,6.39501776655385));
#52752=CARTESIAN_POINT('Ctrl Pts',(4.88150295217893,-0.794772684000883,
6.3501717405442));
#52753=CARTESIAN_POINT('Ctrl Pts',(4.81225615197418,-0.636309800095221,
6.35334452626117));
#52754=CARTESIAN_POINT('Ctrl Pts',(4.73980482549258,-0.31943490727717,6.33642842109036));
#52755=CARTESIAN_POINT('Ctrl Pts',(4.696170859758,-0.158333333333338,6.34055762075764));
#52756=CARTESIAN_POINT('Ctrl Pts',(4.69012591704432,0.15833333333334,6.30845198515447));
#52757=CARTESIAN_POINT('Ctrl Pts',(4.72754383863126,0.319434907277177,6.27128669989665));
#52758=CARTESIAN_POINT('Ctrl Pts',(4.78803057335667,0.636309800095228,6.22470119665593));
#52759=CARTESIAN_POINT('Ctrl Pts',(4.84961397558834,0.794772684000868,6.18573688361928));
#52760=CARTESIAN_POINT('Ctrl Pts',(4.89700059988731,1.06847604194532,6.18498545886474));
#52761=CARTESIAN_POINT('Ctrl Pts',(4.91001220404317,1.18514270861215,6.19666573939433));
#52762=CARTESIAN_POINT('Ctrl Pts',(4.91552349854335,1.30000000000054,6.22035156438672));
#52763=CARTESIAN_POINT('Ctrl Pts',(4.93691061846834,-1.30000000000018,6.47575166451482));
#52764=CARTESIAN_POINT('Ctrl Pts',(4.92653611020849,-1.18514270861193,6.44097594222251));
#52765=CARTESIAN_POINT('Ctrl Pts',(4.90867909622876,-1.06847604194522,6.41453646114568));
#52766=CARTESIAN_POINT('Ctrl Pts',(4.85013973656912,-0.79477268400091,6.37271435552521));
#52767=CARTESIAN_POINT('Ctrl Pts',(4.78205759083351,-0.636309800095246,
6.37652947871845));
#52768=CARTESIAN_POINT('Ctrl Pts',(4.70966700916279,-0.319434907277184,
6.36018130843371));
#52769=CARTESIAN_POINT('Ctrl Pts',(4.66714547480156,-0.158333333333345,
6.36293868473051));
#52770=CARTESIAN_POINT('Ctrl Pts',(4.66133147057174,0.158333333333347,6.3313827263226));
#52771=CARTESIAN_POINT('Ctrl Pts',(4.69775031582757,0.319434907277193,6.29585311532871));
#52772=CARTESIAN_POINT('Ctrl Pts',(4.75888621980995,0.636309800095257,6.25040153766716));
#52773=CARTESIAN_POINT('Ctrl Pts',(4.82045415980186,0.794772684000902,6.21364759328796));
#52774=CARTESIAN_POINT('Ctrl Pts',(4.8719170783672,1.06847604194536,6.2095231014812));
#52775=CARTESIAN_POINT('Ctrl Pts',(4.88752980681081,1.18514270861219,6.21845908172245));
#52776=CARTESIAN_POINT('Ctrl Pts',(4.89647887314016,1.30000000000058,6.23811638188062));
#52777=CARTESIAN_POINT('Ctrl Pts',(4.92636805940448,-1.30000000000019,6.48376534470158));
#52778=CARTESIAN_POINT('Ctrl Pts',(4.91412619153649,-1.18514270861194,6.45101218262242));
#52779=CARTESIAN_POINT('Ctrl Pts',(4.89487951363381,-1.06847604194523,6.42598062912506));
#52780=CARTESIAN_POINT('Ctrl Pts',(4.83423332490632,-0.794772684000915,
6.38599119352752));
#52781=CARTESIAN_POINT('Ctrl Pts',(4.76631059477317,-0.636309800095249,
6.38886174607922));
#52782=CARTESIAN_POINT('Ctrl Pts',(4.69374505420487,-0.319434907277185,
6.37223471354738));
#52783=CARTESIAN_POINT('Ctrl Pts',(4.65178182810547,-0.158333333333345,
6.37420333831997));
#52784=CARTESIAN_POINT('Ctrl Pts',(4.64610231107768,0.158333333333348,6.34297281401876));
#52785=CARTESIAN_POINT('Ctrl Pts',(4.68219514209646,0.319434907277194,6.30882664971357));
#52786=CARTESIAN_POINT('Ctrl Pts',(4.74358072026792,0.63630980009526,6.26376835475518));
#52787=CARTESIAN_POINT('Ctrl Pts',(4.80473133823679,0.794772684000906,6.22716635240518));
#52788=CARTESIAN_POINT('Ctrl Pts',(4.85833367902391,1.06847604194536,6.22128074130118));
#52789=CARTESIAN_POINT('Ctrl Pts',(4.87540005304793,1.1851427086122,6.22899812669478));
#52790=CARTESIAN_POINT('Ctrl Pts',(4.88633033393167,1.30000000000059,6.24698056044553));
#52791=CARTESIAN_POINT('Ctrl Pts',(4.92512165412919,-1.30000000000019,6.48468994389186));
#52792=CARTESIAN_POINT('Ctrl Pts',(4.91265773749602,-1.18514270861194,6.45216897026815));
#52793=CARTESIAN_POINT('Ctrl Pts',(4.89324644872196,-1.06847604194523,6.42730053234831));
#52794=CARTESIAN_POINT('Ctrl Pts',(4.83235266897639,-0.794772684000915,
6.38752835419998));
#52795=CARTESIAN_POINT('Ctrl Pts',(4.76445543410879,-0.636309800095249,
6.39030617896606));
#52796=CARTESIAN_POINT('Ctrl Pts',(4.69186920163666,-0.319434907277185,
6.3736466176957));
#52797=CARTESIAN_POINT('Ctrl Pts',(4.64996529198419,-0.158333333333345,
6.37550554229197));
#52798=CARTESIAN_POINT('Ctrl Pts',(4.64430108817236,0.158333333333348,6.34431222881329));
#52799=CARTESIAN_POINT('Ctrl Pts',(4.68035913284604,0.319434907277194,6.31033866685585));
#52800=CARTESIAN_POINT('Ctrl Pts',(4.74177782070676,0.63630980009526,6.26533636497439));
#52801=CARTESIAN_POINT('Ctrl Pts',(4.80288296703754,0.794772684000907,6.22876118771136));
#52802=CARTESIAN_POINT('Ctrl Pts',(4.85673799241266,1.06847604194536,6.22267052237588));
#52803=CARTESIAN_POINT('Ctrl Pts',(4.87397495550491,1.1851427086122,6.23024323981494));
#52804=CARTESIAN_POINT('Ctrl Pts',(4.88513703672986,1.30000000000059,6.2480250980354));
#52805=CARTESIAN_POINT('Ctrl Pts',(4.92293833907504,-1.30000000000019,6.48630256823851));
#52806=CARTESIAN_POINT('Ctrl Pts',(4.91008208674477,-1.18514270861194,6.45417672305587));
#52807=CARTESIAN_POINT('Ctrl Pts',(4.89038039954413,-1.06847604194523,6.42958680601259));
#52808=CARTESIAN_POINT('Ctrl Pts',(4.82905123682654,-0.794772684000915,
6.39018868000574));
#52809=CARTESIAN_POINT('Ctrl Pts',(4.76120097554205,-0.636309800095249,
6.39281196796341));
#52810=CARTESIAN_POINT('Ctrl Pts',(4.68858360111441,-0.319434907277185,
6.37610978023243));
#52811=CARTESIAN_POINT('Ctrl Pts',(4.6467921652549,-0.158333333333345,6.37780010804488));
#52812=CARTESIAN_POINT('Ctrl Pts',(4.64115480296635,0.158333333333348,6.34667240984026));
#52813=CARTESIAN_POINT('Ctrl Pts',(4.67714081045394,0.319434907277194,6.31297145333446));
#52814=CARTESIAN_POINT('Ctrl Pts',(4.73861762231401,0.63630980009526,6.26806722692365));
#52815=CARTESIAN_POINT('Ctrl Pts',(4.7996545888502,0.794772684000906,6.23156801465449));
#52816=CARTESIAN_POINT('Ctrl Pts',(4.8539535036347,1.06847604194536,6.22512301388828));
#52817=CARTESIAN_POINT('Ctrl Pts',(4.87148787148143,1.1851427086122,6.23243986365501));
#52818=CARTESIAN_POINT('Ctrl Pts',(4.88305261893776,1.30000000000059,6.24986336520934));
#52819=CARTESIAN_POINT('Ctrl Pts',(4.91855575959217,-1.30000000000019,6.48948322463651));
#52820=CARTESIAN_POINT('Ctrl Pts',(4.90489971974153,-1.18514270861194,6.45810477885079));
#52821=CARTESIAN_POINT('Ctrl Pts',(4.88460837725371,-1.06847604194523,6.43404695026136));
#52822=CARTESIAN_POINT('Ctrl Pts',(4.82240244035806,-0.794772684000913,
6.39538064367556));
#52823=CARTESIAN_POINT('Ctrl Pts',(4.75466619892734,-0.636309800095248,
6.39775306830035));
#52824=CARTESIAN_POINT('Ctrl Pts',(4.6819970277539,-0.319434907277185,6.38099611983521));
#52825=CARTESIAN_POINT('Ctrl Pts',(4.64043601582692,-0.158333333333345,
6.38236366871908));
#52826=CARTESIAN_POINT('Ctrl Pts',(4.63485083995942,0.158333333333347,6.35136490007434));
#52827=CARTESIAN_POINT('Ctrl Pts',(4.67067489536199,0.319434907277194,6.31816401775939));
#52828=CARTESIAN_POINT('Ctrl Pts',(4.73227663170893,0.636309800095259,6.27347865485972));
#52829=CARTESIAN_POINT('Ctrl Pts',(4.79321242094628,0.794772684000905,6.23722144826176));
#52830=CARTESIAN_POINT('Ctrl Pts',(4.84840411962865,1.06847604194536,6.23007975932987));
#52831=CARTESIAN_POINT('Ctrl Pts',(4.86652887652838,1.1851427086122,6.23687296384654));
#52832=CARTESIAN_POINT('Ctrl Pts',(4.8788879490222,1.30000000000059,6.25355074539284));
#52833=CARTESIAN_POINT('Ctrl Pts',(4.90969678062161,-1.30000000000019,6.49559848148463));
#52834=CARTESIAN_POINT('Ctrl Pts',(4.89429034770527,-1.18514270861194,6.4652752091426));
#52835=CARTESIAN_POINT('Ctrl Pts',(4.87273109405207,-1.06847604194523,6.44202331212106));
#52836=CARTESIAN_POINT('Ctrl Pts',(4.80871065842956,-0.794772684000916,
6.40464307008932));
#52837=CARTESIAN_POINT('Ctrl Pts',(4.74137158253816,-0.636309800095248,
6.40701333983432));
#52838=CARTESIAN_POINT('Ctrl Pts',(4.66876019540481,-0.319434907277185,
6.39060475719409));
#52839=CARTESIAN_POINT('Ctrl Pts',(4.62784934778019,-0.158333333333345,
6.39184122976634));
#52840=CARTESIAN_POINT('Ctrl Pts',(4.62236214305987,0.158333333333347,6.36109576080471));
#52841=CARTESIAN_POINT('Ctrl Pts',(4.65756162412944,0.319434907277194,6.32810519387628));
#52842=CARTESIAN_POINT('Ctrl Pts',(4.71945257185647,0.636309800095259,6.28394196729414));
#52843=CARTESIAN_POINT('Ctrl Pts',(4.78056554749451,0.794772684000907,6.2491212948399));
#52844=CARTESIAN_POINT('Ctrl Pts',(4.83759362894242,1.06847604194536,6.24071710639619));
#52845=CARTESIAN_POINT('Ctrl Pts',(4.85685476193013,1.18514270861219,6.24635519381419));
#52846=CARTESIAN_POINT('Ctrl Pts',(4.87069168454543,1.30000000000058,6.26126923042159));
#52847=CARTESIAN_POINT('Ctrl Pts',(4.89713958049952,-1.30000000000017,6.50462396405601));
#52848=CARTESIAN_POINT('Ctrl Pts',(4.87937217586078,-1.18514270861192,6.47622076642019));
#52849=CARTESIAN_POINT('Ctrl Pts',(4.8560702776099,-1.06847604194522,6.45432379139764));
#52850=CARTESIAN_POINT('Ctrl Pts',(4.78945244370591,-0.794772684000906,
6.41876807442275));
#52851=CARTESIAN_POINT('Ctrl Pts',(4.7224340152446,-0.63630980009524,6.42040187127375));
#52852=CARTESIAN_POINT('Ctrl Pts',(4.6496605599142,-0.31943490727718,6.40378804953575));
#52853=CARTESIAN_POINT('Ctrl Pts',(4.60942850882551,-0.158333333333343,
6.40413794851151));
#52854=CARTESIAN_POINT('Ctrl Pts',(4.60410214916729,0.158333333333345,6.37381907547874));
#52855=CARTESIAN_POINT('Ctrl Pts',(4.63883571633811,0.31943490727719,6.34230925296491));
#52856=CARTESIAN_POINT('Ctrl Pts',(4.70111036527886,0.63630980009525,6.29887887268815));
#52857=CARTESIAN_POINT('Ctrl Pts',(4.76195747457999,0.794772684000895,6.26481378454199));
#52858=CARTESIAN_POINT('Ctrl Pts',(4.82158826959047,1.06847604194535,6.25454543594719));
#52859=CARTESIAN_POINT('Ctrl Pts',(4.84256297288892,1.18514270861218,6.25874685006882));
#52860=CARTESIAN_POINT('Ctrl Pts',(4.8587004178645,1.30000000000057,6.27159446593894));
#52861=CARTESIAN_POINT('Ctrl Pts',(4.88212929215244,-1.30000000000016,6.51567079219986));
#52862=CARTESIAN_POINT('Ctrl Pts',(4.86159707438084,-1.18514270861191,6.48979833670658));
#52863=CARTESIAN_POINT('Ctrl Pts',(4.83624723042465,-1.06847604194521,6.46967229640823));
#52864=CARTESIAN_POINT('Ctrl Pts',(4.76655433941777,-0.794772684000905,
6.43645248578523));
#52865=CARTESIAN_POINT('Ctrl Pts',(4.69987163509091,-0.636309800095237,
6.43704889500626));
#52866=CARTESIAN_POINT('Ctrl Pts',(4.62683906545535,-0.319434907277178,
6.41999118933009));
#52867=CARTESIAN_POINT('Ctrl Pts',(4.58735092903532,-0.158333333333342,
6.41905017668548));
#52868=CARTESIAN_POINT('Ctrl Pts',(4.58215666749824,0.158333333333344,6.38906625062512));
#52869=CARTESIAN_POINT('Ctrl Pts',(4.61629639064893,0.319434907277187,6.35926187789649));
#52870=CARTESIAN_POINT('Ctrl Pts',(4.67906261951202,0.636309800095246,6.31679552289548));
#52871=CARTESIAN_POINT('Ctrl Pts',(4.73968915183838,0.79477268400089,6.28389249252736));
#52872=CARTESIAN_POINT('Ctrl Pts',(4.80250707499649,1.06847604194534,6.27154949174964));
#52873=CARTESIAN_POINT('Ctrl Pts',(4.82555758093061,1.18514270861218,6.27407497603294));
#52874=CARTESIAN_POINT('Ctrl Pts',(4.84446704149716,1.30000000000056,6.28446877228295));
#52875=CARTESIAN_POINT('Ctrl Pts',(4.86182565717412,-1.30000000000016,6.52956179564368));
#52876=CARTESIAN_POINT('Ctrl Pts',(4.83734621833198,-1.18514270861191,6.50630411448896));
#52877=CARTESIAN_POINT('Ctrl Pts',(4.80909398668839,-1.06847604194521,6.48803936152431));
#52878=CARTESIAN_POINT('Ctrl Pts',(4.73510977363616,-0.794772684000899,
6.45737879127558));
#52879=CARTESIAN_POINT('Ctrl Pts',(4.66899789504025,-0.636309800095234,
6.45694585784103));
#52880=CARTESIAN_POINT('Ctrl Pts',(4.59585217179943,-0.319434907277178,
6.43999002672486));
#52881=CARTESIAN_POINT('Ctrl Pts',(4.55769689007927,-0.158333333333342,
6.43834269264524));
#52882=CARTESIAN_POINT('Ctrl Pts',(4.55286565414339,0.158333333333344,6.40937925847717));
#52883=CARTESIAN_POINT('Ctrl Pts',(4.5862140872802,0.319434907277186,6.38184240151));
#52884=CARTESIAN_POINT('Ctrl Pts',(4.64946925549905,0.636309800095244,6.34025146852919));
#52885=CARTESIAN_POINT('Ctrl Pts',(4.70941285168286,0.794772684000888,6.30792389975058));
#52886=CARTESIAN_POINT('Ctrl Pts',(4.77637892632758,1.06847604194534,6.29250110299389));
#52887=CARTESIAN_POINT('Ctrl Pts',(4.80222293614429,1.18514270861217,6.29281684556559));
#52888=CARTESIAN_POINT('Ctrl Pts',(4.82492382340163,1.30000000000056,6.30012428795403));
#52889=CARTESIAN_POINT('Ctrl Pts',(4.84154147293362,-1.30000000000014,6.54358302839007));
#52890=CARTESIAN_POINT('Ctrl Pts',(4.81313480855745,-1.1851427086119,6.52301053449656));
#52891=CARTESIAN_POINT('Ctrl Pts',(4.78201025093487,-1.0684760419452,6.50670714550205));
#52892=CARTESIAN_POINT('Ctrl Pts',(4.70382741926839,-0.79477268400089,6.47890554179115));
#52893=CARTESIAN_POINT('Ctrl Pts',(4.63845673257079,-0.636309800095226,
6.47797802085801));
#52894=CARTESIAN_POINT('Ctrl Pts',(4.5651715809394,-0.319434907277173,6.4610415223539));
#52895=CARTESIAN_POINT('Ctrl Pts',(4.52823440680283,-0.158333333333339,
6.4582792046978));
#52896=CARTESIAN_POINT('Ctrl Pts',(4.523479643894,0.158333333333342,6.42952429902268));
#52897=CARTESIAN_POINT('Ctrl Pts',(4.55560208671196,0.319434907277181,6.40310820853837));
#52898=CARTESIAN_POINT('Ctrl Pts',(4.61932427998526,0.636309800095235,6.36233567863279));
#52899=CARTESIAN_POINT('Ctrl Pts',(4.67901776100319,0.794772684000877,6.33174657323979));
#52900=CARTESIAN_POINT('Ctrl Pts',(4.75038445471543,1.06847604194532,6.31392860517125));
#52901=CARTESIAN_POINT('Ctrl Pts',(4.77910498021926,1.18514270861216,6.31226155035503));
#52902=CARTESIAN_POINT('Ctrl Pts',(4.80565403391551,1.30000000000054,6.3166401788787));
#52903=CARTESIAN_POINT('Ctrl Pts',(4.82116243215177,-1.30000000000014,6.55733558918724));
#52904=CARTESIAN_POINT('Ctrl Pts',(4.78883341287566,-1.18514270861189,6.53951145811885));
#52905=CARTESIAN_POINT('Ctrl Pts',(4.75478741066505,-1.06847604194519,6.52504768752977));
#52906=CARTESIAN_POINT('Ctrl Pts',(4.67216776061922,-0.794772684000887,
6.49939658894659));
#52907=CARTESIAN_POINT('Ctrl Pts',(4.60704322956664,-0.636309800095225,
6.49637469731541));
#52908=CARTESIAN_POINT('Ctrl Pts',(4.53351417304343,-0.319434907277172,
6.47915083859645));
#52909=CARTESIAN_POINT('Ctrl Pts',(4.49807225560928,-0.158333333333339,
6.47619891866663));
#52910=CARTESIAN_POINT('Ctrl Pts',(4.49360873628281,0.158333333333341,6.44834180152489));
#52911=CARTESIAN_POINT('Ctrl Pts',(4.52460924588721,0.319434907277181,6.42334992397671));
#52912=CARTESIAN_POINT('Ctrl Pts',(4.58900139539972,0.636309800095234,6.38400740246072));
#52913=CARTESIAN_POINT('Ctrl Pts',(4.64866261035791,0.794772684000875,6.35580900848947));
#52914=CARTESIAN_POINT('Ctrl Pts',(4.72438699513373,1.06847604194532,6.33545359086945));
#52915=CARTESIAN_POINT('Ctrl Pts',(4.7558936377855,1.18514270861215,6.33152370410616));
#52916=CARTESIAN_POINT('Ctrl Pts',(4.78612864278456,1.30000000000054,6.33247503662476));
#52917=CARTESIAN_POINT('Ctrl Pts',(4.80064499571522,-1.30000000000014,6.57074186966073));
#52918=CARTESIAN_POINT('Ctrl Pts',(4.76413166792447,-1.18514270861189,6.55480952312448));
#52919=CARTESIAN_POINT('Ctrl Pts',(4.72705540277594,-1.06847604194519,6.54182573186236));
#52920=CARTESIAN_POINT('Ctrl Pts',(4.64010131528972,-0.794772684000882,
6.51864232918802));
#52921=CARTESIAN_POINT('Ctrl Pts',(4.57609739480573,-0.63630980009522,6.51635936434249));
#52922=CARTESIAN_POINT('Ctrl Pts',(4.50238395474208,-0.31943490727717,6.49901640971187));
#52923=CARTESIAN_POINT('Ctrl Pts',(4.4677782557077,-0.158333333333338,6.49368883985741));
#52924=CARTESIAN_POINT('Ctrl Pts',(4.46341909854567,0.15833333333334,6.4661459081692));
#52925=CARTESIAN_POINT('Ctrl Pts',(4.4936600016079,0.319434907277179,6.44376797469062));
#52926=CARTESIAN_POINT('Ctrl Pts',(4.55850563825248,0.63630980009523,6.40533910736424));
#52927=CARTESIAN_POINT('Ctrl Pts',(4.61736729464155,0.794772684000869,6.37742243298241));
#52928=CARTESIAN_POINT('Ctrl Pts',(4.69750095462133,1.06847604194531,6.35465771123057));
#52929=CARTESIAN_POINT('Ctrl Pts',(4.73199779532328,1.18514270861215,6.34900925101938));
#52930=CARTESIAN_POINT('Ctrl Pts',(4.76630458456664,1.30000000000053,6.34756633512731));
#52931=CARTESIAN_POINT('Ctrl Pts',(4.77472662307008,-1.30000000000012,6.58645074781878));
#52932=CARTESIAN_POINT('Ctrl Pts',(4.73330827518786,-1.18514270861187,6.5740302963003));
#52933=CARTESIAN_POINT('Ctrl Pts',(4.69256680491827,-1.06847604194517,6.56335519378605));
#52934=CARTESIAN_POINT('Ctrl Pts',(4.60000958098637,-0.794772684000873,
6.54272567678683));
#52935=CARTESIAN_POINT('Ctrl Pts',(4.53619379013752,-0.636309800095217,
6.53733495387666));
#52936=CARTESIAN_POINT('Ctrl Pts',(4.46216853663192,-0.31943490727717,6.5196152407362));
#52937=CARTESIAN_POINT('Ctrl Pts',(4.42953403920399,-0.158333333333337,
6.5144177485044));
#52938=CARTESIAN_POINT('Ctrl Pts',(4.42559058451556,0.15833333333334,6.4882478384849));
#52939=CARTESIAN_POINT('Ctrl Pts',(4.45441449289897,0.319434907277177,6.4676825932433));
#52940=CARTESIAN_POINT('Ctrl Pts',(4.52013657539244,0.636309800095227,6.4312667028111));
#52941=CARTESIAN_POINT('Ctrl Pts',(4.5789001329555,0.794772684000868,6.4062686380822));
#52942=CARTESIAN_POINT('Ctrl Pts',(4.66470405570312,1.06847604194531,6.380980410857));
#52943=CARTESIAN_POINT('Ctrl Pts',(4.70283664676022,1.18514270861214,6.3729180923415));
#52944=CARTESIAN_POINT('Ctrl Pts',(4.74196049006563,1.30000000000052,6.36773979185513));
#52945=CARTESIAN_POINT('Ctrl Pts',(4.75153496462463,-1.30000000000011,6.60128956561562));
#52946=CARTESIAN_POINT('Ctrl Pts',(4.70542491577634,-1.18514270861187,6.59109134143449));
#52947=CARTESIAN_POINT('Ctrl Pts',(4.66124595282902,-1.06847604194517,6.58201508893444));
#52948=CARTESIAN_POINT('Ctrl Pts',(4.56364490519314,-0.794772684000872,
6.56363910899422));
#52949=CARTESIAN_POINT('Ctrl Pts',(4.50077518794686,-0.636309800095211,
6.55803052449013));
#52950=CARTESIAN_POINT('Ctrl Pts',(4.42634106799007,-0.319434907277165,
6.53945370326785));
#52951=CARTESIAN_POINT('Ctrl Pts',(4.39468669995836,-0.158333333333335,
6.53155092825692));
#52952=CARTESIAN_POINT('Ctrl Pts',(4.39076683331099,0.158333333333338,6.50551318054222));
#52953=CARTESIAN_POINT('Ctrl Pts',(4.41852656654882,0.319434907277173,6.48750688101309));
#52954=CARTESIAN_POINT('Ctrl Pts',(4.48492480491589,0.636309800095219,6.45278458692865));
#52955=CARTESIAN_POINT('Ctrl Pts',(4.54334400499924,0.794772684000856,6.42982150976879));
#52956=CARTESIAN_POINT('Ctrl Pts',(4.63422280032256,1.0684760419453,6.40216138117284));
#52957=CARTESIAN_POINT('Ctrl Pts',(4.67566990004589,1.18514270861213,6.39198737148927));
#52958=CARTESIAN_POINT('Ctrl Pts',(4.71922603638829,1.30000000000051,6.38361239688253));
#52959=CARTESIAN_POINT('Ctrl Pts',(4.73570235451822,-1.30000000000011,6.60979664855893));
#52960=CARTESIAN_POINT('Ctrl Pts',(4.68648240632083,-1.18514270861186,6.60116566063527));
#52961=CARTESIAN_POINT('Ctrl Pts',(4.64000788798049,-1.06847604194516,6.59316231854331));
#52962=CARTESIAN_POINT('Ctrl Pts',(4.53898494560996,-0.794772684000866,
6.57612298467915));
#52963=CARTESIAN_POINT('Ctrl Pts',(4.47648015595929,-0.636309800095209,
6.56945074464614));
#52964=CARTESIAN_POINT('Ctrl Pts',(4.40194285334807,-0.319434907277165,
6.55094083724988));
#52965=CARTESIAN_POINT('Ctrl Pts',(4.3714743653883,-0.158333333333335,6.54314363023759));
#52966=CARTESIAN_POINT('Ctrl Pts',(4.36771574607594,0.158333333333337,6.51772130069368));
#52967=CARTESIAN_POINT('Ctrl Pts',(4.39449091929033,0.319434907277172,6.5004228962701));
#52968=CARTESIAN_POINT('Ctrl Pts',(4.46123916429103,0.636309800095217,6.46648384759227));
#52969=CARTESIAN_POINT('Ctrl Pts',(4.51931896438363,0.794772684000856,6.44459016033573));
#52970=CARTESIAN_POINT('Ctrl Pts',(4.61378982530285,1.06847604194529,6.41598308369089));
#52971=CARTESIAN_POINT('Ctrl Pts',(4.65761426622038,1.18514270861212,6.40490552984303));
#52972=CARTESIAN_POINT('Ctrl Pts',(4.70437021285387,1.30000000000051,6.3951333656302));
#52973=CARTESIAN_POINT('Ctrl Pts',(4.7252393646867,-1.3000000000001,6.61586137002474));
#52974=CARTESIAN_POINT('Ctrl Pts',(4.67382252237325,-1.18514270861186,6.60782874010441));
#52975=CARTESIAN_POINT('Ctrl Pts',(4.62574478186383,-1.06847604194516,6.60027689400989));
#52976=CARTESIAN_POINT('Ctrl Pts',(4.52238957652034,-0.794772684000865,
6.58394132560799));
#52977=CARTESIAN_POINT('Ctrl Pts',(4.46034180597355,-0.636309800095209,
6.57733202806776));
#52978=CARTESIAN_POINT('Ctrl Pts',(4.38571589031662,-0.319434907277165,
6.55878086823184));
#52979=CARTESIAN_POINT('Ctrl Pts',(4.35586566462306,-0.158333333333335,
6.55040045163682));
#52980=CARTESIAN_POINT('Ctrl Pts',(4.35213895544039,0.158333333333337,6.52512591111799));
#52981=CARTESIAN_POINT('Ctrl Pts',(4.37827665702741,0.319434907277172,6.50841589181447));
#52982=CARTESIAN_POINT('Ctrl Pts',(4.44528264043256,0.636309800095217,6.4751096245853));
#52983=CARTESIAN_POINT('Ctrl Pts',(4.50321590295328,0.794772684000856,6.45419665430419));
#52984=CARTESIAN_POINT('Ctrl Pts',(4.60006593612573,1.0684760419453,6.42491863672633));
#52985=CARTESIAN_POINT('Ctrl Pts',(4.64544722920282,1.18514270861213,6.41314989514694));
#52986=CARTESIAN_POINT('Ctrl Pts',(4.69428702464404,1.30000000000051,6.40228578094015));
#52987=CARTESIAN_POINT('Ctrl Pts',(4.71234108790911,-1.30000000000011,6.62410664981093));
#52988=CARTESIAN_POINT('Ctrl Pts',(4.65836817745684,-1.18514270861186,6.61751085829036));
#52989=CARTESIAN_POINT('Ctrl Pts',(4.60837884174036,-1.06847604194516,6.61085327576169));
#52990=CARTESIAN_POINT('Ctrl Pts',(4.50209633045397,-0.794772684000865,
6.59533017868569));
#52991=CARTESIAN_POINT('Ctrl Pts',(4.4401961854101,-0.636309800095209,6.58721850187003));
#52992=CARTESIAN_POINT('Ctrl Pts',(4.3652774986666,-0.319434907277166,6.56794003407505));
#52993=CARTESIAN_POINT('Ctrl Pts',(4.33619889704844,-0.158333333333335,
6.5588500831238));
#52994=CARTESIAN_POINT('Ctrl Pts',(4.33261304783716,0.158333333333337,6.53412644399904));
#52995=CARTESIAN_POINT('Ctrl Pts',(4.35814120400026,0.319434907277172,6.51885093956372));
#52996=CARTESIAN_POINT('Ctrl Pts',(4.42568365918782,0.636309800095217,6.48703954013807));
#52997=CARTESIAN_POINT('Ctrl Pts',(4.48368809821893,0.794772684000856,6.46807029115539));
#52998=CARTESIAN_POINT('Ctrl Pts',(4.58339644619586,1.0684760419453,6.43758944376375));
#52999=CARTESIAN_POINT('Ctrl Pts',(4.63057769859682,1.18514270861212,6.42450991647051));
#53000=CARTESIAN_POINT('Ctrl Pts',(4.68178015411791,1.30000000000051,6.41154489129317));
#53001=CARTESIAN_POINT('Ctrl Pts',(4.69635329463591,-1.3000000000001,6.63210460558044));
#53002=CARTESIAN_POINT('Ctrl Pts',(4.63915551108548,-1.18514270861185,6.62668263242346));
#53003=CARTESIAN_POINT('Ctrl Pts',(4.58679981984083,-1.06847604194516,6.620852896027));
#53004=CARTESIAN_POINT('Ctrl Pts',(4.47703390122908,-0.794772684000863,
6.6064430240604));
#53005=CARTESIAN_POINT('Ctrl Pts',(4.41565432462298,-0.636309800095207,
6.59776964441761));
#53006=CARTESIAN_POINT('Ctrl Pts',(4.340636532308,-0.319434907277165,6.57857504094738));
#53007=CARTESIAN_POINT('Ctrl Pts',(4.31265878703245,-0.158333333333335,
6.56931862491168));
#53008=CARTESIAN_POINT('Ctrl Pts',(4.30919534601676,0.158333333333337,6.5451218747419));
#53009=CARTESIAN_POINT('Ctrl Pts',(4.33378623887568,0.319434907277173,6.53073886803835));
#53010=CARTESIAN_POINT('Ctrl Pts',(4.40159324575602,0.636309800095218,6.49951119778951));
#53011=CARTESIAN_POINT('Ctrl Pts',(4.45906063875119,0.794772684000854,6.48106534498985));
#53012=CARTESIAN_POINT('Ctrl Pts',(4.56234421467301,1.06847604194529,6.44960463262572));
#53013=CARTESIAN_POINT('Ctrl Pts',(4.6119386373717,1.18514270861212,6.43572580559705));
#53014=CARTESIAN_POINT('Ctrl Pts',(4.66641984978617,1.3000000000005,6.42158632818787));
#53015=CARTESIAN_POINT('Ctrl Pts',(4.672740123946,-1.3000000000001,6.64549193416045));
#53016=CARTESIAN_POINT('Ctrl Pts',(4.61083841229515,-1.18514270861186,6.64225703122094));
#53017=CARTESIAN_POINT('Ctrl Pts',(4.55498406308354,-1.06847604194516,6.63779961664745));
#53018=CARTESIAN_POINT('Ctrl Pts',(4.43991995978582,-0.794772684000864,
6.62467785084282));
#53019=CARTESIAN_POINT('Ctrl Pts',(4.37902881615403,-0.636309800095206,
6.6140804027378));
#53020=CARTESIAN_POINT('Ctrl Pts',(4.30343931027374,-0.319434907277164,
6.59329323836205));
#53021=CARTESIAN_POINT('Ctrl Pts',(4.27661637159808,-0.158333333333334,
6.58169995518562));
#53022=CARTESIAN_POINT('Ctrl Pts',(4.27331855534109,0.158333333333336,6.558253636353));
#53023=CARTESIAN_POINT('Ctrl Pts',(4.29694261300081,0.31943490727717,6.54718967402276));
#53024=CARTESIAN_POINT('Ctrl Pts',(4.36561318065384,0.636309800095214,6.51861108957765));
#53025=CARTESIAN_POINT('Ctrl Pts',(4.42276020605754,0.794772684000853,6.50239596111591));
#53026=CARTESIAN_POINT('Ctrl Pts',(4.53144245410637,1.06847604194529,6.46968503431283));
#53027=CARTESIAN_POINT('Ctrl Pts',(4.58453968076316,1.18514270861212,6.45429464940842));
#53028=CARTESIAN_POINT('Ctrl Pts',(4.64368961597056,1.3000000000005,6.43767322775339));
#53029=CARTESIAN_POINT('Ctrl Pts',(4.64616298310555,-1.30000000000009,6.65922290148753));
#53030=CARTESIAN_POINT('Ctrl Pts',(4.57884821129795,-1.18514270861185,6.65787295346516));
#53031=CARTESIAN_POINT('Ctrl Pts',(4.51897037773764,-1.06847604194515,6.65451742945261));
#53032=CARTESIAN_POINT('Ctrl Pts',(4.39782141879937,-0.794772684000858,
6.64213221596193));
#53033=CARTESIAN_POINT('Ctrl Pts',(4.33736029833944,-0.636309800095203,
6.62862782895121));
#53034=CARTESIAN_POINT('Ctrl Pts',(4.26142549421988,-0.319434907277163,
6.60727042170557));
#53035=CARTESIAN_POINT('Ctrl Pts',(4.23663037107786,-0.158333333333334,
6.59630683043));
#53036=CARTESIAN_POINT('Ctrl Pts',(4.23356409439211,0.158333333333336,6.57403153571279));
#53037=CARTESIAN_POINT('Ctrl Pts',(4.25543929850625,0.319434907277169,6.56394883342396));
#53038=CARTESIAN_POINT('Ctrl Pts',(4.32483019778521,0.636309800095212,6.53742968234783));
#53039=CARTESIAN_POINT('Ctrl Pts',(4.38179799022299,0.794772684000848,6.52455367094891));
#53040=CARTESIAN_POINT('Ctrl Pts',(4.49652643255578,1.06847604194529,6.49051542299507));
#53041=CARTESIAN_POINT('Ctrl Pts',(4.55353612285477,1.18514270861211,6.4734061804994));
#53042=CARTESIAN_POINT('Ctrl Pts',(4.61789381187462,1.3000000000005,6.4539215918059));
#53043=CARTESIAN_POINT('Ctrl Pts',(4.61959384082983,-1.30000000000009,6.67287273622477));
#53044=CARTESIAN_POINT('Ctrl Pts',(4.54688106239739,-1.18514270861185,6.67316414663884));
#53045=CARTESIAN_POINT('Ctrl Pts',(4.48298529463437,-1.06847604194515,6.67068658498385));
#53046=CARTESIAN_POINT('Ctrl Pts',(4.35574234728053,-0.794772684000856,
6.65856604251577));
#53047=CARTESIAN_POINT('Ctrl Pts',(4.29577879950244,-0.636309800095202,
6.64235039988357));
#53048=CARTESIAN_POINT('Ctrl Pts',(4.21924951501912,-0.319434907277163,
6.61918589916601));
#53049=CARTESIAN_POINT('Ctrl Pts',(4.19599251313008,-0.158333333333334,
6.60669429060777));
#53050=CARTESIAN_POINT('Ctrl Pts',(4.19305991900079,0.158333333333336,6.58526803818489));
#53051=CARTESIAN_POINT('Ctrl Pts',(4.21356435840231,0.319434907277169,6.57792549211187));
#53052=CARTESIAN_POINT('Ctrl Pts',(4.28375344830649,0.636309800095211,6.55420327081868));
#53053=CARTESIAN_POINT('Ctrl Pts',(4.34026573204614,0.79477268400085,6.54394750424994));
#53054=CARTESIAN_POINT('Ctrl Pts',(4.4611881714325,1.06847604194528,6.50951686686024));
#53055=CARTESIAN_POINT('Ctrl Pts',(4.52225280844087,1.18514270861211,6.49136607426142));
#53056=CARTESIAN_POINT('Ctrl Pts',(4.59203923906518,1.30000000000049,6.46996823620894));
#53057=CARTESIAN_POINT('Ctrl Pts',(4.60066248946871,-1.30000000000009,6.68136532610089));
#53058=CARTESIAN_POINT('Ctrl Pts',(4.52402803840086,-1.18514270861185,6.6828157790179));
#53059=CARTESIAN_POINT('Ctrl Pts',(4.45719926929767,-1.06847604194515,6.6808807938454));
#53060=CARTESIAN_POINT('Ctrl Pts',(4.32546453057817,-0.794772684000855,
6.66858955176316));
#53061=CARTESIAN_POINT('Ctrl Pts',(4.26556250120118,-0.636309800095201,
6.64892274713424));
#53062=CARTESIAN_POINT('Ctrl Pts',(4.18890570850718,-0.319434907277161,
6.62592093780954));
#53063=CARTESIAN_POINT('Ctrl Pts',(4.16761019334189,-0.158333333333333,
6.61643242376773));
#53064=CARTESIAN_POINT('Ctrl Pts',(4.16488682183599,0.158333333333335,6.59622710193004));
#53065=CARTESIAN_POINT('Ctrl Pts',(4.18371953328468,0.319434907277168,6.58773074716968));
#53066=CARTESIAN_POINT('Ctrl Pts',(4.25429825648514,0.636309800095209,6.56505286778703));
#53067=CARTESIAN_POINT('Ctrl Pts',(4.31073095914166,0.794772684000847,6.55762692818754));
#53068=CARTESIAN_POINT('Ctrl Pts',(4.43618954910262,1.06847604194528,6.52305558630728));
#53069=CARTESIAN_POINT('Ctrl Pts',(4.50019375550391,1.18514270861211,6.50416016967104));
#53070=CARTESIAN_POINT('Ctrl Pts',(4.5738957934113,1.30000000000049,6.48133398930408));
#53071=CARTESIAN_POINT('Ctrl Pts',(4.58731275561848,-1.30000000000009,6.68772391623227));
#53072=CARTESIAN_POINT('Ctrl Pts',(4.50789187753129,-1.18514270861184,6.68910077756878));
#53073=CARTESIAN_POINT('Ctrl Pts',(4.43907033323774,-1.06847604194515,6.68729338620038));
#53074=CARTESIAN_POINT('Ctrl Pts',(4.3045653796696,-0.794772684000855,6.67576168981605));
#53075=CARTESIAN_POINT('Ctrl Pts',(4.2455327159996,-0.636309800095199,6.6575524797122));
#53076=CARTESIAN_POINT('Ctrl Pts',(4.16902454304607,-0.319434907277159,
6.63541503524111));
#53077=CARTESIAN_POINT('Ctrl Pts',(4.14873681505423,-0.158333333333333,
6.62612005228647));
#53078=CARTESIAN_POINT('Ctrl Pts',(4.14587644666081,0.158333333333335,6.60534948552149));
#53079=CARTESIAN_POINT('Ctrl Pts',(4.16337892247362,0.319434907277168,6.59525003245809));
#53080=CARTESIAN_POINT('Ctrl Pts',(4.23390772464296,0.636309800095208,6.57227624871251));
#53081=CARTESIAN_POINT('Ctrl Pts',(4.2901072464585,0.794772684000843,6.56648684843127));
#53082=CARTESIAN_POINT('Ctrl Pts',(4.41844626576087,1.06847604194528,6.53152294131612));
#53083=CARTESIAN_POINT('Ctrl Pts',(4.48438193971655,1.1851427086121,6.51208260176214));
#53084=CARTESIAN_POINT('Ctrl Pts',(4.56070008160123,1.30000000000048,6.4883365025039));
#53085=CARTESIAN_POINT('Ctrl Pts',(4.5709651981178,-1.30000000000009,6.69448853267874));
#53086=CARTESIAN_POINT('Ctrl Pts',(4.48783488180397,-1.18514270861184,6.69584068605108));
#53087=CARTESIAN_POINT('Ctrl Pts',(4.41637026894378,-1.06847604194515,6.6944294937794));
#53088=CARTESIAN_POINT('Ctrl Pts',(4.27822282548381,-0.794772684000853,
6.68478547608066));
#53089=CARTESIAN_POINT('Ctrl Pts',(4.22041348676743,-0.636309800095197,
6.66979426696317));
#53090=CARTESIAN_POINT('Ctrl Pts',(4.14417396510687,-0.319434907277159,
6.64979950085998));
#53091=CARTESIAN_POINT('Ctrl Pts',(4.12518931827153,-0.158333333333332,
6.64060101194686));
#53092=CARTESIAN_POINT('Ctrl Pts',(4.12232618138738,0.158333333333335,6.61992583140733));
#53093=CARTESIAN_POINT('Ctrl Pts',(4.13843207228677,0.319434907277167,6.60948413798752));
#53094=CARTESIAN_POINT('Ctrl Pts',(4.20887140515095,0.636309800095207,6.58525683316955));
#53095=CARTESIAN_POINT('Ctrl Pts',(4.26426538681998,0.794772684000841,6.57813941511196));
#53096=CARTESIAN_POINT('Ctrl Pts',(4.39634797677891,1.06847604194528,6.54149178548603));
#53097=CARTESIAN_POINT('Ctrl Pts',(4.46489389934355,1.1851427086121,6.52133356456642));
#53098=CARTESIAN_POINT('Ctrl Pts',(4.54481208542189,1.30000000000048,6.49688052366376));
#53099=CARTESIAN_POINT('Ctrl Pts',(4.55986191625149,-1.30000000000008,6.69922697939143));
#53100=CARTESIAN_POINT('Ctrl Pts',(4.4739076611286,-1.18514270861184,6.69922519060322));
#53101=CARTESIAN_POINT('Ctrl Pts',(4.40061540553236,-1.06847604194514,6.69755530380812));
#53102=CARTESIAN_POINT('Ctrl Pts',(4.26054738497045,-0.794772684000851,
6.68984389115396));
#53103=CARTESIAN_POINT('Ctrl Pts',(4.20510952843759,-0.636309800095196,
6.6810122975644));
#53104=CARTESIAN_POINT('Ctrl Pts',(4.13001103025471,-0.319434907277159,
6.66430370364935));
#53105=CARTESIAN_POINT('Ctrl Pts',(4.11199983529727,-0.158333333333332,
6.65462349396618));
#53106=CARTESIAN_POINT('Ctrl Pts',(4.1092062507607,0.158333333333334,6.63409216511655));
#53107=CARTESIAN_POINT('Ctrl Pts',(4.12443963758816,0.319434907277167,6.62411656351297));
#53108=CARTESIAN_POINT('Ctrl Pts',(4.19381566981051,0.636309800095206,6.59722095262982));
#53109=CARTESIAN_POINT('Ctrl Pts',(4.24681642623153,0.79477268400084,6.58511749178966));
#53110=CARTESIAN_POINT('Ctrl Pts',(4.38081889489758,1.06847604194527,6.54648422762646));
#53111=CARTESIAN_POINT('Ctrl Pts',(4.45118854322608,1.1851427086121,6.52626110695219));
#53112=CARTESIAN_POINT('Ctrl Pts',(4.53392313647836,1.30000000000048,6.50253777415639));
#53113=CARTESIAN_POINT('Ctrl Pts',(4.55333646119707,-1.30000000000008,6.70483180220308));
#53114=CARTESIAN_POINT('Ctrl Pts',(4.46759044005478,-1.18514270861184,6.70468931916621));
#53115=CARTESIAN_POINT('Ctrl Pts',(4.39457954353637,-1.06847604194514,6.70321883895621));
#53116=CARTESIAN_POINT('Ctrl Pts',(4.25533045233314,-0.794772684000851,
6.69675379636771));
#53117=CARTESIAN_POINT('Ctrl Pts',(4.20084799529369,-0.636309800095196,
6.6903034367033));
#53118=CARTESIAN_POINT('Ctrl Pts',(4.1264371815048,-0.319434907277159,6.675134858055));
#53119=CARTESIAN_POINT('Ctrl Pts',(4.1083738762426,-0.158333333333332,6.66544968261944));
#53120=CARTESIAN_POINT('Ctrl Pts',(4.10569625638312,0.158333333333334,6.6451248466368));
#53121=CARTESIAN_POINT('Ctrl Pts',(4.12120905306814,0.319434907277167,6.63561768729212));
#53122=CARTESIAN_POINT('Ctrl Pts',(4.18990683146856,0.636309800095206,6.607079215074));
#53123=CARTESIAN_POINT('Ctrl Pts',(4.24157890048061,0.79477268400084,6.59157705531633));
#53124=CARTESIAN_POINT('Ctrl Pts',(4.37480433638251,1.06847604194527,6.55184520336775));
#53125=CARTESIAN_POINT('Ctrl Pts',(4.44499154163423,1.1851427086121,6.53172693228782));
#53126=CARTESIAN_POINT('Ctrl Pts',(4.52769759742463,1.30000000000048,6.50868883662629));
#53127=CARTESIAN_POINT('Ctrl Pts',(4.55333646119701,-1.3,6.70483180220308));
#53128=CARTESIAN_POINT('Ctrl Pts',(4.46759044005475,-1.18514270861178,6.70468931916621));
#53129=CARTESIAN_POINT('Ctrl Pts',(4.39457954353636,-1.06847604194512,6.70321883895621));
#53130=CARTESIAN_POINT('Ctrl Pts',(4.25533045233314,-0.794772684000851,
6.69675379636771));
#53131=CARTESIAN_POINT('Ctrl Pts',(4.20084799529369,-0.636309800095197,
6.6903034367033));
#53132=CARTESIAN_POINT('Ctrl Pts',(4.1264371815048,-0.319434907277159,6.675134858055));
#53133=CARTESIAN_POINT('Ctrl Pts',(4.1083738762426,-0.158333333333332,6.66544968261944));
#53134=CARTESIAN_POINT('Ctrl Pts',(4.10569625638312,0.158333333333334,6.6451248466368));
#53135=CARTESIAN_POINT('Ctrl Pts',(4.12120905306815,0.319434907277167,6.63561768729212));
#53136=CARTESIAN_POINT('Ctrl Pts',(4.18990683146856,0.636309800095206,6.607079215074));
#53137=CARTESIAN_POINT('Ctrl Pts',(4.24157890048061,0.79477268400084,6.59157705531633));
#53138=CARTESIAN_POINT('Ctrl Pts',(4.37480433638243,1.06847604194511,6.55184520336778));
#53139=CARTESIAN_POINT('Ctrl Pts',(4.44499154163404,1.18514270861178,6.53172693228788));
#53140=CARTESIAN_POINT('Ctrl Pts',(4.52769759742429,1.3,6.50868883662639));
#53141=CARTESIAN_POINT('',(4.89593598449868,-1.2,6.47040364879548));
#53142=CARTESIAN_POINT('Ctrl Pts',(4.89593598449868,-1.2,6.47040364879548));
#53143=CARTESIAN_POINT('Ctrl Pts',(4.88552007488463,-1.21198332754869,6.48180974294822));
#53144=CARTESIAN_POINT('Ctrl Pts',(4.86715275551669,-1.23320804299601,6.5029687954801));
#53145=CARTESIAN_POINT('Ctrl Pts',(4.83662477530882,-1.26800122851154,6.53578088853726));
#53146=CARTESIAN_POINT('Ctrl Pts',(4.8232775251527,-1.28318627910763,6.55035026134636));
#53147=CARTESIAN_POINT('Ctrl Pts',(4.80833879006001,-1.29999999996669,6.56566721641765));
#53148=CARTESIAN_POINT('',(4.87041241528844,-0.653834841370086,6.31592822427069));
#53149=CARTESIAN_POINT('Ctrl Pts',(4.87041241532541,-0.653834841368829,
6.31592822426901));
#53150=CARTESIAN_POINT('Ctrl Pts',(4.87328845860714,-0.717304357747199,
6.33177254516113));
#53151=CARTESIAN_POINT('Ctrl Pts',(4.87561663331839,-0.764718184626917,
6.34493691099469));
#53152=CARTESIAN_POINT('Ctrl Pts',(4.88435675347613,-0.949625201953965,
6.39576546853942));
#53153=CARTESIAN_POINT('Ctrl Pts',(4.88944388081821,-1.05881455110567,6.42683856795065));
#53154=CARTESIAN_POINT('Ctrl Pts',(4.89593598449868,-1.2,6.47040364879548));
#53155=CARTESIAN_POINT('',(4.84356468978495,0.653834841531101,6.17902933643107));
#53156=CARTESIAN_POINT('Ctrl Pts',(4.84356468978495,0.653834841531099,6.17902933643107));
#53157=CARTESIAN_POINT('Ctrl Pts',(4.81027480171635,0.575967894595913,6.20394293927447));
#53158=CARTESIAN_POINT('Ctrl Pts',(4.78258938258321,0.493633270675005,6.22560831669507));
#53159=CARTESIAN_POINT('Ctrl Pts',(4.74428430246563,0.338128732286169,6.25868470950295));
#53160=CARTESIAN_POINT('Ctrl Pts',(4.73158136615163,0.265653446049887,6.27127805152257));
#53161=CARTESIAN_POINT('Ctrl Pts',(4.71755921729924,0.129712949542664,6.2912135864992));
#53162=CARTESIAN_POINT('Ctrl Pts',(4.71484070144113,0.0666229865808594,
6.29903019023757));
#53163=CARTESIAN_POINT('Ctrl Pts',(4.71704007282426,-0.0595430897305052,
6.31217543572927));
#53164=CARTESIAN_POINT('Ctrl Pts',(4.72195733819667,-0.122775140765603,
6.31760388022771));
#53165=CARTESIAN_POINT('Ctrl Pts',(4.74092964991683,-0.260125061892429,
6.32597746664295));
#53166=CARTESIAN_POINT('Ctrl Pts',(4.75649191430833,-0.333942206836294,
6.32829157281983));
#53167=CARTESIAN_POINT('Ctrl Pts',(4.80133465609412,-0.491210015044957,
6.32745084093312));
#53168=CARTESIAN_POINT('Ctrl Pts',(4.83265724001896,-0.574353127738433,
6.32346804471193));
#53169=CARTESIAN_POINT('Ctrl Pts',(4.87041241526413,-0.653834841386618,
6.31592822432322));
#53170=CARTESIAN_POINT('',(4.85795990615321,1.2,6.24988129678031));
#53171=CARTESIAN_POINT('Ctrl Pts',(4.85795990615321,1.2,6.24988129678031));
#53172=CARTESIAN_POINT('Ctrl Pts',(4.85544249344361,1.13014930724506,6.23700975770938));
#53173=CARTESIAN_POINT('Ctrl Pts',(4.85277540338472,1.05323054854764,6.22352942609793));
#53174=CARTESIAN_POINT('Ctrl Pts',(4.84602121616902,0.796444496061531,6.19067038861466));
#53175=CARTESIAN_POINT('Ctrl Pts',(4.84489099862009,0.73982206670996,6.18532144929078));
#53176=CARTESIAN_POINT('Ctrl Pts',(4.84356468978495,0.653834841531101,6.17902933643107));
#53177=CARTESIAN_POINT('Ctrl Pts',(4.77352764767187,1.30000000000002,6.34213416147271));
#53178=CARTESIAN_POINT('Ctrl Pts',(4.78797295912602,1.28314836924958,6.32724218773947));
#53179=CARTESIAN_POINT('Ctrl Pts',(4.80202291543942,1.26652615695483,6.31171709974393));
#53180=CARTESIAN_POINT('Ctrl Pts',(4.83031567071051,1.23309342866822,6.28121078500142));
#53181=CARTESIAN_POINT('Ctrl Pts',(4.8447116454302,1.21600083823975,6.26550527072992));
#53182=CARTESIAN_POINT('Ctrl Pts',(4.85795990615321,1.2,6.24988129678031));
#53183=CARTESIAN_POINT('Ctrl Pts',(4.55333646119701,-1.3,6.70483180220308));
#53184=CARTESIAN_POINT('Ctrl Pts',(4.46759044005475,-1.18514270861178,6.70468931916621));
#53185=CARTESIAN_POINT('Ctrl Pts',(4.39457954353636,-1.06847604194512,6.70321883895621));
#53186=CARTESIAN_POINT('Ctrl Pts',(4.25533045233313,-0.794772684000851,
6.69675379636771));
#53187=CARTESIAN_POINT('Ctrl Pts',(4.20084799529369,-0.636309800095197,
6.6903034367033));
#53188=CARTESIAN_POINT('Ctrl Pts',(4.1264371815048,-0.319434907277159,6.675134858055));
#53189=CARTESIAN_POINT('Ctrl Pts',(4.1083738762426,-0.158333333333332,6.66544968261944));
#53190=CARTESIAN_POINT('Ctrl Pts',(4.10569625638312,0.158333333333334,6.6451248466368));
#53191=CARTESIAN_POINT('Ctrl Pts',(4.12120905306814,0.319434907277167,6.63561768729212));
#53192=CARTESIAN_POINT('Ctrl Pts',(4.18990683146856,0.636309800095206,6.607079215074));
#53193=CARTESIAN_POINT('Ctrl Pts',(4.24157890048061,0.79477268400084,6.59157705531633));
#53194=CARTESIAN_POINT('Ctrl Pts',(4.37480433638243,1.06847604194511,6.55184520336778));
#53195=CARTESIAN_POINT('Ctrl Pts',(4.44499154163404,1.18514270861178,6.53172693228788));
#53196=CARTESIAN_POINT('Ctrl Pts',(4.52769759742429,1.3,6.50868883662639));
#53197=CARTESIAN_POINT('Ctrl Pts',(4.559720379007,-1.3,6.78150223240952));
#53198=CARTESIAN_POINT('Ctrl Pts',(4.47399349175896,-1.18514270861178,6.77962754301943));
#53199=CARTESIAN_POINT('Ctrl Pts',(4.40104080402149,-1.06847604194512,6.77695192352273));
#53200=CARTESIAN_POINT('Ctrl Pts',(4.26201645755201,-0.794772684000851,
6.76892039845776));
#53201=CARTESIAN_POINT('Ctrl Pts',(4.20777282266716,-0.636309800095197,
6.76314676763589));
#53202=CARTESIAN_POINT('Ctrl Pts',(4.13378893043112,-0.319434907277159,
6.74849045958165));
#53203=CARTESIAN_POINT('Ctrl Pts',(4.11602990877888,-0.158333333333332,
6.74000897151971));
#53204=CARTESIAN_POINT('Ctrl Pts',(4.11370927434805,0.158333333333334,6.71964661485659));
#53205=CARTESIAN_POINT('Ctrl Pts',(4.12926944463902,0.319434907277167,6.70889880747554));
#53206=CARTESIAN_POINT('Ctrl Pts',(4.19827830828669,0.636309800095206,6.67977049702301));
#53207=CARTESIAN_POINT('Ctrl Pts',(4.25004328077839,0.79477268400084,6.6635567426537));
#53208=CARTESIAN_POINT('Ctrl Pts',(4.38381424022261,1.06847604194511,6.62531041472351));
#53209=CARTESIAN_POINT('Ctrl Pts',(4.45430894480039,1.18514270861178,6.60635884545937));
#53210=CARTESIAN_POINT('Ctrl Pts',(4.53739386231511,1.3,6.58501112512597));
#53211=CARTESIAN_POINT('Ctrl Pts',(4.56610429681699,-1.3,6.85817266261596));
#53212=CARTESIAN_POINT('Ctrl Pts',(4.48039654346318,-1.18514270861178,6.85456576687265));
#53213=CARTESIAN_POINT('Ctrl Pts',(4.40750206450663,-1.06847604194512,6.85068500808926));
#53214=CARTESIAN_POINT('Ctrl Pts',(4.26870246277088,-0.794772684000851,
6.84108700054782));
#53215=CARTESIAN_POINT('Ctrl Pts',(4.21469765004064,-0.636309800095197,
6.83599009856847));
#53216=CARTESIAN_POINT('Ctrl Pts',(4.14114067935745,-0.319434907277159,
6.8218460611083));
#53217=CARTESIAN_POINT('Ctrl Pts',(4.12368594131515,-0.158333333333332,
6.81456826041999));
#53218=CARTESIAN_POINT('Ctrl Pts',(4.12172229231298,0.158333333333334,6.79416838307638));
#53219=CARTESIAN_POINT('Ctrl Pts',(4.1373298362099,0.319434907277167,6.78217992765896));
#53220=CARTESIAN_POINT('Ctrl Pts',(4.20664978510482,0.636309800095206,6.75246177897202));
#53221=CARTESIAN_POINT('Ctrl Pts',(4.25850766107617,0.79477268400084,6.73553642999107));
#53222=CARTESIAN_POINT('Ctrl Pts',(4.39282414406279,1.06847604194511,6.69877562607923));
#53223=CARTESIAN_POINT('Ctrl Pts',(4.46362634796674,1.18514270861178,6.68099075863087));
#53224=CARTESIAN_POINT('Ctrl Pts',(4.54709012720593,1.3,6.66133341362554));
#53225=CARTESIAN_POINT('Ctrl Pts',(4.57248821462698,-1.3,6.9348430928224));
#53226=CARTESIAN_POINT('Ctrl Pts',(4.48679959516739,-1.18514270861178,6.92950399072586));
#53227=CARTESIAN_POINT('Ctrl Pts',(4.41396332499177,-1.06847604194512,6.92441809265578));
#53228=CARTESIAN_POINT('Ctrl Pts',(4.27538846798975,-0.794772684000851,
6.91325360263787));
#53229=CARTESIAN_POINT('Ctrl Pts',(4.22162247741411,-0.636309800095197,
6.90883342950106));
#53230=CARTESIAN_POINT('Ctrl Pts',(4.14849242828377,-0.319434907277159,
6.89520166263496));
#53231=CARTESIAN_POINT('Ctrl Pts',(4.13134197385142,-0.158333333333332,
6.88912754932026));
#53232=CARTESIAN_POINT('Ctrl Pts',(4.12973531027791,0.158333333333334,6.86869015129617));
#53233=CARTESIAN_POINT('Ctrl Pts',(4.14539022778078,0.319434907277167,6.85546104784238));
#53234=CARTESIAN_POINT('Ctrl Pts',(4.21502126192296,0.636309800095206,6.82515306092103));
#53235=CARTESIAN_POINT('Ctrl Pts',(4.26697204137396,0.79477268400084,6.80751611732844));
#53236=CARTESIAN_POINT('Ctrl Pts',(4.40183404790297,1.06847604194511,6.77224083743496));
#53237=CARTESIAN_POINT('Ctrl Pts',(4.47294375113309,1.18514270861178,6.75562267180236));
#53238=CARTESIAN_POINT('Ctrl Pts',(4.55678639209675,1.3,6.73765570212511));
#53239=CARTESIAN_POINT('Ctrl Pts',(4.57248821462698,-1.3,6.9348430928224));
#53240=CARTESIAN_POINT('Ctrl Pts',(4.48679959516739,-1.18514270861178,6.92950399072586));
#53241=CARTESIAN_POINT('Ctrl Pts',(4.41396332499177,-1.06847604194512,6.92441809265578));
#53242=CARTESIAN_POINT('Ctrl Pts',(4.27538846798975,-0.794772684000851,
6.91325360263787));
#53243=CARTESIAN_POINT('Ctrl Pts',(4.22162247741411,-0.636309800095197,
6.90883342950106));
#53244=CARTESIAN_POINT('Ctrl Pts',(4.14849242828377,-0.319434907277159,
6.89520166263496));
#53245=CARTESIAN_POINT('Ctrl Pts',(4.13134197385143,-0.158333333333332,
6.88912754932026));
#53246=CARTESIAN_POINT('Ctrl Pts',(4.12973531027791,0.158333333333334,6.86869015129617));
#53247=CARTESIAN_POINT('Ctrl Pts',(4.14539022778078,0.319434907277167,6.85546104784238));
#53248=CARTESIAN_POINT('Ctrl Pts',(4.21502126192295,0.636309800095206,6.82515306092103));
#53249=CARTESIAN_POINT('Ctrl Pts',(4.26697204137395,0.79477268400084,6.80751611732844));
#53250=CARTESIAN_POINT('Ctrl Pts',(4.40183404790297,1.06847604194511,6.77224083743496));
#53251=CARTESIAN_POINT('Ctrl Pts',(4.47294375113309,1.18514270861178,6.75562267180236));
#53252=CARTESIAN_POINT('Ctrl Pts',(4.55678639209675,1.3,6.73765570212511));
#53253=CARTESIAN_POINT('Ctrl Pts',(4.57248821462698,-1.3,6.9348430928224));
#53254=CARTESIAN_POINT('Ctrl Pts',(4.48679959516739,-1.18514270861178,6.92950399072586));
#53255=CARTESIAN_POINT('Ctrl Pts',(4.41396332499177,-1.06847604194512,6.92441809265578));
#53256=CARTESIAN_POINT('Ctrl Pts',(4.27538846798975,-0.794772684000851,
6.91325360263787));
#53257=CARTESIAN_POINT('Ctrl Pts',(4.22162247741411,-0.636309800095197,
6.90883342950106));
#53258=CARTESIAN_POINT('Ctrl Pts',(4.14849242828377,-0.319434907277159,
6.89520166263495));
#53259=CARTESIAN_POINT('Ctrl Pts',(4.13134197385142,-0.158333333333332,
6.88912754932025));
#53260=CARTESIAN_POINT('Ctrl Pts',(4.12973531027791,0.158333333333334,6.86869015129617));
#53261=CARTESIAN_POINT('Ctrl Pts',(4.14539022778078,0.319434907277167,6.85546104784237));
#53262=CARTESIAN_POINT('Ctrl Pts',(4.21502126192295,0.636309800095206,6.82515306092102));
#53263=CARTESIAN_POINT('Ctrl Pts',(4.26697204137396,0.79477268400084,6.80751611732844));
#53264=CARTESIAN_POINT('Ctrl Pts',(4.40183404790374,1.06847604194666,6.77224083743476));
#53265=CARTESIAN_POINT('Ctrl Pts',(4.47294375113495,1.18514270861482,6.75562267180193));
#53266=CARTESIAN_POINT('Ctrl Pts',(4.55678639210004,1.3000000000045,6.73765570212441));
#53267=CARTESIAN_POINT('Ctrl Pts',(4.57985658845472,-1.3,6.93956537747332));
#53268=CARTESIAN_POINT('Ctrl Pts',(4.4939975863417,-1.18514270861178,6.93356194558967));
#53269=CARTESIAN_POINT('Ctrl Pts',(4.42096106045723,-1.06847604194512,6.92841142118886));
#53270=CARTESIAN_POINT('Ctrl Pts',(4.28185455997266,-0.794772684000851,
6.91848306637304));
#53271=CARTESIAN_POINT('Ctrl Pts',(4.22749554624361,-0.636309800095197,
6.91766357207286));
#53272=CARTESIAN_POINT('Ctrl Pts',(4.1540436348186,-0.319434907277159,6.90577978298097));
#53273=CARTESIAN_POINT('Ctrl Pts',(4.13706908978531,-0.158333333333332,
6.89918937142415));
#53274=CARTESIAN_POINT('Ctrl Pts',(4.13553292450502,0.158333333333334,6.87852588248496));
#53275=CARTESIAN_POINT('Ctrl Pts',(4.1511379029416,0.319434907277167,6.86531247060522));
#53276=CARTESIAN_POINT('Ctrl Pts',(4.22112140677529,0.636309800095206,6.83335514381765));
#53277=CARTESIAN_POINT('Ctrl Pts',(4.27351162156741,0.79477268400084,6.81319036325118));
#53278=CARTESIAN_POINT('Ctrl Pts',(4.40891552697402,1.06847604194666,6.77652568448102));
#53279=CARTESIAN_POINT('Ctrl Pts',(4.48025898194898,1.18514270861482,6.75965397193426));
#53280=CARTESIAN_POINT('Ctrl Pts',(4.56433455845715,1.3000000000045,6.74178132772021));
#53281=CARTESIAN_POINT('Ctrl Pts',(4.59168572246724,-1.30000000000002,6.94280967669042));
#53282=CARTESIAN_POINT('Ctrl Pts',(4.50842963072979,-1.1851427086118,6.93550875066837));
#53283=CARTESIAN_POINT('Ctrl Pts',(4.437190204196,-1.06847604194513,6.93004561131568));
#53284=CARTESIAN_POINT('Ctrl Pts',(4.30037377805058,-0.794772684000862,
6.92167032136784));
#53285=CARTESIAN_POINT('Ctrl Pts',(4.24470982715029,-0.636309800095207,
6.92623862411642));
#53286=CARTESIAN_POINT('Ctrl Pts',(4.17077209362945,-0.319434907277164,
6.91719495861301));
#53287=CARTESIAN_POINT('Ctrl Pts',(4.15284748798856,-0.158333333333335,
6.91033447894196));
#53288=CARTESIAN_POINT('Ctrl Pts',(4.15134880332261,0.158333333333337,6.88950691599258));
#53289=CARTESIAN_POINT('Ctrl Pts',(4.16800480359992,0.319434907277172,6.87653626951492));
#53290=CARTESIAN_POINT('Ctrl Pts',(4.2384211693924,0.636309800095216,6.84112601890762));
#53291=CARTESIAN_POINT('Ctrl Pts',(4.29185181052877,0.794772684000852,6.8144698216443));
#53292=CARTESIAN_POINT('Ctrl Pts',(4.42497591024534,1.06847604194667,6.77632001966336));
#53293=CARTESIAN_POINT('Ctrl Pts',(4.49458557019052,1.18514270861484,6.76008017149172));
#53294=CARTESIAN_POINT('Ctrl Pts',(4.5761804000472,1.30000000000452,6.74411411083662));
#53295=CARTESIAN_POINT('Ctrl Pts',(4.60901351621805,-1.30000000000003,6.94776612680297));
#53296=CARTESIAN_POINT('Ctrl Pts',(4.52942942664903,-1.18514270861181,6.94042190776583));
#53297=CARTESIAN_POINT('Ctrl Pts',(4.46089500922349,-1.06847604194514,6.93513362968046));
#53298=CARTESIAN_POINT('Ctrl Pts',(4.32809374783802,-0.794772684000868,
6.92766628427501));
#53299=CARTESIAN_POINT('Ctrl Pts',(4.27191634453898,-0.636309800095211,
6.93373309324915));
#53300=CARTESIAN_POINT('Ctrl Pts',(4.1981511998046,-0.319434907277166,6.92597574477209));
#53301=CARTESIAN_POINT('Ctrl Pts',(4.1789303220762,-0.158333333333336,6.9197783105525));
#53302=CARTESIAN_POINT('Ctrl Pts',(4.17740932610982,0.158333333333338,6.8988415262861));
#53303=CARTESIAN_POINT('Ctrl Pts',(4.19532242039286,0.319434907277174,6.88542037767051));
#53304=CARTESIAN_POINT('Ctrl Pts',(4.26555510730558,0.63630980009522,6.84784592269368));
#53305=CARTESIAN_POINT('Ctrl Pts',(4.31951206683825,0.794772684000859,6.8178513996686));
#53306=CARTESIAN_POINT('Ctrl Pts',(4.44867433870729,1.06847604194668,6.77863163545275));
#53307=CARTESIAN_POINT('Ctrl Pts',(4.51561242266566,1.18514270861485,6.76255514417353));
#53308=CARTESIAN_POINT('Ctrl Pts',(4.59357902902374,1.30000000000453,6.74737894430877));
#53309=CARTESIAN_POINT('Ctrl Pts',(4.6233534298674,-1.30000000000005,6.95207556239594));
#53310=CARTESIAN_POINT('Ctrl Pts',(4.54651014232481,-1.18514270861182,6.94505581919046));
#53311=CARTESIAN_POINT('Ctrl Pts',(4.4799715641937,-1.06847604194515,6.93986541852847));
#53312=CARTESIAN_POINT('Ctrl Pts',(4.35006007790447,-0.794772684000877,
6.93210070189737));
#53313=CARTESIAN_POINT('Ctrl Pts',(4.29331731838996,-0.636309800095217,
6.9365561992288));
#53314=CARTESIAN_POINT('Ctrl Pts',(4.21956531577933,-0.319434907277168,
6.92900915459488));
#53315=CARTESIAN_POINT('Ctrl Pts',(4.19938038514094,-0.158333333333338,
6.92456854816355));
#53316=CARTESIAN_POINT('Ctrl Pts',(4.19784131139462,0.158333333333339,6.90424024601326));
#53317=CARTESIAN_POINT('Ctrl Pts',(4.21669151098746,0.319434907277178,6.89059198569614));
#53318=CARTESIAN_POINT('Ctrl Pts',(4.28689229982556,0.636309800095227,6.85217017386736));
#53319=CARTESIAN_POINT('Ctrl Pts',(4.34140188971318,0.794772684000865,6.82045193860963));
#53320=CARTESIAN_POINT('Ctrl Pts',(4.46771360256903,1.06847604194669,6.78102673047936));
#53321=CARTESIAN_POINT('Ctrl Pts',(4.53268578500315,1.18514270861486,6.76523453140521));
#53322=CARTESIAN_POINT('Ctrl Pts',(4.60795448968593,1.30000000000454,6.75071584500868));
#53323=CARTESIAN_POINT('Ctrl Pts',(4.64065212265408,-1.30000000000006,6.95781610440239));
#53324=CARTESIAN_POINT('Ctrl Pts',(4.56736875666192,-1.18514270861184,6.95137736045384));
#53325=CARTESIAN_POINT('Ctrl Pts',(4.50344330243136,-1.06847604194516,6.94637658530222));
#53326=CARTESIAN_POINT('Ctrl Pts',(4.37738136312857,-0.794772684000886,
6.93814578988592));
#53327=CARTESIAN_POINT('Ctrl Pts',(4.32005877814057,-0.636309800095224,
6.94041641143475));
#53328=CARTESIAN_POINT('Ctrl Pts',(4.24644502861887,-0.319434907277172,
6.93216354244808));
#53329=CARTESIAN_POINT('Ctrl Pts',(4.22505541355766,-0.158333333333339,
6.92921338110318));
#53330=CARTESIAN_POINT('Ctrl Pts',(4.22347657514697,0.158333333333341,6.90773716913098));
#53331=CARTESIAN_POINT('Ctrl Pts',(4.2434536947023,0.31943490727718,6.89074124728874));
#53332=CARTESIAN_POINT('Ctrl Pts',(4.3135126355416,0.636309800095232,6.85213185666438));
#53333=CARTESIAN_POINT('Ctrl Pts',(4.36867916688973,0.794772684000874,6.82364499201943));
#53334=CARTESIAN_POINT('Ctrl Pts',(4.49121503331224,1.0684760419467,6.78527105908375));
#53335=CARTESIAN_POINT('Ctrl Pts',(4.55360760784926,1.18514270861487,6.76955654046397));
#53336=CARTESIAN_POINT('Ctrl Pts',(4.62535152074995,1.30000000000456,6.75473815689801));
#53337=CARTESIAN_POINT('Ctrl Pts',(4.65772891567358,-1.3000000000001,6.9650122729636));
#53338=CARTESIAN_POINT('Ctrl Pts',(4.58785149243056,-1.18514270861187,6.95886872864369));
#53339=CARTESIAN_POINT('Ctrl Pts',(4.52642377891097,-1.06847604194519,6.95380579361821));
#53340=CARTESIAN_POINT('Ctrl Pts',(4.40403399192852,-0.794772684000904,
6.94460582451793));
#53341=CARTESIAN_POINT('Ctrl Pts',(4.34613524203725,-0.636309800095241,
6.94495603954721));
#53342=CARTESIAN_POINT('Ctrl Pts',(4.27264773874593,-0.319434907277181,
6.93470095333162));
#53343=CARTESIAN_POINT('Ctrl Pts',(4.25011864464721,-0.158333333333343,
6.93042203799672));
#53344=CARTESIAN_POINT('Ctrl Pts',(4.24850364252821,0.158333333333345,6.90847420714758));
#53345=CARTESIAN_POINT('Ctrl Pts',(4.26954211934693,0.319434907277189,6.89234795461961));
#53346=CARTESIAN_POINT('Ctrl Pts',(4.33948661664487,0.63630980009525,6.85475459626415));
#53347=CARTESIAN_POINT('Ctrl Pts',(4.39531220514294,0.794772684000897,6.82742116863333));
#53348=CARTESIAN_POINT('Ctrl Pts',(4.5142895898812,1.06847604194673,6.78952706502359));
#53349=CARTESIAN_POINT('Ctrl Pts',(4.57424140111991,1.18514270861491,6.77380152188313));
#53350=CARTESIAN_POINT('Ctrl Pts',(4.64264412229035,1.30000000000459,6.75875338894005));
#53351=CARTESIAN_POINT('Ctrl Pts',(4.68074462869342,-1.3000000000001,6.97223030803504));
#53352=CARTESIAN_POINT('Ctrl Pts',(4.61546701102458,-1.18514270861187,6.96711220410798));
#53353=CARTESIAN_POINT('Ctrl Pts',(4.55741287000154,-1.0684760419452,6.96255256638903));
#53354=CARTESIAN_POINT('Ctrl Pts',(4.43998386665053,-0.794772684000911,
6.95330905976739));
#53355=CARTESIAN_POINT('Ctrl Pts',(4.38130823543249,-0.636309800095243,
6.95178561930535));
#53356=CARTESIAN_POINT('Ctrl Pts',(4.307995220275,-0.319434907277182,6.93983193085731));
#53357=CARTESIAN_POINT('Ctrl Pts',(4.28392004501045,-0.158333333333344,
6.93449206360987));
#53358=CARTESIAN_POINT('Ctrl Pts',(4.28228212154936,0.158333333333346,6.91164478340126));
#53359=CARTESIAN_POINT('Ctrl Pts',(4.30482303330787,0.319434907277191,6.89508261334793));
#53360=CARTESIAN_POINT('Ctrl Pts',(4.37458856844489,0.636309800095253,6.85857264532631));
#53361=CARTESIAN_POINT('Ctrl Pts',(4.4312245980318,0.794772684000898,6.83394799296566));
#53362=CARTESIAN_POINT('Ctrl Pts',(4.54529186856434,1.06847604194673,6.79691837208924));
#53363=CARTESIAN_POINT('Ctrl Pts',(4.60189712594626,1.18514270861491,6.78112435439916));
#53364=CARTESIAN_POINT('Ctrl Pts',(4.66573214590514,1.3000000000046,6.76556506981383));
#53365=CARTESIAN_POINT('Ctrl Pts',(4.70347027821068,-1.30000000000016,6.9823724522687));
#53366=CARTESIAN_POINT('Ctrl Pts',(4.64271971394712,-1.18514270861193,6.97849915325402));
#53367=CARTESIAN_POINT('Ctrl Pts',(4.58800010266077,-1.06847604194524,6.9744350044508));
#53368=CARTESIAN_POINT('Ctrl Pts',(4.47551956183392,-0.794772684000947,
6.96460510649433));
#53369=CARTESIAN_POINT('Ctrl Pts',(4.41619320511171,-0.636309800095273,
6.95982737803518));
#53370=CARTESIAN_POINT('Ctrl Pts',(4.34312042184911,-0.319434907277197,
6.94537946334079));
#53371=CARTESIAN_POINT('Ctrl Pts',(4.31751409845567,-0.158333333333351,
6.93882991032973));
#53372=CARTESIAN_POINT('Ctrl Pts',(4.31585533458879,0.158333333333353,6.91545225315629));
#53373=CARTESIAN_POINT('Ctrl Pts',(4.33985068426229,0.319434907277205,6.89984296341105));
#53374=CARTESIAN_POINT('Ctrl Pts',(4.40944733987471,0.636309800095282,6.86418963648015));
#53375=CARTESIAN_POINT('Ctrl Pts',(4.4669199632229,0.794772684000936,6.84053040220008));
#53376=CARTESIAN_POINT('Ctrl Pts',(4.57615689899014,1.06847604194678,6.80362722765851));
#53377=CARTESIAN_POINT('Ctrl Pts',(4.62946163274559,1.18514270861497,6.7876436506777));
#53378=CARTESIAN_POINT('Ctrl Pts',(4.68878647838988,1.30000000000466,6.77165051357786));
#53379=CARTESIAN_POINT('Ctrl Pts',(4.73772090176179,-1.30000000000017,6.99560535184883));
#53380=CARTESIAN_POINT('Ctrl Pts',(4.68380518377452,-1.18514270861193,6.99338267515873));
#53381=CARTESIAN_POINT('Ctrl Pts',(4.63410339321969,-1.06847604194525,6.99025797323616));
#53382=CARTESIAN_POINT('Ctrl Pts',(4.52901732959112,-0.794772684000953,
6.98095542796402));
#53383=CARTESIAN_POINT('Ctrl Pts',(4.46854489566491,-0.636309800095279,
6.97453050087433));
#53384=CARTESIAN_POINT('Ctrl Pts',(4.39581782749983,-0.3194349072772,6.95729884977924));
#53385=CARTESIAN_POINT('Ctrl Pts',(4.36803658709379,-0.158333333333352,
6.94725609926108));
#53386=CARTESIAN_POINT('Ctrl Pts',(4.3663924659603,0.158333333333354,6.92263405197941));
#53387=CARTESIAN_POINT('Ctrl Pts',(4.39256517391286,0.319434907277205,6.90860399762272));
#53388=CARTESIAN_POINT('Ctrl Pts',(4.46187079413096,0.636309800095285,6.87456354401537));
#53389=CARTESIAN_POINT('Ctrl Pts',(4.52053080970807,0.794772684000943,6.8533649349418));
#53390=CARTESIAN_POINT('Ctrl Pts',(4.62246797863368,1.0684760419468,6.81620646621921));
#53391=CARTESIAN_POINT('Ctrl Pts',(4.67080332086836,1.18514270861498,6.79941891700058));
#53392=CARTESIAN_POINT('Ctrl Pts',(4.72334918205387,1.30000000000467,6.78192834281648));
#53393=CARTESIAN_POINT('Ctrl Pts',(4.77170045210599,-1.30000000000031,7.01099742213157));
#53394=CARTESIAN_POINT('Ctrl Pts',(4.72457989536022,-1.18514270861206,7.01054672126873));
#53395=CARTESIAN_POINT('Ctrl Pts',(4.67987505604944,-1.06847604194537,7.00838749823058));
#53396=CARTESIAN_POINT('Ctrl Pts',(4.5821787246065,-0.794772684001035,6.99945223304775));
#53397=CARTESIAN_POINT('Ctrl Pts',(4.52064605182507,-0.636309800095346,
6.9902351849925));
#53398=CARTESIAN_POINT('Ctrl Pts',(4.4482758509293,-0.319434907277234,6.97114789687891));
#53399=CARTESIAN_POINT('Ctrl Pts',(4.41826092950754,-0.15833333333337,6.96037904196055));
#53400=CARTESIAN_POINT('Ctrl Pts',(4.41663733815419,0.158333333333371,6.93485712386133));
#53401=CARTESIAN_POINT('Ctrl Pts',(4.44502504936253,0.319434907277241,6.92068169288381));
#53402=CARTESIAN_POINT('Ctrl Pts',(4.51409548293143,0.636309800095355,6.88660607626106));
#53403=CARTESIAN_POINT('Ctrl Pts',(4.57398757726845,0.794772684001026,6.86635219269857));
#53404=CARTESIAN_POINT('Ctrl Pts',(4.66867345823415,1.06847604194691,6.82852799893898));
#53405=CARTESIAN_POINT('Ctrl Pts',(4.71205687341492,1.18514270861511,6.81112568365538));
#53406=CARTESIAN_POINT('Ctrl Pts',(4.7578376943638,1.30000000000481,6.79269374504232));
#53407=CARTESIAN_POINT('Ctrl Pts',(4.80284656862992,-1.3000000000004,7.0246922001963));
#53408=CARTESIAN_POINT('Ctrl Pts',(4.76180440192939,-1.18514270861215,7.02714890150709));
#53409=CARTESIAN_POINT('Ctrl Pts',(4.7215804598047,-1.06847604194545,7.02680909351662));
#53410=CARTESIAN_POINT('Ctrl Pts',(4.6305453691801,-0.794772684001097,7.01956357315458));
#53411=CARTESIAN_POINT('Ctrl Pts',(4.56812621870751,-0.636309800095391,
7.0079220313082));
#53412=CARTESIAN_POINT('Ctrl Pts',(4.49617888379903,-0.319434907277255,
6.98635594713443));
#53413=CARTESIAN_POINT('Ctrl Pts',(4.46425646853839,-0.15833333333338,6.97271361979845));
#53414=CARTESIAN_POINT('Ctrl Pts',(4.46270091772386,0.158333333333382,6.94610378427663));
#53415=CARTESIAN_POINT('Ctrl Pts',(4.49305793527175,0.319434907277263,6.93331088443485));
#53416=CARTESIAN_POINT('Ctrl Pts',(4.56185678259714,0.636309800095399,6.9003189849978));
#53417=CARTESIAN_POINT('Ctrl Pts',(4.62279227031746,0.794772684001082,6.8820914801612));
#53418=CARTESIAN_POINT('Ctrl Pts',(4.71084723147589,1.06847604194698,6.84306730324731));
#53419=CARTESIAN_POINT('Ctrl Pts',(4.74972412878629,1.18514270861519,6.8243806532821));
#53420=CARTESIAN_POINT('Ctrl Pts',(4.78936219347922,1.3000000000049,6.80389947354956));
#53421=CARTESIAN_POINT('Ctrl Pts',(4.81971140125444,-1.30000000000041,7.03315528836703));
#53422=CARTESIAN_POINT('Ctrl Pts',(4.78205573170685,-1.18514270861216,7.03656810206538));
#53423=CARTESIAN_POINT('Ctrl Pts',(4.74432372331691,-1.06847604194546,7.03679188724867));
#53424=CARTESIAN_POINT('Ctrl Pts',(4.65697887767639,-0.794772684001105,
7.02994158195739));
#53425=CARTESIAN_POINT('Ctrl Pts',(4.59403847146914,-0.636309800095399,
7.01716029480937));
#53426=CARTESIAN_POINT('Ctrl Pts',(4.52228780611912,-0.319434907277259,
6.99474285236196));
#53427=CARTESIAN_POINT('Ctrl Pts',(4.48928384359097,-0.158333333333382,
6.98032903146902));
#53428=CARTESIAN_POINT('Ctrl Pts',(4.48772670483764,0.158333333333384,6.95368112889899));
#53429=CARTESIAN_POINT('Ctrl Pts',(4.51913133053022,0.319434907277267,6.9418614804413));
#53430=CARTESIAN_POINT('Ctrl Pts',(4.58779617081258,0.636309800095406,6.90915489343853));
#53431=CARTESIAN_POINT('Ctrl Pts',(4.64936530997947,0.794772684001091,6.89103472616041));
#53432=CARTESIAN_POINT('Ctrl Pts',(4.73382833875133,1.068476041947,6.85105551647746));
#53433=CARTESIAN_POINT('Ctrl Pts',(4.77024949270081,1.1851427086152,6.83169607364316));
#53434=CARTESIAN_POINT('Ctrl Pts',(4.80653088510784,1.30000000000491,6.8102827064707));
#53435=CARTESIAN_POINT('Ctrl Pts',(4.83096799856834,-1.30000000000042,7.03863230490359));
#53436=CARTESIAN_POINT('Ctrl Pts',(4.79552525970306,-1.18514270861216,7.04304197726479));
#53437=CARTESIAN_POINT('Ctrl Pts',(4.7594275305241,-1.06847604194546,7.04386721275325));
#53438=CARTESIAN_POINT('Ctrl Pts',(4.67452139613975,-0.794772684001107,
7.03749290557919));
#53439=CARTESIAN_POINT('Ctrl Pts',(4.61129369378158,-0.6363098000954,7.02353895100331));
#53440=CARTESIAN_POINT('Ctrl Pts',(4.53968737529017,-0.31943490727726,7.00048559153463));
#53441=CARTESIAN_POINT('Ctrl Pts',(4.50593463306667,-0.158333333333383,
6.98581607785175));
#53442=CARTESIAN_POINT('Ctrl Pts',(4.50439362104787,0.158333333333385,6.95890559981965));
#53443=CARTESIAN_POINT('Ctrl Pts',(4.5365515958803,0.319434907277268,6.94703279480892));
#53444=CARTESIAN_POINT('Ctrl Pts',(4.60512847966881,0.636309800095408,6.91452153408074));
#53445=CARTESIAN_POINT('Ctrl Pts',(4.66706162126644,0.794772684001093,6.89726615352155));
#53446=CARTESIAN_POINT('Ctrl Pts',(4.74911765294583,1.068476041947,6.85682604989947));
#53447=CARTESIAN_POINT('Ctrl Pts',(4.78390477172902,1.1851427086152,6.8369783580517));
#53448=CARTESIAN_POINT('Ctrl Pts',(4.81795999365678,1.30000000000492,6.81478799676077));
#53449=CARTESIAN_POINT('Ctrl Pts',(4.85064503155324,-1.30000000000048,7.04822977209989));
#53450=CARTESIAN_POINT('Ctrl Pts',(4.81903273181648,-1.18514270861222,7.05464112033737));
#53451=CARTESIAN_POINT('Ctrl Pts',(4.78575590538376,-1.06847604194551,7.05679631184695));
#53452=CARTESIAN_POINT('Ctrl Pts',(4.70503438966276,-0.794772684001141,
7.05194266189598));
#53453=CARTESIAN_POINT('Ctrl Pts',(4.64119241175957,-0.63630980009543,7.03711520378676));
#53454=CARTESIAN_POINT('Ctrl Pts',(4.569903924195,-0.319434907277277,7.01237065244096));
#53455=CARTESIAN_POINT('Ctrl Pts',(4.53507152662869,-0.15833333333339,6.99506602236045));
#53456=CARTESIAN_POINT('Ctrl Pts',(4.53364402719554,0.158333333333392,6.96692253685092));
#53457=CARTESIAN_POINT('Ctrl Pts',(4.56703024750014,0.31943490727728,6.95587817161925));
#53458=CARTESIAN_POINT('Ctrl Pts',(4.63544906689471,0.636309800095436,6.92371507805114));
#53459=CARTESIAN_POINT('Ctrl Pts',(4.69805011618501,0.794772684001133,6.90760418502399));
#53460=CARTESIAN_POINT('Ctrl Pts',(4.77591426929651,1.06847604194705,6.86601741539685));
#53461=CARTESIAN_POINT('Ctrl Pts',(4.80784953659453,1.18514270861526,6.84516416546964));
#53462=CARTESIAN_POINT('Ctrl Pts',(4.83801556445957,1.30000000000498,6.82145903724525));
#53463=CARTESIAN_POINT('Ctrl Pts',(4.87871671758069,-1.30000000000054,7.06204569683692));
#53464=CARTESIAN_POINT('Ctrl Pts',(4.85261429636222,-1.18514270861228,7.07091863093545));
#53465=CARTESIAN_POINT('Ctrl Pts',(4.82339622580947,-1.06847604194556,7.07467246919414));
#53466=CARTESIAN_POINT('Ctrl Pts',(4.74869886453194,-0.794772684001184,
7.07151845106283));
#53467=CARTESIAN_POINT('Ctrl Pts',(4.68402722643482,-0.636309800095464,
7.05490525161979));
#53468=CARTESIAN_POINT('Ctrl Pts',(4.61311119848741,-0.319434907277293,
7.02872583981344));
#53469=CARTESIAN_POINT('Ctrl Pts',(4.57655793236568,-0.158333333333399,
7.00971783538784));
#53470=CARTESIAN_POINT('Ctrl Pts',(4.57519716966948,0.1583333333334,6.98097470457716));
#53471=CARTESIAN_POINT('Ctrl Pts',(4.61036071493994,0.319434907277299,6.97097376742859));
#53472=CARTESIAN_POINT('Ctrl Pts',(4.6785639529302,0.636309800095471,6.93914692873393));
#53473=CARTESIAN_POINT('Ctrl Pts',(4.74215816227969,0.794772684001174,6.92381055693346));
#53474=CARTESIAN_POINT('Ctrl Pts',(4.81404997075486,1.06847604194711,6.88067792422925));
#53475=CARTESIAN_POINT('Ctrl Pts',(4.84191306424059,1.18514270861532,6.85863141173312));
#53476=CARTESIAN_POINT('Ctrl Pts',(4.86651995117699,1.30000000000505,6.8332089052171));
#53477=CARTESIAN_POINT('Ctrl Pts',(4.91215937291756,-1.30000000000072,7.08002716631402));
#53478=CARTESIAN_POINT('Ctrl Pts',(4.89251476135823,-1.18514270861244,7.09277168660335));
#53479=CARTESIAN_POINT('Ctrl Pts',(4.86807491003913,-1.0684760419457,7.09900844705983));
#53480=CARTESIAN_POINT('Ctrl Pts',(4.80053600118698,-0.794772684001288,
7.09838238428716));
#53481=CARTESIAN_POINT('Ctrl Pts',(4.73507778921139,-0.636309800095545,
7.07844833130014));
#53482=CARTESIAN_POINT('Ctrl Pts',(4.66466571408515,-0.319434907277332,
7.05037683229815));
#53483=CARTESIAN_POINT('Ctrl Pts',(4.62598644584666,-0.158333333333419,
7.02995740311529));
#53484=CARTESIAN_POINT('Ctrl Pts',(4.62473318702404,0.158333333333421,7.00024857509394));
#53485=CARTESIAN_POINT('Ctrl Pts',(4.66209924063571,0.319434907277341,6.99060220955304));
#53486=CARTESIAN_POINT('Ctrl Pts',(4.73008064343413,0.636309800095553,6.95888608045245));
#53487=CARTESIAN_POINT('Ctrl Pts',(4.79480850862359,0.794772684001275,6.94538259911256));
#53488=CARTESIAN_POINT('Ctrl Pts',(4.8596126378628,1.06847604194724,6.89966616634739));
#53489=CARTESIAN_POINT('Ctrl Pts',(4.88264845166585,1.18514270861547,6.87556527970286));
#53490=CARTESIAN_POINT('Ctrl Pts',(4.90066877295375,1.30000000000521,6.84715245619721));
#53491=CARTESIAN_POINT('Ctrl Pts',(4.93725468010072,-1.3000000000009,7.09313254193612));
#53492=CARTESIAN_POINT('Ctrl Pts',(4.92251910617382,-1.1851427086126,7.10818590821563));
#53493=CARTESIAN_POINT('Ctrl Pts',(4.90167952468772,-1.06847604194585,7.11607516844198));
#53494=CARTESIAN_POINT('Ctrl Pts',(4.83943444394655,-0.7947726840014,7.11775041964863));
#53495=CARTESIAN_POINT('Ctrl Pts',(4.77307358991183,-0.636309800095634,
7.09754354905514));
#53496=CARTESIAN_POINT('Ctrl Pts',(4.70299017031348,-0.319434907277378,
7.06849582648515));
#53497=CARTESIAN_POINT('Ctrl Pts',(4.66292407258137,-0.158333333333441,
7.0456896209772));
#53498=CARTESIAN_POINT('Ctrl Pts',(4.66180668659304,0.158333333333443,7.01506827046914));
#53499=CARTESIAN_POINT('Ctrl Pts',(4.70074790993159,0.319434907277388,7.0064583020073));
#53500=CARTESIAN_POINT('Ctrl Pts',(4.7685705480685,0.636309800095645,6.97475153656514));
#53501=CARTESIAN_POINT('Ctrl Pts',(4.83420160951624,0.794772684001386,6.96180863596743));
#53502=CARTESIAN_POINT('Ctrl Pts',(4.89371750845255,1.06847604194739,6.91403814004657));
#53503=CARTESIAN_POINT('Ctrl Pts',(4.91313980712197,1.18514270861564,6.88848593338276));
#53504=CARTESIAN_POINT('Ctrl Pts',(4.92622217709251,1.3000000000054,6.85805959766812));
#53505=CARTESIAN_POINT('Ctrl Pts',(4.95249061094029,-1.30000000000096,7.10174801877597));
#53506=CARTESIAN_POINT('Ctrl Pts',(4.94070585124906,-1.18514270861266,7.11849736921204));
#53507=CARTESIAN_POINT('Ctrl Pts',(4.9220425490444,-1.06847604194591,7.12752623178392));
#53508=CARTESIAN_POINT('Ctrl Pts',(4.8630357781171,-0.794772684001439,7.13054883909814));
#53509=CARTESIAN_POINT('Ctrl Pts',(4.79622705686757,-0.636309800095667,
7.10950393241955));
#53510=CARTESIAN_POINT('Ctrl Pts',(4.72640341159517,-0.319434907277394,
7.07947600393533));
#53511=CARTESIAN_POINT('Ctrl Pts',(4.68551672620583,-0.158333333333449,
7.05503452127875));
#53512=CARTESIAN_POINT('Ctrl Pts',(4.68445951073731,0.158333333333451,7.02403999448838));
#53513=CARTESIAN_POINT('Ctrl Pts',(4.72429471911312,0.319434907277403,7.01652446843246));
#53514=CARTESIAN_POINT('Ctrl Pts',(4.79195320377858,0.636309800095676,6.98537928389906));
#53515=CARTESIAN_POINT('Ctrl Pts',(4.85806437875647,0.794772684001427,6.97348302681867));
#53516=CARTESIAN_POINT('Ctrl Pts',(4.9143815398544,1.06847604194745,6.92419940749604));
#53517=CARTESIAN_POINT('Ctrl Pts',(4.93163769063275,1.1851427086157,6.89740020700775));
#53518=CARTESIAN_POINT('Ctrl Pts',(4.94177237990647,1.30000000000546,6.86513485869803));
#53519=CARTESIAN_POINT('Ctrl Pts',(4.95733067203265,-1.30000000000097,7.10451141794751));
#53520=CARTESIAN_POINT('Ctrl Pts',(4.94647610786229,-1.18514270861266,7.12183906008298));
#53521=CARTESIAN_POINT('Ctrl Pts',(4.92850102344608,-1.06847604194591,7.13124929539685));
#53522=CARTESIAN_POINT('Ctrl Pts',(4.87052515631817,-0.794772684001442,
7.13469802785336));
#53523=CARTESIAN_POINT('Ctrl Pts',(4.80359922661366,-0.636309800095668,
7.11325670664432));
#53524=CARTESIAN_POINT('Ctrl Pts',(4.73385490618067,-0.319434907277395,
7.0829648622029));
#53525=CARTESIAN_POINT('Ctrl Pts',(4.69267438292149,-0.15833333333345,7.05823840696025));
#53526=CARTESIAN_POINT('Ctrl Pts',(4.69164133602762,0.158333333333452,7.02708359220464));
#53527=CARTESIAN_POINT('Ctrl Pts',(4.73179205882609,0.319434907277404,7.01968331650939));
#53528=CARTESIAN_POINT('Ctrl Pts',(4.79942552436748,0.636309800095677,6.9884947697978));
#53529=CARTESIAN_POINT('Ctrl Pts',(4.86571380921929,0.794772684001429,6.976708471892));
#53530=CARTESIAN_POINT('Ctrl Pts',(4.92100610955694,1.06847604194745,6.92700584775463));
#53531=CARTESIAN_POINT('Ctrl Pts',(4.93756098960259,1.1851427086157,6.89991592312669));
#53532=CARTESIAN_POINT('Ctrl Pts',(4.94673676165919,1.30000000000546,6.8672504981963));
#53533=CARTESIAN_POINT('Ctrl Pts',(4.96008932255006,-1.30000000000097,7.10613091373259));
#53534=CARTESIAN_POINT('Ctrl Pts',(4.94975998138204,-1.18514270861267,7.1238253241681));
#53535=CARTESIAN_POINT('Ctrl Pts',(4.9321750309227,-1.06847604194591,7.13347119770518));
#53536=CARTESIAN_POINT('Ctrl Pts',(4.87478836856172,-0.794772684001444,
7.13716136488657));
#53537=CARTESIAN_POINT('Ctrl Pts',(4.80781052390886,-0.63630980009567,7.11540215248782));
#53538=CARTESIAN_POINT('Ctrl Pts',(4.73811441601435,-0.319434907277396,
7.08494616615572));
#53539=CARTESIAN_POINT('Ctrl Pts',(4.69675812744069,-0.15833333333345,7.06011197857061));
#53540=CARTESIAN_POINT('Ctrl Pts',(4.69573759385705,0.158333333333452,7.02887605276384));
#53541=CARTESIAN_POINT('Ctrl Pts',(4.73607110158677,0.319434907277405,7.02152412363642));
#53542=CARTESIAN_POINT('Ctrl Pts',(4.80369303355971,0.636309800095679,6.99029024862042));
#53543=CARTESIAN_POINT('Ctrl Pts',(4.87008576851561,0.794772684001431,6.97854073298898));
#53544=CARTESIAN_POINT('Ctrl Pts',(4.92479332431127,1.06847604194745,6.928592729483));
#53545=CARTESIAN_POINT('Ctrl Pts',(4.94094715647548,1.1851427086157,6.90133988204735));
#53546=CARTESIAN_POINT('Ctrl Pts',(4.9495739470145,1.30000000000547,6.86845482713801));
#53547=CARTESIAN_POINT('Ctrl Pts',(4.96284649527735,-1.30000000000097,7.1077561478983));
#53548=CARTESIAN_POINT('Ctrl Pts',(4.95304069625497,-1.18514270861267,7.12582630027899));
#53549=CARTESIAN_POINT('Ctrl Pts',(4.93584495681872,-1.06847604194592,7.13571277356245));
#53550=CARTESIAN_POINT('Ctrl Pts',(4.87904711801652,-0.794772684001446,
7.13964656877545));
#53551=CARTESIAN_POINT('Ctrl Pts',(4.81202080450033,-0.636309800095671,
7.11754979988703));
#53552=CARTESIAN_POINT('Ctrl Pts',(4.74237295771725,-0.319434907277396,
7.0869326009472));
#53553=CARTESIAN_POINT('Ctrl Pts',(4.70083792287829,-0.15833333333345,7.06201365483902));
#53554=CARTESIAN_POINT('Ctrl Pts',(4.69983004401309,0.158333333333452,7.03069623555303));
#53555=CARTESIAN_POINT('Ctrl Pts',(4.74034847566072,0.319434907277405,7.02337647020484));
#53556=CARTESIAN_POINT('Ctrl Pts',(4.80796111658925,0.636309800095681,6.99207894680393));
#53557=CARTESIAN_POINT('Ctrl Pts',(4.87446055457127,0.794772684001433,6.98034563087335));
#53558=CARTESIAN_POINT('Ctrl Pts',(4.92858340434634,1.06847604194745,6.93015259185655));
#53559=CARTESIAN_POINT('Ctrl Pts',(4.94433555464321,1.18514270861571,6.9027428538463));
#53560=CARTESIAN_POINT('Ctrl Pts',(4.95241207901841,1.30000000000547,6.86965008458096));
#53561=CARTESIAN_POINT('Ctrl Pts',(4.96629038502904,-1.30000000000098,7.10979928916033));
#53562=CARTESIAN_POINT('Ctrl Pts',(4.95713670065089,-1.18514270861268,7.12835135544506));
#53563=CARTESIAN_POINT('Ctrl Pts',(4.94042605295921,-1.06847604194592,7.13854596531376));
#53564=CARTESIAN_POINT('Ctrl Pts',(4.88436301681819,-0.794772684001452,
7.14279015731071));
#53565=CARTESIAN_POINT('Ctrl Pts',(4.81727907004437,-0.636309800095676,
7.12025291182898));
#53566=CARTESIAN_POINT('Ctrl Pts',(4.74769202939327,-0.319434907277399,
7.08943460009879));
#53567=CARTESIAN_POINT('Ctrl Pts',(4.70593253920081,-0.158333333333452,
7.06442226739939));
#53568=CARTESIAN_POINT('Ctrl Pts',(4.70494017607543,0.158333333333454,7.0330076981234));
#53569=CARTESIAN_POINT('Ctrl Pts',(4.74568956954566,0.319434907277408,7.02572793492377));
#53570=CARTESIAN_POINT('Ctrl Pts',(4.81329136002281,0.636309800095685,6.99434448950996));
#53571=CARTESIAN_POINT('Ctrl Pts',(4.87992526190969,0.794772684001439,6.98262174097569));
#53572=CARTESIAN_POINT('Ctrl Pts',(4.93331876013669,1.06847604194746,6.93211213018218));
#53573=CARTESIAN_POINT('Ctrl Pts',(4.94856952183904,1.18514270861572,6.90450207555735));
#53574=CARTESIAN_POINT('Ctrl Pts',(4.95595897828523,1.30000000000548,6.87114570525484));
#53575=CARTESIAN_POINT('Ctrl Pts',(4.97042752796124,-1.30000000000099,7.11222067280422));
#53576=CARTESIAN_POINT('Ctrl Pts',(4.96206120246261,-1.18514270861269,7.13132279160153));
#53577=CARTESIAN_POINT('Ctrl Pts',(4.94593429676918,-1.06847604194593,7.14187758047346));
#53578=CARTESIAN_POINT('Ctrl Pts',(4.89074942569216,-0.794772684001456,
7.14651521223085));
#53579=CARTESIAN_POINT('Ctrl Pts',(4.82357707335456,-0.63630980009568,7.1235618642295));
#53580=CARTESIAN_POINT('Ctrl Pts',(4.75406052371135,-0.319434907277401,
7.09251675749891));
#53581=CARTESIAN_POINT('Ctrl Pts',(4.71204634504394,-0.158333333333453,
7.06730418522112));
#53582=CARTESIAN_POINT('Ctrl Pts',(4.71107332656958,0.158333333333454,7.03577415975341));
#53583=CARTESIAN_POINT('Ctrl Pts',(4.75209106551394,0.319434907277409,7.02860172769455));
#53584=CARTESIAN_POINT('Ctrl Pts',(4.81967335398172,0.636309800095689,6.99716397318012));
#53585=CARTESIAN_POINT('Ctrl Pts',(4.88646202340049,0.794772684001444,6.98550864356446));
#53586=CARTESIAN_POINT('Ctrl Pts',(4.93898422941487,1.06847604194747,6.93458752317071));
#53587=CARTESIAN_POINT('Ctrl Pts',(4.95363781148886,1.18514270861572,6.90670098220033));
#53588=CARTESIAN_POINT('Ctrl Pts',(4.96021005879261,1.30000000000549,6.87296976646473));
#53589=CARTESIAN_POINT('Ctrl Pts',(4.97388248677194,-1.300000000001,7.11419330698134));
#53590=CARTESIAN_POINT('Ctrl Pts',(4.96618059363683,-1.1851427086127,7.13370484739741));
#53591=CARTESIAN_POINT('Ctrl Pts',(4.95054344986816,-1.06847604194594,7.1445400528125));
#53592=CARTESIAN_POINT('Ctrl Pts',(4.89608650315763,-0.794772684001463,
7.14952747534969));
#53593=CARTESIAN_POINT('Ctrl Pts',(4.82881225868493,-0.636309800095686,
7.12639344125074));
#53594=CARTESIAN_POINT('Ctrl Pts',(4.75935076571616,-0.319434907277404,
7.09517759987284));
#53595=CARTESIAN_POINT('Ctrl Pts',(4.71714499090967,-0.158333333333454,
7.06966810286072));
#53596=CARTESIAN_POINT('Ctrl Pts',(4.71618917228211,0.158333333333456,7.03804039880248));
#53597=CARTESIAN_POINT('Ctrl Pts',(4.75741862739402,0.319434907277412,7.03103876207293));
#53598=CARTESIAN_POINT('Ctrl Pts',(4.82497494583709,0.636309800095695,6.99963073021055));
#53599=CARTESIAN_POINT('Ctrl Pts',(4.89188220977964,0.794772684001451,6.98811958001273));
#53600=CARTESIAN_POINT('Ctrl Pts',(4.94368264879308,1.06847604194748,6.93682171039539));
#53601=CARTESIAN_POINT('Ctrl Pts',(4.95784437193867,1.18514270861573,6.9086581737759));
#53602=CARTESIAN_POINT('Ctrl Pts',(4.96374532757619,1.3000000000055,6.87453604752103));
#53603=CARTESIAN_POINT('Ctrl Pts',(4.97630421138477,-1.300000000001,7.11555377724202));
#53604=CARTESIAN_POINT('Ctrl Pts',(4.96907109514182,-1.1851427086127,7.13533017872965));
#53605=CARTESIAN_POINT('Ctrl Pts',(4.95377823876846,-1.06847604194594,7.1463530476813));
#53606=CARTESIAN_POINT('Ctrl Pts',(4.89982906917387,-0.794772684001465,
7.15159566878068));
#53607=CARTESIAN_POINT('Ctrl Pts',(4.83247110010632,-0.636309800095687,
7.12840880700605));
#53608=CARTESIAN_POINT('Ctrl Pts',(4.76304610150664,-0.319434907277404,
7.09708440442982));
#53609=CARTESIAN_POINT('Ctrl Pts',(4.72071445783629,-0.158333333333454,
7.0713148078593));
#53610=CARTESIAN_POINT('Ctrl Pts',(4.71977122477105,0.158333333333456,7.03961757193506));
#53611=CARTESIAN_POINT('Ctrl Pts',(4.76114467462826,0.319434907277413,7.03276470241732));
#53612=CARTESIAN_POINT('Ctrl Pts',(4.82867884935533,0.636309800095696,7.0014087449179));
#53613=CARTESIAN_POINT('Ctrl Pts',(4.89566416734629,0.794772684001452,6.9900399194674));
#53614=CARTESIAN_POINT('Ctrl Pts',(4.94696107898536,1.06847604194748,6.93846538579834));
#53615=CARTESIAN_POINT('Ctrl Pts',(4.96078097285189,1.18514270861574,6.91008837141033));
#53616=CARTESIAN_POINT('Ctrl Pts',(4.96621622827414,1.3000000000055,6.87565904723499));
#53617=CARTESIAN_POINT('Ctrl Pts',(4.97751550866759,-1.30000000000101,7.11623101982547));
#53618=CARTESIAN_POINT('Ctrl Pts',(4.97051729691734,-1.1851427086127,7.13613666114551));
#53619=CARTESIAN_POINT('Ctrl Pts',(4.95539676594355,-1.06847604194594,7.14725219990602));
#53620=CARTESIAN_POINT('Ctrl Pts',(4.90170113227145,-0.794772684001466,
7.15262442273227));
#53621=CARTESIAN_POINT('Ctrl Pts',(4.83429936465745,-0.636309800095687,
7.1294227924869));
#53622=CARTESIAN_POINT('Ctrl Pts',(4.764892248713,-0.319434907277404,7.09804621852923));
#53623=CARTESIAN_POINT('Ctrl Pts',(4.72249891275604,-0.158333333333454,
7.07213879181453));
#53624=CARTESIAN_POINT('Ctrl Pts',(4.72156205558291,0.158333333333456,7.04040671329765));
#53625=CARTESIAN_POINT('Ctrl Pts',(4.7630068896913,0.319434907277413,7.03363250408665));
#53626=CARTESIAN_POINT('Ctrl Pts',(4.83052941439548,0.636309800095697,7.00230729896226));
#53627=CARTESIAN_POINT('Ctrl Pts',(4.89755300497442,0.794772684001453,6.99101596247396));
#53628=CARTESIAN_POINT('Ctrl Pts',(4.94859845261492,1.06847604194748,6.93930114815657));
#53629=CARTESIAN_POINT('Ctrl Pts',(4.96224783122096,1.18514270861574,6.91081442761733));
#53630=CARTESIAN_POINT('Ctrl Pts',(4.96745090556956,1.3000000000055,6.87622641343428));
#53631=CARTESIAN_POINT('Ctrl Pts',(4.97812123381433,-1.30000000000101,7.1165690665992));
#53632=CARTESIAN_POINT('Ctrl Pts',(4.9712405789915,-1.1851427086127,7.13653863761121));
#53633=CARTESIAN_POINT('Ctrl Pts',(4.95620624288918,-1.06847604194594,7.14770027504741));
#53634=CARTESIAN_POINT('Ctrl Pts',(4.90263728399023,-0.794772684001466,
7.15313780182181));
#53635=CARTESIAN_POINT('Ctrl Pts',(4.83521322869637,-0.636309800095687,
7.12993111711226));
#53636=CARTESIAN_POINT('Ctrl Pts',(4.76581487589349,-0.319434907277404,
7.09852959461544));
#53637=CARTESIAN_POINT('Ctrl Pts',(4.72339074516187,-0.158333333333454,
7.07255305525712));
#53638=CARTESIAN_POINT('Ctrl Pts',(4.72245710661183,0.158333333333456,7.04080347291612));
#53639=CARTESIAN_POINT('Ctrl Pts',(4.76393775562899,0.319434907277413,7.03406779705712));
#53640=CARTESIAN_POINT('Ctrl Pts',(4.83145440374682,0.636309800095696,7.00275852022833));
#53641=CARTESIAN_POINT('Ctrl Pts',(4.89849685066599,0.794772684001453,6.99150802023193));
#53642=CARTESIAN_POINT('Ctrl Pts',(4.94941660947784,1.06847604194748,6.93972298463305));
#53643=CARTESIAN_POINT('Ctrl Pts',(4.96298081810854,1.18514270861574,6.91118089734209));
#53644=CARTESIAN_POINT('Ctrl Pts',(4.96806795854315,1.3000000000055,6.8765125458464));
#53645=CARTESIAN_POINT('Ctrl Pts',(4.97846737342916,-1.30000000000101,7.1167621372107));
#53646=CARTESIAN_POINT('Ctrl Pts',(4.97165389322874,-1.1851427086127,7.13676826564106));
#53647=CARTESIAN_POINT('Ctrl Pts',(4.95666881041786,-1.06847604194594,7.14795626906208));
#53648=CARTESIAN_POINT('Ctrl Pts',(4.9031722346155,-0.794772684001466,7.1534311622856));
#53649=CARTESIAN_POINT('Ctrl Pts',(4.83573539246057,-0.636309800095688,
7.13022194721542));
#53650=CARTESIAN_POINT('Ctrl Pts',(4.76634214031379,-0.319434907277405,
7.09880555346919));
#53651=CARTESIAN_POINT('Ctrl Pts',(4.72390064694252,-0.158333333333454,
7.07278793416587));
#53652=CARTESIAN_POINT('Ctrl Pts',(4.72296883574537,0.158333333333456,7.04102843310387));
#53653=CARTESIAN_POINT('Ctrl Pts',(4.76446968198849,0.319434907277413,7.03431659521749));
#53654=CARTESIAN_POINT('Ctrl Pts',(4.83198289997454,0.636309800095697,7.00301690285337));
#53655=CARTESIAN_POINT('Ctrl Pts',(4.89903625057841,0.794772684001453,6.99178893957758));
#53656=CARTESIAN_POINT('Ctrl Pts',(4.94988421697014,1.06847604194748,6.93996342244769));
#53657=CARTESIAN_POINT('Ctrl Pts',(4.96339975863266,1.18514270861574,6.91138957243487));
#53658=CARTESIAN_POINT('Ctrl Pts',(4.9684206414094,1.3000000000055,6.87667521845023));
#53659=CARTESIAN_POINT('Ctrl Pts',(4.98971731443253,-1.30000000000093,7.12303343632508));
#53660=CARTESIAN_POINT('Ctrl Pts',(4.98508891455217,-1.18514270861263,7.14421273284097));
#53661=CARTESIAN_POINT('Ctrl Pts',(4.97170506847732,-1.06847604194588,7.15625196709077));
#53662=CARTESIAN_POINT('Ctrl Pts',(4.92055887438486,-0.794772684001422,
7.16294963435057));
#53663=CARTESIAN_POINT('Ctrl Pts',(4.85270237754255,-0.636309800095653,
7.13967947678175));
#53664=CARTESIAN_POINT('Ctrl Pts',(4.78346413868162,-0.319434907277387,
7.10785049809407));
#53665=CARTESIAN_POINT('Ctrl Pts',(4.74044174664496,-0.158333333333446,
7.08061369858619));
#53666=CARTESIAN_POINT('Ctrl Pts',(4.73957082539452,0.158333333333448,7.04852441713683));
#53667=CARTESIAN_POINT('Ctrl Pts',(4.78175076018467,0.319434907277395,7.04243439289715));
#53668=CARTESIAN_POINT('Ctrl Pts',(4.84915701604034,0.636309800095661,7.01142060033288));
#53669=CARTESIAN_POINT('Ctrl Pts',(4.91654958673662,0.794772684001409,7.00102617359138));
#53670=CARTESIAN_POINT('Ctrl Pts',(4.96506311114736,1.06847604194742,6.94791011372403));
#53671=CARTESIAN_POINT('Ctrl Pts',(4.97699869546298,1.18514270861567,6.91830327291942));
#53672=CARTESIAN_POINT('Ctrl Pts',(4.97987015697993,1.30000000000543,6.88208156548295));
#53673=CARTESIAN_POINT('Ctrl Pts',(5.01178389861922,-1.3000000000005,7.13627644036779));
#53674=CARTESIAN_POINT('Ctrl Pts',(5.01131141371871,-1.18514270861224,7.16062282534453));
#53675=CARTESIAN_POINT('Ctrl Pts',(5.00100904105187,-1.06847604194552,7.17476947647352));
#53676=CARTESIAN_POINT('Ctrl Pts',(4.9544994920063,-0.794772684001155,7.18388764497125));
#53677=CARTESIAN_POINT('Ctrl Pts',(4.88616940395213,-0.636309800095441,
7.15851802196042));
#53678=CARTESIAN_POINT('Ctrl Pts',(4.81732321849579,-0.319434907277282,
7.12548645290095));
#53679=CARTESIAN_POINT('Ctrl Pts',(4.77299709493401,-0.158333333333393,
7.09689357667308));
#53680=CARTESIAN_POINT('Ctrl Pts',(4.77223561752897,0.158333333333395,7.06422913948137));
#53681=CARTESIAN_POINT('Ctrl Pts',(4.81577330570672,0.319434907277287,7.05922075284174));
#53682=CARTESIAN_POINT('Ctrl Pts',(4.88312332797933,0.636309800095447,7.02762546170713));
#53683=CARTESIAN_POINT('Ctrl Pts',(4.95151460519703,0.794772684001146,7.01634068080159));
#53684=CARTESIAN_POINT('Ctrl Pts',(4.99538366475049,1.06847604194707,6.96116272290421));
#53685=CARTESIAN_POINT('Ctrl Pts',(5.00409750598239,1.18514270861528,6.93043959360876));
#53686=CARTESIAN_POINT('Ctrl Pts',(5.00253589807423,1.300000000005,6.89287782844697));
#53687=CARTESIAN_POINT('Ctrl Pts',(5.03373827646428,-1.3,7.14940561675095));
#53688=CARTESIAN_POINT('Ctrl Pts',(5.03743514540704,-1.18514270861178,7.17662169039555));
#53689=CARTESIAN_POINT('Ctrl Pts',(5.03020931803737,-1.06847604194511,7.19274767803129));
#53690=CARTESIAN_POINT('Ctrl Pts',(4.98828259773197,-0.794772684000847,
7.20438161821808));
#53691=CARTESIAN_POINT('Ctrl Pts',(4.91934781307154,-0.636309800095196,
7.17772787593842));
#53692=CARTESIAN_POINT('Ctrl Pts',(4.85084550516311,-0.319434907277159,
7.14381723154251));
#53693=CARTESIAN_POINT('Ctrl Pts',(4.80525449214962,-0.158333333333332,
7.11377207003864));
#53694=CARTESIAN_POINT('Ctrl Pts',(4.80463957298797,0.158333333333334,7.08035575294124));
#53695=CARTESIAN_POINT('Ctrl Pts',(4.84964913467179,0.319434907277167,7.07559389246093));
#53696=CARTESIAN_POINT('Ctrl Pts',(4.91683072495962,0.636309800095206,7.04427067070441));
#53697=CARTESIAN_POINT('Ctrl Pts',(4.98579503969525,0.794772684000841,7.03523465559988));
#53698=CARTESIAN_POINT('Ctrl Pts',(5.02510837557537,1.06847604194666,6.97733180991118));
#53699=CARTESIAN_POINT('Ctrl Pts',(5.03075217902059,1.18514270861482,6.94436545494296));
#53700=CARTESIAN_POINT('Ctrl Pts',(5.02502249951107,1.3000000000045,6.90349674139346));
#53701=CARTESIAN_POINT('Ctrl Pts',(5.0446386636865,-1.3,7.15639922225603));
#53702=CARTESIAN_POINT('Ctrl Pts',(5.05044042294362,-1.18514270861178,7.18489122215592));
#53703=CARTESIAN_POINT('Ctrl Pts',(5.04476129211945,-1.06847604194512,7.20192692863061));
#53704=CARTESIAN_POINT('Ctrl Pts',(5.0051182109774,-0.794772684000851,7.21481648893273));
#53705=CARTESIAN_POINT('Ctrl Pts',(4.93580560547694,-0.636309800095197,
7.18795105230746));
#53706=CARTESIAN_POINT('Ctrl Pts',(4.86748690268215,-0.319434907277159,
7.15354929193199));
#53707=CARTESIAN_POINT('Ctrl Pts',(4.82135018302871,-0.158333333333332,
7.12232171799169));
#53708=CARTESIAN_POINT('Ctrl Pts',(4.82082865786803,0.158333333333334,7.08844490884846));
#53709=CARTESIAN_POINT('Ctrl Pts',(4.86650233516518,0.319434907277167,7.08425772830895));
#53710=CARTESIAN_POINT('Ctrl Pts',(4.93363960349709,0.636309800095206,7.05278755158574));
#53711=CARTESIAN_POINT('Ctrl Pts',(5.00304362126358,0.79477268400084,7.04374488751153));
#53712=CARTESIAN_POINT('Ctrl Pts',(5.04007197138552,1.06847604194666,6.98466339093232));
#53713=CARTESIAN_POINT('Ctrl Pts',(5.0441424144131,1.18514270861482,6.95094305803163));
#53714=CARTESIAN_POINT('Ctrl Pts',(5.03625509973595,1.3000000000045,6.90907658291435));
#53715=CARTESIAN_POINT('',(4.94063912830279,1.2,6.89572216005206));
#53716=CARTESIAN_POINT('Ctrl Pts',(4.94063912830279,1.2,6.89572216005206));
#53717=CARTESIAN_POINT('Ctrl Pts',(4.92390473453183,1.21597616111059,6.88390203159158));
#53718=CARTESIAN_POINT('Ctrl Pts',(4.90745111372174,1.23156175617616,6.87117277576754));
#53719=CARTESIAN_POINT('Ctrl Pts',(4.87600876742023,1.261382346883,6.84892960913813));
#53720=CARTESIAN_POINT('Ctrl Pts',(4.84864612923132,1.28723399810768,6.82956657428991));
#53721=CARTESIAN_POINT('Ctrl Pts',(4.83514898734333,1.30000000000497,6.82074511190421));
#53722=CARTESIAN_POINT('',(4.94779107629418,0.653834841369961,7.05213700604833));
#53723=CARTESIAN_POINT('Ctrl Pts',(4.94779107633072,0.653834841368704,7.05213700604228));
#53724=CARTESIAN_POINT('Ctrl Pts',(4.94730914812078,0.717423550067115,7.03601072567456));
#53725=CARTESIAN_POINT('Ctrl Pts',(4.9468618942627,0.763685300918966,7.02296808068869));
#53726=CARTESIAN_POINT('Ctrl Pts',(4.94482981071674,0.949868242106328,6.9711151806119));
#53727=CARTESIAN_POINT('Ctrl Pts',(4.94322281841657,1.06483235008049,6.93767421437741));
#53728=CARTESIAN_POINT('Ctrl Pts',(4.9406391283028,1.2,6.89572216005206));
#53729=CARTESIAN_POINT('',(4.94999291725008,-0.653834841531101,7.19162628075221));
#53730=CARTESIAN_POINT('Ctrl Pts',(4.94999291725008,-0.6538348415311,7.1916262807522));
#53731=CARTESIAN_POINT('Ctrl Pts',(4.91226053268323,-0.57598825529314,7.17418301909822));
#53732=CARTESIAN_POINT('Ctrl Pts',(4.88066779187612,-0.493638204898488,
7.15874635405016));
#53733=CARTESIAN_POINT('Ctrl Pts',(4.83632237990281,-0.338136439546806,
7.13434742800906));
#53734=CARTESIAN_POINT('Ctrl Pts',(4.82127841502355,-0.265661862329625,
7.12466561743286));
#53735=CARTESIAN_POINT('Ctrl Pts',(4.80341669336683,-0.129718290004032,
7.10807972575262));
#53736=CARTESIAN_POINT('Ctrl Pts',(4.79913211996351,-0.0666263115009711,
7.10100067551947));
#53737=CARTESIAN_POINT('Ctrl Pts',(4.79855022586424,0.0595444515987862,
7.0876845625097));
#53738=CARTESIAN_POINT('Ctrl Pts',(4.80223154791772,0.122778289585405,7.08135019967731));
#53739=CARTESIAN_POINT('Ctrl Pts',(4.81904908132387,0.260130845872543,7.06921455582952));
#53740=CARTESIAN_POINT('Ctrl Pts',(4.83379007158933,0.333945959033105,7.06371918300369));
#53741=CARTESIAN_POINT('Ctrl Pts',(4.87782753950601,0.491210667319418,7.05522657143219));
#53742=CARTESIAN_POINT('Ctrl Pts',(4.90929426434707,0.574355066564918,7.05261167566303));
#53743=CARTESIAN_POINT('Ctrl Pts',(4.94779107625945,0.653834841386506,7.05213700600196));
#53744=CARTESIAN_POINT('',(4.94934486610223,-1.2,7.11946804120388));
#53745=CARTESIAN_POINT('Ctrl Pts',(4.94934486610223,-1.2,7.11946804120388));
#53746=CARTESIAN_POINT('Ctrl Pts',(4.94954877297065,-1.13394982025349,7.13199977925508));
#53747=CARTESIAN_POINT('Ctrl Pts',(4.9497650894168,-1.03818575991279,7.14834426936692));
#53748=CARTESIAN_POINT('Ctrl Pts',(4.94997573806144,-0.796404165621293,
7.17980499094405));
#53749=CARTESIAN_POINT('Ctrl Pts',(4.94998207838412,-0.739512578337757,
7.18521905498287));
#53750=CARTESIAN_POINT('Ctrl Pts',(4.94999291725008,-0.653834841531101,
7.1916262807522));
#53751=CARTESIAN_POINT('Ctrl Pts',(4.84757809483801,-1.3,7.04674656791213));
#53752=CARTESIAN_POINT('Ctrl Pts',(4.86730712653357,-1.28070206600169,7.06007770157836));
#53753=CARTESIAN_POINT('Ctrl Pts',(4.88299831626126,-1.26532349056323,7.07130878936968));
#53754=CARTESIAN_POINT('Ctrl Pts',(4.92478995175362,-1.224253828607,7.10129971725897));
#53755=CARTESIAN_POINT('Ctrl Pts',(4.92948688426405,-1.21960121810543,7.10384727574809));
#53756=CARTESIAN_POINT('Ctrl Pts',(4.94934486610223,-1.2,7.11946804120388));
#53757=CARTESIAN_POINT('Origin',(0.,1.25,7.2));
#53758=CARTESIAN_POINT('Origin',(0.,1.2,7.2));
#53759=CARTESIAN_POINT('Origin',(0.,0.92691742076555,7.2));
#53760=CARTESIAN_POINT('Origin',(0.,0.653834841531101,7.2));
#53761=CARTESIAN_POINT('Origin',(0.,0.,7.2));
#53762=CARTESIAN_POINT('Origin',(0.,-0.653834841531101,7.2));
#53763=CARTESIAN_POINT('Origin',(0.,-0.926917420765551,7.2));
#53764=CARTESIAN_POINT('Origin',(0.,-1.2,7.2));
#53765=CARTESIAN_POINT('Origin',(0.,-1.25,7.2));
#53766=CARTESIAN_POINT('Ctrl Pts',(5.03625509974048,-1.30000000000004,7.49092341708498));
#53767=CARTESIAN_POINT('Ctrl Pts',(5.04414241441886,-1.18514270861181,7.44905694196869));
#53768=CARTESIAN_POINT('Ctrl Pts',(5.04007197139197,-1.06847604194513,7.41533660906868));
#53769=CARTESIAN_POINT('Ctrl Pts',(5.00304362127007,-0.794772684000851,
7.35625511248991));
#53770=CARTESIAN_POINT('Ctrl Pts',(4.93363960349964,-0.636309800095197,
7.34721244841535));
#53771=CARTESIAN_POINT('Ctrl Pts',(4.86650233516645,-0.319434907277159,
7.31574227169205));
#53772=CARTESIAN_POINT('Ctrl Pts',(4.82082865787052,-0.158333333333332,
7.31155509115263));
#53773=CARTESIAN_POINT('Ctrl Pts',(4.82135018303129,0.158333333333334,7.27767828200944));
#53774=CARTESIAN_POINT('Ctrl Pts',(4.86748690268524,0.319434907277167,7.24645070806922));
#53775=CARTESIAN_POINT('Ctrl Pts',(4.93580560547818,0.636309800095206,7.21204894769365));
#53776=CARTESIAN_POINT('Ctrl Pts',(5.00511821097388,0.79477268400084,7.18518351106812));
#53777=CARTESIAN_POINT('Ctrl Pts',(5.04476129211656,1.06847604194523,7.19807307137016));
#53778=CARTESIAN_POINT('Ctrl Pts',(5.05044042294223,1.18514270861202,7.21510877784489));
#53779=CARTESIAN_POINT('Ctrl Pts',(5.04463866368783,1.30000000000036,7.24360077774488));
#53780=CARTESIAN_POINT('Ctrl Pts',(5.0250224995653,-1.30000000000004,7.49650325861012));
#53781=CARTESIAN_POINT('Ctrl Pts',(5.03075217910044,-1.18514270861181,7.45563454506349));
#53782=CARTESIAN_POINT('Ctrl Pts',(5.02510837566901,-1.06847604194513,7.42266819009693));
#53783=CARTESIAN_POINT('Ctrl Pts',(4.98579503979313,-0.794772684000851,
7.36476534440886));
#53784=CARTESIAN_POINT('Ctrl Pts',(4.9168307250082,-0.636309800095197,7.35572932930014));
#53785=CARTESIAN_POINT('Ctrl Pts',(4.84964913470353,-0.319434907277159,
7.32440610754237));
#53786=CARTESIAN_POINT('Ctrl Pts',(4.80463957303099,-0.158333333333332,
7.31964424706344));
#53787=CARTESIAN_POINT('Ctrl Pts',(4.80525449219255,0.158333333333334,7.286227929966));
#53788=CARTESIAN_POINT('Ctrl Pts',(4.85084550521323,0.319434907277167,7.25618276846203));
#53789=CARTESIAN_POINT('Ctrl Pts',(4.91934781310058,0.636309800095206,7.22227212406456));
#53790=CARTESIAN_POINT('Ctrl Pts',(4.98828259770888,0.794772684000842,7.19561838178182));
#53791=CARTESIAN_POINT('Ctrl Pts',(5.03020931801556,1.06847604194523,7.20725232196856));
#53792=CARTESIAN_POINT('Ctrl Pts',(5.03743514539826,1.18514270861202,7.22337830960505));
#53793=CARTESIAN_POINT('Ctrl Pts',(5.03373827648099,1.30000000000036,7.25059438325115));
#53794=CARTESIAN_POINT('Ctrl Pts',(5.00253629492169,-1.30000000000007,7.5071180066086));
#53795=CARTESIAN_POINT('Ctrl Pts',(5.0041000765162,-1.18514270861184,7.46957409453477));
#53796=CARTESIAN_POINT('Ctrl Pts',(4.99538754505344,-1.06847604194516,7.43886314014003));
#53797=CARTESIAN_POINT('Ctrl Pts',(4.95151951550678,-0.79477268400087,7.38370019095));
#53798=CARTESIAN_POINT('Ctrl Pts',(4.88312596255923,-0.636309800095213,
7.37241107226535));
#53799=CARTESIAN_POINT('Ctrl Pts',(4.81577396602792,-0.319434907277168,
7.34080030142118));
#53800=CARTESIAN_POINT('Ctrl Pts',(4.77223465376658,-0.158333333333336,
7.33576655937609));
#53801=CARTESIAN_POINT('Ctrl Pts',(4.77299491001348,0.158333333333338,7.30308535487117));
#53802=CARTESIAN_POINT('Ctrl Pts',(4.81731919591816,0.319434907277172,7.27447936700617));
#53803=CARTESIAN_POINT('Ctrl Pts',(4.8861694321273,0.63630980009522,7.2414733246328));
#53804=CARTESIAN_POINT('Ctrl Pts',(4.95451014435092,0.794772684000861,7.21617408048259));
#53805=CARTESIAN_POINT('Ctrl Pts',(5.00102041438665,1.06847604194526,7.22530225004274));
#53806=CARTESIAN_POINT('Ctrl Pts',(5.01132079453024,1.18514270861205,7.23943924357551));
#53807=CARTESIAN_POINT('Ctrl Pts',(5.01178898229432,1.30000000000039,7.26376198427049));
#53808=CARTESIAN_POINT('Ctrl Pts',(4.97960768346775,-1.30000000000009,7.5180473284774));
#53809=CARTESIAN_POINT('Ctrl Pts',(4.9766898729321,-1.18514270861186,7.48188505323422));
#53810=CARTESIAN_POINT('Ctrl Pts',(4.96471982623668,-1.06847604194517,7.45231951336133));
#53811=CARTESIAN_POINT('Ctrl Pts',(4.91615414734792,-0.794772684000884,
7.39925698006668));
#53812=CARTESIAN_POINT('Ctrl Pts',(4.84876618885557,-0.636309800095224,
7.3888440607498));
#53813=CARTESIAN_POINT('Ctrl Pts',(4.78135491398204,-0.319434907277172,
7.35780243811579));
#53814=CARTESIAN_POINT('Ctrl Pts',(4.73918890339539,-0.158333333333339,
7.35165944877986));
#53815=CARTESIAN_POINT('Ctrl Pts',(4.74005905500855,0.158333333333341,7.31954667302313));
#53816=CARTESIAN_POINT('Ctrl Pts',(4.78306310332938,0.31943490727718,7.29230286563965));
#53817=CARTESIAN_POINT('Ctrl Pts',(4.85231222804514,0.636309800095233,7.26052816522222));
#53818=CARTESIAN_POINT('Ctrl Pts',(4.92018013385201,0.794772684000875,7.23739729695367));
#53819=CARTESIAN_POINT('Ctrl Pts',(4.97138152451334,1.06847604194528,7.24408340050477));
#53820=CARTESIAN_POINT('Ctrl Pts',(4.98479812888538,1.18514270861207,7.25608266977393));
#53821=CARTESIAN_POINT('Ctrl Pts',(4.98946815281066,1.30000000000041,7.27718704182951));
#53822=CARTESIAN_POINT('Ctrl Pts',(4.96762951206948,-1.3000000000001,7.52369694152733));
#53823=CARTESIAN_POINT('Ctrl Pts',(4.96246471251451,-1.18514270861186,7.48912650638533));
#53824=CARTESIAN_POINT('Ctrl Pts',(4.94884267675674,-1.06847604194518,7.46065043105714));
#53825=CARTESIAN_POINT('Ctrl Pts',(4.8978351415846,-0.794772684000887,7.40894419077206));
#53826=CARTESIAN_POINT('Ctrl Pts',(4.83079936287769,-0.636309800095225,
7.39764041936882));
#53827=CARTESIAN_POINT('Ctrl Pts',(4.76327466385806,-0.319434907277173,
7.36628860048776));
#53828=CARTESIAN_POINT('Ctrl Pts',(4.72181854707695,-0.158333333333339,
7.35948896452109));
#53829=CARTESIAN_POINT('Ctrl Pts',(4.72275225828287,0.158333333333341,7.32771916071371));
#53830=CARTESIAN_POINT('Ctrl Pts',(4.76514949861775,0.319434907277181,7.30175698426488));
#53831=CARTESIAN_POINT('Ctrl Pts',(4.83456100171557,0.636309800095235,7.27041665039979));
#53832=CARTESIAN_POINT('Ctrl Pts',(4.90198920287092,0.794772684000876,7.2473480172949));
#53833=CARTESIAN_POINT('Ctrl Pts',(4.95564985032951,1.06847604194528,7.25275781317528));
#53834=CARTESIAN_POINT('Ctrl Pts',(4.9707419647311,1.18514270861207,7.26386848383299));
#53835=CARTESIAN_POINT('Ctrl Pts',(4.97769848757239,1.30000000000041,7.28374812496449));
#53836=CARTESIAN_POINT('Ctrl Pts',(4.96621805807752,-1.3000000000001,7.52434179038395));
#53837=CARTESIAN_POINT('Ctrl Pts',(4.96078772625744,-1.18514270861186,7.48995179094868));
#53838=CARTESIAN_POINT('Ctrl Pts',(4.94697072767715,-1.06847604194518,7.46160074156553));
#53839=CARTESIAN_POINT('Ctrl Pts',(4.89567581891261,-0.794772684000887,
7.41005532859067));
#53840=CARTESIAN_POINT('Ctrl Pts',(4.82868432317164,-0.636309800095225,
7.39866670011986));
#53841=CARTESIAN_POINT('Ctrl Pts',(4.76114622750612,-0.319434907277173,
7.36727937712788));
#53842=CARTESIAN_POINT('Ctrl Pts',(4.71977103742867,-0.158333333333339,
7.36038548847363));
#53843=CARTESIAN_POINT('Ctrl Pts',(4.7207120039862,0.158333333333341,7.32865541212252));
#53844=CARTESIAN_POINT('Ctrl Pts',(4.76303921752189,0.319434907277181,7.30285410419705));
#53845=CARTESIAN_POINT('Ctrl Pts',(4.83247147220263,0.636309800095235,7.2715754267178));
#53846=CARTESIAN_POINT('Ctrl Pts',(4.89984974091479,0.794772684000876,7.24852423454693));
#53847=CARTESIAN_POINT('Ctrl Pts',(4.95380019818296,1.06847604194528,7.25378609204053));
#53848=CARTESIAN_POINT('Ctrl Pts',(4.96908923651688,1.18514270861207,7.26479066039715));
#53849=CARTESIAN_POINT('Ctrl Pts',(4.97631415929477,1.30000000000041,7.28452213397244));
#53850=CARTESIAN_POINT('Ctrl Pts',(4.9637474723205,-1.3000000000001,7.52546764988381));
#53851=CARTESIAN_POINT('Ctrl Pts',(4.9578515887148,-1.18514270861186,7.49138561279624));
#53852=CARTESIAN_POINT('Ctrl Pts',(4.94369283991791,-1.06847604194518,7.46324840340755));
#53853=CARTESIAN_POINT('Ctrl Pts',(4.89189442617697,-0.794772684000887,
7.41197956213334));
#53854=CARTESIAN_POINT('Ctrl Pts',(4.82498061700849,-0.636309800095225,
7.40044630641422));
#53855=CARTESIAN_POINT('Ctrl Pts',(4.75742044765574,-0.319434907277173,
7.36900715748394));
#53856=CARTESIAN_POINT('Ctrl Pts',(4.71618974295627,-0.158333333333339,
7.36196748723083));
#53857=CARTESIAN_POINT('Ctrl Pts',(4.7171432438584,0.158333333333341,7.33030631010084));
#53858=CARTESIAN_POINT('Ctrl Pts',(4.75934399763486,0.319434907277181,7.30476100870489));
#53859=CARTESIAN_POINT('Ctrl Pts',(4.82881267223018,0.636309800095235,7.27359032242174));
#53860=CARTESIAN_POINT('Ctrl Pts',(4.89610772436469,0.794772684000877,7.25059534316193));
#53861=CARTESIAN_POINT('Ctrl Pts',(4.95056595954635,1.06847604194528,7.25560230833908));
#53862=CARTESIAN_POINT('Ctrl Pts',(4.96619919450976,1.18514270861207,7.26641881217423));
#53863=CARTESIAN_POINT('Ctrl Pts',(4.9738927123029,1.30000000000042,7.28588449014569));
#53864=CARTESIAN_POINT('Ctrl Pts',(4.95879774516821,-1.3000000000001,7.5276563571909));
#53865=CARTESIAN_POINT('Ctrl Pts',(4.95196211656313,-1.18514270861186,7.49412296198952));
#53866=CARTESIAN_POINT('Ctrl Pts',(4.93711477351148,-1.06847604194518,7.46637434836761));
#53867=CARTESIAN_POINT('Ctrl Pts',(4.88430577775183,-0.794772684000886,
7.41563350249997));
#53868=CARTESIAN_POINT('Ctrl Pts',(4.81755779821641,-0.636309800095225,
7.40389731948821));
#53869=CARTESIAN_POINT('Ctrl Pts',(4.74996087059343,-0.319434907277173,
7.37241417162736));
#53870=CARTESIAN_POINT('Ctrl Pts',(4.70902588150169,-0.158333333333339,
7.36513038159391));
#53871=CARTESIAN_POINT('Ctrl Pts',(4.71000378351542,0.158333333333341,7.3336081834644));
#53872=CARTESIAN_POINT('Ctrl Pts',(4.7519379321394,0.319434907277181,7.3084896567254));
#53873=CARTESIAN_POINT('Ctrl Pts',(4.82148347571844,0.636309800095234,7.27755709497504));
#53874=CARTESIAN_POINT('Ctrl Pts',(4.88863357496422,0.794772684000876,7.25480084860166));
#53875=CARTESIAN_POINT('Ctrl Pts',(4.94411080355287,1.06847604194528,7.25931676866177));
#53876=CARTESIAN_POINT('Ctrl Pts',(4.96043010760253,1.18514270861207,7.26974266752768));
#53877=CARTESIAN_POINT('Ctrl Pts',(4.96905467907973,1.30000000000041,7.28863969079682));
#53878=CARTESIAN_POINT('Ctrl Pts',(4.95170655585734,-1.30000000000009,7.53066301974529));
#53879=CARTESIAN_POINT('Ctrl Pts',(4.94349922945896,-1.18514270861186,7.49767213261703));
#53880=CARTESIAN_POINT('Ctrl Pts',(4.92765097558884,-1.06847604194517,7.47033625580933));
#53881=CARTESIAN_POINT('Ctrl Pts',(4.87338626769454,-0.794772684000885,
7.42024911698156));
#53882=CARTESIAN_POINT('Ctrl Pts',(4.80690758119547,-0.636309800095224,
7.408498441716));
#53883=CARTESIAN_POINT('Ctrl Pts',(4.73928911609014,-0.319434907277173,
7.37718751125002));
#53884=CARTESIAN_POINT('Ctrl Pts',(4.69881519121616,-0.158333333333339,
7.36981610804418));
#53885=CARTESIAN_POINT('Ctrl Pts',(4.69982263937953,0.158333333333341,7.33847081935012));
#53886=CARTESIAN_POINT('Ctrl Pts',(4.74130467688739,0.31943490727718,7.31350778961374));
#53887=CARTESIAN_POINT('Ctrl Pts',(4.81097388788422,0.636309800095233,7.28298543955834));
#53888=CARTESIAN_POINT('Ctrl Pts',(4.87801805469122,0.794772684000875,7.26117165117431));
#53889=CARTESIAN_POINT('Ctrl Pts',(4.93496342103356,1.06847604194528,7.26506331349464));
#53890=CARTESIAN_POINT('Ctrl Pts',(4.9522499344413,1.18514270861207,7.27485794428191));
#53891=CARTESIAN_POINT('Ctrl Pts',(4.96217342220097,1.30000000000041,7.29276264943828));
#53892=CARTESIAN_POINT('Ctrl Pts',(4.94318957929729,-1.30000000000009,7.53423305499234));
#53893=CARTESIAN_POINT('Ctrl Pts',(4.93332953624159,-1.18514270861186,7.50185198254238));
#53894=CARTESIAN_POINT('Ctrl Pts',(4.91627433805312,-1.06847604194517,7.47497318322297));
#53895=CARTESIAN_POINT('Ctrl Pts',(4.8602511706145,-0.794772684000885,7.42558913136725));
#53896=CARTESIAN_POINT('Ctrl Pts',(4.79408885098585,-0.636309800095225,
7.41376001035497));
#53897=CARTESIAN_POINT('Ctrl Pts',(4.72644038716081,-0.319434907277173,
7.38262462152606));
#53898=CARTESIAN_POINT('Ctrl Pts',(4.68652131684815,-0.158333333333339,
7.37515634458014));
#53899=CARTESIAN_POINT('Ctrl Pts',(4.68756990475403,0.158333333333341,7.34408617678325));
#53900=CARTESIAN_POINT('Ctrl Pts',(4.72852508143549,0.319434907277181,7.31945437181908));
#53901=CARTESIAN_POINT('Ctrl Pts',(4.79833486731633,0.636309800095234,7.28939992686437));
#53902=CARTESIAN_POINT('Ctrl Pts',(4.86521212340213,0.794772684000876,7.2684628347598));
#53903=CARTESIAN_POINT('Ctrl Pts',(4.92392569863787,1.06847604194528,7.27163090554263));
#53904=CARTESIAN_POINT('Ctrl Pts',(4.94238557203983,1.18514270861207,7.28073645836866));
#53905=CARTESIAN_POINT('Ctrl Pts',(4.95389038767657,1.30000000000041,7.29757622356745));
#53906=CARTESIAN_POINT('Ctrl Pts',(4.92622393725722,-1.30000000000009,7.54194881348275));
#53907=CARTESIAN_POINT('Ctrl Pts',(4.91314484487837,-1.18514270861185,7.51153479287278));
#53908=CARTESIAN_POINT('Ctrl Pts',(4.89372426348806,-1.06847604194517,7.48599119980892));
#53909=CARTESIAN_POINT('Ctrl Pts',(4.8342087271754,-0.794772684000883,7.43823205181034));
#53910=CARTESIAN_POINT('Ctrl Pts',(4.76857066695711,-0.636309800095222,
7.42528661629812));
#53911=CARTESIAN_POINT('Ctrl Pts',(4.70074680043619,-0.319434907277171,
7.39357266963));
#53912=CARTESIAN_POINT('Ctrl Pts',(4.66180971695086,-0.158333333333338,
7.38496016242235));
#53913=CARTESIAN_POINT('Ctrl Pts',(4.66292672045037,0.15833333333334,7.35430893144978));
#53914=CARTESIAN_POINT('Ctrl Pts',(4.70298799249483,0.319434907277179,7.33144843630135));
#53915=CARTESIAN_POINT('Ctrl Pts',(4.77307247926823,0.636309800095231,7.30240192157892));
#53916=CARTESIAN_POINT('Ctrl Pts',(4.83944016939201,0.794772684000872,7.28225470268924));
#53917=CARTESIAN_POINT('Ctrl Pts',(4.90168661026715,1.06847604194527,7.2839604412694));
#53918=CARTESIAN_POINT('Ctrl Pts',(4.92252564715923,1.18514270861206,7.29185791074353));
#53919=CARTESIAN_POINT('Ctrl Pts',(4.93725954314648,1.30000000000041,7.30691449866427));
#53920=CARTESIAN_POINT('Ctrl Pts',(4.90065660867547,-1.30000000000008,7.55262755751749));
#53921=CARTESIAN_POINT('Ctrl Pts',(4.88263466293015,-1.18514270861185,7.52418493048915));
#53922=CARTESIAN_POINT('Ctrl Pts',(4.85959630730382,-1.06847604194516,7.50006003157311));
#53923=CARTESIAN_POINT('Ctrl Pts',(4.79478418664526,-0.794772684000876,
7.45430150460558));
#53924=CARTESIAN_POINT('Ctrl Pts',(4.7300403503272,-0.636309800095217,7.44075615110194));
#53925=CARTESIAN_POINT('Ctrl Pts',(4.66206323450965,-0.319434907277169,
7.40908706908356));
#53926=CARTESIAN_POINT('Ctrl Pts',(4.62471215024605,-0.158333333333337,
7.39950084206595));
#53927=CARTESIAN_POINT('Ctrl Pts',(4.62599014559949,0.158333333333339,7.36997551533005));
#53928=CARTESIAN_POINT('Ctrl Pts',(4.66470153449349,0.319434907277176,7.34982371775994));
#53929=CARTESIAN_POINT('Ctrl Pts',(4.73511417675659,0.636309800095225,7.32178508532075));
#53930=CARTESIAN_POINT('Ctrl Pts',(4.80053155068804,0.794772684000865,7.30156262702942));
#53931=CARTESIAN_POINT('Ctrl Pts',(4.86806019542745,1.06847604194527,7.30088393315434));
#53932=CARTESIAN_POINT('Ctrl Pts',(4.89250121694453,1.18514270861206,7.30713907296468));
#53933=CARTESIAN_POINT('Ctrl Pts',(4.91215261185388,1.30000000000041,7.31994313401581));
#53934=CARTESIAN_POINT('Ctrl Pts',(4.86653286362622,-1.30000000000007,7.56699602339097));
#53935=CARTESIAN_POINT('Ctrl Pts',(4.84193012512882,-1.18514270861184,7.54156815072991));
#53936=CARTESIAN_POINT('Ctrl Pts',(4.81406891318095,-1.06847604194516,7.51951951330367));
#53937=CARTESIAN_POINT('Ctrl Pts',(4.74217621443908,-0.794772684000874,
7.47638945944037));
#53938=CARTESIAN_POINT('Ctrl Pts',(4.67856929883686,-0.63630980009521,7.46107138749974));
#53939=CARTESIAN_POINT('Ctrl Pts',(4.61036610444347,-0.319434907277163,
7.42924713609238));
#53940=CARTESIAN_POINT('Ctrl Pts',(4.57522062589997,-0.158333333333335,
7.41932126812144));
#53941=CARTESIAN_POINT('Ctrl Pts',(4.57656999719294,0.158333333333337,7.39040121976789));
#53942=CARTESIAN_POINT('Ctrl Pts',(4.61308700479027,0.319434907277172,7.37101508989296));
#53943=CARTESIAN_POINT('Ctrl Pts',(4.68399363758603,0.636309800095217,7.34472965801132));
#53944=CARTESIAN_POINT('Ctrl Pts',(4.74868416146106,0.794772684000855,7.32832235074326));
#53945=CARTESIAN_POINT('Ctrl Pts',(4.82339340706111,1.06847604194525,7.32530219441606));
#53946=CARTESIAN_POINT('Ctrl Pts',(4.85261650093078,1.18514270861204,7.32911395995992));
#53947=CARTESIAN_POINT('Ctrl Pts',(4.87872382450021,1.30000000000039,7.33804480481385));
#53948=CARTESIAN_POINT('Ctrl Pts',(4.8322831212685,-1.30000000000007,7.58030962560515));
#53949=CARTESIAN_POINT('Ctrl Pts',(4.80099763659862,-1.18514270861183,7.556825992742));
#53950=CARTESIAN_POINT('Ctrl Pts',(4.76824497763037,-1.06847604194515,7.53617635724849));
#53951=CARTESIAN_POINT('Ctrl Pts',(4.68919031713033,-0.794772684000866,
7.49501866917608));
#53952=CARTESIAN_POINT('Ctrl Pts',(4.62681181703605,-0.636309800095206,
7.4792780833236));
#53953=CARTESIAN_POINT('Ctrl Pts',(4.55835898630226,-0.319434907277162,
7.44716273305618));
#53954=CARTESIAN_POINT('Ctrl Pts',(4.52530841472525,-0.158333333333334,
7.4354970781266));
#53955=CARTESIAN_POINT('Ctrl Pts',(4.52677534967624,0.158333333333336,7.40763889322388));
#53956=CARTESIAN_POINT('Ctrl Pts',(4.56133568964948,0.319434907277171,7.39136145828312));
#53957=CARTESIAN_POINT('Ctrl Pts',(4.63268931261174,0.636309800095214,7.36690463706524));
#53958=CARTESIAN_POINT('Ctrl Pts',(4.69626304790192,0.794772684000848,7.35165672911438));
#53959=CARTESIAN_POINT('Ctrl Pts',(4.77817412582395,1.06847604194525,7.34637870177531));
#53960=CARTESIAN_POINT('Ctrl Pts',(4.81227352272635,1.18514270861204,7.34830992636712));
#53961=CARTESIAN_POINT('Ctrl Pts',(4.84501604600325,1.30000000000038,7.35445703801565));
#53962=CARTESIAN_POINT('Ctrl Pts',(4.80369703210636,-1.30000000000006,7.59113993557896));
#53963=CARTESIAN_POINT('Ctrl Pts',(4.76686780308405,-1.18514270861182,7.56989617465925));
#53964=CARTESIAN_POINT('Ctrl Pts',(4.73004535157928,-1.06847604194514,7.55067186892));
#53965=CARTESIAN_POINT('Ctrl Pts',(4.64499377971837,-0.79477268400086,7.51092522231064));
#53966=CARTESIAN_POINT('Ctrl Pts',(4.58352304285331,-0.636309800095202,
7.4929261169799));
#53967=CARTESIAN_POINT('Ctrl Pts',(4.51483597746967,-0.31943490727716,7.46015120183153));
#53968=CARTESIAN_POINT('Ctrl Pts',(4.48360461045807,-0.158333333333334,
7.44800193996648));
#53969=CARTESIAN_POINT('Ctrl Pts',(4.48516732851818,0.158333333333336,7.42127916339769));
#53970=CARTESIAN_POINT('Ctrl Pts',(4.51800961074064,0.319434907277173,7.40706991303503));
#53971=CARTESIAN_POINT('Ctrl Pts',(4.58978164616749,0.636309800095214,7.38467047618168));
#53972=CARTESIAN_POINT('Ctrl Pts',(4.65258624879034,0.794772684000844,7.37171976821259));
#53973=CARTESIAN_POINT('Ctrl Pts',(4.74054992968274,1.06847604194524,7.36491717020787));
#53974=CARTESIAN_POINT('Ctrl Pts',(4.77871036700213,1.18514270861203,7.3652032319829));
#53975=CARTESIAN_POINT('Ctrl Pts',(4.81695502355821,1.30000000000037,7.36871994814812));
#53976=CARTESIAN_POINT('Ctrl Pts',(4.78072070206189,-1.30000000000005,7.59826996426713));
#53977=CARTESIAN_POINT('Ctrl Pts',(4.73939596944773,-1.18514270861182,7.57810409291054));
#53978=CARTESIAN_POINT('Ctrl Pts',(4.69928638575355,-1.06847604194514,7.55968520884557));
#53979=CARTESIAN_POINT('Ctrl Pts',(4.60943246062009,-0.794772684000857,
7.52116979209764));
#53980=CARTESIAN_POINT('Ctrl Pts',(4.54882050012122,-0.6363098000952,7.50324893132566));
#53981=CARTESIAN_POINT('Ctrl Pts',(4.47997038535647,-0.319434907277159,
7.47030730395309));
#53982=CARTESIAN_POINT('Ctrl Pts',(4.45015536348438,-0.158333333333333,
7.45697243813239));
#53983=CARTESIAN_POINT('Ctrl Pts',(4.45172513689568,0.158333333333335,7.4305333745949));
#53984=CARTESIAN_POINT('Ctrl Pts',(4.48311660067188,0.319434907277171,7.41751656523236));
#53985=CARTESIAN_POINT('Ctrl Pts',(4.55515064760831,0.636309800095212,7.39642572006936));
#53986=CARTESIAN_POINT('Ctrl Pts',(4.6172815010005,0.794772684000843,7.38520208752937));
#53987=CARTESIAN_POINT('Ctrl Pts',(4.71013514431173,1.06847604194524,7.37760971985347));
#53988=CARTESIAN_POINT('Ctrl Pts',(4.75159422184822,1.18514270861203,7.3769152536041));
#53989=CARTESIAN_POINT('Ctrl Pts',(4.79431947529833,1.30000000000037,7.37881277574731));
#53990=CARTESIAN_POINT('Ctrl Pts',(4.76786499505706,-1.30000000000005,7.60368176740185));
#53991=CARTESIAN_POINT('Ctrl Pts',(4.72403017506114,-1.18514270861182,7.58434250585805));
#53992=CARTESIAN_POINT('Ctrl Pts',(4.68207593127194,-1.06847604194514,7.56639781277273));
#53993=CARTESIAN_POINT('Ctrl Pts',(4.58949774244669,-0.794772684000855,
7.52816371404363));
#53994=CARTESIAN_POINT('Ctrl Pts',(4.52928725147374,-0.636309800095199,
7.50909410570766));
#53995=CARTESIAN_POINT('Ctrl Pts',(4.46031010843157,-0.319434907277159,
7.47547069309426));
#53996=CARTESIAN_POINT('Ctrl Pts',(4.43129639052106,-0.158333333333333,
7.46149895232343));
#53997=CARTESIAN_POINT('Ctrl Pts',(4.43290065961814,0.158333333333335,7.43554361832388));
#53998=CARTESIAN_POINT('Ctrl Pts',(4.46353033253678,0.31943490727717,7.42390395304713));
#53999=CARTESIAN_POINT('Ctrl Pts',(4.5357514528591,0.63630980009521,7.40395766267498));
#54000=CARTESIAN_POINT('Ctrl Pts',(4.59753036765001,0.794772684000841,7.39381410651702));
#54001=CARTESIAN_POINT('Ctrl Pts',(4.69310019596524,1.06847604194524,7.38543317330055));
#54002=CARTESIAN_POINT('Ctrl Pts',(4.73638310392889,1.18514270861202,7.3839008144956));
#54003=CARTESIAN_POINT('Ctrl Pts',(4.78158028238967,1.30000000000037,7.38446389233092));
#54004=CARTESIAN_POINT('Ctrl Pts',(4.75923927618336,-1.30000000000005,7.60624853723847));
#54005=CARTESIAN_POINT('Ctrl Pts',(4.71371888822517,-1.18514270861182,7.58733968665901));
#54006=CARTESIAN_POINT('Ctrl Pts',(4.67053009679902,-1.06847604194514,7.56968470619033));
#54007=CARTESIAN_POINT('Ctrl Pts',(4.5761418031398,-0.794772684000856,7.53179486023267));
#54008=CARTESIAN_POINT('Ctrl Pts',(4.51623070437183,-0.636309800095199,
7.51239178373076));
#54009=CARTESIAN_POINT('Ctrl Pts',(4.44719492422517,-0.319434907277159,
7.47876712691051));
#54010=CARTESIAN_POINT('Ctrl Pts',(4.41874093581131,-0.158333333333333,
7.46481603696944));
#54011=CARTESIAN_POINT('Ctrl Pts',(4.42035217695484,0.158333333333335,7.43907172064773));
#54012=CARTESIAN_POINT('Ctrl Pts',(4.45042291996238,0.31943490727717,7.42764711885315));
#54013=CARTESIAN_POINT('Ctrl Pts',(4.52272945180426,0.63630980009521,7.40808159523841));
#54014=CARTESIAN_POINT('Ctrl Pts',(4.58422871234628,0.794772684000842,7.39842119779554));
#54015=CARTESIAN_POINT('Ctrl Pts',(4.68165701495636,1.06847604194524,7.38997292819499));
#54016=CARTESIAN_POINT('Ctrl Pts',(4.72619958205877,1.18514270861203,7.38826513261078));
#54017=CARTESIAN_POINT('Ctrl Pts',(4.77311161413808,1.30000000000037,7.38850648431319));
#54018=CARTESIAN_POINT('Ctrl Pts',(4.75348070600748,-1.30000000000005,7.60784584718064));
#54019=CARTESIAN_POINT('Ctrl Pts',(4.70683011197265,-1.18514270861182,7.58912773525085));
#54020=CARTESIAN_POINT('Ctrl Pts',(4.66281435287995,-1.06847604194514,7.5716076021723));
#54021=CARTESIAN_POINT('Ctrl Pts',(4.56721613986662,-0.794772684000856,
7.53390016067141));
#54022=CARTESIAN_POINT('Ctrl Pts',(4.50751187293003,-0.636309800095199,
7.51438143784491));
#54023=CARTESIAN_POINT('Ctrl Pts',(4.43844157285354,-0.319434907277159,
7.48082496512931));
#54024=CARTESIAN_POINT('Ctrl Pts',(4.41036344576932,-0.158333333333333,
7.46692564018267));
#54025=CARTESIAN_POINT('Ctrl Pts',(4.41198144907926,0.158333333333335,7.441363506674));
#54026=CARTESIAN_POINT('Ctrl Pts',(4.44167897603494,0.31943490727717,7.43008701444388));
#54027=CARTESIAN_POINT('Ctrl Pts',(4.51404218765837,0.63630980009521,7.41078836318461));
#54028=CARTESIAN_POINT('Ctrl Pts',(4.57535476318257,0.794772684000841,7.40145625908929));
#54029=CARTESIAN_POINT('Ctrl Pts',(4.67402065827908,1.06847604194524,7.39295150913252));
#54030=CARTESIAN_POINT('Ctrl Pts',(4.71940216420826,1.18514270861202,7.39111669715767));
#54031=CARTESIAN_POINT('Ctrl Pts',(4.76745636601108,1.30000000000037,7.39112846433221));
#54032=CARTESIAN_POINT('Ctrl Pts',(4.74343057879297,-1.30000000000005,7.61127081391063));
#54033=CARTESIAN_POINT('Ctrl Pts',(4.69479529387935,-1.18514270861182,7.59271990632606));
#54034=CARTESIAN_POINT('Ctrl Pts',(4.64932744556142,-1.06847604194514,7.57531939333081));
#54035=CARTESIAN_POINT('Ctrl Pts',(4.55160503231467,-0.794772684000857,
7.53777836898805));
#54036=CARTESIAN_POINT('Ctrl Pts',(4.49227113018039,-0.6363098000952,7.51826466037316));
#54037=CARTESIAN_POINT('Ctrl Pts',(4.42312822731368,-0.319434907277159,
7.48458776204415));
#54038=CARTESIAN_POINT('Ctrl Pts',(4.39568514603662,-0.158333333333333,
7.47029425012699));
#54039=CARTESIAN_POINT('Ctrl Pts',(4.39730494690124,0.158333333333335,7.4448710587498));
#54040=CARTESIAN_POINT('Ctrl Pts',(4.42635287440999,0.31943490727717,7.4340199568158));
#54041=CARTESIAN_POINT('Ctrl Pts',(4.4988256565189,0.63630980009521,7.41534420247766));
#54042=CARTESIAN_POINT('Ctrl Pts',(4.55984006195317,0.794772684000842,7.40686093806267));
#54043=CARTESIAN_POINT('Ctrl Pts',(4.66066222458958,1.06847604194524,7.39819903766625));
#54044=CARTESIAN_POINT('Ctrl Pts',(4.70749909041594,1.18514270861203,7.39603518760888));
#54045=CARTESIAN_POINT('Ctrl Pts',(4.75753064369264,1.30000000000037,7.39545690322072));
#54046=CARTESIAN_POINT('Ctrl Pts',(4.72909269571893,-1.30000000000005,7.61656804117484));
#54047=CARTESIAN_POINT('Ctrl Pts',(4.67765262468082,-1.18514270861182,7.59884377256573));
#54048=CARTESIAN_POINT('Ctrl Pts',(4.63012539389608,-1.06847604194514,7.5818984556327));
#54049=CARTESIAN_POINT('Ctrl Pts',(4.52936742673965,-0.794772684000858,
7.54455091781885));
#54050=CARTESIAN_POINT('Ctrl Pts',(4.47049638455632,-0.6363098000952,7.52370599516994));
#54051=CARTESIAN_POINT('Ctrl Pts',(4.40122132489785,-0.319434907277159,
7.48931759022313));
#54052=CARTESIAN_POINT('Ctrl Pts',(4.37468286868284,-0.158333333333333,
7.47450898079698));
#54053=CARTESIAN_POINT('Ctrl Pts',(4.37632493538259,0.158333333333335,7.44964337104086));
#54054=CARTESIAN_POINT('Ctrl Pts',(4.40447438467914,0.31943490727717,7.44002129711005));
#54055=CARTESIAN_POINT('Ctrl Pts',(4.47715751069514,0.63630980009521,7.42287433160762));
#54056=CARTESIAN_POINT('Ctrl Pts',(4.53783231460736,0.794772684000843,7.41626767988291));
#54057=CARTESIAN_POINT('Ctrl Pts',(4.64170473749484,1.06847604194524,7.40702856231035));
#54058=CARTESIAN_POINT('Ctrl Pts',(4.69057892767158,1.18514270861202,7.40397220206445));
#54059=CARTESIAN_POINT('Ctrl Pts',(4.74336478500964,1.30000000000037,7.40185875322678));
#54060=CARTESIAN_POINT('Ctrl Pts',(4.71179724858884,-1.30000000000005,7.62108876395165));
#54061=CARTESIAN_POINT('Ctrl Pts',(4.65696649830876,-1.18514270861182,7.60388388473665));
#54062=CARTESIAN_POINT('Ctrl Pts',(4.60695810500404,-1.06847604194514,7.58727783427176));
#54063=CARTESIAN_POINT('Ctrl Pts',(4.5025693216476,-0.794772684000857,7.55029794987688));
#54064=CARTESIAN_POINT('Ctrl Pts',(4.44432282135363,-0.6363098000952,7.52893227478901));
#54065=CARTESIAN_POINT('Ctrl Pts',(4.37493188734826,-0.31943490727716,7.4945638321171));
#54066=CARTESIAN_POINT('Ctrl Pts',(4.34949958004939,-0.158333333333333,
7.47981019719062));
#54067=CARTESIAN_POINT('Ctrl Pts',(4.3511508890067,0.158333333333335,7.45549244158879));
#54068=CARTESIAN_POINT('Ctrl Pts',(4.3782011752311,0.319434907277169,7.44657555188257));
#54069=CARTESIAN_POINT('Ctrl Pts',(4.45102359755922,0.63630980009521,7.43009211444813));
#54070=CARTESIAN_POINT('Ctrl Pts',(4.51106842473165,0.794772684000843,7.42392158711869));
#54071=CARTESIAN_POINT('Ctrl Pts',(4.6186361277069,1.06847604194524,7.41448353620949));
#54072=CARTESIAN_POINT('Ctrl Pts',(4.67003232286398,1.18514270861203,7.41114697329846));
#54073=CARTESIAN_POINT('Ctrl Pts',(4.72626264033635,1.30000000000037,7.40855923000074));
#54074=CARTESIAN_POINT('Ctrl Pts',(4.68590468587279,-1.30000000000005,7.62938620214826));
#54075=CARTESIAN_POINT('Ctrl Pts',(4.62599255528755,-1.18514270861182,7.61324620206889));
#54076=CARTESIAN_POINT('Ctrl Pts',(4.57225708453609,-1.06847604194514,7.59720278860638));
#54077=CARTESIAN_POINT('Ctrl Pts',(4.46238671720871,-0.79477268400086,7.56036242844115));
#54078=CARTESIAN_POINT('Ctrl Pts',(4.40501323857521,-0.636309800095201,
7.53737430405052));
#54079=CARTESIAN_POINT('Ctrl Pts',(4.33539413439024,-0.31943490727716,7.50142300748779));
#54080=CARTESIAN_POINT('Ctrl Pts',(4.31159708863585,-0.158333333333333,
7.48469201207812));
#54081=CARTESIAN_POINT('Ctrl Pts',(4.31325645221777,0.158333333333335,7.46109374815198));
#54082=CARTESIAN_POINT('Ctrl Pts',(4.33865773735432,0.319434907277168,7.45508785741748));
#54083=CARTESIAN_POINT('Ctrl Pts',(4.41176912970336,0.636309800095209,7.44121662497348));
#54084=CARTESIAN_POINT('Ctrl Pts',(4.47102658985925,0.794772684000846,7.43704322311659));
#54085=CARTESIAN_POINT('Ctrl Pts',(4.58415795221862,1.06847604194524,7.42743491767402));
#54086=CARTESIAN_POINT('Ctrl Pts',(4.63931218712884,1.18514270861202,7.42334114155557));
#54087=CARTESIAN_POINT('Ctrl Pts',(4.70065028211401,1.30000000000036,7.41931266872195));
#54088=CARTESIAN_POINT('Ctrl Pts',(4.65997285225604,-1.30000000000004,7.63611399060629));
#54089=CARTESIAN_POINT('Ctrl Pts',(4.59502018717183,-1.18514270861181,7.62090823517882));
#54090=CARTESIAN_POINT('Ctrl Pts',(4.5375965812993,-1.06847604194514,7.60524155890487));
#54091=CARTESIAN_POINT('Ctrl Pts',(4.42233019714286,-0.794772684000858,
7.56798358324191));
#54092=CARTESIAN_POINT('Ctrl Pts',(4.36590065335152,-0.636309800095198,
7.54205387854712));
#54093=CARTESIAN_POINT('Ctrl Pts',(4.29608547850594,-0.319434907277158,
7.50531053618865));
#54094=CARTESIAN_POINT('Ctrl Pts',(4.27389244970255,-0.158333333333333,
7.48940950321921));
#54095=CARTESIAN_POINT('Ctrl Pts',(4.27552401124187,0.158333333333334,7.46700810106707));
#54096=CARTESIAN_POINT('Ctrl Pts',(4.29923520182961,0.319434907277168,7.46181003652398));
#54097=CARTESIAN_POINT('Ctrl Pts',(4.37260473719026,0.636309800095207,7.45027063487121));
#54098=CARTESIAN_POINT('Ctrl Pts',(4.43110737170687,0.794772684000841,7.44930808338118));
#54099=CARTESIAN_POINT('Ctrl Pts',(4.54974418748316,1.06847604194523,7.43989901659481));
#54100=CARTESIAN_POINT('Ctrl Pts',(4.60861517528759,1.18514270861202,7.43508138351226));
#54101=CARTESIAN_POINT('Ctrl Pts',(4.67500366927415,1.30000000000036,7.42951895371868));
#54102=CARTESIAN_POINT('Ctrl Pts',(4.63687848316797,-1.30000000000004,7.64278362359798));
#54103=CARTESIAN_POINT('Ctrl Pts',(4.56734946810552,-1.18514270861181,7.6277193111944));
#54104=CARTESIAN_POINT('Ctrl Pts',(4.50657400117256,-1.06847604194514,7.61194573999381));
#54105=CARTESIAN_POINT('Ctrl Pts',(4.38639296178727,-0.794772684000858,
7.57386710532048));
#54106=CARTESIAN_POINT('Ctrl Pts',(4.33078037996717,-0.636309800095198,
7.54632081086968));
#54107=CARTESIAN_POINT('Ctrl Pts',(4.26079711972564,-0.319434907277158,
7.5084122504634));
#54108=CARTESIAN_POINT('Ctrl Pts',(4.2401246124826,-0.158333333333332,7.49191187221995));
#54109=CARTESIAN_POINT('Ctrl Pts',(4.24173169812143,0.158333333333334,7.47008700208653));
#54110=CARTESIAN_POINT('Ctrl Pts',(4.26387907057827,0.319434907277167,7.4663085322291));
#54111=CARTESIAN_POINT('Ctrl Pts',(4.3374051720377,0.636309800095206,7.4566122680534));
#54112=CARTESIAN_POINT('Ctrl Pts',(4.39510148966059,0.79477268400084,7.45739853999331));
#54113=CARTESIAN_POINT('Ctrl Pts',(4.51872055606065,1.06847604194523,7.44840780746785));
#54114=CARTESIAN_POINT('Ctrl Pts',(4.58098662417127,1.18514270861202,7.44334161528439));
#54115=CARTESIAN_POINT('Ctrl Pts',(4.65200864708575,1.30000000000036,7.43710098588828));
#54116=CARTESIAN_POINT('Ctrl Pts',(4.62245430981321,-1.30000000000005,7.64588206265252));
#54117=CARTESIAN_POINT('Ctrl Pts',(4.55013160928749,-1.18514270861182,7.63120092471038));
#54118=CARTESIAN_POINT('Ctrl Pts',(4.48731630235014,-1.06847604194514,7.61551111620122));
#54119=CARTESIAN_POINT('Ctrl Pts',(4.36416435830239,-0.794772684000858,
7.57693428901595));
#54120=CARTESIAN_POINT('Ctrl Pts',(4.30911474602555,-0.636309800095199,
7.54764413863052));
#54121=CARTESIAN_POINT('Ctrl Pts',(4.23903212360004,-0.319434907277158,
7.50902218476997));
#54122=CARTESIAN_POINT('Ctrl Pts',(4.21922995277278,-0.158333333333333,
7.49271556413392));
#54123=CARTESIAN_POINT('Ctrl Pts',(4.22079997598892,0.158333333333335,7.47152050406351));
#54124=CARTESIAN_POINT('Ctrl Pts',(4.24199652951127,0.319434907277168,7.46836398924111));
#54125=CARTESIAN_POINT('Ctrl Pts',(4.31563494327749,0.636309800095207,7.4602853261014));
#54126=CARTESIAN_POINT('Ctrl Pts',(4.37286400473976,0.794772684000841,7.4629571255785));
#54127=CARTESIAN_POINT('Ctrl Pts',(4.49955541502258,1.06847604194524,7.45478068246077));
#54128=CARTESIAN_POINT('Ctrl Pts',(4.56390770899303,1.18514270861202,7.44972028485976));
#54129=CARTESIAN_POINT('Ctrl Pts',(4.6377722798019,1.30000000000036,7.44313876891631));
#54130=CARTESIAN_POINT('Ctrl Pts',(4.60795019531385,-1.30000000000005,7.6493488567498));
#54131=CARTESIAN_POINT('Ctrl Pts',(4.53267139934727,-1.18514270861182,7.63479518093068));
#54132=CARTESIAN_POINT('Ctrl Pts',(4.46769163127909,-1.06847604194514,7.6189806971343));
#54133=CARTESIAN_POINT('Ctrl Pts',(4.34136818264232,-0.794772684000858,
7.57953335723679));
#54134=CARTESIAN_POINT('Ctrl Pts',(4.28685816211639,-0.636309800095199,
7.54783991273211));
#54135=CARTESIAN_POINT('Ctrl Pts',(4.21665741811185,-0.319434907277158,
7.50944861440254));
#54136=CARTESIAN_POINT('Ctrl Pts',(4.19781321920072,-0.158333333333333,
7.49584497305017));
#54137=CARTESIAN_POINT('Ctrl Pts',(4.19935364590263,0.158333333333335,7.47552237467756));
#54138=CARTESIAN_POINT('Ctrl Pts',(4.219536137998,0.319434907277168,7.47106293288307));
#54139=CARTESIAN_POINT('Ctrl Pts',(4.29328635170139,0.636309800095207,7.46345609177895));
#54140=CARTESIAN_POINT('Ctrl Pts',(4.35002376194345,0.79477268400084,7.4678362313814));
#54141=CARTESIAN_POINT('Ctrl Pts',(4.47994147943138,1.06847604194523,7.4600160329351));
#54142=CARTESIAN_POINT('Ctrl Pts',(4.54648534280962,1.18514270861202,7.45480994003203));
#54143=CARTESIAN_POINT('Ctrl Pts',(4.62333650359142,1.30000000000037,7.4477828283664));
#54144=CARTESIAN_POINT('Ctrl Pts',(4.59357906309859,-1.30000000000004,7.65261768781226));
#54145=CARTESIAN_POINT('Ctrl Pts',(4.515613582606,-1.18514270861181,7.63746571967198));
#54146=CARTESIAN_POINT('Ctrl Pts',(4.44867658010229,-1.06847604194513,7.62139812597335));
#54147=CARTESIAN_POINT('Ctrl Pts',(4.31951670401105,-0.794772684000855,
7.58216349200832));
#54148=CARTESIAN_POINT('Ctrl Pts',(4.26556225269653,-0.636309800095198,
7.55207793454907));
#54149=CARTESIAN_POINT('Ctrl Pts',(4.19532952755911,-0.319434907277159,
7.51449404889587));
#54150=CARTESIAN_POINT('Ctrl Pts',(4.17741300812966,-0.158333333333333,
7.50113035871167));
#54151=CARTESIAN_POINT('Ctrl Pts',(4.17893351407558,0.158333333333335,7.48022729652089));
#54152=CARTESIAN_POINT('Ctrl Pts',(4.19815674351198,0.319434907277168,7.47404087090977));
#54153=CARTESIAN_POINT('Ctrl Pts',(4.27192211671505,0.636309800095207,7.46629086955863));
#54154=CARTESIAN_POINT('Ctrl Pts',(4.32809954591735,0.794772684000841,7.47235465402125));
#54155=CARTESIAN_POINT('Ctrl Pts',(4.46089760304215,1.06847604194523,7.46486667057211));
#54156=CARTESIAN_POINT('Ctrl Pts',(4.52942990010045,1.18514270861202,7.45956477448967));
#54157=CARTESIAN_POINT('Ctrl Pts',(4.60901113594068,1.30000000000036,7.45220225290278));
#54158=CARTESIAN_POINT('Ctrl Pts',(4.57617941896526,-1.30000000000004,7.65590048748505));
#54159=CARTESIAN_POINT('Ctrl Pts',(4.49458263105147,-1.18514270861181,7.6399348939217));
#54160=CARTESIAN_POINT('Ctrl Pts',(4.4249715844402,-1.06847604194513,7.62369292737989));
#54161=CARTESIAN_POINT('Ctrl Pts',(4.29184560127414,-0.794772684000854,
7.58553225860559));
#54162=CARTESIAN_POINT('Ctrl Pts',(4.23841576762044,-0.636309800095198,
7.55884844446226));
#54163=CARTESIAN_POINT('Ctrl Pts',(4.1679993993941,-0.319434907277159,7.52344207579474));
#54164=CARTESIAN_POINT('Ctrl Pts',(4.15134356171619,-0.158333333333332,
7.5105034367935));
#54165=CARTESIAN_POINT('Ctrl Pts',(4.15284239670344,0.158333333333334,7.48968966703876));
#54166=CARTESIAN_POINT('Ctrl Pts',(4.17076731329137,0.319434907277167,7.48282865376814));
#54167=CARTESIAN_POINT('Ctrl Pts',(4.24470469705338,0.636309800095206,7.47377318779266));
#54168=CARTESIAN_POINT('Ctrl Pts',(4.30036736809567,0.79477268400084,7.47832213150233));
#54169=CARTESIAN_POINT('Ctrl Pts',(4.43718403996299,1.06847604194523,7.46992576188581));
#54170=CARTESIAN_POINT('Ctrl Pts',(4.50842391007758,1.18514270861202,7.46445378067426));
#54171=CARTESIAN_POINT('Ctrl Pts',(4.59168078261271,1.30000000000037,7.457144295542));
#54172=CARTESIAN_POINT('Ctrl Pts',(4.56433455848947,-1.30000000000004,7.65821867228285));
#54173=CARTESIAN_POINT('Ctrl Pts',(4.48025898197814,-1.18514270861181,7.64034602806837));
#54174=CARTESIAN_POINT('Ctrl Pts',(4.40891552700136,-1.06847604194513,7.62347431552138));
#54175=CARTESIAN_POINT('Ctrl Pts',(4.27351162159271,-0.794772684000851,
7.58680963675092));
#54176=CARTESIAN_POINT('Ctrl Pts',(4.22112140679108,-0.636309800095197,
7.56664485618359));
#54177=CARTESIAN_POINT('Ctrl Pts',(4.15113790298686,-0.319434907277159,
7.53468752939888));
#54178=CARTESIAN_POINT('Ctrl Pts',(4.13553292461561,-0.158333333333332,
7.52147411752544));
#54179=CARTESIAN_POINT('Ctrl Pts',(4.13706908989959,0.158333333333334,7.50081062858686));
#54180=CARTESIAN_POINT('Ctrl Pts',(4.15404363487222,0.319434907277167,7.49422021702462));
#54181=CARTESIAN_POINT('Ctrl Pts',(4.22749554627325,0.636309800095206,7.48233642793057));
#54182=CARTESIAN_POINT('Ctrl Pts',(4.2818545600116,0.79477268400084,7.4815169336313));
#54183=CARTESIAN_POINT('Ctrl Pts',(4.42096106050366,1.06847604194523,7.47158857881567));
#54184=CARTESIAN_POINT('Ctrl Pts',(4.49399758639363,1.18514270861202,7.46643805441502));
#54185=CARTESIAN_POINT('Ctrl Pts',(4.57985658851437,1.30000000000036,7.4604346225316));
#54186=CARTESIAN_POINT('Ctrl Pts',(4.55678639209678,-1.30000000000004,7.66234429787489));
#54187=CARTESIAN_POINT('Ctrl Pts',(4.4729437511331,-1.18514270861181,7.64437732819764));
#54188=CARTESIAN_POINT('Ctrl Pts',(4.40183404790298,-1.06847604194513,7.62775916256505));
#54189=CARTESIAN_POINT('Ctrl Pts',(4.26697204137397,-0.794772684000851,
7.59248388267156));
#54190=CARTESIAN_POINT('Ctrl Pts',(4.21502126192296,-0.636309800095197,
7.57484693907898));
#54191=CARTESIAN_POINT('Ctrl Pts',(4.14539022778078,-0.319434907277159,
7.54453895215762));
#54192=CARTESIAN_POINT('Ctrl Pts',(4.12973531027791,-0.158333333333332,
7.53130984870383));
#54193=CARTESIAN_POINT('Ctrl Pts',(4.13134197385143,0.158333333333334,7.51087245067975));
#54194=CARTESIAN_POINT('Ctrl Pts',(4.14849242828378,0.319434907277167,7.50479833736505));
#54195=CARTESIAN_POINT('Ctrl Pts',(4.22162247741412,0.636309800095206,7.49116657049894));
#54196=CARTESIAN_POINT('Ctrl Pts',(4.27538846798974,0.79477268400084,7.48674639736213));
#54197=CARTESIAN_POINT('Ctrl Pts',(4.41396332499183,1.06847604194523,7.47558190734422));
#54198=CARTESIAN_POINT('Ctrl Pts',(4.48679959516754,1.18514270861202,7.47049600927413));
#54199=CARTESIAN_POINT('Ctrl Pts',(4.57248821462725,1.30000000000036,7.46515690717758));
#54200=CARTESIAN_POINT('Ctrl Pts',(4.55678639209675,-1.3,7.66234429787489));
#54201=CARTESIAN_POINT('Ctrl Pts',(4.47294375113309,-1.18514270861178,7.64437732819764));
#54202=CARTESIAN_POINT('Ctrl Pts',(4.40183404790297,-1.06847604194512,7.62775916256504));
#54203=CARTESIAN_POINT('Ctrl Pts',(4.26697204137396,-0.794772684000851,
7.59248388267156));
#54204=CARTESIAN_POINT('Ctrl Pts',(4.21502126192295,-0.636309800095197,
7.57484693907897));
#54205=CARTESIAN_POINT('Ctrl Pts',(4.14539022778078,-0.319434907277159,
7.54453895215762));
#54206=CARTESIAN_POINT('Ctrl Pts',(4.12973531027791,-0.158333333333332,
7.53130984870383));
#54207=CARTESIAN_POINT('Ctrl Pts',(4.13134197385143,0.158333333333334,7.51087245067974));
#54208=CARTESIAN_POINT('Ctrl Pts',(4.14849242828378,0.319434907277167,7.50479833736505));
#54209=CARTESIAN_POINT('Ctrl Pts',(4.22162247741411,0.636309800095206,7.49116657049894));
#54210=CARTESIAN_POINT('Ctrl Pts',(4.27538846798974,0.79477268400084,7.48674639736213));
#54211=CARTESIAN_POINT('Ctrl Pts',(4.41396332499177,1.06847604194511,7.47558190734422));
#54212=CARTESIAN_POINT('Ctrl Pts',(4.48679959516739,1.18514270861178,7.47049600927414));
#54213=CARTESIAN_POINT('Ctrl Pts',(4.57248821462698,1.3,7.4651569071776));
#54214=CARTESIAN_POINT('',(4.94063630726094,-1.2,7.50432364248438));
#54215=CARTESIAN_POINT('Ctrl Pts',(4.94063630726094,-1.2,7.50432364248438));
#54216=CARTESIAN_POINT('Ctrl Pts',(4.91543282814962,-1.22406366621288,7.52208787588012));
#54217=CARTESIAN_POINT('Ctrl Pts',(4.89161703542051,-1.24658722057704,7.53992231957329));
#54218=CARTESIAN_POINT('Ctrl Pts',(4.86706934907891,-1.2698559227574,7.55736574712289));
#54219=CARTESIAN_POINT('Ctrl Pts',(4.86506208885659,-1.27176577548985,7.55895005581378));
#54220=CARTESIAN_POINT('Ctrl Pts',(4.83515729345013,-1.30000000000007,7.57914897810145));
#54221=CARTESIAN_POINT('',(4.94779107628116,-0.653834841367199,7.34786299436625));
#54222=CARTESIAN_POINT('Ctrl Pts',(4.94779107631832,-0.653834841365921,
7.3478629943724));
#54223=CARTESIAN_POINT('Ctrl Pts',(4.94731087382852,-0.717195374693346,
7.36393152865268));
#54224=CARTESIAN_POINT('Ctrl Pts',(4.94685161325703,-0.764532971978773,
7.37728967122618));
#54225=CARTESIAN_POINT('Ctrl Pts',(4.94482900656359,-0.949610828965762,
7.42891509030179));
#54226=CARTESIAN_POINT('Ctrl Pts',(4.94332990982166,-1.05888885523217,7.46059351852754));
#54227=CARTESIAN_POINT('Ctrl Pts',(4.94063630726094,-1.2,7.50432364248438));
#54228=CARTESIAN_POINT('',(4.94999291725008,0.653834841531101,7.20837371924883));
#54229=CARTESIAN_POINT('Ctrl Pts',(4.94999291725008,0.653834841531103,7.20837371924884));
#54230=CARTESIAN_POINT('Ctrl Pts',(4.91225397924647,0.575974734740856,7.22582001049342));
#54231=CARTESIAN_POINT('Ctrl Pts',(4.88067089553362,0.493646300356214,7.2412455994813));
#54232=CARTESIAN_POINT('Ctrl Pts',(4.83632534903071,0.338148396013879,7.26563634685165));
#54233=CARTESIAN_POINT('Ctrl Pts',(4.82128042816978,0.265672258741385,7.27532070701134));
#54234=CARTESIAN_POINT('Ctrl Pts',(4.80341717712112,0.129723868038644,7.29191291738494));
#54235=CARTESIAN_POINT('Ctrl Pts',(4.79913221039573,0.066629300779875,7.29899463278343));
#54236=CARTESIAN_POINT('Ctrl Pts',(4.79855028835759,-0.0595469689982444,
7.31231323091239));
#54237=CARTESIAN_POINT('Ctrl Pts',(4.80223201689649,-0.122785107468493,
7.31864896555666));
#54238=CARTESIAN_POINT('Ctrl Pts',(4.81905000979055,-0.260135494715071,
7.33079046336944));
#54239=CARTESIAN_POINT('Ctrl Pts',(4.833790517691,-0.333948532118538,7.33629188943222));
#54240=CARTESIAN_POINT('Ctrl Pts',(4.87782657508354,-0.491208515200836,
7.34478416173381));
#54241=CARTESIAN_POINT('Ctrl Pts',(4.9092926136062,-0.574351663742094,7.34738838935052));
#54242=CARTESIAN_POINT('Ctrl Pts',(4.94779107624583,-0.653834841384027,
7.34786299441341));
#54243=CARTESIAN_POINT('',(4.94934267693687,1.2,7.28066638861011));
#54244=CARTESIAN_POINT('Ctrl Pts',(4.94934267693687,1.2,7.28066638861011));
#54245=CARTESIAN_POINT('Ctrl Pts',(4.94957987508122,1.12296364294518,7.26611293060881));
#54246=CARTESIAN_POINT('Ctrl Pts',(4.94977340107779,1.02715393518566,7.25038272030311));
#54247=CARTESIAN_POINT('Ctrl Pts',(4.9499755995156,0.796382219298827,7.22023948863579));
#54248=CARTESIAN_POINT('Ctrl Pts',(4.94998203044102,0.739891552765075,7.21480928582414));
#54249=CARTESIAN_POINT('Ctrl Pts',(4.94999291725008,0.6538348415311,7.20837371924884));
#54250=CARTESIAN_POINT('Ctrl Pts',(4.84757646506369,1.30000000000001,7.35330497500277));
#54251=CARTESIAN_POINT('Ctrl Pts',(4.86532490684006,1.28264531619758,7.34112851298703));
#54252=CARTESIAN_POINT('Ctrl Pts',(4.8829689846372,1.26535232528287,7.32871014390654));
#54253=CARTESIAN_POINT('Ctrl Pts',(4.92078898353074,1.22818637919983,7.3015438601204));
#54254=CARTESIAN_POINT('Ctrl Pts',(4.93221880462763,1.21690340343215,7.29405567061454));
#54255=CARTESIAN_POINT('Ctrl Pts',(4.94934267693687,1.2,7.28066638861011));
#54256=CARTESIAN_POINT('Ctrl Pts',(4.55678639209675,-1.3,7.66234429787489));
#54257=CARTESIAN_POINT('Ctrl Pts',(4.47294375113309,-1.18514270861178,7.64437732819764));
#54258=CARTESIAN_POINT('Ctrl Pts',(4.40183404790298,-1.06847604194512,7.62775916256505));
#54259=CARTESIAN_POINT('Ctrl Pts',(4.26697204137397,-0.794772684000851,
7.59248388267156));
#54260=CARTESIAN_POINT('Ctrl Pts',(4.21502126192295,-0.636309800095197,
7.57484693907897));
#54261=CARTESIAN_POINT('Ctrl Pts',(4.14539022778077,-0.319434907277159,
7.54453895215762));
#54262=CARTESIAN_POINT('Ctrl Pts',(4.12973531027791,-0.158333333333332,
7.53130984870382));
#54263=CARTESIAN_POINT('Ctrl Pts',(4.13134197385143,0.158333333333334,7.51087245067974));
#54264=CARTESIAN_POINT('Ctrl Pts',(4.14849242828378,0.319434907277167,7.50479833736504));
#54265=CARTESIAN_POINT('Ctrl Pts',(4.22162247741411,0.636309800095206,7.49116657049894));
#54266=CARTESIAN_POINT('Ctrl Pts',(4.27538846798974,0.79477268400084,7.48674639736213));
#54267=CARTESIAN_POINT('Ctrl Pts',(4.41396332499176,1.06847604194511,7.47558190734422));
#54268=CARTESIAN_POINT('Ctrl Pts',(4.48679959516739,1.18514270861178,7.47049600927414));
#54269=CARTESIAN_POINT('Ctrl Pts',(4.57248821462698,1.3,7.4651569071776));
#54270=CARTESIAN_POINT('Ctrl Pts',(4.54709012720593,-1.3,7.73866658637446));
#54271=CARTESIAN_POINT('Ctrl Pts',(4.46362634796674,-1.18514270861178,7.71900924136913));
#54272=CARTESIAN_POINT('Ctrl Pts',(4.39282414406279,-1.06847604194512,7.70122437392077));
#54273=CARTESIAN_POINT('Ctrl Pts',(4.25850766107618,-0.794772684000851,
7.66446357000893));
#54274=CARTESIAN_POINT('Ctrl Pts',(4.20664978510482,-0.636309800095197,
7.64753822102798));
#54275=CARTESIAN_POINT('Ctrl Pts',(4.1373298362099,-0.319434907277159,7.61782007234104));
#54276=CARTESIAN_POINT('Ctrl Pts',(4.12172229231298,-0.158333333333332,
7.60583161692362));
#54277=CARTESIAN_POINT('Ctrl Pts',(4.12368594131515,0.158333333333334,7.58543173958001));
#54278=CARTESIAN_POINT('Ctrl Pts',(4.14114067935745,0.319434907277167,7.5781539388917));
#54279=CARTESIAN_POINT('Ctrl Pts',(4.21469765004064,0.636309800095206,7.56400990143153));
#54280=CARTESIAN_POINT('Ctrl Pts',(4.26870246277087,0.79477268400084,7.55891299945219));
#54281=CARTESIAN_POINT('Ctrl Pts',(4.40750206450663,1.06847604194511,7.54931499191075));
#54282=CARTESIAN_POINT('Ctrl Pts',(4.48039654346318,1.18514270861178,7.54543423312736));
#54283=CARTESIAN_POINT('Ctrl Pts',(4.56610429681699,1.3,7.54182733738404));
#54284=CARTESIAN_POINT('Ctrl Pts',(4.53739386231511,-1.3,7.81498887487404));
#54285=CARTESIAN_POINT('Ctrl Pts',(4.45430894480039,-1.18514270861178,7.79364115454063));
#54286=CARTESIAN_POINT('Ctrl Pts',(4.38381424022261,-1.06847604194512,7.7746895852765));
#54287=CARTESIAN_POINT('Ctrl Pts',(4.2500432807784,-0.794772684000851,7.7364432573463));
#54288=CARTESIAN_POINT('Ctrl Pts',(4.19827830828669,-0.636309800095197,
7.72022950297699));
#54289=CARTESIAN_POINT('Ctrl Pts',(4.12926944463902,-0.319434907277159,
7.69110119252446));
#54290=CARTESIAN_POINT('Ctrl Pts',(4.11370927434805,-0.158333333333332,
7.68035338514341));
#54291=CARTESIAN_POINT('Ctrl Pts',(4.11602990877888,0.158333333333334,7.65999102848028));
#54292=CARTESIAN_POINT('Ctrl Pts',(4.13378893043113,0.319434907277167,7.65150954041835));
#54293=CARTESIAN_POINT('Ctrl Pts',(4.20777282266716,0.636309800095206,7.63685323236411));
#54294=CARTESIAN_POINT('Ctrl Pts',(4.262016457552,0.79477268400084,7.63107960154224));
#54295=CARTESIAN_POINT('Ctrl Pts',(4.40104080402149,1.06847604194511,7.62304807647727));
#54296=CARTESIAN_POINT('Ctrl Pts',(4.47399349175896,1.18514270861178,7.62037245698058));
#54297=CARTESIAN_POINT('Ctrl Pts',(4.559720379007,1.3,7.61849776759048));
#54298=CARTESIAN_POINT('Ctrl Pts',(4.52769759742428,-1.3,7.89131116337361));
#54299=CARTESIAN_POINT('Ctrl Pts',(4.44499154163403,-1.18514270861178,7.86827306771213));
#54300=CARTESIAN_POINT('Ctrl Pts',(4.37480433638243,-1.06847604194512,7.84815479663223));
#54301=CARTESIAN_POINT('Ctrl Pts',(4.24157890048062,-0.794772684000851,
7.80842294468367));
#54302=CARTESIAN_POINT('Ctrl Pts',(4.18990683146856,-0.636309800095197,
7.792920784926));
#54303=CARTESIAN_POINT('Ctrl Pts',(4.12120905306814,-0.319434907277159,
7.76438231270788));
#54304=CARTESIAN_POINT('Ctrl Pts',(4.10569625638312,-0.158333333333332,
7.7548751533632));
#54305=CARTESIAN_POINT('Ctrl Pts',(4.1083738762426,0.158333333333334,7.73455031738056));
#54306=CARTESIAN_POINT('Ctrl Pts',(4.1264371815048,0.319434907277167,7.724865141945));
#54307=CARTESIAN_POINT('Ctrl Pts',(4.20084799529369,0.636309800095206,7.7096965632967));
#54308=CARTESIAN_POINT('Ctrl Pts',(4.25533045233313,0.79477268400084,7.70324620363229));
#54309=CARTESIAN_POINT('Ctrl Pts',(4.39457954353636,1.06847604194511,7.69678116104379));
#54310=CARTESIAN_POINT('Ctrl Pts',(4.46759044005475,1.18514270861178,7.69531068083379));
#54311=CARTESIAN_POINT('Ctrl Pts',(4.55333646119701,1.3,7.69516819779692));
#54312=CARTESIAN_POINT('Ctrl Pts',(4.52769759742429,-1.3,7.89131116337361));
#54313=CARTESIAN_POINT('Ctrl Pts',(4.44499154163404,-1.18514270861178,7.86827306771213));
#54314=CARTESIAN_POINT('Ctrl Pts',(4.37480433638243,-1.06847604194512,7.84815479663222));
#54315=CARTESIAN_POINT('Ctrl Pts',(4.24157890048062,-0.794772684000851,
7.80842294468367));
#54316=CARTESIAN_POINT('Ctrl Pts',(4.18990683146856,-0.636309800095197,
7.792920784926));
#54317=CARTESIAN_POINT('Ctrl Pts',(4.12120905306814,-0.319434907277159,
7.76438231270788));
#54318=CARTESIAN_POINT('Ctrl Pts',(4.10569625638312,-0.158333333333332,
7.7548751533632));
#54319=CARTESIAN_POINT('Ctrl Pts',(4.1083738762426,0.158333333333334,7.73455031738056));
#54320=CARTESIAN_POINT('Ctrl Pts',(4.1264371815048,0.319434907277167,7.724865141945));
#54321=CARTESIAN_POINT('Ctrl Pts',(4.20084799529369,0.636309800095206,7.7096965632967));
#54322=CARTESIAN_POINT('Ctrl Pts',(4.25533045233313,0.79477268400084,7.70324620363229));
#54323=CARTESIAN_POINT('Ctrl Pts',(4.39457954353635,1.06847604194511,7.69678116104379));
#54324=CARTESIAN_POINT('Ctrl Pts',(4.46759044005475,1.18514270861178,7.69531068083379));
#54325=CARTESIAN_POINT('Ctrl Pts',(4.55333646119701,1.3,7.69516819779692));
#54326=CARTESIAN_POINT('Ctrl Pts',(4.52769759742604,-1.30000000000244,7.8913111633741));
#54327=CARTESIAN_POINT('Ctrl Pts',(4.44499154163503,-1.18514270861343,7.86827306771241));
#54328=CARTESIAN_POINT('Ctrl Pts',(4.37480433638284,-1.06847604194595,7.84815479663235));
#54329=CARTESIAN_POINT('Ctrl Pts',(4.24157890048062,-0.794772684000851,
7.80842294468367));
#54330=CARTESIAN_POINT('Ctrl Pts',(4.18990683146856,-0.636309800095196,
7.792920784926));
#54331=CARTESIAN_POINT('Ctrl Pts',(4.12120905306814,-0.319434907277159,
7.76438231270788));
#54332=CARTESIAN_POINT('Ctrl Pts',(4.10569625638312,-0.158333333333332,
7.7548751533632));
#54333=CARTESIAN_POINT('Ctrl Pts',(4.1083738762426,0.158333333333334,7.73455031738056));
#54334=CARTESIAN_POINT('Ctrl Pts',(4.1264371815048,0.319434907277167,7.72486514194501));
#54335=CARTESIAN_POINT('Ctrl Pts',(4.20084799529369,0.636309800095206,7.70969656329671));
#54336=CARTESIAN_POINT('Ctrl Pts',(4.25533045233313,0.79477268400084,7.7032462036323));
#54337=CARTESIAN_POINT('Ctrl Pts',(4.39457954353637,1.06847604194513,7.69678116104379));
#54338=CARTESIAN_POINT('Ctrl Pts',(4.46759044005478,1.18514270861182,7.69531068083379));
#54339=CARTESIAN_POINT('Ctrl Pts',(4.55333646119706,1.30000000000007,7.69516819779692));
#54340=CARTESIAN_POINT('Ctrl Pts',(4.53392313642068,-1.30000000000244,7.89746222583649));
#54341=CARTESIAN_POINT('Ctrl Pts',(4.45118854317531,-1.18514270861343,7.87373889304186));
#54342=CARTESIAN_POINT('Ctrl Pts',(4.38081889485167,-1.06847604194595,7.85351577236843));
#54343=CARTESIAN_POINT('Ctrl Pts',(4.24681642619259,-0.794772684000851,
7.81488250820649));
#54344=CARTESIAN_POINT('Ctrl Pts',(4.19381566978082,-0.636309800095196,
7.80277904736738));
#54345=CARTESIAN_POINT('Ctrl Pts',(4.12443963753454,-0.319434907277159,
7.77588343648135));
#54346=CARTESIAN_POINT('Ctrl Pts',(4.10920625064663,-0.158333333333332,
7.76590783487045));
#54347=CARTESIAN_POINT('Ctrl Pts',(4.11199983518693,0.158333333333334,7.74537650602099));
#54348=CARTESIAN_POINT('Ctrl Pts',(4.13001103020958,0.319434907277167,7.73569629634525));
#54349=CARTESIAN_POINT('Ctrl Pts',(4.20510952842189,0.636309800095206,7.71898770243354));
#54350=CARTESIAN_POINT('Ctrl Pts',(4.26054738494527,0.79477268400084,7.71015610884286));
#54351=CARTESIAN_POINT('Ctrl Pts',(4.40061540550434,1.06847604194513,7.70244469618862));
#54352=CARTESIAN_POINT('Ctrl Pts',(4.47390766109764,1.18514270861182,7.70077480939336));
#54353=CARTESIAN_POINT('Ctrl Pts',(4.5598619162159,1.30000000000007,7.70077302060486));
#54354=CARTESIAN_POINT('Ctrl Pts',(4.54480756132074,-1.30000000000244,7.9031313104298));
#54355=CARTESIAN_POINT('Ctrl Pts',(4.46489083553443,-1.18514270861343,7.87867015857436));
#54356=CARTESIAN_POINT('Ctrl Pts',(4.39634596099135,-1.06847604194595,7.85850593886263));
#54357=CARTESIAN_POINT('Ctrl Pts',(4.26426483974512,-0.794772684000851,
7.82184933034068));
#54358=CARTESIAN_POINT('Ctrl Pts',(4.20887006018204,-0.636309800095195,
7.81473397539683));
#54359=CARTESIAN_POINT('Ctrl Pts',(4.13843139653786,-0.319434907277158,
7.79050397880872));
#54360=CARTESIAN_POINT('Ctrl Pts',(4.12232754980889,-0.158333333333332,
7.78005767523933));
#54361=CARTESIAN_POINT('Ctrl Pts',(4.12518911467222,0.158333333333334,7.75938696584332));
#54362=CARTESIAN_POINT('Ctrl Pts',(4.14416864038823,0.319434907277167,7.75020180904442));
#54363=CARTESIAN_POINT('Ctrl Pts',(4.22040735616573,0.636309800095205,7.73021018349228));
#54364=CARTESIAN_POINT('Ctrl Pts',(4.27822012753513,0.794772684000839,7.71521033816527));
#54365=CARTESIAN_POINT('Ctrl Pts',(4.41636977068153,1.06847604194513,7.70556351793047));
#54366=CARTESIAN_POINT('Ctrl Pts',(4.48783523330211,1.18514270861182,7.7041518618103));
#54367=CARTESIAN_POINT('Ctrl Pts',(4.57096629697396,1.30000000000006,7.7055043005997));
#54368=CARTESIAN_POINT('Ctrl Pts',(4.56073300810824,-1.30000000000243,7.91156448348569));
#54369=CARTESIAN_POINT('Ctrl Pts',(4.48442324017247,-1.18514270861343,7.8878141720034));
#54370=CARTESIAN_POINT('Ctrl Pts',(4.41849168518471,-1.06847604194595,7.86837871921155));
#54371=CARTESIAN_POINT('Ctrl Pts',(4.29015235166538,-0.794772684000849,
7.83344712197293));
#54372=CARTESIAN_POINT('Ctrl Pts',(4.23393748623805,-0.636309800095195,
7.8277112028804));
#54373=CARTESIAN_POINT('Ctrl Pts',(4.16339507988998,-0.319434907277158,
7.804796401206));
#54374=CARTESIAN_POINT('Ctrl Pts',(4.14588138546196,-0.158333333333332,
7.7947403583322));
#54375=CARTESIAN_POINT('Ctrl Pts',(4.14874058420388,0.158333333333334,7.7739769333919));
#54376=CARTESIAN_POINT('Ctrl Pts',(4.16904183231081,0.319434907277167,7.76463591973765));
#54377=CARTESIAN_POINT('Ctrl Pts',(4.24555415646176,0.636309800095206,7.7424739257509));
#54378=CARTESIAN_POINT('Ctrl Pts',(4.30458812558598,0.794772684000839,7.72425389573271));
#54379=CARTESIAN_POINT('Ctrl Pts',(4.43908143338691,1.06847604194513,7.71273200536022));
#54380=CARTESIAN_POINT('Ctrl Pts',(4.50789470780772,1.18514270861182,7.71093554617766));
#54381=CARTESIAN_POINT('Ctrl Pts',(4.58730408717054,1.30000000000006,7.71233002722669));
#54382=CARTESIAN_POINT('Ctrl Pts',(4.57382741729863,-1.30000000000243,7.91886372538083));
#54383=CARTESIAN_POINT('Ctrl Pts',(4.50011834828894,-1.18514270861343,7.89601079220276));
#54384=CARTESIAN_POINT('Ctrl Pts',(4.43611194809718,-1.06847604194595,7.87708349177196));
#54385=CARTESIAN_POINT('Ctrl Pts',(4.31065946519988,-0.794772684000845,
7.84242663834982));
#54386=CARTESIAN_POINT('Ctrl Pts',(4.2542467506077,-0.636309800095193,7.83492820952284));
#54387=CARTESIAN_POINT('Ctrl Pts',(4.18369130649239,-0.319434907277157,
7.81215028741846));
#54388=CARTESIAN_POINT('Ctrl Pts',(4.16488401333284,-0.158333333333331,
7.80356975748878));
#54389=CARTESIAN_POINT('Ctrl Pts',(4.16760272647753,0.158333333333333,7.78337191057216));
#54390=CARTESIAN_POINT('Ctrl Pts',(4.18885680806588,0.319434907277164,7.77400698678823));
#54391=CARTESIAN_POINT('Ctrl Pts',(4.26550396617013,0.636309800095202,7.75105538623989));
#54392=CARTESIAN_POINT('Ctrl Pts',(4.32541781011878,0.794772684000836,7.73137058834162));
#54393=CARTESIAN_POINT('Ctrl Pts',(4.45717945460002,1.06847604194513,7.71905327456052));
#54394=CARTESIAN_POINT('Ctrl Pts',(4.52402445451157,1.18514270861182,7.71709979233987));
#54395=CARTESIAN_POINT('Ctrl Pts',(4.60067972068886,1.30000000000006,7.71852453663296));
#54396=CARTESIAN_POINT('Ctrl Pts',(4.58698548913814,-1.30000000000243,7.92639668444855));
#54397=CARTESIAN_POINT('Ctrl Pts',(4.51610702437853,-1.18514270861343,7.90459440423691));
#54398=CARTESIAN_POINT('Ctrl Pts',(4.4542148014283,-1.06847604194595,7.88626268544465));
#54399=CARTESIAN_POINT('Ctrl Pts',(4.33199140118815,-0.794772684000845,
7.85193043894911));
#54400=CARTESIAN_POINT('Ctrl Pts',(4.27544799960624,-0.636309800095193,
7.84267294551725));
#54401=CARTESIAN_POINT('Ctrl Pts',(4.20509654546967,-0.319434907277158,
7.81947012356536));
#54402=CARTESIAN_POINT('Ctrl Pts',(4.18502425031126,-0.158333333333331,
7.81196684122426));
#54403=CARTESIAN_POINT('Ctrl Pts',(4.18789652359372,0.158333333333334,7.79090500173329));
#54404=CARTESIAN_POINT('Ctrl Pts',(4.21065422441233,0.319434907277165,7.7790726717311));
#54405=CARTESIAN_POINT('Ctrl Pts',(4.28723692830633,0.636309800095203,7.75585784273532));
#54406=CARTESIAN_POINT('Ctrl Pts',(4.34717946538134,0.794772684000837,7.73863682367033));
#54407=CARTESIAN_POINT('Ctrl Pts',(4.47565859061765,1.06847604194513,7.72650961893564));
#54408=CARTESIAN_POINT('Ctrl Pts',(4.54036052502848,1.18514270861182,7.72422790455448));
#54409=CARTESIAN_POINT('Ctrl Pts',(4.61415054115615,1.30000000000006,7.7249138933646));
#54410=CARTESIAN_POINT('Ctrl Pts',(4.59965290246012,-1.30000000000243,7.9352726802013));
#54411=CARTESIAN_POINT('Ctrl Pts',(4.53148144844337,-1.18514270861343,7.91440595450751));
#54412=CARTESIAN_POINT('Ctrl Pts',(4.47163014578841,-1.06847604194595,7.89650759170913));
#54413=CARTESIAN_POINT('Ctrl Pts',(4.35258287753016,-0.794772684000846,
7.86201630519716));
#54414=CARTESIAN_POINT('Ctrl Pts',(4.29598055952938,-0.636309800095193,
7.85080058306915));
#54415=CARTESIAN_POINT('Ctrl Pts',(4.22608334988363,-0.319434907277157,
7.82600970215437));
#54416=CARTESIAN_POINT('Ctrl Pts',(4.20522035605998,-0.158333333333331,
7.8176557606092));
#54417=CARTESIAN_POINT('Ctrl Pts',(4.20818531124961,0.158333333333333,7.79597947196624));
#54418=CARTESIAN_POINT('Ctrl Pts',(4.23182022180882,0.319434907277164,7.78420148504121));
#54419=CARTESIAN_POINT('Ctrl Pts',(4.30815003712369,0.636309800095202,7.76169357626058));
#54420=CARTESIAN_POINT('Ctrl Pts',(4.36828391922503,0.794772684000836,7.74628043878177));
#54421=CARTESIAN_POINT('Ctrl Pts',(4.49374998194681,1.06847604194513,7.73402993457807));
#54422=CARTESIAN_POINT('Ctrl Pts',(4.55647188035704,1.18514270861181,7.7312467586804));
#54423=CARTESIAN_POINT('Ctrl Pts',(4.62760606760105,1.30000000000006,7.73098319622891));
#54424=CARTESIAN_POINT('Ctrl Pts',(4.62058857472608,-1.30000000000242,7.94740044967756));
#54425=CARTESIAN_POINT('Ctrl Pts',(4.55682246865916,-1.18514270861342,7.92810801062365));
#54426=CARTESIAN_POINT('Ctrl Pts',(4.50024585615088,-1.06847604194595,7.91113510616114));
#54427=CARTESIAN_POINT('Ctrl Pts',(4.38615173151841,-0.794772684000848,
7.87728289036243));
#54428=CARTESIAN_POINT('Ctrl Pts',(4.32908918141778,-0.636309800095194,
7.86428752440045));
#54429=CARTESIAN_POINT('Ctrl Pts',(4.25969428741779,-0.319434907277158,
7.83785273071171));
#54430=CARTESIAN_POINT('Ctrl Pts',(4.23756287865151,-0.158333333333331,
7.82795116092122));
#54431=CARTESIAN_POINT('Ctrl Pts',(4.24063325570311,0.158333333333333,7.80566477392697));
#54432=CARTESIAN_POINT('Ctrl Pts',(4.26568526094983,0.319434907277163,7.79454110809123));
#54433=CARTESIAN_POINT('Ctrl Pts',(4.34163938416832,0.636309800095201,7.77301126161501));
#54434=CARTESIAN_POINT('Ctrl Pts',(4.40223043329164,0.794772684000837,7.75938974055269));
#54435=CARTESIAN_POINT('Ctrl Pts',(4.52273003821343,1.06847604194513,7.7468944981955));
#54436=CARTESIAN_POINT('Ctrl Pts',(4.58215662922367,1.18514270861182,7.74350690324006));
#54437=CARTESIAN_POINT('Ctrl Pts',(4.64884999722391,1.30000000000006,7.74214044075126));
#54438=CARTESIAN_POINT('Ctrl Pts',(4.648594134421,-1.30000000000242,7.96634699489031));
#54439=CARTESIAN_POINT('Ctrl Pts',(4.590425503944,-1.18514270861342,7.95036965591271));
#54440=CARTESIAN_POINT('Ctrl Pts',(4.53808890713736,-1.06847604194595,7.93529776095));
#54441=CARTESIAN_POINT('Ctrl Pts',(4.43065406308698,-0.794772684000845,
7.90257042527186));
#54442=CARTESIAN_POINT('Ctrl Pts',(4.3736277410315,-0.636309800095188,7.88520288404559));
#54443=CARTESIAN_POINT('Ctrl Pts',(4.30526704996447,-0.319434907277153,
7.85555771503743));
#54444=CARTESIAN_POINT('Ctrl Pts',(4.28146640826412,-0.15833333333333,7.84357758256878));
#54445=CARTESIAN_POINT('Ctrl Pts',(4.28477232272335,0.158333333333332,7.82001009819072));
#54446=CARTESIAN_POINT('Ctrl Pts',(4.31173064007393,0.319434907277162,7.80929521920069));
#54447=CARTESIAN_POINT('Ctrl Pts',(4.38712719264106,0.636309800095196,7.78915795492929));
#54448=CARTESIAN_POINT('Ctrl Pts',(4.44813248358814,0.794772684000826,7.77910758672209));
#54449=CARTESIAN_POINT('Ctrl Pts',(4.5620254058037,1.06847604194512,7.76584719773633));
#54450=CARTESIAN_POINT('Ctrl Pts',(4.61711174649682,1.18514270861181,7.76112877184541));
#54451=CARTESIAN_POINT('Ctrl Pts',(4.67798440200465,1.30000000000006,7.75743185110967));
#54452=CARTESIAN_POINT('Ctrl Pts',(4.68165552287129,-1.30000000000242,7.98886506857474));
#54453=CARTESIAN_POINT('Ctrl Pts',(4.63044692290565,-1.18514270861342,7.9759028451139));
#54454=CARTESIAN_POINT('Ctrl Pts',(4.58326800846122,-1.06847604194594,7.96280091003532));
#54455=CARTESIAN_POINT('Ctrl Pts',(4.48358465767529,-0.794772684000843,
7.93221005718464));
#54456=CARTESIAN_POINT('Ctrl Pts',(4.4255974463165,-0.636309800095188,7.91320356677101));
#54457=CARTESIAN_POINT('Ctrl Pts',(4.3581626577691,-0.319434907277154,7.88096518691823));
#54458=CARTESIAN_POINT('Ctrl Pts',(4.33281031472247,-0.158333333333329,
7.86496806667059));
#54459=CARTESIAN_POINT('Ctrl Pts',(4.33640145193234,0.158333333333332,7.84022588101273));
#54460=CARTESIAN_POINT('Ctrl Pts',(4.36531510784172,0.31943490727716,7.8318139044389));
#54461=CARTESIAN_POINT('Ctrl Pts',(4.44012553436285,0.636309800095195,7.81297575562654));
#54462=CARTESIAN_POINT('Ctrl Pts',(4.50196696609397,0.794772684000829,7.80507489872517));
#54463=CARTESIAN_POINT('Ctrl Pts',(4.6082648302697,1.06847604194512,7.78952242190487));
#54464=CARTESIAN_POINT('Ctrl Pts',(4.65828629564362,1.1851427086118,7.78276118857335));
#54465=CARTESIAN_POINT('Ctrl Pts',(4.71231681971385,1.30000000000005,7.77597081284977));
#54466=CARTESIAN_POINT('Ctrl Pts',(4.70425563008758,-1.30000000000241,8.00520911535597));
#54467=CARTESIAN_POINT('Ctrl Pts',(4.65747659860534,-1.18514270861341,7.99545421885104));
#54468=CARTESIAN_POINT('Ctrl Pts',(4.61364357336526,-1.06847604194593,7.98435965147816));
#54469=CARTESIAN_POINT('Ctrl Pts',(4.51918638006031,-0.794772684000833,
7.95563407368116));
#54470=CARTESIAN_POINT('Ctrl Pts',(4.46117060216464,-0.636309800095182,
7.93352610681582));
#54471=CARTESIAN_POINT('Ctrl Pts',(4.3944737386267,-0.319434907277151,7.89939714677356));
#54472=CARTESIAN_POINT('Ctrl Pts',(4.36771834352831,-0.158333333333328,
7.88204658024336));
#54473=CARTESIAN_POINT('Ctrl Pts',(4.37150210807931,0.158333333333331,7.85651957051754));
#54474=CARTESIAN_POINT('Ctrl Pts',(4.40196138338493,0.319434907277159,7.8487048664006));
#54475=CARTESIAN_POINT('Ctrl Pts',(4.47652822152956,0.636309800095191,7.83010030917989));
#54476=CARTESIAN_POINT('Ctrl Pts',(4.53908134358413,0.794772684000821,7.82329415309885));
#54477=CARTESIAN_POINT('Ctrl Pts',(4.64012069704688,1.06847604194511,7.80627724109663));
#54478=CARTESIAN_POINT('Ctrl Pts',(4.68659362897972,1.1851427086118,7.79832390296704));
#54479=CARTESIAN_POINT('Ctrl Pts',(4.73580330060843,1.30000000000004,7.78978321737488));
#54480=CARTESIAN_POINT('Ctrl Pts',(4.71911478157206,-1.30000000000241,8.01670270298301));
#54481=CARTESIAN_POINT('Ctrl Pts',(4.67550859596122,-1.18514270861341,8.00842616314175));
#54482=CARTESIAN_POINT('Ctrl Pts',(4.63403254674509,-1.06847604194593,7.99829893819727));
#54483=CARTESIAN_POINT('Ctrl Pts',(4.54313561700505,-0.794772684000834,
7.97062756981452));
#54484=CARTESIAN_POINT('Ctrl Pts',(4.4847695101651,-0.63630980009518,7.94750775051987));
#54485=CARTESIAN_POINT('Ctrl Pts',(4.41844002242372,-0.31943490727715,7.91254580530321));
#54486=CARTESIAN_POINT('Ctrl Pts',(4.39079099009392,-0.158333333333328,
7.89416363326185));
#54487=CARTESIAN_POINT('Ctrl Pts',(4.39467503626453,0.15833333333333,7.86825657552279));
#54488=CARTESIAN_POINT('Ctrl Pts',(4.42614665727086,0.319434907277158,7.86098063695745));
#54489=CARTESIAN_POINT('Ctrl Pts',(4.50051285189156,0.636309800095188,7.84266468354586));
#54490=CARTESIAN_POINT('Ctrl Pts',(4.56342960718383,0.794772684000817,7.83690727777958));
#54491=CARTESIAN_POINT('Ctrl Pts',(4.66107975269782,1.06847604194511,7.81843533592283));
#54492=CARTESIAN_POINT('Ctrl Pts',(4.70528836283365,1.18514270861179,7.80929952045736));
#54493=CARTESIAN_POINT('Ctrl Pts',(4.75143645340681,1.30000000000004,7.79902370870333));
#54494=CARTESIAN_POINT('Ctrl Pts',(4.72917527752257,-1.30000000000241,8.02388370350364));
#54495=CARTESIAN_POINT('Ctrl Pts',(4.68746973293028,-1.18514270861341,8.0172359429138));
#54496=CARTESIAN_POINT('Ctrl Pts',(4.64742498238625,-1.06847604194593,8.00817660875066));
#54497=CARTESIAN_POINT('Ctrl Pts',(4.55875036419719,-0.794772684000832,
7.98167651713242));
#54498=CARTESIAN_POINT('Ctrl Pts',(4.50030656371858,-0.636309800095181,
7.95745763891306));
#54499=CARTESIAN_POINT('Ctrl Pts',(4.43433331923585,-0.31943490727715,7.92159031498128));
#54500=CARTESIAN_POINT('Ctrl Pts',(4.406226867755,-0.158333333333328,7.90202581739956));
#54501=CARTESIAN_POINT('Ctrl Pts',(4.41020012676641,0.15833333333333,7.87579960455339));
#54502=CARTESIAN_POINT('Ctrl Pts',(4.44224001576719,0.319434907277158,7.86926331378344));
#54503=CARTESIAN_POINT('Ctrl Pts',(4.51638761628297,0.636309800095189,7.85145424983308));
#54504=CARTESIAN_POINT('Ctrl Pts',(4.57950403080941,0.794772684000818,7.84655447181586));
#54505=CARTESIAN_POINT('Ctrl Pts',(4.67484086149381,1.06847604194511,7.82732413314217));
#54506=CARTESIAN_POINT('Ctrl Pts',(4.71752144744068,1.18514270861179,7.81747635695453));
#54507=CARTESIAN_POINT('Ctrl Pts',(4.76161483790889,1.30000000000004,7.80610490563682));
#54508=CARTESIAN_POINT('Ctrl Pts',(4.74172894757775,-1.30000000000241,8.03290675645279));
#54509=CARTESIAN_POINT('Ctrl Pts',(4.70251496843966,-1.18514270861341,8.0279335814323));
#54510=CARTESIAN_POINT('Ctrl Pts',(4.66432929110832,-1.06847604194593,8.01998788039034));
#54511=CARTESIAN_POINT('Ctrl Pts',(4.57848832033929,-0.794772684000832,
7.9947645916901));
#54512=CARTESIAN_POINT('Ctrl Pts',(4.51980586395291,-0.63630980009518,7.96957855615327));
#54513=CARTESIAN_POINT('Ctrl Pts',(4.45421672472527,-0.319434907277149,
7.93278122892627));
#54514=CARTESIAN_POINT('Ctrl Pts',(4.42551702402987,-0.158333333333328,
7.91186617049926));
#54515=CARTESIAN_POINT('Ctrl Pts',(4.42961312616382,0.15833333333333,7.88520561246107));
#54516=CARTESIAN_POINT('Ctrl Pts',(4.46235615477674,0.319434907277157,7.87959528850274));
#54517=CARTESIAN_POINT('Ctrl Pts',(4.53639625640105,0.636309800095188,7.86181163555795));
#54518=CARTESIAN_POINT('Ctrl Pts',(4.60003239837384,0.794772684000817,7.85702810288057));
#54519=CARTESIAN_POINT('Ctrl Pts',(4.69261022068255,1.0684760419451,7.83634193258301));
#54520=CARTESIAN_POINT('Ctrl Pts',(4.73339856048218,1.18514270861179,7.82551824541604));
#54521=CARTESIAN_POINT('Ctrl Pts',(4.77490173115041,1.30000000000004,7.81282514770576));
#54522=CARTESIAN_POINT('Ctrl Pts',(4.7564618490923,-1.3000000000024,8.04470262929104));
#54523=CARTESIAN_POINT('Ctrl Pts',(4.72034281583928,-1.1851427086134,8.04142414791164));
#54524=CARTESIAN_POINT('Ctrl Pts',(4.68447303677349,-1.06847604194592,8.03456109230727));
#54525=CARTESIAN_POINT('Ctrl Pts',(4.60218249844279,-0.794772684000827,
8.01042497736035));
#54526=CARTESIAN_POINT('Ctrl Pts',(4.54336090312408,-0.636309800095178,
7.98361406151805));
#54527=CARTESIAN_POINT('Ctrl Pts',(4.47807488179141,-0.31943490727715,7.94623932848582));
#54528=CARTESIAN_POINT('Ctrl Pts',(4.4482447018158,-0.158333333333327,7.92507344115463));
#54529=CARTESIAN_POINT('Ctrl Pts',(4.45228443140408,0.15833333333333,7.89856270081334));
#54530=CARTESIAN_POINT('Ctrl Pts',(4.48599321781917,0.319434907277156,7.89364309040658));
#54531=CARTESIAN_POINT('Ctrl Pts',(4.55983607370581,0.636309800095186,7.87615116563573));
#54532=CARTESIAN_POINT('Ctrl Pts',(4.62395355451121,0.794772684000817,7.87202113959796));
#54533=CARTESIAN_POINT('Ctrl Pts',(4.71318387302268,1.0684760419451,7.84979792163711));
#54534=CARTESIAN_POINT('Ctrl Pts',(4.75171193677337,1.18514270861179,7.83781462940899));
#54535=CARTESIAN_POINT('Ctrl Pts',(4.79014356570032,1.30000000000003,7.82346765255661));
#54536=CARTESIAN_POINT('Ctrl Pts',(4.7712546831859,-1.3000000000024,8.05621111744062));
#54537=CARTESIAN_POINT('Ctrl Pts',(4.73782127143929,-1.1851427086134,8.05576903410186));
#54538=CARTESIAN_POINT('Ctrl Pts',(4.70398052542868,-1.06847604194592,8.05080464184715));
#54539=CARTESIAN_POINT('Ctrl Pts',(4.62486060868961,-0.794772684000826,
8.02888846433499));
#54540=CARTESIAN_POINT('Ctrl Pts',(4.56590680565344,-0.636309800095177,
8.00062210173252));
#54541=CARTESIAN_POINT('Ctrl Pts',(4.50130284875518,-0.319434907277149,
7.96156634483499));
#54542=CARTESIAN_POINT('Ctrl Pts',(4.47101716764841,-0.158333333333327,
7.93805678516888));
#54543=CARTESIAN_POINT('Ctrl Pts',(4.47550015163245,0.158333333333329,7.91011414982581));
#54544=CARTESIAN_POINT('Ctrl Pts',(4.51032201344223,0.319434907277155,7.90534098618133));
#54545=CARTESIAN_POINT('Ctrl Pts',(4.5839491280442,0.636309800095185,7.88817234152425));
#54546=CARTESIAN_POINT('Ctrl Pts',(4.64809446566682,0.794772684000815,7.88619635929522));
#54547=CARTESIAN_POINT('Ctrl Pts',(4.73395633620671,1.0684760419451,7.86243688302862));
#54548=CARTESIAN_POINT('Ctrl Pts',(4.77030033016138,1.18514270861179,7.84900000871981));
#54549=CARTESIAN_POINT('Ctrl Pts',(4.80582189580988,1.30000000000003,7.83241085700264));
#54550=CARTESIAN_POINT('Ctrl Pts',(4.78614006404298,-1.3000000000024,8.06749734457243));
#54551=CARTESIAN_POINT('Ctrl Pts',(4.7558739845875,-1.18514270861339,8.06852826690951));
#54552=CARTESIAN_POINT('Ctrl Pts',(4.72435205105478,-1.06847604194592,8.06463278387327));
#54553=CARTESIAN_POINT('Ctrl Pts',(4.64862880450213,-0.794772684000822,
8.04425245683455));
#54554=CARTESIAN_POINT('Ctrl Pts',(4.58905049079883,-0.636309800095173,
8.01579961384292));
#54555=CARTESIAN_POINT('Ctrl Pts',(4.52465769933224,-0.319434907277147,
7.97644430868896));
#54556=CARTESIAN_POINT('Ctrl Pts',(4.49360222816118,-0.158333333333326,
7.95160804540723));
#54557=CARTESIAN_POINT('Ctrl Pts',(4.49801779013193,0.158333333333329,7.92388996056146));
#54558=CARTESIAN_POINT('Ctrl Pts',(4.53341734858637,0.319434907277155,7.92106635405216));
#54559=CARTESIAN_POINT('Ctrl Pts',(4.60694991064819,0.636309800095182,7.90384333626878));
#54560=CARTESIAN_POINT('Ctrl Pts',(4.67213697337497,0.79477268400081,7.90064758224056));
#54561=CARTESIAN_POINT('Ctrl Pts',(4.7547849514279,1.06847604194509,7.87493106055155));
#54562=CARTESIAN_POINT('Ctrl Pts',(4.7888369662119,1.18514270861178,7.86045823849655));
#54563=CARTESIAN_POINT('Ctrl Pts',(4.8211657484902,1.30000000000002,7.84264432373467));
#54564=CARTESIAN_POINT('Ctrl Pts',(4.80572350694021,-1.30000000000239,8.08315709719347));
#54565=CARTESIAN_POINT('Ctrl Pts',(4.77908700046572,-1.18514270861339,8.08778233032985));
#54566=CARTESIAN_POINT('Ctrl Pts',(4.75031148872691,-1.06847604194591,8.08626823027757));
#54567=CARTESIAN_POINT('Ctrl Pts',(4.678892770022,-0.794772684000819,8.06858726842701));
#54568=CARTESIAN_POINT('Ctrl Pts',(4.61928686686011,-0.636309800095172,
8.03774084106113));
#54569=CARTESIAN_POINT('Ctrl Pts',(4.55560515980317,-0.319434907277147,
7.9968316679897));
#54570=CARTESIAN_POINT('Ctrl Pts',(4.52350426881947,-0.158333333333326,
7.97033427815847));
#54571=CARTESIAN_POINT('Ctrl Pts',(4.52826408571188,0.158333333333328,7.94154897326003));
#54572=CARTESIAN_POINT('Ctrl Pts',(4.56517584864967,0.319434907277153,7.93885087863263));
#54573=CARTESIAN_POINT('Ctrl Pts',(4.63844896451369,0.63630980009518,7.92196196446686));
#54574=CARTESIAN_POINT('Ctrl Pts',(4.70380856892106,0.794772684000809,7.92110560016767));
#54575=CARTESIAN_POINT('Ctrl Pts',(4.78201031557717,1.06847604194509,7.89325959006359));
#54576=CARTESIAN_POINT('Ctrl Pts',(4.81315056856757,1.18514270861178,7.87690867767859));
#54577=CARTESIAN_POINT('Ctrl Pts',(4.84158043608123,1.30000000000002,7.85626035888629));
#54578=CARTESIAN_POINT('Ctrl Pts',(4.8212811930343,-1.30000000000238,8.09687619887558));
#54579=CARTESIAN_POINT('Ctrl Pts',(4.79789839802072,-1.18514270861338,8.10352243427901));
#54580=CARTESIAN_POINT('Ctrl Pts',(4.77153676353432,-1.06847604194591,8.10340154917221));
#54581=CARTESIAN_POINT('Ctrl Pts',(4.70375439914706,-0.794772684000816,
8.08748887825612));
#54582=CARTESIAN_POINT('Ctrl Pts',(4.6437836694552,-0.636309800095168,8.05567077476759));
#54583=CARTESIAN_POINT('Ctrl Pts',(4.58042492723703,-0.319434907277145,
8.01425946128189));
#54584=CARTESIAN_POINT('Ctrl Pts',(4.54732450489343,-0.158333333333325,
7.98688135529432));
#54585=CARTESIAN_POINT('Ctrl Pts',(4.55217177108714,0.158333333333327,7.957862440906));
#54586=CARTESIAN_POINT('Ctrl Pts',(4.59014492374784,0.319434907277152,7.95586253562142));
#54587=CARTESIAN_POINT('Ctrl Pts',(4.66332532960197,0.636309800095177,7.93889586442583));
#54588=CARTESIAN_POINT('Ctrl Pts',(4.72925564548018,0.794772684000805,7.93852029008944));
#54589=CARTESIAN_POINT('Ctrl Pts',(4.8040169197097,1.06847604194509,7.90843996467499));
#54590=CARTESIAN_POINT('Ctrl Pts',(4.83280848967938,1.18514270861177,7.89054411235512));
#54591=CARTESIAN_POINT('Ctrl Pts',(4.85803024418299,1.30000000000001,7.86777306600139));
#54592=CARTESIAN_POINT('Ctrl Pts',(4.83597411107337,-1.30000000000238,8.10851922151873));
#54593=CARTESIAN_POINT('Ctrl Pts',(4.81534154679997,-1.18514270861338,8.11774719602154));
#54594=CARTESIAN_POINT('Ctrl Pts',(4.79102914000993,-1.0684760419459,8.11941808524342));
#54595=CARTESIAN_POINT('Ctrl Pts',(4.72636144428147,-0.794772684000813,
8.10581979481759));
#54596=CARTESIAN_POINT('Ctrl Pts',(4.66610399033152,-0.636309800095166,
8.07295558482936));
#54597=CARTESIAN_POINT('Ctrl Pts',(4.60315685786802,-0.319434907277144,
8.03076446959183));
#54598=CARTESIAN_POINT('Ctrl Pts',(4.56938641996014,-0.158333333333324,
8.00187873773164));
#54599=CARTESIAN_POINT('Ctrl Pts',(4.57440911732778,0.158333333333327,7.97237130554391));
#54600=CARTESIAN_POINT('Ctrl Pts',(4.61325945310722,0.319434907277151,7.97127415946121));
#54601=CARTESIAN_POINT('Ctrl Pts',(4.68632094515445,0.636309800095175,7.95432920870802));
#54602=CARTESIAN_POINT('Ctrl Pts',(4.75276714075305,0.794772684000803,7.95446014804467));
#54603=CARTESIAN_POINT('Ctrl Pts',(4.82435463557553,1.06847604194508,7.92231770894031));
#54604=CARTESIAN_POINT('Ctrl Pts',(4.85098494139824,1.18514270861177,7.90297455592258));
#54605=CARTESIAN_POINT('Ctrl Pts',(4.87325797911311,1.30000000000001,7.87820152078065));
#54606=CARTESIAN_POINT('Ctrl Pts',(4.84561392829011,-1.30000000000238,8.11673827460531));
#54607=CARTESIAN_POINT('Ctrl Pts',(4.82702732226811,-1.18514270861338,8.12708722672374));
#54608=CARTESIAN_POINT('Ctrl Pts',(4.80420024520761,-1.0684760419459,8.12961304670658));
#54609=CARTESIAN_POINT('Ctrl Pts',(4.74166879425471,-0.794772684000813,
8.11737519591012));
#54610=CARTESIAN_POINT('Ctrl Pts',(4.68085372121343,-0.636309800095166,
8.08482027135769));
#54611=CARTESIAN_POINT('Ctrl Pts',(4.61809033912233,-0.319434907277144,
8.04236144674853));
#54612=CARTESIAN_POINT('Ctrl Pts',(4.58394762600498,-0.158333333333324,
8.01228869742108));
#54613=CARTESIAN_POINT('Ctrl Pts',(4.58920734463784,0.158333333333327,7.98211214185068));
#54614=CARTESIAN_POINT('Ctrl Pts',(4.62883416859871,0.31943490727715,7.98104157223286));
#54615=CARTESIAN_POINT('Ctrl Pts',(4.70185414805629,0.636309800095174,7.9640021533145));
#54616=CARTESIAN_POINT('Ctrl Pts',(4.76848548414612,0.794772684000801,7.96494516785146));
#54617=CARTESIAN_POINT('Ctrl Pts',(4.83789792807451,1.06847604194508,7.93160930152804));
#54618=CARTESIAN_POINT('Ctrl Pts',(4.86307582681345,1.18514270861177,7.91133835210395));
#54619=CARTESIAN_POINT('Ctrl Pts',(4.88338554929927,1.30000000000001,7.8852263145716));
#54620=CARTESIAN_POINT('Ctrl Pts',(4.85873584770498,-1.30000000000237,8.1283093707173));
#54621=CARTESIAN_POINT('Ctrl Pts',(4.84257246164534,-1.18514270861337,8.14123666706622));
#54622=CARTESIAN_POINT('Ctrl Pts',(4.82158036271301,-1.0684760419459,8.14548959140894));
#54623=CARTESIAN_POINT('Ctrl Pts',(4.76192912200796,-0.794772684000808,
8.13527516279878));
#54624=CARTESIAN_POINT('Ctrl Pts',(4.70109465465751,-0.636309800095162,
8.10115575541734));
#54625=CARTESIAN_POINT('Ctrl Pts',(4.6388360645949,-0.319434907277142,8.057667241152));
#54626=CARTESIAN_POINT('Ctrl Pts',(4.60413233863675,-0.158333333333323,
8.0260704578481));
#54627=CARTESIAN_POINT('Ctrl Pts',(4.60945901730333,0.158333333333325,7.9957454086737));
#54628=CARTESIAN_POINT('Ctrl Pts',(4.64966106351442,0.319434907277146,7.99617478942981));
#54629=CARTESIAN_POINT('Ctrl Pts',(4.72242009293445,0.636309800095168,7.97960917517307));
#54630=CARTESIAN_POINT('Ctrl Pts',(4.78943626148876,0.794772684000797,7.98127127696966));
#54631=CARTESIAN_POINT('Ctrl Pts',(4.85606191180836,1.06847604194508,7.94569709957012));
#54632=CARTESIAN_POINT('Ctrl Pts',(4.87937077991199,1.18514270861176,7.92377780620357));
#54633=CARTESIAN_POINT('Ctrl Pts',(4.89714874081958,1.3,7.89533796271355));
#54634=CARTESIAN_POINT('Ctrl Pts',(4.8706912457249,-1.30000000000236,8.13874397736797));
#54635=CARTESIAN_POINT('Ctrl Pts',(4.85688868177773,-1.18514270861336,8.15357144495233));
#54636=CARTESIAN_POINT('Ctrl Pts',(4.83764494620884,-1.06847604194588,8.1591651370575));
#54637=CARTESIAN_POINT('Ctrl Pts',(4.7806178724,-0.794772684000799,8.15075581626738));
#54638=CARTESIAN_POINT('Ctrl Pts',(4.71942401154056,-0.636309800095158,
8.11613756897579));
#54639=CARTESIAN_POINT('Ctrl Pts',(4.65752261305664,-0.31943490727714,8.07199190908468));
#54640=CARTESIAN_POINT('Ctrl Pts',(4.62236539069558,-0.158333333333322,
8.0388868963487));
#54641=CARTESIAN_POINT('Ctrl Pts',(4.62787715410413,0.158333333333325,8.00806696958337));
#54642=CARTESIAN_POINT('Ctrl Pts',(4.668801765522,0.319434907277146,8.00925309041465));
#54643=CARTESIAN_POINT('Ctrl Pts',(4.7414095381692,0.636309800095166,7.99285929145396));
#54644=CARTESIAN_POINT('Ctrl Pts',(4.80871779191284,0.794772684000793,7.99533965620724));
#54645=CARTESIAN_POINT('Ctrl Pts',(4.87272998284456,1.06847604194507,7.95798539139597));
#54646=CARTESIAN_POINT('Ctrl Pts',(4.89429019408294,1.18514270861175,7.93472762094081));
#54647=CARTESIAN_POINT('Ctrl Pts',(4.9097021109908,1.29999999999999,7.90438135715535));
#54648=CARTESIAN_POINT('Ctrl Pts',(4.87889684647338,-1.30000000000235,8.14643349039401));
#54649=CARTESIAN_POINT('Ctrl Pts',(4.86655780869544,-1.18514270861336,8.16306500747547));
#54650=CARTESIAN_POINT('Ctrl Pts',(4.84844221023227,-1.06847604194588,8.16983725152211));
#54651=CARTESIAN_POINT('Ctrl Pts',(4.79324654298962,-0.7947726840008,8.16270559700147));
#54652=CARTESIAN_POINT('Ctrl Pts',(4.73225201339823,-0.636309800095157,
8.12659044263502));
#54653=CARTESIAN_POINT('Ctrl Pts',(4.67064679511124,-0.31943490727714,8.08190437626722));
#54654=CARTESIAN_POINT('Ctrl Pts',(4.6348639598759,-0.158333333333322,8.04859156898635));
#54655=CARTESIAN_POINT('Ctrl Pts',(4.64046671223474,0.158333333333324,8.01753912185134));
#54656=CARTESIAN_POINT('Ctrl Pts',(4.68202664064609,0.319434907277145,8.01890020375431));
#54657=CARTESIAN_POINT('Ctrl Pts',(4.75468914238488,0.636309800095165,8.00216643618904));
#54658=CARTESIAN_POINT('Ctrl Pts',(4.82240570180082,0.794772684000792,8.0046151258808));
#54659=CARTESIAN_POINT('Ctrl Pts',(4.88460734747703,1.06847604194507,7.96596225571329));
#54660=CARTESIAN_POINT('Ctrl Pts',(4.90490036841996,1.18514270861175,7.94189610211271));
#54661=CARTESIAN_POINT('Ctrl Pts',(4.91856162269072,1.29999999999999,7.91049519017706));
#54662=CARTESIAN_POINT('Ctrl Pts',(4.88305998021748,-1.30000000000235,8.15012560460764));
#54663=CARTESIAN_POINT('Ctrl Pts',(4.87151822466341,-1.18514270861335,8.16749476044765));
#54664=CARTESIAN_POINT('Ctrl Pts',(4.85399470886098,-1.06847604194588,8.17478603452684));
#54665=CARTESIAN_POINT('Ctrl Pts',(4.79969281896955,-0.794772684000798,
8.16834841332337));
#54666=CARTESIAN_POINT('Ctrl Pts',(4.73859249823662,-0.636309800095156,
8.13200389578888));
#54667=CARTESIAN_POINT('Ctrl Pts',(4.67711069858125,-0.319434907277139,
8.08710327929875));
#54668=CARTESIAN_POINT('Ctrl Pts',(4.64116622640158,-0.158333333333322,
8.05328987531924));
#54669=CARTESIAN_POINT('Ctrl Pts',(4.64682226011323,0.158333333333324,8.02210546727675));
#54670=CARTESIAN_POINT('Ctrl Pts',(4.68861499160051,0.319434907277145,8.02378241015381));
#54671=CARTESIAN_POINT('Ctrl Pts',(4.76122617498029,0.636309800095164,8.00710189634627));
#54672=CARTESIAN_POINT('Ctrl Pts',(4.8290550323816,0.79477268400079,8.00980623275754));
#54673=CARTESIAN_POINT('Ctrl Pts',(4.8903791407941,1.06847604194507,7.970423587409));
#54674=CARTESIAN_POINT('Ctrl Pts',(4.91008229512971,1.18514270861175,7.94582590060862));
#54675=CARTESIAN_POINT('Ctrl Pts',(4.92294366955132,1.29999999999998,7.91367781490841));
#54676=CARTESIAN_POINT('Ctrl Pts',(4.88514455500464,-1.30000000000235,8.15196328232576));
#54677=CARTESIAN_POINT('Ctrl Pts',(4.87400495537845,-1.18514270861335,8.16969222727159));
#54678=CARTESIAN_POINT('Ctrl Pts',(4.85677856536373,-1.06847604194588,8.17724016881156));
#54679=CARTESIAN_POINT('Ctrl Pts',(4.80292045484665,-0.794772684000798,
8.17115726915921));
#54680=CARTESIAN_POINT('Ctrl Pts',(4.74175272104858,-0.636309800095156,
8.13473473304));
#54681=CARTESIAN_POINT('Ctrl Pts',(4.68032963434567,-0.319434907277139,
8.08973453534491));
#54682=CARTESIAN_POINT('Ctrl Pts',(4.64431371975998,-0.158333333333322,
8.05564697256633));
#54683=CARTESIAN_POINT('Ctrl Pts',(4.64999636724652,0.158333333333324,8.02439766002777));
#54684=CARTESIAN_POINT('Ctrl Pts',(4.69190028777524,0.319434907277145,8.02624679249682));
#54685=CARTESIAN_POINT('Ctrl Pts',(4.76448021785442,0.636309800095164,8.00960915225664));
#54686=CARTESIAN_POINT('Ctrl Pts',(4.83235724904279,0.794772684000791,8.01246456073939));
#54687=CARTESIAN_POINT('Ctrl Pts',(4.89324610269253,1.06847604194507,7.97270739073841));
#54688=CARTESIAN_POINT('Ctrl Pts',(4.91265872028842,1.18514270861175,7.94783152281172));
#54689=CARTESIAN_POINT('Ctrl Pts',(4.92512742688961,1.29999999999999,7.91528919270343));
#54690=CARTESIAN_POINT('Ctrl Pts',(4.88633804800046,-1.30000000000235,8.15300735731721));
#54691=CARTESIAN_POINT('Ctrl Pts',(4.87543043244414,-1.18514270861335,8.17093640497652));
#54692=CARTESIAN_POINT('Ctrl Pts',(4.85837471443863,-1.06847604194588,8.17862880124875));
#54693=CARTESIAN_POINT('Ctrl Pts',(4.80476924728013,-0.794772684000798,
8.17275106295702));
#54694=CARTESIAN_POINT('Ctrl Pts',(4.74355576934846,-0.636309800095156,
8.13630239380284));
#54695=CARTESIAN_POINT('Ctrl Pts',(4.6821652161533,-0.319434907277139,8.0912477084203));
#54696=CARTESIAN_POINT('Ctrl Pts',(4.64611367300213,-0.158333333333322,
8.05698977168253));
#54697=CARTESIAN_POINT('Ctrl Pts',(4.65181164585589,0.158333333333324,8.02570319836857));
#54698=CARTESIAN_POINT('Ctrl Pts',(4.69377602562051,0.319434907277145,8.02765895368757));
#54699=CARTESIAN_POINT('Ctrl Pts',(4.76633527724332,0.636309800095164,8.0110538625209));
#54700=CARTESIAN_POINT('Ctrl Pts',(4.83423660945324,0.79477268400079,8.01400531325613));
#54701=CARTESIAN_POINT('Ctrl Pts',(4.89487784889872,1.06847604194507,7.97403099752843));
#54702=CARTESIAN_POINT('Ctrl Pts',(4.91412607104847,1.18514270861175,7.9489914413801));
#54703=CARTESIAN_POINT('Ctrl Pts',(4.92637316977141,1.29999999999998,7.91621572916757));
#54704=CARTESIAN_POINT('Ctrl Pts',(4.89648125291073,-1.30000000000236,8.1618847443129));
#54705=CARTESIAN_POINT('Ctrl Pts',(4.88755289139152,-1.18514270861336,8.1814935536347));
#54706=CARTESIAN_POINT('Ctrl Pts',(4.8719501946499,-1.06847604194589,8.19040611650862));
#54707=CARTESIAN_POINT('Ctrl Pts',(4.82048579430827,-0.794772684000802,
8.18628545062815));
#54708=CARTESIAN_POINT('Ctrl Pts',(4.7588575532274,-0.636309800095158,8.14967904496894));
#54709=CARTESIAN_POINT('Ctrl Pts',(4.69772882947847,-0.31943490727714,8.10419982071705));
#54710=CARTESIAN_POINT('Ctrl Pts',(4.66137129118492,-0.158333333333322,
8.06850588104074));
#54711=CARTESIAN_POINT('Ctrl Pts',(4.66720410790064,0.158333333333325,8.03689346131535));
#54712=CARTESIAN_POINT('Ctrl Pts',(4.70970157980417,0.319434907277146,8.03970566614566));
#54713=CARTESIAN_POINT('Ctrl Pts',(4.78208575622587,0.636309800095167,8.02337817109365));
#54714=CARTESIAN_POINT('Ctrl Pts',(4.85017318446032,0.794772684000793,8.02719981142593));
#54715=CARTESIAN_POINT('Ctrl Pts',(4.90870759397174,1.06847604194507,7.98539139166514));
#54716=CARTESIAN_POINT('Ctrl Pts',(4.92656098233666,1.18514270861175,7.95895753979858));
#54717=CARTESIAN_POINT('Ctrl Pts',(4.93693038210267,1.29999999999999,7.92418715182528));
#54718=CARTESIAN_POINT('Ctrl Pts',(4.91551177580483,-1.30000000000243,8.1796774361804));
#54719=CARTESIAN_POINT('Ctrl Pts',(4.90997910059319,-1.18514270861342,8.2034115442133));
#54720=CARTESIAN_POINT('Ctrl Pts',(4.89695697654872,-1.06847604194594,8.21511380608156));
#54721=CARTESIAN_POINT('Ctrl Pts',(4.84957113987627,-0.794772684000837,
8.21435240042376));
#54722=CARTESIAN_POINT('Ctrl Pts',(4.7880382363761,-0.636309800095189,8.17525965214434));
#54723=CARTESIAN_POINT('Ctrl Pts',(4.72756392935862,-0.319434907277156,
8.12863812941445));
#54724=CARTESIAN_POINT('Ctrl Pts',(4.69012508813819,-0.158333333333331,
8.09152310390475));
#54725=CARTESIAN_POINT('Ctrl Pts',(4.69616504778515,0.158333333333333,8.05942743143656));
#54726=CARTESIAN_POINT('Ctrl Pts',(4.73980031308552,0.319434907277166,8.06355300046823));
#54727=CARTESIAN_POINT('Ctrl Pts',(4.81225887622818,0.636309800095201,8.046618523019));
#54728=CARTESIAN_POINT('Ctrl Pts',(4.8815204951006,0.794772684000832,8.04975140675556));
#54729=CARTESIAN_POINT('Ctrl Pts',(4.93590306301374,1.06847604194512,8.00490599430512));
#54730=CARTESIAN_POINT('Ctrl Pts',(4.9508094610885,1.18514270861181,7.97668237716761));
#54731=CARTESIAN_POINT('Ctrl Pts',(4.95708205866118,1.30000000000005,7.93964706025608));
#54732=CARTESIAN_POINT('Ctrl Pts',(4.9342581816127,-1.30000000000244,8.19708426160756));
#54733=CARTESIAN_POINT('Ctrl Pts',(4.93221572521055,-1.18514270861343,8.22447422101744));
#54734=CARTESIAN_POINT('Ctrl Pts',(4.92179501815014,-1.06847604194595,8.23874548314703));
#54735=CARTESIAN_POINT('Ctrl Pts',(4.87836566510154,-0.794772684000851,
8.24140813851867));
#54736=CARTESIAN_POINT('Ctrl Pts',(4.81647889550278,-0.636309800095196,
8.20100449682226));
#54737=CARTESIAN_POINT('Ctrl Pts',(4.75652394679049,-0.319434907277159,
8.15359245070489));
#54738=CARTESIAN_POINT('Ctrl Pts',(4.7181759471255,-0.158333333333332,8.11472494346454));
#54739=CARTESIAN_POINT('Ctrl Pts',(4.72452210841152,0.158333333333334,8.08191100418775));
#54740=CARTESIAN_POINT('Ctrl Pts',(4.76953814964653,0.319434907277167,8.08661121585654));
#54741=CARTESIAN_POINT('Ctrl Pts',(4.84176412499727,0.636309800095206,8.0699403196767));
#54742=CARTESIAN_POINT('Ctrl Pts',(4.91110009717076,0.79477268400084,8.07544025046478));
#54743=CARTESIAN_POINT('Ctrl Pts',(4.96159302088875,1.06847604194513,8.02697642301351));
#54744=CARTESIAN_POINT('Ctrl Pts',(4.97396758428922,1.18514270861182,7.99590387471389));
#54745=CARTESIAN_POINT('Ctrl Pts',(4.97686019535986,1.30000000000007,7.95473697325649));
#54746=CARTESIAN_POINT('Ctrl Pts',(4.94346631687566,-1.30000000000244,8.20619135799069));
#54747=CARTESIAN_POINT('Ctrl Pts',(4.94321747389921,-1.18514270861343,8.23526699291014));
#54748=CARTESIAN_POINT('Ctrl Pts',(4.93412052317187,-1.06847604194595,8.25074967063335));
#54749=CARTESIAN_POINT('Ctrl Pts',(4.89266384819064,-0.794772684000851,
8.25511530308793));
#54750=CARTESIAN_POINT('Ctrl Pts',(4.83045152777307,-0.636309800095196,
8.21442603970566));
#54751=CARTESIAN_POINT('Ctrl Pts',(4.77077828071587,-0.319434907277159,
8.16657178332084));
#54752=CARTESIAN_POINT('Ctrl Pts',(4.73214233677919,-0.158333333333332,
8.12643424340246));
#54753=CARTESIAN_POINT('Ctrl Pts',(4.73867559286303,0.158333333333334,8.09318929264053));
#54754=CARTESIAN_POINT('Ctrl Pts',(4.78422175451366,0.319434907277167,8.0985897035147));
#54755=CARTESIAN_POINT('Ctrl Pts',(4.85643493010519,0.636309800095206,8.08176584863399));
#54756=CARTESIAN_POINT('Ctrl Pts',(4.92620237914194,0.79477268400084,8.08735069514893));
#54757=CARTESIAN_POINT('Ctrl Pts',(4.9747053048224,1.06847604194513,8.03725889790454));
#54758=CARTESIAN_POINT('Ctrl Pts',(4.98569765033206,1.18514270861182,8.00512172787457));
#54759=CARTESIAN_POINT('Ctrl Pts',(4.98668722203483,1.30000000000007,7.9625302707577));
#54760=CARTESIAN_POINT('',(4.8959368873413,1.2,7.92959029267854));
#54761=CARTESIAN_POINT('Ctrl Pts',(4.8959368873413,1.2,7.92959029267854));
#54762=CARTESIAN_POINT('Ctrl Pts',(4.88797220813117,1.20916354636366,7.92086623504881));
#54763=CARTESIAN_POINT('Ctrl Pts',(4.88028989526128,1.21806687773866,7.91188259563126));
#54764=CARTESIAN_POINT('Ctrl Pts',(4.86522920737885,1.23542022164275,7.89477196315859));
#54765=CARTESIAN_POINT('Ctrl Pts',(4.86314220261871,1.23778099745235,7.89270625656617));
#54766=CARTESIAN_POINT('Ctrl Pts',(4.84481687043038,1.25867329971331,7.87296100721959));
#54767=CARTESIAN_POINT('Ctrl Pts',(4.83773131952392,1.26674820983433,7.86524036225158));
#54768=CARTESIAN_POINT('Ctrl Pts',(4.82529292629485,1.28086872210545,7.85193070389807));
#54769=CARTESIAN_POINT('Ctrl Pts',(4.81441133228405,1.29318854035898,7.84038199481636));
#54770=CARTESIAN_POINT('Ctrl Pts',(4.80835060740606,1.29999999999429,7.83424319965858));
#54771=CARTESIAN_POINT('',(4.87041241537771,0.653834841366681,8.0840717752332));
#54772=CARTESIAN_POINT('Ctrl Pts',(4.87041241541545,0.653834841365399,8.08407177523491));
#54773=CARTESIAN_POINT('Ctrl Pts',(4.87329721488191,0.717497006726158,8.06817921590771));
#54774=CARTESIAN_POINT('Ctrl Pts',(4.87561886639402,0.764618542304357,8.05505318984721));
#54775=CARTESIAN_POINT('Ctrl Pts',(4.88438527422149,0.949828857079461,8.0040620818735));
#54776=CARTESIAN_POINT('Ctrl Pts',(4.88934246800722,1.05665635942843,7.9738423354926));
#54777=CARTESIAN_POINT('Ctrl Pts',(4.8959368873413,1.2,7.92959029267854));
#54778=CARTESIAN_POINT('',(4.84356468978474,-0.653834841531101,8.22097066356995));
#54779=CARTESIAN_POINT('Ctrl Pts',(4.84356468978474,-0.653834841531103,
8.22097066356995));
#54780=CARTESIAN_POINT('Ctrl Pts',(4.81028563170247,-0.575993226556318,
8.19606516572056));
#54781=CARTESIAN_POINT('Ctrl Pts',(4.78259195720601,-0.493634718961504,
8.17437906484961));
#54782=CARTESIAN_POINT('Ctrl Pts',(4.74428736208887,-0.338122806465111,
8.14129310529133));
#54783=CARTESIAN_POINT('Ctrl Pts',(4.73158435908654,-0.265648779501229,
8.12870181591131));
#54784=CARTESIAN_POINT('Ctrl Pts',(4.71756129813914,-0.129709195779501,
8.10877449802887));
#54785=CARTESIAN_POINT('Ctrl Pts',(4.71484216847727,-0.0666211038089427,
8.10096227158569));
#54786=CARTESIAN_POINT('Ctrl Pts',(4.71704128756279,0.0595424094985919,
8.08781794729412));
#54787=CARTESIAN_POINT('Ctrl Pts',(4.72195866570481,0.122770513587566,8.08238767852916));
#54788=CARTESIAN_POINT('Ctrl Pts',(4.74093133359303,0.260121498042269,8.07400881902309));
#54789=CARTESIAN_POINT('Ctrl Pts',(4.75649446970959,0.333942046842514,8.07169269259132));
#54790=CARTESIAN_POINT('Ctrl Pts',(4.80133469428488,0.491203290822365,8.07254015000573));
#54791=CARTESIAN_POINT('Ctrl Pts',(4.83265376689795,0.574345776646004,8.07653115452104));
#54792=CARTESIAN_POINT('Ctrl Pts',(4.87041241535288,0.653834841383564,8.08407177517955));
#54793=CARTESIAN_POINT('',(4.8579715305892,-1.2,8.1500592655118));
#54794=CARTESIAN_POINT('Ctrl Pts',(4.8579715305892,-1.2,8.1500592655118));
#54795=CARTESIAN_POINT('Ctrl Pts',(4.85616916586142,-1.14986030831313,8.15927536060516));
#54796=CARTESIAN_POINT('Ctrl Pts',(4.85301485103969,-1.06105460662833,8.17530456062274));
#54797=CARTESIAN_POINT('Ctrl Pts',(4.84589300490481,-0.792168471237582,
8.2099540488437));
#54798=CARTESIAN_POINT('Ctrl Pts',(4.84486899479601,-0.738395515500054,
8.21478293857185));
#54799=CARTESIAN_POINT('Ctrl Pts',(4.84356468978474,-0.653834841531101,
8.22097066356995));
#54800=CARTESIAN_POINT('Ctrl Pts',(4.77352143851608,-1.29999999999999,8.05790038817305));
#54801=CARTESIAN_POINT('Ctrl Pts',(4.78821579301464,-1.28289249508473,8.0728526865888));
#54802=CARTESIAN_POINT('Ctrl Pts',(4.80235089926343,-1.26612407112286,8.08872140664403));
#54803=CARTESIAN_POINT('Ctrl Pts',(4.82249641224789,-1.2423446920112,8.11029336074994));
#54804=CARTESIAN_POINT('Ctrl Pts',(4.82684436345377,-1.23728814171469,8.11454897743682));
#54805=CARTESIAN_POINT('Ctrl Pts',(4.84402176769152,-1.21675291282038,8.13403542652456));
#54806=CARTESIAN_POINT('Ctrl Pts',(4.85107260119958,-1.20833011795947,8.14193421309319));
#54807=CARTESIAN_POINT('Ctrl Pts',(4.8579715305892,-1.2,8.1500592655118));
#54808=CARTESIAN_POINT('Origin',(0.,1.25,7.2));
#54809=CARTESIAN_POINT('Origin',(0.,1.2,7.2));
#54810=CARTESIAN_POINT('Origin',(0.,0.92691742076555,7.2));
#54811=CARTESIAN_POINT('Origin',(0.,0.653834841531101,7.2));
#54812=CARTESIAN_POINT('Origin',(0.,0.,7.2));
#54813=CARTESIAN_POINT('Origin',(0.,-0.653834841531101,7.2));
#54814=CARTESIAN_POINT('Origin',(0.,-0.926917420765551,7.2));
#54815=CARTESIAN_POINT('Origin',(0.,-1.2,7.2));
#54816=CARTESIAN_POINT('Origin',(0.,-1.25,7.2));
#54817=CARTESIAN_POINT('Ctrl Pts',(4.86571446294981,-1.30000000000085,8.53166235559583));
#54818=CARTESIAN_POINT('Ctrl Pts',(4.88213395050881,-1.18514270861236,8.49235062834033));
#54819=CARTESIAN_POINT('Ctrl Pts',(4.88516330785635,-1.06847604194541,8.45852087292604));
#54820=CARTESIAN_POINT('Ctrl Pts',(4.86122784987519,-0.794772684000851,
8.39303182191765));
#54821=CARTESIAN_POINT('Ctrl Pts',(4.79522055198899,-0.636309800095197,
8.36975685506468));
#54822=CARTESIAN_POINT('Ctrl Pts',(4.73609341170194,-0.319434907277159,
8.32501575423208));
#54823=CARTESIAN_POINT('Ctrl Pts',(4.69228837762394,-0.158333333333332,
8.31142398216115));
#54824=CARTESIAN_POINT('Ctrl Pts',(4.69984189087714,0.158333333333334,8.2783958937552));
#54825=CARTESIAN_POINT('Ctrl Pts',(4.75146299021043,0.319434907277167,8.25744308062087));
#54826=CARTESIAN_POINT('Ctrl Pts',(4.82544129359938,0.636309800095206,8.23799733826065));
#54827=CARTESIAN_POINT('Ctrl Pts',(4.89882489071899,0.79477268400084,8.22612987688632));
#54828=CARTESIAN_POINT('Ctrl Pts',(4.93492178514811,1.06847604194527,8.24698002939988));
#54829=CARTESIAN_POINT('Ctrl Pts',(4.93693489080205,1.1851427086121,8.26482422250729));
#54830=CARTESIAN_POINT('Ctrl Pts',(4.92533609403332,1.30000000000048,8.29148735027329));
#54831=CARTESIAN_POINT('Ctrl Pts',(4.85356720775251,-1.30000000000085,8.53478487530141));
#54832=CARTESIAN_POINT('Ctrl Pts',(4.86766876337789,-1.18514270861236,8.49600050856059));
#54833=CARTESIAN_POINT('Ctrl Pts',(4.86900238119364,-1.06847604194541,8.46258113483096));
#54834=CARTESIAN_POINT('Ctrl Pts',(4.84258681457994,-0.794772684000851,
8.39776990311183));
#54835=CARTESIAN_POINT('Ctrl Pts',(4.77700822871636,-0.636309800095197,
8.37459285932004));
#54836=CARTESIAN_POINT('Ctrl Pts',(4.71780718134389,-0.319434907277159,
8.32998628707835));
#54837=CARTESIAN_POINT('Ctrl Pts',(4.67477123304741,-0.158333333333332,
8.3159704706055));
#54838=CARTESIAN_POINT('Ctrl Pts',(4.68232035773856,0.158333333333334,8.28341222909386));
#54839=CARTESIAN_POINT('Ctrl Pts',(4.73316183806893,0.319434907277167,8.26350253105835));
#54840=CARTESIAN_POINT('Ctrl Pts',(4.80721762558706,0.636309800095206,8.2445753462594));
#54841=CARTESIAN_POINT('Ctrl Pts',(4.88018764438341,0.79477268400084,8.23283639981901));
#54842=CARTESIAN_POINT('Ctrl Pts',(4.91877933308295,1.06847604194527,8.25293316580915));
#54843=CARTESIAN_POINT('Ctrl Pts',(4.92249447744504,1.1851427086121,8.27020909591394));
#54844=CARTESIAN_POINT('Ctrl Pts',(4.91321985409419,1.30000000000048,8.29606181078497));
#54845=CARTESIAN_POINT('Ctrl Pts',(4.82936001910001,-1.30000000000095,8.54053438201199));
#54846=CARTESIAN_POINT('Ctrl Pts',(4.83869374469277,-1.18514270861245,8.50414804058056));
#54847=CARTESIAN_POINT('Ctrl Pts',(4.83655611686211,-1.06847604194549,8.47229936964699));
#54848=CARTESIAN_POINT('Ctrl Pts',(4.8051166476979,-0.79477268400091,8.40920549509364));
#54849=CARTESIAN_POINT('Ctrl Pts',(4.74057070959264,-0.636309800095242,
8.38388404752927));
#54850=CARTESIAN_POINT('Ctrl Pts',(4.68126380914895,-0.319434907277181,
8.33894697122637));
#54851=CARTESIAN_POINT('Ctrl Pts',(4.6397195201453,-0.158333333333344,8.32499215906552));
#54852=CARTESIAN_POINT('Ctrl Pts',(4.64725601130599,0.158333333333346,8.29321406701575));
#54853=CARTESIAN_POINT('Ctrl Pts',(4.69655683600114,0.319434907277193,8.27451647045124));
#54854=CARTESIAN_POINT('Ctrl Pts',(4.7707668114283,0.636309800095254,8.25650478146261));
#54855=CARTESIAN_POINT('Ctrl Pts',(4.84288041121132,0.794772684000897,8.24580151540382));
#54856=CARTESIAN_POINT('Ctrl Pts',(4.88647885739907,1.06847604194535,8.26438230695372));
#54857=CARTESIAN_POINT('Ctrl Pts',(4.89361505177938,1.18514270861218,8.28037652552305));
#54858=CARTESIAN_POINT('Ctrl Pts',(4.88901528866695,1.30000000000057,8.30432202648592));
#54859=CARTESIAN_POINT('Ctrl Pts',(4.804847149059,-1.30000000000139,8.54644403858434));
#54860=CARTESIAN_POINT('Ctrl Pts',(4.80955580396485,-1.18514270861285,8.51043725219642));
#54861=CARTESIAN_POINT('Ctrl Pts',(4.8040269923979,-1.06847604194585,8.47900494843386));
#54862=CARTESIAN_POINT('Ctrl Pts',(4.76760373609304,-0.794772684001179,
8.41695800871827));
#54863=CARTESIAN_POINT('Ctrl Pts',(4.70385131375091,-0.636309800095458,
8.39270228722005));
#54864=CARTESIAN_POINT('Ctrl Pts',(4.64436342255841,-0.319434907277289,
8.34837684794173));
#54865=CARTESIAN_POINT('Ctrl Pts',(4.6043649205092,-0.158333333333397,8.33379951860146));
#54866=CARTESIAN_POINT('Ctrl Pts',(4.61189316275056,0.158333333333399,8.30253910350606));
#54867=CARTESIAN_POINT('Ctrl Pts',(4.65965294569226,0.319434907277298,8.28459752774881));
#54868=CARTESIAN_POINT('Ctrl Pts',(4.73400064132595,0.636309800095468,8.26781120582232));
#54869=CARTESIAN_POINT('Ctrl Pts',(4.80519641332386,0.794772684001165,8.25934293293309));
#54870=CARTESIAN_POINT('Ctrl Pts',(4.85384625361791,1.06847604194571,8.27653965866762));
#54871=CARTESIAN_POINT('Ctrl Pts',(4.86444620305697,1.18514270861259,8.29107480451648));
#54872=CARTESIAN_POINT('Ctrl Pts',(4.86458738872603,1.30000000000101,8.31270127084519));
#54873=CARTESIAN_POINT('Ctrl Pts',(4.79233830189581,-1.30000000000142,8.54935194863464));
#54874=CARTESIAN_POINT('Ctrl Pts',(4.79459546837754,-1.18514270861288,8.51436530006081));
#54875=CARTESIAN_POINT('Ctrl Pts',(4.78728007149443,-1.06847604194588,8.48361409219813));
#54876=CARTESIAN_POINT('Ctrl Pts',(4.74826550489687,-0.794772684001197,
8.42235736561713));
#54877=CARTESIAN_POINT('Ctrl Pts',(4.68502149708521,-0.636309800095474,
8.39740911729828));
#54878=CARTESIAN_POINT('Ctrl Pts',(4.6254874340275,-0.319434907277297,8.35277492053589));
#54879=CARTESIAN_POINT('Ctrl Pts',(4.58629839263221,-0.158333333333401,
8.33765864174457));
#54880=CARTESIAN_POINT('Ctrl Pts',(4.59381754228615,0.158333333333403,8.30673962323839));
#54881=CARTESIAN_POINT('Ctrl Pts',(4.64074037977057,0.319434907277307,8.28993872672475));
#54882=CARTESIAN_POINT('Ctrl Pts',(4.71515318994323,0.636309800095484,8.27362628256271));
#54883=CARTESIAN_POINT('Ctrl Pts',(4.78591880090055,0.794772684001185,8.26513493816583));
#54884=CARTESIAN_POINT('Ctrl Pts',(4.83716058558056,1.06847604194574,8.28161897342502));
#54885=CARTESIAN_POINT('Ctrl Pts',(4.84953046676123,1.18514270861262,8.29564628708797));
#54886=CARTESIAN_POINT('Ctrl Pts',(4.85208955922982,1.30000000000105,8.31656558634388));
#54887=CARTESIAN_POINT('Ctrl Pts',(4.79158070392031,-1.30000000000142,8.5495235549734));
#54888=CARTESIAN_POINT('Ctrl Pts',(4.79368911312494,-1.18514270861288,8.51459945078696));
#54889=CARTESIAN_POINT('Ctrl Pts',(4.78626529793112,-1.06847604194588,8.48389016235608));
#54890=CARTESIAN_POINT('Ctrl Pts',(4.74709345442893,-0.794772684001196,
8.42268263027507));
#54891=CARTESIAN_POINT('Ctrl Pts',(4.68388019310939,-0.636309800095473,
8.39769404782994));
#54892=CARTESIAN_POINT('Ctrl Pts',(4.62434337779062,-0.319434907277297,
8.35304004667076));
#54893=CARTESIAN_POINT('Ctrl Pts',(4.58520366881382,-0.158333333333401,
8.3378870715479));
#54894=CARTESIAN_POINT('Ctrl Pts',(4.59272226060636,0.158333333333403,8.30698817777221));
#54895=CARTESIAN_POINT('Ctrl Pts',(4.63959412927933,0.319434907277307,8.29025879047028));
#54896=CARTESIAN_POINT('Ctrl Pts',(4.71401075228064,0.636309800095484,8.27397722462864));
#54897=CARTESIAN_POINT('Ctrl Pts',(4.78475025061342,0.794772684001185,8.26548651872526));
#54898=CARTESIAN_POINT('Ctrl Pts',(4.83614917978268,1.06847604194574,8.28192769191487));
#54899=CARTESIAN_POINT('Ctrl Pts',(4.84862638815205,1.18514270861262,8.29592383538026));
#54900=CARTESIAN_POINT('Ctrl Pts',(4.85133211297141,1.30000000000105,8.31679934764279));
#54901=CARTESIAN_POINT('Ctrl Pts',(4.79025491811528,-1.30000000000142,8.5498229553338));
#54902=CARTESIAN_POINT('Ctrl Pts',(4.79210326372372,-1.18514270861288,8.51500570025586));
#54903=CARTESIAN_POINT('Ctrl Pts',(4.78448988078939,-1.06847604194588,8.48436813993301));
#54904=CARTESIAN_POINT('Ctrl Pts',(4.74504295741298,-0.794772684001196,
8.42324517759365));
#54905=CARTESIAN_POINT('Ctrl Pts',(4.6818832785033,-0.636309800095473,8.39818804809511));
#54906=CARTESIAN_POINT('Ctrl Pts',(4.62234144669066,-0.319434907277297,
8.35350183815101));
#54907=CARTESIAN_POINT('Ctrl Pts',(4.58328782589623,-0.158333333333401,
8.33828810279069));
#54908=CARTESIAN_POINT('Ctrl Pts',(4.59080541024151,0.158333333333403,8.30742477131116));
#54909=CARTESIAN_POINT('Ctrl Pts',(4.63758835707064,0.319434907277307,8.29081652143042));
#54910=CARTESIAN_POINT('Ctrl Pts',(4.71201166433516,0.636309800095484,8.27458905607121));
#54911=CARTESIAN_POINT('Ctrl Pts',(4.78270525737022,0.794772684001185,8.26610317864001));
#54912=CARTESIAN_POINT('Ctrl Pts',(4.83437911060835,1.06847604194574,8.28247029593681));
#54913=CARTESIAN_POINT('Ctrl Pts',(4.84704412936208,1.18514270861262,8.29641178690816));
#54914=CARTESIAN_POINT('Ctrl Pts',(4.85000647050771,1.30000000000105,8.31721005023453));
#54915=CARTESIAN_POINT('Ctrl Pts',(4.78760459323741,-1.30000000000142,8.55040694471682));
#54916=CARTESIAN_POINT('Ctrl Pts',(4.78893359553989,-1.18514270861287,8.51579282764292));
#54917=CARTESIAN_POINT('Ctrl Pts',(4.78094149445432,-1.06847604194587,8.48529275713613));
#54918=CARTESIAN_POINT('Ctrl Pts',(4.74094452862561,-0.794772684001195,
8.42433576332957));
#54919=CARTESIAN_POINT('Ctrl Pts',(4.67789067928778,-0.636309800095472,
8.39915697652538));
#54920=CARTESIAN_POINT('Ctrl Pts',(4.61833799057227,-0.319434907277297,
8.35441543238267));
#54921=CARTESIAN_POINT('Ctrl Pts',(4.57945618696832,-0.158333333333401,
8.33908544628562));
#54922=CARTESIAN_POINT('Ctrl Pts',(4.58697165641103,0.158333333333403,8.30829237081323));
#54923=CARTESIAN_POINT('Ctrl Pts',(4.63357745927118,0.319434907277307,8.29191182788788));
#54924=CARTESIAN_POINT('Ctrl Pts',(4.70801385789431,0.636309800095483,8.27579888129089));
#54925=CARTESIAN_POINT('Ctrl Pts',(4.77861443131758,0.794772684001183,8.26734960385899));
#54926=CARTESIAN_POINT('Ctrl Pts',(4.83083801918334,1.06847604194574,8.28357264681678));
#54927=CARTESIAN_POINT('Ctrl Pts',(4.84387884673486,1.18514270861261,8.29740161341555));
#54928=CARTESIAN_POINT('Ctrl Pts',(4.84735484572544,1.30000000000104,8.31803719243965));
#54929=CARTESIAN_POINT('Ctrl Pts',(4.7823073456323,-1.30000000000142,8.55152432972443));
#54930=CARTESIAN_POINT('Ctrl Pts',(4.78260296703768,-1.18514270861287,8.51725343981543));
#54931=CARTESIAN_POINT('Ctrl Pts',(4.77385649639675,-1.06847604194587,8.4869912924405));
#54932=CARTESIAN_POINT('Ctrl Pts',(4.73276135799954,-0.794772684001193,
8.42634067528254));
#54933=CARTESIAN_POINT('Ctrl Pts',(4.66991234341115,-0.63630980009547,8.40099325973968));
#54934=CARTESIAN_POINT('Ctrl Pts',(4.61033295745482,-0.319434907277296,
8.35620033016389));
#54935=CARTESIAN_POINT('Ctrl Pts',(4.57179084334347,-0.1583333333334,8.3406966133674));
#54936=CARTESIAN_POINT('Ctrl Pts',(4.57930142550142,0.158333333333402,8.31004323747091));
#54937=CARTESIAN_POINT('Ctrl Pts',(4.62555820738196,0.319434907277305,8.29401937448729));
#54938=CARTESIAN_POINT('Ctrl Pts',(4.70002040071875,0.63630980009548,8.27815427484438));
#54939=CARTESIAN_POINT('Ctrl Pts',(4.77042932246061,0.794772684001181,8.26991151323194));
#54940=CARTESIAN_POINT('Ctrl Pts',(4.82375149465376,1.06847604194573,8.28586807724426));
#54941=CARTESIAN_POINT('Ctrl Pts',(4.83754449001921,1.18514270861261,8.29945840142342));
#54942=CARTESIAN_POINT('Ctrl Pts',(4.8420492881889,1.30000000000104,8.31973204446977));
#54943=CARTESIAN_POINT('Ctrl Pts',(4.7747469216486,-1.30000000000139,8.55297979474255));
#54944=CARTESIAN_POINT('Ctrl Pts',(4.77358950033188,-1.18514270861285,8.51894026910112));
#54945=CARTESIAN_POINT('Ctrl Pts',(4.76377912280778,-1.06847604194585,8.48886494552462));
#54946=CARTESIAN_POINT('Ctrl Pts',(4.72112512831088,-0.794772684001178,
8.42854303132101));
#54947=CARTESIAN_POINT('Ctrl Pts',(4.65854136944843,-0.636309800095459,
8.40325147775868));
#54948=CARTESIAN_POINT('Ctrl Pts',(4.59890417967612,-0.31943490727729,8.35863062757503));
#54949=CARTESIAN_POINT('Ctrl Pts',(4.56083048148958,-0.158333333333398,
8.34313951944532));
#54950=CARTESIAN_POINT('Ctrl Pts',(4.56833232593917,0.158333333333399,8.31267406642545));
#54951=CARTESIAN_POINT('Ctrl Pts',(4.61411391094263,0.319434907277299,8.29672355810624));
#54952=CARTESIAN_POINT('Ctrl Pts',(4.68861212424133,0.636309800095469,8.28127684869272));
#54953=CARTESIAN_POINT('Ctrl Pts',(4.75872285528296,0.794772684001166,8.27390069142831));
#54954=CARTESIAN_POINT('Ctrl Pts',(4.8136117200716,1.06847604194571,8.28954194395389));
#54955=CARTESIAN_POINT('Ctrl Pts',(4.82848228909124,1.18514270861259,8.30271669851244));
#54956=CARTESIAN_POINT('Ctrl Pts',(4.83446407139639,1.30000000000102,8.32229568897672));
#54957=CARTESIAN_POINT('Ctrl Pts',(4.76567097848328,-1.30000000000139,8.55472712245201));
#54958=CARTESIAN_POINT('Ctrl Pts',(4.76276845286623,-1.18514270861284,8.520959348338));
#54959=CARTESIAN_POINT('Ctrl Pts',(4.75168150209505,-1.06847604194585,8.4910915121608));
#54960=CARTESIAN_POINT('Ctrl Pts',(4.70716076848207,-0.794772684001175,
8.43110047236531));
#54961=CARTESIAN_POINT('Ctrl Pts',(4.6449053265792,-0.636309800095455,8.40577518511714));
#54962=CARTESIAN_POINT('Ctrl Pts',(4.58520363494991,-0.319434907277288,
8.36130772192686));
#54963=CARTESIAN_POINT('Ctrl Pts',(4.54769257845807,-0.158333333333397,
8.34583811065994));
#54964=CARTESIAN_POINT('Ctrl Pts',(4.55517888930291,0.158333333333399,8.31563506213017));
#54965=CARTESIAN_POINT('Ctrl Pts',(4.60037871346206,0.319434907277297,8.29986928442809));
#54966=CARTESIAN_POINT('Ctrl Pts',(4.67491709128006,0.636309800095465,8.28491811559864));
#54967=CARTESIAN_POINT('Ctrl Pts',(4.74467985764269,0.794772684001162,8.27841169407885));
#54968=CARTESIAN_POINT('Ctrl Pts',(4.80144680785053,1.06847604194571,8.29373247175476));
#54969=CARTESIAN_POINT('Ctrl Pts',(4.81760758149724,1.18514270861258,8.30648005005701));
#54970=CARTESIAN_POINT('Ctrl Pts',(4.8253568194685,1.30000000000101,8.32534340969635));
#54971=CARTESIAN_POINT('Ctrl Pts',(4.75354538128605,-1.30000000000136,8.55733659235512));
#54972=CARTESIAN_POINT('Ctrl Pts',(4.74827750446818,-1.18514270861282,8.52434007795708));
#54973=CARTESIAN_POINT('Ctrl Pts',(4.7354669278131,-1.06847604194583,8.49497482578842));
#54974=CARTESIAN_POINT('Ctrl Pts',(4.68844678745697,-0.794772684001161,
8.43552416096171));
#54975=CARTESIAN_POINT('Ctrl Pts',(4.62668088567543,-0.636309800095444,
8.40961132816583));
#54976=CARTESIAN_POINT('Ctrl Pts',(4.56694039954845,-0.319434907277282,
8.36478405455998));
#54977=CARTESIAN_POINT('Ctrl Pts',(4.53022662309791,-0.158333333333394,
8.34871583916773));
#54978=CARTESIAN_POINT('Ctrl Pts',(4.53769481795827,0.158333333333396,8.31884484338701));
#54979=CARTESIAN_POINT('Ctrl Pts',(4.58206034218961,0.319434907277293,8.30419551308267));
#54980=CARTESIAN_POINT('Ctrl Pts',(4.65663911943659,0.636309800095455,8.28990208029129));
#54981=CARTESIAN_POINT('Ctrl Pts',(4.72596785410255,0.794772684001148,8.28367740836966));
#54982=CARTESIAN_POINT('Ctrl Pts',(4.78524673561844,1.06847604194569,8.2984751364591));
#54983=CARTESIAN_POINT('Ctrl Pts',(4.80312837789116,1.18514270861256,8.31076137562564));
#54984=CARTESIAN_POINT('Ctrl Pts',(4.81323203112739,1.30000000000098,8.32892846577867));
#54985=CARTESIAN_POINT('Ctrl Pts',(4.73837355545878,-1.3000000000013,8.5606497694795));
#54986=CARTESIAN_POINT('Ctrl Pts',(4.73015115072486,-1.18514270861277,8.52857893756578));
#54987=CARTESIAN_POINT('Ctrl Pts',(4.71518579190561,-1.06847604194578,8.49983387381159));
#54988=CARTESIAN_POINT('Ctrl Pts',(4.66503524636295,-0.794772684001123,
8.44111021587534));
#54989=CARTESIAN_POINT('Ctrl Pts',(4.60386429694356,-0.636309800095414,
8.4146314440745));
#54990=CARTESIAN_POINT('Ctrl Pts',(4.54407057347046,-0.319434907277268,
8.36944529380717));
#54991=CARTESIAN_POINT('Ctrl Pts',(4.50835673161846,-0.158333333333386,
8.35269305007124));
#54992=CARTESIAN_POINT('Ctrl Pts',(4.51581536651864,0.158333333333388,8.32309148513968));
#54993=CARTESIAN_POINT('Ctrl Pts',(4.5591620075005,0.319434907277275,8.30942565772959));
#54994=CARTESIAN_POINT('Ctrl Pts',(4.63379367323015,0.636309800095423,8.29597871598314));
#54995=CARTESIAN_POINT('Ctrl Pts',(4.70255993381258,0.79477268400111,8.2905739348661));
#54996=CARTESIAN_POINT('Ctrl Pts',(4.76496472644855,1.06847604194564,8.30490136991313));
#54997=CARTESIAN_POINT('Ctrl Pts',(4.78499194360679,1.18514270861251,8.31663757162872));
#54998=CARTESIAN_POINT('Ctrl Pts',(4.7980336555166,1.30000000000093,8.33390815931181));
#54999=CARTESIAN_POINT('Ctrl Pts',(4.71416590268322,-1.30000000000123,8.56515386171744));
#55000=CARTESIAN_POINT('Ctrl Pts',(4.70126884943509,-1.1851427086127,8.53391407158018));
#55001=CARTESIAN_POINT('Ctrl Pts',(4.6828939690976,-1.06847604194572,8.50570019546546));
#55002=CARTESIAN_POINT('Ctrl Pts',(4.62778944322383,-0.79477268400108,8.44751096419801));
#55003=CARTESIAN_POINT('Ctrl Pts',(4.56758615172801,-0.636309800095381,
8.42009138315412));
#55004=CARTESIAN_POINT('Ctrl Pts',(4.50765180405554,-0.319434907277252,
8.37491070370344));
#55005=CARTESIAN_POINT('Ctrl Pts',(4.47342625780318,-0.158333333333378,
8.35817574772211));
#55006=CARTESIAN_POINT('Ctrl Pts',(4.48079197929825,0.15833333333338,8.32974691733967));
#55007=CARTESIAN_POINT('Ctrl Pts',(4.52249044329594,0.319434907277261,8.31789680836533));
#55008=CARTESIAN_POINT('Ctrl Pts',(4.59720988426097,0.636309800095392,8.30548824584704));
#55009=CARTESIAN_POINT('Ctrl Pts',(4.66512072251762,0.794772684001071,8.30029297084602));
#55010=CARTESIAN_POINT('Ctrl Pts',(4.73256761032737,1.06847604194558,8.31349399926102));
#55011=CARTESIAN_POINT('Ctrl Pts',(4.75604532845754,1.18514270861244,8.3243512014707));
#55012=CARTESIAN_POINT('Ctrl Pts',(4.77380550613851,1.30000000000085,8.34035136983552));
#55013=CARTESIAN_POINT('Ctrl Pts',(4.69297040123395,-1.30000000000116,8.5690572456906));
#55014=CARTESIAN_POINT('Ctrl Pts',(4.67599576681304,-1.18514270861264,8.53842933539974));
#55015=CARTESIAN_POINT('Ctrl Pts',(4.65463186400387,-1.06847604194566,8.51072878569245));
#55016=CARTESIAN_POINT('Ctrl Pts',(4.5951368866336,-0.794772684001033,8.4534977629572));
#55017=CARTESIAN_POINT('Ctrl Pts',(4.53562583044008,-0.636309800095344,
8.42662864582605));
#55018=CARTESIAN_POINT('Ctrl Pts',(4.47556129846,-0.319434907277232,8.38150467738444));
#55019=CARTESIAN_POINT('Ctrl Pts',(4.44274572059359,-0.158333333333369,
8.36393984045405));
#55020=CARTESIAN_POINT('Ctrl Pts',(4.45013328538506,0.158333333333371,8.33535479141151));
#55021=CARTESIAN_POINT('Ctrl Pts',(4.49048336803185,0.319434907277241,8.32363781472797));
#55022=CARTESIAN_POINT('Ctrl Pts',(4.56529653139247,0.636309800095353,8.31195535572491));
#55023=CARTESIAN_POINT('Ctrl Pts',(4.63236078486284,0.794772684001023,8.30841184376824));
#55024=CARTESIAN_POINT('Ctrl Pts',(4.70417877575155,1.06847604194552,8.32125124762597));
#55025=CARTESIAN_POINT('Ctrl Pts',(4.73066645536988,1.18514270861238,8.33147975320106));
#55026=CARTESIAN_POINT('Ctrl Pts',(4.75255446746963,1.30000000000078,8.34637906216803));
#55027=CARTESIAN_POINT('Ctrl Pts',(4.66873124297124,-1.30000000000112,8.57357009359638));
#55028=CARTESIAN_POINT('Ctrl Pts',(4.6470379636447,-1.1851427086126,8.54401642914705));
#55029=CARTESIAN_POINT('Ctrl Pts',(4.6222509633327,-1.06847604194563,8.51686786821153));
#55030=CARTESIAN_POINT('Ctrl Pts',(4.55784091961646,-0.794772684001013,
8.45970553165579));
#55031=CARTESIAN_POINT('Ctrl Pts',(4.49947416501879,-0.636309800095329,
8.43045783746727));
#55032=CARTESIAN_POINT('Ctrl Pts',(4.43931646189135,-0.319434907277226,
8.38487602674139));
#55033=CARTESIAN_POINT('Ctrl Pts',(4.40791159835173,-0.158333333333365,
8.36800874541527));
#55034=CARTESIAN_POINT('Ctrl Pts',(4.4151748412205,0.158333333333367,8.340614333267));
#55035=CARTESIAN_POINT('Ctrl Pts',(4.45390149438311,0.319434907277231,8.32995536807035));
#55036=CARTESIAN_POINT('Ctrl Pts',(4.52873464474054,0.636309800095336,8.32000527084179));
#55037=CARTESIAN_POINT('Ctrl Pts',(4.59480833328335,0.794772684001006,8.31860316319239));
#55038=CARTESIAN_POINT('Ctrl Pts',(4.67164168169231,1.0684760419455,8.3308669948441));
#55039=CARTESIAN_POINT('Ctrl Pts',(4.70159534229404,1.18514270861235,8.34013252429138));
#55040=CARTESIAN_POINT('Ctrl Pts',(4.72824435392736,1.30000000000075,8.35335502488365));
#55041=CARTESIAN_POINT('Ctrl Pts',(4.64455763696824,-1.30000000000109,8.57733417227618));
#55042=CARTESIAN_POINT('Ctrl Pts',(4.61828683665992,-1.18514270861258,8.5476972423875));
#55043=CARTESIAN_POINT('Ctrl Pts',(4.59013172517861,-1.0684760419456,8.52065311316078));
#55044=CARTESIAN_POINT('Ctrl Pts',(4.52073464948133,-0.794772684000996,
8.46416565270476));
#55045=CARTESIAN_POINT('Ctrl Pts',(4.46301202251514,-0.636309800095314,
8.43666670116118));
#55046=CARTESIAN_POINT('Ctrl Pts',(4.40271193562758,-0.319434907277218,
8.39105221918814));
#55047=CARTESIAN_POINT('Ctrl Pts',(4.37306118991602,-0.158333333333361,
8.37213853899525));
#55048=CARTESIAN_POINT('Ctrl Pts',(4.38032974813031,0.158333333333363,8.3447461412619));
#55049=CARTESIAN_POINT('Ctrl Pts',(4.41734870731225,0.319434907277224,8.33576102998205));
#55050=CARTESIAN_POINT('Ctrl Pts',(4.49225133334755,0.636309800095321,8.32661065767595));
#55051=CARTESIAN_POINT('Ctrl Pts',(4.55746683780738,0.794772684000987,8.32525270685827));
#55052=CARTESIAN_POINT('Ctrl Pts',(4.63929995689959,1.06847604194547,8.3371877182811));
#55053=CARTESIAN_POINT('Ctrl Pts',(4.67267882086693,1.18514270861232,8.34615086292065));
#55054=CARTESIAN_POINT('Ctrl Pts',(4.70401402376247,1.30000000000072,8.35891092799055));
#55055=CARTESIAN_POINT('Ctrl Pts',(4.62194387170432,-1.30000000000104,8.58059186454667));
#55056=CARTESIAN_POINT('Ctrl Pts',(4.59121967798365,-1.18514270861253,8.5520201756949));
#55057=CARTESIAN_POINT('Ctrl Pts',(4.55984620022608,-1.06847604194556,8.5254566912415));
#55058=CARTESIAN_POINT('Ctrl Pts',(4.48586721434936,-0.794772684000964,
8.46872908204751));
#55059=CARTESIAN_POINT('Ctrl Pts',(4.42933519750432,-0.636309800095286,
8.43828658202844));
#55060=CARTESIAN_POINT('Ctrl Pts',(4.36898105086931,-0.319434907277203,
8.39200530408134));
#55061=CARTESIAN_POINT('Ctrl Pts',(4.34063582129055,-0.158333333333354,
8.3738316313857));
#55062=CARTESIAN_POINT('Ctrl Pts',(4.347703736149,0.158333333333356,8.34811560974449));
#55063=CARTESIAN_POINT('Ctrl Pts',(4.38307446740542,0.319434907277211,8.34101388650739));
#55064=CARTESIAN_POINT('Ctrl Pts',(4.45791184029579,0.636309800095295,8.33401595714426));
#55065=CARTESIAN_POINT('Ctrl Pts',(4.52220357437114,0.794772684000952,8.33446497927006));
#55066=CARTESIAN_POINT('Ctrl Pts',(4.60874194005757,1.06847604194542,8.34592495844054));
#55067=CARTESIAN_POINT('Ctrl Pts',(4.64537970251158,1.18514270861227,8.35401420591919));
#55068=CARTESIAN_POINT('Ctrl Pts',(4.68119597547639,1.30000000000066,8.36523210052768));
#55069=CARTESIAN_POINT('Ctrl Pts',(4.60387932238281,-1.30000000000102,8.58288177294599));
#55070=CARTESIAN_POINT('Ctrl Pts',(4.56967256179496,-1.18514270861251,8.55453114462641));
#55071=CARTESIAN_POINT('Ctrl Pts',(4.53575217283572,-1.06847604194555,8.52813075555004));
#55072=CARTESIAN_POINT('Ctrl Pts',(4.45805086433994,-0.794772684000954,
8.47164601819983));
#55073=CARTESIAN_POINT('Ctrl Pts',(4.40215448199083,-0.636309800095278,
8.44131145778521));
#55074=CARTESIAN_POINT('Ctrl Pts',(4.3417232110165,-0.319434907277199,8.3947729050014));
#55075=CARTESIAN_POINT('Ctrl Pts',(4.31460517397489,-0.158333333333352,
8.37588671898424));
#55076=CARTESIAN_POINT('Ctrl Pts',(4.32166562292817,0.158333333333354,8.35014628586842));
#55077=CARTESIAN_POINT('Ctrl Pts',(4.35582539932203,0.319434907277208,8.34343069045799));
#55078=CARTESIAN_POINT('Ctrl Pts',(4.43067640655517,0.636309800095287,8.33725541085188));
#55079=CARTESIAN_POINT('Ctrl Pts',(4.49420718713358,0.794772684000941,8.33880717160197));
#55080=CARTESIAN_POINT('Ctrl Pts',(4.58444004850034,1.06847604194541,8.35062203874628));
#55081=CARTESIAN_POINT('Ctrl Pts',(4.6236371583146,1.18514270861225,8.35864762097586));
#55082=CARTESIAN_POINT('Ctrl Pts',(4.66297291571444,1.30000000000065,8.3695845672322));
#55083=CARTESIAN_POINT('Ctrl Pts',(4.59493977879337,-1.30000000000102,8.58342037655318));
#55084=CARTESIAN_POINT('Ctrl Pts',(4.55898890691848,-1.18514270861251,8.55517513605593));
#55085=CARTESIAN_POINT('Ctrl Pts',(4.52379498416204,-1.06847604194554,8.5288359222857));
#55086=CARTESIAN_POINT('Ctrl Pts',(4.44423868596545,-0.794772684000949,
8.47239037237364));
#55087=CARTESIAN_POINT('Ctrl Pts',(4.3886850447675,-0.636309800095275,8.44191394461041));
#55088=CARTESIAN_POINT('Ctrl Pts',(4.3282078191952,-0.319434907277198,8.39529412085592));
#55089=CARTESIAN_POINT('Ctrl Pts',(4.30168710817396,-0.158333333333352,
8.376177369922));
#55090=CARTESIAN_POINT('Ctrl Pts',(4.30869497686896,0.158333333333354,8.35080710552607));
#55091=CARTESIAN_POINT('Ctrl Pts',(4.34218746912544,0.319434907277206,8.34476661947023));
#55092=CARTESIAN_POINT('Ctrl Pts',(4.41701272620334,0.636309800095284,8.33927511988198));
#55093=CARTESIAN_POINT('Ctrl Pts',(4.48017134140349,0.794772684000937,8.34139007320928));
#55094=CARTESIAN_POINT('Ctrl Pts',(4.5722811881534,1.06847604194541,8.35308146316041));
#55095=CARTESIAN_POINT('Ctrl Pts',(4.61277899908719,1.18514270861225,8.36084944837583));
#55096=CARTESIAN_POINT('Ctrl Pts',(4.65390368130292,1.30000000000064,8.37132464930549));
#55097=CARTESIAN_POINT('Ctrl Pts',(4.58581707049687,-1.30000000000101,8.5850986834178));
#55098=CARTESIAN_POINT('Ctrl Pts',(4.54812928518205,-1.1851427086125,8.55694519581164));
#55099=CARTESIAN_POINT('Ctrl Pts',(4.51167300653039,-1.06847604194554,8.53061718102351));
#55100=CARTESIAN_POINT('Ctrl Pts',(4.43029673654555,-0.794772684000947,
8.47401140735594));
#55101=CARTESIAN_POINT('Ctrl Pts',(4.37512370956665,-0.636309800095272,
8.44312610006982));
#55102=CARTESIAN_POINT('Ctrl Pts',(4.31464442091295,-0.319434907277196,
8.3961375598802));
#55103=CARTESIAN_POINT('Ctrl Pts',(4.28874071971753,-0.158333333333351,
8.3766748156319));
#55104=CARTESIAN_POINT('Ctrl Pts',(4.29571856586336,0.158333333333353,8.3515037707682));
#55105=CARTESIAN_POINT('Ctrl Pts',(4.32854762139582,0.319434907277205,8.34606041006935));
#55106=CARTESIAN_POINT('Ctrl Pts',(4.40334720226197,0.636309800095282,8.34123768071327));
#55107=CARTESIAN_POINT('Ctrl Pts',(4.46612092809186,0.794772684000934,8.34401580888935));
#55108=CARTESIAN_POINT('Ctrl Pts',(4.56010178861599,1.0684760419454,8.35566243892948));
#55109=CARTESIAN_POINT('Ctrl Pts',(4.60189886394712,1.18514270861224,8.36320630783392));
#55110=CARTESIAN_POINT('Ctrl Pts',(4.64481218242255,1.30000000000064,8.37325265104859));
#55111=CARTESIAN_POINT('Ctrl Pts',(4.57976379072891,-1.30000000000101,8.58604105405601));
#55112=CARTESIAN_POINT('Ctrl Pts',(4.5409029819475,-1.18514270861251,8.55803781082764));
#55113=CARTESIAN_POINT('Ctrl Pts',(4.50359549349079,-1.06847604194554,8.53177312762207));
#55114=CARTESIAN_POINT('Ctrl Pts',(4.42099621250913,-0.794772684000947,
8.47511287663577));
#55115=CARTESIAN_POINT('Ctrl Pts',(4.36609611660324,-0.636309800095273,
8.44383161138913));
#55116=CARTESIAN_POINT('Ctrl Pts',(4.30561120695117,-0.319434907277196,
8.39662026242517));
#55117=CARTESIAN_POINT('Ctrl Pts',(4.28009950000537,-0.158333333333351,
8.37705031023949));
#55118=CARTESIAN_POINT('Ctrl Pts',(4.28705418197413,0.158333333333353,8.35202817045905));
#55119=CARTESIAN_POINT('Ctrl Pts',(4.31945284716805,0.319434907277205,8.34690681074705));
#55120=CARTESIAN_POINT('Ctrl Pts',(4.39424189157949,0.636309800095282,8.34247599005533));
#55121=CARTESIAN_POINT('Ctrl Pts',(4.45676575258676,0.794772684000934,8.34561202054393));
#55122=CARTESIAN_POINT('Ctrl Pts',(4.55198658002281,1.0684760419454,8.35730905319397));
#55123=CARTESIAN_POINT('Ctrl Pts',(4.59464305750395,1.18514270861224,8.36477760337297));
#55124=CARTESIAN_POINT('Ctrl Pts',(4.63873844454854,1.30000000000064,8.37465149171453));
#55125=CARTESIAN_POINT('Ctrl Pts',(4.55272395833052,-1.300000000001,8.58902013595507));
#55126=CARTESIAN_POINT('Ctrl Pts',(4.50863897250943,-1.18514270861249,8.56133756355169));
#55127=CARTESIAN_POINT('Ctrl Pts',(4.46752661973699,-1.06847604194553,8.53519270549119));
#55128=CARTESIAN_POINT('Ctrl Pts',(4.37941623735034,-0.794772684000935,
8.47834528086133));
#55129=CARTESIAN_POINT('Ctrl Pts',(4.32563627330862,-0.636309800095265,
8.44600322061239));
#55130=CARTESIAN_POINT('Ctrl Pts',(4.26502966611551,-0.319434907277193,
8.39842680825674));
#55131=CARTESIAN_POINT('Ctrl Pts',(4.24119970548086,-0.158333333333349,
8.37893073249655));
#55132=CARTESIAN_POINT('Ctrl Pts',(4.24805168854086,0.158333333333351,8.35452321283523));
#55133=CARTESIAN_POINT('Ctrl Pts',(4.27863088493474,0.319434907277202,8.35002401984986));
#55134=CARTESIAN_POINT('Ctrl Pts',(4.3534037771156,0.636309800095275,8.34704434662279));
#55135=CARTESIAN_POINT('Ctrl Pts',(4.41477543889416,0.794772684000924,8.35178927068111));
#55136=CARTESIAN_POINT('Ctrl Pts',(4.51551564193555,1.06847604194539,8.36419369067576));
#55137=CARTESIAN_POINT('Ctrl Pts',(4.56200224101305,1.18514270861223,8.37166838660108));
#55138=CARTESIAN_POINT('Ctrl Pts',(4.61136873806383,1.30000000000062,8.38124836466505));
#55139=CARTESIAN_POINT('Ctrl Pts',(4.5151925571782,-1.30000000000092,8.59274412866428));
#55140=CARTESIAN_POINT('Ctrl Pts',(4.46392074810623,-1.18514270861242,8.56502773770619));
#55141=CARTESIAN_POINT('Ctrl Pts',(4.41759507396831,-1.06847604194547,8.53861206670473));
#55142=CARTESIAN_POINT('Ctrl Pts',(4.32200006045904,-0.794772684000893,
8.48059150556247));
#55143=CARTESIAN_POINT('Ctrl Pts',(4.26994723219476,-0.63630980009523,8.44614168876008));
#55144=CARTESIAN_POINT('Ctrl Pts',(4.2092355775166,-0.319434907277175,8.39769428151512));
#55145=CARTESIAN_POINT('Ctrl Pts',(4.1876899933838,-0.158333333333341,8.37830484137755));
#55146=CARTESIAN_POINT('Ctrl Pts',(4.19425108882492,0.158333333333343,8.35548232070467));
#55147=CARTESIAN_POINT('Ctrl Pts',(4.22206620441759,0.319434907277185,8.35330808608328));
#55148=CARTESIAN_POINT('Ctrl Pts',(4.29673623293127,0.63630980009524,8.35270348350687));
#55149=CARTESIAN_POINT('Ctrl Pts',(4.35663864633831,0.794772684000882,8.35888172484033));
#55150=CARTESIAN_POINT('Ctrl Pts',(4.46510943585546,1.06847604194533,8.37153350165183));
#55151=CARTESIAN_POINT('Ctrl Pts',(4.51694046916774,1.18514270861216,8.37865665368745));
#55152=CARTESIAN_POINT('Ctrl Pts',(4.57364955024915,1.30000000000055,8.38742647237151));
#55153=CARTESIAN_POINT('Ctrl Pts',(4.47343222775881,-1.3000000000009,8.59504533441471));
#55154=CARTESIAN_POINT('Ctrl Pts',(4.41421631652258,-1.18514270861241,8.56655289837235));
#55155=CARTESIAN_POINT('Ctrl Pts',(4.36211950350135,-1.06847604194545,8.53934631629306));
#55156=CARTESIAN_POINT('Ctrl Pts',(4.2582119845381,-0.794772684000882,8.4794642489208));
#55157=CARTESIAN_POINT('Ctrl Pts',(4.20788743033015,-0.636309800095223,
8.44374706396478));
#55158=CARTESIAN_POINT('Ctrl Pts',(4.14724168103829,-0.319434907277172,
8.39349114738577));
#55159=CARTESIAN_POINT('Ctrl Pts',(4.12869895428878,-0.158333333333339,
8.3723767125966));
#55160=CARTESIAN_POINT('Ctrl Pts',(4.13506288582316,0.158333333333341,8.35034892732963));
#55161=CARTESIAN_POINT('Ctrl Pts',(4.15967453768392,0.31943490727718,8.35037750099606));
#55162=CARTESIAN_POINT('Ctrl Pts',(4.23388406413583,0.636309800095232,8.35384577337839));
#55163=CARTESIAN_POINT('Ctrl Pts',(4.29165071350381,0.794772684000874,8.36416771399849));
#55164=CARTESIAN_POINT('Ctrl Pts',(4.40846370800721,1.06847604194532,8.37947686697347));
#55165=CARTESIAN_POINT('Ctrl Pts',(4.46620340952472,1.18514270861215,8.38712836816309));
#55166=CARTESIAN_POINT('Ctrl Pts',(4.5311187955872,1.30000000000053,8.39580460547946));
#55167=CARTESIAN_POINT('Ctrl Pts',(4.45248023998025,-1.30000000000089,8.59655638746898));
#55168=CARTESIAN_POINT('Ctrl Pts',(4.38926946308294,-1.1851427086124,8.56782729269431));
#55169=CARTESIAN_POINT('Ctrl Pts',(4.33431432026877,-1.06847604194544,8.54013571994062));
#55170=CARTESIAN_POINT('Ctrl Pts',(4.22642911289548,-0.794772684000875,
8.47855953062353));
#55171=CARTESIAN_POINT('Ctrl Pts',(4.17742023988668,-0.636309800095217,
8.4401428888402));
#55172=CARTESIAN_POINT('Ctrl Pts',(4.11682467017945,-0.319434907277169,
8.38890277567568));
#55173=CARTESIAN_POINT('Ctrl Pts',(4.09936599852457,-0.158333333333337,
8.36882989779298));
#55174=CARTESIAN_POINT('Ctrl Pts',(4.10550426669319,0.158333333333339,8.34773080031627));
#55175=CARTESIAN_POINT('Ctrl Pts',(4.12864650391549,0.319434907277176,8.34824411924068));
#55176=CARTESIAN_POINT('Ctrl Pts',(4.2026714803712,0.636309800095225,8.353370960919));
#55177=CARTESIAN_POINT('Ctrl Pts',(4.25938213523715,0.794772684000867,8.36556525651938));
#55178=CARTESIAN_POINT('Ctrl Pts',(4.38038199558138,1.06847604194531,8.38183854958373));
#55179=CARTESIAN_POINT('Ctrl Pts',(4.44107950063504,1.18514270861214,8.38959222333433));
#55180=CARTESIAN_POINT('Ctrl Pts',(4.51009815468601,1.30000000000052,8.39805546525291));
#55181=CARTESIAN_POINT('Ctrl Pts',(4.44055346921691,-1.30000000000089,8.59708300700727));
#55182=CARTESIAN_POINT('Ctrl Pts',(4.37512897133373,-1.1851427086124,8.56774417847339));
#55183=CARTESIAN_POINT('Ctrl Pts',(4.31855986272212,-1.06847604194544,8.53957731078554));
#55184=CARTESIAN_POINT('Ctrl Pts',(4.20833162594993,-0.794772684000876,
8.4772136756684));
#55185=CARTESIAN_POINT('Ctrl Pts',(4.15973807352451,-0.636309800095216,
8.4388551336058));
#55186=CARTESIAN_POINT('Ctrl Pts',(4.0991733537175,-0.319434907277169,8.38710636932283));
#55187=CARTESIAN_POINT('Ctrl Pts',(4.08263878805536,-0.158333333333337,
8.36637619752324));
#55188=CARTESIAN_POINT('Ctrl Pts',(4.08874703354869,0.158333333333339,8.34535216591385));
#55189=CARTESIAN_POINT('Ctrl Pts',(4.1109595054656,0.319434907277176,8.34642176979204));
#55190=CARTESIAN_POINT('Ctrl Pts',(4.18484285157782,0.636309800095225,8.35256881810733));
#55191=CARTESIAN_POINT('Ctrl Pts',(4.24094387836209,0.794772684000865,8.36565943751016));
#55192=CARTESIAN_POINT('Ctrl Pts',(4.36429193579309,1.06847604194531,8.38295709174074));
#55193=CARTESIAN_POINT('Ctrl Pts',(4.4266554629292,1.18514270861214,8.39110489681365));
#55194=CARTESIAN_POINT('Ctrl Pts',(4.49798971363549,1.30000000000052,8.39991299338431));
#55195=CARTESIAN_POINT('Ctrl Pts',(4.42874610728218,-1.30000000000089,8.59716779009637));
#55196=CARTESIAN_POINT('Ctrl Pts',(4.36104944410423,-1.18514270861239,8.56782645212229));
#55197=CARTESIAN_POINT('Ctrl Pts',(4.30286558845658,-1.06847604194544,8.5394506370321));
#55198=CARTESIAN_POINT('Ctrl Pts',(4.19042573069578,-0.794772684000873,
8.47612737862547));
#55199=CARTESIAN_POINT('Ctrl Pts',(4.14268582717973,-0.636309800095214,
8.43593245973611));
#55200=CARTESIAN_POINT('Ctrl Pts',(4.08216704826761,-0.319434907277167,
8.38356446522101));
#55201=CARTESIAN_POINT('Ctrl Pts',(4.06617938619645,-0.158333333333336,
8.36352866686382));
#55202=CARTESIAN_POINT('Ctrl Pts',(4.07211627433835,0.158333333333338,8.34315532356739));
#55203=CARTESIAN_POINT('Ctrl Pts',(4.0935029512946,0.319434907277174,8.34450734638869));
#55204=CARTESIAN_POINT('Ctrl Pts',(4.16721035297765,0.636309800095221,8.35193477966307));
#55205=CARTESIAN_POINT('Ctrl Pts',(4.22263710270724,0.794772684000862,8.36643754302171));
#55206=CARTESIAN_POINT('Ctrl Pts',(4.34825873408589,1.0684760419453,8.38477500098801));
#55207=CARTESIAN_POINT('Ctrl Pts',(4.41225549120837,1.18514270861213,8.39320114282303));
#55208=CARTESIAN_POINT('Ctrl Pts',(4.48587205596967,1.30000000000051,8.40211582040922));
#55209=CARTESIAN_POINT('Ctrl Pts',(4.41383823973829,-1.30000000000088,8.59752605734597));
#55210=CARTESIAN_POINT('Ctrl Pts',(4.34323575450361,-1.18514270861238,8.5676056254189));
#55211=CARTESIAN_POINT('Ctrl Pts',(4.28296381514232,-1.06847604194543,8.53861966994724));
#55212=CARTESIAN_POINT('Ctrl Pts',(4.1675892054439,-0.794772684000868,8.47381514174061));
#55213=CARTESIAN_POINT('Ctrl Pts',(4.12081646532826,-0.636309800095211,
8.43166487740207));
#55214=CARTESIAN_POINT('Ctrl Pts',(4.0601312471902,-0.319434907277166,8.37952336556475));
#55215=CARTESIAN_POINT('Ctrl Pts',(4.04456692395272,-0.158333333333336,
8.36214229211));
#55216=CARTESIAN_POINT('Ctrl Pts',(4.05031201861363,0.158333333333338,8.34253290146348));
#55217=CARTESIAN_POINT('Ctrl Pts',(4.07096892152584,0.319434907277174,8.34241060896167));
#55218=CARTESIAN_POINT('Ctrl Pts',(4.1446856098719,0.63630980009522,8.35031938332042));
#55219=CARTESIAN_POINT('Ctrl Pts',(4.19927279717264,0.794772684000859,8.36638813371899));
#55220=CARTESIAN_POINT('Ctrl Pts',(4.3279741058351,1.0684760419453,8.38579543790554));
#55221=CARTESIAN_POINT('Ctrl Pts',(4.394144356726,1.18514270861212,8.39456864998641));
#55222=CARTESIAN_POINT('Ctrl Pts',(4.47077483084128,1.3000000000005,8.40371437127727));
#55223=CARTESIAN_POINT('Ctrl Pts',(4.39909825262287,-1.30000000000087,8.59776299484767));
#55224=CARTESIAN_POINT('Ctrl Pts',(4.32598568401036,-1.18514270861238,8.56674430457492));
#55225=CARTESIAN_POINT('Ctrl Pts',(4.26385091414587,-1.06847604194543,8.5371202391769));
#55226=CARTESIAN_POINT('Ctrl Pts',(4.14566807694991,-0.794772684000864,
8.47190458428794));
#55227=CARTESIAN_POINT('Ctrl Pts',(4.09914404087926,-0.636309800095205,
8.43126500260843));
#55228=CARTESIAN_POINT('Ctrl Pts',(4.03826094217273,-0.319434907277162,
8.37989489122064));
#55229=CARTESIAN_POINT('Ctrl Pts',(4.0235202967205,-0.158333333333334,8.36307402300566));
#55230=CARTESIAN_POINT('Ctrl Pts',(4.02935455541677,0.158333333333336,8.34294364536773));
#55231=CARTESIAN_POINT('Ctrl Pts',(4.04944030504608,0.319434907277171,8.34091036272037));
#55232=CARTESIAN_POINT('Ctrl Pts',(4.12320374117167,0.636309800095214,8.3486767622445));
#55233=CARTESIAN_POINT('Ctrl Pts',(4.17689422261378,0.794772684000851,8.36628209985493));
#55234=CARTESIAN_POINT('Ctrl Pts',(4.30834589610362,1.06847604194529,8.38657626165297));
#55235=CARTESIAN_POINT('Ctrl Pts',(4.37648195465194,1.18514270861211,8.39564439436043));
#55236=CARTESIAN_POINT('Ctrl Pts',(4.45585351305934,1.30000000000049,8.40499606910577));
#55237=CARTESIAN_POINT('Ctrl Pts',(4.38139541625333,-1.30000000000087,8.59735867632509));
#55238=CARTESIAN_POINT('Ctrl Pts',(4.30490212107633,-1.18514270861237,8.56477350564691));
#55239=CARTESIAN_POINT('Ctrl Pts',(4.24018872966067,-1.06847604194542,8.53441534828401));
#55240=CARTESIAN_POINT('Ctrl Pts',(4.11790178387139,-0.79477268400086,8.46942677791799));
#55241=CARTESIAN_POINT('Ctrl Pts',(4.07117551004531,-0.636309800095203,
8.4322641765055));
#55242=CARTESIAN_POINT('Ctrl Pts',(4.00965947048976,-0.319434907277162,
8.38299063618185));
#55243=CARTESIAN_POINT('Ctrl Pts',(3.99606948519409,-0.158333333333334,
8.36682478193899));
#55244=CARTESIAN_POINT('Ctrl Pts',(4.00186652210145,0.158333333333336,8.34676496522745));
#55245=CARTESIAN_POINT('Ctrl Pts',(4.02082206384393,0.31943490727717,8.343799130353));
#55246=CARTESIAN_POINT('Ctrl Pts',(4.09502514480978,0.636309800095212,8.35032173930797));
#55247=CARTESIAN_POINT('Ctrl Pts',(4.14852626078949,0.794772684000848,8.36633918891102));
#55248=CARTESIAN_POINT('Ctrl Pts',(4.28409749953885,1.06847604194528,8.38658611297483));
#55249=CARTESIAN_POINT('Ctrl Pts',(4.35491742327389,1.18514270861211,8.3960546780065));
#55250=CARTESIAN_POINT('Ctrl Pts',(4.43787350489881,1.3000000000005,8.40622766486509));
#55251=CARTESIAN_POINT('Ctrl Pts',(4.36932387841482,-1.30000000000085,8.59718401041862));
#55252=CARTESIAN_POINT('Ctrl Pts',(4.29080148664772,-1.18514270861236,8.56222163109241));
#55253=CARTESIAN_POINT('Ctrl Pts',(4.22452488361658,-1.06847604194541,8.53088546759122));
#55254=CARTESIAN_POINT('Ctrl Pts',(4.09970289376746,-0.794772684000851,
8.46686994510332));
#55255=CARTESIAN_POINT('Ctrl Pts',(4.05265002448005,-0.636309800095197,
8.43625327523035));
#55256=CARTESIAN_POINT('Ctrl Pts',(3.99084012998883,-0.319434907277159,
8.39044390410473));
#55257=CARTESIAN_POINT('Ctrl Pts',(3.97832338063956,-0.158333333333332,
8.37427477954486));
#55258=CARTESIAN_POINT('Ctrl Pts',(3.98412215794982,0.158333333333334,8.35438222413835));
#55259=CARTESIAN_POINT('Ctrl Pts',(4.00209599199945,0.319434907277167,8.35146503522703));
#55260=CARTESIAN_POINT('Ctrl Pts',(4.07641358158954,0.636309800095206,8.35511244653024));
#55261=CARTESIAN_POINT('Ctrl Pts',(4.12975510290133,0.79477268400084,8.36561273460513));
#55262=CARTESIAN_POINT('Ctrl Pts',(4.2678860136409,1.06847604194527,8.38482320588403));
#55263=CARTESIAN_POINT('Ctrl Pts',(4.34039737044288,1.1851427086121,8.39497038038826));
#55264=CARTESIAN_POINT('Ctrl Pts',(4.42562833104232,1.30000000000048,8.40694922819818));
#55265=CARTESIAN_POINT('Ctrl Pts',(4.36108289177536,-1.30000000000085,8.59965012915573));
#55266=CARTESIAN_POINT('Ctrl Pts',(4.28280795672178,-1.18514270861236,8.56464391562799));
#55267=CARTESIAN_POINT('Ctrl Pts',(4.21670728203312,-1.06847604194541,8.53360435815366));
#55268=CARTESIAN_POINT('Ctrl Pts',(4.09212647700321,-0.794772684000851,
8.47106053995604));
#55269=CARTESIAN_POINT('Ctrl Pts',(4.04497787349014,-0.636309800095197,
8.44300783150171));
#55270=CARTESIAN_POINT('Ctrl Pts',(3.98316982931346,-0.319434907277159,
8.39888504076963));
#55271=CARTESIAN_POINT('Ctrl Pts',(3.97060749458542,-0.158333333333332,
8.38269018459881));
#55272=CARTESIAN_POINT('Ctrl Pts',(3.97642822268415,0.158333333333334,8.36303343689645));
#55273=CARTESIAN_POINT('Ctrl Pts',(3.99446677770813,0.319434907277167,8.36065783751042));
#55274=CARTESIAN_POINT('Ctrl Pts',(4.06883296350448,0.636309800095206,8.36252854962085));
#55275=CARTESIAN_POINT('Ctrl Pts',(4.12234304385769,0.79477268400084,8.36938354588133));
#55276=CARTESIAN_POINT('Ctrl Pts',(4.26021093575307,1.06847604194527,8.38727435958102));
#55277=CARTESIAN_POINT('Ctrl Pts',(4.33251297633895,1.1851427086121,8.39744311267129));
#55278=CARTESIAN_POINT('Ctrl Pts',(4.41743915561804,1.30000000000048,8.41003634852119));
#55279=CARTESIAN_POINT('Ctrl Pts',(4.36108289177477,-1.3,8.59965012915547));
#55280=CARTESIAN_POINT('Ctrl Pts',(4.28280795672145,-1.18514270861178,8.56464391562783));
#55281=CARTESIAN_POINT('Ctrl Pts',(4.21670728203298,-1.06847604194512,8.53360435815359));
#55282=CARTESIAN_POINT('Ctrl Pts',(4.09212647700321,-0.794772684000851,
8.47106053995604));
#55283=CARTESIAN_POINT('Ctrl Pts',(4.04497787349014,-0.636309800095197,
8.44300783150172));
#55284=CARTESIAN_POINT('Ctrl Pts',(3.98316982931346,-0.319434907277159,
8.39888504076963));
#55285=CARTESIAN_POINT('Ctrl Pts',(3.97060749458543,-0.158333333333332,
8.38269018459881));
#55286=CARTESIAN_POINT('Ctrl Pts',(3.97642822268415,0.158333333333334,8.36303343689646));
#55287=CARTESIAN_POINT('Ctrl Pts',(3.99446677770813,0.319434907277167,8.36065783751042));
#55288=CARTESIAN_POINT('Ctrl Pts',(4.06883296350448,0.636309800095206,8.36252854962085));
#55289=CARTESIAN_POINT('Ctrl Pts',(4.12234304385769,0.79477268400084,8.36938354588133));
#55290=CARTESIAN_POINT('Ctrl Pts',(4.26021093575299,1.06847604194511,8.38727435958101));
#55291=CARTESIAN_POINT('Ctrl Pts',(4.33251297633875,1.18514270861178,8.39744311267126));
#55292=CARTESIAN_POINT('Ctrl Pts',(4.41743915561768,1.3,8.41003634852114));
#55293=CARTESIAN_POINT('',(4.76940206616454,-1.2,8.52487883644709));
#55294=CARTESIAN_POINT('Ctrl Pts',(4.76940206616454,-1.2,8.52487883644709));
#55295=CARTESIAN_POINT('Ctrl Pts',(4.74086940653868,-1.22420816645153,8.53714660115925));
#55296=CARTESIAN_POINT('Ctrl Pts',(4.71399385696744,-1.24658523341453,8.54972059636386));
#55297=CARTESIAN_POINT('Ctrl Pts',(4.69025100715547,-1.26662254821489,8.55981762870885));
#55298=CARTESIAN_POINT('Ctrl Pts',(4.67047629062826,-1.28318703090522,8.56846418154303));
#55299=CARTESIAN_POINT('Ctrl Pts',(4.65060554698671,-1.30000000000007,8.57636043474656));
#55300=CARTESIAN_POINT('',(4.80892752503401,-0.653834841367355,8.37333544163683));
#55301=CARTESIAN_POINT('Ctrl Pts',(4.80892752506904,-0.653834841366079,
8.37333544165056));
#55302=CARTESIAN_POINT('Ctrl Pts',(4.80510631376661,-0.717372755970661,
8.38899671596228));
#55303=CARTESIAN_POINT('Ctrl Pts',(4.80185727169085,-0.764980891039073,
8.40205461129384));
#55304=CARTESIAN_POINT('Ctrl Pts',(4.78917211258712,-0.949603287575588,
8.45202527125908));
#55305=CARTESIAN_POINT('Ctrl Pts',(4.78137785082631,-1.05619298999675,8.4817674737032));
#55306=CARTESIAN_POINT('Ctrl Pts',(4.76940206616454,-1.2,8.52487883644709));
#55307=CARTESIAN_POINT('',(4.84008270153004,0.653834841531101,8.23735213035386));
#55308=CARTESIAN_POINT('Ctrl Pts',(4.84008270153004,0.653834841531101,8.23735213035386));
#55309=CARTESIAN_POINT('Ctrl Pts',(4.79955227883107,0.5759960847206,8.24656828401657));
#55310=CARTESIAN_POINT('Ctrl Pts',(4.76543198768065,0.493633454934372,8.25510837225716));
#55311=CARTESIAN_POINT('Ctrl Pts',(4.71698053238237,0.338119094433763,8.26975736934253));
#55312=CARTESIAN_POINT('Ctrl Pts',(4.70025310872036,0.265645306504652,8.27610002608688));
#55313=CARTESIAN_POINT('Ctrl Pts',(4.67933681317188,0.129705370528769,8.28860475229142));
#55314=CARTESIAN_POINT('Ctrl Pts',(4.67367570084384,0.0666195825707109,
8.2946347965237));
#55315=CARTESIAN_POINT('Ctrl Pts',(4.67033844848027,-0.0595394781896691,
8.30753682247028));
#55316=CARTESIAN_POINT('Ctrl Pts',(4.67262159856367,-0.122765359287329,
8.31449795558557));
#55317=CARTESIAN_POINT('Ctrl Pts',(4.68654652654254,-0.260118360054571,
8.32986539262948));
#55318=CARTESIAN_POINT('Ctrl Pts',(4.69982349924885,-0.333937574098211,
8.33830433699626));
#55319=CARTESIAN_POINT('Ctrl Pts',(4.74113217604531,-0.491200648055129,
8.35576690161105));
#55320=CARTESIAN_POINT('Ctrl Pts',(4.77136431588038,-0.574341701776784,
8.36486586118048));
#55321=CARTESIAN_POINT('Ctrl Pts',(4.80892752498969,-0.653834841384169,
8.37333544167558));
#55322=CARTESIAN_POINT('',(4.82444304868815,1.2,8.30781283164827));
#55323=CARTESIAN_POINT('Ctrl Pts',(4.82444304868815,1.2,8.30781283164826));
#55324=CARTESIAN_POINT('Ctrl Pts',(4.82709025840723,1.13751278178995,8.29628442886868));
#55325=CARTESIAN_POINT('Ctrl Pts',(4.83082368709463,1.03911229509008,8.27981174430919));
#55326=CARTESIAN_POINT('Ctrl Pts',(4.83770053806196,0.793513023910657,8.24849002828812));
#55327=CARTESIAN_POINT('Ctrl Pts',(4.83876380524827,0.737991207933235,8.24350584314984));
#55328=CARTESIAN_POINT('Ctrl Pts',(4.84008270153004,0.653834841531101,8.23735213035386));
#55329=CARTESIAN_POINT('Ctrl Pts',(4.70979663593523,1.30000000000007,8.35772002147865));
#55330=CARTESIAN_POINT('Ctrl Pts',(4.72902725870907,1.28316203921417,8.35002540406659));
#55331=CARTESIAN_POINT('Ctrl Pts',(4.74814123467411,1.26659312888534,8.34147687556873));
#55332=CARTESIAN_POINT('Ctrl Pts',(4.78056818711222,1.23822793610611,8.32771710635259));
#55333=CARTESIAN_POINT('Ctrl Pts',(4.80199451884191,1.21941459056863,8.31882500817011));
#55334=CARTESIAN_POINT('Ctrl Pts',(4.82444304868815,1.2,8.30781283164826));
#55335=CARTESIAN_POINT('Ctrl Pts',(4.36108289177477,-1.3,8.59965012915547));
#55336=CARTESIAN_POINT('Ctrl Pts',(4.28280795672145,-1.18514270861178,8.56464391562783));
#55337=CARTESIAN_POINT('Ctrl Pts',(4.21670728203298,-1.06847604194512,8.53360435815359));
#55338=CARTESIAN_POINT('Ctrl Pts',(4.09212647700321,-0.794772684000851,
8.47106053995605));
#55339=CARTESIAN_POINT('Ctrl Pts',(4.04497787349015,-0.636309800095197,
8.44300783150172));
#55340=CARTESIAN_POINT('Ctrl Pts',(3.98316982931346,-0.319434907277159,
8.39888504076964));
#55341=CARTESIAN_POINT('Ctrl Pts',(3.97060749458543,-0.158333333333332,
8.38269018459882));
#55342=CARTESIAN_POINT('Ctrl Pts',(3.97642822268415,0.158333333333334,8.36303343689646));
#55343=CARTESIAN_POINT('Ctrl Pts',(3.99446677770813,0.319434907277167,8.36065783751042));
#55344=CARTESIAN_POINT('Ctrl Pts',(4.06883296350448,0.636309800095206,8.36252854962085));
#55345=CARTESIAN_POINT('Ctrl Pts',(4.12234304385769,0.794772684000841,8.36938354588133));
#55346=CARTESIAN_POINT('Ctrl Pts',(4.26021093575299,1.06847604194511,8.38727435958102));
#55347=CARTESIAN_POINT('Ctrl Pts',(4.33251297633875,1.18514270861178,8.39744311267126));
#55348=CARTESIAN_POINT('Ctrl Pts',(4.41743915561768,1.3,8.41003634852114));
#55349=CARTESIAN_POINT('Ctrl Pts',(4.33573021748671,-1.3,8.67228862570577));
#55350=CARTESIAN_POINT('Ctrl Pts',(4.25817731391276,-1.18514270861178,8.63570774538836));
#55351=CARTESIAN_POINT('Ctrl Pts',(4.19261998989961,-1.06847604194512,8.60359091403708));
#55352=CARTESIAN_POINT('Ctrl Pts',(4.06888164522439,-0.794772684000851,
8.53970745480723));
#55353=CARTESIAN_POINT('Ctrl Pts',(4.02167596618816,-0.636309800095197,
8.51237010663451));
#55354=CARTESIAN_POINT('Ctrl Pts',(3.96004957503508,-0.319434907277159,
8.46888894301598));
#55355=CARTESIAN_POINT('Ctrl Pts',(3.94727563345509,-0.158333333333332,
8.45391747327181));
#55356=CARTESIAN_POINT('Ctrl Pts',(3.95343774500623,0.158333333333334,8.4343716477771));
#55357=CARTESIAN_POINT('Ctrl Pts',(3.97202419499029,0.319434907277167,8.43088192859436));
#55358=CARTESIAN_POINT('Ctrl Pts',(4.04691448012462,0.636309800095206,8.43234032643418));
#55359=CARTESIAN_POINT('Ctrl Pts',(4.10079886363324,0.794772684000841,8.43858303591896));
#55360=CARTESIAN_POINT('Ctrl Pts',(4.2385608990303,1.06847604194511,8.45805282775219));
#55361=CARTESIAN_POINT('Ctrl Pts',(4.3106693138487,1.18514270861178,8.46941248723032));
#55362=CARTESIAN_POINT('Ctrl Pts',(4.39525406294861,1.3,8.48370405472888));
#55363=CARTESIAN_POINT('Ctrl Pts',(4.31037754319865,-1.3,8.74492712225608));
#55364=CARTESIAN_POINT('Ctrl Pts',(4.23354667110408,-1.18514270861178,8.70677157514888));
#55365=CARTESIAN_POINT('Ctrl Pts',(4.16853269776624,-1.06847604194512,8.67357746992056));
#55366=CARTESIAN_POINT('Ctrl Pts',(4.04563681344557,-0.794772684000851,
8.60835436965841));
#55367=CARTESIAN_POINT('Ctrl Pts',(3.99837405888618,-0.636309800095197,
8.58173238176729));
#55368=CARTESIAN_POINT('Ctrl Pts',(3.93692932075669,-0.319434907277159,
8.53889284526232));
#55369=CARTESIAN_POINT('Ctrl Pts',(3.92394377232475,-0.158333333333332,
8.5251447619448));
#55370=CARTESIAN_POINT('Ctrl Pts',(3.93044726732831,0.158333333333334,8.50570985865775));
#55371=CARTESIAN_POINT('Ctrl Pts',(3.94958161227244,0.319434907277167,8.50110601967831));
#55372=CARTESIAN_POINT('Ctrl Pts',(4.02499599674477,0.636309800095206,8.50215210324751));
#55373=CARTESIAN_POINT('Ctrl Pts',(4.07925468340879,0.794772684000841,8.50778252595658));
#55374=CARTESIAN_POINT('Ctrl Pts',(4.21691086230761,1.06847604194511,8.52883129592335));
#55375=CARTESIAN_POINT('Ctrl Pts',(4.28882565135864,1.18514270861178,8.54138186178938));
#55376=CARTESIAN_POINT('Ctrl Pts',(4.37306897027954,1.3,8.55737176093662));
#55377=CARTESIAN_POINT('Ctrl Pts',(4.28502486891058,-1.3,8.81756561880638));
#55378=CARTESIAN_POINT('Ctrl Pts',(4.20891602829539,-1.18514270861178,8.77783540490941));
#55379=CARTESIAN_POINT('Ctrl Pts',(4.14444540563287,-1.06847604194512,8.74356402580405));
#55380=CARTESIAN_POINT('Ctrl Pts',(4.02239198166675,-0.794772684000851,
8.67700128450959));
#55381=CARTESIAN_POINT('Ctrl Pts',(3.9750721515842,-0.636309800095197,8.65109465690008));
#55382=CARTESIAN_POINT('Ctrl Pts',(3.91380906647831,-0.319434907277159,
8.60889674750867));
#55383=CARTESIAN_POINT('Ctrl Pts',(3.90061191119441,-0.158333333333332,
8.59637205061779));
#55384=CARTESIAN_POINT('Ctrl Pts',(3.90745678965039,0.158333333333334,8.5770480695384));
#55385=CARTESIAN_POINT('Ctrl Pts',(3.9271390295546,0.319434907277167,8.57133011076225));
#55386=CARTESIAN_POINT('Ctrl Pts',(4.00307751336492,0.636309800095206,8.57196388006084));
#55387=CARTESIAN_POINT('Ctrl Pts',(4.05771050318434,0.794772684000841,8.57698201599421));
#55388=CARTESIAN_POINT('Ctrl Pts',(4.19526082558493,1.06847604194511,8.59960976409452));
#55389=CARTESIAN_POINT('Ctrl Pts',(4.26698198886859,1.18514270861178,8.61335123634844));
#55390=CARTESIAN_POINT('Ctrl Pts',(4.35088387761047,1.3,8.63103946714436));
#55391=CARTESIAN_POINT('Ctrl Pts',(4.28502486891058,-1.3,8.81756561880638));
#55392=CARTESIAN_POINT('Ctrl Pts',(4.20891602829539,-1.18514270861178,8.77783540490941));
#55393=CARTESIAN_POINT('Ctrl Pts',(4.14444540563287,-1.06847604194512,8.74356402580405));
#55394=CARTESIAN_POINT('Ctrl Pts',(4.02239198166675,-0.794772684000851,
8.67700128450959));
#55395=CARTESIAN_POINT('Ctrl Pts',(3.9750721515842,-0.636309800095197,8.65109465690008));
#55396=CARTESIAN_POINT('Ctrl Pts',(3.91380906647831,-0.319434907277159,
8.60889674750867));
#55397=CARTESIAN_POINT('Ctrl Pts',(3.90061191119441,-0.158333333333332,
8.59637205061778));
#55398=CARTESIAN_POINT('Ctrl Pts',(3.90745678965039,0.158333333333334,8.5770480695384));
#55399=CARTESIAN_POINT('Ctrl Pts',(3.9271390295546,0.319434907277167,8.57133011076225));
#55400=CARTESIAN_POINT('Ctrl Pts',(4.00307751336492,0.636309800095206,8.57196388006084));
#55401=CARTESIAN_POINT('Ctrl Pts',(4.05771050318434,0.79477268400084,8.5769820159942));
#55402=CARTESIAN_POINT('Ctrl Pts',(4.19526082558492,1.06847604194511,8.59960976409452));
#55403=CARTESIAN_POINT('Ctrl Pts',(4.26698198886859,1.18514270861178,8.61335123634844));
#55404=CARTESIAN_POINT('Ctrl Pts',(4.35088387761047,1.3,8.63103946714436));
#55405=CARTESIAN_POINT('Ctrl Pts',(4.28502486891387,-1.30000000000496,8.8175656188081));
#55406=CARTESIAN_POINT('Ctrl Pts',(4.20891602829725,-1.18514270861514,8.77783540491039));
#55407=CARTESIAN_POINT('Ctrl Pts',(4.14444540563363,-1.06847604194682,8.74356402580447));
#55408=CARTESIAN_POINT('Ctrl Pts',(4.02239198166675,-0.794772684000851,
8.67700128450959));
#55409=CARTESIAN_POINT('Ctrl Pts',(3.9750721515842,-0.636309800095197,8.65109465690009));
#55410=CARTESIAN_POINT('Ctrl Pts',(3.91380906647831,-0.319434907277159,
8.60889674750867));
#55411=CARTESIAN_POINT('Ctrl Pts',(3.90061191119441,-0.158333333333332,
8.59637205061778));
#55412=CARTESIAN_POINT('Ctrl Pts',(3.90745678965039,0.158333333333334,8.5770480695384));
#55413=CARTESIAN_POINT('Ctrl Pts',(3.9271390295546,0.319434907277167,8.57133011076225));
#55414=CARTESIAN_POINT('Ctrl Pts',(4.00307751336492,0.636309800095206,8.57196388006084));
#55415=CARTESIAN_POINT('Ctrl Pts',(4.05771050318434,0.79477268400084,8.57698201599421));
#55416=CARTESIAN_POINT('Ctrl Pts',(4.19526082558559,1.06847604194643,8.59960976409463));
#55417=CARTESIAN_POINT('Ctrl Pts',(4.26698198887019,1.18514270861437,8.61335123634875));
#55418=CARTESIAN_POINT('Ctrl Pts',(4.35088387761328,1.30000000000384,8.63103946714495));
#55419=CARTESIAN_POINT('Ctrl Pts',(4.28983548714786,-1.30000000000496,8.8248766281363));
#55420=CARTESIAN_POINT('Ctrl Pts',(4.21384120149965,-1.18514270861514,8.78447021791069));
#55421=CARTESIAN_POINT('Ctrl Pts',(4.14921392203966,-1.06847604194682,8.75005834837911));
#55422=CARTESIAN_POINT('Ctrl Pts',(4.02617203610171,-0.794772684000851,
8.68440863389773));
#55423=CARTESIAN_POINT('Ctrl Pts',(3.9768459243883,-0.636309800095197,8.66155018583716));
#55424=CARTESIAN_POINT('Ctrl Pts',(3.91457783683306,-0.319434907277159,
8.62081822041216));
#55425=CARTESIAN_POINT('Ctrl Pts',(3.90175138019541,-0.158333333333332,
8.60789341040585));
#55426=CARTESIAN_POINT('Ctrl Pts',(3.90875262150677,0.158333333333334,8.58839155923708));
#55427=CARTESIAN_POINT('Ctrl Pts',(3.92838285746568,0.319434907277167,8.58266762337897));
#55428=CARTESIAN_POINT('Ctrl Pts',(4.00531418532213,0.636309800095206,8.58193800807378));
#55429=CARTESIAN_POINT('Ctrl Pts',(4.06137678322636,0.79477268400084,8.58482558447746));
#55430=CARTESIAN_POINT('Ctrl Pts',(4.19998727431994,1.06847604194643,8.60640446367549));
#55431=CARTESIAN_POINT('Ctrl Pts',(4.2720251072689,1.18514270861437,8.62000938469766));
#55432=CARTESIAN_POINT('Ctrl Pts',(4.35610142759692,1.30000000000384,8.63787852951341));
#55433=CARTESIAN_POINT('Ctrl Pts',(4.29930376072963,-1.30000000000496,8.83268461488515));
#55434=CARTESIAN_POINT('Ctrl Pts',(4.2262195627153,-1.18514270861514,8.79214240758744));
#55435=CARTESIAN_POINT('Ctrl Pts',(4.16336519692289,-1.06847604194682,8.75816761714088));
#55436=CARTESIAN_POINT('Ctrl Pts',(4.04179199687415,-0.794772684000852,
8.69485110130973));
#55437=CARTESIAN_POINT('Ctrl Pts',(3.98908680587602,-0.636309800095197,
8.67637440288014));
#55438=CARTESIAN_POINT('Ctrl Pts',(3.92522495352783,-0.319434907277159,
8.63802912135571));
#55439=CARTESIAN_POINT('Ctrl Pts',(3.9116447724459,-0.158333333333332,8.6244628589329));
#55440=CARTESIAN_POINT('Ctrl Pts',(3.91874146174287,0.158333333333334,8.60483888933969));
#55441=CARTESIAN_POINT('Ctrl Pts',(3.93921600502161,0.319434907277167,8.5998008173125));
#55442=CARTESIAN_POINT('Ctrl Pts',(4.01794542822412,0.636309800095206,8.59609656237777));
#55443=CARTESIAN_POINT('Ctrl Pts',(4.07761409240379,0.794772684000841,8.59344330335423));
#55444=CARTESIAN_POINT('Ctrl Pts',(4.21475015139629,1.06847604194643,8.6127300716576));
#55445=CARTESIAN_POINT('Ctrl Pts',(4.28494704343638,1.18514270861437,8.62620793882529));
#55446=CARTESIAN_POINT('Ctrl Pts',(4.36597970897014,1.30000000000384,8.64481514580727));
#55447=CARTESIAN_POINT('Ctrl Pts',(4.31312792074545,-1.30000000000496,8.84424454249127));
#55448=CARTESIAN_POINT('Ctrl Pts',(4.243424146701,-1.18514270861514,8.80514758315398));
#55449=CARTESIAN_POINT('Ctrl Pts',(4.18297452507387,-1.06847604194682,8.77242899407481));
#55450=CARTESIAN_POINT('Ctrl Pts',(4.0647027495816,-0.794772684000851,8.71157781925591));
#55451=CARTESIAN_POINT('Ctrl Pts',(4.01090852828359,-0.636309800095196,
8.69427998926102));
#55452=CARTESIAN_POINT('Ctrl Pts',(3.94667172175643,-0.319434907277159,
8.65719965161783));
#55453=CARTESIAN_POINT('Ctrl Pts',(3.93163133024526,-0.158333333333332,
8.64372198961442));
#55454=CARTESIAN_POINT('Ctrl Pts',(3.93874497628404,0.158333333333334,8.62400686072403));
#55455=CARTESIAN_POINT('Ctrl Pts',(3.96054477515934,0.319434907277168,8.6190912105333));
#55456=CARTESIAN_POINT('Ctrl Pts',(4.03999312514226,0.636309800095207,8.61332080472688));
#55457=CARTESIAN_POINT('Ctrl Pts',(4.10152595983501,0.794772684000841,8.60777135386286));
#55458=CARTESIAN_POINT('Ctrl Pts',(4.23547535188849,1.06847604194643,8.6244638114006));
#55459=CARTESIAN_POINT('Ctrl Pts',(4.30315793171355,1.18514270861437,8.63701391339769));
#55460=CARTESIAN_POINT('Ctrl Pts',(4.38054136285748,1.30000000000383,8.65488857104023));
#55461=CARTESIAN_POINT('Ctrl Pts',(4.3244187971589,-1.30000000000496,8.85410663226077));
#55462=CARTESIAN_POINT('Ctrl Pts',(4.25707252974643,-1.18514270861514,8.81642818419089));
#55463=CARTESIAN_POINT('Ctrl Pts',(4.19840048318692,-1.06847604194682,8.78460695411973));
#55464=CARTESIAN_POINT('Ctrl Pts',(4.08289550377498,-0.794772684000848,
8.72462489215008));
#55465=CARTESIAN_POINT('Ctrl Pts',(4.02927403638533,-0.636309800095195,
8.70556215389797));
#55466=CARTESIAN_POINT('Ctrl Pts',(3.96499593377808,-0.319434907277158,
8.66861314096609));
#55467=CARTESIAN_POINT('Ctrl Pts',(3.94838335269583,-0.158333333333332,
8.65630976419325));
#55468=CARTESIAN_POINT('Ctrl Pts',(3.95524198209584,0.158333333333334,8.63711868842999));
#55469=CARTESIAN_POINT('Ctrl Pts',(3.97797880426114,0.319434907277165,8.63237791717527));
#55470=CARTESIAN_POINT('Ctrl Pts',(4.05772333724245,0.636309800095204,8.62586295336701));
#55471=CARTESIAN_POINT('Ctrl Pts',(4.12042170706468,0.794772684000838,8.61906302296074));
#55472=CARTESIAN_POINT('Ctrl Pts',(4.25186429647709,1.06847604194643,8.63440942857542));
#55473=CARTESIAN_POINT('Ctrl Pts',(4.31765404311617,1.18514270861437,8.64639681988873));
#55474=CARTESIAN_POINT('Ctrl Pts',(4.39233690986531,1.30000000000383,8.66372871216506));
#55475=CARTESIAN_POINT('Ctrl Pts',(4.33572321977573,-1.30000000000496,8.86421064164255));
#55476=CARTESIAN_POINT('Ctrl Pts',(4.27092732418113,-1.18514270861514,8.82814842879662));
#55477=CARTESIAN_POINT('Ctrl Pts',(4.21419946894931,-1.06847604194682,8.79734935690205));
#55478=CARTESIAN_POINT('Ctrl Pts',(4.10178556224008,-0.794772684000849,
8.73835624797819));
#55479=CARTESIAN_POINT('Ctrl Pts',(4.04840193500903,-0.636309800095196,
8.71754578928925));
#55480=CARTESIAN_POINT('Ctrl Pts',(3.98441167665988,-0.319434907277159,
8.68022362769928));
#55481=CARTESIAN_POINT('Ctrl Pts',(3.9663377392371,-0.158333333333332,8.66871093771688));
#55482=CARTESIAN_POINT('Ctrl Pts',(3.97352620747206,0.158333333333334,8.64870668848889));
#55483=CARTESIAN_POINT('Ctrl Pts',(3.99824681020785,0.319434907277166,8.64186510293906));
#55484=CARTESIAN_POINT('Ctrl Pts',(4.07798307430565,0.636309800095205,8.63507917158918));
#55485=CARTESIAN_POINT('Ctrl Pts',(4.14019739114876,0.79477268400084,8.63069489993545));
#55486=CARTESIAN_POINT('Ctrl Pts',(4.26838958459523,1.06847604194643,8.64554477741727));
#55487=CARTESIAN_POINT('Ctrl Pts',(4.33215125685333,1.18514270861437,8.65676559192588));
#55488=CARTESIAN_POINT('Ctrl Pts',(4.40418495081513,1.30000000000384,8.67277925922339));
#55489=CARTESIAN_POINT('Ctrl Pts',(4.34626852229784,-1.30000000000496,8.87552627072083));
#55490=CARTESIAN_POINT('Ctrl Pts',(4.28392604793638,-1.18514270861514,8.84094205580928));
#55491=CARTESIAN_POINT('Ctrl Pts',(4.2291044621075,-1.06847604194682,8.81099126755198));
#55492=CARTESIAN_POINT('Ctrl Pts',(4.11983038888185,-0.794772684000851,
8.75250309752858));
#55493=CARTESIAN_POINT('Ctrl Pts',(4.06679618167507,-0.636309800095197,
8.72976507628461));
#55494=CARTESIAN_POINT('Ctrl Pts',(4.00358038221854,-0.319434907277159,
8.69098406914389));
#55495=CARTESIAN_POINT('Ctrl Pts',(3.98490986621235,-0.158333333333332,
8.67847487346248));
#55496=CARTESIAN_POINT('Ctrl Pts',(3.99231677038997,0.158333333333334,8.65788882672129));
#55497=CARTESIAN_POINT('Ctrl Pts',(4.01788418085971,0.319434907277166,8.65128274813801));
#55498=CARTESIAN_POINT('Ctrl Pts',(4.0972261638769,0.636309800095205,8.64513560267597));
#55499=CARTESIAN_POINT('Ctrl Pts',(4.15925187332272,0.79477268400084,8.64255931406753));
#55500=CARTESIAN_POINT('Ctrl Pts',(4.28452235248451,1.06847604194643,8.65666215032348));
#55501=CARTESIAN_POINT('Ctrl Pts',(4.34645140535157,1.18514270861437,8.6669808430935));
#55502=CARTESIAN_POINT('Ctrl Pts',(4.41608456238495,1.30000000000383,8.68151363337989));
#55503=CARTESIAN_POINT('Ctrl Pts',(4.36422521226682,-1.30000000000495,8.89174180979307));
#55504=CARTESIAN_POINT('Ctrl Pts',(4.30586457287734,-1.18514270861514,8.85961335725795));
#55505=CARTESIAN_POINT('Ctrl Pts',(4.25405375016242,-1.06847604194682,8.83124862077492));
#55506=CARTESIAN_POINT('Ctrl Pts',(4.14949177177681,-0.794772684000853,
8.77441534216264));
#55507=CARTESIAN_POINT('Ctrl Pts',(4.09637737283048,-0.636309800095197,
8.74984090708147));
#55508=CARTESIAN_POINT('Ctrl Pts',(4.03399467514183,-0.319434907277159,
8.70955638867894));
#55509=CARTESIAN_POINT('Ctrl Pts',(4.01440519392537,-0.158333333333332,
8.69526969200356));
#55510=CARTESIAN_POINT('Ctrl Pts',(4.02204202455759,0.158333333333334,8.67410888232258));
#55511=CARTESIAN_POINT('Ctrl Pts',(4.04885947795462,0.319434907277165,8.66843761565224));
#55512=CARTESIAN_POINT('Ctrl Pts',(4.12763066499831,0.636309800095204,8.66316897698633));
#55513=CARTESIAN_POINT('Ctrl Pts',(4.18973120740827,0.794772684000841,8.66243987109688));
#55514=CARTESIAN_POINT('Ctrl Pts',(4.31019462438223,1.06847604194643,8.67527067605611));
#55515=CARTESIAN_POINT('Ctrl Pts',(4.36902600111067,1.18514270861437,8.68431305960336));
#55516=CARTESIAN_POINT('Ctrl Pts',(4.43454460496874,1.30000000000384,8.69684384665918));
#55517=CARTESIAN_POINT('Ctrl Pts',(4.38767994763338,-1.30000000000497,8.91609640196983));
#55518=CARTESIAN_POINT('Ctrl Pts',(4.33410494967261,-1.18514270861515,8.88837512378823));
#55519=CARTESIAN_POINT('Ctrl Pts',(4.28604603319652,-1.06847604194683,8.86275198152183));
#55520=CARTESIAN_POINT('Ctrl Pts',(4.1877635737022,-0.794772684000858,8.80840451068953));
#55521=CARTESIAN_POINT('Ctrl Pts',(4.13559346017687,-0.636309800095199,
8.7795612982255));
#55522=CARTESIAN_POINT('Ctrl Pts',(4.07488993204494,-0.319434907277158,
8.73635149198173));
#55523=CARTESIAN_POINT('Ctrl Pts',(4.054100148061,-0.158333333333332,8.71968410253834));
#55524=CARTESIAN_POINT('Ctrl Pts',(4.06223420124964,0.158333333333334,8.69731819149294));
#55525=CARTESIAN_POINT('Ctrl Pts',(4.09083196103889,0.319434907277167,8.69244165562464));
#55526=CARTESIAN_POINT('Ctrl Pts',(4.16876816599636,0.636309800095206,8.68841938571338));
#55527=CARTESIAN_POINT('Ctrl Pts',(4.2305305830476,0.794772684000839,8.69127158429364));
#55528=CARTESIAN_POINT('Ctrl Pts',(4.3446903395284,1.06847604194643,8.70198094260544));
#55529=CARTESIAN_POINT('Ctrl Pts',(4.39955289097199,1.18514270861438,8.70881915620342));
#55530=CARTESIAN_POINT('Ctrl Pts',(4.45986246531419,1.30000000000385,8.717859899007));
#55531=CARTESIAN_POINT('Ctrl Pts',(4.41533706763821,-1.30000000000497,8.94499626631974));
#55532=CARTESIAN_POINT('Ctrl Pts',(4.36794300895912,-1.18514270861515,8.92167148680998));
#55533=CARTESIAN_POINT('Ctrl Pts',(4.32451940762636,-1.06847604194683,8.89904773381702));
#55534=CARTESIAN_POINT('Ctrl Pts',(4.23337475244403,-0.79477268400086,8.84840185003111));
#55535=CARTESIAN_POINT('Ctrl Pts',(4.1806055452744,-0.636309800095201,8.81775565383643));
#55536=CARTESIAN_POINT('Ctrl Pts',(4.12134692798048,-0.31943490727716,8.77220167135861));
#55537=CARTESIAN_POINT('Ctrl Pts',(4.09987465453343,-0.158333333333333,
8.75128226254503));
#55538=CARTESIAN_POINT('Ctrl Pts',(4.10853203043528,0.158333333333335,8.72782643002757));
#55539=CARTESIAN_POINT('Ctrl Pts',(4.13856365854856,0.319434907277167,8.72560883261724));
#55540=CARTESIAN_POINT('Ctrl Pts',(4.21565638940201,0.636309800095208,8.72273554692928));
#55541=CARTESIAN_POINT('Ctrl Pts',(4.27778957553113,0.794772684000846,8.72786458211374));
#55542=CARTESIAN_POINT('Ctrl Pts',(4.3849967272625,1.06847604194643,8.73475299590499));
#55543=CARTESIAN_POINT('Ctrl Pts',(4.43532980429784,1.18514270861438,8.73853999810118));
#55544=CARTESIAN_POINT('Ctrl Pts',(4.48958995480018,1.30000000000384,8.7431322634042));
#55545=CARTESIAN_POINT('Ctrl Pts',(4.43404520828974,-1.30000000000497,8.96568188497049));
#55546=CARTESIAN_POINT('Ctrl Pts',(4.39031687507281,-1.18514270861515,8.94641560147379));
#55547=CARTESIAN_POINT('Ctrl Pts',(4.34974854817529,-1.06847604194683,8.92645120558581));
#55548=CARTESIAN_POINT('Ctrl Pts',(4.26332784413169,-0.794772684000854,
8.87871667794048));
#55549=CARTESIAN_POINT('Ctrl Pts',(4.21117558585354,-0.636309800095199,
8.84503073916913));
#55550=CARTESIAN_POINT('Ctrl Pts',(4.15303192935944,-0.31943490727716,8.79778076666981));
#55551=CARTESIAN_POINT('Ctrl Pts',(4.13046881562288,-0.158333333333333,
8.77524556471387));
#55552=CARTESIAN_POINT('Ctrl Pts',(4.1394779046875,0.158333333333335,8.75106187745542));
#55553=CARTESIAN_POINT('Ctrl Pts',(4.17089728038284,0.319434907277167,8.74974959162166));
#55554=CARTESIAN_POINT('Ctrl Pts',(4.24770310043635,0.636309800095207,8.74705432034812));
#55555=CARTESIAN_POINT('Ctrl Pts',(4.31030454314704,0.794772684000842,8.75340274182129));
#55556=CARTESIAN_POINT('Ctrl Pts',(4.4126725008907,1.06847604194643,8.7577656338405));
#55557=CARTESIAN_POINT('Ctrl Pts',(4.45978245913997,1.18514270861438,8.7596488012543));
#55558=CARTESIAN_POINT('Ctrl Pts',(4.50969107983768,1.30000000000385,8.76152660178787));
#55559=CARTESIAN_POINT('Ctrl Pts',(4.44619000963321,-1.30000000000497,8.98001366847455));
#55560=CARTESIAN_POINT('Ctrl Pts',(4.40525777118481,-1.18514270861515,8.9628531698774));
#55561=CARTESIAN_POINT('Ctrl Pts',(4.36679375885251,-1.06847604194683,8.94432506201643));
#55562=CARTESIAN_POINT('Ctrl Pts',(4.28363629176136,-0.794772684000856,
8.89836197533397));
#55563=CARTESIAN_POINT('Ctrl Pts',(4.23135175689816,-0.636309800095199,
8.86361341927445));
#55564=CARTESIAN_POINT('Ctrl Pts',(4.17374064951435,-0.319434907277159,
8.81562502062927));
#55565=CARTESIAN_POINT('Ctrl Pts',(4.15051793125772,-0.158333333333333,
8.79189493686576));
#55566=CARTESIAN_POINT('Ctrl Pts',(4.1597041449006,0.158333333333334,8.76736032302134));
#55567=CARTESIAN_POINT('Ctrl Pts',(4.19200174471018,0.319434907277166,8.76678545613091));
#55568=CARTESIAN_POINT('Ctrl Pts',(4.26855128330622,0.636309800095206,8.76433080554314));
#55569=CARTESIAN_POINT('Ctrl Pts',(4.33129030207517,0.794772684000839,8.77178079794625));
#55570=CARTESIAN_POINT('Ctrl Pts',(4.43064562884352,1.06847604194643,8.77401583737565));
#55571=CARTESIAN_POINT('Ctrl Pts',(4.47578660915789,1.18514270861438,8.77427158274088));
#55572=CARTESIAN_POINT('Ctrl Pts',(4.52306133030603,1.30000000000385,8.77381560771872));
#55573=CARTESIAN_POINT('Ctrl Pts',(4.45453765168186,-1.30000000000497,8.98912942527086));
#55574=CARTESIAN_POINT('Ctrl Pts',(4.41512586643895,-1.18514270861515,8.97395729129967));
#55575=CARTESIAN_POINT('Ctrl Pts',(4.37783983971279,-1.06847604194683,8.9567713308798));
#55576=CARTESIAN_POINT('Ctrl Pts',(4.2966125863621,-0.794772684000855,8.9124159823096));
#55577=CARTESIAN_POINT('Ctrl Pts',(4.24448056452864,-0.636309800095199,
8.87657622648389));
#55578=CARTESIAN_POINT('Ctrl Pts',(4.18740615513335,-0.31943490727716,8.82777629898448));
#55579=CARTESIAN_POINT('Ctrl Pts',(4.16398183654532,-0.158333333333333,
8.80279462257431));
#55580=CARTESIAN_POINT('Ctrl Pts',(4.17332167501868,0.158333333333335,8.77796636634553));
#55581=CARTESIAN_POINT('Ctrl Pts',(4.20602135108615,0.319434907277167,8.77823311288337));
#55582=CARTESIAN_POINT('Ctrl Pts',(4.28225168210284,0.636309800095207,8.77622883251019));
#55583=CARTESIAN_POINT('Ctrl Pts',(4.34500767159721,0.794772684000841,8.78455925488412));
#55584=CARTESIAN_POINT('Ctrl Pts',(4.44225791319782,1.06847604194643,8.78557151883606));
#55585=CARTESIAN_POINT('Ctrl Pts',(4.48605228741681,1.18514270861438,8.78481316963859));
#55586=CARTESIAN_POINT('Ctrl Pts',(4.53154500974223,1.30000000000385,8.78285829968693));
#55587=CARTESIAN_POINT('Ctrl Pts',(4.4649410339563,-1.30000000000497,9.00056527592849));
#55588=CARTESIAN_POINT('Ctrl Pts',(4.42761818610944,-1.18514270861515,8.9875491573474));
#55589=CARTESIAN_POINT('Ctrl Pts',(4.39191905643545,-1.06847604194683,8.97183901834883));
#55590=CARTESIAN_POINT('Ctrl Pts',(4.31319803910584,-0.794772684000856,
8.92932172835859));
#55591=CARTESIAN_POINT('Ctrl Pts',(4.26103365036649,-0.6363098000952,8.89248633726872));
#55592=CARTESIAN_POINT('Ctrl Pts',(4.20452828810145,-0.319434907277159,
8.84285662377426));
#55593=CARTESIAN_POINT('Ctrl Pts',(4.18080445888963,-0.158333333333333,
8.81643061427704));
#55594=CARTESIAN_POINT('Ctrl Pts',(4.19035476432787,0.158333333333335,8.79120304025113));
#55595=CARTESIAN_POINT('Ctrl Pts',(4.22354972932494,0.319434907277167,8.79252163388763));
#55596=CARTESIAN_POINT('Ctrl Pts',(4.29966963900563,0.636309800095207,8.79051984200613));
#55597=CARTESIAN_POINT('Ctrl Pts',(4.36290981102847,0.794772684000841,8.79907206384702));
#55598=CARTESIAN_POINT('Ctrl Pts',(4.4577640286338,1.06847604194643,8.7980867009406));
#55599=CARTESIAN_POINT('Ctrl Pts',(4.49991041851912,1.18514270861438,8.79598035517156));
#55600=CARTESIAN_POINT('Ctrl Pts',(4.54314432218328,1.30000000000385,8.79219419072437));
#55601=CARTESIAN_POINT('Ctrl Pts',(4.47689956690015,-1.30000000000497,9.01516635057687));
#55602=CARTESIAN_POINT('Ctrl Pts',(4.44225166083132,-1.18514270861515,9.00445134978857));
#55603=CARTESIAN_POINT('Ctrl Pts',(4.40859270265779,-1.06847604194683,8.99028169280819));
#55604=CARTESIAN_POINT('Ctrl Pts',(4.3331184433025,-0.794772684000854,8.94956600364834));
#55605=CARTESIAN_POINT('Ctrl Pts',(4.28115576151042,-0.636309800095201,
8.9111123353338));
#55606=CARTESIAN_POINT('Ctrl Pts',(4.22506688969079,-0.319434907277161,
8.86098093531374));
#55607=CARTESIAN_POINT('Ctrl Pts',(4.20028938187868,-0.158333333333333,
8.83407467074119));
#55608=CARTESIAN_POINT('Ctrl Pts',(4.20975340442327,0.158333333333335,8.80898190960155));
#55609=CARTESIAN_POINT('Ctrl Pts',(4.24374949284336,0.319434907277167,8.81117674665288));
#55610=CARTESIAN_POINT('Ctrl Pts',(4.31961584470656,0.636309800095208,8.80941924984648));
#55611=CARTESIAN_POINT('Ctrl Pts',(4.38319093328862,0.794772684000844,8.81871083360723));
#55612=CARTESIAN_POINT('Ctrl Pts',(4.47509038699624,1.06847604194644,8.81552607287147));
#55613=CARTESIAN_POINT('Ctrl Pts',(4.51526700412506,1.18514270861438,8.8118155481022));
#55614=CARTESIAN_POINT('Ctrl Pts',(4.55584037008276,1.30000000000385,8.80577306347917));
#55615=CARTESIAN_POINT('Ctrl Pts',(4.48897649417153,-1.30000000000497,9.02949874664839));
#55616=CARTESIAN_POINT('Ctrl Pts',(4.45636582527148,-1.18514270861515,9.02211642542208));
#55617=CARTESIAN_POINT('Ctrl Pts',(4.42429681123459,-1.06847604194683,9.01022573801647));
#55618=CARTESIAN_POINT('Ctrl Pts',(4.35146230451729,-0.794772684000857,
8.97234064361614));
#55619=CARTESIAN_POINT('Ctrl Pts',(4.29967282671666,-0.636309800095202,
8.9324359539744));
#55620=CARTESIAN_POINT('Ctrl Pts',(4.24460051930937,-0.319434907277161,
8.88080222914568));
#55621=CARTESIAN_POINT('Ctrl Pts',(4.21986464943619,-0.158333333333333,
8.85150900811807));
#55622=CARTESIAN_POINT('Ctrl Pts',(4.2300599323088,0.158333333333335,8.82510783226668));
#55623=CARTESIAN_POINT('Ctrl Pts',(4.26511440832616,0.319434907277168,8.82767716361691));
#55624=CARTESIAN_POINT('Ctrl Pts',(4.34070257223563,0.636309800095209,8.82619093901148));
#55625=CARTESIAN_POINT('Ctrl Pts',(4.40385706271878,0.794772684000845,8.83759526436711));
#55626=CARTESIAN_POINT('Ctrl Pts',(4.49278112351848,1.06847604194644,8.83220749269224));
#55627=CARTESIAN_POINT('Ctrl Pts',(4.53112363495319,1.18514270861438,8.82662108018919));
#55628=CARTESIAN_POINT('Ctrl Pts',(4.56931672686336,1.30000000000385,8.81778042190455));
#55629=CARTESIAN_POINT('Ctrl Pts',(4.50119014476422,-1.30000000000497,9.04363299068084));
#55630=CARTESIAN_POINT('Ctrl Pts',(4.47137138258233,-1.18514270861515,9.03834985209589));
#55631=CARTESIAN_POINT('Ctrl Pts',(4.44134828489834,-1.06847604194683,9.02798673076185));
#55632=CARTESIAN_POINT('Ctrl Pts',(4.37151686726173,-0.794772684000857,
8.99231007094768));
#55633=CARTESIAN_POINT('Ctrl Pts',(4.31915516652733,-0.636309800095201,
8.95209331628435));
#55634=CARTESIAN_POINT('Ctrl Pts',(4.26435157519034,-0.319434907277161,
8.90021066968859));
#55635=CARTESIAN_POINT('Ctrl Pts',(4.23913849393376,-0.158333333333333,
8.86945988638939));
#55636=CARTESIAN_POINT('Ctrl Pts',(4.24922113999326,0.158333333333335,8.84326434603573));
#55637=CARTESIAN_POINT('Ctrl Pts',(4.28443545905308,0.319434907277168,8.84786052209751));
#55638=CARTESIAN_POINT('Ctrl Pts',(4.3599424971951,0.636309800095209,8.84630136132387));
#55639=CARTESIAN_POINT('Ctrl Pts',(4.42436953276321,0.794772684000845,8.8567291738621));
#55640=CARTESIAN_POINT('Ctrl Pts',(4.51055686536067,1.06847604194644,8.84875895539504));
#55641=CARTESIAN_POINT('Ctrl Pts',(4.54687289339834,1.18514270861438,8.8416827346635));
#55642=CARTESIAN_POINT('Ctrl Pts',(4.58219764674743,1.30000000000385,8.83098030544912));
#55643=CARTESIAN_POINT('Ctrl Pts',(4.51708986244,-1.30000000000497,9.06302202413031));
#55644=CARTESIAN_POINT('Ctrl Pts',(4.49007411997201,-1.18514270861515,9.06200911533405));
#55645=CARTESIAN_POINT('Ctrl Pts',(4.46224233834228,-1.06847604194683,9.05454625268663));
#55646=CARTESIAN_POINT('Ctrl Pts',(4.3960601413376,-0.794772684000856,9.02240486332576));
#55647=CARTESIAN_POINT('Ctrl Pts',(4.34416897458864,-0.636309800095202,
8.97984128700459));
#55648=CARTESIAN_POINT('Ctrl Pts',(4.29038389170619,-0.319434907277162,
8.92658673382167));
#55649=CARTESIAN_POINT('Ctrl Pts',(4.26449353889939,-0.158333333333333,
8.89399392534927));
#55650=CARTESIAN_POINT('Ctrl Pts',(4.27513479329512,0.158333333333335,8.86682608840896));
#55651=CARTESIAN_POINT('Ctrl Pts',(4.31180224590399,0.319434907277168,8.87185929610473));
#55652=CARTESIAN_POINT('Ctrl Pts',(4.38698609048331,0.63630980009521,8.87057291631606));
#55653=CARTESIAN_POINT('Ctrl Pts',(4.45109551779406,0.794772684000846,8.88332483627587));
#55654=CARTESIAN_POINT('Ctrl Pts',(4.53337656398258,1.06847604194644,8.87234725348443));
#55655=CARTESIAN_POINT('Ctrl Pts',(4.56723495535358,1.18514270861439,8.86282861704834));
#55656=CARTESIAN_POINT('Ctrl Pts',(4.59933532201359,1.30000000000385,8.84854313300709));
#55657=CARTESIAN_POINT('Ctrl Pts',(4.52945512605073,-1.30000000000498,9.0796760470566));
#55658=CARTESIAN_POINT('Ctrl Pts',(4.50520200778997,-1.18514270861516,9.08131599846587));
#55659=CARTESIAN_POINT('Ctrl Pts',(4.47944179574346,-1.06847604194683,9.0757175030803));
#55660=CARTESIAN_POINT('Ctrl Pts',(4.41644886446555,-0.794772684000859,
9.04606159862226));
#55661=CARTESIAN_POINT('Ctrl Pts',(4.36440246445019,-0.636309800095204,
9.00247234903706));
#55662=CARTESIAN_POINT('Ctrl Pts',(4.31103754745527,-0.319434907277162,
8.94879399171032));
#55663=CARTESIAN_POINT('Ctrl Pts',(4.28435267089773,-0.158333333333334,
8.91513189120031));
#55664=CARTESIAN_POINT('Ctrl Pts',(4.29512809994144,0.158333333333336,8.88775363725623));
#55665=CARTESIAN_POINT('Ctrl Pts',(4.33268871755653,0.319434907277169,8.89369019344123));
#55666=CARTESIAN_POINT('Ctrl Pts',(4.40779807930735,0.636309800095212,8.89230842428382));
#55667=CARTESIAN_POINT('Ctrl Pts',(4.47236566437713,0.794772684000848,8.90564944314382));
#55668=CARTESIAN_POINT('Ctrl Pts',(4.55174598911817,1.06847604194644,8.89177115316105));
#55669=CARTESIAN_POINT('Ctrl Pts',(4.58362827123485,1.18514270861439,8.88025305729823));
#55670=CARTESIAN_POINT('Ctrl Pts',(4.61303203421851,1.30000000000385,8.86322426306484));
#55671=CARTESIAN_POINT('Ctrl Pts',(4.54140619220528,-1.30000000000498,9.09411954148937));
#55672=CARTESIAN_POINT('Ctrl Pts',(4.51930652660192,-1.18514270861516,9.09885640928562));
#55673=CARTESIAN_POINT('Ctrl Pts',(4.49517828166395,-1.06847604194683,9.0954364657231));
#55674=CARTESIAN_POINT('Ctrl Pts',(4.43475078494002,-0.794772684000859,
9.06869184593323));
#55675=CARTESIAN_POINT('Ctrl Pts',(4.38264124396578,-0.636309800095204,
9.02402001715036));
#55676=CARTESIAN_POINT('Ctrl Pts',(4.32984101530184,-0.319434907277163,
8.96966456229311));
#55677=CARTESIAN_POINT('Ctrl Pts',(4.30281425189962,-0.158333333333334,
8.93438845416319));
#55678=CARTESIAN_POINT('Ctrl Pts',(4.31386287852357,0.158333333333336,8.9065687867174));
#55679=CARTESIAN_POINT('Ctrl Pts',(4.352093867694,0.319434907277169,8.91357065040671));
#55680=CARTESIAN_POINT('Ctrl Pts',(4.42708240901013,0.636309800095211,8.91218538636726));
#55681=CARTESIAN_POINT('Ctrl Pts',(4.49204923449338,0.794772684000849,8.92612918110719));
#55682=CARTESIAN_POINT('Ctrl Pts',(4.56875388326351,1.06847604194644,8.90957401593609));
#55683=CARTESIAN_POINT('Ctrl Pts',(4.59882305789642,1.18514270861439,8.89619090930866));
#55684=CARTESIAN_POINT('Ctrl Pts',(4.62575880689679,1.30000000000385,8.87659081362708));
#55685=CARTESIAN_POINT('Ctrl Pts',(4.54912648699166,-1.30000000000498,9.10416325960802));
#55686=CARTESIAN_POINT('Ctrl Pts',(4.52879502626638,-1.18514270861516,9.11042192478117));
#55687=CARTESIAN_POINT('Ctrl Pts',(4.50594191402208,-1.06847604194684,9.10814700627611));
#55688=CARTESIAN_POINT('Ctrl Pts',(4.44732113352516,-0.794772684000862,
9.08317720399946));
#55689=CARTESIAN_POINT('Ctrl Pts',(4.39460181867289,-0.636309800095205,
9.03869202390378));
#55690=CARTESIAN_POINT('Ctrl Pts',(4.34203697549782,-0.319434907277163,
8.98411292642917));
#55691=CARTESIAN_POINT('Ctrl Pts',(4.31489287862101,-0.158333333333334,
8.94759833383886));
#55692=CARTESIAN_POINT('Ctrl Pts',(4.3263124676311,0.158333333333336,8.91917344459879));
#55693=CARTESIAN_POINT('Ctrl Pts',(4.36529744874918,0.319434907277169,8.92636274356103));
#55694=CARTESIAN_POINT('Ctrl Pts',(4.44026502444849,0.636309800095212,8.92487644722071));
#55695=CARTESIAN_POINT('Ctrl Pts',(4.505244095131,0.79477268400085,8.93965306842763));
#55696=CARTESIAN_POINT('Ctrl Pts',(4.58006936595371,1.06847604194644,8.92147834091787));
#55697=CARTESIAN_POINT('Ctrl Pts',(4.60891078384074,1.18514270861439,8.90688574169778));
#55698=CARTESIAN_POINT('Ctrl Pts',(4.63420453242497,1.30000000000386,8.88556770935661));
#55699=CARTESIAN_POINT('Ctrl Pts',(4.55955577529855,-1.30000000000498,9.11820985555783));
#55700=CARTESIAN_POINT('Ctrl Pts',(4.54105857280266,-1.18514270861516,9.1274941410361));
#55701=CARTESIAN_POINT('Ctrl Pts',(4.51964128858355,-1.06847604194684,9.12728996869032));
#55702=CARTESIAN_POINT('Ctrl Pts',(4.4634171045838,-0.794772684000861,9.10489805399411));
#55703=CARTESIAN_POINT('Ctrl Pts',(4.41100399482857,-0.636309800095205,
9.05887870635694));
#55704=CARTESIAN_POINT('Ctrl Pts',(4.35914697435268,-0.319434907277163,
9.00339740234672));
#55705=CARTESIAN_POINT('Ctrl Pts',(4.33177102369644,-0.158333333333334,
8.96527542330471));
#55706=CARTESIAN_POINT('Ctrl Pts',(4.34328698802605,0.158333333333336,8.9367192103428));
#55707=CARTESIAN_POINT('Ctrl Pts',(4.38252275214732,0.319434907277167,8.94549528055361));
#55708=CARTESIAN_POINT('Ctrl Pts',(4.4571365668548,0.636309800095211,8.94441818850174));
#55709=CARTESIAN_POINT('Ctrl Pts',(4.52234252698688,0.79477268400085,8.95997819955137));
#55710=CARTESIAN_POINT('Ctrl Pts',(4.59490732490742,1.06847604194644,8.93903467779169));
#55711=CARTESIAN_POINT('Ctrl Pts',(4.62226330419147,1.18514270861439,8.92244116718351));
#55712=CARTESIAN_POINT('Ctrl Pts',(4.64556465053033,1.30000000000386,8.898319820503));
#55713=CARTESIAN_POINT('Ctrl Pts',(4.56908022620465,-1.30000000000498,9.13090239008075));
#55714=CARTESIAN_POINT('Ctrl Pts',(4.55249723205479,-1.18514270861516,9.14253591637494));
#55715=CARTESIAN_POINT('Ctrl Pts',(4.53251137184418,-1.06847604194684,9.14400653961888));
#55716=CARTESIAN_POINT('Ctrl Pts',(4.47847873525912,-0.794772684000863,
9.12392563438181));
#55717=CARTESIAN_POINT('Ctrl Pts',(4.42581774727667,-0.636309800095209,
9.07734372287633));
#55718=CARTESIAN_POINT('Ctrl Pts',(4.37444674746134,-0.319434907277166,
9.02129387638326));
#55719=CARTESIAN_POINT('Ctrl Pts',(4.34694084754741,-0.158333333333335,
8.98160230860927));
#55720=CARTESIAN_POINT('Ctrl Pts',(4.35874071915001,0.158333333333337,8.95260057221036));
#55721=CARTESIAN_POINT('Ctrl Pts',(4.39852582926343,0.319434907277171,8.96226720782046));
#55722=CARTESIAN_POINT('Ctrl Pts',(4.47295593970602,0.636309800095217,8.96132678156408));
#55723=CARTESIAN_POINT('Ctrl Pts',(4.53827746161824,0.794772684000856,8.9777478532546));
#55724=CARTESIAN_POINT('Ctrl Pts',(4.60865612671007,1.06847604194645,8.95451974947366));
#55725=CARTESIAN_POINT('Ctrl Pts',(4.6345800275273,1.1851427086144,8.9362534324678));
#55726=CARTESIAN_POINT('Ctrl Pts',(4.65596351282986,1.30000000000386,8.90977538389685));
#55727=CARTESIAN_POINT('Ctrl Pts',(4.57550772428327,-1.30000000000498,9.1401299753939));
#55728=CARTESIAN_POINT('Ctrl Pts',(4.55998119412574,-1.18514270861516,9.1538323657346));
#55729=CARTESIAN_POINT('Ctrl Pts',(4.54085378640419,-1.06847604194684,9.15669030357686));
#55730=CARTESIAN_POINT('Ctrl Pts',(4.48834690061704,-0.794772684000866,
9.13823985702445));
#55731=CARTESIAN_POINT('Ctrl Pts',(4.43619211733095,-0.63630980009521,9.09023518980654));
#55732=CARTESIAN_POINT('Ctrl Pts',(4.38522319009914,-0.319434907277167,
9.03371831030787));
#55733=CARTESIAN_POINT('Ctrl Pts',(4.35714856386029,-0.158333333333335,
8.99369341011036));
#55734=CARTESIAN_POINT('Ctrl Pts',(4.36908576900311,0.158333333333337,8.96448317410072));
#55735=CARTESIAN_POINT('Ctrl Pts',(4.40945590413185,0.319434907277171,8.97445308559024));
#55736=CARTESIAN_POINT('Ctrl Pts',(4.48401021979826,0.636309800095217,8.97319151796637));
#55737=CARTESIAN_POINT('Ctrl Pts',(4.54973770956819,0.794772684000858,8.98966648233755));
#55738=CARTESIAN_POINT('Ctrl Pts',(4.61861542110489,1.06847604194645,8.96479170360382));
#55739=CARTESIAN_POINT('Ctrl Pts',(4.64346791710096,1.1851427086144,8.94547119712179));
#55740=CARTESIAN_POINT('Ctrl Pts',(4.66335829993943,1.30000000000386,8.91759755417022));
#55741=CARTESIAN_POINT('Ctrl Pts',(4.57881223363908,-1.30000000000498,9.14460699339319));
#55742=CARTESIAN_POINT('Ctrl Pts',(4.5639121987517,-1.18514270861516,9.15919665540848));
#55743=CARTESIAN_POINT('Ctrl Pts',(4.54525602294494,-1.06847604194684,9.16268537215633));
#55744=CARTESIAN_POINT('Ctrl Pts',(4.49347908773936,-0.794772684000865,
9.14509960145507));
#55745=CARTESIAN_POINT('Ctrl Pts',(4.44126851719988,-0.63630980009521,9.09684858201501));
#55746=CARTESIAN_POINT('Ctrl Pts',(4.39046492224128,-0.319434907277166,
9.04014749524157));
#55747=CARTESIAN_POINT('Ctrl Pts',(4.3623362735984,-0.158333333333335,8.99959933142438));
#55748=CARTESIAN_POINT('Ctrl Pts',(4.37435302808331,0.158333333333337,8.97027110368226));
#55749=CARTESIAN_POINT('Ctrl Pts',(4.41488519752389,0.319434907277171,8.98059839181612));
#55750=CARTESIAN_POINT('Ctrl Pts',(4.48937824100214,0.636309800095217,8.97937824996481));
#55751=CARTESIAN_POINT('Ctrl Pts',(4.5551624237004,0.794772684000857,8.99612661572198));
#55752=CARTESIAN_POINT('Ctrl Pts',(4.62333351307415,1.06847604194645,8.97035555419667));
#55753=CARTESIAN_POINT('Ctrl Pts',(4.64771955111663,1.1851427086144,8.95039248736616));
#55754=CARTESIAN_POINT('Ctrl Pts',(4.66698288859931,1.30000000000386,8.92162169132757));
#55755=CARTESIAN_POINT('Ctrl Pts',(4.5804691755298,-1.30000000000498,9.14683792771085));
#55756=CARTESIAN_POINT('Ctrl Pts',(4.56588770201385,-1.18514270861516,9.16186312841252));
#55757=CARTESIAN_POINT('Ctrl Pts',(4.5474687940014,-1.06847604194684,9.16566467794608));
#55758=CARTESIAN_POINT('Ctrl Pts',(4.49605219044009,-0.794772684000865,
9.1485181383841));
#55759=CARTESIAN_POINT('Ctrl Pts',(4.44379190666503,-0.63630980009521,9.10017678111588));
#55760=CARTESIAN_POINT('Ctrl Pts',(4.39306644821312,-0.319434907277166,
9.04339049217918));
#55761=CARTESIAN_POINT('Ctrl Pts',(4.36492491951435,-0.158333333333335,
9.00255930733304));
#55762=CARTESIAN_POINT('Ctrl Pts',(4.37698119812884,0.158333333333337,8.97317313112529));
#55763=CARTESIAN_POINT('Ctrl Pts',(4.41758632105313,0.319434907277172,8.98369197243874));
#55764=CARTESIAN_POINT('Ctrl Pts',(4.49203987838997,0.636309800095217,8.98250727246983));
#55765=CARTESIAN_POINT('Ctrl Pts',(4.55783977349975,0.794772684000857,8.99941342141394));
#55766=CARTESIAN_POINT('Ctrl Pts',(4.62566299182014,1.06847604194645,8.97318552162207));
#55767=CARTESIAN_POINT('Ctrl Pts',(4.64982268195567,1.1851427086144,8.95288994480363));
#55768=CARTESIAN_POINT('Ctrl Pts',(4.66878390411358,1.30000000000386,8.92365187714725));
#55769=CARTESIAN_POINT('Ctrl Pts',(4.58141951381765,-1.30000000000498,9.14810732654966));
#55770=CARTESIAN_POINT('Ctrl Pts',(4.56702335251096,-1.18514270861516,9.16337648868155));
#55771=CARTESIAN_POINT('Ctrl Pts',(4.54874135366842,-1.06847604194684,9.16735482092146));
#55772=CARTESIAN_POINT('Ctrl Pts',(4.49752921697429,-0.794772684000865,
9.15046148848517));
#55773=CARTESIAN_POINT('Ctrl Pts',(4.44522961904313,-0.63630980009521,9.10208506291557));
#55774=CARTESIAN_POINT('Ctrl Pts',(4.39454731060875,-0.319434907277166,
9.04525224300041));
#55775=CARTESIAN_POINT('Ctrl Pts',(4.36640635472226,-0.158333333333335,
9.00424699940882));
#55776=CARTESIAN_POINT('Ctrl Pts',(4.37848537183999,0.158333333333337,8.97482756115475));
#55777=CARTESIAN_POINT('Ctrl Pts',(4.41912746697037,0.319434907277171,8.98546326183054));
#55778=CARTESIAN_POINT('Ctrl Pts',(4.49355403117831,0.636309800095217,8.98430609907814));
#55779=CARTESIAN_POINT('Ctrl Pts',(4.55935772741226,0.794772684000857,9.00131124541432));
#55780=CARTESIAN_POINT('Ctrl Pts',(4.626983888122,1.06847604194645,8.97481946469352));
#55781=CARTESIAN_POINT('Ctrl Pts',(4.65101680698759,1.1851427086144,8.95432959774862));
#55782=CARTESIAN_POINT('Ctrl Pts',(4.66980978554356,1.30000000000386,8.92481717411571));
#55783=CARTESIAN_POINT('Ctrl Pts',(4.589495289761,-1.30000000000499,9.1588996934203));
#55784=CARTESIAN_POINT('Ctrl Pts',(4.57668584766636,-1.18514270861516,9.17622343193904));
#55785=CARTESIAN_POINT('Ctrl Pts',(4.55957141230676,-1.06847604194684,9.18169735807558));
#55786=CARTESIAN_POINT('Ctrl Pts',(4.51008824724248,-0.794772684000866,
9.16696778535652));
#55787=CARTESIAN_POINT('Ctrl Pts',(4.4574158485065,-0.63630980009521,9.11835068551886));
#55788=CARTESIAN_POINT('Ctrl Pts',(4.40707795604764,-0.319434907277166,
9.06115697298211));
#55789=CARTESIAN_POINT('Ctrl Pts',(4.37893625271658,-0.158333333333335,
9.01868349747425));
#55790=CARTESIAN_POINT('Ctrl Pts',(4.39121487505806,0.158333333333337,8.98897343669169));
#55791=CARTESIAN_POINT('Ctrl Pts',(4.43220026295886,0.319434907277172,9.0005578427106));
#55792=CARTESIAN_POINT('Ctrl Pts',(4.50639783396403,0.636309800095217,8.99963585647209));
#55793=CARTESIAN_POINT('Ctrl Pts',(4.57220265609131,0.794772684000856,9.01753081392735));
#55794=CARTESIAN_POINT('Ctrl Pts',(4.63814941728848,1.06847604194645,8.98880692016474));
#55795=CARTESIAN_POINT('Ctrl Pts',(4.66110791114137,1.1851427086144,8.96666319460686));
#55796=CARTESIAN_POINT('Ctrl Pts',(4.67847898949305,1.30000000000386,8.93480925277583));
#55797=CARTESIAN_POINT('Ctrl Pts',(4.60440976406856,-1.30000000000497,9.18026138249439));
#55798=CARTESIAN_POINT('Ctrl Pts',(4.59406355054399,-1.18514270861514,9.20232644769543));
#55799=CARTESIAN_POINT('Ctrl Pts',(4.57889302949929,-1.06847604194682,9.21106553327939));
#55800=CARTESIAN_POINT('Ctrl Pts',(4.53270097556317,-0.794772684000849,
9.20046889045802));
#55801=CARTESIAN_POINT('Ctrl Pts',(4.48064018084823,-0.636309800095198,
9.14943754449245));
#55802=CARTESIAN_POINT('Ctrl Pts',(4.43118040068378,-0.319434907277161,
9.09126173355088));
#55803=CARTESIAN_POINT('Ctrl Pts',(4.40227632851896,-0.158333333333333,
9.04717378278747));
#55804=CARTESIAN_POINT('Ctrl Pts',(4.41485754451359,0.158333333333335,9.01703496000808));
#55805=CARTESIAN_POINT('Ctrl Pts',(4.4566818611374,0.31943490727717,9.03014210602715));
#55806=CARTESIAN_POINT('Ctrl Pts',(4.53107809583426,0.63630980009521,9.02864236167228));
#55807=CARTESIAN_POINT('Ctrl Pts',(4.59817489800802,0.794772684000843,9.04610702271642));
#55808=CARTESIAN_POINT('Ctrl Pts',(4.66069269942063,1.06847604194643,9.01354866946066));
#55809=CARTESIAN_POINT('Ctrl Pts',(4.68114117144808,1.18514270861438,8.98904126395909));
#55810=CARTESIAN_POINT('Ctrl Pts',(4.69497647578415,1.30000000000384,8.95411975767454));
#55811=CARTESIAN_POINT('Ctrl Pts',(4.61912732702719,-1.30000000000496,9.20118553969072));
#55812=CARTESIAN_POINT('Ctrl Pts',(4.6114348104255,-1.18514270861514,9.22755231220806));
#55813=CARTESIAN_POINT('Ctrl Pts',(4.59827465857687,-1.06847604194682,9.23934512619528));
#55814=CARTESIAN_POINT('Ctrl Pts',(4.55524074391044,-0.794772684000851,
9.23292012593516));
#55815=CARTESIAN_POINT('Ctrl Pts',(4.50310673817058,-0.636309800095197,
9.18053241784251));
#55816=CARTESIAN_POINT('Ctrl Pts',(4.45431946760892,-0.319434907277159,
9.12169110392727));
#55817=CARTESIAN_POINT('Ctrl Pts',(4.42489047289185,-0.158333333333332,
9.07569994752371));
#55818=CARTESIAN_POINT('Ctrl Pts',(4.43792035692505,0.158333333333334,9.04492251267268));
#55819=CARTESIAN_POINT('Ctrl Pts',(4.48097546069836,0.319434907277167,9.05887937468661));
#55820=CARTESIAN_POINT('Ctrl Pts',(4.55508919941058,0.636309800095206,9.05758940224239));
#55821=CARTESIAN_POINT('Ctrl Pts',(4.62176651432713,0.79477268400084,9.07738490555604));
#55822=CARTESIAN_POINT('Ctrl Pts',(4.6812322428251,1.06847604194643,9.04047819815655));
#55823=CARTESIAN_POINT('Ctrl Pts',(4.69979673838051,1.18514270861437,9.01265747598786));
#55824=CARTESIAN_POINT('Ctrl Pts',(4.71118521904681,1.30000000000384,8.97299157775552));
#55825=CARTESIAN_POINT('Ctrl Pts',(4.62624077063439,-1.30000000000496,9.21200810313932));
#55826=CARTESIAN_POINT('Ctrl Pts',(4.61995220105635,-1.18514270861514,9.24039662831204));
#55827=CARTESIAN_POINT('Ctrl Pts',(4.60783501082454,-1.06847604194682,9.25364960997313));
#55828=CARTESIAN_POINT('Ctrl Pts',(4.566376597632,-0.794772684000851,9.24930051549322));
#55829=CARTESIAN_POINT('Ctrl Pts',(4.5139835392274,-0.636309800095197,9.19656574141252));
#55830=CARTESIAN_POINT('Ctrl Pts',(4.46556375514821,-0.319434907277159,
9.13735044965255));
#55831=CARTESIAN_POINT('Ctrl Pts',(4.43611716307415,-0.158333333333332,
9.09005714685182));
#55832=CARTESIAN_POINT('Ctrl Pts',(4.44941966576161,0.158333333333334,9.05889701834647));
#55833=CARTESIAN_POINT('Ctrl Pts',(4.49284772594685,0.319434907277167,9.07364899676505));
#55834=CARTESIAN_POINT('Ctrl Pts',(4.5669807465074,0.636309800095206,9.07220674691494));
#55835=CARTESIAN_POINT('Ctrl Pts',(4.63406245451013,0.79477268400084,9.09217501942727));
#55836=CARTESIAN_POINT('Ctrl Pts',(4.6919201451545,1.06847604194643,9.05326217342387));
#55837=CARTESIAN_POINT('Ctrl Pts',(4.70935397490034,1.18514270861437,9.02411271480519));
#55838=CARTESIAN_POINT('Ctrl Pts',(4.71917718395066,1.30000000000384,8.98265772673976));
#55839=CARTESIAN_POINT('',(4.63725822693025,1.2,8.93157042500954));
#55840=CARTESIAN_POINT('Ctrl Pts',(4.63725822693025,1.2,8.93157042500954));
#55841=CARTESIAN_POINT('Ctrl Pts',(4.63128124328469,1.20916376532628,8.92138093370866));
#55842=CARTESIAN_POINT('Ctrl Pts',(4.62563454624119,1.21806711335843,8.91099649596368));
#55843=CARTESIAN_POINT('Ctrl Pts',(4.61446044706189,1.23542033719071,8.89112890253183));
#55844=CARTESIAN_POINT('Ctrl Pts',(4.61284959590184,1.2377794891268,8.88867625506117));
#55845=CARTESIAN_POINT('Ctrl Pts',(4.59902849842327,1.25867388818129,8.86555040087628));
#55846=CARTESIAN_POINT('Ctrl Pts',(4.59370304156697,1.26674865903275,8.85652559222203));
#55847=CARTESIAN_POINT('Ctrl Pts',(4.58430375459195,1.28086893631048,8.84092122371427));
#55848=CARTESIAN_POINT('Ctrl Pts',(4.57606112972981,1.2931885321623,8.82736295603023));
#55849=CARTESIAN_POINT('Ctrl Pts',(4.57140911795195,1.30000000000385,8.82009835388732));
#55850=CARTESIAN_POINT('',(4.58017336109578,0.65383484136663,9.07736836607464));
#55851=CARTESIAN_POINT('Ctrl Pts',(4.58017336113235,0.653834841365347,9.07736836608417));
#55852=CARTESIAN_POINT('Ctrl Pts',(4.58629935664999,0.71749686228372,9.06242291265736));
#55853=CARTESIAN_POINT('Ctrl Pts',(4.59129975116674,0.764620654576998,9.05006536969652));
#55854=CARTESIAN_POINT('Ctrl Pts',(4.61047635077669,0.949828416998684,9.00201087745227));
#55855=CARTESIAN_POINT('Ctrl Pts',(4.6216073392214,1.05665100713802,8.9734845202946));
#55856=CARTESIAN_POINT('Ctrl Pts',(4.63725822693025,1.2,8.93157042500954));
#55857=CARTESIAN_POINT('',(4.52544944337377,-0.653834841531101,9.20569372922889));
#55858=CARTESIAN_POINT('Ctrl Pts',(4.52544944337376,-0.6538348415311,9.20569372922889));
#55859=CARTESIAN_POINT('Ctrl Pts',(4.49807563320008,-0.575992875294331,
9.17441322987441));
#55860=CARTESIAN_POINT('Ctrl Pts',(4.47549584426781,-0.493634267952995,
9.1474433434323));
#55861=CARTESIAN_POINT('Ctrl Pts',(4.44490715110221,-0.33812193113357,9.10711659987178));
#55862=CARTESIAN_POINT('Ctrl Pts',(4.43509965619256,-0.265647808821891,
9.09215933056172));
#55863=CARTESIAN_POINT('Ctrl Pts',(4.42552631194356,-0.129708474507909,
9.0697518790094));
#55864=CARTESIAN_POINT('Ctrl Pts',(4.42449090793631,-0.066620743275029,
9.06154502477452));
#55865=CARTESIAN_POINT('Ctrl Pts',(4.42937482211724,0.0595420623316575,
9.04914518506414));
#55866=CARTESIAN_POINT('Ctrl Pts',(4.43531371317915,0.122769838845346,9.04485596687489));
#55867=CARTESIAN_POINT('Ctrl Pts',(4.45561375097078,0.260120332718061,9.0406046621017));
#55868=CARTESIAN_POINT('Ctrl Pts',(4.47131835950836,0.333940862872961,9.0415746906149));
#55869=CARTESIAN_POINT('Ctrl Pts',(4.51500250949231,0.491202455585993,9.05172634132229));
#55870=CARTESIAN_POINT('Ctrl Pts',(4.54480743097227,0.57434536642225,9.06214198151124));
#55871=CARTESIAN_POINT('Ctrl Pts',(4.58017336108264,0.653834841383517,9.07736836601699));
#55872=CARTESIAN_POINT('',(4.55428580344216,-1.2,9.13932483626781));
#55873=CARTESIAN_POINT('Ctrl Pts',(4.55428580344216,-1.2,9.13932483626781));
#55874=CARTESIAN_POINT('Ctrl Pts',(4.55060440973257,-1.14982825705369,9.14797017447775));
#55875=CARTESIAN_POINT('Ctrl Pts',(4.54418965220607,-1.0610632869042,9.16298565727555));
#55876=CARTESIAN_POINT('Ctrl Pts',(4.53001580454928,-0.792138505468391,
9.195405511297));
#55877=CARTESIAN_POINT('Ctrl Pts',(4.52801179202698,-0.738397016064537,
9.19991229853613));
#55878=CARTESIAN_POINT('Ctrl Pts',(4.52544944337376,-0.653834841531101,
9.20569372922889));
#55879=CARTESIAN_POINT('Ctrl Pts',(4.4908419881269,-1.3,9.03162175071067));
#55880=CARTESIAN_POINT('Ctrl Pts',(4.50210674878835,-1.28289219427241,9.04930258333981));
#55881=CARTESIAN_POINT('Ctrl Pts',(4.51263386006301,-1.26612351152865,9.06776363958348));
#55882=CARTESIAN_POINT('Ctrl Pts',(4.52785419473793,-1.24234399593774,9.09305279140919));
#55883=CARTESIAN_POINT('Ctrl Pts',(4.53122248474684,-1.23728725185213,9.09811956679317));
#55884=CARTESIAN_POINT('Ctrl Pts',(4.54397312679041,-1.2167518469017,9.12075188380719));
#55885=CARTESIAN_POINT('Ctrl Pts',(4.54922724341664,-1.20832960273817,9.12994352731759));
#55886=CARTESIAN_POINT('Ctrl Pts',(4.55428580344217,-1.2,9.13932483626781));
#55887=CARTESIAN_POINT('Origin',(0.,1.25,7.2));
#55888=CARTESIAN_POINT('Origin',(0.,1.2,7.2));
#55889=CARTESIAN_POINT('Origin',(0.,0.92691742076555,7.2));
#55890=CARTESIAN_POINT('Origin',(0.,0.653834841531101,7.2));
#55891=CARTESIAN_POINT('Origin',(0.,0.,7.2));
#55892=CARTESIAN_POINT('Origin',(0.,-0.653834841531101,7.2));
#55893=CARTESIAN_POINT('Origin',(0.,-0.926917420765551,7.2));
#55894=CARTESIAN_POINT('Origin',(0.,-1.2,7.2));
#55895=CARTESIAN_POINT('Origin',(0.,-1.25,7.2));
#55896=CARTESIAN_POINT('Ctrl Pts',(4.48251875583964,-1.30000000000184,9.51420125914222));
#55897=CARTESIAN_POINT('Ctrl Pts',(4.50675280588356,-1.18514270861303,9.47916239086718));
#55898=CARTESIAN_POINT('Ctrl Pts',(4.51674956615302,-1.06847604194575,9.4467017355834));
#55899=CARTESIAN_POINT('Ctrl Pts',(4.50695309468149,-0.794772684000851,
9.37766731592577));
#55900=CARTESIAN_POINT('Ctrl Pts',(4.44722735233531,-0.636309800095197,
9.34117727403155));
#55901=CARTESIAN_POINT('Ctrl Pts',(4.39869447984843,-0.319434907277159,
9.28512064988765));
#55902=CARTESIAN_POINT('Ctrl Pts',(4.35867257917745,-0.158333333333332,
9.26271831194526));
#55903=CARTESIAN_POINT('Ctrl Pts',(4.37292795574814,0.158333333333334,9.23198243022624));
#55904=CARTESIAN_POINT('Ctrl Pts',(4.42777734501438,0.319434907277167,9.22222011637453));
#55905=CARTESIAN_POINT('Ctrl Pts',(4.50418204215397,0.636309800095206,9.21858026428182));
#55906=CARTESIAN_POINT('Ctrl Pts',(4.57842941556978,0.79477268400084,9.22222944316713));
#55907=CARTESIAN_POINT('Ctrl Pts',(4.6094025157868,1.06847604194648,9.25012893617736));
#55908=CARTESIAN_POINT('Ctrl Pts',(4.60766161389181,1.18514270861448,9.26800173905295));
#55909=CARTESIAN_POINT('Ctrl Pts',(4.59077270268428,1.30000000000399,9.29167068805804));
#55910=CARTESIAN_POINT('Ctrl Pts',(4.47625324740048,-1.30000000000184,9.51446562353792));
#55911=CARTESIAN_POINT('Ctrl Pts',(4.49929883545649,-1.18514270861303,9.4794437109002));
#55912=CARTESIAN_POINT('Ctrl Pts',(4.50842359237374,-1.06847604194575,9.44700748050992));
#55913=CARTESIAN_POINT('Ctrl Pts',(4.4973437014707,-0.794772684000851,9.37804674271844));
#55914=CARTESIAN_POINT('Ctrl Pts',(4.43781745126807,-0.636309800095197,
9.34164915954862));
#55915=CARTESIAN_POINT('Ctrl Pts',(4.38923444772865,-0.319434907277159,
9.28565064674039));
#55916=CARTESIAN_POINT('Ctrl Pts',(4.34963276865795,-0.158333333333332,
9.26312087075345));
#55917=CARTESIAN_POINT('Ctrl Pts',(4.36383715556681,0.158333333333334,9.23261432262395));
#55918=CARTESIAN_POINT('Ctrl Pts',(4.41819681569251,0.319434907277167,9.22328112308529));
#55919=CARTESIAN_POINT('Ctrl Pts',(4.49458550119995,0.636309800095206,9.21990293883793));
#55920=CARTESIAN_POINT('Ctrl Pts',(4.56861724441485,0.79477268400084,9.22357197712616));
#55921=CARTESIAN_POINT('Ctrl Pts',(4.60088880207979,1.06847604194648,9.25136235697374));
#55922=CARTESIAN_POINT('Ctrl Pts',(4.60003939698503,1.18514270861448,9.26913417417586));
#55923=CARTESIAN_POINT('Ctrl Pts',(4.58437142526133,1.30000000000399,9.29264838287906));
#55924=CARTESIAN_POINT('Ctrl Pts',(4.4636537898411,-1.30000000000163,9.5151766357535));
#55925=CARTESIAN_POINT('Ctrl Pts',(4.48437051028303,-1.18514270861284,9.48004204082684));
#55926=CARTESIAN_POINT('Ctrl Pts',(4.49178865623133,-1.06847604194558,9.44753738145579));
#55927=CARTESIAN_POINT('Ctrl Pts',(4.47820368991595,-0.794772684000723,
9.37852079302433));
#55928=CARTESIAN_POINT('Ctrl Pts',(4.4191182508642,-0.636309800095096,9.34213437097525));
#55929=CARTESIAN_POINT('Ctrl Pts',(4.37038259295847,-0.319434907277108,
9.28643717126287));
#55930=CARTESIAN_POINT('Ctrl Pts',(4.33146875773393,-0.158333333333307,
9.2642035768315));
#55931=CARTESIAN_POINT('Ctrl Pts',(4.34553130112576,0.158333333333309,9.23430515295839));
#55932=CARTESIAN_POINT('Ctrl Pts',(4.39899684163401,0.319434907277116,9.22553420796642));
#55933=CARTESIAN_POINT('Ctrl Pts',(4.47538050033928,0.636309800095105,9.22258354874013));
#55934=CARTESIAN_POINT('Ctrl Pts',(4.54896787756259,0.794772684000714,9.22632763177204));
#55935=CARTESIAN_POINT('Ctrl Pts',(4.58383417417162,1.06847604194631,9.25390659861801));
#55936=CARTESIAN_POINT('Ctrl Pts',(4.58476621776767,1.18514270861429,9.27148350566701));
#55937=CARTESIAN_POINT('Ctrl Pts',(4.57153797708125,1.30000000000378,9.29469940691876));
#55938=CARTESIAN_POINT('Ctrl Pts',(4.44507713121895,-1.3000000000013,9.51538739937688));
#55939=CARTESIAN_POINT('Ctrl Pts',(4.46185228716617,-1.18514270861254,9.48147746182544));
#55940=CARTESIAN_POINT('Ctrl Pts',(4.46643042464635,-1.06847604194531,9.44972969566701));
#55941=CARTESIAN_POINT('Ctrl Pts',(4.44882928541479,-0.794772684000524,
9.38138105318114));
#55942=CARTESIAN_POINT('Ctrl Pts',(4.390854245645,-0.636309800094935,9.34354911727094));
#55943=CARTESIAN_POINT('Ctrl Pts',(4.34213240301002,-0.319434907277027,
9.28744768961452));
#55944=CARTESIAN_POINT('Ctrl Pts',(4.30436347268256,-0.158333333333267,
9.26527844603672));
#55945=CARTESIAN_POINT('Ctrl Pts',(4.3183608160147,0.158333333333269,9.23567613861453));
#55946=CARTESIAN_POINT('Ctrl Pts',(4.37056632183711,0.319434907277035,9.22726662244557));
#55947=CARTESIAN_POINT('Ctrl Pts',(4.44690506070763,0.636309800094944,9.22505924439812));
#55948=CARTESIAN_POINT('Ctrl Pts',(4.51956844370301,0.794772684000513,9.22997966496454));
#55949=CARTESIAN_POINT('Ctrl Pts',(4.55835037802316,1.06847604194604,9.25723650525971));
#55950=CARTESIAN_POINT('Ctrl Pts',(4.56202364758899,1.18514270861399,9.27430113235338));
#55951=CARTESIAN_POINT('Ctrl Pts',(4.55258292436565,1.30000000000345,9.29663191034234));
#55952=CARTESIAN_POINT('Ctrl Pts',(4.42643317267789,-1.30000000000096,9.515578775066));
#55953=CARTESIAN_POINT('Ctrl Pts',(4.43974876127799,-1.18514270861223,9.48130961825889));
#55954=CARTESIAN_POINT('Ctrl Pts',(4.4417700587056,-1.06847604194503,9.44939627659556));
#55955=CARTESIAN_POINT('Ctrl Pts',(4.42034758809898,-0.794772684000313,
9.38111247737266));
#55956=CARTESIAN_POINT('Ctrl Pts',(4.36277825954423,-0.636309800094768,
9.34422411328257));
#55957=CARTESIAN_POINT('Ctrl Pts',(4.31387722949841,-0.319434907276944,
9.28837259268112));
#55958=CARTESIAN_POINT('Ctrl Pts',(4.2774674602139,-0.158333333333226,9.26549350140391));
#55959=CARTESIAN_POINT('Ctrl Pts',(4.29133181086155,0.158333333333228,9.23645138949429));
#55960=CARTESIAN_POINT('Ctrl Pts',(4.34207293703372,0.319434907276952,9.22919622035688));
#55961=CARTESIAN_POINT('Ctrl Pts',(4.41826339299713,0.636309800094779,9.22811567796723));
#55962=CARTESIAN_POINT('Ctrl Pts',(4.490057534896,0.794772684000307,9.2339656388837));
#55963=CARTESIAN_POINT('Ctrl Pts',(4.5327322702054,1.06847604194576,9.26098446136783));
#55964=CARTESIAN_POINT('Ctrl Pts',(4.53913143621231,1.18514270861368,9.2776017498823));
#55965=CARTESIAN_POINT('Ctrl Pts',(4.53345745656538,1.30000000000311,9.29914087980385));
#55966=CARTESIAN_POINT('Ctrl Pts',(4.41373519238219,-1.30000000000076,9.51624950733163));
#55967=CARTESIAN_POINT('Ctrl Pts',(4.42460441374993,-1.18514270861205,9.4821579466063));
#55968=CARTESIAN_POINT('Ctrl Pts',(4.42484694140117,-1.06847604194486,9.45034196039577));
#55969=CARTESIAN_POINT('Ctrl Pts',(4.40085744044516,-0.794772684000194,
9.38209769983969));
#55970=CARTESIAN_POINT('Ctrl Pts',(4.34386504757947,-0.63630980009467,9.34478404741106));
#55971=CARTESIAN_POINT('Ctrl Pts',(4.29486459997575,-0.319434907276894,
9.28904431421725));
#55972=CARTESIAN_POINT('Ctrl Pts',(4.25911395670897,-0.158333333333201,
9.26661498524898));
#55973=CARTESIAN_POINT('Ctrl Pts',(4.27291141754749,0.158333333333204,9.23785393627474));
#55974=CARTESIAN_POINT('Ctrl Pts',(4.32289562721979,0.319434907276904,9.2305201364458));
#55975=CARTESIAN_POINT('Ctrl Pts',(4.39911219346208,0.636309800094681,9.2297168481906));
#55976=CARTESIAN_POINT('Ctrl Pts',(4.47031997754529,0.794772684000183,9.2361776056407));
#55977=CARTESIAN_POINT('Ctrl Pts',(4.51562250607443,1.06847604194559,9.26301592798594));
#55978=CARTESIAN_POINT('Ctrl Pts',(4.52384920305348,1.18514270861349,9.27936931824648));
#55979=CARTESIAN_POINT('Ctrl Pts',(4.52069281103532,1.30000000000291,9.30045878348211));
#55980=CARTESIAN_POINT('Ctrl Pts',(4.40732364295139,-1.30000000000072,9.5163476170774));
#55981=CARTESIAN_POINT('Ctrl Pts',(4.41688212528442,-1.185142708612,9.4825166004766));
#55982=CARTESIAN_POINT('Ctrl Pts',(4.41617619561562,-1.06847604194482,9.45085919745731));
#55983=CARTESIAN_POINT('Ctrl Pts',(4.3908325117472,-0.794772684000164,9.38274574564437));
#55984=CARTESIAN_POINT('Ctrl Pts',(4.33416209500732,-0.636309800094647,
9.34514478063228));
#55985=CARTESIAN_POINT('Ctrl Pts',(4.28517680049427,-0.319434907276883,
9.28922943073272));
#55986=CARTESIAN_POINT('Ctrl Pts',(4.24989006589237,-0.158333333333196,
9.26657728374074));
#55987=CARTESIAN_POINT('Ctrl Pts',(4.26364781909912,0.158333333333198,9.23798085352293));
#55988=CARTESIAN_POINT('Ctrl Pts',(4.31309155506437,0.319434907276893,9.23116227835363));
#55989=CARTESIAN_POINT('Ctrl Pts',(4.38928716252029,0.636309800094658,9.2306096286486));
#55990=CARTESIAN_POINT('Ctrl Pts',(4.46029277662821,0.794772684000154,9.23699316303097));
#55991=CARTESIAN_POINT('Ctrl Pts',(4.50693744924969,1.06847604194556,9.26375131247191));
#55992=CARTESIAN_POINT('Ctrl Pts',(4.5160820507918,1.18514270861345,9.28004256007604));
#55993=CARTESIAN_POINT('Ctrl Pts',(4.51418050345352,1.30000000000286,9.30104244387841));
#55994=CARTESIAN_POINT('Ctrl Pts',(4.40693494709678,-1.30000000000072,9.51635378924249));
#55995=CARTESIAN_POINT('Ctrl Pts',(4.41641424333561,-1.185142708612,9.48253774192878));
#55996=CARTESIAN_POINT('Ctrl Pts',(4.41565098622941,-1.06847604194483,9.45088943875991));
#55997=CARTESIAN_POINT('Ctrl Pts',(4.39022536238229,-0.794772684000165,
9.38278344984892));
#55998=CARTESIAN_POINT('Ctrl Pts',(4.33357424794786,-0.636309800094647,
9.34516565367199));
#55999=CARTESIAN_POINT('Ctrl Pts',(4.28458959106321,-0.319434907276883,
9.28924061795055));
#56000=CARTESIAN_POINT('Ctrl Pts',(4.24933053908302,-0.158333333333196,
9.26657659299652));
#56001=CARTESIAN_POINT('Ctrl Pts',(4.26308592317885,0.158333333333198,9.23798998978505));
#56002=CARTESIAN_POINT('Ctrl Pts',(4.31249752241387,0.319434907276893,9.23120031554562));
#56003=CARTESIAN_POINT('Ctrl Pts',(4.38869191352301,0.636309800094659,9.23066271091136));
#56004=CARTESIAN_POINT('Ctrl Pts',(4.45968470525621,0.794772684000155,9.23704377278317));
#56005=CARTESIAN_POINT('Ctrl Pts',(4.50641071191899,1.06847604194556,9.26379718946541));
#56006=CARTESIAN_POINT('Ctrl Pts',(4.51561104408737,1.18514270861345,9.28008433893661));
#56007=CARTESIAN_POINT('Ctrl Pts',(4.51378575150887,1.30000000000286,9.30107807510901));
#56008=CARTESIAN_POINT('Ctrl Pts',(4.40625511335241,-1.30000000000072,9.51636345978948));
#56009=CARTESIAN_POINT('Ctrl Pts',(4.41559577277618,-1.185142708612,9.48257376197577));
#56010=CARTESIAN_POINT('Ctrl Pts',(4.41473214646469,-1.06847604194482,9.45094150564397));
#56011=CARTESIAN_POINT('Ctrl Pts',(4.38916305550854,-0.794772684000165,
9.38284878692444));
#56012=CARTESIAN_POINT('Ctrl Pts',(4.33254567044107,-0.636309800094647,
9.34520178464511));
#56013=CARTESIAN_POINT('Ctrl Pts',(4.28356221756368,-0.319434907276883,
9.28925946376379));
#56014=CARTESIAN_POINT('Ctrl Pts',(4.24835188088717,-0.158333333333196,
9.26657361786353));
#56015=CARTESIAN_POINT('Ctrl Pts',(4.26210308617438,0.158333333333198,9.23800430500409));
#56016=CARTESIAN_POINT('Ctrl Pts',(4.3114581334876,0.319434907276893,9.2312663631012));
#56017=CARTESIAN_POINT('Ctrl Pts',(4.3876502593518,0.636309800094659,9.23075555468273));
#56018=CARTESIAN_POINT('Ctrl Pts',(4.45862071633395,0.794772684000154,9.23713186553507));
#56019=CARTESIAN_POINT('Ctrl Pts',(4.50548899771879,1.06847604194556,9.26387717733866));
#56020=CARTESIAN_POINT('Ctrl Pts',(4.51478681262742,1.18514270861345,9.28015730713193));
#56021=CARTESIAN_POINT('Ctrl Pts',(4.51309490007407,1.30000000000286,9.3011405122501));
#56022=CARTESIAN_POINT('Ctrl Pts',(4.40489630813951,-1.30000000000072,9.51637992315095));
#56023=CARTESIAN_POINT('Ctrl Pts',(4.4139602797652,-1.185142708612,9.48264089498604));
#56024=CARTESIAN_POINT('Ctrl Pts',(4.41289624599819,-1.06847604194483,9.45103956130732));
#56025=CARTESIAN_POINT('Ctrl Pts',(4.38704039657951,-0.794772684000165,
9.38297266059196));
#56026=CARTESIAN_POINT('Ctrl Pts',(4.33048964010808,-0.636309800094648,
9.34526993358207));
#56027=CARTESIAN_POINT('Ctrl Pts',(4.28150803914452,-0.319434907276883,
9.28929483673244));
#56028=CARTESIAN_POINT('Ctrl Pts',(4.24639473941324,-0.158333333333196,
9.26656675541383));
#56029=CARTESIAN_POINT('Ctrl Pts',(4.26013758794051,0.158333333333198,9.2380318952314));
#56030=CARTESIAN_POINT('Ctrl Pts',(4.30938034274635,0.319434907276893,9.23139432594687));
#56031=CARTESIAN_POINT('Ctrl Pts',(4.38556764694175,0.63630980009466,9.23093822745109));
#56032=CARTESIAN_POINT('Ctrl Pts',(4.45649207513945,0.794772684000156,9.23731024709754));
#56033=CARTESIAN_POINT('Ctrl Pts',(4.50364469895256,1.06847604194556,9.26404023102797));
#56034=CARTESIAN_POINT('Ctrl Pts',(4.51313763686427,1.18514270861345,9.2803057751366));
#56035=CARTESIAN_POINT('Ctrl Pts',(4.51171288901579,1.30000000000287,9.30126644375381));
#56036=CARTESIAN_POINT('Ctrl Pts',(4.40295803520288,-1.30000000000072,9.51639394221811));
#56037=CARTESIAN_POINT('Ctrl Pts',(4.41162876886495,-1.18514270861201,9.48272037623868));
#56038=CARTESIAN_POINT('Ctrl Pts',(4.41027958777538,-1.06847604194483,9.45115925064401));
#56039=CARTESIAN_POINT('Ctrl Pts',(4.38401470200241,-0.794772684000167,
9.38312689662002));
#56040=CARTESIAN_POINT('Ctrl Pts',(4.32755626093074,-0.636309800094648,
9.34535399900702));
#56041=CARTESIAN_POINT('Ctrl Pts',(4.27857540304651,-0.319434907276883,
9.28933824055801));
#56042=CARTESIAN_POINT('Ctrl Pts',(4.24359943941272,-0.158333333333196,
9.26655422181915));
#56043=CARTESIAN_POINT('Ctrl Pts',(4.257330269631,0.158333333333198,9.2380684615706));
#56044=CARTESIAN_POINT('Ctrl Pts',(4.30641513030752,0.319434907276894,9.2315648170422));
#56045=CARTESIAN_POINT('Ctrl Pts',(4.38259460579412,0.63630980009466,9.23119055161795));
#56046=CARTESIAN_POINT('Ctrl Pts',(4.45344909871239,0.794772684000156,9.23757258812502));
#56047=CARTESIAN_POINT('Ctrl Pts',(4.50100714780742,1.06847604194556,9.26428370184697));
#56048=CARTESIAN_POINT('Ctrl Pts',(4.51077922924535,1.18514270861345,9.2805268872598));
#56049=CARTESIAN_POINT('Ctrl Pts',(4.50973727486727,1.30000000000287,9.30145100669949));
#56050=CARTESIAN_POINT('Ctrl Pts',(4.40063620137717,-1.30000000000072,9.51639636097817));
#56051=CARTESIAN_POINT('Ctrl Pts',(4.40884040560399,-1.18514270861201,9.48278358005253));
#56052=CARTESIAN_POINT('Ctrl Pts',(4.40715216314469,-1.06847604194483,9.45126031194313));
#56053=CARTESIAN_POINT('Ctrl Pts',(4.38039845450992,-0.794772684000169,
9.38326244901355));
#56054=CARTESIAN_POINT('Ctrl Pts',(4.32404406839143,-0.63630980009465,9.3454270707552));
#56055=CARTESIAN_POINT('Ctrl Pts',(4.27505914465387,-0.319434907276884,
9.28937895677977));
#56056=CARTESIAN_POINT('Ctrl Pts',(4.24024360938201,-0.158333333333197,
9.26654337849712));
#56057=CARTESIAN_POINT('Ctrl Pts',(4.25396001813677,0.158333333333199,9.23811575818366));
#56058=CARTESIAN_POINT('Ctrl Pts',(4.30286294992823,0.319434907276894,9.2317445901503));
#56059=CARTESIAN_POINT('Ctrl Pts',(4.37903153532005,0.636309800094662,9.23147471197206));
#56060=CARTESIAN_POINT('Ctrl Pts',(4.44979163239843,0.794772684000159,9.23790935230491));
#56061=CARTESIAN_POINT('Ctrl Pts',(4.49783488694176,1.06847604194556,9.2646031551418));
#56062=CARTESIAN_POINT('Ctrl Pts',(4.50794326995182,1.18514270861346,9.28081450128029));
#56063=CARTESIAN_POINT('Ctrl Pts',(4.50736389125802,1.30000000000287,9.30168243541202));
#56064=CARTESIAN_POINT('Ctrl Pts',(4.39600056929137,-1.30000000000072,9.51637194624509));
#56065=CARTESIAN_POINT('Ctrl Pts',(4.4032848721401,-1.18514270861201,9.48283732300393));
#56066=CARTESIAN_POINT('Ctrl Pts',(4.40092622520048,-1.06847604194483,9.45136419869777));
#56067=CARTESIAN_POINT('Ctrl Pts',(4.37320013584774,-0.79477268400017,9.3834174603151));
#56068=CARTESIAN_POINT('Ctrl Pts',(4.31703826235303,-0.636309800094651,
9.34550726188743));
#56069=CARTESIAN_POINT('Ctrl Pts',(4.2680325520994,-0.319434907276885,9.28943663898676));
#56070=CARTESIAN_POINT('Ctrl Pts',(4.23352528126376,-0.158333333333197,
9.26654268431001));
#56071=CARTESIAN_POINT('Ctrl Pts',(4.24721267322164,0.158333333333199,9.23823022692339));
#56072=CARTESIAN_POINT('Ctrl Pts',(4.29577139823858,0.319434907276895,9.23205090857317));
#56073=CARTESIAN_POINT('Ctrl Pts',(4.37191577184974,0.636309800094663,9.23200082102078));
#56074=CARTESIAN_POINT('Ctrl Pts',(4.4424629594934,0.79477268400016,9.23863489727255));
#56075=CARTESIAN_POINT('Ctrl Pts',(4.49147316778346,1.06847604194556,9.26530786724832));
#56076=CARTESIAN_POINT('Ctrl Pts',(4.50225681955632,1.18514270861346,9.28144515444429));
#56077=CARTESIAN_POINT('Ctrl Pts',(4.50260941994036,1.30000000000287,9.30217398846459));
#56078=CARTESIAN_POINT('Ctrl Pts',(4.39061441318341,-1.30000000000076,9.51626458451879));
#56079=CARTESIAN_POINT('Ctrl Pts',(4.3968636067614,-1.18514270861204,9.48269776371229));
#56080=CARTESIAN_POINT('Ctrl Pts',(4.39374548939964,-1.06847604194486,9.45121006362946));
#56081=CARTESIAN_POINT('Ctrl Pts',(4.36490165232186,-0.794772684000192,
9.38327036214381));
#56082=CARTESIAN_POINT('Ctrl Pts',(4.30892116882036,-0.636309800094669,
9.34541395146925));
#56083=CARTESIAN_POINT('Ctrl Pts',(4.25985708215244,-0.319434907276894,
9.28943161594754));
#56084=CARTESIAN_POINT('Ctrl Pts',(4.22567540968377,-0.158333333333201,
9.26658863881072));
#56085=CARTESIAN_POINT('Ctrl Pts',(4.23932815218653,0.158333333333203,9.23840732600793));
#56086=CARTESIAN_POINT('Ctrl Pts',(4.28753888340787,0.319434907276904,9.23225185888506));
#56087=CARTESIAN_POINT('Ctrl Pts',(4.36364609441846,0.636309800094681,9.23249532729164));
#56088=CARTESIAN_POINT('Ctrl Pts',(4.43387415143865,0.794772684000182,9.23963750981833));
#56089=CARTESIAN_POINT('Ctrl Pts',(4.48400376887349,1.06847604194559,9.26631847888963));
#56090=CARTESIAN_POINT('Ctrl Pts',(4.49558416661022,1.18514270861349,9.28233330857485));
#56091=CARTESIAN_POINT('Ctrl Pts',(4.4970457081814,1.30000000000291,9.3028137650616));
#56092=CARTESIAN_POINT('Ctrl Pts',(4.38138051521408,-1.30000000000076,9.51606529202356));
#56093=CARTESIAN_POINT('Ctrl Pts',(4.3858740921445,-1.18514270861204,9.48237596358173));
#56094=CARTESIAN_POINT('Ctrl Pts',(4.38146750644091,-1.06847604194486,9.45081488014051));
#56095=CARTESIAN_POINT('Ctrl Pts',(4.35072625577525,-0.794772684000191,
9.38281913532378));
#56096=CARTESIAN_POINT('Ctrl Pts',(4.29505520611644,-0.636309800094668,
9.3450577261607));
#56097=CARTESIAN_POINT('Ctrl Pts',(4.24588137556484,-0.319434907276893,
9.28926085579798));
#56098=CARTESIAN_POINT('Ctrl Pts',(4.21223423013499,-0.158333333333201,
9.26659537988078));
#56099=CARTESIAN_POINT('Ctrl Pts',(4.22582062844705,0.158333333333203,9.23865691599574));
#56100=CARTESIAN_POINT('Ctrl Pts',(4.27344941401814,0.319434907276903,9.23247303789332));
#56101=CARTESIAN_POINT('Ctrl Pts',(4.3494926805306,0.636309800094679,9.23321668657625));
#56102=CARTESIAN_POINT('Ctrl Pts',(4.41916887909758,0.79477268400018,9.24125576604867));
#56103=CARTESIAN_POINT('Ctrl Pts',(4.4712039151015,1.06847604194559,9.26800796128312));
#56104=CARTESIAN_POINT('Ctrl Pts',(4.48414225235254,1.18514270861349,9.2838457080482));
#56105=CARTESIAN_POINT('Ctrl Pts',(4.48749488785651,1.30000000000291,9.30394116752782));
#56106=CARTESIAN_POINT('Ctrl Pts',(4.36900022363105,-1.30000000000082,9.5160307765818));
#56107=CARTESIAN_POINT('Ctrl Pts',(4.37103552052153,-1.1851427086121,9.48255553524329));
#56108=CARTESIAN_POINT('Ctrl Pts',(4.36484769496369,-1.06847604194491,9.45109997584673));
#56109=CARTESIAN_POINT('Ctrl Pts',(4.3315555221693,-0.794772684000226,9.38309721029964));
#56110=CARTESIAN_POINT('Ctrl Pts',(4.27646882106592,-0.636309800094698,
9.3449197704111));
#56111=CARTESIAN_POINT('Ctrl Pts',(4.22731242869909,-0.319434907276909,
9.28882624102019));
#56112=CARTESIAN_POINT('Ctrl Pts',(4.19454828163421,-0.158333333333209,
9.26580707041848));
#56113=CARTESIAN_POINT('Ctrl Pts',(4.20804004063657,0.158333333333211,9.23821287817429));
#56114=CARTESIAN_POINT('Ctrl Pts',(4.25463605943907,0.319434907276918,9.23289355404711));
#56115=CARTESIAN_POINT('Ctrl Pts',(4.33058140830202,0.63630980009471,9.23429579125412));
#56116=CARTESIAN_POINT('Ctrl Pts',(4.39976178926623,0.794772684000219,9.24257867334419));
#56117=CARTESIAN_POINT('Ctrl Pts',(4.45436072170246,1.06847604194564,9.26934382114282));
#56118=CARTESIAN_POINT('Ctrl Pts',(4.46907953701949,1.18514270861355,9.28507758450468));
#56119=CARTESIAN_POINT('Ctrl Pts',(4.47488331289161,1.30000000000297,9.30495947049279));
#56120=CARTESIAN_POINT('Ctrl Pts',(4.35192791261779,-1.30000000000091,9.51610713954233));
#56121=CARTESIAN_POINT('Ctrl Pts',(4.35054611088779,-1.18514270861218,9.48303106026128));
#56122=CARTESIAN_POINT('Ctrl Pts',(4.3418827947019,-1.06847604194499,9.45179530857522));
#56123=CARTESIAN_POINT('Ctrl Pts',(4.30504704616706,-0.794772684000287,
9.38388599839058));
#56124=CARTESIAN_POINT('Ctrl Pts',(4.25076713902507,-0.636309800094743,
9.34512876400693));
#56125=CARTESIAN_POINT('Ctrl Pts',(4.20165589012478,-0.31943490727693,9.2885679982112));
#56126=CARTESIAN_POINT('Ctrl Pts',(4.17013613981169,-0.15833333333322,9.26498708049703));
#56127=CARTESIAN_POINT('Ctrl Pts',(4.18355074309137,0.158333333333222,9.23769387423214));
#56128=CARTESIAN_POINT('Ctrl Pts',(4.22879523333919,0.319434907276941,9.23330848676313));
#56129=CARTESIAN_POINT('Ctrl Pts',(4.30459933720093,0.636309800094755,9.23564601060515));
#56130=CARTESIAN_POINT('Ctrl Pts',(4.37300885395577,0.794772684000274,9.2445977591603));
#56131=CARTESIAN_POINT('Ctrl Pts',(4.43108597948329,1.06847604194572,9.27154766519164));
#56132=CARTESIAN_POINT('Ctrl Pts',(4.4482401057954,1.18514270861363,9.28717976384003));
#56133=CARTESIAN_POINT('Ctrl Pts',(4.45740892274821,1.30000000000306,9.30677834540822));
#56134=CARTESIAN_POINT('Ctrl Pts',(4.32733788924607,-1.30000000000102,9.51541096929758));
#56135=CARTESIAN_POINT('Ctrl Pts',(4.32121146294237,-1.18514270861228,9.48217278909515));
#56136=CARTESIAN_POINT('Ctrl Pts',(4.30910080586344,-1.06847604194508,9.45075308655846));
#56137=CARTESIAN_POINT('Ctrl Pts',(4.26729799505055,-0.794772684000351,
9.38236833540205));
#56138=CARTESIAN_POINT('Ctrl Pts',(4.21413587457917,-0.636309800094796,
9.34297025808628));
#56139=CARTESIAN_POINT('Ctrl Pts',(4.1648852499766,-0.319434907276958,9.28638795906878));
#56140=CARTESIAN_POINT('Ctrl Pts',(4.13484613211291,-0.158333333333233,
9.26304383309945));
#56141=CARTESIAN_POINT('Ctrl Pts',(4.14792251264182,0.158333333333235,9.23688755391369));
#56142=CARTESIAN_POINT('Ctrl Pts',(4.19114634054308,0.319434907276968,9.23402788190919));
#56143=CARTESIAN_POINT('Ctrl Pts',(4.26681195134328,0.636309800094809,9.23742851588972));
#56144=CARTESIAN_POINT('Ctrl Pts',(4.33436034864448,0.794772684000341,9.2463596608503));
#56145=CARTESIAN_POINT('Ctrl Pts',(4.39760093960311,1.06847604194581,9.27326308511272));
#56146=CARTESIAN_POINT('Ctrl Pts',(4.4183083085949,1.18514270861373,9.2887637381985));
#56147=CARTESIAN_POINT('Ctrl Pts',(4.43234853804718,1.30000000000317,9.30811954887692));
#56148=CARTESIAN_POINT('Ctrl Pts',(4.30273880285957,-1.30000000000114,9.51468456739312));
#56149=CARTESIAN_POINT('Ctrl Pts',(4.29187060135338,-1.18514270861239,9.48126859996238));
#56150=CARTESIAN_POINT('Ctrl Pts',(4.27627765814262,-1.06847604194517,9.44976536215955));
#56151=CARTESIAN_POINT('Ctrl Pts',(4.22933974144936,-0.794772684000421,
9.38140536871477));
#56152=CARTESIAN_POINT('Ctrl Pts',(4.17691683537209,-0.636309800094852,
9.34251697935878));
#56153=CARTESIAN_POINT('Ctrl Pts',(4.12751372739255,-0.319434907276985,
9.28594210505695));
#56154=CARTESIAN_POINT('Ctrl Pts',(4.09917775569068,-0.158333333333247,
9.26219277655249));
#56155=CARTESIAN_POINT('Ctrl Pts',(4.11230177225596,0.158333333333249,9.23590136321851));
#56156=CARTESIAN_POINT('Ctrl Pts',(4.1540238940554,0.319434907276995,9.23276786236089));
#56157=CARTESIAN_POINT('Ctrl Pts',(4.22962573168682,0.636309800094862,9.23699369261186));
#56158=CARTESIAN_POINT('Ctrl Pts',(4.29580778766756,0.794772684000408,9.24765378099704));
#56159=CARTESIAN_POINT('Ctrl Pts',(4.36402625703275,1.0684760419459,9.27517340626912));
#56160=CARTESIAN_POINT('Ctrl Pts',(4.388256376591,1.18514270861384,9.29065921387979));
#56161=CARTESIAN_POINT('Ctrl Pts',(4.40718736806254,1.30000000000329,9.30971860302339));
#56162=CARTESIAN_POINT('Ctrl Pts',(4.28117479265866,-1.30000000000118,9.51412312894823));
#56163=CARTESIAN_POINT('Ctrl Pts',(4.26607290792941,-1.18514270861243,9.48076524600039));
#56164=CARTESIAN_POINT('Ctrl Pts',(4.24745842260437,-1.0684760419452,9.44908372835292));
#56165=CARTESIAN_POINT('Ctrl Pts',(4.19634042761899,-0.794772684000445,
9.37976582392113));
#56166=CARTESIAN_POINT('Ctrl Pts',(4.14539567067865,-0.636309800094874,
9.33884536284604));
#56167=CARTESIAN_POINT('Ctrl Pts',(4.09603748520983,-0.319434907276998,
9.28173674872678));
#56168=CARTESIAN_POINT('Ctrl Pts',(4.06882109985603,-0.158333333333252,
9.25872525037652));
#56169=CARTESIAN_POINT('Ctrl Pts',(4.08153941272377,0.158333333333254,9.23368959813871));
#56170=CARTESIAN_POINT('Ctrl Pts',(4.12148988815201,0.319434907277006,9.23175370316326));
#56171=CARTESIAN_POINT('Ctrl Pts',(4.19672222414941,0.636309800094885,9.23768671925175));
#56172=CARTESIAN_POINT('Ctrl Pts',(4.26176605935896,0.794772684000438,9.24968928688449));
#56173=CARTESIAN_POINT('Ctrl Pts',(4.33438372448306,1.06847604194594,9.27762359043197));
#56174=CARTESIAN_POINT('Ctrl Pts',(4.36174457272238,1.18514270861388,9.29295079370866));
#56175=CARTESIAN_POINT('Ctrl Pts',(4.38503277271829,1.30000000000333,9.31151347532423));
#56176=CARTESIAN_POINT('Ctrl Pts',(4.27051303598667,-1.3000000000012,9.51346869990321));
#56177=CARTESIAN_POINT('Ctrl Pts',(4.25344088139478,-1.18514270861245,9.4797098983446));
#56178=CARTESIAN_POINT('Ctrl Pts',(4.23336359696833,-1.06847604194522,9.44780039991522));
#56179=CARTESIAN_POINT('Ctrl Pts',(4.18003860240438,-0.79477268400046,9.3783553352506));
#56180=CARTESIAN_POINT('Ctrl Pts',(4.12924913693472,-0.636309800094885,
9.33814873258178));
#56181=CARTESIAN_POINT('Ctrl Pts',(4.07980211357947,-0.319434907277003,
9.28110399012567));
#56182=CARTESIAN_POINT('Ctrl Pts',(4.05341076727602,-0.158333333333255,
9.25769362498906));
#56183=CARTESIAN_POINT('Ctrl Pts',(4.0661756651677,0.158333333333257,9.23250840130699));
#56184=CARTESIAN_POINT('Ctrl Pts',(4.10543111529468,0.319434907277012,9.23055773383978));
#56185=CARTESIAN_POINT('Ctrl Pts',(4.18067724121201,0.636309800094896,9.23666009916673));
#56186=CARTESIAN_POINT('Ctrl Pts',(4.24524187540873,0.794772684000452,9.24893194569463));
#56187=CARTESIAN_POINT('Ctrl Pts',(4.32002843361178,1.06847604194596,9.27718049743058));
#56188=CARTESIAN_POINT('Ctrl Pts',(4.34889750809698,1.1851427086139,9.29264391254179));
#56189=CARTESIAN_POINT('Ctrl Pts',(4.37426332713616,1.30000000000335,9.31134299142965));
#56190=CARTESIAN_POINT('Ctrl Pts',(4.26513816686888,-1.30000000000121,9.51325891814912));
#56191=CARTESIAN_POINT('Ctrl Pts',(4.24707151218177,-1.18514270861245,9.47932840796016));
#56192=CARTESIAN_POINT('Ctrl Pts',(4.22626625202657,-1.06847604194523,9.44729494305863));
#56193=CARTESIAN_POINT('Ctrl Pts',(4.17187521250272,-0.794772684000461,
9.37767378498013));
#56194=CARTESIAN_POINT('Ctrl Pts',(4.12125301165255,-0.636309800094886,
9.33755155961958));
#56195=CARTESIAN_POINT('Ctrl Pts',(4.07179835604984,-0.319434907277004,
9.28043168037745));
#56196=CARTESIAN_POINT('Ctrl Pts',(4.04582179527502,-0.158333333333255,
9.25681962487196));
#56197=CARTESIAN_POINT('Ctrl Pts',(4.05854114942379,0.158333333333257,9.2317767541839));
#56198=CARTESIAN_POINT('Ctrl Pts',(4.09731949157577,0.319434907277012,9.23021766431748));
#56199=CARTESIAN_POINT('Ctrl Pts',(4.17251465742636,0.636309800094897,9.23658830540946));
#56200=CARTESIAN_POINT('Ctrl Pts',(4.23690164518344,0.794772684000453,9.24881082069698));
#56201=CARTESIAN_POINT('Ctrl Pts',(4.31276279944828,1.06847604194596,9.27725003928142));
#56202=CARTESIAN_POINT('Ctrl Pts',(4.34237324230651,1.1851427086139,9.29282104199691));
#56203=CARTESIAN_POINT('Ctrl Pts',(4.3687566452743,1.30000000000336,9.31165276347954));
#56204=CARTESIAN_POINT('Ctrl Pts',(4.26245981977714,-1.30000000000121,9.51312991696811));
#56205=CARTESIAN_POINT('Ctrl Pts',(4.24389098837022,-1.18514270861245,9.47912613808092));
#56206=CARTESIAN_POINT('Ctrl Pts',(4.22271888801939,-1.06847604194523,9.4470378528054));
#56207=CARTESIAN_POINT('Ctrl Pts',(4.16779302870235,-0.794772684000462,
9.37733266801583));
#56208=CARTESIAN_POINT('Ctrl Pts',(4.11726184280991,-0.636309800094887,
9.33723297019308));
#56209=CARTESIAN_POINT('Ctrl Pts',(4.06780584876013,-0.319434907277004,
9.28006824332014));
#56210=CARTESIAN_POINT('Ctrl Pts',(4.04203758847583,-0.158333333333256,
9.25635174774498));
#56211=CARTESIAN_POINT('Ctrl Pts',(4.05473007673294,0.158333333333258,9.23139149387313));
#56212=CARTESIAN_POINT('Ctrl Pts',(4.09326328303475,0.319434907277013,9.23004610934002));
#56213=CARTESIAN_POINT('Ctrl Pts',(4.16842537053399,0.636309800094898,9.23657560160018));
#56214=CARTESIAN_POINT('Ctrl Pts',(4.23271443442531,0.794772684000455,9.24880740652821));
#56215=CARTESIAN_POINT('Ctrl Pts',(4.30911750776002,1.06847604194596,9.27732764435698));
#56216=CARTESIAN_POINT('Ctrl Pts',(4.3391041711311,1.1851427086139,9.29293405573285));
#56217=CARTESIAN_POINT('Ctrl Pts',(4.36600543843937,1.30000000000336,9.31180152430741));
#56218=CARTESIAN_POINT('Ctrl Pts',(4.26112167304248,-1.30000000000121,9.51306293852468));
#56219=CARTESIAN_POINT('Ctrl Pts',(4.24229982152744,-1.18514270861245,9.47902777087902));
#56220=CARTESIAN_POINT('Ctrl Pts',(4.22094355162894,-1.06847604194523,9.44691397418521));
#56221=CARTESIAN_POINT('Ctrl Pts',(4.16575128238195,-0.794772684000462,
9.37716343074742));
#56222=CARTESIAN_POINT('Ctrl Pts',(4.11527210765485,-0.636309800094887,
9.33705607537697));
#56223=CARTESIAN_POINT('Ctrl Pts',(4.06581685723877,-0.319434907277004,
9.27986478205432));
#56224=CARTESIAN_POINT('Ctrl Pts',(4.04015061657582,-0.158333333333255,
9.2561022147184));
#56225=CARTESIAN_POINT('Ctrl Pts',(4.05282623100244,0.158333333333258,9.23119371657798));
#56226=CARTESIAN_POINT('Ctrl Pts',(4.09123284757633,0.319434907277012,9.22996738025275));
#56227=CARTESIAN_POINT('Ctrl Pts',(4.16637549742435,0.636309800094898,9.23658563659111));
#56228=CARTESIAN_POINT('Ctrl Pts',(4.23061539482181,0.794772684000454,9.24882385034909));
#56229=CARTESIAN_POINT('Ctrl Pts',(4.30729007606217,1.06847604194596,9.27738261100104));
#56230=CARTESIAN_POINT('Ctrl Pts',(4.33746559938657,1.1851427086139,9.29300416345298));
#56231=CARTESIAN_POINT('Ctrl Pts',(4.36462701760318,1.30000000000336,9.31188523907697));
#56232=CARTESIAN_POINT('Ctrl Pts',(4.26035799968545,-1.30000000000121,9.51302203515777));
#56233=CARTESIAN_POINT('Ctrl Pts',(4.24139110836822,-1.18514270861245,9.4789700338413));
#56234=CARTESIAN_POINT('Ctrl Pts',(4.21992935678055,-1.06847604194523,9.44684220684509));
#56235=CARTESIAN_POINT('Ctrl Pts',(4.16458479088466,-0.794772684000462,
9.37706572694382));
#56236=CARTESIAN_POINT('Ctrl Pts',(4.11413635908148,-0.636309800094887,
9.33695116082272));
#56237=CARTESIAN_POINT('Ctrl Pts',(4.064681560807,-0.319434907277004,9.27974460162218));
#56238=CARTESIAN_POINT('Ctrl Pts',(4.0390729692768,-0.158333333333255,9.25595759594241));
#56239=CARTESIAN_POINT('Ctrl Pts',(4.05173850640223,0.158333333333258,9.23107985921052));
#56240=CARTESIAN_POINT('Ctrl Pts',(4.09007277335858,0.319434907277012,9.22992136116913));
#56241=CARTESIAN_POINT('Ctrl Pts',(4.16520386142014,0.636309800094898,9.23659179838107));
#56242=CARTESIAN_POINT('Ctrl Pts',(4.22941469577267,0.794772684000454,9.2488370629054));
#56243=CARTESIAN_POINT('Ctrl Pts',(4.30624506240245,1.06847604194596,9.27741642908466));
#56244=CARTESIAN_POINT('Ctrl Pts',(4.33652905264565,1.1851427086139,9.29304491214065));
#56245=CARTESIAN_POINT('Ctrl Pts',(4.36384001426349,1.30000000000336,9.31193092960344));
#56246=CARTESIAN_POINT('Ctrl Pts',(4.25386871221725,-1.30000000000122,9.5126707048174));
#56247=CARTESIAN_POINT('Ctrl Pts',(4.23366468109142,-1.18514270861246,9.47848859867081));
#56248=CARTESIAN_POINT('Ctrl Pts',(4.21130410672917,-1.06847604194523,9.44624842090527));
#56249=CARTESIAN_POINT('Ctrl Pts',(4.15466466044384,-0.794772684000465,
9.37625340368326));
#56250=CARTESIAN_POINT('Ctrl Pts',(4.10448617408231,-0.636309800094891,
9.33605325953235));
#56251=CARTESIAN_POINT('Ctrl Pts',(4.05503843749056,-0.319434907277006,
9.27870748019983));
#56252=CARTESIAN_POINT('Ctrl Pts',(4.02991987648068,-0.158333333333256,
9.25471095276929));
#56253=CARTESIAN_POINT('Ctrl Pts',(4.0424964711577,0.158333333333258,9.23010493361964));
#56254=CARTESIAN_POINT('Ctrl Pts',(4.08020951067749,0.319434907277014,9.22954365534675));
#56255=CARTESIAN_POINT('Ctrl Pts',(4.15523843700153,0.636309800094901,9.23667053804519));
#56256=CARTESIAN_POINT('Ctrl Pts',(4.21920311517671,0.794772684000459,9.24897446745093));
#56257=CARTESIAN_POINT('Ctrl Pts',(4.29735601881323,1.06847604194597,9.27772965857063));
#56258=CARTESIAN_POINT('Ctrl Pts',(4.32856167605119,1.18514270861391,9.2934164645392));
#56259=CARTESIAN_POINT('Ctrl Pts',(4.35714349439314,1.30000000000336,9.3123430197254));
#56260=CARTESIAN_POINT('Ctrl Pts',(4.24178124330891,-1.3000000000013,9.51117036285141));
#56261=CARTESIAN_POINT('Ctrl Pts',(4.21909655253804,-1.18514270861253,9.47704359218079));
#56262=CARTESIAN_POINT('Ctrl Pts',(4.19496119016866,-1.0684760419453,9.44473352233143));
#56263=CARTESIAN_POINT('Ctrl Pts',(4.13585233323443,-0.794772684000518,
9.37428773969915));
#56264=CARTESIAN_POINT('Ctrl Pts',(4.08651822363923,-0.63630980009493,9.33301961812018));
#56265=CARTESIAN_POINT('Ctrl Pts',(4.03705041811503,-0.319434907277025,
9.27550054041365));
#56266=CARTESIAN_POINT('Ctrl Pts',(4.012560323088,-0.158333333333266,9.25196927902043));
#56267=CARTESIAN_POINT('Ctrl Pts',(4.02483699477286,0.158333333333268,9.2282262725902));
#56268=CARTESIAN_POINT('Ctrl Pts',(4.06145877578896,0.319434907277035,9.22848581931836));
#56269=CARTESIAN_POINT('Ctrl Pts',(4.13622860300854,0.636309800094941,9.23668211508822));
#56270=CARTESIAN_POINT('Ctrl Pts',(4.19949354935448,0.794772684000507,9.24987010723203));
#56271=CARTESIAN_POINT('Ctrl Pts',(4.28028599443832,1.06847604194603,9.27860275469367));
#56272=CARTESIAN_POINT('Ctrl Pts',(4.31337706345077,1.18514270861398,9.29399745869907));
#56273=CARTESIAN_POINT('Ctrl Pts',(4.34458714565379,1.30000000000345,9.31234956827316));
#56274=CARTESIAN_POINT('Ctrl Pts',(4.22320612684256,-1.30000000000134,9.51079938881643));
#56275=CARTESIAN_POINT('Ctrl Pts',(4.19704373245862,-1.18514270861257,9.47626373784351));
#56276=CARTESIAN_POINT('Ctrl Pts',(4.17038815369448,-1.06847604194534,9.44359119137219));
#56277=CARTESIAN_POINT('Ctrl Pts',(4.10766907973974,-0.794772684000543,
9.37241521701459));
#56278=CARTESIAN_POINT('Ctrl Pts',(4.0591594781697,-0.636309800094952,9.33075549355686));
#56279=CARTESIAN_POINT('Ctrl Pts',(4.00971417153467,-0.319434907277036,
9.27284812988568));
#56280=CARTESIAN_POINT('Ctrl Pts',(3.98640076421902,-0.158333333333271,
9.24934159322923));
#56281=CARTESIAN_POINT('Ctrl Pts',(3.99868569747104,0.158333333333273,9.22555001433102));
#56282=CARTESIAN_POINT('Ctrl Pts',(4.03419060433982,0.319434907277044,9.22553226129214));
#56283=CARTESIAN_POINT('Ctrl Pts',(4.1088497531818,0.636309800094962,9.23443344293737));
#56284=CARTESIAN_POINT('Ctrl Pts',(4.1711027666005,0.794772684000536,9.24868382172846));
#56285=CARTESIAN_POINT('Ctrl Pts',(4.25538439556395,1.06847604194607,9.27869255642126));
#56286=CARTESIAN_POINT('Ctrl Pts',(4.29096174293842,1.18514270861402,9.29464472144887));
#56287=CARTESIAN_POINT('Ctrl Pts',(4.32563404345099,1.30000000000348,9.31355938218873));
#56288=CARTESIAN_POINT('Ctrl Pts',(4.2054458088272,-1.30000000000139,9.50826165136687));
#56289=CARTESIAN_POINT('Ctrl Pts',(4.17587338761788,-1.18514270861262,9.47309275299579));
#56290=CARTESIAN_POINT('Ctrl Pts',(4.14671963387226,-1.06847604194538,9.43996758529192));
#56291=CARTESIAN_POINT('Ctrl Pts',(4.08033583612687,-0.794772684000577,
9.36816324791727));
#56292=CARTESIAN_POINT('Ctrl Pts',(4.03239495345726,-0.636309800094979,
9.32680868495316));
#56293=CARTESIAN_POINT('Ctrl Pts',(3.98289150201526,-0.31943490727705,9.26872905500331));
#56294=CARTESIAN_POINT('Ctrl Pts',(3.96095814577377,-0.158333333333278,
9.24469994491065));
#56295=CARTESIAN_POINT('Ctrl Pts',(3.97306681687221,0.15833333333328,9.22138423758945));
#56296=CARTESIAN_POINT('Ctrl Pts',(4.00701746190735,0.319434907277058,9.22231997097444));
#56297=CARTESIAN_POINT('Ctrl Pts',(4.08137154369871,0.63630980009499,9.23245431244624));
#56298=CARTESIAN_POINT('Ctrl Pts',(4.1426660014168,0.794772684000571,9.24761943765885));
#56299=CARTESIAN_POINT('Ctrl Pts',(4.23063602231676,1.06847604194612,9.27826577639269));
#56300=CARTESIAN_POINT('Ctrl Pts',(4.26883860452601,1.18514270861407,9.29433484784612));
#56301=CARTESIAN_POINT('Ctrl Pts',(4.3071648065072,1.30000000000354,9.31320732627382));
#56302=CARTESIAN_POINT('Ctrl Pts',(4.18686936798153,-1.30000000000144,9.50784799049483));
#56303=CARTESIAN_POINT('Ctrl Pts',(4.1537455453232,-1.18514270861266,9.47244915742316));
#56304=CARTESIAN_POINT('Ctrl Pts',(4.12205853653029,-1.06847604194542,9.43898252789801));
#56305=CARTESIAN_POINT('Ctrl Pts',(4.0521745347172,-0.794772684000604,9.36613169544727));
#56306=CARTESIAN_POINT('Ctrl Pts',(4.00540931861376,-0.636309800095,9.32344327305321));
#56307=CARTESIAN_POINT('Ctrl Pts',(3.95609732960451,-0.319434907277061,
9.26452386114696));
#56308=CARTESIAN_POINT('Ctrl Pts',(3.9353800935742,-0.158333333333284,9.24041782432346));
#56309=CARTESIAN_POINT('Ctrl Pts',(3.94730070634834,0.158333333333286,9.21760153467538));
#56310=CARTESIAN_POINT('Ctrl Pts',(3.97972332532001,0.319434907277068,9.21939301129695));
#56311=CARTESIAN_POINT('Ctrl Pts',(4.05375515190992,0.63630980009501,9.23081529726131));
#56312=CARTESIAN_POINT('Ctrl Pts',(4.11404925717502,0.794772684000596,9.24703854429435));
#56313=CARTESIAN_POINT('Ctrl Pts',(4.2056799580573,1.06847604194615,9.27843300161521));
#56314=CARTESIAN_POINT('Ctrl Pts',(4.24649949110921,1.18514270861411,9.29465790225651));
#56315=CARTESIAN_POINT('Ctrl Pts',(4.28847502205294,1.30000000000358,9.31351820624413));
#56316=CARTESIAN_POINT('Ctrl Pts',(4.16917315736043,-1.30000000000149,9.5051037777749));
#56317=CARTESIAN_POINT('Ctrl Pts',(4.13281824485764,-1.1851427086127,9.46859744828135));
#56318=CARTESIAN_POINT('Ctrl Pts',(4.09875074033596,-1.06847604194545,9.43436481465258));
#56319=CARTESIAN_POINT('Ctrl Pts',(4.02533235974092,-0.794772684000632,
9.36053327505436));
#56320=CARTESIAN_POINT('Ctrl Pts',(3.97904689603395,-0.636309800095023,
9.31837014559696));
#56321=CARTESIAN_POINT('Ctrl Pts',(3.92952225134954,-0.319434907277072,
9.25968834249974));
#56322=CARTESIAN_POINT('Ctrl Pts',(3.90987087920662,-0.158333333333289,
9.23593319703193));
#56323=CARTESIAN_POINT('Ctrl Pts',(3.92167555233481,0.158333333333291,9.21338919330623));
#56324=CARTESIAN_POINT('Ctrl Pts',(3.95296650613317,0.319434907277081,9.21493431476278));
#56325=CARTESIAN_POINT('Ctrl Pts',(4.02687269945799,0.636309800095034,9.22701531286196));
#56326=CARTESIAN_POINT('Ctrl Pts',(4.0862629071067,0.794772684000624,9.24384636807182));
#56327=CARTESIAN_POINT('Ctrl Pts',(4.18128339050235,1.06847604194619,9.2767867802146));
#56328=CARTESIAN_POINT('Ctrl Pts',(4.22450478135387,1.18514270861415,9.29383823078633));
#56329=CARTESIAN_POINT('Ctrl Pts',(4.26981671665059,1.30000000000363,9.31368244807567));
#56330=CARTESIAN_POINT('Ctrl Pts',(4.15072826470058,-1.30000000000153,9.50428049865681));
#56331=CARTESIAN_POINT('Ctrl Pts',(4.11092006387152,-1.18514270861274,9.4672585114039));
#56332=CARTESIAN_POINT('Ctrl Pts',(4.07439573712881,-1.06847604194549,9.43247028158174));
#56333=CARTESIAN_POINT('Ctrl Pts',(3.99760364176302,-0.794772684000661,
9.35726293785791));
#56334=CARTESIAN_POINT('Ctrl Pts',(3.95249877951535,-0.636309800095045,
9.31381998566838));
#56335=CARTESIAN_POINT('Ctrl Pts',(3.90321841546551,-0.319434907277083,
9.25418271625328));
#56336=CARTESIAN_POINT('Ctrl Pts',(3.88484358864865,-0.158333333333294,
9.23019185009763));
#56337=CARTESIAN_POINT('Ctrl Pts',(3.89640048618951,0.158333333333296,9.20826547681166));
#56338=CARTESIAN_POINT('Ctrl Pts',(3.92606467876695,0.31943490727709,9.21084090843296));
#56339=CARTESIAN_POINT('Ctrl Pts',(3.99943055395677,0.636309800095054,9.22477498876752));
#56340=CARTESIAN_POINT('Ctrl Pts',(4.05750970766444,0.794772684000651,9.24358249041576));
#56341=CARTESIAN_POINT('Ctrl Pts',(4.15618511747296,1.06847604194623,9.2772753226398));
#56342=CARTESIAN_POINT('Ctrl Pts',(4.2021015888093,1.1851427086142,9.29425122806245));
#56343=CARTESIAN_POINT('Ctrl Pts',(4.2512216028599,1.30000000000368,9.31361866028035));
#56344=CARTESIAN_POINT('Ctrl Pts',(4.13311774283548,-1.30000000000156,9.50129808886456));
#56345=CARTESIAN_POINT('Ctrl Pts',(4.09001770799959,-1.18514270861277,9.463322669032));
#56346=CARTESIAN_POINT('Ctrl Pts',(4.05109040073584,-1.06847604194552,9.4278236837884));
#56347=CARTESIAN_POINT('Ctrl Pts',(3.97080036901856,-0.794772684000679,
9.35153498563776));
#56348=CARTESIAN_POINT('Ctrl Pts',(3.92636363324339,-0.636309800095061,
9.3081280151374));
#56349=CARTESIAN_POINT('Ctrl Pts',(3.87696881815577,-0.319434907277091,
9.24846564558703));
#56350=CARTESIAN_POINT('Ctrl Pts',(3.859680635308,-0.158333333333299,9.22476527997279));
#56351=CARTESIAN_POINT('Ctrl Pts',(3.87107002642811,0.158333333333301,9.20323489741686));
#56352=CARTESIAN_POINT('Ctrl Pts',(3.89943998848835,0.319434907277099,9.20600033683233));
#56353=CARTESIAN_POINT('Ctrl Pts',(3.97266075653131,0.63630980009507,9.22059396562998));
#56354=CARTESIAN_POINT('Ctrl Pts',(4.02997743362364,0.79477268400067,9.23954790476794));
#56355=CARTESIAN_POINT('Ctrl Pts',(4.13207914134066,1.06847604194625,9.27465870538211));
#56356=CARTESIAN_POINT('Ctrl Pts',(4.18039578318188,1.18514270861422,9.29246707686264));
#56357=CARTESIAN_POINT('Ctrl Pts',(4.23283302083448,1.30000000000371,9.31288565522111));
#56358=CARTESIAN_POINT('Ctrl Pts',(4.10903671786866,-1.30000000000159,9.49882516426784));
#56359=CARTESIAN_POINT('Ctrl Pts',(4.061351450167,-1.1851427086128,9.46007569419142));
#56360=CARTESIAN_POINT('Ctrl Pts',(4.01917031236304,-1.06847604194555,9.42376332368494));
#56361=CARTESIAN_POINT('Ctrl Pts',(3.93443908688951,-0.794772684000702,
9.34550467109699));
#56362=CARTESIAN_POINT('Ctrl Pts',(3.89161685908087,-0.636309800095078,
9.30038240926461));
#56363=CARTESIAN_POINT('Ctrl Pts',(3.84262378705535,-0.319434907277099,
9.23930224859468));
#56364=CARTESIAN_POINT('Ctrl Pts',(3.82713019619362,-0.158333333333302,
9.2150928225414));
#56365=CARTESIAN_POINT('Ctrl Pts',(3.83816214263699,0.158333333333304,9.19438010112749));
#56366=CARTESIAN_POINT('Ctrl Pts',(3.86415948701236,0.319434907277105,9.19892024455919));
#56367=CARTESIAN_POINT('Ctrl Pts',(3.93669973058322,0.636309800095086,9.21568467338448));
#56368=CARTESIAN_POINT('Ctrl Pts',(3.99271182765839,0.794772684000693,9.23585465060728));
#56369=CARTESIAN_POINT('Ctrl Pts',(4.09946236095896,1.06847604194628,9.27261956501576));
#56370=CARTESIAN_POINT('Ctrl Pts',(4.15113581682079,1.18514270861425,9.29105755113202));
#56371=CARTESIAN_POINT('Ctrl Pts',(4.20827437817544,1.30000000000374,9.31201935419136));
#56372=CARTESIAN_POINT('Ctrl Pts',(4.08562660246539,-1.3000000000017,9.49464937055466));
#56373=CARTESIAN_POINT('Ctrl Pts',(4.03371314955642,-1.1851427086129,9.4542482621586));
#56374=CARTESIAN_POINT('Ctrl Pts',(3.98845561452364,-1.06847604194563,9.41668722866343));
#56375=CARTESIAN_POINT('Ctrl Pts',(3.89927815666511,-0.794772684000763,
9.33647486840692));
#56376=CARTESIAN_POINT('Ctrl Pts',(3.8573058510564,-0.636309800095127,9.29149740985962));
#56377=CARTESIAN_POINT('Ctrl Pts',(3.80838819730487,-0.319434907277124,
9.22985627576571));
#56378=CARTESIAN_POINT('Ctrl Pts',(3.79467846287215,-0.158333333333315,
9.20528955941735));
#56379=CARTESIAN_POINT('Ctrl Pts',(3.80554313196228,0.158333333333317,9.18491910142369));
#56380=CARTESIAN_POINT('Ctrl Pts',(3.82971530510416,0.319434907277131,9.18977189492765));
#56381=CARTESIAN_POINT('Ctrl Pts',(3.90158282183463,0.636309800095136,9.20858255798319));
#56382=CARTESIAN_POINT('Ctrl Pts',(3.95581854544446,0.794772684000755,9.23100648829692));
#56383=CARTESIAN_POINT('Ctrl Pts',(4.06686014882141,1.06847604194636,9.27036243486625));
#56384=CARTESIAN_POINT('Ctrl Pts',(4.1217476047809,1.18514270861435,9.28985272324412));
#56385=CARTESIAN_POINT('Ctrl Pts',(4.18345672109462,1.30000000000384,9.31179756901142));
#56386=CARTESIAN_POINT('Ctrl Pts',(4.06476527097544,-1.30000000000171,9.49189931303782));
#56387=CARTESIAN_POINT('Ctrl Pts',(4.00893066569573,-1.18514270861291,9.45058725719531));
#56388=CARTESIAN_POINT('Ctrl Pts',(3.96094698949746,-1.06847604194565,9.41203188116684));
#56389=CARTESIAN_POINT('Ctrl Pts',(3.86823231512926,-0.794772684000776,
9.32932973140712));
#56390=CARTESIAN_POINT('Ctrl Pts',(3.82824956240086,-0.636309800095136,
9.28164581924606));
#56391=CARTESIAN_POINT('Ctrl Pts',(3.77963133894567,-0.319434907277128,
9.21892992138924));
#56392=CARTESIAN_POINT('Ctrl Pts',(3.76674394264146,-0.158333333333317,
9.19563699343125));
#56393=CARTESIAN_POINT('Ctrl Pts',(3.77714975638311,0.158333333333319,9.17623377571701));
#56394=CARTESIAN_POINT('Ctrl Pts',(3.79968841658033,0.319434907277137,9.18150531272934));
#56395=CARTESIAN_POINT('Ctrl Pts',(3.87103949709614,0.636309800095146,9.20188357154754));
#56396=CARTESIAN_POINT('Ctrl Pts',(3.92397236152757,0.794772684000764,9.22562109864878));
#56397=CARTESIAN_POINT('Ctrl Pts',(4.03895466182375,1.06847604194638,9.26668233308603));
#56398=CARTESIAN_POINT('Ctrl Pts',(4.09671988751846,1.18514270861436,9.28687634149948));
#56399=CARTESIAN_POINT('Ctrl Pts',(4.16247876162346,1.30000000000386,9.30949047140706));
#56400=CARTESIAN_POINT('Ctrl Pts',(4.05300830437315,-1.30000000000172,9.48988652188689));
#56401=CARTESIAN_POINT('Ctrl Pts',(3.9951467741753,-1.18514270861292,9.44748701561431));
#56402=CARTESIAN_POINT('Ctrl Pts',(3.94568816028232,-1.06847604194565,9.40811724880978));
#56403=CARTESIAN_POINT('Ctrl Pts',(3.85084128568987,-0.794772684000781,
9.32416451586521));
#56404=CARTESIAN_POINT('Ctrl Pts',(3.81121873941074,-0.63630980009514,9.27670424684079));
#56405=CARTESIAN_POINT('Ctrl Pts',(3.76272615397381,-0.31943490727713,9.21352490123455));
#56406=CARTESIAN_POINT('Ctrl Pts',(3.75088814885211,-0.158333333333318,
9.18976750887703));
#56407=CARTESIAN_POINT('Ctrl Pts',(3.76125912769879,0.15833333333332,9.17040872169655));
#56408=CARTESIAN_POINT('Ctrl Pts',(3.78279108341697,0.319434907277138,9.17598169012332));
#56409=CARTESIAN_POINT('Ctrl Pts',(3.85378766382737,0.636309800095149,9.19733648673911));
#56410=CARTESIAN_POINT('Ctrl Pts',(3.9059106641595,0.794772684000769,9.22188953620525));
#56411=CARTESIAN_POINT('Ctrl Pts',(4.02296625161793,1.06847604194638,9.26447013023481));
#56412=CARTESIAN_POINT('Ctrl Pts',(4.08227787528785,1.18514270861437,9.28540156791325));
#56413=CARTESIAN_POINT('Ctrl Pts',(4.15023209615361,1.30000000000387,9.30883288188111));
#56414=CARTESIAN_POINT('Ctrl Pts',(4.04144316270885,-1.30000000000174,9.48751020962183));
#56415=CARTESIAN_POINT('Ctrl Pts',(3.98134733969823,-1.18514270861294,9.44466768895473));
#56416=CARTESIAN_POINT('Ctrl Pts',(3.93034658136215,-1.06847604194567,9.40477431602907));
#56417=CARTESIAN_POINT('Ctrl Pts',(3.83353604579894,-0.794772684000792,
9.31942576518684));
#56418=CARTESIAN_POINT('Ctrl Pts',(3.79515903035351,-0.636309800095149,
9.27027912947151));
#56419=CARTESIAN_POINT('Ctrl Pts',(3.74684641269738,-0.319434907277135,
9.20648707084666));
#56420=CARTESIAN_POINT('Ctrl Pts',(3.7353888107615,-0.15833333333332,9.18354148532602));
#56421=CARTESIAN_POINT('Ctrl Pts',(3.74544793581991,0.158333333333322,9.16480478031421));
#56422=CARTESIAN_POINT('Ctrl Pts',(3.76610354892916,0.319434907277142,9.17051118864721));
#56423=CARTESIAN_POINT('Ctrl Pts',(3.8366599070298,0.636309800095158,9.19308757189826));
#56424=CARTESIAN_POINT('Ctrl Pts',(3.88783887820413,0.794772684000781,9.21885807701802));
#56425=CARTESIAN_POINT('Ctrl Pts',(4.00690630380797,1.0684760419464,9.26291631106989));
#56426=CARTESIAN_POINT('Ctrl Pts',(4.06775871787748,1.18514270861439,9.28445566000726));
#56427=CARTESIAN_POINT('Ctrl Pts',(4.13792366935522,1.30000000000389,9.30846318087929));
#56428=CARTESIAN_POINT('Ctrl Pts',(4.02679641465004,-1.30000000000176,9.48473812544725));
#56429=CARTESIAN_POINT('Ctrl Pts',(3.96397800532106,-1.18514270861296,9.44073038492449));
#56430=CARTESIAN_POINT('Ctrl Pts',(3.91106087662922,-1.06847604194569,9.39981049157656));
#56431=CARTESIAN_POINT('Ctrl Pts',(3.81168566233224,-0.794772684000809,
9.31241089664204));
#56432=CARTESIAN_POINT('Ctrl Pts',(3.77465916953601,-0.636309800095161,
9.26155524778288));
#56433=CARTESIAN_POINT('Ctrl Pts',(3.72613506221229,-0.31943490727714,9.19795344267425));
#56434=CARTESIAN_POINT('Ctrl Pts',(3.71453984184334,-0.158333333333323,
9.1776908962965));
#56435=CARTESIAN_POINT('Ctrl Pts',(3.72425182411421,0.158333333333325,9.15966462875999));
#56436=CARTESIAN_POINT('Ctrl Pts',(3.74449936440215,0.319434907277149,9.1637828297215));
#56437=CARTESIAN_POINT('Ctrl Pts',(3.8149645362383,0.63630980009517,9.1868330859365));
#56438=CARTESIAN_POINT('Ctrl Pts',(3.86499909873929,0.794772684000796,9.21395294551675));
#56439=CARTESIAN_POINT('Ctrl Pts',(3.98685367567479,1.06847604194642,9.2597023465543));
#56440=CARTESIAN_POINT('Ctrl Pts',(4.0497576568466,1.18514270861441,9.28203736398851));
#56441=CARTESIAN_POINT('Ctrl Pts',(4.12281928799156,1.30000000000391,9.30690417833001));
#56442=CARTESIAN_POINT('Ctrl Pts',(4.01233725084441,-1.30000000000178,9.48188657085733));
#56443=CARTESIAN_POINT('Ctrl Pts',(3.9472834804975,-1.18514270861298,9.43630715904329));
#56444=CARTESIAN_POINT('Ctrl Pts',(3.89267239169235,-1.0684760419457,9.39438957704579));
#56445=CARTESIAN_POINT('Ctrl Pts',(3.79063453505462,-0.794772684000821,
9.306011136471));
#56446=CARTESIAN_POINT('Ctrl Pts',(3.75355465833583,-0.636309800095172,
9.25664233164415));
#56447=CARTESIAN_POINT('Ctrl Pts',(3.70467963936613,-0.319434907277146,
9.1937453763877));
#56448=CARTESIAN_POINT('Ctrl Pts',(3.69376706484766,-0.158333333333326,
9.17421339617309));
#56449=CARTESIAN_POINT('Ctrl Pts',(3.70366827837763,0.158333333333328,9.15571193937935));
#56450=CARTESIAN_POINT('Ctrl Pts',(3.72374766534792,0.319434907277155,9.15786439977874));
#56451=CARTESIAN_POINT('Ctrl Pts',(3.79428666548469,0.636309800095182,9.18078991485239));
#56452=CARTESIAN_POINT('Ctrl Pts',(3.84313183150337,0.79477268400081,9.20920658112124));
#56453=CARTESIAN_POINT('Ctrl Pts',(3.96749298935426,1.06847604194644,9.25639049870806));
#56454=CARTESIAN_POINT('Ctrl Pts',(4.03225771668887,1.18514270861443,9.27942293886111));
#56455=CARTESIAN_POINT('Ctrl Pts',(4.10795583415916,1.30000000000393,9.3050636495802));
#56456=CARTESIAN_POINT('Ctrl Pts',(3.99511068658432,-1.3000000000018,9.47779791444803));
#56457=CARTESIAN_POINT('Ctrl Pts',(3.9270731722259,-1.18514270861299,9.42999191937879));
#56458=CARTESIAN_POINT('Ctrl Pts',(3.87009092852604,-1.06847604194572,9.38682542708467));
#56459=CARTESIAN_POINT('Ctrl Pts',(3.7639904331415,-0.794772684000831,9.29782037399825));
#56460=CARTESIAN_POINT('Ctrl Pts',(3.72599406279882,-0.63630980009518,9.25179941472985));
#56461=CARTESIAN_POINT('Ctrl Pts',(3.67606437133554,-0.31943490727715,9.19082028115558));
#56462=CARTESIAN_POINT('Ctrl Pts',(3.66613937014711,-0.158333333333328,
9.17217087182118));
#56463=CARTESIAN_POINT('Ctrl Pts',(3.67598751442257,0.15833333333333,9.15373611402291));
#56464=CARTESIAN_POINT('Ctrl Pts',(3.69515312446211,0.319434907277158,9.15474944508824));
#56465=CARTESIAN_POINT('Ctrl Pts',(3.76638028263996,0.636309800095189,9.17655145167988));
#56466=CARTESIAN_POINT('Ctrl Pts',(3.81537314735066,0.794772684000819,9.20336749787024));
#56467=CARTESIAN_POINT('Ctrl Pts',(3.94377298237415,1.06847604194645,9.25136176898206));
#56468=CARTESIAN_POINT('Ctrl Pts',(4.01107872912038,1.18514270861444,9.27534533028923));
#56469=CARTESIAN_POINT('Ctrl Pts',(4.09011069171359,1.30000000000395,9.30253751130213));
#56470=CARTESIAN_POINT('Ctrl Pts',(3.9833527785113,-1.30000000000184,9.47508570286668));
#56471=CARTESIAN_POINT('Ctrl Pts',(3.9138153768009,-1.18514270861303,9.42456161217328));
#56472=CARTESIAN_POINT('Ctrl Pts',(3.85550223129827,-1.06847604194575,9.38013053843038));
#56473=CARTESIAN_POINT('Ctrl Pts',(3.74671747692744,-0.794772684000851,
9.29156195773824));
#56474=CARTESIAN_POINT('Ctrl Pts',(3.70705838932682,-0.636309800095197,
9.25183149394815));
#56475=CARTESIAN_POINT('Ctrl Pts',(3.65612349313465,-0.319434907277159,
9.19417216781756));
#56476=CARTESIAN_POINT('Ctrl Pts',(3.64724201481595,-0.158333333333332,
9.17575399890262));
#56477=CARTESIAN_POINT('Ctrl Pts',(3.65704996975842,0.158333333333334,9.15750177715454));
#56478=CARTESIAN_POINT('Ctrl Pts',(3.67523755008904,0.319434907277167,9.15838530604779));
#56479=CARTESIAN_POINT('Ctrl Pts',(3.74717278258775,0.636309800095206,9.17740450837209));
#56480=CARTESIAN_POINT('Ctrl Pts',(3.79716553103066,0.79477268400084,9.19876566584626));
#56481=CARTESIAN_POINT('Ctrl Pts',(3.92828386839332,1.06847604194648,9.24627537344296));
#56482=CARTESIAN_POINT('Ctrl Pts',(3.99710096186775,1.18514270861448,9.27127676663499));
#56483=CARTESIAN_POINT('Ctrl Pts',(4.07797887898519,1.30000000000399,9.30071436100847));
#56484=CARTESIAN_POINT('Ctrl Pts',(3.97477914228584,-1.30000000000184,9.47578453352629));
#56485=CARTESIAN_POINT('Ctrl Pts',(3.90549290340901,-1.18514270861303,9.42526901565753));
#56486=CARTESIAN_POINT('Ctrl Pts',(3.84729017393194,-1.06847604194575,9.38116464394731));
#56487=CARTESIAN_POINT('Ctrl Pts',(3.73843534938598,-0.794772684000851,
9.29408575241927));
#56488=CARTESIAN_POINT('Ctrl Pts',(3.69814954202848,-0.636309800095197,
9.25684331707449));
#56489=CARTESIAN_POINT('Ctrl Pts',(3.64686579593571,-0.319434907277159,
9.20083410021132));
#56490=CARTESIAN_POINT('Ctrl Pts',(3.6379450782909,-0.158333333333332,9.18238128424967));
#56491=CARTESIAN_POINT('Ctrl Pts',(3.64772547716597,0.158333333333334,9.16436428106718));
#56492=CARTESIAN_POINT('Ctrl Pts',(3.66586376136843,0.319434907277167,9.16579102070237));
#56493=CARTESIAN_POINT('Ctrl Pts',(3.73821592466294,0.636309800095206,9.18308245269344));
#56494=CARTESIAN_POINT('Ctrl Pts',(3.78913144751243,0.79477268400084,9.20091302212069));
#56495=CARTESIAN_POINT('Ctrl Pts',(3.9202668858623,1.06847604194648,9.24707722512988));
#56496=CARTESIAN_POINT('Ctrl Pts',(3.98887475074185,1.18514270861448,9.27205620607566));
#56497=CARTESIAN_POINT('Ctrl Pts',(4.06932680828582,1.30000000000399,9.30203139503673));
#56498=CARTESIAN_POINT('Ctrl Pts',(3.97477914228473,-1.3,9.47578453352548));
#56499=CARTESIAN_POINT('Ctrl Pts',(3.90549290340839,-1.18514270861178,9.42526901565706));
#56500=CARTESIAN_POINT('Ctrl Pts',(3.84729017393168,-1.06847604194512,9.38116464394711));
#56501=CARTESIAN_POINT('Ctrl Pts',(3.73843534938597,-0.794772684000851,
9.29408575241928));
#56502=CARTESIAN_POINT('Ctrl Pts',(3.69814954202848,-0.636309800095197,
9.25684331707449));
#56503=CARTESIAN_POINT('Ctrl Pts',(3.64686579593571,-0.319434907277159,
9.20083410021132));
#56504=CARTESIAN_POINT('Ctrl Pts',(3.6379450782909,-0.158333333333332,9.18238128424967));
#56505=CARTESIAN_POINT('Ctrl Pts',(3.64772547716596,0.158333333333334,9.16436428106718));
#56506=CARTESIAN_POINT('Ctrl Pts',(3.66586376136843,0.319434907277167,9.16579102070237));
#56507=CARTESIAN_POINT('Ctrl Pts',(3.73821592466293,0.636309800095206,9.18308245269344));
#56508=CARTESIAN_POINT('Ctrl Pts',(3.78913144751243,0.79477268400084,9.20091302212069));
#56509=CARTESIAN_POINT('Ctrl Pts',(3.92026688586164,1.06847604194511,9.24707722512964));
#56510=CARTESIAN_POINT('Ctrl Pts',(3.98887475074027,1.18514270861178,9.27205620607508));
#56511=CARTESIAN_POINT('Ctrl Pts',(4.06932680828303,1.3,9.30203139503569));
#56512=CARTESIAN_POINT('',(4.38969958549801,-1.2,9.48758334254264));
#56513=CARTESIAN_POINT('Ctrl Pts',(4.38969958549801,-1.2,9.48758334254265));
#56514=CARTESIAN_POINT('Ctrl Pts',(4.37179496097857,-1.21424592766347,9.49111483394103));
#56515=CARTESIAN_POINT('Ctrl Pts',(4.37023623801035,-1.2152654494871,9.49188100659603));
#56516=CARTESIAN_POINT('Ctrl Pts',(4.34578951938456,-1.23433940646938,9.49736529100142));
#56517=CARTESIAN_POINT('Ctrl Pts',(4.34413559802252,-1.23568262283785,9.4976366021116));
#56518=CARTESIAN_POINT('Ctrl Pts',(4.30607628505062,-1.26582530512805,9.50500210141761));
#56519=CARTESIAN_POINT('Ctrl Pts',(4.28598494523318,-1.28169477849993,9.50887284971023));
#56520=CARTESIAN_POINT('Ctrl Pts',(4.26568396548156,-1.29775190384789,9.51262878777734));
#56521=CARTESIAN_POINT('Ctrl Pts',(4.26402397189108,-1.29906490328061,9.51293567589886));
#56522=CARTESIAN_POINT('Ctrl Pts',(4.26284481534483,-1.30000000000121,9.51314808870421));
#56523=CARTESIAN_POINT('',(4.45989077443978,-0.653834841416792,9.34752748057694));
#56524=CARTESIAN_POINT('Ctrl Pts',(4.45989077444373,-0.653834841406665,
9.34752748062317));
#56525=CARTESIAN_POINT('Ctrl Pts',(4.45335390424296,-0.71324393711409,9.36110296562405));
#56526=CARTESIAN_POINT('Ctrl Pts',(4.44674825867249,-0.767188910741388,
9.37466736400092));
#56527=CARTESIAN_POINT('Ctrl Pts',(4.42424889216865,-0.949633080775671,
9.42030531501031));
#56528=CARTESIAN_POINT('Ctrl Pts',(4.40765622707638,-1.07514642494888,9.4531259041501));
#56529=CARTESIAN_POINT('Ctrl Pts',(4.38969958549801,-1.2,9.48758334254265));
#56530=CARTESIAN_POINT('',(4.51863764645953,0.653834841531101,9.22099327559463));
#56531=CARTESIAN_POINT('Ctrl Pts',(4.51863764645953,0.653834841531103,9.22099327559463));
#56532=CARTESIAN_POINT('Ctrl Pts',(4.47693045016882,0.575722054508995,9.22158335555513));
#56533=CARTESIAN_POINT('Ctrl Pts',(4.44183847005026,0.493687365915951,9.22304499129017));
#56534=CARTESIAN_POINT('Ctrl Pts',(4.39135806826372,0.338003356428067,9.22732111455017));
#56535=CARTESIAN_POINT('Ctrl Pts',(4.37365341868297,0.265535567213328,9.23010606782248));
#56536=CARTESIAN_POINT('Ctrl Pts',(4.35059352006431,0.12961539563281,9.23802064758203));
#56537=CARTESIAN_POINT('Ctrl Pts',(4.34382820017673,0.0665936360836524,
9.24270343198728));
#56538=CARTESIAN_POINT('Ctrl Pts',(4.33790267606707,-0.059460756060269,
9.25457757758834));
#56539=CARTESIAN_POINT('Ctrl Pts',(4.3386898198503,-0.122628115771336,9.26183704158793));
#56540=CARTESIAN_POINT('Ctrl Pts',(4.34915453823114,-0.259985608121654,
9.27964603169459));
#56541=CARTESIAN_POINT('Ctrl Pts',(4.36043113662999,-0.33385866782113,9.29057829402112));
#56542=CARTESIAN_POINT('Ctrl Pts',(4.39738321548536,-0.491574905831985,
9.31616686070628));
#56543=CARTESIAN_POINT('Ctrl Pts',(4.42520378272057,-0.575006518919015,
9.33156382633747));
#56544=CARTESIAN_POINT('Ctrl Pts',(4.45989077438544,-0.653834841429743,
9.34752748063108));
#56545=CARTESIAN_POINT('',(4.48864234752075,1.2,9.28676540992117));
#56546=CARTESIAN_POINT('Ctrl Pts',(4.48864234752074,1.2,9.28676540992118));
#56547=CARTESIAN_POINT('Ctrl Pts',(4.49218132781357,1.15574893393819,9.27915304643561));
#56548=CARTESIAN_POINT('Ctrl Pts',(4.49913702961667,1.06765896451643,9.26416425729077));
#56549=CARTESIAN_POINT('Ctrl Pts',(4.51513968970315,0.771844892429185,9.22886092983354));
#56550=CARTESIAN_POINT('Ctrl Pts',(4.51659259837948,0.720814231765372,9.22556569617361));
#56551=CARTESIAN_POINT('Ctrl Pts',(4.51863764645953,0.6538348415311,9.22099327559463));
#56552=CARTESIAN_POINT('Ctrl Pts',(4.36609756959132,1.2999999999998,9.31179828885494));
#56553=CARTESIAN_POINT('Ctrl Pts',(4.37593955631733,1.29200222100087,9.30981805892408));
#56554=CARTESIAN_POINT('Ctrl Pts',(4.38571147514364,1.28374785188112,9.30854997600552));
#56555=CARTESIAN_POINT('Ctrl Pts',(4.41170127702802,1.26274495050229,9.302916177652));
#56556=CARTESIAN_POINT('Ctrl Pts',(4.41770216098965,1.25781029718418,9.30177599792278));
#56557=CARTESIAN_POINT('Ctrl Pts',(4.44118715552041,1.23854687998326,9.29721179869033));
#56558=CARTESIAN_POINT('Ctrl Pts',(4.46588814099277,1.21819525011631,9.29254900537115));
#56559=CARTESIAN_POINT('Ctrl Pts',(4.48864234752075,1.2,9.28676540992118));
#56560=CARTESIAN_POINT('Ctrl Pts',(3.97477914228473,-1.3,9.47578453352548));
#56561=CARTESIAN_POINT('Ctrl Pts',(3.90549290340839,-1.18514270861178,9.42526901565706));
#56562=CARTESIAN_POINT('Ctrl Pts',(3.84729017393169,-1.06847604194512,9.38116464394711));
#56563=CARTESIAN_POINT('Ctrl Pts',(3.73843534938598,-0.794772684000851,
9.29408575241928));
#56564=CARTESIAN_POINT('Ctrl Pts',(3.69814954202848,-0.636309800095196,
9.2568433170745));
#56565=CARTESIAN_POINT('Ctrl Pts',(3.64686579593571,-0.319434907277159,
9.20083410021132));
#56566=CARTESIAN_POINT('Ctrl Pts',(3.6379450782909,-0.158333333333332,9.18238128424968));
#56567=CARTESIAN_POINT('Ctrl Pts',(3.64772547716597,0.158333333333334,9.16436428106718));
#56568=CARTESIAN_POINT('Ctrl Pts',(3.66586376136843,0.319434907277167,9.16579102070238));
#56569=CARTESIAN_POINT('Ctrl Pts',(3.73821592466294,0.636309800095206,9.18308245269344));
#56570=CARTESIAN_POINT('Ctrl Pts',(3.78913144751243,0.79477268400084,9.20091302212069));
#56571=CARTESIAN_POINT('Ctrl Pts',(3.92026688586164,1.06847604194511,9.24707722512965));
#56572=CARTESIAN_POINT('Ctrl Pts',(3.98887475074027,1.18514270861178,9.27205620607508));
#56573=CARTESIAN_POINT('Ctrl Pts',(4.06932680828303,1.3,9.30203139503569));
#56574=CARTESIAN_POINT('Ctrl Pts',(3.93487809212144,-1.3,9.54156458726909));
#56575=CARTESIAN_POINT('Ctrl Pts',(3.86662549823905,-1.18514270861178,9.48965893164399));
#56576=CARTESIAN_POINT('Ctrl Pts',(3.80917822375501,-1.06847604194512,9.4446137960335));
#56577=CARTESIAN_POINT('Ctrl Pts',(3.70142597681593,-0.794772684000851,
9.35639969520083));
#56578=CARTESIAN_POINT('Ctrl Pts',(3.6609356094067,-0.636309800095196,9.31984512113064));
#56579=CARTESIAN_POINT('Ctrl Pts',(3.60969614500507,-0.319434907277159,
9.26450127807643));
#56580=CARTESIAN_POINT('Ctrl Pts',(3.60031408828524,-0.158333333333332,
9.2472011190744));
#56581=CARTESIAN_POINT('Ctrl Pts',(3.61040534854147,0.158333333333334,9.22936359179401));
#56582=CARTESIAN_POINT('Ctrl Pts',(3.6293111934153,0.319434907277167,9.22981447159066));
#56583=CARTESIAN_POINT('Ctrl Pts',(3.70226172817696,0.636309800095206,9.2468115657467));
#56584=CARTESIAN_POINT('Ctrl Pts',(3.75367067633866,0.79477268400084,9.26412105033525));
#56585=CARTESIAN_POINT('Ctrl Pts',(3.88437428339459,1.06847604194511,9.31180771821361));
#56586=CARTESIAN_POINT('Ctrl Pts',(3.95254515033271,1.18514270861178,9.33791132432438));
#56587=CARTESIAN_POINT('Ctrl Pts',(4.0323101357604,1.3,9.36947674498659));
#56588=CARTESIAN_POINT('Ctrl Pts',(3.89497704195815,-1.3,9.60734464101269));
#56589=CARTESIAN_POINT('Ctrl Pts',(3.8277580930697,-1.18514270861178,9.55404884763092));
#56590=CARTESIAN_POINT('Ctrl Pts',(3.77106627357833,-1.06847604194512,9.50806294811988));
#56591=CARTESIAN_POINT('Ctrl Pts',(3.66441660424588,-0.794772684000851,
9.41871363798238));
#56592=CARTESIAN_POINT('Ctrl Pts',(3.62372167678492,-0.636309800095196,
9.38284692518678));
#56593=CARTESIAN_POINT('Ctrl Pts',(3.57252649407444,-0.319434907277159,
9.32816845594153));
#56594=CARTESIAN_POINT('Ctrl Pts',(3.56268309827958,-0.158333333333332,
9.31202095389912));
#56595=CARTESIAN_POINT('Ctrl Pts',(3.57308521991698,0.158333333333334,9.29436290252083));
#56596=CARTESIAN_POINT('Ctrl Pts',(3.59275862546217,0.319434907277167,9.29383792247894));
#56597=CARTESIAN_POINT('Ctrl Pts',(3.66630753169098,0.636309800095206,9.31054067879995));
#56598=CARTESIAN_POINT('Ctrl Pts',(3.71820990516489,0.79477268400084,9.32732907854981));
#56599=CARTESIAN_POINT('Ctrl Pts',(3.84848168092753,1.06847604194511,9.37653821129757));
#56600=CARTESIAN_POINT('Ctrl Pts',(3.91621554992515,1.18514270861178,9.40376644257368));
#56601=CARTESIAN_POINT('Ctrl Pts',(3.99529346323778,1.3,9.43692209493747));
#56602=CARTESIAN_POINT('Ctrl Pts',(3.85507599179486,-1.3,9.6731246947563));
#56603=CARTESIAN_POINT('Ctrl Pts',(3.78889068790036,-1.18514270861178,9.61843876361785));
#56604=CARTESIAN_POINT('Ctrl Pts',(3.73295432340165,-1.06847604194512,9.57151210020627));
#56605=CARTESIAN_POINT('Ctrl Pts',(3.62740723167584,-0.794772684000851,
9.48102758076393));
#56606=CARTESIAN_POINT('Ctrl Pts',(3.58650774416314,-0.636309800095196,
9.44584872924292));
#56607=CARTESIAN_POINT('Ctrl Pts',(3.5353568431438,-0.319434907277159,9.39183563380664));
#56608=CARTESIAN_POINT('Ctrl Pts',(3.52505210827392,-0.158333333333332,
9.37684078872385));
#56609=CARTESIAN_POINT('Ctrl Pts',(3.53576509129249,0.158333333333334,9.35936221324765));
#56610=CARTESIAN_POINT('Ctrl Pts',(3.55620605750904,0.319434907277167,9.35786137336723));
#56611=CARTESIAN_POINT('Ctrl Pts',(3.630353335205,0.636309800095206,9.37426979185321));
#56612=CARTESIAN_POINT('Ctrl Pts',(3.68274913399112,0.79477268400084,9.39053710676437));
#56613=CARTESIAN_POINT('Ctrl Pts',(3.81258907846048,1.06847604194511,9.44126870438153));
#56614=CARTESIAN_POINT('Ctrl Pts',(3.8798859495176,1.18514270861178,9.46962156082298));
#56615=CARTESIAN_POINT('Ctrl Pts',(3.95827679071515,1.3,9.50436744488836));
#56616=CARTESIAN_POINT('Ctrl Pts',(3.85507599179486,-1.3,9.6731246947563));
#56617=CARTESIAN_POINT('Ctrl Pts',(3.78889068790036,-1.18514270861178,9.61843876361785));
#56618=CARTESIAN_POINT('Ctrl Pts',(3.73295432340165,-1.06847604194512,9.57151210020627));
#56619=CARTESIAN_POINT('Ctrl Pts',(3.62740723167584,-0.794772684000851,
9.48102758076393));
#56620=CARTESIAN_POINT('Ctrl Pts',(3.58650774416314,-0.636309800095197,
9.44584872924292));
#56621=CARTESIAN_POINT('Ctrl Pts',(3.5353568431438,-0.319434907277159,9.39183563380664));
#56622=CARTESIAN_POINT('Ctrl Pts',(3.52505210827391,-0.158333333333332,
9.37684078872385));
#56623=CARTESIAN_POINT('Ctrl Pts',(3.53576509129248,0.158333333333334,9.35936221324765));
#56624=CARTESIAN_POINT('Ctrl Pts',(3.55620605750904,0.319434907277167,9.35786137336722));
#56625=CARTESIAN_POINT('Ctrl Pts',(3.630353335205,0.636309800095206,9.3742697918532));
#56626=CARTESIAN_POINT('Ctrl Pts',(3.68274913399112,0.79477268400084,9.39053710676437));
#56627=CARTESIAN_POINT('Ctrl Pts',(3.81258907846048,1.06847604194511,9.44126870438153));
#56628=CARTESIAN_POINT('Ctrl Pts',(3.8798859495176,1.18514270861178,9.46962156082298));
#56629=CARTESIAN_POINT('Ctrl Pts',(3.95827679071515,1.3,9.50436744488836));
#56630=CARTESIAN_POINT('Ctrl Pts',(3.85507599179591,-1.30000000000182,9.67312469475717));
#56631=CARTESIAN_POINT('Ctrl Pts',(3.78889068790095,-1.18514270861302,9.61843876361835));
#56632=CARTESIAN_POINT('Ctrl Pts',(3.73295432340189,-1.06847604194574,9.57151210020649));
#56633=CARTESIAN_POINT('Ctrl Pts',(3.62740723167583,-0.794772684000851,
9.48102758076393));
#56634=CARTESIAN_POINT('Ctrl Pts',(3.58650774416313,-0.636309800095197,
9.44584872924292));
#56635=CARTESIAN_POINT('Ctrl Pts',(3.5353568431438,-0.319434907277159,9.39183563380664));
#56636=CARTESIAN_POINT('Ctrl Pts',(3.52505210827391,-0.158333333333332,
9.37684078872385));
#56637=CARTESIAN_POINT('Ctrl Pts',(3.53576509129248,0.158333333333334,9.35936221324765));
#56638=CARTESIAN_POINT('Ctrl Pts',(3.55620605750903,0.319434907277167,9.35786137336722));
#56639=CARTESIAN_POINT('Ctrl Pts',(3.630353335205,0.636309800095206,9.3742697918532));
#56640=CARTESIAN_POINT('Ctrl Pts',(3.68274913399112,0.79477268400084,9.39053710676436));
#56641=CARTESIAN_POINT('Ctrl Pts',(3.81258907846058,1.06847604194533,9.44126870438157));
#56642=CARTESIAN_POINT('Ctrl Pts',(3.87988594951784,1.18514270861221,9.46962156082308));
#56643=CARTESIAN_POINT('Ctrl Pts',(3.95827679071559,1.30000000000064,9.50436744488855));
#56644=CARTESIAN_POINT('Ctrl Pts',(3.85826144216853,-1.30000000000182,9.68127612476138));
#56645=CARTESIAN_POINT('Ctrl Pts',(3.79232877906293,-1.18514270861302,9.62595259112397));
#56646=CARTESIAN_POINT('Ctrl Pts',(3.73626839069632,-1.06847604194574,9.57885593655991));
#56647=CARTESIAN_POINT('Ctrl Pts',(3.62956460831631,-0.794772684000851,
9.48905897930467));
#56648=CARTESIAN_POINT('Ctrl Pts',(3.58606892907603,-0.636309800095197,
9.45644456788996));
#56649=CARTESIAN_POINT('Ctrl Pts',(3.53363020043342,-0.319434907277159,
9.40365643026874));
#56650=CARTESIAN_POINT('Ctrl Pts',(3.52377125174929,-0.158333333333332,
9.38834728808437));
#56651=CARTESIAN_POINT('Ctrl Pts',(3.53467416199073,0.158333333333334,9.37072723907264));
#56652=CARTESIAN_POINT('Ctrl Pts',(3.55506550337818,0.319434907277167,9.36920974049564));
#56653=CARTESIAN_POINT('Ctrl Pts',(3.63046739269399,0.636309800095206,9.3844909914869));
#56654=CARTESIAN_POINT('Ctrl Pts',(3.68470452743246,0.79477268400084,9.39897153694001));
#56655=CARTESIAN_POINT('Ctrl Pts',(3.81579954547164,1.06847604194533,9.44889760742223));
#56656=CARTESIAN_POINT('Ctrl Pts',(3.88343455679883,1.18514270861221,9.47718273592917));
#56657=CARTESIAN_POINT('Ctrl Pts',(3.96195840369317,1.30000000000064,9.51214184697453));
#56658=CARTESIAN_POINT('Ctrl Pts',(3.86592075441267,-1.3000000000016,9.69085660596058));
#56659=CARTESIAN_POINT('Ctrl Pts',(3.80285615568279,-1.18514270861281,9.6360113152689));
#56660=CARTESIAN_POINT('Ctrl Pts',(3.74843370181331,-1.06847604194556,9.58971588520396));
#56661=CARTESIAN_POINT('Ctrl Pts',(3.64267202968321,-0.794772684000714,
9.50251606882662));
#56662=CARTESIAN_POINT('Ctrl Pts',(3.59495986472817,-0.636309800095087,
9.4734863929025));
#56663=CARTESIAN_POINT('Ctrl Pts',(3.54045869646006,-0.319434907277103,
9.42271066769787));
#56664=CARTESIAN_POINT('Ctrl Pts',(3.52998469589636,-0.158333333333305,
9.40663233159606));
#56665=CARTESIAN_POINT('Ctrl Pts',(3.54101091709157,0.158333333333307,9.38890595207223));
#56666=CARTESIAN_POINT('Ctrl Pts',(3.56210793646514,0.319434907277111,9.38820387356399));
#56667=CARTESIAN_POINT('Ctrl Pts',(3.63989001762102,0.636309800095095,9.40094537760262));
#56668=CARTESIAN_POINT('Ctrl Pts',(3.69878792708314,0.794772684000703,9.41078085457383));
#56669=CARTESIAN_POINT('Ctrl Pts',(3.82891377614039,1.06847604194514,9.45816504858586));
#56670=CARTESIAN_POINT('Ctrl Pts',(3.89477549884898,1.185142708612,9.48594306864129));
#56671=CARTESIAN_POINT('Ctrl Pts',(3.97017228584713,1.30000000000041,9.52098824692175));
#56672=CARTESIAN_POINT('Ctrl Pts',(3.87702049239457,-1.30000000000152,9.70505728721452));
#56673=CARTESIAN_POINT('Ctrl Pts',(3.81695192563871,-1.18514270861274,9.65233487555218));
#56674=CARTESIAN_POINT('Ctrl Pts',(3.76461562236306,-1.06847604194549,9.60776978846544));
#56675=CARTESIAN_POINT('Ctrl Pts',(3.66157136742828,-0.794772684000663,
9.52366057371701));
#56676=CARTESIAN_POINT('Ctrl Pts',(3.61256958719336,-0.636309800095047,
9.49553345653393));
#56677=CARTESIAN_POINT('Ctrl Pts',(3.55745187272802,-0.319434907277084,
9.44590006181212));
#56678=CARTESIAN_POINT('Ctrl Pts',(3.54553271193669,-0.158333333333295,
9.42960489072957));
#56679=CARTESIAN_POINT('Ctrl Pts',(3.55660302454435,0.158333333333297,9.41177959321342));
#56680=CARTESIAN_POINT('Ctrl Pts',(3.57898330847349,0.319434907277092,9.41144980867689));
#56681=CARTESIAN_POINT('Ctrl Pts',(3.65789132771862,0.636309800095056,9.42232934580547));
#56682=CARTESIAN_POINT('Ctrl Pts',(3.71918153657403,0.794772684000653,9.42976789819879));
#56683=CARTESIAN_POINT('Ctrl Pts',(3.84673170978875,1.06847604194508,9.47395772293737));
#56684=CARTESIAN_POINT('Ctrl Pts',(3.91033538333747,1.18514270861193,9.50029893905725));
#56685=CARTESIAN_POINT('Ctrl Pts',(3.98233098664991,1.30000000000033,9.53385323356206));
#56686=CARTESIAN_POINT('Ctrl Pts',(3.88609751225472,-1.30000000000136,9.71696191407412));
#56687=CARTESIAN_POINT('Ctrl Pts',(3.8280562708361,-1.18514270861259,9.66611118291763));
#56688=CARTESIAN_POINT('Ctrl Pts',(3.77727688753419,-1.06847604194536,9.622797964979));
#56689=CARTESIAN_POINT('Ctrl Pts',(3.67674269870558,-0.794772684000565,
9.54014893016903));
#56690=CARTESIAN_POINT('Ctrl Pts',(3.62822311218295,-0.636309800094969,
9.51039538953031));
#56691=CARTESIAN_POINT('Ctrl Pts',(3.57299221293527,-0.319434907277045,
9.46094020063014));
#56692=CARTESIAN_POINT('Ctrl Pts',(3.55926865253983,-0.158333333333275,
9.44549008317312));
#56693=CARTESIAN_POINT('Ctrl Pts',(3.56996630046896,0.158333333333277,9.42814702429819));
#56694=CARTESIAN_POINT('Ctrl Pts',(3.59323177200466,0.31943490727705,9.42819201949836));
#56695=CARTESIAN_POINT('Ctrl Pts',(3.67260716245088,0.636309800094976,9.43837320885701));
#56696=CARTESIAN_POINT('Ctrl Pts',(3.73535384608084,0.794772684000557,9.44474638814701));
#56697=CARTESIAN_POINT('Ctrl Pts',(3.8607200019921,1.06847604194495,9.4870934019074));
#56698=CARTESIAN_POINT('Ctrl Pts',(3.92256824207985,1.18514270861178,9.51250695438991));
#56699=CARTESIAN_POINT('Ctrl Pts',(3.99199835863522,1.30000000000017,9.54500360620956));
#56700=CARTESIAN_POINT('Ctrl Pts',(3.89668925415032,-1.30000000000122,9.7318062296122));
#56701=CARTESIAN_POINT('Ctrl Pts',(3.84118533284187,-1.18514270861247,9.68351819215851));
#56702=CARTESIAN_POINT('Ctrl Pts',(3.7924107075366,-1.06847604194525,9.64189074955766));
#56703=CARTESIAN_POINT('Ctrl Pts',(3.69527758570974,-0.794772684000484,
9.56111033616606));
#56704=CARTESIAN_POINT('Ctrl Pts',(3.6476050737869,-0.636309800094904,9.52920935386177));
#56705=CARTESIAN_POINT('Ctrl Pts',(3.59290071013923,-0.319434907277012,
9.47926493980645));
#56706=CARTESIAN_POINT('Ctrl Pts',(3.57729331001879,-0.158333333333259,
9.4643543837362));
#56707=CARTESIAN_POINT('Ctrl Pts',(3.58862627895774,0.158333333333261,9.44606816444191));
#56708=CARTESIAN_POINT('Ctrl Pts',(3.61478304260594,0.319434907277019,9.44405152824428));
#56709=CARTESIAN_POINT('Ctrl Pts',(3.69416799578257,0.636309800094912,9.45397999004903));
#56710=CARTESIAN_POINT('Ctrl Pts',(3.75556658383759,0.794772684000476,9.46332859835313));
#56711=CARTESIAN_POINT('Ctrl Pts',(3.87726096117718,1.06847604194484,9.50430770534805));
#56712=CARTESIAN_POINT('Ctrl Pts',(3.93697193200774,1.18514270861166,9.52827507090723));
#56713=CARTESIAN_POINT('Ctrl Pts',(4.0037168869396,1.30000000000004,9.55847146503303));
#56714=CARTESIAN_POINT('Ctrl Pts',(3.90634129735519,-1.3000000000009,9.74759065323477));
#56715=CARTESIAN_POINT('Ctrl Pts',(3.85342469448244,-1.18514270861217,9.70153780835584));
#56716=CARTESIAN_POINT('Ctrl Pts',(3.80670493679023,-1.06847604194498,9.66133186724594));
#56717=CARTESIAN_POINT('Ctrl Pts',(3.71308890230765,-0.794772684000283,
9.58195561748694));
#56718=CARTESIAN_POINT('Ctrl Pts',(3.66601329086534,-0.636309800094744,
9.54824301996284));
#56719=CARTESIAN_POINT('Ctrl Pts',(3.61258653861628,-0.319434907276932,
9.49675443327196));
#56720=CARTESIAN_POINT('Ctrl Pts',(3.59690518833244,-0.15833333333322,9.48001577447521));
#56721=CARTESIAN_POINT('Ctrl Pts',(3.608493963035,0.158333333333222,9.461317513484));
#56722=CARTESIAN_POINT('Ctrl Pts',(3.63496333697317,0.31943490727694,9.46067316835298));
#56723=CARTESIAN_POINT('Ctrl Pts',(3.71362666110114,0.636309800094754,9.47139565978765));
#56724=CARTESIAN_POINT('Ctrl Pts',(3.77484661577608,0.794772684000275,9.48210622793863));
#56725=CARTESIAN_POINT('Ctrl Pts',(3.89338202163702,1.06847604194457,9.52137630637699));
#56726=CARTESIAN_POINT('Ctrl Pts',(3.95113583823423,1.18514270861136,9.5438845238286));
#56727=CARTESIAN_POINT('Ctrl Pts',(4.01533388640107,1.29999999999971,9.57190239687566));
#56728=CARTESIAN_POINT('Ctrl Pts',(3.92055275904314,-1.30000000000069,9.76714384265902));
#56729=CARTESIAN_POINT('Ctrl Pts',(3.87074553539678,-1.18514270861199,9.72462993178228));
#56730=CARTESIAN_POINT('Ctrl Pts',(3.82646932967549,-1.06847604194481,9.68679759168984));
#56731=CARTESIAN_POINT('Ctrl Pts',(3.73696019491823,-0.794772684000161,
9.61021268279958));
#56732=CARTESIAN_POINT('Ctrl Pts',(3.69053367825845,-0.636309800094645,
9.57431182373749));
#56733=CARTESIAN_POINT('Ctrl Pts',(3.63824691831124,-0.319434907276882,
9.5215524571651));
#56734=CARTESIAN_POINT('Ctrl Pts',(3.62175628555497,-0.158333333333195,
9.50327554072841));
#56735=CARTESIAN_POINT('Ctrl Pts',(3.63382136573945,0.158333333333197,9.48387740247822));
#56736=CARTESIAN_POINT('Ctrl Pts',(3.66183719787731,0.319434907276889,9.48366594610305));
#56737=CARTESIAN_POINT('Ctrl Pts',(3.73979935576851,0.636309800094653,9.49505957507951));
#56738=CARTESIAN_POINT('Ctrl Pts',(3.80018656415803,0.794772684000152,9.50830811335043));
#56739=CARTESIAN_POINT('Ctrl Pts',(3.91424294631096,1.0684760419444,9.5454000284948));
#56740=CARTESIAN_POINT('Ctrl Pts',(3.96930245432026,1.18514270861118,9.5659264892443));
#56741=CARTESIAN_POINT('Ctrl Pts',(4.03005068871032,1.29999999999951,9.59092369506821));
#56742=CARTESIAN_POINT('Ctrl Pts',(3.94293405228111,-1.30000000000015,9.80416499781465));
#56743=CARTESIAN_POINT('Ctrl Pts',(3.8983024693755,-1.18514270861149,9.76803405560948));
#56744=CARTESIAN_POINT('Ctrl Pts',(3.85820837626867,-1.06847604194437,9.73438444526762));
#56745=CARTESIAN_POINT('Ctrl Pts',(3.77606550955316,-0.794772683999828,
9.66237948678966));
#56746=CARTESIAN_POINT('Ctrl Pts',(3.73140337306608,-0.636309800094378,
9.62201111664065));
#56747=CARTESIAN_POINT('Ctrl Pts',(3.68201299142563,-0.319434907276748,
9.56597413151367));
#56748=CARTESIAN_POINT('Ctrl Pts',(3.66527160877993,-0.158333333333129,
9.54356452515937));
#56749=CARTESIAN_POINT('Ctrl Pts',(3.67795836472447,0.158333333333131,9.52326664911772));
#56750=CARTESIAN_POINT('Ctrl Pts',(3.70674579656327,0.319434907276756,9.52630170301223));
#56751=CARTESIAN_POINT('Ctrl Pts',(3.78328326010629,0.636309800094388,9.53911263248325));
#56752=CARTESIAN_POINT('Ctrl Pts',(3.84350301597519,0.794772683999818,9.55503418266844));
#56753=CARTESIAN_POINT('Ctrl Pts',(3.95059279887267,1.06847604194395,9.58729351177311));
#56754=CARTESIAN_POINT('Ctrl Pts',(4.00127565766729,1.18514270861068,9.60400458986381));
#56755=CARTESIAN_POINT('Ctrl Pts',(4.0562861763077,1.29999999999897,9.62346287780173));
#56756=CARTESIAN_POINT('Ctrl Pts',(3.96875291306454,-1.29999999999862,9.84603918270511));
#56757=CARTESIAN_POINT('Ctrl Pts',(3.93016088876956,-1.1851427086101,9.81706547124778));
#56758=CARTESIAN_POINT('Ctrl Pts',(3.89466683773055,-1.06847604194311,9.78844476197471));
#56759=CARTESIAN_POINT('Ctrl Pts',(3.81982541723873,-0.794772683998892,
9.72314070366436));
#56760=CARTESIAN_POINT('Ctrl Pts',(3.77508220407105,-0.636309800093627,
9.68031539928032));
#56761=CARTESIAN_POINT('Ctrl Pts',(3.72755718756055,-0.319434907276371,
9.62250450440374));
#56762=CARTESIAN_POINT('Ctrl Pts',(3.71010374373434,-0.158333333332942,
9.59611900134765));
#56763=CARTESIAN_POINT('Ctrl Pts',(3.723858703403,0.158333333332944,9.57443114782916));
#56764=CARTESIAN_POINT('Ctrl Pts',(3.75491767159857,0.319434907276382,9.57935654222014));
#56765=CARTESIAN_POINT('Ctrl Pts',(3.8307649395092,0.63630980009364,9.59252694118864));
#56766=CARTESIAN_POINT('Ctrl Pts',(3.89074061160296,0.79477268399888,9.61149586566595));
#56767=CARTESIAN_POINT('Ctrl Pts',(3.99041779475234,1.06847604194269,9.63743017681932));
#56768=CARTESIAN_POINT('Ctrl Pts',(4.03637498942812,1.18514270860928,9.64938301440751));
#56769=CARTESIAN_POINT('Ctrl Pts',(4.08514281959792,1.29999999999743,9.6620626872465));
#56770=CARTESIAN_POINT('Ctrl Pts',(3.98735158280415,-1.29999999999731,9.87931932511148));
#56771=CARTESIAN_POINT('Ctrl Pts',(3.95241863019103,-1.1851427086089,9.8568395664758));
#56772=CARTESIAN_POINT('Ctrl Pts',(3.91986501806147,-1.06847604194203,9.83267478419246));
#56773=CARTESIAN_POINT('Ctrl Pts',(3.85015641421704,-0.794772683998091,
9.77295656125614));
#56774=CARTESIAN_POINT('Ctrl Pts',(3.80654379785225,-0.636309800092987,
9.72693137572071));
#56775=CARTESIAN_POINT('Ctrl Pts',(3.76096461886723,-0.31943490727605,9.66723501569675));
#56776=CARTESIAN_POINT('Ctrl Pts',(3.74319802800101,-0.158333333332783,
9.63761237718672));
#56777=CARTESIAN_POINT('Ctrl Pts',(3.75756771109968,0.158333333332785,9.61518494541643));
#56778=CARTESIAN_POINT('Ctrl Pts',(3.78960399643097,0.319434907276058,9.62250093354075));
#56779=CARTESIAN_POINT('Ctrl Pts',(3.8646568548837,0.636309800092997,9.63626820689347));
#56780=CARTESIAN_POINT('Ctrl Pts',(3.924559082504,0.794772683998081,9.65734774837526));
#56781=CARTESIAN_POINT('Ctrl Pts',(4.01902525308205,1.06847604194162,9.6779119389689));
#56782=CARTESIAN_POINT('Ctrl Pts',(4.06167184187158,1.18514270860809,9.68588862628807));
#56783=CARTESIAN_POINT('Ctrl Pts',(4.10607411452398,1.29999999999612,9.69294052479679));
#56784=CARTESIAN_POINT('Ctrl Pts',(3.99403512297787,-1.29999999999721,9.89169252950751));
#56785=CARTESIAN_POINT('Ctrl Pts',(3.9606540177041,-1.18514270860881,9.87137520140306));
#56786=CARTESIAN_POINT('Ctrl Pts',(3.92930683107614,-1.06847604194195,9.84871399883852));
#56787=CARTESIAN_POINT('Ctrl Pts',(3.86158731793836,-0.794772683998027,
9.79094726866334));
#56788=CARTESIAN_POINT('Ctrl Pts',(3.81817773071631,-0.636309800092936,
9.74398831071881));
#56789=CARTESIAN_POINT('Ctrl Pts',(3.77313731734351,-0.319434907276024,
9.6838093055602));
#56790=CARTESIAN_POINT('Ctrl Pts',(3.75513147909687,-0.15833333333277,9.65314579603697));
#56791=CARTESIAN_POINT('Ctrl Pts',(3.76958198214413,0.158333333332772,9.63061650050148));
#56792=CARTESIAN_POINT('Ctrl Pts',(3.80185442000686,0.319434907276032,9.63895252512564));
#56793=CARTESIAN_POINT('Ctrl Pts',(3.87670406566407,0.636309800092946,9.65282990370601));
#56794=CARTESIAN_POINT('Ctrl Pts',(3.93688123514687,0.794772683998017,9.67432964771585));
#56795=CARTESIAN_POINT('Ctrl Pts',(4.0295951989573,1.06847604194153,9.69271824339368));
#56796=CARTESIAN_POINT('Ctrl Pts',(4.07106409330812,1.185142708608,9.69918153666264));
#56797=CARTESIAN_POINT('Ctrl Pts',(4.11386944246713,1.29999999999602,9.70414838149625));
#56798=CARTESIAN_POINT('Ctrl Pts',(3.99548245121749,-1.2999999999972,9.89448355290227));
#56799=CARTESIAN_POINT('Ctrl Pts',(3.96245342304708,-1.1851427086088,9.87463893210296));
#56800=CARTESIAN_POINT('Ctrl Pts',(3.93138095929411,-1.06847604194195,9.85230465165239));
#56801=CARTESIAN_POINT('Ctrl Pts',(3.8641174072135,-0.794772683998026,9.79495638400513));
#56802=CARTESIAN_POINT('Ctrl Pts',(3.82076935379783,-0.636309800092935,
9.7477713080824));
#56803=CARTESIAN_POINT('Ctrl Pts',(3.77584147348526,-0.319434907276024,
9.68749407186112));
#56804=CARTESIAN_POINT('Ctrl Pts',(3.75775134690968,-0.15833333333277,9.65663560839093));
#56805=CARTESIAN_POINT('Ctrl Pts',(3.77220906636897,0.158333333332772,9.63409644252598));
#56806=CARTESIAN_POINT('Ctrl Pts',(3.8045508416485,0.319434907276032,9.64263942631028));
#56807=CARTESIAN_POINT('Ctrl Pts',(3.87934780680038,0.636309800092945,9.65655037189766));
#56808=CARTESIAN_POINT('Ctrl Pts',(3.93956300403386,0.794772683998015,9.67817041277619));
#56809=CARTESIAN_POINT('Ctrl Pts',(4.03187898273703,1.06847604194153,9.69608662897828));
#56810=CARTESIAN_POINT('Ctrl Pts',(4.07308576997995,1.18514270860799,9.70221472645836));
#56811=CARTESIAN_POINT('Ctrl Pts',(4.11553917792927,1.29999999999602,9.70671565528587));
#56812=CARTESIAN_POINT('Ctrl Pts',(3.99797166780253,-1.29999999999717,9.89941379417368));
#56813=CARTESIAN_POINT('Ctrl Pts',(3.96557500474023,-1.18514270860878,9.88037837286466));
#56814=CARTESIAN_POINT('Ctrl Pts',(3.93499238939632,-1.06847604194192,9.85860615648363));
#56815=CARTESIAN_POINT('Ctrl Pts',(3.86853124304929,-0.794772683998007,
9.80198543701632));
#56816=CARTESIAN_POINT('Ctrl Pts',(3.82525865750305,-0.636309800092921,
9.75444054534181));
#56817=CARTESIAN_POINT('Ctrl Pts',(3.78052866433776,-0.319434907276017,
9.6939911087952));
#56818=CARTESIAN_POINT('Ctrl Pts',(3.7623170733993,-0.158333333332766,9.66276336039861));
#56819=CARTESIAN_POINT('Ctrl Pts',(3.77679422781962,0.158333333332768,9.64020027376793));
#56820=CARTESIAN_POINT('Ctrl Pts',(3.80924760100915,0.319434907276024,9.64911659737234));
#56821=CARTESIAN_POINT('Ctrl Pts',(3.88394595150036,0.63630980009293,9.66309403400363));
#56822=CARTESIAN_POINT('Ctrl Pts',(3.9442291986607,0.794772683997997,9.68492192453384));
#56823=CARTESIAN_POINT('Ctrl Pts',(4.03583458505829,1.06847604194151,9.7020296605304));
#56824=CARTESIAN_POINT('Ctrl Pts',(4.07657380738917,1.18514270860797,9.70758279402453));
#56825=CARTESIAN_POINT('Ctrl Pts',(4.11839967459347,1.29999999999599,9.71128375600398));
#56826=CARTESIAN_POINT('Ctrl Pts',(4.00320446632834,-1.2999999999971,9.90899225940445));
#56827=CARTESIAN_POINT('Ctrl Pts',(3.97182844926294,-1.18514270860871,9.89183616775541));
#56828=CARTESIAN_POINT('Ctrl Pts',(3.94207265564493,-1.06847604194186,9.87135239871074));
#56829=CARTESIAN_POINT('Ctrl Pts',(3.87707386004942,-0.794772683997962,
9.81634319397025));
#56830=CARTESIAN_POINT('Ctrl Pts',(3.83424674884023,-0.636309800092884,
9.76777093058625));
#56831=CARTESIAN_POINT('Ctrl Pts',(3.78993922064094,-0.319434907275998,
9.70695278349702));
#56832=CARTESIAN_POINT('Ctrl Pts',(3.77129151705819,-0.158333333332757,
9.67520013979713));
#56833=CARTESIAN_POINT('Ctrl Pts',(3.78589928806803,0.158333333332759,9.65247549954131));
#56834=CARTESIAN_POINT('Ctrl Pts',(3.81890980236496,0.319434907276005,9.6617440984977));
#56835=CARTESIAN_POINT('Ctrl Pts',(3.89347127480144,0.636309800092893,9.67578371387904));
#56836=CARTESIAN_POINT('Ctrl Pts',(3.95361913043491,0.794772683997952,9.69835270852644));
#56837=CARTESIAN_POINT('Ctrl Pts',(4.0437826366301,1.06847604194144,9.71386634146029));
#56838=CARTESIAN_POINT('Ctrl Pts',(4.08361996487777,1.1851427086079,9.71822828741913));
#56839=CARTESIAN_POINT('Ctrl Pts',(4.12426618042834,1.29999999999591,9.72023690247649));
#56840=CARTESIAN_POINT('Ctrl Pts',(4.01323645802655,-1.29999999999633,9.92858671349471));
#56841=CARTESIAN_POINT('Ctrl Pts',(3.98384646628841,-1.18514270860801,9.91523289095328));
#56842=CARTESIAN_POINT('Ctrl Pts',(3.95563047679174,-1.06847604194123,9.8974408084055));
#56843=CARTESIAN_POINT('Ctrl Pts',(3.89315807650135,-0.794772683997495,
9.84608426994085));
#56844=CARTESIAN_POINT('Ctrl Pts',(3.85023033533171,-0.63630980009251,9.79657078654875));
#56845=CARTESIAN_POINT('Ctrl Pts',(3.80723555286186,-0.319434907275811,
9.73450522600868));
#56846=CARTESIAN_POINT('Ctrl Pts',(3.78939487367443,-0.158333333332664,
9.69984558077839));
#56847=CARTESIAN_POINT('Ctrl Pts',(3.80497460358648,0.158333333332666,9.6760204528219));
#56848=CARTESIAN_POINT('Ctrl Pts',(3.83867077453724,0.319434907275819,9.686480371128));
#56849=CARTESIAN_POINT('Ctrl Pts',(3.91283863802461,0.636309800092521,9.70077889261199));
#56850=CARTESIAN_POINT('Ctrl Pts',(3.97250164099645,0.794772683997486,9.72506305942813));
#56851=CARTESIAN_POINT('Ctrl Pts',(4.0598594729798,1.06847604194082,9.73728377547029));
#56852=CARTESIAN_POINT('Ctrl Pts',(4.09799742777746,1.1851427086072,9.73913642114516));
#56853=CARTESIAN_POINT('Ctrl Pts',(4.13645936883385,1.29999999999515,9.7375518173424));
#56854=CARTESIAN_POINT('Ctrl Pts',(4.02401382537848,-1.29999999999515,9.9473557434411));
#56855=CARTESIAN_POINT('Ctrl Pts',(3.99658515229895,-1.18514270860693,9.93781974419851));
#56856=CARTESIAN_POINT('Ctrl Pts',(3.96992373723207,-1.06847604194025,9.92269524025967));
#56857=CARTESIAN_POINT('Ctrl Pts',(3.91010305432856,-0.794772683996766,
9.87484404668957));
#56858=CARTESIAN_POINT('Ctrl Pts',(3.86776283598717,-0.636309800091926,
9.82362940522103));
#56859=CARTESIAN_POINT('Ctrl Pts',(3.82540760025208,-0.319434907275517,
9.76107975393186));
#56860=CARTESIAN_POINT('Ctrl Pts',(3.80694211371491,-0.158333333332519,
9.72512312909289));
#56861=CARTESIAN_POINT('Ctrl Pts',(3.82234834042072,0.158333333332521,9.70149098605119));
#56862=CARTESIAN_POINT('Ctrl Pts',(3.85606966362876,0.319434907275526,9.71389736476582));
#56863=CARTESIAN_POINT('Ctrl Pts',(3.93011260755125,0.636309800091936,9.72814322412588));
#56864=CARTESIAN_POINT('Ctrl Pts',(3.99101408165235,0.794772683996756,9.75215086712417));
#56865=CARTESIAN_POINT('Ctrl Pts',(4.07584817888741,1.06847604193984,9.76079341287856));
#56866=CARTESIAN_POINT('Ctrl Pts',(4.11210970515826,1.18514270860611,9.76036799993197));
#56867=CARTESIAN_POINT('Ctrl Pts',(4.14791122041998,1.29999999999395,9.75577613621959));
#56868=CARTESIAN_POINT('Ctrl Pts',(4.03457043750772,-1.29999999999448,9.97065174313936));
#56869=CARTESIAN_POINT('Ctrl Pts',(4.00948073920188,-1.18514270860633,9.96535096285632));
#56870=CARTESIAN_POINT('Ctrl Pts',(3.98464701546341,-1.06847604193971,9.95320760337727));
#56871=CARTESIAN_POINT('Ctrl Pts',(3.92786749811646,-0.794772683996364,
9.90934628691403));
#56872=CARTESIAN_POINT('Ctrl Pts',(3.88575480123707,-0.636309800091603,
9.85670437769421));
#56873=CARTESIAN_POINT('Ctrl Pts',(3.84455648997016,-0.319434907275354,
9.79316184315602));
#56874=CARTESIAN_POINT('Ctrl Pts',(3.82602794471147,-0.158333333332438,
9.75503933008314));
#56875=CARTESIAN_POINT('Ctrl Pts',(3.842391775896,0.15833333333244,9.7303546939524));
#56876=CARTESIAN_POINT('Ctrl Pts',(3.87770341865184,0.319434907275365,9.74321118973647));
#56877=CARTESIAN_POINT('Ctrl Pts',(3.95137966051613,0.636309800091614,9.75765712938725));
#56878=CARTESIAN_POINT('Ctrl Pts',(4.01111397319714,0.794772683996351,9.78428068645223));
#56879=CARTESIAN_POINT('Ctrl Pts',(4.09274234391537,1.06847604193929,9.78918670955597));
#56880=CARTESIAN_POINT('Ctrl Pts',(4.12717304692835,1.18514270860551,9.78579317965512));
#56881=CARTESIAN_POINT('Ctrl Pts',(4.16070055589961,1.29999999999329,9.77688248423786));
#56882=CARTESIAN_POINT('Ctrl Pts',(4.04634921388171,-1.29999999999287,9.99261507851378));
#56883=CARTESIAN_POINT('Ctrl Pts',(4.02330211125708,-1.18514270860486,9.99186037780706));
#56884=CARTESIAN_POINT('Ctrl Pts',(4.00010340364208,-1.06847604193839,9.98289979062435));
#56885=CARTESIAN_POINT('Ctrl Pts',(3.94615951030976,-0.794772683995377,
9.94324180233157));
#56886=CARTESIAN_POINT('Ctrl Pts',(3.90486148846194,-0.636309800090813,
9.88853779748812));
#56887=CARTESIAN_POINT('Ctrl Pts',(3.86425783077975,-0.319434907274957,
9.8246199928221));
#56888=CARTESIAN_POINT('Ctrl Pts',(3.84472846232997,-0.158333333332242,
9.78535172278455));
#56889=CARTESIAN_POINT('Ctrl Pts',(3.86088111472339,0.158333333332244,9.76091246291785));
#56890=CARTESIAN_POINT('Ctrl Pts',(3.89644952316345,0.319434907274968,9.77572751296444));
#56891=CARTESIAN_POINT('Ctrl Pts',(3.97018639102631,0.636309800090824,9.78989274073506));
#56892=CARTESIAN_POINT('Ctrl Pts',(4.03129986387343,0.794772683995363,9.81625797980789));
#56893=CARTESIAN_POINT('Ctrl Pts',(4.11043152187304,1.06847604193797,9.81664722734172));
#56894=CARTESIAN_POINT('Ctrl Pts',(4.1429577847685,1.18514270860404,9.81038162838847));
#56895=CARTESIAN_POINT('Ctrl Pts',(4.17375714792826,1.29999999999168,9.79768193964762));
#56896=CARTESIAN_POINT('Ctrl Pts',(4.05635056619991,-1.29999999998975,10.0142690078584));
#56897=CARTESIAN_POINT('Ctrl Pts',(4.03544628027288,-1.18514270860201,10.0175057276255));
#56898=CARTESIAN_POINT('Ctrl Pts',(4.01384845430562,-1.06847604193582,10.0114363617991));
#56899=CARTESIAN_POINT('Ctrl Pts',(3.96235093945595,-0.79477268399347,9.97591599317089));
#56900=CARTESIAN_POINT('Ctrl Pts',(3.92055436487356,-0.636309800089288,
9.92062666986226));
#56901=CARTESIAN_POINT('Ctrl Pts',(3.8808985634387,-0.319434907274192,9.85594791688383));
#56902=CARTESIAN_POINT('Ctrl Pts',(3.86189554664143,-0.158333333331862,
9.81407600400371));
#56903=CARTESIAN_POINT('Ctrl Pts',(3.87899850634942,0.158333333331864,9.78863250623016));
#56904=CARTESIAN_POINT('Ctrl Pts',(3.91559292543677,0.3194349072742,9.80438067216241));
#56905=CARTESIAN_POINT('Ctrl Pts',(3.98909130197214,0.636309800089297,9.81861847075731));
#56906=CARTESIAN_POINT('Ctrl Pts',(4.04965588928553,0.794772683993459,9.84680488231586));
#56907=CARTESIAN_POINT('Ctrl Pts',(4.12603725524005,1.06847604193541,9.84343121678803));
#56908=CARTESIAN_POINT('Ctrl Pts',(4.15689741615992,1.1851427086012,9.83434719176427));
#56909=CARTESIAN_POINT('Ctrl Pts',(4.18555507488646,1.29999999998857,9.81763947651711));
#56910=CARTESIAN_POINT('Ctrl Pts',(4.06273679756711,-1.29999999998941,10.0279056870545));
#56911=CARTESIAN_POINT('Ctrl Pts',(4.04305412357837,-1.1851427086017,10.0338073315529));
#56912=CARTESIAN_POINT('Ctrl Pts',(4.02240682746204,-1.06847604193554,10.0296324218589));
#56913=CARTESIAN_POINT('Ctrl Pts',(3.97247897286925,-0.794772683993263,
9.9967086892858));
#56914=CARTESIAN_POINT('Ctrl Pts',(3.93074708407459,-0.636309800089121,
9.94065147793032));
#56915=CARTESIAN_POINT('Ctrl Pts',(3.89171929918422,-0.319434907274109,
9.875472533128));
#56916=CARTESIAN_POINT('Ctrl Pts',(3.87294279440502,-0.158333333331821,
9.83207404610695));
#56917=CARTESIAN_POINT('Ctrl Pts',(3.89023914234746,0.158333333331822,9.80644326801721));
#56918=CARTESIAN_POINT('Ctrl Pts',(3.9268624976559,0.319434907274116,9.82345867854917));
#56919=CARTESIAN_POINT('Ctrl Pts',(4.00000036379485,0.63630980008913,9.83796195153213));
#56920=CARTESIAN_POINT('Ctrl Pts',(4.06050936822068,0.794772683993251,9.86696403121066));
#56921=CARTESIAN_POINT('Ctrl Pts',(4.13543227900064,1.06847604193513,9.86089790353117));
#56922=CARTESIAN_POINT('Ctrl Pts',(4.16538632929968,1.18514270860089,9.84987076073));
#56923=CARTESIAN_POINT('Ctrl Pts',(4.19286307798853,1.29999999998823,9.83044227702793));
#56924=CARTESIAN_POINT('Ctrl Pts',(4.06407190888843,-1.29999999998939,10.030785444544));
#56925=CARTESIAN_POINT('Ctrl Pts',(4.0446499038056,-1.18514270860168,10.0372436682821));
#56926=CARTESIAN_POINT('Ctrl Pts',(4.02420436638832,-1.06847604193552,10.0334654494754));
#56927=CARTESIAN_POINT('Ctrl Pts',(3.97460652038925,-0.79477268399325,10.0010887781306));
#56928=CARTESIAN_POINT('Ctrl Pts',(3.93288084414568,-0.636309800089111,
9.94487936290763));
#56929=CARTESIAN_POINT('Ctrl Pts',(3.89398020931323,-0.319434907274104,
9.87960085633521));
#56930=CARTESIAN_POINT('Ctrl Pts',(3.87523649645876,-0.158333333331818,
9.83589642165554));
#56931=CARTESIAN_POINT('Ctrl Pts',(3.89259805848843,0.15833333333182,9.81019947911735));
#56932=CARTESIAN_POINT('Ctrl Pts',(3.92927976210183,0.319434907274111,9.8274250670269));
#56933=CARTESIAN_POINT('Ctrl Pts',(4.00237050489757,0.636309800089121,9.84195343451171));
#56934=CARTESIAN_POINT('Ctrl Pts',(4.06286845920188,0.794772683993239,9.8711272305367));
#56935=CARTESIAN_POINT('Ctrl Pts',(4.13746609783607,1.06847604193511,9.86451433880063));
#56936=CARTESIAN_POINT('Ctrl Pts',(4.16721451160574,1.18514270860087,9.85309427136058));
#56937=CARTESIAN_POINT('Ctrl Pts',(4.19442078549526,1.2999999999882,9.83311661228122));
#56938=CARTESIAN_POINT('Ctrl Pts',(4.06539413056257,-1.29999999998936,10.0336772368117));
#56939=CARTESIAN_POINT('Ctrl Pts',(4.04622008422138,-1.18514270860165,10.0407041704229));
#56940=CARTESIAN_POINT('Ctrl Pts',(4.02597047400536,-1.0684760419355,10.0373281368284));
#56941=CARTESIAN_POINT('Ctrl Pts',(3.97670505576914,-0.79477268399323,10.0054958885001));
#56942=CARTESIAN_POINT('Ctrl Pts',(3.93502274247802,-0.636309800089095,
9.94909767065479));
#56943=CARTESIAN_POINT('Ctrl Pts',(3.89625125716468,-0.319434907274095,
9.88371848291633));
#56944=CARTESIAN_POINT('Ctrl Pts',(3.8775116970533,-0.158333333331814,9.83973775688691));
#56945=CARTESIAN_POINT('Ctrl Pts',(3.89493180960951,0.158333333331816,9.81398187906456));
#56946=CARTESIAN_POINT('Ctrl Pts',(3.93167968973624,0.319434907274104,9.83140992297885));
#56947=CARTESIAN_POINT('Ctrl Pts',(4.00473655379493,0.636309800089104,9.84594927505052));
#56948=CARTESIAN_POINT('Ctrl Pts',(4.06524505505404,0.794772683993218,9.87527100401899));
#56949=CARTESIAN_POINT('Ctrl Pts',(4.13951924770019,1.06847604193508,9.86810947420546));
#56950=CARTESIAN_POINT('Ctrl Pts',(4.16905771469347,1.18514270860084,9.85630127118908));
#56951=CARTESIAN_POINT('Ctrl Pts',(4.19598410281357,1.29999999998817,9.83578482605177));
#56952=CARTESIAN_POINT('Ctrl Pts',(4.06702106849627,-1.29999999998931,10.0373163253182));
#56953=CARTESIAN_POINT('Ctrl Pts',(4.04813576014217,-1.18514270860161,10.0450740546847));
#56954=CARTESIAN_POINT('Ctrl Pts',(4.02812092299354,-1.06847604193546,10.0422101886781));
#56955=CARTESIAN_POINT('Ctrl Pts',(3.97927320774905,-0.7947726839932,10.0110560751343));
#56956=CARTESIAN_POINT('Ctrl Pts',(3.93770348720174,-0.636309800089071,
9.95436547522951));
#56957=CARTESIAN_POINT('Ctrl Pts',(3.89909560486339,-0.319434907274084,
9.88885990982302));
#56958=CARTESIAN_POINT('Ctrl Pts',(3.88030760619111,-0.158333333331808,
9.84458913724083));
#56959=CARTESIAN_POINT('Ctrl Pts',(3.89780562564834,0.15833333333181,9.81875431996012));
#56960=CARTESIAN_POINT('Ctrl Pts',(3.93467978356113,0.319434907274091,9.83638947813788));
#56961=CARTESIAN_POINT('Ctrl Pts',(4.00773187324364,0.63630980008908,9.85090254699385));
#56962=CARTESIAN_POINT('Ctrl Pts',(4.0682867679093,0.794772683993188,9.88037321740751));
#56963=CARTESIAN_POINT('Ctrl Pts',(4.14214844183579,1.06847604193504,9.87253512493884));
#56964=CARTESIAN_POINT('Ctrl Pts',(4.17140894963151,1.1851427086008,9.86025872487337));
#56965=CARTESIAN_POINT('Ctrl Pts',(4.1979579834249,1.29999999998812,9.83909874454217));
#56966=CARTESIAN_POINT('Ctrl Pts',(4.06893477246844,-1.29999999998919,10.0417192296828));
#56967=CARTESIAN_POINT('Ctrl Pts',(4.05035550228226,-1.1851427086015,10.0503926853874));
#56968=CARTESIAN_POINT('Ctrl Pts',(4.03060230955086,-1.06847604193536,10.0481625746812));
#56969=CARTESIAN_POINT('Ctrl Pts',(3.98225648680696,-0.794772683993127,
10.0178211531579));
#56970=CARTESIAN_POINT('Ctrl Pts',(3.94092454857736,-0.636309800089012,
9.96067906367977));
#56971=CARTESIAN_POINT('Ctrl Pts',(3.90251876080255,-0.319434907274054,
9.89501868530541));
#56972=CARTESIAN_POINT('Ctrl Pts',(3.88359133101194,-0.158333333331793,
9.85048421334946));
#56973=CARTESIAN_POINT('Ctrl Pts',(3.90117604894202,0.158333333331795,9.82456207766625));
#56974=CARTESIAN_POINT('Ctrl Pts',(3.93824360631013,0.319434907274062,9.8424022812568));
#56975=CARTESIAN_POINT('Ctrl Pts',(4.01133686890583,0.636309800089021,9.85683391437836));
#56976=CARTESIAN_POINT('Ctrl Pts',(4.07200338624086,0.794772683993115,9.88642225662819));
#56977=CARTESIAN_POINT('Ctrl Pts',(4.14536995439803,1.06847604193494,9.87777292559078));
#56978=CARTESIAN_POINT('Ctrl Pts',(4.1742813560123,1.18514270860069,9.86495189325206));
#56979=CARTESIAN_POINT('Ctrl Pts',(4.20034649038486,1.299999999988,9.84305380349143));
#56980=CARTESIAN_POINT('Ctrl Pts',(4.07083807594505,-1.29999999998909,10.0461309059185));
#56981=CARTESIAN_POINT('Ctrl Pts',(4.05255207824646,-1.18514270860141,10.055732233939));
#56982=CARTESIAN_POINT('Ctrl Pts',(4.03305249272199,-1.06847604193528,10.054143531469));
#56983=CARTESIAN_POINT('Ctrl Pts',(3.98520091862669,-0.794772683993069,
10.0246221019535));
#56984=CARTESIAN_POINT('Ctrl Pts',(3.94412315433243,-0.636309800088966,
9.9670123053312));
#56985=CARTESIAN_POINT('Ctrl Pts',(3.90591806478903,-0.319434907274031,
9.90119978391372));
#56986=CARTESIAN_POINT('Ctrl Pts',(3.88683852260301,-0.158333333331782,
9.8564163676154));
#56987=CARTESIAN_POINT('Ctrl Pts',(3.90450748901525,0.158333333331784,9.83041016796613));
#56988=CARTESIAN_POINT('Ctrl Pts',(3.94177224561851,0.319434907274039,9.84845092754632));
#56989=CARTESIAN_POINT('Ctrl Pts',(4.01491618752075,0.636309800088976,9.86279080280935));
#56990=CARTESIAN_POINT('Ctrl Pts',(4.0757057334192,0.794772683993058,9.89248424162781));
#56991=CARTESIAN_POINT('Ctrl Pts',(4.14858696511739,1.06847604193487,9.88301352662142));
#56992=CARTESIAN_POINT('Ctrl Pts',(4.17715248654312,1.1851427086006,9.86964469808969));
#56993=CARTESIAN_POINT('Ctrl Pts',(4.20273594470819,1.29999999998791,9.84700656262791));
#56994=CARTESIAN_POINT('Ctrl Pts',(4.07228048230189,-1.29999999998897,10.0494243716724));
#56995=CARTESIAN_POINT('Ctrl Pts',(4.05422942402522,-1.1851427086013,10.0597069074288));
#56996=CARTESIAN_POINT('Ctrl Pts',(4.03492509698501,-1.06847604193518,10.0585942639093));
#56997=CARTESIAN_POINT('Ctrl Pts',(3.98743293814549,-0.794772683992996,
10.0296986910705));
#56998=CARTESIAN_POINT('Ctrl Pts',(3.94648567623039,-0.636309800088908,
9.97179668357852));
#56999=CARTESIAN_POINT('Ctrl Pts',(3.90842363585003,-0.319434907274002,
9.90587732661702));
#57000=CARTESIAN_POINT('Ctrl Pts',(3.88927784857038,-0.158333333331767,
9.86086012943157));
#57001=CARTESIAN_POINT('Ctrl Pts',(3.90700922326024,0.158333333331769,9.83479267464078));
#57002=CARTESIAN_POINT('Ctrl Pts',(3.94438905042288,0.319434907274009,9.85301735823453));
#57003=CARTESIAN_POINT('Ctrl Pts',(4.01754473153985,0.636309800088917,9.86731607927766));
#57004=CARTESIAN_POINT('Ctrl Pts',(4.0783981912992,0.794772683992985,9.8971189187593));
#57005=CARTESIAN_POINT('Ctrl Pts',(4.15093233607749,1.06847604193477,9.88701418427292));
#57006=CARTESIAN_POINT('Ctrl Pts',(4.17925759836599,1.18514270860049,9.87321409232173));
#57007=CARTESIAN_POINT('Ctrl Pts',(4.2045107793234,1.29999999998779,9.84998787356118));
#57008=CARTESIAN_POINT('Ctrl Pts',(4.07325465779156,-1.29999999998895,10.0516075489123));
#57009=CARTESIAN_POINT('Ctrl Pts',(4.05537342858916,-1.18514270860128,10.0623313519078));
#57010=CARTESIAN_POINT('Ctrl Pts',(4.03620456978458,-1.06847604193516,10.0615309202005));
#57011=CARTESIAN_POINT('Ctrl Pts',(3.98894598925863,-0.794772683992982,
10.0330584752522));
#57012=CARTESIAN_POINT('Ctrl Pts',(3.94804077865574,-0.636309800088896,
9.97500564443789));
#57013=CARTESIAN_POINT('Ctrl Pts',(3.91006897550654,-0.319434907273996,
9.9090197877421));
#57014=CARTESIAN_POINT('Ctrl Pts',(3.89091373212821,-0.158333333331765,
9.86381201354059));
#57015=CARTESIAN_POINT('Ctrl Pts',(3.90868748732497,0.158333333331766,9.8377033636354));
#57016=CARTESIAN_POINT('Ctrl Pts',(3.94612284879179,0.319434907274004,9.85607234905735));
#57017=CARTESIAN_POINT('Ctrl Pts',(4.01926708677286,0.636309800088906,9.87036400609676));
#57018=CARTESIAN_POINT('Ctrl Pts',(4.08014064074479,0.794772683992971,9.9002641596514));
#57019=CARTESIAN_POINT('Ctrl Pts',(4.15245205032798,1.06847604193475,9.88972747831268));
#57020=CARTESIAN_POINT('Ctrl Pts',(4.18062907000966,1.18514270860047,9.87562707692026));
#57021=CARTESIAN_POINT('Ctrl Pts',(4.20568217956622,1.29999999998777,9.85198721306445));
#57022=CARTESIAN_POINT('Ctrl Pts',(4.07390722870856,-1.29999999998894,10.0530598988483));
#57023=CARTESIAN_POINT('Ctrl Pts',(4.05614258391025,-1.18514270860127,10.0640745886785));
#57024=CARTESIAN_POINT('Ctrl Pts',(4.03706538461292,-1.06847604193515,10.0634809773882));
#57025=CARTESIAN_POINT('Ctrl Pts',(3.98996097438718,-0.794772683992973,
10.0352921187352));
#57026=CARTESIAN_POINT('Ctrl Pts',(3.94907237020012,-0.636309800088889,
9.97714992134904));
#57027=CARTESIAN_POINT('Ctrl Pts',(3.91115931189588,-0.319434907273992,
9.91112104424304));
#57028=CARTESIAN_POINT('Ctrl Pts',(3.89200639945563,-0.158333333331763,
9.86577758659279));
#57029=CARTESIAN_POINT('Ctrl Pts',(3.9098085767008,0.158333333331765,9.8396414179453));
#57030=CARTESIAN_POINT('Ctrl Pts',(3.94727573788883,0.319434907274,9.85811195946995));
#57031=CARTESIAN_POINT('Ctrl Pts',(4.02040749666177,0.636309800088899,9.87240404447289));
#57032=CARTESIAN_POINT('Ctrl Pts',(4.08128868412945,0.794772683992962,9.90237530578483));
#57033=CARTESIAN_POINT('Ctrl Pts',(4.15345377064241,1.06847604193474,9.89154835775589));
#57034=CARTESIAN_POINT('Ctrl Pts',(4.18153497571546,1.18514270860046,9.87724452862485));
#57035=CARTESIAN_POINT('Ctrl Pts',(4.20645979389006,1.29999999998775,9.85332345498654));
#57036=CARTESIAN_POINT('Ctrl Pts',(4.07472883611629,-1.2999999999889,10.0548694806607));
#57037=CARTESIAN_POINT('Ctrl Pts',(4.05711645448729,-1.18514270860124,10.066241372499));
#57038=CARTESIAN_POINT('Ctrl Pts',(4.03815646541594,-1.06847604193512,10.0659036912195));
#57039=CARTESIAN_POINT('Ctrl Pts',(3.99124185494869,-0.794772683992953,
10.0380721235173));
#57040=CARTESIAN_POINT('Ctrl Pts',(3.95035207494585,-0.636309800088874,
9.9798396914538));
#57041=CARTESIAN_POINT('Ctrl Pts',(3.9125096217793,-0.319434907273985,9.91375966696656));
#57042=CARTESIAN_POINT('Ctrl Pts',(3.89337589264243,-0.158333333331759,
9.86823033469163));
#57043=CARTESIAN_POINT('Ctrl Pts',(3.91121402898208,0.158333333331761,9.84205954147312));
#57044=CARTESIAN_POINT('Ctrl Pts',(3.94871139904287,0.319434907273992,9.86066680643706));
#57045=CARTESIAN_POINT('Ctrl Pts',(4.02181843654429,0.636309800088883,9.87496910073066));
#57046=CARTESIAN_POINT('Ctrl Pts',(4.08269805463338,0.794772683992942,9.90504125970458));
#57047=CARTESIAN_POINT('Ctrl Pts',(4.15468415069764,1.06847604193471,9.89384734872794));
#57048=CARTESIAN_POINT('Ctrl Pts',(4.18265120271854,1.18514270860043,9.87928324884646));
#57049=CARTESIAN_POINT('Ctrl Pts',(4.20742519312184,1.29999999998772,9.85500047836999));
#57050=CARTESIAN_POINT('Ctrl Pts',(4.07547411574327,-1.29999999998887,10.0564922662393));
#57051=CARTESIAN_POINT('Ctrl Pts',(4.05800529143892,-1.18514270860121,10.0681792184617));
#57052=CARTESIAN_POINT('Ctrl Pts',(4.03915337222251,-1.0684760419351,10.0680693180286));
#57053=CARTESIAN_POINT('Ctrl Pts',(3.99240644158517,-0.794772683992932,
10.0405623364562));
#57054=CARTESIAN_POINT('Ctrl Pts',(3.95149348925175,-0.636309800088857,
9.98227038205354));
#57055=CARTESIAN_POINT('Ctrl Pts',(3.91371116847997,-0.319434907273976,
9.91614756042613));
#57056=CARTESIAN_POINT('Ctrl Pts',(3.89461012291728,-0.158333333331755,
9.87043553006687));
#57057=CARTESIAN_POINT('Ctrl Pts',(3.91248106890848,0.158333333331757,9.84423334416848));
#57058=CARTESIAN_POINT('Ctrl Pts',(3.94999712337104,0.319434907273984,9.86297239204567));
#57059=CARTESIAN_POINT('Ctrl Pts',(4.02307305740497,0.636309800088866,9.87729330475985));
#57060=CARTESIAN_POINT('Ctrl Pts',(4.08393969766434,0.794772683992921,9.90746875231371));
#57061=CARTESIAN_POINT('Ctrl Pts',(4.15576841570156,1.06847604193468,9.89594071535657));
#57062=CARTESIAN_POINT('Ctrl Pts',(4.18363827625216,1.1851427086004,9.88113649555721));
#57063=CARTESIAN_POINT('Ctrl Pts',(4.20828600683132,1.29999999998768,9.85651811600137));
#57064=CARTESIAN_POINT('Ctrl Pts',(4.07597260778046,-1.29999999998886,10.057572446527));
#57065=CARTESIAN_POINT('Ctrl Pts',(4.0586012438042,-1.1851427086012,10.0694676935615));
#57066=CARTESIAN_POINT('Ctrl Pts',(4.03982201553618,-1.06847604193509,10.0695089994242));
#57067=CARTESIAN_POINT('Ctrl Pts',(3.99318579330915,-0.794772683992927,
10.0422194487507));
#57068=CARTESIAN_POINT('Ctrl Pts',(3.95225110097318,-0.636309800088852,
9.98389400970228));
#57069=CARTESIAN_POINT('Ctrl Pts',(3.91450758576179,-0.319434907273974,
9.91774390726409));
#57070=CARTESIAN_POINT('Ctrl Pts',(3.89543222585983,-0.158333333331754,
9.87190619314399));
#57071=CARTESIAN_POINT('Ctrl Pts',(3.91332514424889,0.158333333331756,9.84568304911986));
#57072=CARTESIAN_POINT('Ctrl Pts',(3.95085174404416,0.319434907273981,9.86451192091105));
#57073=CARTESIAN_POINT('Ctrl Pts',(4.0239045849775,0.636309800088861,9.87884777797579));
#57074=CARTESIAN_POINT('Ctrl Pts',(4.08475912371384,0.794772683992915,9.90909579798807));
#57075=CARTESIAN_POINT('Ctrl Pts',(4.1564839138414,1.06847604193467,9.89734401763171));
#57076=CARTESIAN_POINT('Ctrl Pts',(4.18429053005257,1.18514270860039,9.8823780981469));
#57077=CARTESIAN_POINT('Ctrl Pts',(4.20885675849407,1.29999999998768,9.85753316944717));
#57078=CARTESIAN_POINT('Ctrl Pts',(4.07622210167524,-1.29999999998886,10.0581122784215));
#57079=CARTESIAN_POINT('Ctrl Pts',(4.05889975895958,-1.1851427086012,10.0701113802034));
#57080=CARTESIAN_POINT('Ctrl Pts',(4.04015697781387,-1.06847604193509,10.0702281847756));
#57081=CARTESIAN_POINT('Ctrl Pts',(3.99357590695571,-0.794772683992926,
10.0430475431045));
#57082=CARTESIAN_POINT('Ctrl Pts',(3.95262928543621,-0.636309800088851,
9.984706405372));
#57083=CARTESIAN_POINT('Ctrl Pts',(3.91490488517323,-0.319434907273973,
9.91854294778371));
#57084=CARTESIAN_POINT('Ctrl Pts',(3.89584289171174,-0.158333333331753,
9.87264187569554));
#57085=CARTESIAN_POINT('Ctrl Pts',(3.91374682290024,0.158333333331755,9.84640823972977));
#57086=CARTESIAN_POINT('Ctrl Pts',(3.95127853286302,0.319434907273981,9.86528219251662));
#57087=CARTESIAN_POINT('Ctrl Pts',(4.02431948788694,0.636309800088861,9.87962589094895));
#57088=CARTESIAN_POINT('Ctrl Pts',(4.08516735885034,0.794772683992914,9.90991085607916));
#57089=CARTESIAN_POINT('Ctrl Pts',(4.15684031488721,1.06847604193467,9.89804708400454));
#57090=CARTESIAN_POINT('Ctrl Pts',(4.18461554710164,1.18514270860039,9.88300007185356));
#57091=CARTESIAN_POINT('Ctrl Pts',(4.20914144460686,1.29999999998767,9.85804143488663));
#57092=CARTESIAN_POINT('Ctrl Pts',(4.07643021999955,-1.29999999998885,10.0585619219469));
#57093=CARTESIAN_POINT('Ctrl Pts',(4.05914893020202,-1.18514270860119,10.0706473663804));
#57094=CARTESIAN_POINT('Ctrl Pts',(4.04043658915353,-1.06847604193508,10.0708270173388));
#57095=CARTESIAN_POINT('Ctrl Pts',(3.99390132327006,-0.794772683992922,
10.0437372823191));
#57096=CARTESIAN_POINT('Ctrl Pts',(3.95294397013955,-0.636309800088849,
9.98538384510396));
#57097=CARTESIAN_POINT('Ctrl Pts',(3.91523534848828,-0.319434907273972,
9.91920940614504));
#57098=CARTESIAN_POINT('Ctrl Pts',(3.89618502062803,-0.158333333331753,
9.87325500922776));
#57099=CARTESIAN_POINT('Ctrl Pts',(3.91409812835474,0.158333333331755,9.84701264030445));
#57100=CARTESIAN_POINT('Ctrl Pts',(3.95163379350589,0.31943490727398,9.86592447240053));
#57101=CARTESIAN_POINT('Ctrl Pts',(4.02466453538962,0.636309800088858,9.8802750368039));
#57102=CARTESIAN_POINT('Ctrl Pts',(4.08550645564106,0.794772683992911,9.91059121737707));
#57103=CARTESIAN_POINT('Ctrl Pts',(4.15713636041993,1.06847604193467,9.8986339757222));
#57104=CARTESIAN_POINT('Ctrl Pts',(4.18488564025264,1.18514270860038,9.8835191770097));
#57105=CARTESIAN_POINT('Ctrl Pts',(4.20937826828882,1.29999999998767,9.85846542643763));
#57106=CARTESIAN_POINT('Ctrl Pts',(4.0765759208084,-1.29999999998886,10.0588766470101));
#57107=CARTESIAN_POINT('Ctrl Pts',(4.05932344329039,-1.1851427086012,10.0710224510075));
#57108=CARTESIAN_POINT('Ctrl Pts',(4.04063243052271,-1.06847604193509,10.071246070143));
#57109=CARTESIAN_POINT('Ctrl Pts',(3.99412914770043,-0.794772683992925,
10.0442200430249));
#57110=CARTESIAN_POINT('Ctrl Pts',(3.95316401095664,-0.63630980008885,9.98585826277267));
#57111=CARTESIAN_POINT('Ctrl Pts',(3.91546623180345,-0.319434907273973,
9.91967634285258));
#57112=CARTESIAN_POINT('Ctrl Pts',(3.89642395968892,-0.158333333331753,
9.87368474052135));
#57113=CARTESIAN_POINT('Ctrl Pts',(3.91434351989717,0.158333333331755,9.84743623607467));
#57114=CARTESIAN_POINT('Ctrl Pts',(3.95188221366601,0.319434907273981,9.86637431922968));
#57115=CARTESIAN_POINT('Ctrl Pts',(4.02490582148206,0.63630980008886,9.88072968258797));
#57116=CARTESIAN_POINT('Ctrl Pts',(4.08574333395374,0.794772683992913,9.91106796282547));
#57117=CARTESIAN_POINT('Ctrl Pts',(4.15734306508055,1.06847604193467,9.89904534991704));
#57118=CARTESIAN_POINT('Ctrl Pts',(4.18507419912739,1.18514270860039,9.88388309052645));
#57119=CARTESIAN_POINT('Ctrl Pts',(4.20954359664774,1.29999999998767,9.85876271539161));
#57120=CARTESIAN_POINT('Ctrl Pts',(4.07665927356971,-1.29999999998885,10.0590563943251));
#57121=CARTESIAN_POINT('Ctrl Pts',(4.0594232795469,-1.18514270860119,10.0712366737565));
#57122=CARTESIAN_POINT('Ctrl Pts',(4.04074446090144,-1.06847604193508,10.0714854138474));
#57123=CARTESIAN_POINT('Ctrl Pts',(3.99425943963133,-0.79477268399292,10.0444958104446));
#57124=CARTESIAN_POINT('Ctrl Pts',(3.95328971468093,-0.636309800088847,
9.98612940636483));
#57125=CARTESIAN_POINT('Ctrl Pts',(3.91559824531298,-0.319434907273971,
9.91994309394241));
#57126=CARTESIAN_POINT('Ctrl Pts',(3.89656095268153,-0.158333333331752,
9.87392984326917));
#57127=CARTESIAN_POINT('Ctrl Pts',(3.91448416414649,0.158333333331754,9.84767786770841));
#57128=CARTESIAN_POINT('Ctrl Pts',(3.95202417120306,0.319434907273979,9.86663137801879));
#57129=CARTESIAN_POINT('Ctrl Pts',(4.02504352600686,0.636309800088856,9.88098966516978));
#57130=CARTESIAN_POINT('Ctrl Pts',(4.08587855467762,0.794772683992909,9.91134055056134));
#57131=CARTESIAN_POINT('Ctrl Pts',(4.15746116232731,1.06847604193466,9.89928044564848));
#57132=CARTESIAN_POINT('Ctrl Pts',(4.18518201547413,1.18514270860038,9.88409096295741));
#57133=CARTESIAN_POINT('Ctrl Pts',(4.20963826331322,1.29999999998766,9.8589323701211));
#57134=CARTESIAN_POINT('Ctrl Pts',(4.08202434161241,-1.29999999998988,10.0706609615285));
#57135=CARTESIAN_POINT('Ctrl Pts',(4.06585221433066,-1.18514270860213,10.0850635262272));
#57136=CARTESIAN_POINT('Ctrl Pts',(4.04795985258241,-1.06847604193593,10.0869320838313));
#57137=CARTESIAN_POINT('Ctrl Pts',(4.00265083184004,-0.794772683993552,
10.0622927618923));
#57138=CARTESIAN_POINT('Ctrl Pts',(3.96139094918821,-0.636309800089352,
10.0036217614018));
#57139=CARTESIAN_POINT('Ctrl Pts',(3.92408339830617,-0.319434907274224,
9.93717581140978));
#57140=CARTESIAN_POINT('Ctrl Pts',(3.90531558877303,-0.158333333331878,
9.88981993991924));
#57141=CARTESIAN_POINT('Ctrl Pts',(3.92347994603432,0.15833333333188,9.86333885041616));
#57142=CARTESIAN_POINT('Ctrl Pts',(3.96116781285423,0.319434907274233,9.88322291920571));
#57143=CARTESIAN_POINT('Ctrl Pts',(4.03393554506074,0.636309800089361,9.89774680803204));
#57144=CARTESIAN_POINT('Ctrl Pts',(4.09459577648591,0.794772683993539,9.92892413859132));
#57145=CARTESIAN_POINT('Ctrl Pts',(4.1650575688749,1.06847604193551,9.91446533303684));
#57146=CARTESIAN_POINT('Ctrl Pts',(4.1921052148016,1.18514270860132,9.89753237258154));
#57147=CARTESIAN_POINT('Ctrl Pts',(4.2157002075965,1.2999999999887,9.86992513284393));
#57148=CARTESIAN_POINT('Ctrl Pts',(4.09192286002323,-1.29999999999578,10.0944502050367));
#57149=CARTESIAN_POINT('Ctrl Pts',(4.07727446967434,-1.18514270860751,10.1138220103929));
#57150=CARTESIAN_POINT('Ctrl Pts',(4.06064929695951,-1.06847604194078,10.1191840229114));
#57151=CARTESIAN_POINT('Ctrl Pts',(4.01767505941472,-0.79477268399716,10.0992059203913));
#57152=CARTESIAN_POINT('Ctrl Pts',(3.9771938286849,-0.636309800092241,10.0386265544923));
#57153=CARTESIAN_POINT('Ctrl Pts',(3.94096363261905,-0.319434907275675,
9.97138572994343));
#57154=CARTESIAN_POINT('Ctrl Pts',(3.92206607032949,-0.158333333332597,
9.92205052577164));
#57155=CARTESIAN_POINT('Ctrl Pts',(3.94073450593346,0.158333333332599,9.89509432820567));
#57156=CARTESIAN_POINT('Ctrl Pts',(3.97883278048616,0.319434907275683,9.91670040028087));
#57157=CARTESIAN_POINT('Ctrl Pts',(4.0520050264758,0.63630980009225,9.93060780328429));
#57158=CARTESIAN_POINT('Ctrl Pts',(4.11428870108699,0.794772683997148,9.96133867191485));
#57159=CARTESIAN_POINT('Ctrl Pts',(4.18211124466442,1.06847604194036,9.94259844987382));
#57160=CARTESIAN_POINT('Ctrl Pts',(4.2070799298394,1.1851427086067,9.92301686204623));
#57161=CARTESIAN_POINT('Ctrl Pts',(4.22765943414761,1.2999999999946,9.89196563411893));
#57162=CARTESIAN_POINT('Ctrl Pts',(4.1021184432181,-1.30000000000182,10.1178254069371));
#57163=CARTESIAN_POINT('Ctrl Pts',(4.08911206630516,-1.18514270861302,10.1420166380803));
#57164=CARTESIAN_POINT('Ctrl Pts',(4.07378763145368,-1.06847604194574,10.1508156013653));
#57165=CARTESIAN_POINT('Ctrl Pts',(4.03302994374026,-0.794772684000851,
10.1355837488154));
#57166=CARTESIAN_POINT('Ctrl Pts',(3.99292720807675,-0.636309800095197,
10.073501568554));
#57167=CARTESIAN_POINT('Ctrl Pts',(3.95743985349657,-0.319434907277159,
10.0058026346109));
#57168=CARTESIAN_POINT('Ctrl Pts',(3.93821605201261,-0.158333333333332,
9.95469786326921));
#57169=CARTESIAN_POINT('Ctrl Pts',(3.95736019033645,0.158333333333334,9.92730205443344));
#57170=CARTESIAN_POINT('Ctrl Pts',(3.99657264201183,0.319434907277167,9.94990558494987));
#57171=CARTESIAN_POINT('Ctrl Pts',(4.06933501806659,0.636309800095206,9.964052914227));
#57172=CARTESIAN_POINT('Ctrl Pts',(4.13043955711106,0.79477268400084,9.99727883158207));
#57173=CARTESIAN_POINT('Ctrl Pts',(4.1962791527049,1.06847604194533,9.97354224444612));
#57174=CARTESIAN_POINT('Ctrl Pts',(4.22022222287693,1.18514270861221,9.9501892474666));
#57175=CARTESIAN_POINT('Ctrl Pts',(4.23960884188585,1.30000000000064,9.91375794255148));
#57176=CARTESIAN_POINT('Ctrl Pts',(4.10682630354988,-1.30000000000182,10.1298904394961));
#57177=CARTESIAN_POINT('Ctrl Pts',(4.09477284803666,-1.18514270861302,10.1563511401478));
#57178=CARTESIAN_POINT('Ctrl Pts',(4.08016499765835,-1.06847604194574,10.1667952068529));
#57179=CARTESIAN_POINT('Ctrl Pts',(4.04051677785084,-0.794772684000851,
10.1539214617366));
#57180=CARTESIAN_POINT('Ctrl Pts',(4.00023280952129,-0.636309800095197,
10.0914459396343));
#57181=CARTESIAN_POINT('Ctrl Pts',(3.96518266532825,-0.319434907277159,
10.0234576048956));
#57182=CARTESIAN_POINT('Ctrl Pts',(3.94621238249089,-0.158333333333332,
9.97107548348332));
#57183=CARTESIAN_POINT('Ctrl Pts',(3.96570274858202,0.158333333333334,9.9433620243731));
#57184=CARTESIAN_POINT('Ctrl Pts',(4.00511469268082,0.319434907277167,9.96682083809137));
#57185=CARTESIAN_POINT('Ctrl Pts',(4.07792758948219,0.636309800095206,9.980823226511));
#57186=CARTESIAN_POINT('Ctrl Pts',(4.13939176391744,0.79477268400084,10.0143022156935));
#57187=CARTESIAN_POINT('Ctrl Pts',(4.20407556081207,1.06847604194533,9.98826899902637));
#57188=CARTESIAN_POINT('Ctrl Pts',(4.22718893277723,1.18514270861221,9.96338122303606));
#57189=CARTESIAN_POINT('Ctrl Pts',(4.24541645780274,1.30000000000064,9.92487448592493));
#57190=CARTESIAN_POINT('',(4.17590025661761,1.2,9.85788582275105));
#57191=CARTESIAN_POINT('Ctrl Pts',(4.1759002566176,1.2,9.85788582275105));
#57192=CARTESIAN_POINT('Ctrl Pts',(4.16896082769767,1.2168198732892,9.83746357236339));
#57193=CARTESIAN_POINT('Ctrl Pts',(4.16291248161029,1.23318519494961,9.81637367715788));
#57194=CARTESIAN_POINT('Ctrl Pts',(4.14915525508964,1.26588873502216,9.77666804147682));
#57195=CARTESIAN_POINT('Ctrl Pts',(4.14279328726094,1.28160640282059,9.75708360059621));
#57196=CARTESIAN_POINT('Ctrl Pts',(4.13532454217556,1.29842424618538,9.7371004320105));
#57197=CARTESIAN_POINT('Ctrl Pts',(4.1349729583003,1.29921220855233,9.73616663537405));
#57198=CARTESIAN_POINT('Ctrl Pts',(4.13461958894908,1.29999999999519,9.73523585780992));
#57199=CARTESIAN_POINT('',(4.08975875486489,0.653834841416977,9.98861494773806));
#57200=CARTESIAN_POINT('Ctrl Pts',(4.08975875488793,0.653834841416293,9.98861494775051));
#57201=CARTESIAN_POINT('Ctrl Pts',(4.09893898656859,0.71805776923962,9.97515129873787));
#57202=CARTESIAN_POINT('Ctrl Pts',(4.10629442287966,0.76350939074164,9.96425948435249));
#57203=CARTESIAN_POINT('Ctrl Pts',(4.13517026026942,0.949775842008898,9.92104750271804));
#57204=CARTESIAN_POINT('Ctrl Pts',(4.1507016403391,1.04906307388899,9.89747627742111));
#57205=CARTESIAN_POINT('Ctrl Pts',(4.1759002566176,1.2,9.85788582275105));
#57206=CARTESIAN_POINT('',(4.00955034077163,-0.653834841531101,10.1027583545342));
#57207=CARTESIAN_POINT('Ctrl Pts',(4.00955034077162,-0.653834841531098,
10.1027583545342));
#57208=CARTESIAN_POINT('Ctrl Pts',(3.9892268254758,-0.575795237079985,10.0663779392223));
#57209=CARTESIAN_POINT('Ctrl Pts',(3.97279425521263,-0.493919038588913,
10.0355515093655));
#57210=CARTESIAN_POINT('Ctrl Pts',(3.95122422996677,-0.338198219021382,
9.98967393256177));
#57211=CARTESIAN_POINT('Ctrl Pts',(3.94476187062674,-0.265711864048123,
9.97296500528629));
#57212=CARTESIAN_POINT('Ctrl Pts',(3.94008040260285,-0.129741091012596,
9.9490073533817));
#57213=CARTESIAN_POINT('Ctrl Pts',(3.94077929528986,-0.066641501326757,
9.94075353629532));
#57214=CARTESIAN_POINT('Ctrl Pts',(3.9481430854642,0.0595501401552381,9.92962711164072));
#57215=CARTESIAN_POINT('Ctrl Pts',(3.95484997220342,0.122796625322549,9.92666046019834));
#57216=CARTESIAN_POINT('Ctrl Pts',(3.97559498700695,0.260149217292054,9.92672328284864));
#57217=CARTESIAN_POINT('Ctrl Pts',(3.99074823399124,0.33394912587413,9.93094211655924));
#57218=CARTESIAN_POINT('Ctrl Pts',(4.03134493898561,0.491142174428259,9.94994913888734));
#57219=CARTESIAN_POINT('Ctrl Pts',(4.05829569965353,0.574254018778612,9.96634212921925));
#57220=CARTESIAN_POINT('Ctrl Pts',(4.08975875486384,0.653834841428668,9.98861494769777));
#57221=CARTESIAN_POINT('',(4.05146214282868,-1.2,10.0439680914571));
#57222=CARTESIAN_POINT('Ctrl Pts',(4.05146214282868,-1.2,10.0439680914571));
#57223=CARTESIAN_POINT('Ctrl Pts',(4.04427281420881,-1.1339556629759,10.0542098704782));
#57224=CARTESIAN_POINT('Ctrl Pts',(4.03488407820185,-1.03841658953484,10.067500381683));
#57225=CARTESIAN_POINT('Ctrl Pts',(4.0163549400073,-0.795343226740802,10.0933659085415));
#57226=CARTESIAN_POINT('Ctrl Pts',(4.01340110853449,-0.741643831139491,
10.0974393285217));
#57227=CARTESIAN_POINT('Ctrl Pts',(4.00955034077162,-0.653834841531102,
10.1027583545342));
#57228=CARTESIAN_POINT('Ctrl Pts',(4.01179369694817,-1.29999999999639,9.9254378241233));
#57229=CARTESIAN_POINT('Ctrl Pts',(4.01906436001224,-1.28293734428946,9.945099061467));
#57230=CARTESIAN_POINT('Ctrl Pts',(4.02556213161071,-1.26616775796805,9.96528846164041));
#57231=CARTESIAN_POINT('Ctrl Pts',(4.03670033314328,-1.23890235909598,9.99713900241556));
#57232=CARTESIAN_POINT('Ctrl Pts',(4.04542626944918,-1.21716802518332,10.0226852886214));
#57233=CARTESIAN_POINT('Ctrl Pts',(4.05146214282868,-1.2,10.0439680914571));
#57234=CARTESIAN_POINT('Origin',(0.,1.25,7.2));
#57235=CARTESIAN_POINT('Origin',(0.,1.2,7.2));
#57236=CARTESIAN_POINT('Origin',(0.,0.92691742076555,7.2));
#57237=CARTESIAN_POINT('Origin',(0.,0.653834841531101,7.2));
#57238=CARTESIAN_POINT('Origin',(0.,0.,7.2));
#57239=CARTESIAN_POINT('Origin',(0.,-0.653834841531101,7.2));
#57240=CARTESIAN_POINT('Origin',(0.,-0.926917420765551,7.2));
#57241=CARTESIAN_POINT('Origin',(0.,-1.2,7.2));
#57242=CARTESIAN_POINT('Origin',(0.,-1.25,7.2));
#57243=CARTESIAN_POINT('Ctrl Pts',(3.90341546958847,-1.30000000000005,10.3955984628936));
#57244=CARTESIAN_POINT('Ctrl Pts',(3.93440493784208,-1.18514270861181,10.3663638202781));
#57245=CARTESIAN_POINT('Ctrl Pts',(3.95093219463971,-1.06847604194513,10.3366909515245));
#57246=CARTESIAN_POINT('Ctrl Pts',(3.9557028624898,-0.794772684000851,10.2671282986208));
#57247=CARTESIAN_POINT('Ctrl Pts',(3.90486897722008,-0.636309800095197,
10.2190179716147));
#57248=CARTESIAN_POINT('Ctrl Pts',(3.86905149194761,-0.319434907277159,
10.1540957676241));
#57249=CARTESIAN_POINT('Ctrl Pts',(3.83456187378936,-0.158333333333332,
10.1238619534767));
#57250=CARTESIAN_POINT('Ctrl Pts',(3.85489608531651,0.158333333333334,10.0967615839629));
#57251=CARTESIAN_POINT('Ctrl Pts',(3.9105765830082,0.319434907277167,10.0986164293539));
#57252=CARTESIAN_POINT('Ctrl Pts',(3.986068422003,0.636309800095206,10.1109415465311));
#57253=CARTESIAN_POINT('Ctrl Pts',(4.05793460521832,0.79477268400084,10.1299478790481));
#57254=CARTESIAN_POINT('Ctrl Pts',(4.08243023811811,1.0684760419458,10.1636773708336));
#57255=CARTESIAN_POINT('Ctrl Pts',(4.07701141444102,1.18514270861313,10.1807976562281));
#57256=CARTESIAN_POINT('Ctrl Pts',(4.05557051525715,1.300000000002,10.200437979824));
#57257=CARTESIAN_POINT('Ctrl Pts',(3.8972319130928,-1.30000000000005,10.3945543778395));
#57258=CARTESIAN_POINT('Ctrl Pts',(3.92705536482917,-1.18514270861181,10.3650892251986));
#57259=CARTESIAN_POINT('Ctrl Pts',(3.9427245954191,-1.06847604194513,10.3352589479046));
#57260=CARTESIAN_POINT('Ctrl Pts',(3.94622457031017,-0.794772684000851,
10.2655015288375));
#57261=CARTESIAN_POINT('Ctrl Pts',(3.89556659455229,-0.636309800095197,
10.2175231168598));
#57262=CARTESIAN_POINT('Ctrl Pts',(3.85968799168501,-0.319434907277159,
10.1526473315009));
#57263=CARTESIAN_POINT('Ctrl Pts',(3.82563590813615,-0.158333333333332,
10.1223762331194));
#57264=CARTESIAN_POINT('Ctrl Pts',(3.84587256311358,0.158333333333334,10.0954895843591));
#57265=CARTESIAN_POINT('Ctrl Pts',(3.90098481553906,0.319434907277167,10.0976623464721));
#57266=CARTESIAN_POINT('Ctrl Pts',(3.97640658899012,0.636309800095206,10.1102400844189));
#57267=CARTESIAN_POINT('Ctrl Pts',(4.04805772503971,0.79477268400084,10.1292210103236));
#57268=CARTESIAN_POINT('Ctrl Pts',(4.07384612687898,1.0684760419458,10.1631137378143));
#57269=CARTESIAN_POINT('Ctrl Pts',(4.06932031476021,1.18514270861313,10.1803205969217));
#57270=CARTESIAN_POINT('Ctrl Pts',(4.0491058469209,1.300000000002,10.200063409255));
#57271=CARTESIAN_POINT('Ctrl Pts',(3.88471837690218,-1.29999999999985,10.3927059310096));
#57272=CARTESIAN_POINT('Ctrl Pts',(3.91227329929968,-1.18514270861163,10.3626773220286));
#57273=CARTESIAN_POINT('Ctrl Pts',(3.92628138935286,-1.06847604194497,10.332439936458));
#57274=CARTESIAN_POINT('Ctrl Pts',(3.92734698693467,-0.79477268400073,10.2621032111342));
#57275=CARTESIAN_POINT('Ctrl Pts',(3.8771691524999,-0.636309800095101,10.2141284835984));
#57276=CARTESIAN_POINT('Ctrl Pts',(3.84106775360212,-0.319434907277111,
10.1495363480085));
#57277=CARTESIAN_POINT('Ctrl Pts',(3.80755160262496,-0.158333333333308,
10.1198406743019));
#57278=CARTESIAN_POINT('Ctrl Pts',(3.82753192323713,0.15833333333331,10.0935016391188));
#57279=CARTESIAN_POINT('Ctrl Pts',(3.88173624342239,0.319434907277118,10.0958780309468));
#57280=CARTESIAN_POINT('Ctrl Pts',(3.95709428015321,0.63630980009511,10.1088161402808));
#57281=CARTESIAN_POINT('Ctrl Pts',(4.02825982105977,0.794772684000721,10.1278489843642));
#57282=CARTESIAN_POINT('Ctrl Pts',(4.05663569066553,1.06847604194564,10.1620627825047));
#57283=CARTESIAN_POINT('Ctrl Pts',(4.05390038764762,1.18514270861295,10.1794336337835));
#57284=CARTESIAN_POINT('Ctrl Pts',(4.03614691908903,1.30000000000181,10.1993654508722));
#57285=CARTESIAN_POINT('Ctrl Pts',(3.86050496345744,-1.29999999999983,10.3876974682567));
#57286=CARTESIAN_POINT('Ctrl Pts',(3.88261846239695,-1.18514270861162,10.3580947882787));
#57287=CARTESIAN_POINT('Ctrl Pts',(3.89273073077964,-1.06847604194496,10.3280188949586));
#57288=CARTESIAN_POINT('Ctrl Pts',(3.88836685027176,-0.79477268400072,10.257444347241));
#57289=CARTESIAN_POINT('Ctrl Pts',(3.83991593350838,-0.636309800095094,
10.2081207376447));
#57290=CARTESIAN_POINT('Ctrl Pts',(3.80396032762788,-0.319434907277108,
10.1429732908664));
#57291=CARTESIAN_POINT('Ctrl Pts',(3.77207195551128,-0.158333333333307,
10.113390850971));
#57292=CARTESIAN_POINT('Ctrl Pts',(3.79187459039628,0.158333333333309,10.0874431279985));
#57293=CARTESIAN_POINT('Ctrl Pts',(3.84418233538711,0.319434907277116,10.0902375668533));
#57294=CARTESIAN_POINT('Ctrl Pts',(3.91921823181388,0.636309800095104,10.1042429561577));
#57295=CARTESIAN_POINT('Ctrl Pts',(3.98890458788481,0.794772684000714,10.1244479769042));
#57296=CARTESIAN_POINT('Ctrl Pts',(4.02247474477858,1.06847604194563,10.1593341744568));
#57297=CARTESIAN_POINT('Ctrl Pts',(4.02345098386902,1.18514270861294,10.176811067091));
#57298=CARTESIAN_POINT('Ctrl Pts',(4.01087218502744,1.30000000000179,10.1966639101));
#57299=CARTESIAN_POINT('Ctrl Pts',(3.84178186561024,-1.29999999999939,10.3843671205557));
#57300=CARTESIAN_POINT('Ctrl Pts',(3.86080495295138,-1.18514270861122,10.3532467534984));
#57301=CARTESIAN_POINT('Ctrl Pts',(3.86858527719493,-1.06847604194459,10.3221965910117));
#57302=CARTESIAN_POINT('Ctrl Pts',(3.86058635078354,-0.794772684000451,
10.2506266907062));
#57303=CARTESIAN_POINT('Ctrl Pts',(3.81212911135781,-0.636309800094877,
10.2026892754764));
#57304=CARTESIAN_POINT('Ctrl Pts',(3.77575940271681,-0.319434907276998,
10.1380984101569));
#57305=CARTESIAN_POINT('Ctrl Pts',(3.74512432345125,-0.158333333333252,
10.1085544874522));
#57306=CARTESIAN_POINT('Ctrl Pts',(3.76466940587767,0.158333333333255,10.0831483511506));
#57307=CARTESIAN_POINT('Ctrl Pts',(3.81555764025485,0.319434907277006,10.0862626912517));
#57308=CARTESIAN_POINT('Ctrl Pts',(3.89029698142897,0.636309800094886,10.1011877726536));
#57309=CARTESIAN_POINT('Ctrl Pts',(3.95881995092127,0.79477268400044,10.1223398957364));
#57310=CARTESIAN_POINT('Ctrl Pts',(3.99629237825836,1.06847604194526,10.157799288423));
#57311=CARTESIAN_POINT('Ctrl Pts',(4.00007247219514,1.18514270861254,10.1753757244196));
#57312=CARTESIAN_POINT('Ctrl Pts',(3.99141223476473,1.30000000000135,10.1951795392188));
#57313=CARTESIAN_POINT('Ctrl Pts',(3.82918677459915,-1.29999999999936,10.3819124216719));
#57314=CARTESIAN_POINT('Ctrl Pts',(3.8455386514497,-1.18514270861119,10.350755495859));
#57315=CARTESIAN_POINT('Ctrl Pts',(3.85139900877872,-1.06847604194456,10.3196192408126));
#57316=CARTESIAN_POINT('Ctrl Pts',(3.84070009765322,-0.794772684000428,
10.2477360164746));
#57317=CARTESIAN_POINT('Ctrl Pts',(3.79300134625836,-0.636309800094859,
10.1993514351645));
#57318=CARTESIAN_POINT('Ctrl Pts',(3.75672553111135,-0.31943490727699,10.134439742147));
#57319=CARTESIAN_POINT('Ctrl Pts',(3.72706155916688,-0.158333333333248,
10.1047089972824));
#57320=CARTESIAN_POINT('Ctrl Pts',(3.74646404977274,0.15833333333325,10.0796011966045));
#57321=CARTESIAN_POINT('Ctrl Pts',(3.79611713161317,0.319434907276997,10.0834276162307));
#57322=CARTESIAN_POINT('Ctrl Pts',(3.87071952184266,0.636309800094868,10.0988189902669));
#57323=CARTESIAN_POINT('Ctrl Pts',(3.93885479502108,0.794772684000418,10.1197848490444));
#57324=CARTESIAN_POINT('Ctrl Pts',(3.97898689489694,1.06847604194523,10.155644952634));
#57325=CARTESIAN_POINT('Ctrl Pts',(3.98459288328237,1.18514270861251,10.173473174971));
#57326=CARTESIAN_POINT('Ctrl Pts',(3.97843316105777,1.30000000000132,10.1936071095487));
#57327=CARTESIAN_POINT('Ctrl Pts',(3.8286151440339,-1.29999999999936,10.3817992007246));
#57328=CARTESIAN_POINT('Ctrl Pts',(3.84484631571692,-1.18514270861119,10.3506392320354));
#57329=CARTESIAN_POINT('Ctrl Pts',(3.85061978962886,-1.06847604194456,10.3194982992646));
#57330=CARTESIAN_POINT('Ctrl Pts',(3.8397982954385,-0.794772684000429,10.2476004916214));
#57331=CARTESIAN_POINT('Ctrl Pts',(3.79213265237141,-0.63630980009486,10.1991981158477));
#57332=CARTESIAN_POINT('Ctrl Pts',(3.75586081820926,-0.31943490727699,10.1342723455195));
#57333=CARTESIAN_POINT('Ctrl Pts',(3.72624169362474,-0.158333333333248,
10.1045317909193));
#57334=CARTESIAN_POINT('Ctrl Pts',(3.74563757775941,0.15833333333325,10.0794377892856));
#57335=CARTESIAN_POINT('Ctrl Pts',(3.79523397063094,0.319434907276997,10.0832975993543));
#57336=CARTESIAN_POINT('Ctrl Pts',(3.86982958656818,0.636309800094869,10.0987112338179));
#57337=CARTESIAN_POINT('Ctrl Pts',(3.93794685561963,0.794772684000419,10.1196693783045));
#57338=CARTESIAN_POINT('Ctrl Pts',(3.97819966709136,1.06847604194523,10.1555480993504));
#57339=CARTESIAN_POINT('Ctrl Pts',(3.98388865979907,1.18514270861251,10.1733877785578));
#57340=CARTESIAN_POINT('Ctrl Pts',(3.97784269464199,1.30000000000132,10.1935365680694));
#57341=CARTESIAN_POINT('Ctrl Pts',(3.82804377053059,-1.29999999999936,10.381685549878));
#57342=CARTESIAN_POINT('Ctrl Pts',(3.844154236367,-1.18514270861119,10.3505225480926));
#57343=CARTESIAN_POINT('Ctrl Pts',(3.84984083038205,-1.06847604194456,10.3193769349447));
#57344=CARTESIAN_POINT('Ctrl Pts',(3.83889677096033,-0.794772684000428,
10.2474645091452));
#57345=CARTESIAN_POINT('Ctrl Pts',(3.79126435532817,-0.636309800094859,
10.1990440997006));
#57346=CARTESIAN_POINT('Ctrl Pts',(3.75499635039537,-0.31943490727699,10.1341045185275));
#57347=CARTESIAN_POINT('Ctrl Pts',(3.72542163358055,-0.158333333333248,
10.104354973886));
#57348=CARTESIAN_POINT('Ctrl Pts',(3.74481096465794,0.15833333333325,10.0792746415237));
#57349=CARTESIAN_POINT('Ctrl Pts',(3.79435128175347,0.319434907276997,10.0831666439978));
#57350=CARTESIAN_POINT('Ctrl Pts',(3.86894013913835,0.636309800094868,10.0986025144048));
#57351=CARTESIAN_POINT('Ctrl Pts',(3.93703879316676,0.794772684000419,10.1195541647746));
#57352=CARTESIAN_POINT('Ctrl Pts',(3.97741223777967,1.06847604194523,10.155451656625));
#57353=CARTESIAN_POINT('Ctrl Pts',(3.9831843006373,1.18514270861251,10.1733026583442));
#57354=CARTESIAN_POINT('Ctrl Pts',(3.97725225816315,1.30000000000132,10.1934659676937));
#57355=CARTESIAN_POINT('Ctrl Pts',(3.82690210090624,-1.29999999999936,10.3814562692382));
#57356=CARTESIAN_POINT('Ctrl Pts',(3.84277195760607,-1.18514270861119,10.3502856909788));
#57357=CARTESIAN_POINT('Ctrl Pts',(3.84828524002961,-1.06847604194457,10.3191298633125));
#57358=CARTESIAN_POINT('Ctrl Pts',(3.83709626695257,-0.794772684000429,
10.2471877455224));
#57359=CARTESIAN_POINT('Ctrl Pts',(3.78952903120354,-0.63630980009486,10.1987335903228));
#57360=CARTESIAN_POINT('Ctrl Pts',(3.75326808760653,-0.31943490727699,10.1337674532044));
#57361=CARTESIAN_POINT('Ctrl Pts',(3.72378212165099,-0.158333333333248,
10.1040000534961));
#57362=CARTESIAN_POINT('Ctrl Pts',(3.74315831541199,0.158333333333251,10.0789470831623));
#57363=CARTESIAN_POINT('Ctrl Pts',(3.79258701178728,0.319434907276997,10.0829024027525));
#57364=CARTESIAN_POINT('Ctrl Pts',(3.86716187256129,0.636309800094869,10.0983836951478));
#57365=CARTESIAN_POINT('Ctrl Pts',(3.93522189720306,0.79477268400042,10.1193251494811));
#57366=CARTESIAN_POINT('Ctrl Pts',(3.97583634524737,1.06847604194523,10.155260735818));
#57367=CARTESIAN_POINT('Ctrl Pts',(3.98177469585523,1.18514270861251,10.173134107549));
#57368=CARTESIAN_POINT('Ctrl Pts',(3.97607090742614,1.30000000000132,10.1933256672303));
#57369=CARTESIAN_POINT('Ctrl Pts',(3.82443325455095,-1.29999999999936,10.3809508004002));
#57370=CARTESIAN_POINT('Ctrl Pts',(3.83978528105836,-1.18514270861119,10.3497573367654));
#57371=CARTESIAN_POINT('Ctrl Pts',(3.84492505588982,-1.06847604194457,10.3185756333572));
#57372=CARTESIAN_POINT('Ctrl Pts',(3.83320661963357,-0.79477268400043,10.2465668290817));
#57373=CARTESIAN_POINT('Ctrl Pts',(3.78577595644831,-0.63630980009486,10.1980479216123));
#57374=CARTESIAN_POINT('Ctrl Pts',(3.74952702321827,-0.31943490727699,10.1330301437214));
#57375=CARTESIAN_POINT('Ctrl Pts',(3.72023070654343,-0.158333333333248,
10.1032290247907));
#57376=CARTESIAN_POINT('Ctrl Pts',(3.73957843869313,0.158333333333251,10.078235079962));
#57377=CARTESIAN_POINT('Ctrl Pts',(3.78877035130657,0.319434907276997,10.0823175948477));
#57378=CARTESIAN_POINT('Ctrl Pts',(3.86331326275209,0.636309800094869,10.0979005853927));
#57379=CARTESIAN_POINT('Ctrl Pts',(3.93128157816105,0.79477268400042,10.1188360067461));
#57380=CARTESIAN_POINT('Ctrl Pts',(3.97241679402589,1.06847604194523,10.1548570128613));
#57381=CARTESIAN_POINT('Ctrl Pts',(3.97871623257295,1.18514270861251,10.1727772922235));
#57382=CARTESIAN_POINT('Ctrl Pts',(3.97350919892911,1.30000000000132,10.1930256921104));
#57383=CARTESIAN_POINT('Ctrl Pts',(3.82065344079858,-1.29999999999937,10.3801385168388));
#57384=CARTESIAN_POINT('Ctrl Pts',(3.83523203439744,-1.18514270861119,10.3488676639844));
#57385=CARTESIAN_POINT('Ctrl Pts',(3.83981066839133,-1.06847604194457,10.3176215936814));
#57386=CARTESIAN_POINT('Ctrl Pts',(3.82728632169733,-0.794772684000434,
10.2454941731782));
#57387=CARTESIAN_POINT('Ctrl Pts',(3.78003649534408,-0.636309800094864,
10.1969280615303));
#57388=CARTESIAN_POINT('Ctrl Pts',(3.74378425590443,-0.319434907276992,
10.1318704540711));
#57389=CARTESIAN_POINT('Ctrl Pts',(3.71476004854344,-0.158333333333249,
10.1020547371762));
#57390=CARTESIAN_POINT('Ctrl Pts',(3.73406460988566,0.158333333333251,10.0771492785743));
#57391=CARTESIAN_POINT('Ctrl Pts',(3.78292725211545,0.319434907276999,10.0813588866284));
#57392=CARTESIAN_POINT('Ctrl Pts',(3.85741403110121,0.636309800094873,10.0971130422566));
#57393=CARTESIAN_POINT('Ctrl Pts',(3.92519231535607,0.794772684000425,10.1181374888045));
#57394=CARTESIAN_POINT('Ctrl Pts',(3.9671225199414,1.06847604194524,10.1543025913043));
#57395=CARTESIAN_POINT('Ctrl Pts',(3.97398362703879,1.18514270861251,10.1722827757587));
#57396=CARTESIAN_POINT('Ctrl Pts',(3.96955580933573,1.30000000000132,10.1925886118444));
#57397=CARTESIAN_POINT('Ctrl Pts',(3.81614245087933,-1.29999999999937,10.3791150120397));
#57398=CARTESIAN_POINT('Ctrl Pts',(3.82983834935375,-1.1851427086112,10.3476691706384));
#57399=CARTESIAN_POINT('Ctrl Pts',(3.83377063915946,-1.06847604194458,10.3162969473966));
#57400=CARTESIAN_POINT('Ctrl Pts',(3.82029912603461,-0.794772684000437,
10.2439909083921));
#57401=CARTESIAN_POINT('Ctrl Pts',(3.77321602696589,-0.636309800094866,
10.1954579000826));
#57402=CARTESIAN_POINT('Ctrl Pts',(3.7369168456406,-0.319434907276993,10.1304313131957));
#57403=CARTESIAN_POINT('Ctrl Pts',(3.7081728540808,-0.15833333333325,10.1006862676617));
#57404=CARTESIAN_POINT('Ctrl Pts',(3.72742496407903,0.158333333333252,10.0758859834643));
#57405=CARTESIAN_POINT('Ctrl Pts',(3.775962962915,0.319434907277,10.0801096387451));
#57406=CARTESIAN_POINT('Ctrl Pts',(3.85037350037145,0.636309800094875,10.0960886735164));
#57407=CARTESIAN_POINT('Ctrl Pts',(3.91783701116371,0.794772684000426,10.1173953048217));
#57408=CARTESIAN_POINT('Ctrl Pts',(3.96070864750431,1.06847604194524,10.1537588347598));
#57409=CARTESIAN_POINT('Ctrl Pts',(3.96825327759921,1.18514270861252,10.1717915915041));
#57410=CARTESIAN_POINT('Ctrl Pts',(3.96478499496778,1.30000000000133,10.192116680284));
#57411=CARTESIAN_POINT('Ctrl Pts',(3.81014719913854,-1.29999999999938,10.3777111866877));
#57412=CARTESIAN_POINT('Ctrl Pts',(3.82270608604597,-1.18514270861121,10.3459599070711));
#57413=CARTESIAN_POINT('Ctrl Pts',(3.82580088545279,-1.06847604194459,10.3143755614268));
#57414=CARTESIAN_POINT('Ctrl Pts',(3.81108655578441,-0.794772684000444,
10.2417950554328));
#57415=CARTESIAN_POINT('Ctrl Pts',(3.76418481193213,-0.636309800094871,
10.1933794802241));
#57416=CARTESIAN_POINT('Ctrl Pts',(3.72779025172961,-0.319434907276995,
10.1284546694874));
#57417=CARTESIAN_POINT('Ctrl Pts',(3.69938415143322,-0.158333333333251,
10.0988725580143));
#57418=CARTESIAN_POINT('Ctrl Pts',(3.71856629006732,0.158333333333253,10.0742101181523));
#57419=CARTESIAN_POINT('Ctrl Pts',(3.76672800780696,0.319434907277003,10.0783396132334));
#57420=CARTESIAN_POINT('Ctrl Pts',(3.84102706820497,0.63630980009488,10.0946383424229));
#57421=CARTESIAN_POINT('Ctrl Pts',(3.90799558118256,0.794772684000434,10.1164728658535));
#57422=CARTESIAN_POINT('Ctrl Pts',(3.95211208871403,1.06847604194525,10.1531224721248));
#57423=CARTESIAN_POINT('Ctrl Pts',(3.96057690181205,1.18514270861253,10.1712079622024));
#57424=CARTESIAN_POINT('Ctrl Pts',(3.95841012657538,1.30000000000134,10.1915146858042));
#57425=CARTESIAN_POINT('Ctrl Pts',(3.80264558611359,-1.29999999999939,10.3759652989145));
#57426=CARTESIAN_POINT('Ctrl Pts',(3.81378061794709,-1.18514270861122,10.3438347634036));
#57427=CARTESIAN_POINT('Ctrl Pts',(3.81583146444968,-1.06847604194459,10.3119786158427));
#57428=CARTESIAN_POINT('Ctrl Pts',(3.79958304474167,-0.794772684000448,
10.2390184332324));
#57429=CARTESIAN_POINT('Ctrl Pts',(3.75294760073062,-0.636309800094874,
10.1906800667924));
#57430=CARTESIAN_POINT('Ctrl Pts',(3.71645495728067,-0.319434907276997,
10.1258446517031));
#57431=CARTESIAN_POINT('Ctrl Pts',(3.68847208962925,-0.158333333333252,
10.0964653215993));
#57432=CARTESIAN_POINT('Ctrl Pts',(3.70755240882307,0.158333333333254,10.0719990818131));
#57433=CARTESIAN_POINT('Ctrl Pts',(3.75520362998421,0.319434907277005,10.0760810388163));
#57434=CARTESIAN_POINT('Ctrl Pts',(3.82936372624179,0.636309800094884,10.0927734438064));
#57435=CARTESIAN_POINT('Ctrl Pts',(3.89577441947964,0.794772684000437,10.115148633787));
#57436=CARTESIAN_POINT('Ctrl Pts',(3.94143070159432,1.06847604194526,10.1521886133447));
#57437=CARTESIAN_POINT('Ctrl Pts',(3.95102321959067,1.18514270861253,10.1703851611552));
#57438=CARTESIAN_POINT('Ctrl Pts',(3.95044534278784,1.30000000000135,10.1907450220921));
#57439=CARTESIAN_POINT('Ctrl Pts',(3.79051760574996,-1.29999999999941,10.3734001477454));
#57440=CARTESIAN_POINT('Ctrl Pts',(3.79917807880938,-1.18514270861123,10.3410116256646));
#57441=CARTESIAN_POINT('Ctrl Pts',(3.79944890201863,-1.06847604194461,10.3089148904893));
#57442=CARTESIAN_POINT('Ctrl Pts',(3.78069278831246,-0.794772684000462,
10.2354390974279));
#57443=CARTESIAN_POINT('Ctrl Pts',(3.73473563294115,-0.636309800094885,
10.1867768390611));
#57444=CARTESIAN_POINT('Ctrl Pts',(3.69834920030187,-0.319434907277002,
10.1216048277028));
#57445=CARTESIAN_POINT('Ctrl Pts',(3.6713374077935,-0.158333333333255,10.0920043628996));
#57446=CARTESIAN_POINT('Ctrl Pts',(3.69026903992965,0.158333333333257,10.0678283520062));
#57447=CARTESIAN_POINT('Ctrl Pts',(3.73671140064775,0.31943490727701,10.0725764750798));
#57448=CARTESIAN_POINT('Ctrl Pts',(3.81064390796835,0.636309800094894,10.089881330195));
#57449=CARTESIAN_POINT('Ctrl Pts',(3.87654066801923,0.79477268400045,10.1123448087573));
#57450=CARTESIAN_POINT('Ctrl Pts',(3.92470370339651,1.06847604194527,10.1499305823319));
#57451=CARTESIAN_POINT('Ctrl Pts',(3.93605571402822,1.18514270861255,10.1684059123361));
#57452=CARTESIAN_POINT('Ctrl Pts',(3.9379117418931,1.30000000000137,10.1890870836542));
#57453=CARTESIAN_POINT('Ctrl Pts',(3.77531269856596,-1.29999999999947,10.3702508598051));
#57454=CARTESIAN_POINT('Ctrl Pts',(3.7808830596038,-1.18514270861129,10.3375282984927));
#57455=CARTESIAN_POINT('Ctrl Pts',(3.77892690458547,-1.06847604194466,10.3051304292443));
#57456=CARTESIAN_POINT('Ctrl Pts',(3.75702003740151,-0.794772684000497,
10.2310349737318));
#57457=CARTESIAN_POINT('Ctrl Pts',(3.71188048972456,-0.636309800094912,
10.1820244175521));
#57458=CARTESIAN_POINT('Ctrl Pts',(3.67559935454688,-0.319434907277015,
10.1164887747854));
#57459=CARTESIAN_POINT('Ctrl Pts',(3.64976156025509,-0.158333333333261,
10.0866994517134));
#57460=CARTESIAN_POINT('Ctrl Pts',(3.66855436893452,0.158333333333263,10.0627999913768));
#57461=CARTESIAN_POINT('Ctrl Pts',(3.71364679734388,0.319434907277024,10.0680628729313));
#57462=CARTESIAN_POINT('Ctrl Pts',(3.78726682550946,0.636309800094921,10.0861941513323));
#57463=CARTESIAN_POINT('Ctrl Pts',(3.85231154121724,0.794772684000484,10.1091939955424));
#57464=CARTESIAN_POINT('Ctrl Pts',(3.90352518701274,1.06847604194532,10.1476179483369));
#57465=CARTESIAN_POINT('Ctrl Pts',(3.91706593765084,1.1851427086126,10.1664548632847));
#57466=CARTESIAN_POINT('Ctrl Pts',(3.9219789493147,1.30000000000142,10.1874963877634));
#57467=CARTESIAN_POINT('Ctrl Pts',(3.75144143449034,-1.29999999999955,10.3644010333803));
#57468=CARTESIAN_POINT('Ctrl Pts',(3.75240741099658,-1.18514270861136,10.3305289846406));
#57469=CARTESIAN_POINT('Ctrl Pts',(3.7471129191241,-1.06847604194473,10.2972421000756));
#57470=CARTESIAN_POINT('Ctrl Pts',(3.72041864938193,-0.79477268400055,10.2216945840175));
#57471=CARTESIAN_POINT('Ctrl Pts',(3.676449916003,-0.636309800094955,10.1723815037641));
#57472=CARTESIAN_POINT('Ctrl Pts',(3.64000955362952,-0.319434907277037,
10.1068397469521));
#57473=CARTESIAN_POINT('Ctrl Pts',(3.61556008210046,-0.158333333333272,
10.0776086571675));
#57474=CARTESIAN_POINT('Ctrl Pts',(3.63383454621419,0.158333333333274,10.0546636777887));
#57475=CARTESIAN_POINT('Ctrl Pts',(3.67672943965919,0.319434907277046,10.0608301121857));
#57476=CARTESIAN_POINT('Ctrl Pts',(3.75004534089352,0.636309800094965,10.0798783695091));
#57477=CARTESIAN_POINT('Ctrl Pts',(3.81422848444124,0.794772684000539,10.1027155580515));
#57478=CARTESIAN_POINT('Ctrl Pts',(3.87050679078574,1.06847604194539,10.1421616302036));
#57479=CARTESIAN_POINT('Ctrl Pts',(3.8875527138798,1.18514270861268,10.1616070485395));
#57480=CARTESIAN_POINT('Ctrl Pts',(3.89728376656809,1.30000000000151,10.1834231421977));
#57481=CARTESIAN_POINT('Ctrl Pts',(3.72739820580732,-1.29999999999965,10.3587858048955));
#57482=CARTESIAN_POINT('Ctrl Pts',(3.72376039659815,-1.18514270861146,10.3237624646455));
#57483=CARTESIAN_POINT('Ctrl Pts',(3.71509786759347,-1.06847604194481,10.2896362036518));
#57484=CARTESIAN_POINT('Ctrl Pts',(3.68347758474028,-0.794772684000613,
10.2128701463635));
#57485=CARTESIAN_POINT('Ctrl Pts',(3.64034334348832,-0.636309800095004,
10.1638240822689));
#57486=CARTESIAN_POINT('Ctrl Pts',(3.60378905924222,-0.319434907277061,
10.0981981455333));
#57487=CARTESIAN_POINT('Ctrl Pts',(3.58098080217359,-0.158333333333283,
10.0691232838899));
#57488=CARTESIAN_POINT('Ctrl Pts',(3.59917771711532,0.158333333333285,10.0463299146732));
#57489=CARTESIAN_POINT('Ctrl Pts',(3.64045609269603,0.319434907277065,10.052281540449));
#57490=CARTESIAN_POINT('Ctrl Pts',(3.71351968645555,0.636309800095008,10.0721509398841));
#57491=CARTESIAN_POINT('Ctrl Pts',(3.77629943079809,0.7947726840006,10.0958594558066));
#57492=CARTESIAN_POINT('Ctrl Pts',(3.83726787830799,1.06847604194547,10.1370353786994));
#57493=CARTESIAN_POINT('Ctrl Pts',(3.85767445872077,1.18514270861277,10.1573602260567));
#57494=CARTESIAN_POINT('Ctrl Pts',(3.87209663772287,1.3000000000016,10.1801863894691));
#57495=CARTESIAN_POINT('Ctrl Pts',(3.70360350260276,-1.29999999999968,10.3527512023952));
#57496=CARTESIAN_POINT('Ctrl Pts',(3.69524543931284,-1.18514270861149,10.3167362009834));
#57497=CARTESIAN_POINT('Ctrl Pts',(3.68324054739408,-1.06847604194484,10.2817005801307));
#57498=CARTESIAN_POINT('Ctrl Pts',(3.64708194181316,-0.794772684000633,
10.2030238521252));
#57499=CARTESIAN_POINT('Ctrl Pts',(3.60585793754741,-0.63630980009502,10.1524461653563));
#57500=CARTESIAN_POINT('Ctrl Pts',(3.5693783489072,-0.319434907277069,10.0864042491589));
#57501=CARTESIAN_POINT('Ctrl Pts',(3.54762896415299,-0.158333333333288,
10.0584464163139));
#57502=CARTESIAN_POINT('Ctrl Pts',(3.56523065483139,0.15833333333329,10.0366788876955));
#57503=CARTESIAN_POINT('Ctrl Pts',(3.60455752023384,0.319434907277076,10.0429968367841));
#57504=CARTESIAN_POINT('Ctrl Pts',(3.67693979951042,0.636309800095027,10.0644398611071));
#57505=CARTESIAN_POINT('Ctrl Pts',(3.73796629905055,0.794772684000619,10.0896540846223));
#57506=CARTESIAN_POINT('Ctrl Pts',(3.80379882167682,1.0684760419455,10.1322624369106));
#57507=CARTESIAN_POINT('Ctrl Pts',(3.82778999860573,1.1851427086128,10.1530748961532));
#57508=CARTESIAN_POINT('Ctrl Pts',(3.84727589275395,1.30000000000164,10.1762562377278));
#57509=CARTESIAN_POINT('Ctrl Pts',(3.68570115410586,-1.29999999999973,10.3482444573312));
#57510=CARTESIAN_POINT('Ctrl Pts',(3.67428383436732,-1.18514270861152,10.3106980921864));
#57511=CARTESIAN_POINT('Ctrl Pts',(3.65997227456622,-1.06847604194487,10.2746581733336));
#57512=CARTESIAN_POINT('Ctrl Pts',(3.62022343487266,-0.794772684000658,
10.1948789433209));
#57513=CARTESIAN_POINT('Ctrl Pts',(3.57884262070824,-0.636309800095039,
10.1458049927457));
#57514=CARTESIAN_POINT('Ctrl Pts',(3.54228491914268,-0.319434907277079,
10.079684590746));
#57515=CARTESIAN_POINT('Ctrl Pts',(3.52237947065255,-0.158333333333293,
10.050831400517));
#57516=CARTESIAN_POINT('Ctrl Pts',(3.54007106517567,0.158333333333295,10.0289178015944));
#57517=CARTESIAN_POINT('Ctrl Pts',(3.57782735161353,0.319434907277085,10.035674057266));
#57518=CARTESIAN_POINT('Ctrl Pts',(3.65009718999559,0.636309800095045,10.0575314775792));
#57519=CARTESIAN_POINT('Ctrl Pts',(3.71059118059011,0.794772684000643,10.082369063769));
#57520=CARTESIAN_POINT('Ctrl Pts',(3.77984387637945,1.06847604194553,10.1264643368999));
#57521=CARTESIAN_POINT('Ctrl Pts',(3.80618333956597,1.18514270861284,10.1482800998854));
#57522=CARTESIAN_POINT('Ctrl Pts',(3.82888533999698,1.30000000000168,10.1728244160087));
#57523=CARTESIAN_POINT('Ctrl Pts',(3.66853450170536,-1.29999999999975,10.3426239775828));
#57524=CARTESIAN_POINT('Ctrl Pts',(3.65350080759412,-1.18514270861155,10.3044212694721));
#57525=CARTESIAN_POINT('Ctrl Pts',(3.63664732387774,-1.06847604194489,10.2677322320564));
#57526=CARTESIAN_POINT('Ctrl Pts',(3.5935083269295,-0.794772684000673,10.1864700981242));
#57527=CARTESIAN_POINT('Ctrl Pts',(3.55376029588737,-0.636309800095053,
10.1359540029149));
#57528=CARTESIAN_POINT('Ctrl Pts',(3.5173108952179,-0.319434907277086,10.0694354783221));
#57529=CARTESIAN_POINT('Ctrl Pts',(3.49827260555614,-0.158333333333296,
10.0412853620192));
#57530=CARTESIAN_POINT('Ctrl Pts',(3.515186898278,0.158333333333298,10.0206766993231));
#57531=CARTESIAN_POINT('Ctrl Pts',(3.55086120578275,0.319434907277093,10.0287266459559));
#57532=CARTESIAN_POINT('Ctrl Pts',(3.62233062874898,0.636309800095061,10.0522310448285));
#57533=CARTESIAN_POINT('Ctrl Pts',(3.68168671424421,0.794772684000661,10.0778898702516));
#57534=CARTESIAN_POINT('Ctrl Pts',(3.7547029246493,1.06847604194556,10.1228699535018));
#57535=CARTESIAN_POINT('Ctrl Pts',(3.78380047762748,1.18514270861286,10.144941328333));
#57536=CARTESIAN_POINT('Ctrl Pts',(3.81038957161665,1.30000000000171,10.1696138666328));
#57537=CARTESIAN_POINT('Ctrl Pts',(3.65042204492736,-1.29999999999978,10.3384258601433));
#57538=CARTESIAN_POINT('Ctrl Pts',(3.63209486961421,-1.18514270861158,10.2990618837114));
#57539=CARTESIAN_POINT('Ctrl Pts',(3.61286153133498,-1.06847604194492,10.2614783916334));
#57540=CARTESIAN_POINT('Ctrl Pts',(3.56633525456491,-0.794772684000693,
10.1787662814238));
#57541=CARTESIAN_POINT('Ctrl Pts',(3.52740334221702,-0.636309800095068,
10.1281600041754));
#57542=CARTESIAN_POINT('Ctrl Pts',(3.49104594994429,-0.319434907277094,
10.0612870409283));
#57543=CARTESIAN_POINT('Ctrl Pts',(3.47317522219543,-0.1583333333333,10.0333749380405));
#57544=CARTESIAN_POINT('Ctrl Pts',(3.49016458763537,0.158333333333302,10.0126203440089));
#57545=CARTESIAN_POINT('Ctrl Pts',(3.52488674318907,0.3194349072771,10.0200149695696));
#57546=CARTESIAN_POINT('Ctrl Pts',(3.59613121861891,0.636309800095075,10.0441293295008));
#57547=CARTESIAN_POINT('Ctrl Pts',(3.65419761495957,0.794772684000681,10.0707537876965));
#57548=CARTESIAN_POINT('Ctrl Pts',(3.73039928648562,1.06847604194558,10.1176424164178));
#57549=CARTESIAN_POINT('Ctrl Pts',(3.76184998177745,1.18514270861289,10.1407124916779));
#57550=CARTESIAN_POINT('Ctrl Pts',(3.79176649230761,1.30000000000173,10.1665562922197));
#57551=CARTESIAN_POINT('Ctrl Pts',(3.63654746083435,-1.2999999999998,10.333034031973));
#57552=CARTESIAN_POINT('Ctrl Pts',(3.61550547136668,-1.18514270861159,10.2926301002341));
#57553=CARTESIAN_POINT('Ctrl Pts',(3.59428098834889,-1.06847604194493,10.2542942008572));
#57554=CARTESIAN_POINT('Ctrl Pts',(3.54482659002603,-0.794772684000701,
10.1705081726912));
#57555=CARTESIAN_POINT('Ctrl Pts',(3.50633075381572,-0.636309800095076,
10.1202089866768));
#57556=CARTESIAN_POINT('Ctrl Pts',(3.4699133232566,-0.319434907277098,10.0532488577123));
#57557=CARTESIAN_POINT('Ctrl Pts',(3.45318708873705,-0.158333333333302,
10.0252571936496));
#57558=CARTESIAN_POINT('Ctrl Pts',(3.46993367159814,0.158333333333304,10.0048871610833));
#57559=CARTESIAN_POINT('Ctrl Pts',(3.5032635327371,0.319434907277105,10.0127351329886));
#57560=CARTESIAN_POINT('Ctrl Pts',(3.5740837383614,0.636309800095084,10.0377419331908));
#57561=CARTESIAN_POINT('Ctrl Pts',(3.63128566085972,0.79477268400069,10.0648118403662));
#57562=CARTESIAN_POINT('Ctrl Pts',(3.71032993277458,1.06847604194559,10.1129544035429));
#57563=CARTESIAN_POINT('Ctrl Pts',(3.74384697749113,1.18514270861291,10.1366687284428));
#57564=CARTESIAN_POINT('Ctrl Pts',(3.77666573049112,1.30000000000175,10.163258246501));
#57565=CARTESIAN_POINT('Ctrl Pts',(3.62446370502867,-1.29999999999981,10.3302238019512));
#57566=CARTESIAN_POINT('Ctrl Pts',(3.60122766761322,-1.18514270861159,10.2890330237839));
#57567=CARTESIAN_POINT('Ctrl Pts',(3.57844949673732,-1.06847604194493,10.2500408126944));
#57568=CARTESIAN_POINT('Ctrl Pts',(3.52688512855879,-0.794772684000705,
10.1650401344845));
#57569=CARTESIAN_POINT('Ctrl Pts',(3.48917206155801,-0.636309800095079,
10.1142973381355));
#57570=CARTESIAN_POINT('Ctrl Pts',(3.45299373509218,-0.3194349072771,10.046822738906));
#57571=CARTESIAN_POINT('Ctrl Pts',(3.43720357052491,-0.158333333333303,
10.0187504466707));
#57572=CARTESIAN_POINT('Ctrl Pts',(3.4537702078461,0.158333333333305,9.99866359183929));
#57573=CARTESIAN_POINT('Ctrl Pts',(3.48590490068051,0.319434907277106,10.0069760041332));
#57574=CARTESIAN_POINT('Ctrl Pts',(3.55628069468287,0.636309800095087,10.0328691020645));
#57575=CARTESIAN_POINT('Ctrl Pts',(3.61260245590577,0.794772684000694,10.0606382417998));
#57576=CARTESIAN_POINT('Ctrl Pts',(3.69401004463299,1.0684760419456,10.109639868439));
#57577=CARTESIAN_POINT('Ctrl Pts',(3.72928544829501,1.18514270861291,10.1336918740997));
#57578=CARTESIAN_POINT('Ctrl Pts',(3.76459792690738,1.30000000000176,10.1605848969381));
#57579=CARTESIAN_POINT('Ctrl Pts',(3.60720160452376,-1.29999999999982,10.3246930658666));
#57580=CARTESIAN_POINT('Ctrl Pts',(3.58063922988522,-1.18514270861161,10.2823745958345));
#57581=CARTESIAN_POINT('Ctrl Pts',(3.55547182313521,-1.06847604194495,10.2424875527587));
#57582=CARTESIAN_POINT('Ctrl Pts',(3.50055273370511,-0.794772684000714,
10.155957586552));
#57583=CARTESIAN_POINT('Ctrl Pts',(3.46384163195749,-0.636309800095088,
10.104820967497));
#57584=CARTESIAN_POINT('Ctrl Pts',(3.42770026301507,-0.319434907277105,
10.0370681906501));
#57585=CARTESIAN_POINT('Ctrl Pts',(3.41292545540548,-0.158333333333305,
10.0094712140234));
#57586=CARTESIAN_POINT('Ctrl Pts',(3.42927917675529,0.158333333333307,9.98970646933673));
#57587=CARTESIAN_POINT('Ctrl Pts',(3.46011271931971,0.319434907277111,9.99795680932176));
#57588=CARTESIAN_POINT('Ctrl Pts',(3.53016630719154,0.636309800095096,10.024598568368));
#57589=CARTESIAN_POINT('Ctrl Pts',(3.58554467377616,0.794772684000705,10.0527059489922));
#57590=CARTESIAN_POINT('Ctrl Pts',(3.67010612733831,1.06847604194562,10.1036611532208));
#57591=CARTESIAN_POINT('Ctrl Pts',(3.70765640796908,1.18514270861293,10.1288493866877));
#57592=CARTESIAN_POINT('Ctrl Pts',(3.7461534492941,1.30000000000178,10.1571692337871));
#57593=CARTESIAN_POINT('Ctrl Pts',(3.58378319929592,-1.29999999999985,10.3178735693703));
#57594=CARTESIAN_POINT('Ctrl Pts',(3.55311880004611,-1.18514270861164,10.2735172558038));
#57595=CARTESIAN_POINT('Ctrl Pts',(3.52502338935574,-1.06847604194497,10.2320295366664));
#57596=CARTESIAN_POINT('Ctrl Pts',(3.46605224769,-0.794772684000734,10.142811632861));
#57597=CARTESIAN_POINT('Ctrl Pts',(3.43067766881984,-0.636309800095103,
10.0911930054387));
#57598=CARTESIAN_POINT('Ctrl Pts',(3.39475905345327,-0.319434907277112,
10.0228204783981));
#57599=CARTESIAN_POINT('Ctrl Pts',(3.38152701401965,-0.158333333333309,
9.99557018368774));
#57600=CARTESIAN_POINT('Ctrl Pts',(3.39744303920166,0.158333333333311,9.9764535028626));
#57601=CARTESIAN_POINT('Ctrl Pts',(3.42625716100374,0.31943490727712,9.98498852827799));
#57602=CARTESIAN_POINT('Ctrl Pts',(3.49527579114069,0.636309800095112,10.0136041065402));
#57603=CARTESIAN_POINT('Ctrl Pts',(3.54840272315516,0.794772684000723,10.0438906055675));
#57604=CARTESIAN_POINT('Ctrl Pts',(3.6373929333043,1.06847604194564,10.097067130942));
#57605=CARTESIAN_POINT('Ctrl Pts',(3.6783751929315,1.18514270861296,10.1230878921532));
#57606=CARTESIAN_POINT('Ctrl Pts',(3.72181914762449,1.30000000000182,10.1521112671253));
#57607=CARTESIAN_POINT('Ctrl Pts',(3.56138672197762,-1.29999999999988,10.3095005735531));
#57608=CARTESIAN_POINT('Ctrl Pts',(3.5264945322361,-1.18514270861167,10.2633053010594));
#57609=CARTESIAN_POINT('Ctrl Pts',(3.49537043823022,-1.068476041945,10.2203754927062));
#57610=CARTESIAN_POINT('Ctrl Pts',(3.43217260967728,-0.794772684000756,
10.1287429227498));
#57611=CARTESIAN_POINT('Ctrl Pts',(3.39811853902977,-0.63630980009512,10.0766656342623));
#57612=CARTESIAN_POINT('Ctrl Pts',(3.36231880711828,-0.31943490727712,10.007828718619));
#57613=CARTESIAN_POINT('Ctrl Pts',(3.35051604805238,-0.158333333333313,
9.98109823159642));
#57614=CARTESIAN_POINT('Ctrl Pts',(3.36603468341215,0.158333333333315,9.96255096961667));
#57615=CARTESIAN_POINT('Ctrl Pts',(3.3928274124033,0.319434907277128,9.97140476165473));
#57616=CARTESIAN_POINT('Ctrl Pts',(3.46131434058875,0.636309800095128,10.0010963434057));
#57617=CARTESIAN_POINT('Ctrl Pts',(3.51336861172402,0.794772684000745,10.0314617398297));
#57618=CARTESIAN_POINT('Ctrl Pts',(3.60651490650398,1.06847604194567,10.0872896694177));
#57619=CARTESIAN_POINT('Ctrl Pts',(3.65047241819542,1.18514270861299,10.1149204214575));
#57620=CARTESIAN_POINT('Ctrl Pts',(3.69806786197832,1.30000000000184,10.1460160834469));
#57621=CARTESIAN_POINT('Ctrl Pts',(3.53855149764873,-1.2999999999999,10.3017508966993));
#57622=CARTESIAN_POINT('Ctrl Pts',(3.49941489950663,-1.18514270861168,10.2537129280734));
#57623=CARTESIAN_POINT('Ctrl Pts',(3.46532473422636,-1.06847604194501,10.2092310982888));
#57624=CARTESIAN_POINT('Ctrl Pts',(3.39822790216101,-0.794772684000764,
10.1146845650534));
#57625=CARTESIAN_POINT('Ctrl Pts',(3.3660310219522,-0.636309800095125,10.0613869862023));
#57626=CARTESIAN_POINT('Ctrl Pts',(3.33082756807032,-0.319434907277123,
9.99139500095045));
#57627=CARTESIAN_POINT('Ctrl Pts',(3.32078738128955,-0.158333333333315,
9.96471106885896));
#57628=CARTESIAN_POINT('Ctrl Pts',(3.33573966037722,0.158333333333317,9.94695881112389));
#57629=CARTESIAN_POINT('Ctrl Pts',(3.35992214767888,0.319434907277132,9.95690953203665));
#57630=CARTESIAN_POINT('Ctrl Pts',(3.42723218548264,0.636309800095136,9.98866572202563));
#57631=CARTESIAN_POINT('Ctrl Pts',(3.4776049539938,0.794772684000752,10.020182490244));
#57632=CARTESIAN_POINT('Ctrl Pts',(3.57489815356795,1.06847604194568,10.078696696035));
#57633=CARTESIAN_POINT('Ctrl Pts',(3.62200692329494,1.185142708613,10.1076542382111));
#57634=CARTESIAN_POINT('Ctrl Pts',(3.67410984172149,1.30000000000186,10.1402406910412));
#57635=CARTESIAN_POINT('Ctrl Pts',(3.51929591785351,-1.29999999999997,10.2939294651204));
#57636=CARTESIAN_POINT('Ctrl Pts',(3.47679697345141,-1.18514270861175,10.2438286551357));
#57637=CARTESIAN_POINT('Ctrl Pts',(3.4402855928125,-1.06847604194507,10.1977848253857));
#57638=CARTESIAN_POINT('Ctrl Pts',(3.36976946956097,-0.794772684000805,
10.1007868035652));
#57639=CARTESIAN_POINT('Ctrl Pts',(3.338399999449,-0.636309800095159,10.0476074585909));
#57640=CARTESIAN_POINT('Ctrl Pts',(3.30347328960332,-0.31943490727714,9.97698760693245));
#57641=CARTESIAN_POINT('Ctrl Pts',(3.29508348591708,-0.158333333333323,
9.95018329512672));
#57642=CARTESIAN_POINT('Ctrl Pts',(3.30987058860113,0.158333333333325,9.93261597869159));
#57643=CARTESIAN_POINT('Ctrl Pts',(3.33244160595743,0.31943490727715,9.9425092179148));
#57644=CARTESIAN_POINT('Ctrl Pts',(3.39872273155985,0.63630980009517,9.97600898940697));
#57645=CARTESIAN_POINT('Ctrl Pts',(3.4470306553148,0.794772684000795,10.0093452012326));
#57646=CARTESIAN_POINT('Ctrl Pts',(3.54741396098122,1.06847604194573,10.0709607253317));
#57647=CARTESIAN_POINT('Ctrl Pts',(3.5970435863886,1.18514270861306,10.1014181357824));
#57648=CARTESIAN_POINT('Ctrl Pts',(3.65285062374829,1.30000000000192,10.1356618793814));
#57649=CARTESIAN_POINT('Ctrl Pts',(3.49657587699451,-1.29999999999997,10.2859305508819));
#57650=CARTESIAN_POINT('Ctrl Pts',(3.45002544710238,-1.18514270861174,10.2336461217128));
#57651=CARTESIAN_POINT('Ctrl Pts',(3.41074789121993,-1.06847604194507,10.1857246550423));
#57652=CARTESIAN_POINT('Ctrl Pts',(3.33681067357917,-0.794772684000805,
10.085095796556));
#57653=CARTESIAN_POINT('Ctrl Pts',(3.30793311972073,-0.63630980009516,10.0298699456148));
#57654=CARTESIAN_POINT('Ctrl Pts',(3.27349123802796,-0.319434907277141,
9.95827558428957));
#57655=CARTESIAN_POINT('Ctrl Pts',(3.2658527784058,-0.158333333333323,9.93297551112294));
#57656=CARTESIAN_POINT('Ctrl Pts',(3.27998125659245,0.158333333333325,9.91627742782468));
#57657=CARTESIAN_POINT('Ctrl Pts',(3.3006655020231,0.319434907277149,9.92615406278584));
#57658=CARTESIAN_POINT('Ctrl Pts',(3.36609144291574,0.63630980009517,9.96113927045787));
#57659=CARTESIAN_POINT('Ctrl Pts',(3.4127066905504,0.794772684000796,9.99550087406892));
#57660=CARTESIAN_POINT('Ctrl Pts',(3.51714884489834,1.06847604194574,10.0599476959581));
#57661=CARTESIAN_POINT('Ctrl Pts',(3.56984258657858,1.18514270861306,10.091908326306));
#57662=CARTESIAN_POINT('Ctrl Pts',(3.63002093128492,1.30000000000192,10.1279329457959));
#57663=CARTESIAN_POINT('Ctrl Pts',(3.4802295000654,-1.3,10.2789860295797));
#57664=CARTESIAN_POINT('Ctrl Pts',(3.43091440205945,-1.18514270861177,10.2247844835619));
#57665=CARTESIAN_POINT('Ctrl Pts',(3.38968103217071,-1.06847604194509,10.175373649079));
#57666=CARTESIAN_POINT('Ctrl Pts',(3.31309410771521,-0.794772684000823,
10.0722922388441));
#57667=CARTESIAN_POINT('Ctrl Pts',(3.28513733028894,-0.636309800095174,
10.0169134300136));
#57668=CARTESIAN_POINT('Ctrl Pts',(3.25116537962811,-0.319434907277147,
9.94448213163101));
#57669=CARTESIAN_POINT('Ctrl Pts',(3.24507410638107,-0.158333333333326,
9.91889631942219));
#57670=CARTESIAN_POINT('Ctrl Pts',(3.25900350812188,0.158333333333329,9.90241295720868));
#57671=CARTESIAN_POINT('Ctrl Pts',(3.27802168356298,0.319434907277155,9.91261429661292));
#57672=CARTESIAN_POINT('Ctrl Pts',(3.34240884201399,0.636309800095183,9.94923181440477));
#57673=CARTESIAN_POINT('Ctrl Pts',(3.38741908809698,0.794772684000813,9.98480266593302));
#57674=CARTESIAN_POINT('Ctrl Pts',(3.49424009078888,1.06847604194576,10.0522670360987));
#57675=CARTESIAN_POINT('Ctrl Pts',(3.548901837997,1.18514270861309,10.0858023098939));
#57676=CARTESIAN_POINT('Ctrl Pts',(3.61198647845601,1.30000000000195,10.1236700314407));
#57677=CARTESIAN_POINT('Ctrl Pts',(3.46380404043217,-1.30000000000001,10.2720051436094));
#57678=CARTESIAN_POINT('Ctrl Pts',(3.41143469758712,-1.18514270861178,10.2160283216677));
#57679=CARTESIAN_POINT('Ctrl Pts',(3.36815068395304,-1.0684760419451,10.1650646631163));
#57680=CARTESIAN_POINT('Ctrl Pts',(3.2891448815123,-0.79477268400083,10.0589098269297));
#57681=CARTESIAN_POINT('Ctrl Pts',(3.2637249951748,-0.63630980009518,10.0011599660398));
#57682=CARTESIAN_POINT('Ctrl Pts',(3.22953275013871,-0.319434907277151,
9.92878866647668));
#57683=CARTESIAN_POINT('Ctrl Pts',(3.22230664903844,-0.158333333333328,
9.90666524664121));
#57684=CARTESIAN_POINT('Ctrl Pts',(3.2354888075062,0.15833333333333,9.89114113457973));
#57685=CARTESIAN_POINT('Ctrl Pts',(3.25440572980874,0.319434907277158,9.89944511143236));
#57686=CARTESIAN_POINT('Ctrl Pts',(3.31848682912671,0.636309800095189,9.93672262432642));
#57687=CARTESIAN_POINT('Ctrl Pts',(3.36175770004629,0.79477268400082,9.97370681958844));
#57688=CARTESIAN_POINT('Ctrl Pts',(3.47142677497237,1.06847604194577,10.0437803832112));
#57689=CARTESIAN_POINT('Ctrl Pts',(3.5283166481924,1.1851427086131,10.078680079522));
#57690=CARTESIAN_POINT('Ctrl Pts',(3.59462471573652,1.30000000000196,10.1181472229327));
#57691=CARTESIAN_POINT('Ctrl Pts',(3.45022017105532,-1.30000000000002,10.2662412177575));
#57692=CARTESIAN_POINT('Ctrl Pts',(3.39606660535214,-1.18514270861179,10.2081259394358));
#57693=CARTESIAN_POINT('Ctrl Pts',(3.35136323908567,-1.06847604194511,10.1557680049425));
#57694=CARTESIAN_POINT('Ctrl Pts',(3.26992137133707,-0.794772684000838,
10.04811131809));
#57695=CARTESIAN_POINT('Ctrl Pts',(3.2438885726079,-0.636309800095184,9.99214438464443));
#57696=CARTESIAN_POINT('Ctrl Pts',(3.20916354990404,-0.319434907277152,
9.92045275636352));
#57697=CARTESIAN_POINT('Ctrl Pts',(3.20258479929904,-0.158333333333329,
9.89903738322094));
#57698=CARTESIAN_POINT('Ctrl Pts',(3.21612697191109,0.158333333333331,9.88298698307226));
#57699=CARTESIAN_POINT('Ctrl Pts',(3.23530727064128,0.319434907277161,9.88928439861708));
#57700=CARTESIAN_POINT('Ctrl Pts',(3.29953270823961,0.636309800095194,9.92638319912416));
#57701=CARTESIAN_POINT('Ctrl Pts',(3.34140180159176,0.794772684000824,9.96433113446368));
#57702=CARTESIAN_POINT('Ctrl Pts',(3.45322975452854,1.06847604194578,10.036354963907));
#57703=CARTESIAN_POINT('Ctrl Pts',(3.51178755380993,1.18514270861311,10.072358936718));
#57704=CARTESIAN_POINT('Ctrl Pts',(3.58049697518027,1.30000000000198,10.1131904353198));
#57705=CARTESIAN_POINT('Ctrl Pts',(3.43423105359299,-1.30000000000003,10.258649491102));
#57706=CARTESIAN_POINT('Ctrl Pts',(3.37760262054861,-1.1851427086118,10.1977714595931));
#57707=CARTESIAN_POINT('Ctrl Pts',(3.33083250059634,-1.06847604194512,10.1437157323749));
#57708=CARTESIAN_POINT('Ctrl Pts',(3.2455588425677,-0.794772684000841,10.0345970763986));
#57709=CARTESIAN_POINT('Ctrl Pts',(3.21800531622045,-0.636309800095188,
9.98161924932007));
#57710=CARTESIAN_POINT('Ctrl Pts',(3.18185839235816,-0.319434907277154,
9.91157187300279));
#57711=CARTESIAN_POINT('Ctrl Pts',(3.17601680631054,-0.15833333333333,9.89127734987168));
#57712=CARTESIAN_POINT('Ctrl Pts',(3.18947052405278,0.158333333333332,9.87531030441977));
#57713=CARTESIAN_POINT('Ctrl Pts',(3.20799409399132,0.319434907277162,9.88030865988734));
#57714=CARTESIAN_POINT('Ctrl Pts',(3.27311723848317,0.636309800095197,9.91646578453442));
#57715=CARTESIAN_POINT('Ctrl Pts',(3.315456288054,0.794772684000828,9.95289384391755));
#57716=CARTESIAN_POINT('Ctrl Pts',(3.43106717232058,1.06847604194578,10.0265379844801));
#57717=CARTESIAN_POINT('Ctrl Pts',(3.49191566964394,1.18514270861312,10.0639884215424));
#57718=CARTESIAN_POINT('Ctrl Pts',(3.56356899629696,1.30000000000199,10.1070114760016));
#57719=CARTESIAN_POINT('Ctrl Pts',(3.42329004793795,-1.30000000000005,10.2535552330257));
#57720=CARTESIAN_POINT('Ctrl Pts',(3.36577675441716,-1.18514270861181,10.1896775761705));
#57721=CARTESIAN_POINT('Ctrl Pts',(3.31797563071956,-1.06847604194513,10.1340934433128));
#57722=CARTESIAN_POINT('Ctrl Pts',(3.22998252760056,-0.794772684000851,
10.0248426763922));
#57723=CARTESIAN_POINT('Ctrl Pts',(3.19945051412027,-0.636309800095197,
9.97773483060053));
#57724=CARTESIAN_POINT('Ctrl Pts',(3.16161671560349,-0.319434907277159,
9.91074553869703));
#57725=CARTESIAN_POINT('Ctrl Pts',(3.15675867153595,-0.158333333333332,
9.89088328778878));
#57726=CARTESIAN_POINT('Ctrl Pts',(3.17014714941586,0.158333333333334,9.8750691093734));
#57727=CARTESIAN_POINT('Ctrl Pts',(3.18775359149335,0.319434907277167,9.87971474161891));
#57728=CARTESIAN_POINT('Ctrl Pts',(3.25416255205695,0.636309800095206,9.91327450455847));
#57729=CARTESIAN_POINT('Ctrl Pts',(3.29862160463217,0.79477268400084,9.94456294634815));
#57730=CARTESIAN_POINT('Ctrl Pts',(3.41699686809867,1.0684760419458,10.0182954880635));
#57731=CARTESIAN_POINT('Ctrl Pts',(3.47911206103839,1.18514270861313,10.0570584190905));
#57732=CARTESIAN_POINT('Ctrl Pts',(3.55210218159882,1.300000000002,10.1026681958956));
#57733=CARTESIAN_POINT('Ctrl Pts',(3.41475847117042,-1.30000000000005,10.2524562333547));
#57734=CARTESIAN_POINT('Ctrl Pts',(3.3574890695822,-1.18514270861181,10.1886391816766));
#57735=CARTESIAN_POINT('Ctrl Pts',(3.30972802388307,-1.06847604194513,10.133397568411));
#57736=CARTESIAN_POINT('Ctrl Pts',(3.22135665799747,-0.794772684000851,
10.0255893689635));
#57737=CARTESIAN_POINT('Ctrl Pts',(3.18969432988981,-0.636309800095197,
9.98078487986184));
#57738=CARTESIAN_POINT('Ctrl Pts',(3.15117622767193,-0.319434907277159,
9.91533710840653));
#57739=CARTESIAN_POINT('Ctrl Pts',(3.14628700527777,-0.158333333333332,
9.89543280925802));
#57740=CARTESIAN_POINT('Ctrl Pts',(3.15959962456677,0.158333333333334,9.87984298008964));
#57741=CARTESIAN_POINT('Ctrl Pts',(3.17704490789093,0.319434907277167,9.88500970337775));
#57742=CARTESIAN_POINT('Ctrl Pts',(3.24422091196343,0.636309800095206,9.91696613669794));
#57743=CARTESIAN_POINT('Ctrl Pts',(3.29031662464091,0.79477268400084,9.94499299784744));
#57744=CARTESIAN_POINT('Ctrl Pts',(3.40898836153082,1.0684760419458,10.0174129929739));
#57745=CARTESIAN_POINT('Ctrl Pts',(3.47090355779047,1.18514270861313,10.0561105004451));
#57746=CARTESIAN_POINT('Ctrl Pts',(3.54336535263118,1.300000000002,10.1021575829223));
#57747=CARTESIAN_POINT('Ctrl Pts',(3.4147584711704,-1.3,10.2524562333546));
#57748=CARTESIAN_POINT('Ctrl Pts',(3.35748906958219,-1.18514270861178,10.1886391816766));
#57749=CARTESIAN_POINT('Ctrl Pts',(3.30972802388306,-1.06847604194512,10.133397568411));
#57750=CARTESIAN_POINT('Ctrl Pts',(3.22135665799747,-0.794772684000851,
10.0255893689635));
#57751=CARTESIAN_POINT('Ctrl Pts',(3.18969432988981,-0.636309800095197,
9.98078487986184));
#57752=CARTESIAN_POINT('Ctrl Pts',(3.15117622767193,-0.319434907277159,
9.91533710840653));
#57753=CARTESIAN_POINT('Ctrl Pts',(3.14628700527777,-0.158333333333332,
9.89543280925802));
#57754=CARTESIAN_POINT('Ctrl Pts',(3.15959962456677,0.158333333333334,9.87984298008964));
#57755=CARTESIAN_POINT('Ctrl Pts',(3.17704490789093,0.319434907277167,9.88500970337774));
#57756=CARTESIAN_POINT('Ctrl Pts',(3.24422091196343,0.636309800095206,9.91696613669794));
#57757=CARTESIAN_POINT('Ctrl Pts',(3.29031662464091,0.79477268400084,9.94499299784744));
#57758=CARTESIAN_POINT('Ctrl Pts',(3.40898836153052,1.06847604194511,10.0174129929737));
#57759=CARTESIAN_POINT('Ctrl Pts',(3.47090355778975,1.18514270861178,10.0561105004446));
#57760=CARTESIAN_POINT('Ctrl Pts',(3.54336535262991,1.3,10.1021575829215));
#57761=CARTESIAN_POINT('',(3.81826036790159,-1.2,10.3501409115962));
#57762=CARTESIAN_POINT('Ctrl Pts',(3.81826036790159,-1.2,10.3501409115962));
#57763=CARTESIAN_POINT('Ctrl Pts',(3.79666911560247,-1.21682679214414,10.3498705750651));
#57764=CARTESIAN_POINT('Ctrl Pts',(3.77476187409666,-1.23325258729674,10.3505181001901));
#57765=CARTESIAN_POINT('Ctrl Pts',(3.74202710674506,-1.25864657309861,10.3500191474087));
#57766=CARTESIAN_POINT('Ctrl Pts',(3.7314954635025,-1.26676751286954,10.3499115167687));
#57767=CARTESIAN_POINT('Ctrl Pts',(3.71258831258587,-1.28141947219131,10.3495705776323));
#57768=CARTESIAN_POINT('Ctrl Pts',(3.69913033630965,-1.29187184462129,10.3492642451596));
#57769=CARTESIAN_POINT('Ctrl Pts',(3.69072511418734,-1.298457549969,10.348970093154));
#57770=CARTESIAN_POINT('Ctrl Pts',(3.68974253591884,-1.29922936208746,10.3489325435325));
#57771=CARTESIAN_POINT('Ctrl Pts',(3.68876499475237,-1.29999999999972,10.3488907274614));
#57772=CARTESIAN_POINT('',(3.91593538932197,-0.653834841327623,10.227862286537));
#57773=CARTESIAN_POINT('Ctrl Pts',(3.9159353893185,-0.653834841312177,10.2278622866113));
#57774=CARTESIAN_POINT('Ctrl Pts',(3.90700550388882,-0.711393414252494,
10.2394113106641));
#57775=CARTESIAN_POINT('Ctrl Pts',(3.89748289441163,-0.767209744945321,
10.2516191953437));
#57776=CARTESIAN_POINT('Ctrl Pts',(3.87754062849598,-0.881633194810645,
10.2769213651307));
#57777=CARTESIAN_POINT('Ctrl Pts',(3.86793349028196,-0.939021993186391,
10.2890044992134));
#57778=CARTESIAN_POINT('Ctrl Pts',(3.84975474046838,-1.03714157084077,10.3115895811745));
#57779=CARTESIAN_POINT('Ctrl Pts',(3.84918980540933,-1.03956975094,10.3123276742784));
#57780=CARTESIAN_POINT('Ctrl Pts',(3.83021697552951,-1.13871235067932,10.3356129960789));
#57781=CARTESIAN_POINT('Ctrl Pts',(3.82499289590527,-1.16608643702209,10.3419804687545));
#57782=CARTESIAN_POINT('Ctrl Pts',(3.81826036790159,-1.2,10.3501409115962));
#57783=CARTESIAN_POINT('',(3.99970644340964,0.653834841531101,10.1163073168902));
#57784=CARTESIAN_POINT('Ctrl Pts',(3.99970644340962,0.653834841531101,10.1163073168902));
#57785=CARTESIAN_POINT('Ctrl Pts',(3.95879318609505,0.575732021690897,10.1082141213102));
#57786=CARTESIAN_POINT('Ctrl Pts',(3.9241762431234,0.493687875304555,10.1023287044845));
#57787=CARTESIAN_POINT('Ctrl Pts',(3.8739058242527,0.33806901713317,10.0960431987292));
#57788=CARTESIAN_POINT('Ctrl Pts',(3.85599434530751,0.26561107497815,10.095104067982));
#57789=CARTESIAN_POINT('Ctrl Pts',(3.83175003836914,0.129684465390305,10.0980902516012));
#57790=CARTESIAN_POINT('Ctrl Pts',(3.82414429286697,0.0666362255820432,
10.1012767240369));
#57791=CARTESIAN_POINT('Ctrl Pts',(3.81587160814996,-0.0594727714086463,
10.111667545938));
#57792=CARTESIAN_POINT('Ctrl Pts',(3.81513703688267,-0.122669468213772,
10.118928970212));
#57793=CARTESIAN_POINT('Ctrl Pts',(3.82170332152409,-0.260037978472135,
10.1384960942812));
#57794=CARTESIAN_POINT('Ctrl Pts',(3.83047324685118,-0.333902761432303,
10.1515184133504));
#57795=CARTESIAN_POINT('Ctrl Pts',(3.86128895474085,-0.491493501304615,
10.1841880364153));
#57796=CARTESIAN_POINT('Ctrl Pts',(3.88528595310545,-0.574905758777795,
10.2050069107913));
#57797=CARTESIAN_POINT('Ctrl Pts',(3.91593538921434,-0.653834841350336,
10.2278622866029));
#57798=CARTESIAN_POINT('',(3.95671216659572,1.2,10.1743787302079));
#57799=CARTESIAN_POINT('Ctrl Pts',(3.95671216659571,1.2,10.1743787302079));
#57800=CARTESIAN_POINT('Ctrl Pts',(3.96397347835393,1.13608680445646,10.1647192607237));
#57801=CARTESIAN_POINT('Ctrl Pts',(3.97397889641972,1.03790262443427,10.1513283596737));
#57802=CARTESIAN_POINT('Ctrl Pts',(3.9927072208627,0.79689965730155,10.1259111994147));
#57803=CARTESIAN_POINT('Ctrl Pts',(3.99584992410113,0.741366419488911,10.1215965211651));
#57804=CARTESIAN_POINT('Ctrl Pts',(3.99970644340962,0.653834841531098,10.1163073168902));
#57805=CARTESIAN_POINT('Ctrl Pts',(3.83165700304165,1.29999999999992,10.1733658723815));
#57806=CARTESIAN_POINT('Ctrl Pts',(3.85238006927995,1.28313652450894,10.1741677159342));
#57807=CARTESIAN_POINT('Ctrl Pts',(3.87334649564944,1.26654461476687,10.1741346610164));
#57808=CARTESIAN_POINT('Ctrl Pts',(3.90825716504668,1.23847808482738,10.1746669753888));
#57809=CARTESIAN_POINT('Ctrl Pts',(3.93166057066595,1.21946611443686,10.1753082311882));
#57810=CARTESIAN_POINT('Ctrl Pts',(3.95671216659572,1.2,10.1743787302079));
#57811=CARTESIAN_POINT('Ctrl Pts',(3.4147584711704,-1.3,10.2524562333546));
#57812=CARTESIAN_POINT('Ctrl Pts',(3.35748906958219,-1.18514270861178,10.1886391816766));
#57813=CARTESIAN_POINT('Ctrl Pts',(3.30972802388306,-1.06847604194512,10.133397568411));
#57814=CARTESIAN_POINT('Ctrl Pts',(3.22135665799746,-0.794772684000851,
10.0255893689635));
#57815=CARTESIAN_POINT('Ctrl Pts',(3.18969432988981,-0.636309800095197,
9.98078487986184));
#57816=CARTESIAN_POINT('Ctrl Pts',(3.15117622767193,-0.319434907277159,
9.91533710840652));
#57817=CARTESIAN_POINT('Ctrl Pts',(3.14628700527777,-0.158333333333332,
9.89543280925802));
#57818=CARTESIAN_POINT('Ctrl Pts',(3.15959962456677,0.158333333333334,9.87984298008963));
#57819=CARTESIAN_POINT('Ctrl Pts',(3.17704490789093,0.319434907277167,9.88500970337774));
#57820=CARTESIAN_POINT('Ctrl Pts',(3.24422091196343,0.636309800095206,9.91696613669794));
#57821=CARTESIAN_POINT('Ctrl Pts',(3.29031662464091,0.79477268400084,9.94499299784744));
#57822=CARTESIAN_POINT('Ctrl Pts',(3.40898836153052,1.06847604194511,10.0174129929737));
#57823=CARTESIAN_POINT('Ctrl Pts',(3.47090355778975,1.18514270861178,10.0561105004446));
#57824=CARTESIAN_POINT('Ctrl Pts',(3.54336535262991,1.3,10.1021575829215));
#57825=CARTESIAN_POINT('Ctrl Pts',(3.3620529124905,-1.3,10.3085029402952));
#57826=CARTESIAN_POINT('Ctrl Pts',(3.30608359416459,-1.18514270861178,10.2435410355842));
#57827=CARTESIAN_POINT('Ctrl Pts',(3.25925709076723,-1.06847604194512,10.1875362842913));
#57828=CARTESIAN_POINT('Ctrl Pts',(3.17220023180818,-0.794772684000851,
10.0788469213604));
#57829=CARTESIAN_POINT('Ctrl Pts',(3.14019479937607,-0.636309800095197,
10.0346727316879));
#57830=CARTESIAN_POINT('Ctrl Pts',(3.10158167219449,-0.319434907277159,
9.96988500070868));
#57831=CARTESIAN_POINT('Ctrl Pts',(3.09600154123355,-0.158333333333332,
9.95101225241256));
#57832=CARTESIAN_POINT('Ctrl Pts',(3.10958091369844,0.158333333333334,9.93566260888257));
#57833=CARTESIAN_POINT('Ctrl Pts',(3.12797987732074,0.319434907277167,9.94003438204794));
#57834=CARTESIAN_POINT('Ctrl Pts',(3.19580237328514,0.636309800095206,9.97182731794448));
#57835=CARTESIAN_POINT('Ctrl Pts',(3.24248906837777,0.79477268400084,9.99944707010018));
#57836=CARTESIAN_POINT('Ctrl Pts',(3.36042187227873,1.06847604194511,10.0732664778114));
#57837=CARTESIAN_POINT('Ctrl Pts',(3.42167579733126,1.18514270861178,10.1129731777087));
#57838=CARTESIAN_POINT('Ctrl Pts',(3.49313490646867,1.3,10.1604328911839));
#57839=CARTESIAN_POINT('Ctrl Pts',(3.3093473538106,-1.3,10.3645496472358));
#57840=CARTESIAN_POINT('Ctrl Pts',(3.25467811874699,-1.18514270861178,10.2984428894918));
#57841=CARTESIAN_POINT('Ctrl Pts',(3.20878615765139,-1.06847604194512,10.2416750001716));
#57842=CARTESIAN_POINT('Ctrl Pts',(3.12304380561889,-0.794772684000851,
10.1321044737573));
#57843=CARTESIAN_POINT('Ctrl Pts',(3.09069526886232,-0.636309800095197,
10.0885605835139));
#57844=CARTESIAN_POINT('Ctrl Pts',(3.05198711671704,-0.319434907277159,
10.0244328930108));
#57845=CARTESIAN_POINT('Ctrl Pts',(3.04571607718934,-0.158333333333332,
10.0065916955671));
#57846=CARTESIAN_POINT('Ctrl Pts',(3.05956220283012,0.158333333333334,9.99148223767551));
#57847=CARTESIAN_POINT('Ctrl Pts',(3.07891484675056,0.319434907277167,9.99505906071815));
#57848=CARTESIAN_POINT('Ctrl Pts',(3.14738383460685,0.636309800095206,10.026688499191));
#57849=CARTESIAN_POINT('Ctrl Pts',(3.19466151211463,0.79477268400084,10.0539011423529));
#57850=CARTESIAN_POINT('Ctrl Pts',(3.31185538302693,1.06847604194511,10.129119962649));
#57851=CARTESIAN_POINT('Ctrl Pts',(3.37244803687278,1.18514270861178,10.1698358549729));
#57852=CARTESIAN_POINT('Ctrl Pts',(3.44290446030743,1.3,10.2187081994464));
#57853=CARTESIAN_POINT('Ctrl Pts',(3.25664179513071,-1.3,10.4205963541764));
#57854=CARTESIAN_POINT('Ctrl Pts',(3.20327264332939,-1.18514270861178,10.3533447433995));
#57855=CARTESIAN_POINT('Ctrl Pts',(3.15831522453555,-1.06847604194512,10.2958137160519));
#57856=CARTESIAN_POINT('Ctrl Pts',(3.0738873794296,-0.794772684000851,10.1853620261542));
#57857=CARTESIAN_POINT('Ctrl Pts',(3.04119573834857,-0.636309800095197,
10.14244843534));
#57858=CARTESIAN_POINT('Ctrl Pts',(3.0023925612396,-0.319434907277159,10.078980785313));
#57859=CARTESIAN_POINT('Ctrl Pts',(2.99543061314513,-0.158333333333332,
10.0621711387217));
#57860=CARTESIAN_POINT('Ctrl Pts',(3.00954349196179,0.158333333333334,10.0473018664684));
#57861=CARTESIAN_POINT('Ctrl Pts',(3.02984981618037,0.319434907277167,10.0500837393884));
#57862=CARTESIAN_POINT('Ctrl Pts',(3.09896529592856,0.636309800095206,10.0815496804376));
#57863=CARTESIAN_POINT('Ctrl Pts',(3.14683395585149,0.79477268400084,10.1083552146057));
#57864=CARTESIAN_POINT('Ctrl Pts',(3.26328889377514,1.06847604194511,10.1849734474866));
#57865=CARTESIAN_POINT('Ctrl Pts',(3.32322027641429,1.18514270861178,10.226698532237));
#57866=CARTESIAN_POINT('Ctrl Pts',(3.39267401414619,1.3,10.2769835077089));
#57867=CARTESIAN_POINT('Ctrl Pts',(3.2566417951307,-1.3,10.4205963541764));
#57868=CARTESIAN_POINT('Ctrl Pts',(3.20327264332939,-1.18514270861178,10.3533447433995));
#57869=CARTESIAN_POINT('Ctrl Pts',(3.15831522453555,-1.06847604194512,10.2958137160519));
#57870=CARTESIAN_POINT('Ctrl Pts',(3.0738873794296,-0.794772684000851,10.1853620261542));
#57871=CARTESIAN_POINT('Ctrl Pts',(3.04119573834857,-0.636309800095197,
10.14244843534));
#57872=CARTESIAN_POINT('Ctrl Pts',(3.0023925612396,-0.319434907277159,10.078980785313));
#57873=CARTESIAN_POINT('Ctrl Pts',(2.99543061314513,-0.158333333333332,
10.0621711387217));
#57874=CARTESIAN_POINT('Ctrl Pts',(3.00954349196179,0.158333333333334,10.0473018664685));
#57875=CARTESIAN_POINT('Ctrl Pts',(3.02984981618038,0.319434907277167,10.0500837393884));
#57876=CARTESIAN_POINT('Ctrl Pts',(3.09896529592856,0.636309800095206,10.0815496804376));
#57877=CARTESIAN_POINT('Ctrl Pts',(3.14683395585149,0.79477268400084,10.1083552146057));
#57878=CARTESIAN_POINT('Ctrl Pts',(3.26328889377514,1.06847604194511,10.1849734474866));
#57879=CARTESIAN_POINT('Ctrl Pts',(3.32322027641429,1.18514270861178,10.226698532237));
#57880=CARTESIAN_POINT('Ctrl Pts',(3.39267401414619,1.3,10.2769835077089));
#57881=CARTESIAN_POINT('Ctrl Pts',(3.25664179513082,-1.30000000000024,10.4205963541766));
#57882=CARTESIAN_POINT('Ctrl Pts',(3.20327264332946,-1.18514270861195,10.3533447433995));
#57883=CARTESIAN_POINT('Ctrl Pts',(3.15831522453558,-1.0684760419452,10.2958137160519));
#57884=CARTESIAN_POINT('Ctrl Pts',(3.0738873794296,-0.794772684000852,10.1853620261542));
#57885=CARTESIAN_POINT('Ctrl Pts',(3.04119573834858,-0.636309800095197,
10.14244843534));
#57886=CARTESIAN_POINT('Ctrl Pts',(3.0023925612396,-0.319434907277159,10.078980785313));
#57887=CARTESIAN_POINT('Ctrl Pts',(2.99543061314513,-0.158333333333333,
10.0621711387217));
#57888=CARTESIAN_POINT('Ctrl Pts',(3.00954349196179,0.158333333333334,10.0473018664685));
#57889=CARTESIAN_POINT('Ctrl Pts',(3.02984981618038,0.319434907277167,10.0500837393884));
#57890=CARTESIAN_POINT('Ctrl Pts',(3.09896529592856,0.636309800095206,10.0815496804376));
#57891=CARTESIAN_POINT('Ctrl Pts',(3.14683395585149,0.79477268400084,10.1083552146057));
#57892=CARTESIAN_POINT('Ctrl Pts',(3.26328889377515,1.06847604194515,10.1849734474866));
#57893=CARTESIAN_POINT('Ctrl Pts',(3.32322027641433,1.18514270861185,10.226698532237));
#57894=CARTESIAN_POINT('Ctrl Pts',(3.39267401414626,1.30000000000011,10.276983507709));
#57895=CARTESIAN_POINT('Ctrl Pts',(3.25806285817532,-1.30000000000024,10.4292319482507));
#57896=CARTESIAN_POINT('Ctrl Pts',(3.20507339136947,-1.18514270861195,10.3614091950932));
#57897=CARTESIAN_POINT('Ctrl Pts',(3.16003000207498,-1.0684760419452,10.3036861052959));
#57898=CARTESIAN_POINT('Ctrl Pts',(3.07432779056413,-0.794772684000852,
10.1936664631924));
#57899=CARTESIAN_POINT('Ctrl Pts',(3.03856351369519,-0.636309800095197,
10.1527214947036));
#57900=CARTESIAN_POINT('Ctrl Pts',(2.99824596803585,-0.319434907277159,
10.0901842798058));
#57901=CARTESIAN_POINT('Ctrl Pts',(2.99178541067131,-0.158333333333333,
10.0731598884183));
#57902=CARTESIAN_POINT('Ctrl Pts',(3.0061134803473,0.158333333333334,10.0581917222558));
#57903=CARTESIAN_POINT('Ctrl Pts',(3.02637472769607,0.319434907277167,10.0609469829295));
#57904=CARTESIAN_POINT('Ctrl Pts',(3.0969517540897,0.636309800095206,10.0915712362213));
#57905=CARTESIAN_POINT('Ctrl Pts',(3.14699300261571,0.79477268400084,10.1170118814022));
#57906=CARTESIAN_POINT('Ctrl Pts',(3.26484306624898,1.06847604194515,10.1931031343167));
#57907=CARTESIAN_POINT('Ctrl Pts',(3.3251192814113,1.18514270861185,10.2348322744656));
#57908=CARTESIAN_POINT('Ctrl Pts',(3.39465878596432,1.30000000000011,10.2853534708356));
#57909=CARTESIAN_POINT('Ctrl Pts',(3.26356969889503,-1.30000000000025,10.4401936173531));
#57910=CARTESIAN_POINT('Ctrl Pts',(3.21329092939248,-1.18514270861195,10.3734371595662));
#57911=CARTESIAN_POINT('Ctrl Pts',(3.16968495310836,-1.0684760419452,10.3168412032106));
#57912=CARTESIAN_POINT('Ctrl Pts',(3.08436191176865,-0.794772684000854,
10.2095660129541));
#57913=CARTESIAN_POINT('Ctrl Pts',(3.04371183747672,-0.636309800095199,
10.1712622580596));
#57914=CARTESIAN_POINT('Ctrl Pts',(3.00095575774754,-0.31943490727716,10.1102671958419));
#57915=CARTESIAN_POINT('Ctrl Pts',(2.99406129097652,-0.158333333333333,
10.09235461781));
#57916=CARTESIAN_POINT('Ctrl Pts',(3.00853841930703,0.158333333333334,10.0773036860582));
#57917=CARTESIAN_POINT('Ctrl Pts',(3.02932442025788,0.319434907277166,10.0810031003646));
#57918=CARTESIAN_POINT('Ctrl Pts',(3.10276218112927,0.636309800095207,10.1096340251586));
#57919=CARTESIAN_POINT('Ctrl Pts',(3.15833123374125,0.794772684000843,10.13149710373));
#57920=CARTESIAN_POINT('Ctrl Pts',(3.27575915332341,1.06847604194515,10.2048959093763));
#57921=CARTESIAN_POINT('Ctrl Pts',(3.33440348949289,1.18514270861185,10.2457583004224));
#57922=CARTESIAN_POINT('Ctrl Pts',(3.40086196657799,1.30000000000011,10.295711459244));
#57923=CARTESIAN_POINT('Ctrl Pts',(3.27142362945863,-1.30000000000024,10.4564287702393));
#57924=CARTESIAN_POINT('Ctrl Pts',(3.22363852910097,-1.18514270861195,10.3923648793724));
#57925=CARTESIAN_POINT('Ctrl Pts',(3.18171939699315,-1.0684760419452,10.3378877549538));
#57926=CARTESIAN_POINT('Ctrl Pts',(3.09842937607048,-0.794772684000849,
10.2341820477573));
#57927=CARTESIAN_POINT('Ctrl Pts',(3.05634439996193,-0.636309800095195,
10.1964809634167));
#57928=CARTESIAN_POINT('Ctrl Pts',(3.01277478602804,-0.319434907277158,
10.1364512789006));
#57929=CARTESIAN_POINT('Ctrl Pts',(3.00454466836801,-0.158333333333332,
10.1179985536727));
#57930=CARTESIAN_POINT('Ctrl Pts',(3.01907920995353,0.158333333333334,10.1028653588534));
#57931=CARTESIAN_POINT('Ctrl Pts',(3.0409919197028,0.319434907277166,10.1072385910851));
#57932=CARTESIAN_POINT('Ctrl Pts',(3.11590270810618,0.636309800095204,10.1342967326359));
#57933=CARTESIAN_POINT('Ctrl Pts',(3.17432978460092,0.794772684000836,10.1542963989277));
#57934=CARTESIAN_POINT('Ctrl Pts',(3.28991423038207,1.06847604194514,10.2240301459796));
#57935=CARTESIAN_POINT('Ctrl Pts',(3.34665398616072,1.18514270861184,10.2630161354823));
#57936=CARTESIAN_POINT('Ctrl Pts',(3.41010127396518,1.3000000000001,10.310802959279));
#57937=CARTESIAN_POINT('Ctrl Pts',(3.27796208619403,-1.30000000000025,10.4698652030683));
#57938=CARTESIAN_POINT('Ctrl Pts',(3.23176481591554,-1.18514270861195,10.4080730465707));
#57939=CARTESIAN_POINT('Ctrl Pts',(3.19109466270881,-1.0684760419452,10.3551662448441));
#57940=CARTESIAN_POINT('Ctrl Pts',(3.10990721889679,-0.794772684000851,
10.2534678959159));
#57941=CARTESIAN_POINT('Ctrl Pts',(3.06857338381887,-0.636309800095197,
10.2143229029676));
#57942=CARTESIAN_POINT('Ctrl Pts',(3.0247851677372,-0.319434907277159,10.1545065948969));
#57943=CARTESIAN_POINT('Ctrl Pts',(3.01454525909152,-0.158333333333332,
10.1365625803566));
#57944=CARTESIAN_POINT('Ctrl Pts',(3.02864087085784,0.158333333333334,10.121803258227));
#57945=CARTESIAN_POINT('Ctrl Pts',(3.05147554439313,0.319434907277166,10.1266183922667));
#57946=CARTESIAN_POINT('Ctrl Pts',(3.12703262374841,0.636309800095204,10.1530499316631));
#57947=CARTESIAN_POINT('Ctrl Pts',(3.18705715886167,0.794772684000839,10.1723497025203));
#57948=CARTESIAN_POINT('Ctrl Pts',(3.3008563485775,1.06847604194514,10.2398340350002));
#57949=CARTESIAN_POINT('Ctrl Pts',(3.35605604577011,1.18514270861185,10.27754874129));
#57950=CARTESIAN_POINT('Ctrl Pts',(3.4171959876029,1.3000000000001,10.3237666868799));
#57951=CARTESIAN_POINT('Ctrl Pts',(3.28607792754349,-1.30000000000025,10.489640941086));
#57952=CARTESIAN_POINT('Ctrl Pts',(3.24218111798405,-1.18514270861195,10.4313369990907));
#57953=CARTESIAN_POINT('Ctrl Pts',(3.20343144405725,-1.0684760419452,10.3807831278332));
#57954=CARTESIAN_POINT('Ctrl Pts',(3.12580285843302,-0.794772684000849,
10.2818977857617));
#57955=CARTESIAN_POINT('Ctrl Pts',(3.08608263838369,-0.636309800095196,
10.2404042408254));
#57956=CARTESIAN_POINT('Ctrl Pts',(3.04321031720232,-0.319434907277159,
10.1799842860208));
#57957=CARTESIAN_POINT('Ctrl Pts',(3.03091044242816,-0.158333333333332,
10.1620145105244));
#57958=CARTESIAN_POINT('Ctrl Pts',(3.04590331244293,0.158333333333334,10.1463791141261));
#57959=CARTESIAN_POINT('Ctrl Pts',(3.07216452409039,0.319434907277166,10.1498515511517));
#57960=CARTESIAN_POINT('Ctrl Pts',(3.14767740070571,0.636309800095205,10.1761051872238));
#57961=CARTESIAN_POINT('Ctrl Pts',(3.20558241578882,0.794772684000837,10.1983580205055));
#57962=CARTESIAN_POINT('Ctrl Pts',(3.31561037222147,1.06847604194514,10.2633608929864));
#57963=CARTESIAN_POINT('Ctrl Pts',(3.36876295429219,1.18514270861185,10.298899079907));
#57964=CARTESIAN_POINT('Ctrl Pts',(3.42744109303151,1.30000000000011,10.3418381188451));
#57965=CARTESIAN_POINT('Ctrl Pts',(3.29502533151816,-1.30000000000025,10.5123524713943));
#57966=CARTESIAN_POINT('Ctrl Pts',(3.25382565282047,-1.18514270861195,10.4577554197642));
#57967=CARTESIAN_POINT('Ctrl Pts',(3.21726195101644,-1.0684760419452,10.4097280550216));
#57968=CARTESIAN_POINT('Ctrl Pts',(3.143502519354,-0.794772684000853,10.3139525255965));
#57969=CARTESIAN_POINT('Ctrl Pts',(3.10460687574095,-0.636309800095195,
10.2706384477954));
#57970=CARTESIAN_POINT('Ctrl Pts',(3.06356477871524,-0.319434907277157,
10.2087826959084));
#57971=CARTESIAN_POINT('Ctrl Pts',(3.05174093240499,-0.158333333333332,
10.188339847756));
#57972=CARTESIAN_POINT('Ctrl Pts',(3.06722648156504,0.158333333333334,10.1722176724411));
#57973=CARTESIAN_POINT('Ctrl Pts',(3.0936447643894,0.319434907277168,10.1775056433325));
#57974=CARTESIAN_POINT('Ctrl Pts',(3.16804494235512,0.636309800095206,10.2045513684504));
#57975=CARTESIAN_POINT('Ctrl Pts',(3.22532456748403,0.794772684000835,10.2285080909687));
#57976=CARTESIAN_POINT('Ctrl Pts',(3.33162160566429,1.06847604194514,10.2904224485944));
#57977=CARTESIAN_POINT('Ctrl Pts',(3.3825688942346,1.18514270861184,10.3235343192389));
#57978=CARTESIAN_POINT('Ctrl Pts',(3.43845142224042,1.30000000000011,10.3629576292649));
#57979=CARTESIAN_POINT('Ctrl Pts',(3.30450367753543,-1.30000000000025,10.5347011036464));
#57980=CARTESIAN_POINT('Ctrl Pts',(3.2653523505081,-1.18514270861195,10.4844098414235));
#57981=CARTESIAN_POINT('Ctrl Pts',(3.23053973946106,-1.0684760419452,10.4393268926439));
#57982=CARTESIAN_POINT('Ctrl Pts',(3.1601389455751,-0.794772684000851,10.3472085081238));
#57983=CARTESIAN_POINT('Ctrl Pts',(3.12273813965249,-0.636309800095196,
10.3015948945104));
#57984=CARTESIAN_POINT('Ctrl Pts',(3.08323596962934,-0.319434907277158,
10.2386328801667));
#57985=CARTESIAN_POINT('Ctrl Pts',(3.07090138700804,-0.158333333333333,
10.2165712937593));
#57986=CARTESIAN_POINT('Ctrl Pts',(3.08702512194723,0.158333333333334,10.1998384592567));
#57987=CARTESIAN_POINT('Ctrl Pts',(3.11490498355869,0.319434907277169,10.205802664897));
#57988=CARTESIAN_POINT('Ctrl Pts',(3.18842831382349,0.636309800095208,10.233386726658));
#57989=CARTESIAN_POINT('Ctrl Pts',(3.24412642596474,0.794772684000837,10.2598651214132));
#57990=CARTESIAN_POINT('Ctrl Pts',(3.34662974959848,1.06847604194514,10.3185985123408));
#57991=CARTESIAN_POINT('Ctrl Pts',(3.39549307711668,1.18514270861185,10.3490899716152));
#57992=CARTESIAN_POINT('Ctrl Pts',(3.44884984147448,1.30000000000011,10.384649381518));
#57993=CARTESIAN_POINT('Ctrl Pts',(3.31134556628304,-1.30000000000025,10.555306793775));
#57994=CARTESIAN_POINT('Ctrl Pts',(3.27421412686849,-1.18514270861196,10.5085498757349));
#57995=CARTESIAN_POINT('Ctrl Pts',(3.241079812679,-1.06847604194521,10.4658911880933));
#57996=CARTESIAN_POINT('Ctrl Pts',(3.17376707729655,-0.794772684000857,
10.3768088178691));
#57997=CARTESIAN_POINT('Ctrl Pts',(3.1373310728862,-0.6363098000952,10.329485060397));
#57998=CARTESIAN_POINT('Ctrl Pts',(3.09935867807212,-0.319434907277159,
10.2654171552566));
#57999=CARTESIAN_POINT('Ctrl Pts',(3.0872424959219,-0.158333333333333,10.2413968868924));
#58000=CARTESIAN_POINT('Ctrl Pts',(3.10377833472793,0.158333333333334,10.2242936402102));
#58001=CARTESIAN_POINT('Ctrl Pts',(3.13175556627714,0.319434907277168,10.2318950276049));
#58002=CARTESIAN_POINT('Ctrl Pts',(3.20478477155487,0.636309800095208,10.2597308470479));
#58003=CARTESIAN_POINT('Ctrl Pts',(3.2606917912936,0.794772684000841,10.286994013888));
#58004=CARTESIAN_POINT('Ctrl Pts',(3.3604446389725,1.06847604194515,10.3425115054252));
#58005=CARTESIAN_POINT('Ctrl Pts',(3.40751986583463,1.18514270861185,10.3707253370665));
#58006=CARTESIAN_POINT('Ctrl Pts',(3.458491008006,1.30000000000011,10.4031215353883));
#58007=CARTESIAN_POINT('Ctrl Pts',(3.31769888764463,-1.30000000000025,10.5725971040921));
#58008=CARTESIAN_POINT('Ctrl Pts',(3.28202446624183,-1.18514270861195,10.5290890206369));
#58009=CARTESIAN_POINT('Ctrl Pts',(3.25011584783553,-1.06847604194521,10.4886833545695));
#58010=CARTESIAN_POINT('Ctrl Pts',(3.18510031428796,-0.794772684000854,
10.4025053876304));
#58011=CARTESIAN_POINT('Ctrl Pts',(3.14935000680282,-0.636309800095199,
10.3538691897764));
#58012=CARTESIAN_POINT('Ctrl Pts',(3.11280902090405,-0.31943490727716,10.288776895608));
#58013=CARTESIAN_POINT('Ctrl Pts',(3.10139537328697,-0.158333333333333,
10.2626576970449));
#58014=CARTESIAN_POINT('Ctrl Pts',(3.11834904634676,0.158333333333334,10.245178008912));
#58015=CARTESIAN_POINT('Ctrl Pts',(3.14625294407796,0.319434907277168,10.2542881797259));
#58016=CARTESIAN_POINT('Ctrl Pts',(3.21827130046734,0.636309800095208,10.2828169064337));
#58017=CARTESIAN_POINT('Ctrl Pts',(3.27332792887522,0.79477268400084,10.3116295963842));
#58018=CARTESIAN_POINT('Ctrl Pts',(3.37062679205695,1.06847604194515,10.3644450457924));
#58019=CARTESIAN_POINT('Ctrl Pts',(3.41636433385336,1.18514270861185,10.3905247514617));
#58020=CARTESIAN_POINT('Ctrl Pts',(3.46572234485302,1.30000000000012,10.4198223117566));
#58021=CARTESIAN_POINT('Ctrl Pts',(3.32402656077166,-1.30000000000025,10.5898959986511));
#58022=CARTESIAN_POINT('Ctrl Pts',(3.29037048057002,-1.18514270861195,10.5492220550332));
#58023=CARTESIAN_POINT('Ctrl Pts',(3.25998575361421,-1.06847604194521,10.5108491154506));
#58024=CARTESIAN_POINT('Ctrl Pts',(3.19734843633234,-0.794772684000856,
10.4275157281707));
#58025=CARTESIAN_POINT('Ctrl Pts',(3.16145626521804,-0.636309800095199,
10.3781493048116));
#58026=CARTESIAN_POINT('Ctrl Pts',(3.12549096178903,-0.31943490727716,10.3127222436558));
#58027=CARTESIAN_POINT('Ctrl Pts',(3.11386317686832,-0.158333333333333,
10.2853097158677));
#58028=CARTESIAN_POINT('Ctrl Pts',(3.13122089061224,0.158333333333334,10.267482774936));
#58029=CARTESIAN_POINT('Ctrl Pts',(3.15986025444291,0.319434907277167,10.2774327625591));
#58030=CARTESIAN_POINT('Ctrl Pts',(3.23188702270569,0.636309800095208,10.3058053704956));
#58031=CARTESIAN_POINT('Ctrl Pts',(3.28715017080431,0.794772684000841,10.3352736952322));
#58032=CARTESIAN_POINT('Ctrl Pts',(3.38233829455662,1.06847604194515,10.385099208329));
#58033=CARTESIAN_POINT('Ctrl Pts',(3.42665634566863,1.18514270861185,10.4091142608124));
#58034=CARTESIAN_POINT('Ctrl Pts',(3.47408903618788,1.30000000000011,10.4355767473769));
#58035=CARTESIAN_POINT('Ctrl Pts',(3.32983519550131,-1.30000000000025,10.6075611244657));
#58036=CARTESIAN_POINT('Ctrl Pts',(3.29686746725483,-1.18514270861196,10.5706822971744));
#58037=CARTESIAN_POINT('Ctrl Pts',(3.26722319807112,-1.06847604194521,10.5349111259825));
#58038=CARTESIAN_POINT('Ctrl Pts',(3.2064168612317,-0.794772684000859,10.4548314717062));
#58039=CARTESIAN_POINT('Ctrl Pts',(3.1720371497533,-0.6363098000952,10.4035791334109));
#58040=CARTESIAN_POINT('Ctrl Pts',(3.13770761580401,-0.31943490727716,10.3370342383692));
#58041=CARTESIAN_POINT('Ctrl Pts',(3.12659304393993,-0.158333333333333,
10.3077270416474));
#58042=CARTESIAN_POINT('Ctrl Pts',(3.14448954447489,0.158333333333335,10.2894528640902));
#58043=CARTESIAN_POINT('Ctrl Pts',(3.17330341630422,0.319434907277168,10.3006888317874));
#58044=CARTESIAN_POINT('Ctrl Pts',(3.24448851661404,0.636309800095208,10.3295971513818));
#58045=CARTESIAN_POINT('Ctrl Pts',(3.2988649868747,0.794772684000842,10.3606116427013));
#58046=CARTESIAN_POINT('Ctrl Pts',(3.39169722187798,1.06847604194515,10.4076557293263));
#58047=CARTESIAN_POINT('Ctrl Pts',(3.43473197837859,1.18514270861185,10.429500999216));
#58048=CARTESIAN_POINT('Ctrl Pts',(3.4806178566202,1.30000000000011,10.4528278970506));
#58049=CARTESIAN_POINT('Ctrl Pts',(3.33543431689412,-1.30000000000026,10.6253660208351));
#58050=CARTESIAN_POINT('Ctrl Pts',(3.30447387826058,-1.18514270861196,10.5913293433328));
#58051=CARTESIAN_POINT('Ctrl Pts',(3.27638596789649,-1.06847604194521,10.557568389007));
#58052=CARTESIAN_POINT('Ctrl Pts',(3.21813339093802,-0.794772684000854,
10.4802108063544));
#58053=CARTESIAN_POINT('Ctrl Pts',(3.18404962061072,-0.6363098000952,10.4279113109503));
#58054=CARTESIAN_POINT('Ctrl Pts',(3.15026714188066,-0.319434907277161,
10.361072512131));
#58055=CARTESIAN_POINT('Ctrl Pts',(3.13850778186067,-0.158333333333333,
10.3308077811648));
#58056=CARTESIAN_POINT('Ctrl Pts',(3.15655965464604,0.158333333333334,10.3123911489482));
#58057=CARTESIAN_POINT('Ctrl Pts',(3.18598322614092,0.319434907277166,10.3245779265405));
#58058=CARTESIAN_POINT('Ctrl Pts',(3.25732570813374,0.636309800095207,10.353213507159));
#58059=CARTESIAN_POINT('Ctrl Pts',(3.31244332438267,0.794772684000842,10.3844471357686));
#58060=CARTESIAN_POINT('Ctrl Pts',(3.40324104275787,1.06847604194515,10.4284399262086));
#58061=CARTESIAN_POINT('Ctrl Pts',(3.44478755173034,1.18514270861186,10.4482767546045));
#58062=CARTESIAN_POINT('Ctrl Pts',(3.48857760177768,1.30000000000012,10.4689075625085));
#58063=CARTESIAN_POINT('Ctrl Pts',(3.34094149524622,-1.30000000000025,10.6432126996063));
#58064=CARTESIAN_POINT('Ctrl Pts',(3.31096178439977,-1.18514270861195,10.6127392800863));
#58065=CARTESIAN_POINT('Ctrl Pts',(3.28373855848769,-1.0684760419452,10.5814796933298));
#58066=CARTESIAN_POINT('Ctrl Pts',(3.22721549227442,-0.794772684000855,
10.5074475908752));
#58067=CARTESIAN_POINT('Ctrl Pts',(3.19385314783236,-0.6363098000952,10.4538609714195));
#58068=CARTESIAN_POINT('Ctrl Pts',(3.16133319050392,-0.319434907277161,
10.3862178147945));
#58069=CARTESIAN_POINT('Ctrl Pts',(3.15012119231218,-0.158333333333333,
10.3540840714003));
#58070=CARTESIAN_POINT('Ctrl Pts',(3.16878216455365,0.158333333333334,10.3351886489903));
#58071=CARTESIAN_POINT('Ctrl Pts',(3.19860862575582,0.319434907277166,10.3484737780535));
#58072=CARTESIAN_POINT('Ctrl Pts',(3.26923437586041,0.636309800095207,10.3775329750586));
#58073=CARTESIAN_POINT('Ctrl Pts',(3.32327179259272,0.794772684000843,10.4104342210879));
#58074=CARTESIAN_POINT('Ctrl Pts',(3.4120120682439,1.06847604194515,10.4514071685875));
#58075=CARTESIAN_POINT('Ctrl Pts',(3.45249543045058,1.18514270861185,10.4689059981687));
#58076=CARTESIAN_POINT('Ctrl Pts',(3.49504977768584,1.30000000000011,10.4861679865556));
#58077=CARTESIAN_POINT('Ctrl Pts',(3.34862517899029,-1.30000000000025,10.666765726311));
#58078=CARTESIAN_POINT('Ctrl Pts',(3.32059598526539,-1.18514270861196,10.6405999286535));
#58079=CARTESIAN_POINT('Ctrl Pts',(3.29494534462785,-1.06847604194521,10.6123835725847));
#58080=CARTESIAN_POINT('Ctrl Pts',(3.24118216682178,-0.794772684000855,
10.5424609452606));
#58081=CARTESIAN_POINT('Ctrl Pts',(3.20848037172561,-0.6363098000952,10.4873290346525));
#58082=CARTESIAN_POINT('Ctrl Pts',(3.17698900635549,-0.31943490727716,10.4190869541489));
#58083=CARTESIAN_POINT('Ctrl Pts',(3.16568642237986,-0.158333333333333,
10.3850813153639));
#58084=CARTESIAN_POINT('Ctrl Pts',(3.18435626144325,0.158333333333334,10.3661584983787));
#58085=CARTESIAN_POINT('Ctrl Pts',(3.21391244753801,0.319434907277167,10.3815490559967));
#58086=CARTESIAN_POINT('Ctrl Pts',(3.28428077549263,0.636309800095208,10.410619885086));
#58087=CARTESIAN_POINT('Ctrl Pts',(3.33933815331492,0.794772684000841,10.4438131317773));
#58088=CARTESIAN_POINT('Ctrl Pts',(3.42584267425899,1.06847604194515,10.4803480902833));
#58089=CARTESIAN_POINT('Ctrl Pts',(3.46469322031126,1.18514270861186,10.4948905487474));
#58090=CARTESIAN_POINT('Ctrl Pts',(3.50494971060752,1.30000000000012,10.5081608358921));
#58091=CARTESIAN_POINT('Ctrl Pts',(3.35477242854431,-1.30000000000025,10.6913545086937));
#58092=CARTESIAN_POINT('Ctrl Pts',(3.32803258482394,-1.18514270861196,10.6699233907188));
#58093=CARTESIAN_POINT('Ctrl Pts',(3.30354326255944,-1.06847604194521,10.6450206000984));
#58094=CARTESIAN_POINT('Ctrl Pts',(3.2521671838347,-0.794772684000857,10.579469913662));
#58095=CARTESIAN_POINT('Ctrl Pts',(3.22070121255191,-0.6363098000952,10.5224626389412));
#58096=CARTESIAN_POINT('Ctrl Pts',(3.19080582191474,-0.31943490727716,10.4532693753533));
#58097=CARTESIAN_POINT('Ctrl Pts',(3.17971659705789,-0.158333333333333,
10.417212370891));
#58098=CARTESIAN_POINT('Ctrl Pts',(3.19929932435408,0.158333333333335,10.3975993255158));
#58099=CARTESIAN_POINT('Ctrl Pts',(3.22998407396361,0.319434907277168,10.4139884899421));
#58100=CARTESIAN_POINT('Ctrl Pts',(3.29974200260255,0.636309800095208,10.4433430050657));
#58101=CARTESIAN_POINT('Ctrl Pts',(3.3532409800158,0.794772684000841,10.4788196557371));
#58102=CARTESIAN_POINT('Ctrl Pts',(3.43725631206308,1.06847604194515,10.5111268387956));
#58103=CARTESIAN_POINT('Ctrl Pts',(3.47484407697495,1.18514270861185,10.5224366375833));
#58104=CARTESIAN_POINT('Ctrl Pts',(3.51365248263028,1.30000000000012,10.5310716527117));
#58105=CARTESIAN_POINT('Ctrl Pts',(3.36577222422768,-1.30000000000026,10.7269652643744));
#58106=CARTESIAN_POINT('Ctrl Pts',(3.34162487994577,-1.18514270861196,10.7121939560135));
#58107=CARTESIAN_POINT('Ctrl Pts',(3.31912207672054,-1.06847604194521,10.6921008331891));
#58108=CARTESIAN_POINT('Ctrl Pts',(3.27093531843018,-0.794772684000855,
10.6333872438135));
#58109=CARTESIAN_POINT('Ctrl Pts',(3.23925223091895,-0.636309800095199,
10.5749795322508));
#58110=CARTESIAN_POINT('Ctrl Pts',(3.21075933021502,-0.319434907277159,
10.5050547005001));
#58111=CARTESIAN_POINT('Ctrl Pts',(3.20062822260473,-0.158333333333333,
10.4654774372491));
#58112=CARTESIAN_POINT('Ctrl Pts',(3.22074425502184,0.158333333333334,10.4454751695304));
#58113=CARTESIAN_POINT('Ctrl Pts',(3.25098152631975,0.319434907277168,10.4650006098656));
#58114=CARTESIAN_POINT('Ctrl Pts',(3.32046943854635,0.636309800095208,10.4942832028526));
#58115=CARTESIAN_POINT('Ctrl Pts',(3.37540064930299,0.794772684000839,10.5302830665368));
#58116=CARTESIAN_POINT('Ctrl Pts',(3.45624605781512,1.06847604194515,10.5558276779446));
#58117=CARTESIAN_POINT('Ctrl Pts',(3.49151207624827,1.18514270861185,10.5626262465742));
#58118=CARTESIAN_POINT('Ctrl Pts',(3.52704913138729,1.30000000000012,10.5651660680762));
#58119=CARTESIAN_POINT('Ctrl Pts',(3.37465670933942,-1.30000000000025,10.7639426884239));
#58120=CARTESIAN_POINT('Ctrl Pts',(3.35156199955871,-1.18514270861196,10.7568205400723));
#58121=CARTESIAN_POINT('Ctrl Pts',(3.33024799136158,-1.06847604194521,10.7420448903889));
#58122=CARTESIAN_POINT('Ctrl Pts',(3.28512214545966,-0.794772684000864,
10.6902290646073));
#58123=CARTESIAN_POINT('Ctrl Pts',(3.25658204085502,-0.636309800095202,
10.6281861136521));
#58124=CARTESIAN_POINT('Ctrl Pts',(3.23011273411839,-0.31943490727716,10.5571834304215));
#58125=CARTESIAN_POINT('Ctrl Pts',(3.21894204378883,-0.158333333333334,
10.5155650325798));
#58126=CARTESIAN_POINT('Ctrl Pts',(3.23986811073716,0.158333333333336,10.494972413652));
#58127=CARTESIAN_POINT('Ctrl Pts',(3.27199560830785,0.319434907277173,10.5158512738659));
#58128=CARTESIAN_POINT('Ctrl Pts',(3.34102719092835,0.636309800095214,10.5452075378715));
#58129=CARTESIAN_POINT('Ctrl Pts',(3.39431511704226,0.794772684000845,10.5840586607155));
#58130=CARTESIAN_POINT('Ctrl Pts',(3.472037879555,1.06847604194515,10.6028389087067));
#58131=CARTESIAN_POINT('Ctrl Pts',(3.50562864900718,1.18514270861185,10.6046586260853));
#58132=CARTESIAN_POINT('Ctrl Pts',(3.53916688393195,1.30000000000011,10.6001687873637));
#58133=CARTESIAN_POINT('Ctrl Pts',(3.38277473801816,-1.30000000000025,10.7960140500224));
#58134=CARTESIAN_POINT('Ctrl Pts',(3.36171527708658,-1.18514270861195,10.7948103933562));
#58135=CARTESIAN_POINT('Ctrl Pts',(3.34188342069616,-1.06847604194521,10.7843745616666));
#58136=CARTESIAN_POINT('Ctrl Pts',(3.29890387715655,-0.794772684000861,
10.7389375315884));
#58137=CARTESIAN_POINT('Ctrl Pts',(3.26941563404066,-0.636309800095202,
10.6762284222361));
#58138=CARTESIAN_POINT('Ctrl Pts',(3.24399580987047,-0.319434907277161,
10.6047768627138));
#58139=CARTESIAN_POINT('Ctrl Pts',(3.23409109017862,-0.158333333333334,
10.559888104658));
#58140=CARTESIAN_POINT('Ctrl Pts',(3.2560330799295,0.158333333333335,10.5386146162028));
#58141=CARTESIAN_POINT('Ctrl Pts',(3.28844573931014,0.31943490727717,10.5617080178589));
#58142=CARTESIAN_POINT('Ctrl Pts',(3.3574070174534,0.636309800095212,10.5908900205671));
#58143=CARTESIAN_POINT('Ctrl Pts',(3.41100341783752,0.794772684000845,10.6308930828505));
#58144=CARTESIAN_POINT('Ctrl Pts',(3.48642152170975,1.06847604194515,10.6434518917354));
#58145=CARTESIAN_POINT('Ctrl Pts',(3.5184541323885,1.18514270861186,10.6410018315667));
#58146=CARTESIAN_POINT('Ctrl Pts',(3.54987365109589,1.30000000000012,10.6306654682128));
#58147=CARTESIAN_POINT('Ctrl Pts',(3.38626628437866,-1.30000000000025,10.8115186948131));
#58148=CARTESIAN_POINT('Ctrl Pts',(3.36582717777872,-1.18514270861195,10.8133605040441));
#58149=CARTESIAN_POINT('Ctrl Pts',(3.3465333662151,-1.06847604194521,10.8050994622387));
#58150=CARTESIAN_POINT('Ctrl Pts',(3.30460666243877,-0.79477268400086,10.7626751960902));
#58151=CARTESIAN_POINT('Ctrl Pts',(3.2754688410601,-0.636309800095203,10.699115115923));
#58152=CARTESIAN_POINT('Ctrl Pts',(3.25087387028672,-0.319434907277163,
10.6272400354614));
#58153=CARTESIAN_POINT('Ctrl Pts',(3.24153842421982,-0.158333333333334,
10.5808270561062));
#58154=CARTESIAN_POINT('Ctrl Pts',(3.26376129942525,0.158333333333336,10.5593729013938));
#58155=CARTESIAN_POINT('Ctrl Pts',(3.29598529121409,0.31943490727717,10.583731898213));
#58156=CARTESIAN_POINT('Ctrl Pts',(3.36449073576851,0.636309800095213,10.6131282163632));
#58157=CARTESIAN_POINT('Ctrl Pts',(3.417724398162,0.794772684000848,10.6540551173811));
#58158=CARTESIAN_POINT('Ctrl Pts',(3.49220667372963,1.06847604194516,10.6635405170809));
#58159=CARTESIAN_POINT('Ctrl Pts',(3.5237435755897,1.18514270861186,10.6588825891453));
#58160=CARTESIAN_POINT('Ctrl Pts',(3.55457676205692,1.30000000000012,10.6454608552128));
#58161=CARTESIAN_POINT('Ctrl Pts',(3.38769780288249,-1.30000000000025,10.8176960564688));
#58162=CARTESIAN_POINT('Ctrl Pts',(3.36755620151121,-1.18514270861195,10.8207223471244));
#58163=CARTESIAN_POINT('Ctrl Pts',(3.34850087888628,-1.06847604194521,10.813315256739));
#58164=CARTESIAN_POINT('Ctrl Pts',(3.30698879283185,-0.79477268400086,10.7721001987698));
#58165=CARTESIAN_POINT('Ctrl Pts',(3.27788009191905,-0.636309800095203,
10.7082749221034));
#58166=CARTESIAN_POINT('Ctrl Pts',(3.25355472013789,-0.319434907277162,
10.6362713366291));
#58167=CARTESIAN_POINT('Ctrl Pts',(3.24441619455047,-0.158333333333334,
10.5892701532528));
#58168=CARTESIAN_POINT('Ctrl Pts',(3.266793663605,0.158333333333335,10.5677143586198));
#58169=CARTESIAN_POINT('Ctrl Pts',(3.29904752840448,0.31943490727717,10.5925071897121));
#58170=CARTESIAN_POINT('Ctrl Pts',(3.36745120503604,0.636309800095212,10.6219323865371));
#58171=CARTESIAN_POINT('Ctrl Pts',(3.42058911211841,0.794772684000847,10.6631913608502));
#58172=CARTESIAN_POINT('Ctrl Pts',(3.49466491110876,1.06847604194515,10.6714706894569));
#58173=CARTESIAN_POINT('Ctrl Pts',(3.52596499017303,1.18514270861186,10.6659577209332));
#58174=CARTESIAN_POINT('Ctrl Pts',(3.55650047969752,1.30000000000012,10.6513479693114));
#58175=CARTESIAN_POINT('Ctrl Pts',(3.39109987683895,-1.30000000000025,10.8350139320941));
#58176=CARTESIAN_POINT('Ctrl Pts',(3.37125853817352,-1.18514270861195,10.8416206060688));
#58177=CARTESIAN_POINT('Ctrl Pts',(3.35262039187588,-1.06847604194521,10.8367100040207));
#58178=CARTESIAN_POINT('Ctrl Pts',(3.31234216044733,-0.794772684000859,
10.798758319291));
#58179=CARTESIAN_POINT('Ctrl Pts',(3.28474943875151,-0.636309800095202,
10.7332931428369));
#58180=CARTESIAN_POINT('Ctrl Pts',(3.26137805267955,-0.319434907277162,
10.6608171980619));
#58181=CARTESIAN_POINT('Ctrl Pts',(3.25183148610066,-0.158333333333334,
10.6128327837711));
#58182=CARTESIAN_POINT('Ctrl Pts',(3.27458361122692,0.158333333333335,10.5910290471671));
#58183=CARTESIAN_POINT('Ctrl Pts',(3.307374631408,0.319434907277171,10.6167036041784));
#58184=CARTESIAN_POINT('Ctrl Pts',(3.37608762049819,0.636309800095212,10.6457978387865));
#58185=CARTESIAN_POINT('Ctrl Pts',(3.42976486332244,0.794772684000846,10.6874068292731));
#58186=CARTESIAN_POINT('Ctrl Pts',(3.5026472205099,1.06847604194515,10.692422154672));
#58187=CARTESIAN_POINT('Ctrl Pts',(3.5330325403784,1.18514270861186,10.6847421636972));
#58188=CARTESIAN_POINT('Ctrl Pts',(3.56225510824644,1.30000000000012,10.6672112332187));
#58189=CARTESIAN_POINT('Ctrl Pts',(3.3961039320677,-1.30000000000025,10.8566094221741));
#58190=CARTESIAN_POINT('Ctrl Pts',(3.37730930726364,-1.18514270861196,10.8673460146537));
#58191=CARTESIAN_POINT('Ctrl Pts',(3.35942825207076,-1.06847604194521,10.8654649821272));
#58192=CARTESIAN_POINT('Ctrl Pts',(3.32022996604323,-0.794772684000863,
10.8319701827806));
#58193=CARTESIAN_POINT('Ctrl Pts',(3.29209724359651,-0.636309800095203,
10.7659785582791));
#58194=CARTESIAN_POINT('Ctrl Pts',(3.26926298889969,-0.319434907277162,
10.6933358778177));
#58195=CARTESIAN_POINT('Ctrl Pts',(3.26044497555805,-0.158333333333334,
10.6433146168721));
#58196=CARTESIAN_POINT('Ctrl Pts',(3.28367719243551,0.158333333333335,10.6212189492113));
#58197=CARTESIAN_POINT('Ctrl Pts',(3.31668048625251,0.319434907277168,10.6483297640823));
#58198=CARTESIAN_POINT('Ctrl Pts',(3.38489577202755,0.636309800095211,10.6776248054219));
#58199=CARTESIAN_POINT('Ctrl Pts',(3.43761984386032,0.794772684000848,10.7208148378221));
#58200=CARTESIAN_POINT('Ctrl Pts',(3.50950537524388,1.06847604194515,10.7213304653958));
#58201=CARTESIAN_POINT('Ctrl Pts',(3.53947393670639,1.18514270861186,10.7103847949187));
#58202=CARTESIAN_POINT('Ctrl Pts',(3.56829447671692,1.30000000000011,10.6882702578935));
#58203=CARTESIAN_POINT('Ctrl Pts',(3.40212020418971,-1.30000000000024,10.8881223521638));
#58204=CARTESIAN_POINT('Ctrl Pts',(3.38389046357394,-1.18514270861195,10.9053147692767));
#58205=CARTESIAN_POINT('Ctrl Pts',(3.36664207879231,-1.0684760419452,10.9080258719001));
#58206=CARTESIAN_POINT('Ctrl Pts',(3.32906198771562,-0.794772684000856,
10.8808343278664));
#58207=CARTESIAN_POINT('Ctrl Pts',(3.30230971800406,-0.6363098000952,10.8127663703491));
#58208=CARTESIAN_POINT('Ctrl Pts',(3.28105505508516,-0.319434907277161,
10.7393933092971));
#58209=CARTESIAN_POINT('Ctrl Pts',(3.27279618739657,-0.158333333333333,
10.686782398982));
#58210=CARTESIAN_POINT('Ctrl Pts',(3.29672863406106,0.158333333333335,10.6642612576124));
#58211=CARTESIAN_POINT('Ctrl Pts',(3.32964993153132,0.319434907277167,10.6936694033216));
#58212=CARTESIAN_POINT('Ctrl Pts',(3.39816634206327,0.636309800095208,10.7225569384338));
#58213=CARTESIAN_POINT('Ctrl Pts',(3.45226798793885,0.794772684000844,10.7661248346689));
#58214=CARTESIAN_POINT('Ctrl Pts',(3.52231733001041,1.06847604194515,10.7605319396099));
#58215=CARTESIAN_POINT('Ctrl Pts',(3.5507893843304,1.18514270861185,10.7455636050312));
#58216=CARTESIAN_POINT('Ctrl Pts',(3.57741172837152,1.30000000000011,10.7180478929078));
#58217=CARTESIAN_POINT('Ctrl Pts',(3.4058272992921,-1.30000000000024,10.9069423026201));
#58218=CARTESIAN_POINT('Ctrl Pts',(3.38807550315061,-1.18514270861195,10.9279007195059));
#58219=CARTESIAN_POINT('Ctrl Pts',(3.37125653663408,-1.0684760419452,10.9333212751712));
#58220=CARTESIAN_POINT('Ctrl Pts',(3.33455638240376,-0.794772684000852,
10.9099482753785));
#58221=CARTESIAN_POINT('Ctrl Pts',(3.30823759879944,-0.636309800095197,
10.8408849121294));
#58222=CARTESIAN_POINT('Ctrl Pts',(3.28760112788311,-0.319434907277159,
10.7672871264273));
#58223=CARTESIAN_POINT('Ctrl Pts',(3.2794226920031,-0.158333333333333,10.7133022638828));
#58224=CARTESIAN_POINT('Ctrl Pts',(3.30384439390905,0.158333333333334,10.6904854093681));
#58225=CARTESIAN_POINT('Ctrl Pts',(3.3375004211861,0.319434907277167,10.7207477256399));
#58226=CARTESIAN_POINT('Ctrl Pts',(3.40573136959717,0.636309800095206,10.7497140504626));
#58227=CARTESIAN_POINT('Ctrl Pts',(3.45859257120118,0.79477268400084,10.7949182498349));
#58228=CARTESIAN_POINT('Ctrl Pts',(3.52792852763022,1.06847604194515,10.785389185721));
#58229=CARTESIAN_POINT('Ctrl Pts',(3.55620374536084,1.18514270861185,10.7675245519584));
#58230=CARTESIAN_POINT('Ctrl Pts',(3.58274121443434,1.30000000000011,10.7359200632015));
#58231=CARTESIAN_POINT('Ctrl Pts',(3.40792382026114,-1.30000000000024,10.9197225044722));
#58232=CARTESIAN_POINT('Ctrl Pts',(3.3906322726577,-1.18514270861195,10.9430989210123));
#58233=CARTESIAN_POINT('Ctrl Pts',(3.37417219529069,-1.0684760419452,10.9502776169302));
#58234=CARTESIAN_POINT('Ctrl Pts',(3.33806698632697,-0.794772684000852,
10.9294418656142));
#58235=CARTESIAN_POINT('Ctrl Pts',(3.31165271079239,-0.636309800095197,
10.859956075597));
#58236=CARTESIAN_POINT('Ctrl Pts',(3.29150406597601,-0.319434907277159,
10.7861661143519));
#58237=CARTESIAN_POINT('Ctrl Pts',(3.28383918476484,-0.158333333333333,
10.7309845243911));
#58238=CARTESIAN_POINT('Ctrl Pts',(3.30866559173632,0.158333333333334,10.7079289458231));
#58239=CARTESIAN_POINT('Ctrl Pts',(3.34233892867207,0.319434907277167,10.7390693321137));
#58240=CARTESIAN_POINT('Ctrl Pts',(3.410649428729,0.636309800095206,10.7679043872382));
#58241=CARTESIAN_POINT('Ctrl Pts',(3.46380979023611,0.79477268400084,10.8134309006136));
#58242=CARTESIAN_POINT('Ctrl Pts',(3.53249270106959,1.06847604194515,10.8014150897722));
#58243=CARTESIAN_POINT('Ctrl Pts',(3.56027544998898,1.18514270861185,10.7818767116455));
#58244=CARTESIAN_POINT('Ctrl Pts',(3.58611066068062,1.30000000000011,10.7480011546757));
#58245=CARTESIAN_POINT('',(3.53212178875801,1.2,10.6679411283038));
#58246=CARTESIAN_POINT('Ctrl Pts',(3.53212178875801,1.2,10.6679411283038));
#58247=CARTESIAN_POINT('Ctrl Pts',(3.53076600547773,1.20867356067025,10.656941710424));
#58248=CARTESIAN_POINT('Ctrl Pts',(3.52995217304133,1.21711400407322,10.6457006410991));
#58249=CARTESIAN_POINT('Ctrl Pts',(3.52771878247509,1.23357261918912,10.6243979759498));
#58250=CARTESIAN_POINT('Ctrl Pts',(3.5273107258133,1.23602988985319,10.6213028016734));
#58251=CARTESIAN_POINT('Ctrl Pts',(3.52277567166249,1.26657829400011,10.5820179245844));
#58252=CARTESIAN_POINT('Ctrl Pts',(3.5201115627438,1.28322142352916,10.5607323865177));
#58253=CARTESIAN_POINT('Ctrl Pts',(3.51702417250711,1.30000000000012,10.5396168897045));
#58254=CARTESIAN_POINT('',(3.42060206384614,0.653834841420791,10.7779856792003));
#58255=CARTESIAN_POINT('Ctrl Pts',(3.42060206386547,0.653834841420113,10.7779856792166));
#58256=CARTESIAN_POINT('Ctrl Pts',(3.43245989940398,0.718489900125914,10.7666494301781));
#58257=CARTESIAN_POINT('Ctrl Pts',(3.44115395086233,0.760264441102575,10.7582679025733));
#58258=CARTESIAN_POINT('Ctrl Pts',(3.47874216109659,0.949909181003267,10.7216567942924));
#58259=CARTESIAN_POINT('Ctrl Pts',(3.50505627305355,1.07520346740433,10.6955075414022));
#58260=CARTESIAN_POINT('Ctrl Pts',(3.53212178875801,1.2,10.6679411283038));
#58261=CARTESIAN_POINT('',(3.3184146483206,-0.653834841531101,10.8729585107664));
#58262=CARTESIAN_POINT('Ctrl Pts',(3.3184146483206,-0.653834841531098,10.8729585107664));
#58263=CARTESIAN_POINT('Ctrl Pts',(3.30612340454657,-0.575948840682229,
10.8332259573124));
#58264=CARTESIAN_POINT('Ctrl Pts',(3.29646275965704,-0.493565906078733,
10.7994009548295));
#58265=CARTESIAN_POINT('Ctrl Pts',(3.28493831203399,-0.33802586804748,10.7501065984067));
#58266=CARTESIAN_POINT('Ctrl Pts',(3.28207503415345,-0.265543988072748,
10.7324464737946));
#58267=CARTESIAN_POINT('Ctrl Pts',(3.28246020273128,-0.129635186233274,
10.7080854451719));
#58268=CARTESIAN_POINT('Ctrl Pts',(3.28485202508577,-0.066588188713728,
10.700174008646));
#58269=CARTESIAN_POINT('Ctrl Pts',(3.29435165456499,0.0594976330476124,
10.6908373400304));
#58270=CARTESIAN_POINT('Ctrl Pts',(3.30151562510345,0.122685832955994,10.6893328369104));
#58271=CARTESIAN_POINT('Ctrl Pts',(3.32176598313159,0.260008478785349,10.6937083254578));
#58272=CARTESIAN_POINT('Ctrl Pts',(3.33570383496495,0.333833694405106,10.7009899323094));
#58273=CARTESIAN_POINT('Ctrl Pts',(3.37146808014451,0.491082797991572,10.7280228209757));
#58274=CARTESIAN_POINT('Ctrl Pts',(3.39445295550189,0.574241316481935,10.749653710407));
#58275=CARTESIAN_POINT('Ctrl Pts',(3.42060206385329,0.653834841432093,10.7779856791619));
#58276=CARTESIAN_POINT('',(3.37169896859721,-1.2,10.8241062436359));
#58277=CARTESIAN_POINT('Ctrl Pts',(3.3716989685972,-1.2,10.8241062436359));
#58278=CARTESIAN_POINT('Ctrl Pts',(3.35768718230927,-1.09933264222173,10.8371421543403));
#58279=CARTESIAN_POINT('Ctrl Pts',(3.34788171370128,-1.01093493025459,10.8461501750024));
#58280=CARTESIAN_POINT('Ctrl Pts',(3.32759670212101,-0.799392291359797,
10.8646633041815));
#58281=CARTESIAN_POINT('Ctrl Pts',(3.32365825158216,-0.748331475394995,
10.8682210627876));
#58282=CARTESIAN_POINT('Ctrl Pts',(3.3184146483206,-0.653834841531101,10.8729585107664));
#58283=CARTESIAN_POINT('Ctrl Pts',(3.35750201349686,-1.3,10.6999543181825));
#58284=CARTESIAN_POINT('Ctrl Pts',(3.36058314309854,-1.28290082666877,10.7206934722446));
#58285=CARTESIAN_POINT('Ctrl Pts',(3.36310814969023,-1.26597626730214,10.7416599332655));
#58286=CARTESIAN_POINT('Ctrl Pts',(3.36677349478208,-1.23881242621742,10.7755644053774));
#58287=CARTESIAN_POINT('Ctrl Pts',(3.36768665493843,-1.23284191421401,10.7828987153576));
#58288=CARTESIAN_POINT('Ctrl Pts',(3.37058282004082,-1.21177341596379,10.8090655493132));
#58289=CARTESIAN_POINT('Ctrl Pts',(3.3708960298996,-1.20975903898414,10.8115238378433));
#58290=CARTESIAN_POINT('Ctrl Pts',(3.3716989685972,-1.2,10.8241062436359));
#58291=CARTESIAN_POINT('Origin',(0.,1.25,7.2));
#58292=CARTESIAN_POINT('Origin',(0.,1.2,7.2));
#58293=CARTESIAN_POINT('Origin',(0.,0.92691742076555,7.2));
#58294=CARTESIAN_POINT('Origin',(0.,0.653834841531101,7.2));
#58295=CARTESIAN_POINT('Origin',(0.,0.,7.2));
#58296=CARTESIAN_POINT('Origin',(0.,-0.653834841531101,7.2));
#58297=CARTESIAN_POINT('Origin',(0.,-0.926917420765551,7.2));
#58298=CARTESIAN_POINT('Origin',(0.,-1.2,7.2));
#58299=CARTESIAN_POINT('Origin',(0.,-1.25,7.2));
#58300=CARTESIAN_POINT('Ctrl Pts',(3.1537141966502,-1.30000000000047,11.1373326796344));
#58301=CARTESIAN_POINT('Ctrl Pts',(3.19010469464722,-1.1851427086121,11.1151799568439));
#58302=CARTESIAN_POINT('Ctrl Pts',(3.21244012754455,-1.06847604194528,11.089591721371));
#58303=CARTESIAN_POINT('Ctrl Pts',(3.231569433639,-0.794772684000851,11.0225410569516));
#58304=CARTESIAN_POINT('Ctrl Pts',(3.19184909016007,-0.636309800095197,
10.9649130969828));
#58305=CARTESIAN_POINT('Ctrl Pts',(3.17031238807978,-0.319434907277159,
10.8939627249912));
#58306=CARTESIAN_POINT('Ctrl Pts',(3.14286241424732,-0.158333333333332,
10.857218797395));
#58307=CARTESIAN_POINT('Ctrl Pts',(3.16838675811282,0.158333333333334,10.8349383562761));
#58308=CARTESIAN_POINT('Ctrl Pts',(3.22246485929617,0.319434907277167,10.8483292952657));
#58309=CARTESIAN_POINT('Ctrl Pts',(3.29374448453208,0.636309800095206,10.8760807149496));
#58310=CARTESIAN_POINT('Ctrl Pts',(3.36008858048819,0.79477268400084,10.9096135331648));
#58311=CARTESIAN_POINT('Ctrl Pts',(3.37703616937003,1.06847604194602,10.9476988830827));
#58312=CARTESIAN_POINT('Ctrl Pts',(3.36817625250779,1.18514270861357,10.9633184123723));
#58313=CARTESIAN_POINT('Ctrl Pts',(3.34312043552638,1.30000000000265,10.9780717341732));
#58314=CARTESIAN_POINT('Ctrl Pts',(3.14788284318891,-1.30000000000047,11.1350257766576));
#58315=CARTESIAN_POINT('Ctrl Pts',(3.18318073065629,-1.1851427086121,11.1124051525731));
#58316=CARTESIAN_POINT('Ctrl Pts',(3.20470961435297,-1.06847604194528,11.0864845546345));
#58317=CARTESIAN_POINT('Ctrl Pts',(3.22263648934064,-0.794772684000851,
11.018979188238));
#58318=CARTESIAN_POINT('Ctrl Pts',(3.18306078465209,-0.636309800095197,
10.9615168342817));
#58319=CARTESIAN_POINT('Ctrl Pts',(3.16145464956688,-0.319434907277159,
10.8905991595008));
#58320=CARTESIAN_POINT('Ctrl Pts',(3.13444040099099,-0.158333333333332,
10.8539097309809));
#58321=CARTESIAN_POINT('Ctrl Pts',(3.15982488510821,0.158333333333334,10.8318180571571));
#58322=CARTESIAN_POINT('Ctrl Pts',(3.21328105994455,0.319434907277167,10.8454018207915));
#58323=CARTESIAN_POINT('Ctrl Pts',(3.28443962792562,0.636309800095206,10.8733857734295));
#58324=CARTESIAN_POINT('Ctrl Pts',(3.35057865834427,0.794772684000841,10.9068490294079));
#58325=CARTESIAN_POINT('Ctrl Pts',(3.3687568274511,1.06847604194602,10.9453628297153));
#58326=CARTESIAN_POINT('Ctrl Pts',(3.36075240801503,1.18514270861357,10.9612527084174));
#58327=CARTESIAN_POINT('Ctrl Pts',(3.33687491330406,1.30000000000265,10.9763612687455));
#58328=CARTESIAN_POINT('Ctrl Pts',(3.13602666513719,-1.30000000000068,11.130616336331));
#58329=CARTESIAN_POINT('Ctrl Pts',(3.16922239039855,-1.18514270861229,11.1069731541362));
#58330=CARTESIAN_POINT('Ctrl Pts',(3.18921085134169,-1.06847604194545,11.0803090987668));
#58331=CARTESIAN_POINT('Ctrl Pts',(3.20487677211899,-0.794772684000972,
11.0117309753808));
#58332=CARTESIAN_POINT('Ctrl Pts',(3.1657701772128,-0.636309800095298,10.9543717086895));
#58333=CARTESIAN_POINT('Ctrl Pts',(3.14388752510033,-0.319434907277211,
10.883684741697));
#58334=CARTESIAN_POINT('Ctrl Pts',(3.11727844371661,-0.158333333333358,
10.847669131426));
#58335=CARTESIAN_POINT('Ctrl Pts',(3.1422984644438,0.15833333333336,10.8260597126675));
#58336=CARTESIAN_POINT('Ctrl Pts',(3.19482368720396,0.319434907277218,10.8396543810191));
#58337=CARTESIAN_POINT('Ctrl Pts',(3.26584498679678,0.636309800095308,10.8679775321775));
#58338=CARTESIAN_POINT('Ctrl Pts',(3.33149867825249,0.794772684000967,10.9013899895613));
#58339=CARTESIAN_POINT('Ctrl Pts',(3.35214112151248,1.06847604194619,10.9407558898041));
#58340=CARTESIAN_POINT('Ctrl Pts',(3.34585397033878,1.18514270861376,10.9571786227287));
#58341=CARTESIAN_POINT('Ctrl Pts',(3.32434431918199,1.30000000000286,10.9729840490132));
#58342=CARTESIAN_POINT('Ctrl Pts',(3.11338370685469,-1.30000000000069,11.120683044156));
#58343=CARTESIAN_POINT('Ctrl Pts',(3.14116836728438,-1.1851427086123,11.0963251324237));
#58344=CARTESIAN_POINT('Ctrl Pts',(3.15731256495897,-1.06847604194546,11.0690090454575));
#58345=CARTESIAN_POINT('Ctrl Pts',(3.16771709359208,-0.794772684000982,
10.99906944343));
#58346=CARTESIAN_POINT('Ctrl Pts',(3.1305800846218,-0.636309800095302,10.9407498665654));
#58347=CARTESIAN_POINT('Ctrl Pts',(3.10895551659859,-0.319434907277212,
10.8695500110699));
#58348=CARTESIAN_POINT('Ctrl Pts',(3.08391518852437,-0.158333333333359,
10.8339834973426));
#58349=CARTESIAN_POINT('Ctrl Pts',(3.10868004152326,0.15833333333336,10.8127199071209));
#58350=CARTESIAN_POINT('Ctrl Pts',(3.15926311797835,0.31943490727722,10.8263292826878));
#58351=CARTESIAN_POINT('Ctrl Pts',(3.22974739154896,0.636309800095311,10.855629443145));
#58352=CARTESIAN_POINT('Ctrl Pts',(3.29371057080877,0.794772684000972,10.889880846898));
#58353=CARTESIAN_POINT('Ctrl Pts',(3.31929399286086,1.0684760419462,10.9309844151448));
#58354=CARTESIAN_POINT('Ctrl Pts',(3.31661522091182,1.18514270861377,10.9482825629363));
#58355=CARTESIAN_POINT('Ctrl Pts',(3.30018356156654,1.30000000000287,10.9650866468623));
#58356=CARTESIAN_POINT('Ctrl Pts',(3.09576113927307,-1.30000000000115,11.1135336035834));
#58357=CARTESIAN_POINT('Ctrl Pts',(3.12083758156332,-1.18514270861272,11.0870492973935));
#58358=CARTESIAN_POINT('Ctrl Pts',(3.13490280767704,-1.06847604194583,11.0582957397077));
#58359=CARTESIAN_POINT('Ctrl Pts',(3.14195818158455,-0.794772684001263,
10.9866268444063));
#58360=CARTESIAN_POINT('Ctrl Pts',(3.10452754684833,-0.636309800095527,
10.9296607803433));
#58361=CARTESIAN_POINT('Ctrl Pts',(3.08238301721418,-0.319434907277325,
10.8589183599512));
#58362=CARTESIAN_POINT('Ctrl Pts',(3.05856153306589,-0.158333333333415,
10.8236494878642));
#58363=CARTESIAN_POINT('Ctrl Pts',(3.08296219079103,0.158333333333416,10.8028618150431));
#58364=CARTESIAN_POINT('Ctrl Pts',(3.1320895193213,0.319434907277332,10.8164895636833));
#58365=CARTESIAN_POINT('Ctrl Pts',(3.20209263179147,0.636309800095535,10.8466274087751));
#58366=CARTESIAN_POINT('Ctrl Pts',(3.26472168061616,0.794772684001252,10.8815622465489));
#58367=CARTESIAN_POINT('Ctrl Pts',(3.29400317768701,1.06847604194657,10.9240379528181));
#58368=CARTESIAN_POINT('Ctrl Pts',(3.29404630057274,1.18514270861419,10.9420167516264));
#58369=CARTESIAN_POINT('Ctrl Pts',(3.28145767124855,1.30000000000333,10.959588189879));
#58370=CARTESIAN_POINT('Ctrl Pts',(3.08395155918141,-1.30000000000119,11.1085139514224));
#58371=CARTESIAN_POINT('Ctrl Pts',(3.10642269462814,-1.18514270861275,11.0814385633059));
#58372=CARTESIAN_POINT('Ctrl Pts',(3.11862776653224,-1.06847604194586,11.0522016390918));
#58373=CARTESIAN_POINT('Ctrl Pts',(3.12310726374452,-0.794772684001286,
10.9796649145319));
#58374=CARTESIAN_POINT('Ctrl Pts',(3.08651157953333,-0.636309800095545,
10.9224190632179));
#58375=CARTESIAN_POINT('Ctrl Pts',(3.06452565510273,-0.319434907277333,
10.8513822824859));
#58376=CARTESIAN_POINT('Ctrl Pts',(3.04169295933292,-0.158333333333419,
10.8161325434434));
#58377=CARTESIAN_POINT('Ctrl Pts',(3.06589214051835,0.158333333333421,10.7956070164919));
#58378=CARTESIAN_POINT('Ctrl Pts',(3.11366321570065,0.319434907277342,10.8096745092449));
#58379=CARTESIAN_POINT('Ctrl Pts',(3.18343543624268,0.636309800095554,10.8402399594697));
#58380=CARTESIAN_POINT('Ctrl Pts',(3.24572403615328,0.794772684001273,10.8749119240156));
#58381=CARTESIAN_POINT('Ctrl Pts',(3.27752379286743,1.06847604194661,10.9183325711489));
#58382=CARTESIAN_POINT('Ctrl Pts',(3.27930056278751,1.18514270861422,10.9369373016276));
#58383=CARTESIAN_POINT('Ctrl Pts',(3.26908916624317,1.30000000000337,10.9553515733346));
#58384=CARTESIAN_POINT('Ctrl Pts',(3.08341596161804,-1.30000000000119,11.1082843545824));
#58385=CARTESIAN_POINT('Ctrl Pts',(3.10576966356819,-1.18514270861275,11.0811808930218));
#58386=CARTESIAN_POINT('Ctrl Pts',(3.11789072402595,-1.06847604194586,11.051921328677));
#58387=CARTESIAN_POINT('Ctrl Pts',(3.12225334961287,-0.794772684001286,
10.9793448529261));
#58388=CARTESIAN_POINT('Ctrl Pts',(3.08569374856489,-0.636309800095544,
10.9220884814296));
#58389=CARTESIAN_POINT('Ctrl Pts',(3.06371464384983,-0.319434907277333,
10.8510387599166));
#58390=CARTESIAN_POINT('Ctrl Pts',(3.04092785396088,-0.158333333333419,
10.8157887502987));
#58391=CARTESIAN_POINT('Ctrl Pts',(3.06511770359802,0.158333333333421,10.7952753476931));
#58392=CARTESIAN_POINT('Ctrl Pts',(3.1128263871204,0.319434907277341,10.8093637144019));
#58393=CARTESIAN_POINT('Ctrl Pts',(3.18258735290783,0.636309800095553,10.8399495306449));
#58394=CARTESIAN_POINT('Ctrl Pts',(3.2448599450106,0.794772684001273,10.8746102076726));
#58395=CARTESIAN_POINT('Ctrl Pts',(3.27677390434896,1.0684760419466,10.9180741625951));
#58396=CARTESIAN_POINT('Ctrl Pts',(3.27862948272818,1.18514270861422,10.9367073567007));
#58397=CARTESIAN_POINT('Ctrl Pts',(3.26852626901772,1.30000000000336,10.9551598093241));
#58398=CARTESIAN_POINT('Ctrl Pts',(3.08288070241116,-1.30000000000119,11.1080543928536));
#58399=CARTESIAN_POINT('Ctrl Pts',(3.10511696606915,-1.18514270861275,11.0809228689106));
#58400=CARTESIAN_POINT('Ctrl Pts',(3.11715401779151,-1.06847604194586,11.0516406634302));
#58401=CARTESIAN_POINT('Ctrl Pts',(3.12139979535742,-0.794772684001286,
10.9790244062912));
#58402=CARTESIAN_POINT('Ctrl Pts',(3.08487644576444,-0.636309800095544,
10.9217573025874));
#58403=CARTESIAN_POINT('Ctrl Pts',(3.06290395870727,-0.319434907277333,
10.8506948674407));
#58404=CARTESIAN_POINT('Ctrl Pts',(3.04016247600659,-0.158333333333419,
10.8154452967412));
#58405=CARTESIAN_POINT('Ctrl Pts',(3.06434307409562,0.158333333333421,10.794943901965));
#58406=CARTESIAN_POINT('Ctrl Pts',(3.11199021357481,0.319434907277341,10.8090520991058));
#58407=CARTESIAN_POINT('Ctrl Pts',(3.18173994553404,0.636309800095553,10.8396582599428));
#58408=CARTESIAN_POINT('Ctrl Pts',(3.24399568012213,0.794772684001273,10.8743087136978));
#58409=CARTESIAN_POINT('Ctrl Pts',(3.27602373403694,1.0684760419466,10.9178161103825));
#58410=CARTESIAN_POINT('Ctrl Pts',(3.27795821323474,1.18514270861422,10.9364776510779));
#58411=CARTESIAN_POINT('Ctrl Pts',(3.26796341384691,1.30000000000337,10.9549679925518));
#58412=CARTESIAN_POINT('Ctrl Pts',(3.08181165107633,-1.30000000000119,11.1075927560609));
#58413=CARTESIAN_POINT('Ctrl Pts',(3.10381413880235,-1.18514270861275,11.0804037955591));
#58414=CARTESIAN_POINT('Ctrl Pts',(3.1156837899324,-1.06847604194586,11.0510755651735));
#58415=CARTESIAN_POINT('Ctrl Pts',(3.11969617895471,-0.794772684001285,
10.9783793444991));
#58416=CARTESIAN_POINT('Ctrl Pts',(3.08324360047865,-0.636309800095544,
10.9210927847102));
#58417=CARTESIAN_POINT('Ctrl Pts',(3.06128354178067,-0.319434907277333,
10.8500058420244));
#58418=CARTESIAN_POINT('Ctrl Pts',(3.03863258335772,-0.158333333333419,
10.8147572582684));
#58419=CARTESIAN_POINT('Ctrl Pts',(3.06279464256912,0.158333333333421,10.7942798959418));
#58420=CARTESIAN_POINT('Ctrl Pts',(3.11031943612699,0.319434907277341,10.8084268192463));
#58421=CARTESIAN_POINT('Ctrl Pts',(3.18004603340595,0.636309800095553,10.8390744996214));
#58422=CARTESIAN_POINT('Ctrl Pts',(3.24226610208176,0.794772684001273,10.8737069492674));
#58423=CARTESIAN_POINT('Ctrl Pts',(3.27452197278349,1.0684760419466,10.9173017153762));
#58424=CARTESIAN_POINT('Ctrl Pts',(3.27661445517721,1.18514270861422,10.9360197102487));
#58425=CARTESIAN_POINT('Ctrl Pts',(3.26683704873562,1.30000000000336,10.9545851410903));
#58426=CARTESIAN_POINT('Ctrl Pts',(3.07950184481962,-1.30000000000118,11.1065850333065));
#58427=CARTESIAN_POINT('Ctrl Pts',(3.1010025742002,-1.18514270861275,11.0792660257947));
#58428=CARTESIAN_POINT('Ctrl Pts',(3.11251225821232,-1.06847604194586,11.0498348291874));
#58429=CARTESIAN_POINT('Ctrl Pts',(3.11602061728179,-0.794772684001284,
10.9769632979818));
#58430=CARTESIAN_POINT('Ctrl Pts',(3.07971509019369,-0.636309800095543,
10.9196417946398));
#58431=CARTESIAN_POINT('Ctrl Pts',(3.0577775182899,-0.319434907277332,10.8485068344066));
#58432=CARTESIAN_POINT('Ctrl Pts',(3.03531907925591,-0.158333333333419,
10.8132646959073));
#58433=CARTESIAN_POINT('Ctrl Pts',(3.05944102836239,0.15833333333342,10.7928391501656));
#58434=CARTESIAN_POINT('Ctrl Pts',(3.10670776553142,0.319434907277341,10.8070612599296));
#58435=CARTESIAN_POINT('Ctrl Pts',(3.17638196737474,0.636309800095552,10.8378017732288));
#58436=CARTESIAN_POINT('Ctrl Pts',(3.23851358524906,0.794772684001271,10.872409253674));
#58437=CARTESIAN_POINT('Ctrl Pts',(3.27126108509779,1.0684760419466,10.9161958468731));
#58438=CARTESIAN_POINT('Ctrl Pts',(3.27369701287854,1.18514270861422,10.9350347990276));
#58439=CARTESIAN_POINT('Ctrl Pts',(3.26439368916993,1.30000000000336,10.9537591095938));
#58440=CARTESIAN_POINT('Ctrl Pts',(3.07597350333202,-1.30000000000118,11.1050046386546));
#58441=CARTESIAN_POINT('Ctrl Pts',(3.09673378701756,-1.18514270861275,11.0774491271937));
#58442=CARTESIAN_POINT('Ctrl Pts',(3.10770797139586,-1.06847604194586,11.0478383027321));
#58443=CARTESIAN_POINT('Ctrl Pts',(3.11045268558565,-0.794772684001281,
10.9746831904049));
#58444=CARTESIAN_POINT('Ctrl Pts',(3.07433384945607,-0.636309800095541,
10.9173531191264));
#58445=CARTESIAN_POINT('Ctrl Pts',(3.0524013309648,-0.319434907277331,10.8461785054774));
#58446=CARTESIAN_POINT('Ctrl Pts',(3.03021210964003,-0.158333333333418,
10.8109786470852));
#58447=CARTESIAN_POINT('Ctrl Pts',(3.05427344270787,0.15833333333342,10.7906306695322));
#58448=CARTESIAN_POINT('Ctrl Pts',(3.10119167687428,0.319434907277339,10.8049086363646));
#58449=CARTESIAN_POINT('Ctrl Pts',(3.17077538272656,0.636309800095549,10.8358049063499));
#58450=CARTESIAN_POINT('Ctrl Pts',(3.23270260284628,0.794772684001268,10.8704599665709));
#58451=CARTESIAN_POINT('Ctrl Pts',(3.26619776529465,1.0684760419466,10.9145527946046));
#58452=CARTESIAN_POINT('Ctrl Pts',(3.26917063872204,1.18514270861421,10.9335671180071));
#58453=CARTESIAN_POINT('Ctrl Pts',(3.26061757087094,1.30000000000336,10.9525096133565));
#58454=CARTESIAN_POINT('Ctrl Pts',(3.07177387932149,-1.30000000000117,11.1030656186361));
#58455=CARTESIAN_POINT('Ctrl Pts',(3.09170713418827,-1.18514270861274,11.0751554212305));
#58456=CARTESIAN_POINT('Ctrl Pts',(3.10207532349415,-1.06847604194585,11.0452868189214));
#58457=CARTESIAN_POINT('Ctrl Pts',(3.10393070000947,-0.794772684001278,
10.9717600652894));
#58458=CARTESIAN_POINT('Ctrl Pts',(3.06796806118652,-0.636309800095538,
10.9144970405492));
#58459=CARTESIAN_POINT('Ctrl Pts',(3.0459831831553,-0.31943490727733,10.8433430032635));
#58460=CARTESIAN_POINT('Ctrl Pts',(3.02405337612695,-0.158333333333417,
10.8082705202785));
#58461=CARTESIAN_POINT('Ctrl Pts',(3.04804154375731,0.158333333333419,10.7880145069793));
#58462=CARTESIAN_POINT('Ctrl Pts',(3.09463930414011,0.319434907277338,10.8022387181697));
#58463=CARTESIAN_POINT('Ctrl Pts',(3.16410167785525,0.636309800095547,10.8333391027576));
#58464=CARTESIAN_POINT('Ctrl Pts',(3.22566232834457,0.794772684001265,10.8682047406006));
#58465=CARTESIAN_POINT('Ctrl Pts',(3.26003709903331,1.06847604194659,10.9126873948767));
#58466=CARTESIAN_POINT('Ctrl Pts',(3.26366763250543,1.18514270861421,10.931895253368));
#58467=CARTESIAN_POINT('Ctrl Pts',(3.25604913492926,1.30000000000335,10.9510560775591));
#58468=CARTESIAN_POINT('Ctrl Pts',(3.06620149427961,-1.30000000000116,11.1004459958638));
#58469=CARTESIAN_POINT('Ctrl Pts',(3.08508608417813,-1.18514270861273,11.0720006302833));
#58470=CARTESIAN_POINT('Ctrl Pts',(3.09467918146128,-1.06847604194585,11.041750414312));
#58471=CARTESIAN_POINT('Ctrl Pts',(3.09537594857965,-0.794772684001272,
10.9676967984221));
#58472=CARTESIAN_POINT('Ctrl Pts',(3.0595662544114,-0.636309800095533,10.9105863760201));
#58473=CARTESIAN_POINT('Ctrl Pts',(3.03746693216275,-0.319434907277327,
10.8395120488657));
#58474=CARTESIAN_POINT('Ctrl Pts',(3.01583380496636,-0.158333333333416,
10.8046691506071));
#58475=CARTESIAN_POINT('Ctrl Pts',(3.03972489261492,0.158333333333418,10.7845333994117));
#58476=CARTESIAN_POINT('Ctrl Pts',(3.08597416646741,0.319434907277335,10.7985872716408));
#58477=CARTESIAN_POINT('Ctrl Pts',(3.15526102104843,0.636309800095542,10.8299771972321));
#58478=CARTESIAN_POINT('Ctrl Pts',(3.21622770109064,0.794772684001259,10.8652563127961));
#58479=CARTESIAN_POINT('Ctrl Pts',(3.25176067465168,1.06847604194659,10.9102776134802));
#58480=CARTESIAN_POINT('Ctrl Pts',(3.25628033569737,1.1851427086142,10.9297283604134));
#58481=CARTESIAN_POINT('Ctrl Pts',(3.24993875016055,1.30000000000334,10.9491418014171));
#58482=CARTESIAN_POINT('Ctrl Pts',(3.05922678790802,-1.30000000000116,11.0971785950227));
#58483=CARTESIAN_POINT('Ctrl Pts',(3.07679748390835,-1.18514270861272,11.0680662244352));
#58484=CARTESIAN_POINT('Ctrl Pts',(3.08542594740892,-1.06847604194584,11.0373330959707));
#58485=CARTESIAN_POINT('Ctrl Pts',(3.08470107825154,-0.794772684001268,
10.9625891461495));
#58486=CARTESIAN_POINT('Ctrl Pts',(3.04913580107163,-0.63630980009553,10.9056096207377));
#58487=CARTESIAN_POINT('Ctrl Pts',(3.02692196067527,-0.319434907277326,
10.8346023343472));
#58488=CARTESIAN_POINT('Ctrl Pts',(3.00566068203787,-0.158333333333415,
10.8000457612598));
#58489=CARTESIAN_POINT('Ctrl Pts',(3.02941139388343,0.158333333333417,10.7800807424224));
#58490=CARTESIAN_POINT('Ctrl Pts',(3.07517120501442,0.319434907277334,10.7939819781425));
#58491=CARTESIAN_POINT('Ctrl Pts',(3.14424027851699,0.636309800095539,10.8257280878312));
#58492=CARTESIAN_POINT('Ctrl Pts',(3.20454890558993,0.794772684001255,10.8614200894816));
#58493=CARTESIAN_POINT('Ctrl Pts',(3.24150684993767,1.06847604194658,10.9071433700823));
#58494=CARTESIAN_POINT('Ctrl Pts',(3.24710649000357,1.18514270861419,10.9269372083692));
#58495=CARTESIAN_POINT('Ctrl Pts',(3.24230804545396,1.30000000000333,10.9467329709854));
#58496=CARTESIAN_POINT('Ctrl Pts',(3.04789713145505,-1.30000000000113,11.0921479553257));
#58497=CARTESIAN_POINT('Ctrl Pts',(3.06310098927792,-1.1851427086127,11.0622687081769));
#58498=CARTESIAN_POINT('Ctrl Pts',(3.0700383418749,-1.06847604194582,11.0309301451772));
#58499=CARTESIAN_POINT('Ctrl Pts',(3.06696773340605,-0.794772684001254,
10.9551604838395));
#58500=CARTESIAN_POINT('Ctrl Pts',(3.03213313253594,-0.636309800095519,
10.8980052996912));
#58501=CARTESIAN_POINT('Ctrl Pts',(3.01009318290283,-0.31943490727732,10.8266908353565));
#58502=CARTESIAN_POINT('Ctrl Pts',(2.9898278833591,-0.158333333333412,10.7921197278034));
#58503=CARTESIAN_POINT('Ctrl Pts',(3.01337288367669,0.158333333333414,10.7724076110835));
#58504=CARTESIAN_POINT('Ctrl Pts',(3.05781174577527,0.319434907277328,10.7867090965629));
#58505=CARTESIAN_POINT('Ctrl Pts',(3.12653082973974,0.636309800095527,10.8190069967226));
#58506=CARTESIAN_POINT('Ctrl Pts',(3.18631825942563,0.794772684001241,10.8546786608675));
#58507=CARTESIAN_POINT('Ctrl Pts',(3.22561474329067,1.06847604194656,10.9014569816872));
#58508=CARTESIAN_POINT('Ctrl Pts',(3.23287752278965,1.18514270861417,10.9218892880775));
#58509=CARTESIAN_POINT('Ctrl Pts',(3.23039309000059,1.30000000000331,10.942505299083));
#58510=CARTESIAN_POINT('Ctrl Pts',(3.0336791792996,-1.30000000000107,11.0859062407189));
#58511=CARTESIAN_POINT('Ctrl Pts',(3.04592990848317,-1.18514270861265,11.0550577019385));
#58512=CARTESIAN_POINT('Ctrl Pts',(3.05075153694945,-1.06847604194577,11.0229615337635));
#58513=CARTESIAN_POINT('Ctrl Pts',(3.04472775442659,-0.794772684001217,
10.9459306909737));
#58514=CARTESIAN_POINT('Ctrl Pts',(3.01076502342817,-0.636309800095489,
10.8886050922641));
#58515=CARTESIAN_POINT('Ctrl Pts',(2.9889037303266,-0.319434907277305,10.8169567751465));
#58516=CARTESIAN_POINT('Ctrl Pts',(2.96982639463246,-0.158333333333405,
10.7824447163113));
#58517=CARTESIAN_POINT('Ctrl Pts',(2.99317826302666,0.158333333333407,10.7629740839303));
#58518=CARTESIAN_POINT('Ctrl Pts',(3.03618964023698,0.319434907277314,10.7774983840959));
#58519=CARTESIAN_POINT('Ctrl Pts',(3.10443116313559,0.636309800095498,10.8105397740011));
#58520=CARTESIAN_POINT('Ctrl Pts',(3.16327335920585,0.794772684001204,10.8465592557145));
#58521=CARTESIAN_POINT('Ctrl Pts',(3.20537962279033,1.06847604194651,10.8947916765656));
#58522=CARTESIAN_POINT('Ctrl Pts',(3.21470826575225,1.18514270861411,10.9160326456722));
#58523=CARTESIAN_POINT('Ctrl Pts',(3.21513931036113,1.30000000000325,10.9376365560862));
#58524=CARTESIAN_POINT('Ctrl Pts',(3.01154573504434,-1.30000000000098,11.0752210934067));
#58525=CARTESIAN_POINT('Ctrl Pts',(3.01953178645156,-1.18514270861257,11.0422906197895));
#58526=CARTESIAN_POINT('Ctrl Pts',(3.0212728629428,-1.0684760419457,11.0086306666878));
#58527=CARTESIAN_POINT('Ctrl Pts',(3.01086795657992,-0.794772684001161,
10.9291841978312));
#58528=CARTESIAN_POINT('Ctrl Pts',(2.97811254408224,-0.636309800095444,
10.871806941579));
#58529=CARTESIAN_POINT('Ctrl Pts',(2.95609681690904,-0.319434907277283,
10.8001194966574));
#58530=CARTESIAN_POINT('Ctrl Pts',(2.9382621750574,-0.158333333333394,10.7664414319515));
#58531=CARTESIAN_POINT('Ctrl Pts',(2.96090895269562,0.158333333333396,10.7477962611558));
#58532=CARTESIAN_POINT('Ctrl Pts',(3.00158302123252,0.319434907277291,10.7627472791991));
#58533=CARTESIAN_POINT('Ctrl Pts',(3.06933619159502,0.636309800095453,10.7966226289519));
#58534=CARTESIAN_POINT('Ctrl Pts',(3.1273686119044,0.794772684001148,10.8323048514524));
#58535=CARTESIAN_POINT('Ctrl Pts',(3.17421656341115,1.06847604194644,10.8825900038451));
#58536=CARTESIAN_POINT('Ctrl Pts',(3.18684759319335,1.18514270861404,10.9051546963106));
#58537=CARTESIAN_POINT('Ctrl Pts',(3.19183091043806,1.30000000000316,10.9285175020193));
#58538=CARTESIAN_POINT('Ctrl Pts',(2.98919530248008,-1.30000000000088,11.0647296599117));
#58539=CARTESIAN_POINT('Ctrl Pts',(2.99291765020551,-1.18514270861247,11.0297155831156));
#58540=CARTESIAN_POINT('Ctrl Pts',(2.99153880663323,-1.06847604194561,10.9945342094214));
#58541=CARTESIAN_POINT('Ctrl Pts',(2.97656862975705,-0.794772684001099,
10.9128717088757));
#58542=CARTESIAN_POINT('Ctrl Pts',(2.94457308631418,-0.636309800095394,
10.8559300267459));
#58543=CARTESIAN_POINT('Ctrl Pts',(2.92246346658274,-0.319434907277257,
10.7841365189799));
#58544=CARTESIAN_POINT('Ctrl Pts',(2.90620251148595,-0.158333333333381,
10.7509517716306));
#58545=CARTESIAN_POINT('Ctrl Pts',(2.92874230896034,0.158333333333383,10.7324383617579));
#58546=CARTESIAN_POINT('Ctrl Pts',(2.96787991341664,0.319434907277266,10.7468429609936));
#58547=CARTESIAN_POINT('Ctrl Pts',(3.03521533464832,0.636309800095403,10.7814693124496));
#58548=CARTESIAN_POINT('Ctrl Pts',(3.09169297791346,0.794772684001086,10.8177130535361));
#58549=CARTESIAN_POINT('Ctrl Pts',(3.14276914107174,1.06847604194635,10.8706653479746));
#58550=CARTESIAN_POINT('Ctrl Pts',(3.15850488309139,1.18514270861394,10.8947887211331));
#58551=CARTESIAN_POINT('Ctrl Pts',(3.16786738865772,1.30000000000305,10.9201143812634));
#58552=CARTESIAN_POINT('Ctrl Pts',(2.96717524641191,-1.30000000000084,11.0538796667386));
#58553=CARTESIAN_POINT('Ctrl Pts',(2.96648675545647,-1.18514270861244,11.0169140357705));
#58554=CARTESIAN_POINT('Ctrl Pts',(2.96202768339402,-1.06847604194558,10.9801481702247));
#58555=CARTESIAN_POINT('Ctrl Pts',(2.94301553823612,-0.794772684001075,
10.8956731639161));
#58556=CARTESIAN_POINT('Ctrl Pts',(2.91320656941111,-0.636309800095375,
10.8376308550638));
#58557=CARTESIAN_POINT('Ctrl Pts',(2.89125645448967,-0.319434907277247,
10.7654460382644));
#58558=CARTESIAN_POINT('Ctrl Pts',(2.87579921818227,-0.158333333333377,
10.7335738837162));
#58559=CARTESIAN_POINT('Ctrl Pts',(2.89754362678226,0.158333333333378,10.7159400313523));
#58560=CARTESIAN_POINT('Ctrl Pts',(2.93469623921681,0.319434907277257,10.7302971169921));
#58561=CARTESIAN_POINT('Ctrl Pts',(3.0010380244238,0.636309800095384,10.7663210928599));
#58562=CARTESIAN_POINT('Ctrl Pts',(3.05548748670998,0.794772684001061,10.8036733359117));
#58563=CARTESIAN_POINT('Ctrl Pts',(3.11102365523955,1.06847604194632,10.8590380958667));
#58564=CARTESIAN_POINT('Ctrl Pts',(3.13016434939635,1.1851427086139,10.8843836848376));
#58565=CARTESIAN_POINT('Ctrl Pts',(3.14440618817126,1.30000000000302,10.9111095096614));
#58566=CARTESIAN_POINT('Ctrl Pts',(2.95060113807384,-1.3000000000008,11.0457492105973));
#58567=CARTESIAN_POINT('Ctrl Pts',(2.94723873270801,-1.1851427086124,11.0066494327933));
#58568=CARTESIAN_POINT('Ctrl Pts',(2.94073223438963,-1.06847604194555,10.968421535658));
#58569=CARTESIAN_POINT('Ctrl Pts',(2.91843743795963,-0.794772684001051,
10.8821216645747));
#58570=CARTESIAN_POINT('Ctrl Pts',(2.8881619930355,-0.636309800095356,10.825518085516));
#58571=CARTESIAN_POINT('Ctrl Pts',(2.86615173620415,-0.319434907277238,
10.7532403162218));
#58572=CARTESIAN_POINT('Ctrl Pts',(2.85268458474327,-0.158333333333372,
10.7208755131832));
#58573=CARTESIAN_POINT('Ctrl Pts',(2.8745474532907,0.158333333333374,10.7031173213864));
#58574=CARTESIAN_POINT('Ctrl Pts',(2.91007273900423,0.319434907277246,10.7175764682789));
#58575=CARTESIAN_POINT('Ctrl Pts',(2.97621834270599,0.636309800095365,10.7539824537767));
#58576=CARTESIAN_POINT('Ctrl Pts',(3.03022498028522,0.794772684001038,10.7908558682582));
#58577=CARTESIAN_POINT('Ctrl Pts',(3.08879748892997,1.06847604194629,10.8483861882998));
#58578=CARTESIAN_POINT('Ctrl Pts',(3.11002664482549,1.18514270861387,10.8752013558668));
#58579=CARTESIAN_POINT('Ctrl Pts',(3.12713108794945,1.30000000000298,10.903928947163));
#58580=CARTESIAN_POINT('Ctrl Pts',(2.93497824004345,-1.30000000000077,11.0366822995914));
#58581=CARTESIAN_POINT('Ctrl Pts',(2.92821505089552,-1.18514270861238,10.996188463152));
#58582=CARTESIAN_POINT('Ctrl Pts',(2.91935717498159,-1.06847604194552,10.9567970456551));
#58583=CARTESIAN_POINT('Ctrl Pts',(2.89405456413831,-0.794772684001033,
10.868341799307));
#58584=CARTESIAN_POINT('Ctrl Pts',(2.8656757178425,-0.636309800095341,10.8106674111858));
#58585=CARTESIAN_POINT('Ctrl Pts',(2.84385408820492,-0.31943490727723,10.7380228229021));
#58586=CARTESIAN_POINT('Ctrl Pts',(2.83108911726183,-0.158333333333368,
10.7065259198157));
#58587=CARTESIAN_POINT('Ctrl Pts',(2.85192044163665,0.15833333333337,10.6898824572087));
#58588=CARTESIAN_POINT('Ctrl Pts',(2.88514032487475,0.31943490727724,10.7051740588285));
#58589=CARTESIAN_POINT('Ctrl Pts',(2.95016058666272,0.636309800095351,10.7430246094566));
#58590=CARTESIAN_POINT('Ctrl Pts',(3.00288334881758,0.794772684001019,10.7804648325827));
#58591=CARTESIAN_POINT('Ctrl Pts',(3.06495317918483,1.06847604194626,10.8396431675606));
#58592=CARTESIAN_POINT('Ctrl Pts',(3.08882703350963,1.18514270861384,10.8672818218745));
#58593=CARTESIAN_POINT('Ctrl Pts',(3.10970701250702,1.30000000000295,10.8969430220637));
#58594=CARTESIAN_POINT('Ctrl Pts',(2.91813452753457,-1.30000000000074,11.0288099698746));
#58595=CARTESIAN_POINT('Ctrl Pts',(2.90839140218389,-1.18514270861235,10.9864952742596));
#58596=CARTESIAN_POINT('Ctrl Pts',(2.89739169724188,-1.0684760419455,10.9457340364746));
#58597=CARTESIAN_POINT('Ctrl Pts',(2.86907722810858,-0.794772684001015,
10.8551562212887));
#58598=CARTESIAN_POINT('Ctrl Pts',(2.84151498740897,-0.636309800095327,
10.7975637367191));
#58599=CARTESIAN_POINT('Ctrl Pts',(2.81985692566231,-0.319434907277224,
10.7245917132736));
#58600=CARTESIAN_POINT('Ctrl Pts',(2.80818466611494,-0.158333333333365,
10.6935702763831));
#58601=CARTESIAN_POINT('Ctrl Pts',(2.82911986192055,0.158333333333366,10.6767995837835));
#58602=CARTESIAN_POINT('Ctrl Pts',(2.86154473816526,0.319434907277231,10.6912520800743));
#58603=CARTESIAN_POINT('Ctrl Pts',(2.92621818688126,0.636309800095335,10.7296524559277));
#58604=CARTESIAN_POINT('Ctrl Pts',(2.97747860298749,0.794772684001002,10.7677691469733));
#58605=CARTESIAN_POINT('Ctrl Pts',(3.04226747723685,1.06847604194624,10.829476699648));
#58606=CARTESIAN_POINT('Ctrl Pts',(3.06823542225031,1.18514270861381,10.8585815195564));
#58607=CARTESIAN_POINT('Ctrl Pts',(3.09212660927895,1.30000000000292,10.8900802463102));
#58608=CARTESIAN_POINT('Ctrl Pts',(2.90568427085915,-1.30000000000073,11.0206511408274));
#58609=CARTESIAN_POINT('Ctrl Pts',(2.89350197144723,-1.18514270861233,10.976754637072));
#58610=CARTESIAN_POINT('Ctrl Pts',(2.88071110959298,-1.06847604194549,10.9348433793974));
#58611=CARTESIAN_POINT('Ctrl Pts',(2.84975575892226,-0.794772684001005,
10.8426063054447));
#58612=CARTESIAN_POINT('Ctrl Pts',(2.82255596465368,-0.63630980009532,10.7854051223092));
#58613=CARTESIAN_POINT('Ctrl Pts',(2.80085719239994,-0.319434907277221,
10.7123354663725));
#58614=CARTESIAN_POINT('Ctrl Pts',(2.79032098272189,-0.158333333333363,
10.6814741628591));
#58615=CARTESIAN_POINT('Ctrl Pts',(2.81093878189025,0.158333333333365,10.6650291179649));
#58616=CARTESIAN_POINT('Ctrl Pts',(2.84190760268583,0.319434907277228,10.6796354868406));
#58617=CARTESIAN_POINT('Ctrl Pts',(2.90598056204028,0.636309800095328,10.7188205295066));
#58618=CARTESIAN_POINT('Ctrl Pts',(2.95630282008806,0.794772684000994,10.7571931539108));
#58619=CARTESIAN_POINT('Ctrl Pts',(3.02361144613931,1.06847604194623,10.8207183172819));
#58620=CARTESIAN_POINT('Ctrl Pts',(3.05146661032784,1.1851427086138,10.8508829861494));
#58621=CARTESIAN_POINT('Ctrl Pts',(3.0780415285176,1.3000000000029,10.8837146345004));
#58622=CARTESIAN_POINT('Ctrl Pts',(2.89444889450715,-1.30000000000072,11.0153899166469));
#58623=CARTESIAN_POINT('Ctrl Pts',(2.88028412010224,-1.18514270861233,10.970267544928));
#58624=CARTESIAN_POINT('Ctrl Pts',(2.8661099915129,-1.06847604194548,10.9273912624621));
#58625=CARTESIAN_POINT('Ctrl Pts',(2.83334330890949,-0.794772684001001,
10.8335273880978));
#58626=CARTESIAN_POINT('Ctrl Pts',(2.80700132183935,-0.636309800095317,
10.7760551249637));
#58627=CARTESIAN_POINT('Ctrl Pts',(2.78564335508256,-0.319434907277219,
10.7025319931978));
#58628=CARTESIAN_POINT('Ctrl Pts',(2.77603953129172,-0.158333333333362,
10.6717864454594));
#58629=CARTESIAN_POINT('Ctrl Pts',(2.79642245405076,0.158333333333364,10.6555809652624));
#58630=CARTESIAN_POINT('Ctrl Pts',(2.82612568804013,0.319434907277227,10.6703931004593));
#58631=CARTESIAN_POINT('Ctrl Pts',(2.88957969551012,0.636309800095326,10.710352653672));
#58632=CARTESIAN_POINT('Ctrl Pts',(2.93889565643564,0.794772684000989,10.7492262233861));
#58633=CARTESIAN_POINT('Ctrl Pts',(3.0083373396324,1.06847604194622,10.8140830608064));
#58634=CARTESIAN_POINT('Ctrl Pts',(3.03784222283995,1.1851427086138,10.8449436333644));
#58635=CARTESIAN_POINT('Ctrl Pts',(3.06679325766699,1.3000000000029,10.8785906567437));
#58636=CARTESIAN_POINT('Ctrl Pts',(2.87871424024058,-1.3000000000007,11.0063906910496));
#58637=CARTESIAN_POINT('Ctrl Pts',(2.86153048821051,-1.18514270861231,10.9594734224498));
#58638=CARTESIAN_POINT('Ctrl Pts',(2.8452054816931,-1.06847604194547,10.9152249725586));
#58639=CARTESIAN_POINT('Ctrl Pts',(2.80947532475721,-0.794772684000991,
10.8191677065502));
#58640=CARTESIAN_POINT('Ctrl Pts',(2.78419484317971,-0.636309800095306,
10.7615189991352));
#58641=CARTESIAN_POINT('Ctrl Pts',(2.76293058764447,-0.319434907277213,
10.6877317353546));
#58642=CARTESIAN_POINT('Ctrl Pts',(2.75422099359627,-0.15833333333336,10.6576623718402));
#58643=CARTESIAN_POINT('Ctrl Pts',(2.77432869962127,0.158333333333361,10.6417276821006));
#58644=CARTESIAN_POINT('Ctrl Pts',(2.80277231653527,0.319434907277222,10.6562083569586));
#58645=CARTESIAN_POINT('Ctrl Pts',(2.86575568712979,0.636309800095315,10.6968330257819));
#58646=CARTESIAN_POINT('Ctrl Pts',(2.91407875105576,0.794772684000976,10.7358410645145));
#58647=CARTESIAN_POINT('Ctrl Pts',(2.98619913099117,1.0684760419462,10.8032646501883));
#58648=CARTESIAN_POINT('Ctrl Pts',(3.01769283609529,1.18514270861378,10.835709748802));
#58649=CARTESIAN_POINT('Ctrl Pts',(3.04946200615281,1.30000000000288,10.8714147740814));
#58650=CARTESIAN_POINT('Ctrl Pts',(2.85722596337426,-1.30000000000067,10.9948506738711));
#58651=CARTESIAN_POINT('Ctrl Pts',(2.8364538696826,-1.18514270861228,10.9450867954173));
#58652=CARTESIAN_POINT('Ctrl Pts',(2.81759781234889,-1.06847604194544,10.8986636485962));
#58653=CARTESIAN_POINT('Ctrl Pts',(2.77846297505534,-0.794772684000968,
10.7991346509037));
#58654=CARTESIAN_POINT('Ctrl Pts',(2.75458928518589,-0.636309800095292,
10.741293097816));
#58655=CARTESIAN_POINT('Ctrl Pts',(2.73367131294162,-0.319434907277208,
10.666946408431));
#58656=CARTESIAN_POINT('Ctrl Pts',(2.72639850410211,-0.158333333333356,
10.637537160389));
#58657=CARTESIAN_POINT('Ctrl Pts',(2.74594336818632,0.158333333333358,10.6221453477439));
#58658=CARTESIAN_POINT('Ctrl Pts',(2.77235282520389,0.319434907277214,10.636484262179));
#58659=CARTESIAN_POINT('Ctrl Pts',(2.83391378471908,0.636309800095301,10.6788241077998));
#58660=CARTESIAN_POINT('Ctrl Pts',(2.87958190266052,0.79477268400096,10.7194951393387));
#58661=CARTESIAN_POINT('Ctrl Pts',(2.95557229660141,1.06847604194618,10.7900125175906));
#58662=CARTESIAN_POINT('Ctrl Pts',(2.99024971050842,1.18514270861375,10.823985756658));
#58663=CARTESIAN_POINT('Ctrl Pts',(3.02671111250687,1.30000000000285,10.8614078746738));
#58664=CARTESIAN_POINT('Ctrl Pts',(2.83706008972707,-1.30000000000064,10.9820037922095));
#58665=CARTESIAN_POINT('Ctrl Pts',(2.81253518548399,-1.18514270861225,10.9295618442951));
#58666=CARTESIAN_POINT('Ctrl Pts',(2.79101659633156,-1.06847604194541,10.8810982570713));
#58667=CARTESIAN_POINT('Ctrl Pts',(2.74824953988114,-0.794772684000949,
10.7783284845407));
#58668=CARTESIAN_POINT('Ctrl Pts',(2.725762568292,-0.636309800095276,10.7203131607811));
#58669=CARTESIAN_POINT('Ctrl Pts',(2.70505703675324,-0.319434907277199,
10.6455373550391));
#58670=CARTESIAN_POINT('Ctrl Pts',(2.69907374711529,-0.158333333333352,
10.6169341839772));
#58671=CARTESIAN_POINT('Ctrl Pts',(2.71811137123917,0.158333333333354,10.6020168768041));
#58672=CARTESIAN_POINT('Ctrl Pts',(2.74247756448409,0.319434907277207,10.6162470884632));
#58673=CARTESIAN_POINT('Ctrl Pts',(2.80329498416027,0.636309800095286,10.6595286163612));
#58674=CARTESIAN_POINT('Ctrl Pts',(2.84789785676197,0.794772684000939,10.7000533919715));
#58675=CARTESIAN_POINT('Ctrl Pts',(2.92740222562294,1.06847604194615,10.7740283999209));
#58676=CARTESIAN_POINT('Ctrl Pts',(2.96465501981579,1.18514270861372,10.8101951862368));
#58677=CARTESIAN_POINT('Ctrl Pts',(3.00474611284864,1.30000000000282,10.8505077189715));
#58678=CARTESIAN_POINT('Ctrl Pts',(2.81633525801835,-1.30000000000062,10.9696756101456));
#58679=CARTESIAN_POINT('Ctrl Pts',(2.78804194764148,-1.18514270861224,10.9145486304021));
#58680=CARTESIAN_POINT('Ctrl Pts',(2.76394486494591,-1.0684760419454,10.8639501740209));
#58681=CARTESIAN_POINT('Ctrl Pts',(2.71796990871058,-0.794772684000942,
10.7575194124892));
#58682=CARTESIAN_POINT('Ctrl Pts',(2.69755314336305,-0.636309800095269,
10.6986967248109));
#58683=CARTESIAN_POINT('Ctrl Pts',(2.67767079655553,-0.319434907277195,
10.6229152835093));
#58684=CARTESIAN_POINT('Ctrl Pts',(2.67340159212905,-0.15833333333335,10.5947243926643));
#58685=CARTESIAN_POINT('Ctrl Pts',(2.69171984891177,0.158333333333352,10.5804670646744));
#58686=CARTESIAN_POINT('Ctrl Pts',(2.71330489916008,0.319434907277201,10.595227423328));
#58687=CARTESIAN_POINT('Ctrl Pts',(2.77254205502706,0.636309800095276,10.6402835905659));
#58688=CARTESIAN_POINT('Ctrl Pts',(2.81526104756883,0.794772684000931,10.6815847005431));
#58689=CARTESIAN_POINT('Ctrl Pts',(2.89826319371668,1.06847604194614,10.7590494756952));
#58690=CARTESIAN_POINT('Ctrl Pts',(2.93832246151959,1.1851427086137,10.7971693128279));
#58691=CARTESIAN_POINT('Ctrl Pts',(2.98251244359048,1.30000000000279,10.8398773562828));
#58692=CARTESIAN_POINT('Ctrl Pts',(2.79912697785942,-1.30000000000055,10.9580213491864));
#58693=CARTESIAN_POINT('Ctrl Pts',(2.76797398191822,-1.18514270861218,10.9001773311542));
#58694=CARTESIAN_POINT('Ctrl Pts',(2.74183357444361,-1.06847604194534,10.8475474650426));
#58695=CARTESIAN_POINT('Ctrl Pts',(2.69302408592936,-0.794772684000901,
10.7380076797805));
#58696=CARTESIAN_POINT('Ctrl Pts',(2.67339238690378,-0.636309800095235,
10.679472442146));
#58697=CARTESIAN_POINT('Ctrl Pts',(2.65391067895453,-0.319434907277177,
10.6031350095598));
#58698=CARTESIAN_POINT('Ctrl Pts',(2.65127946748484,-0.158333333333342,
10.5751707266414));
#58699=CARTESIAN_POINT('Ctrl Pts',(2.66939714574104,0.158333333333343,10.561060519015));
#58700=CARTESIAN_POINT('Ctrl Pts',(2.68941821557786,0.319434907277186,10.5754293992273));
#58701=CARTESIAN_POINT('Ctrl Pts',(2.74728684632815,0.636309800095243,10.6219767342921));
#58702=CARTESIAN_POINT('Ctrl Pts',(2.78760864054499,0.794772684000887,10.6646274176482));
#58703=CARTESIAN_POINT('Ctrl Pts',(2.87298857137924,1.06847604194608,10.7457680695785));
#58704=CARTESIAN_POINT('Ctrl Pts',(2.9152015734891,1.18514270861364,10.7858792184749));
#58705=CARTESIAN_POINT('Ctrl Pts',(2.96266976928875,1.30000000000273,10.8309787346044));
#58706=CARTESIAN_POINT('Ctrl Pts',(2.77856646432018,-1.30000000000055,10.945473506968));
#58707=CARTESIAN_POINT('Ctrl Pts',(2.74390448340325,-1.18514270861217,10.8846512852128));
#58708=CARTESIAN_POINT('Ctrl Pts',(2.71544871744191,-1.06847604194534,10.8296097182275));
#58709=CARTESIAN_POINT('Ctrl Pts',(2.66404780361125,-0.794772684000899,
10.7158071563984));
#58710=CARTESIAN_POINT('Ctrl Pts',(2.64727915488273,-0.636309800095235,
10.6557881406909));
#58711=CARTESIAN_POINT('Ctrl Pts',(2.6284743497969,-0.319434907277178,10.5785982396017));
#58712=CARTESIAN_POINT('Ctrl Pts',(2.62626533131418,-0.158333333333342,
10.5522615108711));
#58713=CARTESIAN_POINT('Ctrl Pts',(2.64355804675884,0.158333333333343,10.5388646112871));
#58714=CARTESIAN_POINT('Ctrl Pts',(2.66173699543718,0.319434907277185,10.5528250058107));
#58715=CARTESIAN_POINT('Ctrl Pts',(2.71846023507552,0.636309800095243,10.600647568866));
#58716=CARTESIAN_POINT('Ctrl Pts',(2.75691308777398,0.794772684000889,10.643949379081));
#58717=CARTESIAN_POINT('Ctrl Pts',(2.84567449106146,1.06847604194608,10.7287033424145));
#58718=CARTESIAN_POINT('Ctrl Pts',(2.89057211835406,1.18514270861364,10.7709219103223));
#58719=CARTESIAN_POINT('Ctrl Pts',(2.94194585039009,1.30000000000272,10.8186721958546));
#58720=CARTESIAN_POINT('Ctrl Pts',(2.76402116993866,-1.30000000000053,10.9352822600269));
#58721=CARTESIAN_POINT('Ctrl Pts',(2.72705341699935,-1.18514270861216,10.8720103361742));
#58722=CARTESIAN_POINT('Ctrl Pts',(2.69699423975246,-1.06847604194533,10.815105475105));
#58723=CARTESIAN_POINT('Ctrl Pts',(2.64351171889973,-0.794772684000889,
10.6983530510131));
#58724=CARTESIAN_POINT('Ctrl Pts',(2.62767640765532,-0.636309800095225,
10.6383750495022));
#58725=CARTESIAN_POINT('Ctrl Pts',(2.60950534885464,-0.319434907277172,
10.5604641396208));
#58726=CARTESIAN_POINT('Ctrl Pts',(2.60886846140746,-0.158333333333339,
10.5341700616904));
#58727=CARTESIAN_POINT('Ctrl Pts',(2.62592147012438,0.158333333333341,10.5209421222037));
#58728=CARTESIAN_POINT('Ctrl Pts',(2.64240323947071,0.319434907277179,10.5348738755294));
#58729=CARTESIAN_POINT('Ctrl Pts',(2.69777091651019,0.636309800095232,10.5840772299315));
#58730=CARTESIAN_POINT('Ctrl Pts',(2.73440246840488,0.794772684000875,10.6282281775035));
#58731=CARTESIAN_POINT('Ctrl Pts',(2.82486322897247,1.06847604194607,10.7164281967985));
#58732=CARTESIAN_POINT('Ctrl Pts',(2.87135839004095,1.18514270861362,10.7605960620217));
#58733=CARTESIAN_POINT('Ctrl Pts',(2.92519160082957,1.3000000000027,10.8107532722481));
#58734=CARTESIAN_POINT('Ctrl Pts',(2.74940605748626,-1.30000000000051,10.9250389677115));
#58735=CARTESIAN_POINT('Ctrl Pts',(2.70981978889349,-1.18514270861214,10.8593957950081));
#58736=CARTESIAN_POINT('Ctrl Pts',(2.67807761042904,-1.06847604194531,10.8005458133735));
#58737=CARTESIAN_POINT('Ctrl Pts',(2.62286824557641,-0.794772684000878,
10.6802842132411));
#58738=CARTESIAN_POINT('Ctrl Pts',(2.61000799397286,-0.636309800095218,
10.6185138370675));
#58739=CARTESIAN_POINT('Ctrl Pts',(2.59160907804646,-0.31943490727717,10.5406157221883));
#58740=CARTESIAN_POINT('Ctrl Pts',(2.58914190271259,-0.158333333333338,
10.5174726977482));
#58741=CARTESIAN_POINT('Ctrl Pts',(2.60526434112811,0.158333333333339,10.5050278888623));
#58742=CARTESIAN_POINT('Ctrl Pts',(2.6220415134188,0.319434907277178,10.5170828129627));
#58743=CARTESIAN_POINT('Ctrl Pts',(2.67697248829484,0.636309800095228,10.5668682305745));
#58744=CARTESIAN_POINT('Ctrl Pts',(2.71160879902238,0.794772684000868,10.6120400639937));
#58745=CARTESIAN_POINT('Ctrl Pts',(2.80431283473728,1.06847604194606,10.70338432225));
#58746=CARTESIAN_POINT('Ctrl Pts',(2.85270371729135,1.18514270861361,10.7493499675256));
#58747=CARTESIAN_POINT('Ctrl Pts',(2.9093573403614,1.30000000000269,10.8017417133158));
#58748=CARTESIAN_POINT('Ctrl Pts',(2.73731735276389,-1.3000000000005,10.9165770042155));
#58749=CARTESIAN_POINT('Ctrl Pts',(2.6964303190073,-1.18514270861213,10.8484715701028));
#58750=CARTESIAN_POINT('Ctrl Pts',(2.66358967733224,-1.0684760419453,10.7879629098742));
#58751=CARTESIAN_POINT('Ctrl Pts',(2.60631000069861,-0.794772684000871,
10.6657258674321));
#58752=CARTESIAN_POINT('Ctrl Pts',(2.59248039945063,-0.63630980009521,10.6055712036968));
#58753=CARTESIAN_POINT('Ctrl Pts',(2.57341924514479,-0.319434907277165,
10.5282269350905));
#58754=CARTESIAN_POINT('Ctrl Pts',(2.57143763839085,-0.158333333333336,
10.5059113031678));
#58755=CARTESIAN_POINT('Ctrl Pts',(2.58802141554789,0.158333333333337,10.4930267753833));
#58756=CARTESIAN_POINT('Ctrl Pts',(2.60547335406668,0.319434907277174,10.5031739460727));
#58757=CARTESIAN_POINT('Ctrl Pts',(2.66058247646301,0.636309800095219,10.5528147832921));
#58758=CARTESIAN_POINT('Ctrl Pts',(2.69364714043103,0.794772684000856,10.5986380530358));
#58759=CARTESIAN_POINT('Ctrl Pts',(2.78805721331708,1.06847604194604,10.6923386658196));
#58760=CARTESIAN_POINT('Ctrl Pts',(2.83784990751017,1.1851427086136,10.7397310796062));
#58761=CARTESIAN_POINT('Ctrl Pts',(2.89656867358178,1.30000000000268,10.7939563838551));
#58762=CARTESIAN_POINT('Ctrl Pts',(2.72325603000434,-1.30000000000049,10.9058269403029));
#58763=CARTESIAN_POINT('Ctrl Pts',(2.68052254051567,-1.18514270861212,10.8345047589383));
#58764=CARTESIAN_POINT('Ctrl Pts',(2.64601328600309,-1.0684760419453,10.7719058016326));
#58765=CARTESIAN_POINT('Ctrl Pts',(2.58528963257371,-0.794772684000865,
10.6474420800289));
#58766=CARTESIAN_POINT('Ctrl Pts',(2.56935149160544,-0.636309800095207,
10.5898946254132));
#58767=CARTESIAN_POINT('Ctrl Pts',(2.54855773656525,-0.319434907277164,
10.5138629625327));
#58768=CARTESIAN_POINT('Ctrl Pts',(2.54706392153435,-0.158333333333335,
10.4927970916832));
#58769=CARTESIAN_POINT('Ctrl Pts',(2.56354371788599,0.158333333333336,10.4799758266955));
#58770=CARTESIAN_POINT('Ctrl Pts',(2.58062333772424,0.319434907277171,10.4887158780038));
#58771=CARTESIAN_POINT('Ctrl Pts',(2.6368062477542,0.636309800095216,10.5376223605652));
#58772=CARTESIAN_POINT('Ctrl Pts',(2.67064655634535,0.794772684000852,10.5820567515548));
#58773=CARTESIAN_POINT('Ctrl Pts',(2.76841994636897,1.06847604194604,10.6781287217965));
#58774=CARTESIAN_POINT('Ctrl Pts',(2.82015251793265,1.18514270861359,10.7274121893936));
#58775=CARTESIAN_POINT('Ctrl Pts',(2.88129518337976,1.30000000000268,10.7843931284875));
#58776=CARTESIAN_POINT('Ctrl Pts',(2.71361311550279,-1.30000000000047,10.898569746919));
#58777=CARTESIAN_POINT('Ctrl Pts',(2.67063753707731,-1.1851427086121,10.824130284025));
#58778=CARTESIAN_POINT('Ctrl Pts',(2.63543757366513,-1.06847604194528,10.7598223853803));
#58779=CARTESIAN_POINT('Ctrl Pts',(2.57208184264171,-0.794772684000851,
10.6346642149887));
#58780=CARTESIAN_POINT('Ctrl Pts',(2.55201129877974,-0.636309800095197,
10.5822378261051));
#58781=CARTESIAN_POINT('Ctrl Pts',(2.52893211648025,-0.319434907277159,
10.5088463219352));
#58782=CARTESIAN_POINT('Ctrl Pts',(2.52830982650113,-0.158333333333333,
10.4884080647079));
#58783=CARTESIAN_POINT('Ctrl Pts',(2.54469368659007,0.158333333333334,10.4757230851068));
#58784=CARTESIAN_POINT('Ctrl Pts',(2.56094950441052,0.319434907277167,10.4839277842833));
#58785=CARTESIAN_POINT('Ctrl Pts',(2.61892980279681,0.636309800095206,10.53056138516));
#58786=CARTESIAN_POINT('Ctrl Pts',(2.65591208556864,0.79477268400084,10.5704096562204));
#58787=CARTESIAN_POINT('Ctrl Pts',(2.75637070809838,1.06847604194602,10.6671425661737));
#58788=CARTESIAN_POINT('Ctrl Pts',(2.80906926851073,1.18514270861357,10.7179729089448));
#58789=CARTESIAN_POINT('Ctrl Pts',(2.87098157400095,1.30000000000265,10.7777615020756));
#58790=CARTESIAN_POINT('Ctrl Pts',(2.70549646903697,-1.30000000000047,10.8957209484764));
#58791=CARTESIAN_POINT('Ctrl Pts',(2.6627468523953,-1.1851427086121,10.8213914743752));
#58792=CARTESIAN_POINT('Ctrl Pts',(2.62751487735367,-1.06847604194528,10.7574269431321));
#58793=CARTESIAN_POINT('Ctrl Pts',(2.56348922287021,-0.794772684000851,
10.6336011714019));
#58794=CARTESIAN_POINT('Ctrl Pts',(2.54183416968341,-0.636309800095197,
10.5831927997129));
#58795=CARTESIAN_POINT('Ctrl Pts',(2.51776513723769,-0.319434907277159,
10.5111668553313));
#58796=CARTESIAN_POINT('Ctrl Pts',(2.5171210925739,-0.158333333333333,10.4906809863802));
#58797=CARTESIAN_POINT('Ctrl Pts',(2.53338410693288,0.158333333333334,10.4781996815688));
#58798=CARTESIAN_POINT('Ctrl Pts',(2.54937394678571,0.319434907277167,10.4868805779095));
#58799=CARTESIAN_POINT('Ctrl Pts',(2.60843787791201,0.636309800095206,10.5321053630787));
#58800=CARTESIAN_POINT('Ctrl Pts',(2.64769917658169,0.79477268400084,10.5691036076304));
#58801=CARTESIAN_POINT('Ctrl Pts',(2.74872068765979,1.06847604194602,10.6646142935777));
#58802=CARTESIAN_POINT('Ctrl Pts',(2.80123722412148,1.18514270861357,10.7153390608067));
#58803=CARTESIAN_POINT('Ctrl Pts',(2.86254182811488,1.30000000000265,10.7754455583378));
#58804=CARTESIAN_POINT('Ctrl Pts',(2.70549646903679,-1.3,10.8957209484761));
#58805=CARTESIAN_POINT('Ctrl Pts',(2.6627468523952,-1.18514270861178,10.821391474375));
#58806=CARTESIAN_POINT('Ctrl Pts',(2.62751487735363,-1.06847604194512,10.757426943132));
#58807=CARTESIAN_POINT('Ctrl Pts',(2.56348922287021,-0.794772684000851,
10.6336011714019));
#58808=CARTESIAN_POINT('Ctrl Pts',(2.54183416968341,-0.636309800095197,
10.5831927997129));
#58809=CARTESIAN_POINT('Ctrl Pts',(2.5177651372377,-0.319434907277159,10.5111668553313));
#58810=CARTESIAN_POINT('Ctrl Pts',(2.5171210925739,-0.158333333333332,10.4906809863802));
#58811=CARTESIAN_POINT('Ctrl Pts',(2.53338410693288,0.158333333333334,10.4781996815689));
#58812=CARTESIAN_POINT('Ctrl Pts',(2.54937394678571,0.319434907277167,10.4868805779095));
#58813=CARTESIAN_POINT('Ctrl Pts',(2.60843787791201,0.636309800095206,10.5321053630787));
#58814=CARTESIAN_POINT('Ctrl Pts',(2.64769917658169,0.79477268400084,10.5691036076304));
#58815=CARTESIAN_POINT('Ctrl Pts',(2.74872068765945,1.06847604194511,10.6646142935774));
#58816=CARTESIAN_POINT('Ctrl Pts',(2.80123722412067,1.18514270861178,10.715339060806));
#58817=CARTESIAN_POINT('Ctrl Pts',(2.86254182811346,1.3,10.7754455583364));
#58818=CARTESIAN_POINT('',(3.07986858154633,-1.2,11.0751657410237));
#58819=CARTESIAN_POINT('Ctrl Pts',(3.07986858154632,-1.2,11.0751657410237));
#58820=CARTESIAN_POINT('Ctrl Pts',(3.0588058189093,-1.21682649969802,11.0704122326966));
#58821=CARTESIAN_POINT('Ctrl Pts',(3.03724316373786,-1.23325202986004,11.0664907783325));
#58822=CARTESIAN_POINT('Ctrl Pts',(3.00532794741497,-1.25864588707498,11.0591965660954));
#58823=CARTESIAN_POINT('Ctrl Pts',(2.99504873255066,-1.26676696435895,11.0569015286308));
#58824=CARTESIAN_POINT('Ctrl Pts',(2.97662419564679,-1.28142016386729,11.0526365617568));
#58825=CARTESIAN_POINT('Ctrl Pts',(2.96352566190721,-1.29187129415509,11.0495391320497));
#58826=CARTESIAN_POINT('Ctrl Pts',(2.95536519311266,-1.29845709646629,11.0475038001274));
#58827=CARTESIAN_POINT('Ctrl Pts',(2.9544116176196,-1.29922913626852,11.0472627061011));
#58828=CARTESIAN_POINT('Ctrl Pts',(2.95346386092393,-1.30000000000081,11.047018484776));
#58829=CARTESIAN_POINT('',(3.20083483810839,-0.653834841326313,10.9758649788792));
#58830=CARTESIAN_POINT('Ctrl Pts',(3.20083483808943,-0.653834841310767,
10.9758649789516));
#58831=CARTESIAN_POINT('Ctrl Pts',(3.18968063418913,-0.71148786346381,10.9853204983185));
#58832=CARTESIAN_POINT('Ctrl Pts',(3.17784572765889,-0.767209565144657,
10.9952666810981));
#58833=CARTESIAN_POINT('Ctrl Pts',(3.15307493364191,-0.881644238580126,
11.0158727714609));
#58834=CARTESIAN_POINT('Ctrl Pts',(3.14116546938795,-0.939027188339406,
11.0256944086798));
#58835=CARTESIAN_POINT('Ctrl Pts',(3.1186899032036,-1.03713813150292,11.0440050160884));
#58836=CARTESIAN_POINT('Ctrl Pts',(3.11797981192923,-1.0395835969434,11.0446127766246));
#58837=CARTESIAN_POINT('Ctrl Pts',(3.0945837734477,-1.13871331705522,11.0634417597094));
#58838=CARTESIAN_POINT('Ctrl Pts',(3.08815072335477,-1.16608504285682,11.0685833365413));
#58839=CARTESIAN_POINT('Ctrl Pts',(3.07986858154633,-1.2,11.0751657410237));
#58840=CARTESIAN_POINT('',(3.30596887606183,0.653834841531101,10.8841647344426));
#58841=CARTESIAN_POINT('Ctrl Pts',(3.30596887606185,0.653834841531093,10.8841647344426));
#58842=CARTESIAN_POINT('Ctrl Pts',(3.26763302528942,0.57573341465223,10.8677423429967));
#58843=CARTESIAN_POINT('Ctrl Pts',(3.23499600897867,0.493689278811273,10.8547882313081));
#58844=CARTESIAN_POINT('Ctrl Pts',(3.18713105414667,0.338071090157941,10.8381881285872));
#58845=CARTESIAN_POINT('Ctrl Pts',(3.1698063196683,0.265613244956949,10.833545327178));
#58846=CARTESIAN_POINT('Ctrl Pts',(3.14547080626902,0.129685982985353,10.8314253163346));
#58847=CARTESIAN_POINT('Ctrl Pts',(3.1373686249214,0.0666369657923969,10.8329608190411));
#58848=CARTESIAN_POINT('Ctrl Pts',(3.12711618576932,-0.0594736424808039,
10.8414047274726));
#58849=CARTESIAN_POINT('Ctrl Pts',(3.12488792546582,-0.122671100085152,
10.848354887244));
#58850=CARTESIAN_POINT('Ctrl Pts',(3.12724247067773,-0.26004029845045,10.8688600472412));
#58851=CARTESIAN_POINT('Ctrl Pts',(3.13311315541594,-0.333905072283287,
10.8834214141036));
#58852=CARTESIAN_POINT('Ctrl Pts',(3.15646284017181,-0.491494288206911,
10.9217840503474));
#58853=CARTESIAN_POINT('Ctrl Pts',(3.17560692255383,-0.574905330097381,
10.9471365207566));
#58854=CARTESIAN_POINT('Ctrl Pts',(3.20083483798866,-0.653834841349173,
10.9758649789215));
#58855=CARTESIAN_POINT('',(3.25184183711249,1.2,10.9320268844697));
#58856=CARTESIAN_POINT('Ctrl Pts',(3.25184183711248,1.2,10.9320268844697));
#58857=CARTESIAN_POINT('Ctrl Pts',(3.26095346810344,1.13608448126568,10.924087610778));
#58858=CARTESIAN_POINT('Ctrl Pts',(3.27352444019252,1.03790800343057,10.9130694922008));
#58859=CARTESIAN_POINT('Ctrl Pts',(3.29712370513444,0.796926080875369,10.8921054224812));
#58860=CARTESIAN_POINT('Ctrl Pts',(3.30109675685001,0.741369773818892,10.8885367089974));
#58861=CARTESIAN_POINT('Ctrl Pts',(3.30596887606185,0.653834841531104,10.8841647344426));
#58862=CARTESIAN_POINT('Ctrl Pts',(3.12973060102437,1.3000000000001,10.9050352717634));
#58863=CARTESIAN_POINT('Ctrl Pts',(3.14983364557944,1.28313670183624,10.9101283089392));
#58864=CARTESIAN_POINT('Ctrl Pts',(3.17034835597043,1.26654498650491,10.9144552385832));
#58865=CARTESIAN_POINT('Ctrl Pts',(3.20438384465397,1.23847958744894,10.9222341523255));
#58866=CARTESIAN_POINT('Ctrl Pts',(3.2271445203699,1.21946594797124,10.9277276993067));
#58867=CARTESIAN_POINT('Ctrl Pts',(3.25184183711249,1.2,10.9320268844697));
#58868=CARTESIAN_POINT('Ctrl Pts',(2.70549646903679,-1.3,10.8957209484761));
#58869=CARTESIAN_POINT('Ctrl Pts',(2.6627468523952,-1.18514270861178,10.821391474375));
#58870=CARTESIAN_POINT('Ctrl Pts',(2.62751487735363,-1.06847604194512,10.757426943132));
#58871=CARTESIAN_POINT('Ctrl Pts',(2.56348922287021,-0.794772684000851,
10.6336011714019));
#58872=CARTESIAN_POINT('Ctrl Pts',(2.54183416968341,-0.636309800095197,
10.5831927997129));
#58873=CARTESIAN_POINT('Ctrl Pts',(2.5177651372377,-0.319434907277159,10.5111668553313));
#58874=CARTESIAN_POINT('Ctrl Pts',(2.5171210925739,-0.158333333333332,10.4906809863802));
#58875=CARTESIAN_POINT('Ctrl Pts',(2.53338410693288,0.158333333333334,10.4781996815688));
#58876=CARTESIAN_POINT('Ctrl Pts',(2.54937394678571,0.319434907277167,10.4868805779095));
#58877=CARTESIAN_POINT('Ctrl Pts',(2.60843787791201,0.636309800095206,10.5321053630787));
#58878=CARTESIAN_POINT('Ctrl Pts',(2.64769917658169,0.79477268400084,10.5691036076304));
#58879=CARTESIAN_POINT('Ctrl Pts',(2.74872068765945,1.06847604194511,10.6646142935774));
#58880=CARTESIAN_POINT('Ctrl Pts',(2.80123722412067,1.18514270861178,10.715339060806));
#58881=CARTESIAN_POINT('Ctrl Pts',(2.86254182811346,1.3,10.7754455583364));
#58882=CARTESIAN_POINT('Ctrl Pts',(2.64228988766393,-1.3,10.9395847985784));
#58883=CARTESIAN_POINT('Ctrl Pts',(2.60104997267594,-1.18514270861178,10.8644057917392));
#58884=CARTESIAN_POINT('Ctrl Pts',(2.5668907832622,-1.06847604194512,10.7998891011359));
#58885=CARTESIAN_POINT('Ctrl Pts',(2.50433411476486,-0.794772684000851,
10.6754747228163));
#58886=CARTESIAN_POINT('Ctrl Pts',(2.48221240828625,-0.636309800095197,
10.6256115416015));
#58887=CARTESIAN_POINT('Ctrl Pts',(2.45791319726889,-0.319434907277159,
10.5542114574271));
#58888=CARTESIAN_POINT('Ctrl Pts',(2.4563788705663,-0.158333333333332,10.5345909494989));
#58889=CARTESIAN_POINT('Ctrl Pts',(2.47285287150207,0.158333333333334,10.5224000427974));
#58890=CARTESIAN_POINT('Ctrl Pts',(2.48994083087453,0.319434907277167,10.530501641866));
#58891=CARTESIAN_POINT('Ctrl Pts',(2.54967111951957,0.636309800095206,10.5757009156449));
#58892=CARTESIAN_POINT('Ctrl Pts',(2.58959512893996,0.79477268400084,10.6124238196643));
#58893=CARTESIAN_POINT('Ctrl Pts',(2.68960290025109,1.06847604194511,10.7091497048665));
#58894=CARTESIAN_POINT('Ctrl Pts',(2.7412627929643,1.18514270861178,10.7607241252311));
#58895=CARTESIAN_POINT('Ctrl Pts',(2.80129291984328,1.3,10.8220039143035));
#58896=CARTESIAN_POINT('Ctrl Pts',(2.57908330629106,-1.3,10.9834486486808));
#58897=CARTESIAN_POINT('Ctrl Pts',(2.53935309295667,-1.18514270861178,10.9074201091034));
#58898=CARTESIAN_POINT('Ctrl Pts',(2.50626668917077,-1.06847604194512,10.8423512591397));
#58899=CARTESIAN_POINT('Ctrl Pts',(2.4451790066595,-0.794772684000851,10.7173482742307));
#58900=CARTESIAN_POINT('Ctrl Pts',(2.42259064688909,-0.636309800095197,
10.66803028349));
#58901=CARTESIAN_POINT('Ctrl Pts',(2.39806125730008,-0.319434907277159,
10.5972560595229));
#58902=CARTESIAN_POINT('Ctrl Pts',(2.39563664855869,-0.158333333333332,
10.5785009126177));
#58903=CARTESIAN_POINT('Ctrl Pts',(2.41232163607126,0.158333333333334,10.5666004040259));
#58904=CARTESIAN_POINT('Ctrl Pts',(2.43050771496334,0.319434907277167,10.5741227058226));
#58905=CARTESIAN_POINT('Ctrl Pts',(2.49090436112714,0.636309800095206,10.6192964682111));
#58906=CARTESIAN_POINT('Ctrl Pts',(2.53149108129823,0.79477268400084,10.6557440316982));
#58907=CARTESIAN_POINT('Ctrl Pts',(2.63048511284273,1.06847604194511,10.7536851161556));
#58908=CARTESIAN_POINT('Ctrl Pts',(2.68128836180793,1.18514270861178,10.8061091896562));
#58909=CARTESIAN_POINT('Ctrl Pts',(2.74004401157309,1.3,10.8685622702705));
#58910=CARTESIAN_POINT('Ctrl Pts',(2.5158767249182,-1.3,11.0273124987831));
#58911=CARTESIAN_POINT('Ctrl Pts',(2.47765621323741,-1.18514270861178,10.9504344264676));
#58912=CARTESIAN_POINT('Ctrl Pts',(2.44564259507935,-1.06847604194512,10.8848134171436));
#58913=CARTESIAN_POINT('Ctrl Pts',(2.38602389855415,-0.794772684000851,
10.7592218256451));
#58914=CARTESIAN_POINT('Ctrl Pts',(2.36296888549193,-0.636309800095197,
10.7104490253786));
#58915=CARTESIAN_POINT('Ctrl Pts',(2.33820931733127,-0.319434907277159,
10.6403006616186));
#58916=CARTESIAN_POINT('Ctrl Pts',(2.33489442655109,-0.158333333333332,
10.6224108757364));
#58917=CARTESIAN_POINT('Ctrl Pts',(2.35179040064045,0.158333333333334,10.6108007652544));
#58918=CARTESIAN_POINT('Ctrl Pts',(2.37107459905216,0.319434907277167,10.6177437697791));
#58919=CARTESIAN_POINT('Ctrl Pts',(2.4321376027347,0.636309800095206,10.6628920207773));
#58920=CARTESIAN_POINT('Ctrl Pts',(2.4733870336565,0.79477268400084,10.699064243732));
#58921=CARTESIAN_POINT('Ctrl Pts',(2.57136732543437,1.06847604194511,10.7982205274447));
#58922=CARTESIAN_POINT('Ctrl Pts',(2.62131393065155,1.18514270861178,10.8514942540813));
#58923=CARTESIAN_POINT('Ctrl Pts',(2.67879510330291,1.3,10.9151206262376));
#58924=CARTESIAN_POINT('Ctrl Pts',(2.5158767249182,-1.3,11.0273124987831));
#58925=CARTESIAN_POINT('Ctrl Pts',(2.47765621323741,-1.18514270861178,10.9504344264676));
#58926=CARTESIAN_POINT('Ctrl Pts',(2.44564259507935,-1.06847604194512,10.8848134171436));
#58927=CARTESIAN_POINT('Ctrl Pts',(2.38602389855415,-0.794772684000851,
10.7592218256451));
#58928=CARTESIAN_POINT('Ctrl Pts',(2.36296888549193,-0.636309800095197,
10.7104490253786));
#58929=CARTESIAN_POINT('Ctrl Pts',(2.33820931733128,-0.319434907277159,
10.6403006616186));
#58930=CARTESIAN_POINT('Ctrl Pts',(2.33489442655109,-0.158333333333332,
10.6224108757364));
#58931=CARTESIAN_POINT('Ctrl Pts',(2.35179040064045,0.158333333333334,10.6108007652544));
#58932=CARTESIAN_POINT('Ctrl Pts',(2.37107459905216,0.319434907277167,10.6177437697791));
#58933=CARTESIAN_POINT('Ctrl Pts',(2.4321376027347,0.636309800095206,10.6628920207773));
#58934=CARTESIAN_POINT('Ctrl Pts',(2.4733870336565,0.79477268400084,10.699064243732));
#58935=CARTESIAN_POINT('Ctrl Pts',(2.57136732543437,1.06847604194511,10.7982205274447));
#58936=CARTESIAN_POINT('Ctrl Pts',(2.62131393065155,1.18514270861178,10.8514942540813));
#58937=CARTESIAN_POINT('Ctrl Pts',(2.67879510330291,1.3,10.9151206262376));
#58938=CARTESIAN_POINT('Ctrl Pts',(2.51587672491823,-1.3000000000001,11.0273124987832));
#58939=CARTESIAN_POINT('Ctrl Pts',(2.47765621323743,-1.18514270861185,10.9504344264677));
#58940=CARTESIAN_POINT('Ctrl Pts',(2.44564259507935,-1.06847604194515,10.8848134171436));
#58941=CARTESIAN_POINT('Ctrl Pts',(2.38602389855415,-0.794772684000851,
10.7592218256451));
#58942=CARTESIAN_POINT('Ctrl Pts',(2.36296888549193,-0.636309800095197,
10.7104490253785));
#58943=CARTESIAN_POINT('Ctrl Pts',(2.33820931733127,-0.319434907277159,
10.6403006616186));
#58944=CARTESIAN_POINT('Ctrl Pts',(2.33489442655109,-0.158333333333332,
10.6224108757364));
#58945=CARTESIAN_POINT('Ctrl Pts',(2.35179040064045,0.158333333333334,10.6108007652544));
#58946=CARTESIAN_POINT('Ctrl Pts',(2.37107459905216,0.319434907277167,10.6177437697791));
#58947=CARTESIAN_POINT('Ctrl Pts',(2.4321376027347,0.636309800095206,10.6628920207773));
#58948=CARTESIAN_POINT('Ctrl Pts',(2.4733870336565,0.79477268400084,10.699064243732));
#58949=CARTESIAN_POINT('Ctrl Pts',(2.57136732543439,1.06847604194518,10.7982205274448));
#58950=CARTESIAN_POINT('Ctrl Pts',(2.62131393065161,1.18514270861191,10.8514942540814));
#58951=CARTESIAN_POINT('Ctrl Pts',(2.67879510330301,1.3000000000002,10.9151206262377));
#58952=CARTESIAN_POINT('Ctrl Pts',(2.51547129336052,-1.3000000000001,11.0360548400281));
#58953=CARTESIAN_POINT('Ctrl Pts',(2.47774091682513,-1.18514270861185,10.9586970471128));
#58954=CARTESIAN_POINT('Ctrl Pts',(2.4456831388568,-1.06847604194515,10.8928702980922));
#58955=CARTESIAN_POINT('Ctrl Pts',(2.38472809610279,-0.794772684000851,
10.7674363574331));
#58956=CARTESIAN_POINT('Ctrl Pts',(2.35825829212047,-0.636309800095197,
10.719950323469));
#58957=CARTESIAN_POINT('Ctrl Pts',(2.33182399965475,-0.319434907277159,
10.6503972076724));
#58958=CARTESIAN_POINT('Ctrl Pts',(2.3290441909677,-0.158333333333332,10.6324016146775));
#58959=CARTESIAN_POINT('Ctrl Pts',(2.34617121467972,0.158333333333334,10.6207395120507));
#58960=CARTESIAN_POINT('Ctrl Pts',(2.36541685425652,0.319434907277167,10.6276471138625));
#58961=CARTESIAN_POINT('Ctrl Pts',(2.42808446300845,0.636309800095206,10.6722759426345));
#58962=CARTESIAN_POINT('Ctrl Pts',(2.47174278263681,0.79477268400084,10.707564809271));
#58963=CARTESIAN_POINT('Ctrl Pts',(2.57119727857613,1.06847604194518,10.8064956917392));
#58964=CARTESIAN_POINT('Ctrl Pts',(2.62148033773375,1.18514270861191,10.8598450798671));
#58965=CARTESIAN_POINT('Ctrl Pts',(2.6789962899091,1.3000000000002,10.9237203428529));
#58966=CARTESIAN_POINT('Ctrl Pts',(2.51857146778973,-1.30000000000032,11.0479195112411));
#58967=CARTESIAN_POINT('Ctrl Pts',(2.48325342336936,-1.18514270861205,10.9721660225919));
#58968=CARTESIAN_POINT('Ctrl Pts',(2.45235801114653,-1.06847604194533,10.9077374417252));
#58969=CARTESIAN_POINT('Ctrl Pts',(2.39120059342659,-0.794772684000985,
10.785057333547));
#58970=CARTESIAN_POINT('Ctrl Pts',(2.35943542004083,-0.636309800095307,
10.7391265107922));
#58971=CARTESIAN_POINT('Ctrl Pts',(2.33030727174369,-0.319434907277215,
10.670568975796));
#58972=CARTESIAN_POINT('Ctrl Pts',(2.32728124734563,-0.158333333333359,
10.6516210457096));
#58973=CARTESIAN_POINT('Ctrl Pts',(2.34457235037549,0.158333333333361,10.6399062117895));
#58974=CARTESIAN_POINT('Ctrl Pts',(2.36415032204647,0.31943490727722,10.6478306450851));
#58975=CARTESIAN_POINT('Ctrl Pts',(2.43000480927062,0.636309800095314,10.6911177029276));
#58976=CARTESIAN_POINT('Ctrl Pts',(2.47974272185716,0.794772684000979,10.7240958626731));
#58977=CARTESIAN_POINT('Ctrl Pts',(2.57934531851815,1.06847604194536,10.8203168161419));
#58978=CARTESIAN_POINT('Ctrl Pts',(2.62822954911322,1.18514270861212,10.872477632872));
#58979=CARTESIAN_POINT('Ctrl Pts',(2.68288373684876,1.30000000000043,10.9351487809134));
#58980=CARTESIAN_POINT('Ctrl Pts',(2.5229571659635,-1.30000000000041,11.0653989115702));
#58981=CARTESIAN_POINT('Ctrl Pts',(2.48952415770217,-1.18514270861213,10.9928011317144));
#58982=CARTESIAN_POINT('Ctrl Pts',(2.45983648036719,-1.0684760419454,10.9308015699233));
#58983=CARTESIAN_POINT('Ctrl Pts',(2.39990447041465,-0.794772684001037,
10.8120541831117));
#58984=CARTESIAN_POINT('Ctrl Pts',(2.36657301912039,-0.636309800095346,
10.7664337210332));
#58985=CARTESIAN_POINT('Ctrl Pts',(2.33640023139148,-0.319434907277234,
10.6986777815866));
#58986=CARTESIAN_POINT('Ctrl Pts',(2.3321412631122,-0.15833333333337,10.6789419290149));
#58987=CARTESIAN_POINT('Ctrl Pts',(2.3494892057368,0.158333333333372,10.6671691177473));
#58988=CARTESIAN_POINT('Ctrl Pts',(2.37004660615991,0.319434907277242,10.6759842208015));
#58989=CARTESIAN_POINT('Ctrl Pts',(2.43769368120383,0.636309800095356,10.7180242029322));
#58990=CARTESIAN_POINT('Ctrl Pts',(2.49066133130325,0.794772684001027,10.7497428934053));
#58991=CARTESIAN_POINT('Ctrl Pts',(2.58921334045794,1.06847604194543,10.8419907638107));
#58992=CARTESIAN_POINT('Ctrl Pts',(2.63660706951893,1.18514270861219,10.891924533788));
#58993=CARTESIAN_POINT('Ctrl Pts',(2.68873501458967,1.30000000000051,10.9518613887646));
#58994=CARTESIAN_POINT('Ctrl Pts',(2.52635301603752,-1.30000000000056,11.0799823544973));
#58995=CARTESIAN_POINT('Ctrl Pts',(2.49396067914516,-1.18514270861227,11.0099259838581));
#58996=CARTESIAN_POINT('Ctrl Pts',(2.46515876836807,-1.06847604194553,10.9497039097242));
#58997=CARTESIAN_POINT('Ctrl Pts',(2.40691519525901,-0.794772684001131,
10.833298063362));
#58998=CARTESIAN_POINT('Ctrl Pts',(2.37476208248342,-0.636309800095422,
10.7863545007645));
#58999=CARTESIAN_POINT('Ctrl Pts',(2.34446960788244,-0.319434907277272,
10.7186868616691));
#59000=CARTESIAN_POINT('Ctrl Pts',(2.33822531911909,-0.158333333333389,
10.6989950561829));
#59001=CARTESIAN_POINT('Ctrl Pts',(2.35510922389385,0.158333333333391,10.6874657078855));
#59002=CARTESIAN_POINT('Ctrl Pts',(2.3764579682565,0.31943490727728,10.6968871203843));
#59003=CARTESIAN_POINT('Ctrl Pts',(2.44476635104801,0.636309800095432,10.7385059058195));
#59004=CARTESIAN_POINT('Ctrl Pts',(2.49921534396651,0.794772684001122,10.7700106903359));
#59005=CARTESIAN_POINT('Ctrl Pts',(2.5965131888299,1.06847604194556,10.8597152614524));
#59006=CARTESIAN_POINT('Ctrl Pts',(2.64273478663872,1.18514270861233,10.9080711339211));
#59007=CARTESIAN_POINT('Ctrl Pts',(2.69306135045547,1.30000000000067,10.9659530939042));
#59008=CARTESIAN_POINT('Ctrl Pts',(2.52949729038841,-1.30000000000068,11.0948340954079));
#59009=CARTESIAN_POINT('Ctrl Pts',(2.498246111899,-1.18514270861238,11.027575622754));
#59010=CARTESIAN_POINT('Ctrl Pts',(2.47044007281215,-1.06847604194563,10.9693149858493));
#59011=CARTESIAN_POINT('Ctrl Pts',(2.41416152116015,-0.794772684001209,
10.8555080601903));
#59012=CARTESIAN_POINT('Ctrl Pts',(2.38325128408465,-0.636309800095483,
10.8072772945341));
#59013=CARTESIAN_POINT('Ctrl Pts',(2.35342591954673,-0.319434907277302,
10.739467090569));
#59014=CARTESIAN_POINT('Ctrl Pts',(2.34555635753045,-0.158333333333403,
10.7195360315603));
#59015=CARTESIAN_POINT('Ctrl Pts',(2.36310790745465,0.158333333333405,10.7075878849588));
#59016=CARTESIAN_POINT('Ctrl Pts',(2.38711149284824,0.31943490727731,10.716591055916));
#59017=CARTESIAN_POINT('Ctrl Pts',(2.45557550033893,0.636309800095491,10.7579855523441));
#59018=CARTESIAN_POINT('Ctrl Pts',(2.50844634115406,0.794772684001198,10.7910229501937));
#59019=CARTESIAN_POINT('Ctrl Pts',(2.60342979908886,1.06847604194566,10.878394919682));
#59020=CARTESIAN_POINT('Ctrl Pts',(2.64843089562557,1.18514270861245,10.9249519019435));
#59021=CARTESIAN_POINT('Ctrl Pts',(2.69731826924301,1.30000000000079,10.9802457783254));
#59022=CARTESIAN_POINT('Ctrl Pts',(2.53115568101871,-1.3000000000008,11.1070342157947));
#59023=CARTESIAN_POINT('Ctrl Pts',(2.50071937953504,-1.18514270861249,11.0419082216444));
#59024=CARTESIAN_POINT('Ctrl Pts',(2.47368625233276,-1.06847604194572,10.9851123539511));
#59025=CARTESIAN_POINT('Ctrl Pts',(2.41909633392961,-0.79477268400128,10.8731467961566));
#59026=CARTESIAN_POINT('Ctrl Pts',(2.38929623923248,-0.636309800095539,
10.8238510490312));
#59027=CARTESIAN_POINT('Ctrl Pts',(2.36062812572704,-0.31943490727733,10.7554809547292));
#59028=CARTESIAN_POINT('Ctrl Pts',(2.35278188327807,-0.158333333333417,
10.7346727850495));
#59029=CARTESIAN_POINT('Ctrl Pts',(2.37090460852261,0.158333333333419,10.7223575101951));
#59030=CARTESIAN_POINT('Ctrl Pts',(2.39574478287964,0.319434907277338,10.7316613178487));
#59031=CARTESIAN_POINT('Ctrl Pts',(2.46362685357932,0.636309800095547,10.7732943129577));
#59032=CARTESIAN_POINT('Ctrl Pts',(2.51498647070657,0.794772684001268,10.807725905247));
#59033=CARTESIAN_POINT('Ctrl Pts',(2.60837910365363,1.06847604194575,10.8932897381592));
#59034=CARTESIAN_POINT('Ctrl Pts',(2.65269218043737,1.18514270861255,10.9383714982061));
#59035=CARTESIAN_POINT('Ctrl Pts',(2.70089212374016,1.3000000000009,10.9914976054846));
#59036=CARTESIAN_POINT('Ctrl Pts',(2.53311426036294,-1.30000000000088,11.1191314014661));
#59037=CARTESIAN_POINT('Ctrl Pts',(2.50368560768768,-1.18514270861256,11.0561160669588));
#59038=CARTESIAN_POINT('Ctrl Pts',(2.47752324765872,-1.06847604194579,11.0007904609959));
#59039=CARTESIAN_POINT('Ctrl Pts',(2.42462875166215,-0.794772684001331,
10.8907420546341));
#59040=CARTESIAN_POINT('Ctrl Pts',(2.39556266522996,-0.636309800095579,
10.8405576140811));
#59041=CARTESIAN_POINT('Ctrl Pts',(2.36784559501801,-0.31943490727735,10.7717264801919));
#59042=CARTESIAN_POINT('Ctrl Pts',(2.36022979153471,-0.158333333333428,
10.7498679872182));
#59043=CARTESIAN_POINT('Ctrl Pts',(2.37840647634529,0.15833333333343,10.7375054743309));
#59044=CARTESIAN_POINT('Ctrl Pts',(2.40289325713683,0.319434907277359,10.7478983619531));
#59045=CARTESIAN_POINT('Ctrl Pts',(2.47029455771141,0.636309800095589,10.7897210111506));
#59046=CARTESIAN_POINT('Ctrl Pts',(2.5218467791608,0.794772684001319,10.8245237971547));
#59047=CARTESIAN_POINT('Ctrl Pts',(2.61376060587789,1.06847604194582,10.9081066573638));
#59048=CARTESIAN_POINT('Ctrl Pts',(2.65711797522866,1.18514270861262,10.9518037873114));
#59049=CARTESIAN_POINT('Ctrl Pts',(2.70404662408732,1.30000000000098,11.0030181240723));
#59050=CARTESIAN_POINT('Ctrl Pts',(2.53754735173857,-1.30000000000107,11.1397803649751));
#59051=CARTESIAN_POINT('Ctrl Pts',(2.50931079439629,-1.18514270861273,11.0806753829874));
#59052=CARTESIAN_POINT('Ctrl Pts',(2.48422342692299,-1.06847604194595,11.0281025821637));
#59053=CARTESIAN_POINT('Ctrl Pts',(2.43354184793964,-0.794772684001446,
10.9217395403549));
#59054=CARTESIAN_POINT('Ctrl Pts',(2.40565406829729,-0.636309800095671,
10.8701032747467));
#59055=CARTESIAN_POINT('Ctrl Pts',(2.37936841418338,-0.319434907277396,
10.8006254984324));
#59056=CARTESIAN_POINT('Ctrl Pts',(2.3718237015065,-0.15833333333345,10.7771882625865));
#59057=CARTESIAN_POINT('Ctrl Pts',(2.39085375351299,0.158333333333452,10.7643015226548));
#59058=CARTESIAN_POINT('Ctrl Pts',(2.41672864221899,0.319434907277404,10.7753678578031));
#59059=CARTESIAN_POINT('Ctrl Pts',(2.48320273903407,0.63630980009568,10.8175455453742));
#59060=CARTESIAN_POINT('Ctrl Pts',(2.5324724155591,0.794772684001431,10.8545003349912));
#59061=CARTESIAN_POINT('Ctrl Pts',(2.62157979244895,1.06847604194598,10.9348071271772));
#59062=CARTESIAN_POINT('Ctrl Pts',(2.66363910270278,1.1851427086128,10.9759116346936));
#59063=CARTESIAN_POINT('Ctrl Pts',(2.70918644150855,1.30000000000118,11.023358815049));
#59064=CARTESIAN_POINT('Ctrl Pts',(2.54105191070825,-1.30000000000159,11.1706110977417));
#59065=CARTESIAN_POINT('Ctrl Pts',(2.51417660802196,-1.18514270861321,11.1172681824025));
#59066=CARTESIAN_POINT('Ctrl Pts',(2.49055089600778,-1.06847604194638,11.0686769423299));
#59067=CARTESIAN_POINT('Ctrl Pts',(2.44347797947852,-0.79477268400177,10.9673987775533));
#59068=CARTESIAN_POINT('Ctrl Pts',(2.41870862467442,-0.636309800095931,
10.9130391729152));
#59069=CARTESIAN_POINT('Ctrl Pts',(2.39535351963636,-0.319434907277527,
10.8422287662361));
#59070=CARTESIAN_POINT('Ctrl Pts',(2.38845762174984,-0.158333333333515,
10.8161996107113));
#59071=CARTESIAN_POINT('Ctrl Pts',(2.40788738242878,0.158333333333517,10.8030575116266));
#59072=CARTESIAN_POINT('Ctrl Pts',(2.43309353593705,0.319434907277534,10.8166301418116));
#59073=CARTESIAN_POINT('Ctrl Pts',(2.49830601568335,0.636309800095939,10.8592745745622));
#59074=CARTESIAN_POINT('Ctrl Pts',(2.54726271990942,0.79477268400176,10.8975846532159));
#59075=CARTESIAN_POINT('Ctrl Pts',(2.63319751287982,1.06847604194641,10.9726989423475));
#59076=CARTESIAN_POINT('Ctrl Pts',(2.67337024206067,1.18514270861328,11.0101028369147));
#59077=CARTESIAN_POINT('Ctrl Pts',(2.71651771274338,1.30000000000169,11.0523964335426));
#59078=CARTESIAN_POINT('Ctrl Pts',(2.54573452006115,-1.30000000000214,11.2008309367231));
#59079=CARTESIAN_POINT('Ctrl Pts',(2.52086608529417,-1.18514270861371,11.1529297276386));
#59080=CARTESIAN_POINT('Ctrl Pts',(2.49882047056423,-1.06847604194683,11.1082635887547));
#59081=CARTESIAN_POINT('Ctrl Pts',(2.45441196931678,-0.794772684002102,
11.012549531839));
#59082=CARTESIAN_POINT('Ctrl Pts',(2.42963382118069,-0.636309800096196,
10.9570191287474));
#59083=CARTESIAN_POINT('Ctrl Pts',(2.40791535751862,-0.31943490727766,10.8855638121978));
#59084=CARTESIAN_POINT('Ctrl Pts',(2.40224133814692,-0.158333333333581,
10.8567451642823));
#59085=CARTESIAN_POINT('Ctrl Pts',(2.4227463682387,0.158333333333583,10.8430023574533));
#59086=CARTESIAN_POINT('Ctrl Pts',(2.44848527367546,0.319434907277667,10.8583709235438));
#59087=CARTESIAN_POINT('Ctrl Pts',(2.5128675489143,0.636309800096204,10.9012368723411));
#59088=CARTESIAN_POINT('Ctrl Pts',(2.56049934069731,0.794772684002089,10.9414699237767));
#59089=CARTESIAN_POINT('Ctrl Pts',(2.64370514089814,1.06847604194686,11.0111681329601));
#59090=CARTESIAN_POINT('Ctrl Pts',(2.68243485838104,1.18514270861377,11.0446394012812));
#59091=CARTESIAN_POINT('Ctrl Pts',(2.72387758551865,1.30000000000224,11.0814121657409));
#59092=CARTESIAN_POINT('Ctrl Pts',(2.54836608072529,-1.30000000000248,11.2255071987808));
#59093=CARTESIAN_POINT('Ctrl Pts',(2.52393507525495,-1.18514270861402,11.1824878552591));
#59094=CARTESIAN_POINT('Ctrl Pts',(2.5024945085245,-1.06847604194711,11.1412612342161));
#59095=CARTESIAN_POINT('Ctrl Pts',(2.45987102193083,-0.794772684002315,
11.0501610398079));
#59096=CARTESIAN_POINT('Ctrl Pts',(2.43704879532756,-0.636309800096365,
10.9927988361827));
#59097=CARTESIAN_POINT('Ctrl Pts',(2.41716111947609,-0.319434907277745,
10.9206309940565));
#59098=CARTESIAN_POINT('Ctrl Pts',(2.41189670128007,-0.158333333333623,
10.8898972969641));
#59099=CARTESIAN_POINT('Ctrl Pts',(2.43312364813147,0.158333333333625,10.875776020971));
#59100=CARTESIAN_POINT('Ctrl Pts',(2.45928344885959,0.319434907277752,10.8925936823699));
#59101=CARTESIAN_POINT('Ctrl Pts',(2.52308425970147,0.636309800096373,10.9355794423511));
#59102=CARTESIAN_POINT('Ctrl Pts',(2.56984233349844,0.794772684002302,10.9772056763508));
#59103=CARTESIAN_POINT('Ctrl Pts',(2.65098016815178,1.06847604194714,11.0424969464296));
#59104=CARTESIAN_POINT('Ctrl Pts',(2.68858640056851,1.18514270861408,11.0728076022862));
#59105=CARTESIAN_POINT('Ctrl Pts',(2.72867730323362,1.30000000000258,11.1051667424625));
#59106=CARTESIAN_POINT('Ctrl Pts',(2.54980989363998,-1.30000000000297,11.2393849186444));
#59107=CARTESIAN_POINT('Ctrl Pts',(2.52612452584294,-1.18514270861447,11.198879185939));
#59108=CARTESIAN_POINT('Ctrl Pts',(2.50533570791932,-1.06847604194751,11.1594418349136));
#59109=CARTESIAN_POINT('Ctrl Pts',(2.46400098938739,-0.794772684002612,
11.0708018400401));
#59110=CARTESIAN_POINT('Ctrl Pts',(2.44180654845669,-0.636309800096603,
11.0126237558631));
#59111=CARTESIAN_POINT('Ctrl Pts',(2.42260741951521,-0.319434907277864,
10.9402126409294));
#59112=CARTESIAN_POINT('Ctrl Pts',(2.41731072158857,-0.158333333333682,
10.9085257012698));
#59113=CARTESIAN_POINT('Ctrl Pts',(2.43873104500735,0.158333333333684,10.8942947595499));
#59114=CARTESIAN_POINT('Ctrl Pts',(2.46501515299822,0.319434907277872,10.9119896164857));
#59115=CARTESIAN_POINT('Ctrl Pts',(2.5287277517617,0.636309800096611,10.9549267892209));
#59116=CARTESIAN_POINT('Ctrl Pts',(2.57570949841196,0.794772684002596,10.9969773639694));
#59117=CARTESIAN_POINT('Ctrl Pts',(2.65571139818719,1.06847604194754,11.0597836540679));
#59118=CARTESIAN_POINT('Ctrl Pts',(2.69254102065129,1.18514270861453,11.0883937347858));
#59119=CARTESIAN_POINT('Ctrl Pts',(2.73157040752932,1.30000000000308,11.1184273804406));
#59120=CARTESIAN_POINT('Ctrl Pts',(2.55054244654307,-1.30000000000299,11.2487391367418));
#59121=CARTESIAN_POINT('Ctrl Pts',(2.52732873238259,-1.18514270861449,11.2099260883804));
#59122=CARTESIAN_POINT('Ctrl Pts',(2.50694403362782,-1.06847604194753,11.1717000363166));
#59123=CARTESIAN_POINT('Ctrl Pts',(2.46638689308905,-0.794772684002624,
11.0847462878297));
#59124=CARTESIAN_POINT('Ctrl Pts',(2.44450444954104,-0.636309800096613,
11.0260748419584));
#59125=CARTESIAN_POINT('Ctrl Pts',(2.42574179818932,-0.319434907277869,
10.9535202363304));
#59126=CARTESIAN_POINT('Ctrl Pts',(2.42047967216221,-0.158333333333685,
10.9211814492335));
#59127=CARTESIAN_POINT('Ctrl Pts',(2.44211395856567,0.158333333333686,10.9068395144513));
#59128=CARTESIAN_POINT('Ctrl Pts',(2.46864358766412,0.319434907277877,10.9250337490112));
#59129=CARTESIAN_POINT('Ctrl Pts',(2.53222083393765,0.636309800096621,10.9679728127198));
#59130=CARTESIAN_POINT('Ctrl Pts',(2.57888464825532,0.794772684002608,11.0105378218198));
#59131=CARTESIAN_POINT('Ctrl Pts',(2.65828389481309,1.06847604194756,11.0716024122322));
#59132=CARTESIAN_POINT('Ctrl Pts',(2.69479503048837,1.18514270861455,11.0989748818083));
#59133=CARTESIAN_POINT('Ctrl Pts',(2.73344831003611,1.30000000000309,11.1272872224371));
#59134=CARTESIAN_POINT('Ctrl Pts',(2.55109152476668,-1.30000000000301,11.2549467364805));
#59135=CARTESIAN_POINT('Ctrl Pts',(2.52807171161312,-1.1851427086145,11.2173141635663));
#59136=CARTESIAN_POINT('Ctrl Pts',(2.50787758280969,-1.06847604194754,11.1799299336598));
#59137=CARTESIAN_POINT('Ctrl Pts',(2.46775300157717,-0.794772684002634,
11.0941386059151));
#59138=CARTESIAN_POINT('Ctrl Pts',(2.44615279179159,-0.636309800096621,
11.035109988901));
#59139=CARTESIAN_POINT('Ctrl Pts',(2.42776583447895,-0.319434907277873,
10.9624211245349));
#59140=CARTESIAN_POINT('Ctrl Pts',(2.42267338937598,-0.158333333333687,
10.9295749559879));
#59141=CARTESIAN_POINT('Ctrl Pts',(2.44443627628138,0.158333333333688,10.9151679786746));
#59142=CARTESIAN_POINT('Ctrl Pts',(2.47097314162531,0.319434907277881,10.9337745236639));
#59143=CARTESIAN_POINT('Ctrl Pts',(2.5343382262495,0.636309800096629,10.9767765250291));
#59144=CARTESIAN_POINT('Ctrl Pts',(2.58073260912702,0.794772684002619,11.019711698812));
#59145=CARTESIAN_POINT('Ctrl Pts',(2.65969549076213,1.06847604194757,11.0796337120957));
#59146=CARTESIAN_POINT('Ctrl Pts',(2.69599491986027,1.18514270861457,11.1061818466973));
#59147=CARTESIAN_POINT('Ctrl Pts',(2.73441367245983,1.30000000000311,11.1333400966794));
#59148=CARTESIAN_POINT('Ctrl Pts',(2.55189116477321,-1.30000000000311,11.262654253516));
#59149=CARTESIAN_POINT('Ctrl Pts',(2.52899683365425,-1.1851427086146,11.2265472851811));
#59150=CARTESIAN_POINT('Ctrl Pts',(2.50896306374532,-1.06847604194763,11.1902488904775));
#59151=CARTESIAN_POINT('Ctrl Pts',(2.46928951616223,-0.794772684002696,
11.1059501040369));
#59152=CARTESIAN_POINT('Ctrl Pts',(2.4481159970497,-0.63630980009667,11.04644652644));
#59153=CARTESIAN_POINT('Ctrl Pts',(2.43024865253925,-0.319434907277897,
10.9735674216262));
#59154=CARTESIAN_POINT('Ctrl Pts',(2.4254499088154,-0.158333333333699,10.9400458510263));
#59155=CARTESIAN_POINT('Ctrl Pts',(2.44736033776891,0.158333333333701,10.9255647667845));
#59156=CARTESIAN_POINT('Ctrl Pts',(2.47379113461325,0.319434907277905,10.9447442922543));
#59157=CARTESIAN_POINT('Ctrl Pts',(2.53685547682693,0.636309800096678,10.9878432584808));
#59158=CARTESIAN_POINT('Ctrl Pts',(2.58299396834651,0.794772684002679,11.0312002969059));
#59159=CARTESIAN_POINT('Ctrl Pts',(2.66136955241411,1.06847604194765,11.0897169836481));
#59160=CARTESIAN_POINT('Ctrl Pts',(2.69736482543664,1.18514270861466,11.1152557748196));
#59161=CARTESIAN_POINT('Ctrl Pts',(2.73542948524044,1.30000000000321,11.1410036517289));
#59162=CARTESIAN_POINT('Ctrl Pts',(2.55305163254526,-1.30000000000315,11.2718129170802));
#59163=CARTESIAN_POINT('Ctrl Pts',(2.53025793961708,-1.18514270861464,11.2375568285257));
#59164=CARTESIAN_POINT('Ctrl Pts',(2.51037156929255,-1.06847604194766,11.2025800147505));
#59165=CARTESIAN_POINT('Ctrl Pts',(2.47114657241043,-0.794772684002722,
11.1201115584019));
#59166=CARTESIAN_POINT('Ctrl Pts',(2.45039055789746,-0.636309800096692,
11.0600811018468));
#59167=CARTESIAN_POINT('Ctrl Pts',(2.43317556682532,-0.319434907277908,
10.9869606787218));
#59168=CARTESIAN_POINT('Ctrl Pts',(2.42884313323382,-0.158333333333704,
10.9525799635657));
#59169=CARTESIAN_POINT('Ctrl Pts',(2.45108764636289,0.158333333333706,10.9379354534527));
#59170=CARTESIAN_POINT('Ctrl Pts',(2.47746497352781,0.319434907277916,10.9577646524049));
#59171=CARTESIAN_POINT('Ctrl Pts',(2.54039704684755,0.636309800096699,11.0008658409722));
#59172=CARTESIAN_POINT('Ctrl Pts',(2.58646885103811,0.794772684002707,11.0446111075323));
#59173=CARTESIAN_POINT('Ctrl Pts',(2.66426303314084,1.06847604194769,11.1013745995807));
#59174=CARTESIAN_POINT('Ctrl Pts',(2.69990460744472,1.1851427086147,11.1256927459517));
#59175=CARTESIAN_POINT('Ctrl Pts',(2.73751353717874,1.30000000000325,11.1497582262806));
#59176=CARTESIAN_POINT('Ctrl Pts',(2.55465518880791,-1.30000000000359,11.2904402301687));
#59177=CARTESIAN_POINT('Ctrl Pts',(2.53259793086932,-1.18514270861504,11.2596522944168));
#59178=CARTESIAN_POINT('Ctrl Pts',(2.51339426131821,-1.06847604194802,11.2271485250168));
#59179=CARTESIAN_POINT('Ctrl Pts',(2.47562230300768,-0.794772684002991,
11.1480943963678));
#59180=CARTESIAN_POINT('Ctrl Pts',(2.45581184919151,-0.636309800096907,
11.0869461896583));
#59181=CARTESIAN_POINT('Ctrl Pts',(2.43943340999145,-0.319434907278017,
11.013562248177));
#59182=CARTESIAN_POINT('Ctrl Pts',(2.43507099426907,-0.158333333333758,
10.9779177197142));
#59183=CARTESIAN_POINT('Ctrl Pts',(2.45731084375769,0.15833333333376,10.9632615584176));
#59184=CARTESIAN_POINT('Ctrl Pts',(2.48342526756427,0.319434907278024,10.9844604526388));
#59185=CARTESIAN_POINT('Ctrl Pts',(2.54609837666543,0.636309800096915,11.0275620203848));
#59186=CARTESIAN_POINT('Ctrl Pts',(2.5924380157363,0.794772684002976,11.0718931738382));
#59187=CARTESIAN_POINT('Ctrl Pts',(2.66931583504373,1.06847604194805,11.1250392686005));
#59188=CARTESIAN_POINT('Ctrl Pts',(2.70433250886816,1.1851427086151,11.1468810309115));
#59189=CARTESIAN_POINT('Ctrl Pts',(2.74108829714278,1.3000000000037,11.1675595803679));
#59190=CARTESIAN_POINT('Ctrl Pts',(2.55613434706331,-1.30000000000444,11.3187390268946));
#59191=CARTESIAN_POINT('Ctrl Pts',(2.5344480287897,-1.18514270861581,11.2934483376249));
#59192=CARTESIAN_POINT('Ctrl Pts',(2.51572174253609,-1.06847604194872,11.2648804522911));
#59193=CARTESIAN_POINT('Ctrl Pts',(2.47929854122811,-0.794772684003508,
11.1913119436756));
#59194=CARTESIAN_POINT('Ctrl Pts',(2.46054545403437,-0.636309800097323,
11.1286997802178));
#59195=CARTESIAN_POINT('Ctrl Pts',(2.44617199533978,-0.319434907278226,
11.0546191416089));
#59196=CARTESIAN_POINT('Ctrl Pts',(2.44323962778225,-0.158333333333861,
11.016443183048));
#59197=CARTESIAN_POINT('Ctrl Pts',(2.46696406362689,0.158333333333863,11.0010985155435));
#59198=CARTESIAN_POINT('Ctrl Pts',(2.49395365349794,0.319434907278231,11.0237309533097));
#59199=CARTESIAN_POINT('Ctrl Pts',(2.55597421771634,0.636309800097329,11.0669606588986));
#59200=CARTESIAN_POINT('Ctrl Pts',(2.60024222388047,0.794772684003496,11.1133466204794));
#59201=CARTESIAN_POINT('Ctrl Pts',(2.67532016924119,1.06847604194875,11.1612729977404));
#59202=CARTESIAN_POINT('Ctrl Pts',(2.70962808975909,1.18514270861587,11.1792940119223));
#59203=CARTESIAN_POINT('Ctrl Pts',(2.74574547016027,1.30000000000455,11.194590487417));
#59204=CARTESIAN_POINT('Ctrl Pts',(2.55860850442848,-1.30000000000579,11.3497860913864));
#59205=CARTESIAN_POINT('Ctrl Pts',(2.53751545758815,-1.18514270861704,11.3305075424009));
#59206=CARTESIAN_POINT('Ctrl Pts',(2.51937753972003,-1.06847604194983,11.3062765270361));
#59207=CARTESIAN_POINT('Ctrl Pts',(2.48430226006394,-0.794772684004337,
11.2388568460718));
#59208=CARTESIAN_POINT('Ctrl Pts',(2.46629217650461,-0.636309800097985,
11.174810769052));
#59209=CARTESIAN_POINT('Ctrl Pts',(2.45341294639711,-0.319434907278558,
11.1002998138001));
#59210=CARTESIAN_POINT('Ctrl Pts',(2.4518247445549,-0.158333333334026,11.0594421998351));
#59211=CARTESIAN_POINT('Ctrl Pts',(2.47582090449258,0.158333333334028,11.0439815364231));
#59212=CARTESIAN_POINT('Ctrl Pts',(2.50142593506735,0.319434907278566,11.0693057595259));
#59213=CARTESIAN_POINT('Ctrl Pts',(2.56314151434006,0.636309800097994,11.112472597192));
#59214=CARTESIAN_POINT('Ctrl Pts',(2.60884216623242,0.794772684004321,11.1593650834696));
#59215=CARTESIAN_POINT('Ctrl Pts',(2.68264613957165,1.06847604194986,11.2011751195402));
#59216=CARTESIAN_POINT('Ctrl Pts',(2.71587396605832,1.18514270861711,11.2151093124084));
#59217=CARTESIAN_POINT('Ctrl Pts',(2.75038261367983,1.3000000000059,11.2248796827443));
#59218=CARTESIAN_POINT('Ctrl Pts',(2.55905629130214,-1.30000000000684,11.3752444867707));
#59219=CARTESIAN_POINT('Ctrl Pts',(2.53856232140629,-1.18514270861799,11.360711619204));
#59220=CARTESIAN_POINT('Ctrl Pts',(2.52098885206739,-1.06847604195069,11.3399027700454));
#59221=CARTESIAN_POINT('Ctrl Pts',(2.48713756286471,-0.794772684004976,
11.2773313927096));
#59222=CARTESIAN_POINT('Ctrl Pts',(2.46980256661799,-0.636309800098496,
11.2121016469838));
#59223=CARTESIAN_POINT('Ctrl Pts',(2.45797412929981,-0.319434907278815,
11.137329505581));
#59224=CARTESIAN_POINT('Ctrl Pts',(2.45660151427198,-0.158333333334153,
11.0947466834272));
#59225=CARTESIAN_POINT('Ctrl Pts',(2.48167304904669,0.158333333334155,11.0788160349185));
#59226=CARTESIAN_POINT('Ctrl Pts',(2.50882228821183,0.319434907278822,11.1050728297802));
#59227=CARTESIAN_POINT('Ctrl Pts',(2.57028342039218,0.636309800098504,11.148200745329));
#59228=CARTESIAN_POINT('Ctrl Pts',(2.61397394650306,0.794772684004962,11.1969542390301));
#59229=CARTESIAN_POINT('Ctrl Pts',(2.68644480929014,1.06847604195072,11.2340180199183));
#59230=CARTESIAN_POINT('Ctrl Pts',(2.71921743764465,1.18514270861806,11.2444948363823));
#59231=CARTESIAN_POINT('Ctrl Pts',(2.75339274316326,1.30000000000694,11.2494049319124));
#59232=CARTESIAN_POINT('Ctrl Pts',(2.55994262970328,-1.30000000000743,11.3892732428768));
#59233=CARTESIAN_POINT('Ctrl Pts',(2.53918094648869,-1.18514270861853,11.3776508559804));
#59234=CARTESIAN_POINT('Ctrl Pts',(2.52156741134895,-1.06847604195118,11.3589108084953));
#59235=CARTESIAN_POINT('Ctrl Pts',(2.48814947343831,-0.794772684005335,
11.2991743300279));
#59236=CARTESIAN_POINT('Ctrl Pts',(2.47217241768286,-0.636309800098786,
11.2328962879459));
#59237=CARTESIAN_POINT('Ctrl Pts',(2.46094499315259,-0.319434907278961,
11.1579852824741));
#59238=CARTESIAN_POINT('Ctrl Pts',(2.45936890050809,-0.158333333334225,
11.1145552122263));
#59239=CARTESIAN_POINT('Ctrl Pts',(2.48418278940801,0.158333333334227,11.0987427049723));
#59240=CARTESIAN_POINT('Ctrl Pts',(2.5107119643918,0.319434907278967,11.1262000669487));
#59241=CARTESIAN_POINT('Ctrl Pts',(2.57219996693816,0.636309800098794,11.1692284516201));
#59242=CARTESIAN_POINT('Ctrl Pts',(2.61683048394594,0.794772684005325,11.218088941301));
#59243=CARTESIAN_POINT('Ctrl Pts',(2.68916196690512,1.06847604195121,11.252211993919));
#59244=CARTESIAN_POINT('Ctrl Pts',(2.72165838093492,1.1851427086186,11.2607572364805));
#59245=CARTESIAN_POINT('Ctrl Pts',(2.75534159016708,1.30000000000753,11.2630771165088));
#59246=CARTESIAN_POINT('Ctrl Pts',(2.56043963205252,-1.30000000000761,11.3986684693826));
#59247=CARTESIAN_POINT('Ctrl Pts',(2.53971559392325,-1.18514270861869,11.3889000088412));
#59248=CARTESIAN_POINT('Ctrl Pts',(2.52216612868449,-1.06847604195132,11.3715024840624));
#59249=CARTESIAN_POINT('Ctrl Pts',(2.48895725167271,-0.794772684005442,
11.3136860568827));
#59250=CARTESIAN_POINT('Ctrl Pts',(2.47314153776399,-0.636309800098872,
11.2470051381599));
#59251=CARTESIAN_POINT('Ctrl Pts',(2.46233031765432,-0.319434907279004,
11.171990172431));
#59252=CARTESIAN_POINT('Ctrl Pts',(2.46113595337433,-0.158333333334247,
11.1277883569861));
#59253=CARTESIAN_POINT('Ctrl Pts',(2.48627126153669,0.158333333334249,11.1118421866752));
#59254=CARTESIAN_POINT('Ctrl Pts',(2.51288193508593,0.319434907279011,11.1398722695075));
#59255=CARTESIAN_POINT('Ctrl Pts',(2.57431958909811,0.63630980009888,11.1828654886432));
#59256=CARTESIAN_POINT('Ctrl Pts',(2.61878266938189,0.794772684005431,11.2321557830996));
#59257=CARTESIAN_POINT('Ctrl Pts',(2.6907660779171,1.06847604195135,11.2644332938282));
#59258=CARTESIAN_POINT('Ctrl Pts',(2.72307264878172,1.18514270861876,11.2716932006324));
#59259=CARTESIAN_POINT('Ctrl Pts',(2.75652684020421,1.30000000000771,11.2722412758461));
#59260=CARTESIAN_POINT('Ctrl Pts',(2.56074962849714,-1.30000000000768,11.4049426372132));
#59261=CARTESIAN_POINT('Ctrl Pts',(2.54019409865066,-1.18514270861876,11.396352129411));
#59262=CARTESIAN_POINT('Ctrl Pts',(2.52276515408483,-1.06847604195138,11.3798179070198));
#59263=CARTESIAN_POINT('Ctrl Pts',(2.48972384295886,-0.794772684005487,
11.3232689758011));
#59264=CARTESIAN_POINT('Ctrl Pts',(2.47375221387631,-0.636309800098908,
11.256423467468));
#59265=CARTESIAN_POINT('Ctrl Pts',(2.46313517489945,-0.319434907279023,
11.1813728839924));
#59266=CARTESIAN_POINT('Ctrl Pts',(2.462244652973,-0.158333333334256,11.1366394146029));
#59267=CARTESIAN_POINT('Ctrl Pts',(2.48763458590687,0.158333333334258,11.1205881948526));
#59268=CARTESIAN_POINT('Ctrl Pts',(2.5143615223482,0.319434907279029,11.1489735521833));
#59269=CARTESIAN_POINT('Ctrl Pts',(2.57578657574276,0.636309800098917,11.1919337050089));
#59270=CARTESIAN_POINT('Ctrl Pts',(2.6201004340866,0.794772684005478,11.241524759152));
#59271=CARTESIAN_POINT('Ctrl Pts',(2.69183909251073,1.06847604195141,11.2725770687319));
#59272=CARTESIAN_POINT('Ctrl Pts',(2.72401603463284,1.18514270861883,11.2789816445278));
#59273=CARTESIAN_POINT('Ctrl Pts',(2.75731691182452,1.30000000000778,11.2783494019041));
#59274=CARTESIAN_POINT('Ctrl Pts',(2.56103579688896,-1.30000000000785,11.4160227709829));
#59275=CARTESIAN_POINT('Ctrl Pts',(2.54076331719582,-1.18514270861891,11.4094926909521));
#59276=CARTESIAN_POINT('Ctrl Pts',(2.52354853451578,-1.06847604195152,11.3944645225392));
#59277=CARTESIAN_POINT('Ctrl Pts',(2.4908428345099,-0.79477268400559,11.3401141629314));
#59278=CARTESIAN_POINT('Ctrl Pts',(2.47470146542819,-0.63630980009899,11.2729465823724));
#59279=CARTESIAN_POINT('Ctrl Pts',(2.46446875723411,-0.319434907279063,
11.197819192777));
#59280=CARTESIAN_POINT('Ctrl Pts',(2.46406873556494,-0.158333333334276,
11.1521726753847));
#59281=CARTESIAN_POINT('Ctrl Pts',(2.48992192949735,0.158333333334278,11.135931025976));
#59282=CARTESIAN_POINT('Ctrl Pts',(2.51690809226955,0.31943490727907,11.1649136564021));
#59283=CARTESIAN_POINT('Ctrl Pts',(2.57830893439958,0.636309800098998,11.2078180430919));
#59284=CARTESIAN_POINT('Ctrl Pts',(2.62228210208185,0.794772684005578,11.2579713983951));
#59285=CARTESIAN_POINT('Ctrl Pts',(2.6936023450048,1.06847604195155,11.2868764756407));
#59286=CARTESIAN_POINT('Ctrl Pts',(2.72557456179929,1.18514270861898,11.2917749851617));
#59287=CARTESIAN_POINT('Ctrl Pts',(2.75864710490237,1.30000000000795,11.2890600673027));
#59288=CARTESIAN_POINT('Ctrl Pts',(2.56112206126383,-1.30000000000865,11.4263687093571));
#59289=CARTESIAN_POINT('Ctrl Pts',(2.540699396725,-1.18514270861965,11.4219114957384));
#59290=CARTESIAN_POINT('Ctrl Pts',(2.5234670531941,-1.06847604195218,11.4083652099156));
#59291=CARTESIAN_POINT('Ctrl Pts',(2.49102717206907,-0.794772684006079,
11.3560730046852));
#59292=CARTESIAN_POINT('Ctrl Pts',(2.47555119068125,-0.636309800099382,
11.2882854431247));
#59293=CARTESIAN_POINT('Ctrl Pts',(2.46594535857682,-0.31943490727926,11.21298322481));
#59294=CARTESIAN_POINT('Ctrl Pts',(2.46593945638988,-0.158333333334374,
11.1665098238689));
#59295=CARTESIAN_POINT('Ctrl Pts',(2.4919045200863,0.158333333334376,11.150229554003));
#59296=CARTESIAN_POINT('Ctrl Pts',(2.51854886381738,0.319434907279267,11.1800188124387));
#59297=CARTESIAN_POINT('Ctrl Pts',(2.57967203893382,0.636309800099391,11.2229819527419));
#59298=CARTESIAN_POINT('Ctrl Pts',(2.62345772028888,0.794772684006069,11.2736002846783));
#59299=CARTESIAN_POINT('Ctrl Pts',(2.69463519912823,1.06847604195221,11.3004076861347));
#59300=CARTESIAN_POINT('Ctrl Pts',(2.72657802782751,1.18514270861971,11.3038400737063));
#59301=CARTESIAN_POINT('Ctrl Pts',(2.75965359202203,1.30000000000876,11.299100918071));
#59302=CARTESIAN_POINT('Ctrl Pts',(2.56129546843634,-1.30000000000876,11.4342848832129));
#59303=CARTESIAN_POINT('Ctrl Pts',(2.54091671291285,-1.18514270861975,11.4313604430906));
#59304=CARTESIAN_POINT('Ctrl Pts',(2.52374737348591,-1.06847604195227,11.4189243389879));
#59305=CARTESIAN_POINT('Ctrl Pts',(2.49149715791968,-0.794772684006148,
11.3682206040802));
#59306=CARTESIAN_POINT('Ctrl Pts',(2.4761305193737,-0.636309800099438,11.3001113323577));
#59307=CARTESIAN_POINT('Ctrl Pts',(2.46692567203707,-0.319434907279288,
11.2247053495164));
#59308=CARTESIAN_POINT('Ctrl Pts',(2.46740121156712,-0.158333333334387,
11.1775278104391));
#59309=CARTESIAN_POINT('Ctrl Pts',(2.49354674043552,0.158333333334389,11.161178234315));
#59310=CARTESIAN_POINT('Ctrl Pts',(2.5199846193292,0.319434907279294,11.1915600622205));
#59311=CARTESIAN_POINT('Ctrl Pts',(2.5808818906959,0.636309800099446,11.2345718806749));
#59312=CARTESIAN_POINT('Ctrl Pts',(2.62441089832543,0.794772684006138,11.2855955914427));
#59313=CARTESIAN_POINT('Ctrl Pts',(2.69543525206671,1.0684760419523,11.3108084753575));
#59314=CARTESIAN_POINT('Ctrl Pts',(2.72735024371145,1.18514270861981,11.3131159302143));
#59315=CARTESIAN_POINT('Ctrl Pts',(2.76043641597799,1.30000000000887,11.3068171167106));
#59316=CARTESIAN_POINT('Ctrl Pts',(2.56135170972681,-1.30000000000878,11.4374560436823));
#59317=CARTESIAN_POINT('Ctrl Pts',(2.54098523470469,-1.18514270861976,11.4351463180369));
#59318=CARTESIAN_POINT('Ctrl Pts',(2.52383902071098,-1.06847604195228,11.4231548492346));
#59319=CARTESIAN_POINT('Ctrl Pts',(2.49166728348375,-0.794772684006158,
11.3730853938981));
#59320=CARTESIAN_POINT('Ctrl Pts',(2.47636415999359,-0.636309800099446,
11.304840460273));
#59321=CARTESIAN_POINT('Ctrl Pts',(2.46731911733327,-0.319434907279292,
11.2293936628138));
#59322=CARTESIAN_POINT('Ctrl Pts',(2.46796493347666,-0.158333333334389,
11.1819434771854));
#59323=CARTESIAN_POINT('Ctrl Pts',(2.49418543138234,0.158333333334391,11.1655649762754));
#59324=CARTESIAN_POINT('Ctrl Pts',(2.52056038064123,0.319434907279298,11.1961756769492));
#59325=CARTESIAN_POINT('Ctrl Pts',(2.58138460232752,0.636309800099453,11.239199638653));
#59326=CARTESIAN_POINT('Ctrl Pts',(2.62482644752311,0.794772684006148,11.2903787340127));
#59327=CARTESIAN_POINT('Ctrl Pts',(2.69578560891973,1.06847604195231,11.3149555468183));
#59328=CARTESIAN_POINT('Ctrl Pts',(2.72768216853481,1.18514270861983,11.3168162007128));
#59329=CARTESIAN_POINT('Ctrl Pts',(2.76075969609242,1.30000000000888,11.3098991168989));
#59330=CARTESIAN_POINT('Ctrl Pts',(2.56140557135158,-1.30000000000887,11.4414254376085));
#59331=CARTESIAN_POINT('Ctrl Pts',(2.54104555333389,-1.18514270861985,11.4398867089293));
#59332=CARTESIAN_POINT('Ctrl Pts',(2.52392434518461,-1.06847604195236,11.4284520593091));
#59333=CARTESIAN_POINT('Ctrl Pts',(2.49185322799154,-0.794772684006215,
11.3791741741465));
#59334=CARTESIAN_POINT('Ctrl Pts',(2.47665973194801,-0.636309800099492,
11.3107490308637));
#59335=CARTESIAN_POINT('Ctrl Pts',(2.46781118185094,-0.319434907279315,
11.2352532787707));
#59336=CARTESIAN_POINT('Ctrl Pts',(2.46863056405601,-0.158333333334401,
11.187478369364));
#59337=CARTESIAN_POINT('Ctrl Pts',(2.49495184665048,0.158333333334403,11.1710606307331));
#59338=CARTESIAN_POINT('Ctrl Pts',(2.52128802686867,0.319434907279321,11.2019405645075));
#59339=CARTESIAN_POINT('Ctrl Pts',(2.58205176647432,0.6363098000995,11.2449666625359));
#59340=CARTESIAN_POINT('Ctrl Pts',(2.62540694357562,0.794772684006205,11.2963303662771));
#59341=CARTESIAN_POINT('Ctrl Pts',(2.69627572005436,1.06847604195239,11.3201162448801));
#59342=CARTESIAN_POINT('Ctrl Pts',(2.72813605567496,1.18514270861991,11.3214242688008));
#59343=CARTESIAN_POINT('Ctrl Pts',(2.76118025952548,1.30000000000898,11.3137442911486));
#59344=CARTESIAN_POINT('Ctrl Pts',(2.56141229749596,-1.3000000000089,11.446209086765));
#59345=CARTESIAN_POINT('Ctrl Pts',(2.54101000436551,-1.18514270861988,11.445613246977));
#59346=CARTESIAN_POINT('Ctrl Pts',(2.52389520829441,-1.06847604195239,11.4348550346065));
#59347=CARTESIAN_POINT('Ctrl Pts',(2.49195138143556,-0.794772684006233,
11.3865242982164));
#59348=CARTESIAN_POINT('Ctrl Pts',(2.47702990295093,-0.636309800099506,
11.317831298212));
#59349=CARTESIAN_POINT('Ctrl Pts',(2.46842316379507,-0.319434907279323,
11.242276596958));
#59350=CARTESIAN_POINT('Ctrl Pts',(2.46932820638159,-0.158333333334405,
11.1941611977995));
#59351=CARTESIAN_POINT('Ctrl Pts',(2.49577070833345,0.158333333334406,11.1776961065491));
#59352=CARTESIAN_POINT('Ctrl Pts',(2.52214156267838,0.319434907279329,11.2088659098694));
#59353=CARTESIAN_POINT('Ctrl Pts',(2.58291220881987,0.636309800099515,11.2518611590204));
#59354=CARTESIAN_POINT('Ctrl Pts',(2.62624751185239,0.794772684006224,11.3034099160023));
#59355=CARTESIAN_POINT('Ctrl Pts',(2.6969959403622,1.06847604195242,11.3262520270084));
#59356=CARTESIAN_POINT('Ctrl Pts',(2.72878085125029,1.18514270861994,11.3269107772538));
#59357=CARTESIAN_POINT('Ctrl Pts',(2.76172629981222,1.30000000000901,11.3183407742738));
#59358=CARTESIAN_POINT('Ctrl Pts',(2.56137136298278,-1.30000000000901,11.4510090609822));
#59359=CARTESIAN_POINT('Ctrl Pts',(2.54087625856207,-1.18514270861997,11.4513742353937));
#59360=CARTESIAN_POINT('Ctrl Pts',(2.52374266560532,-1.06847604195247,11.4413014326463));
#59361=CARTESIAN_POINT('Ctrl Pts',(2.49192640226148,-0.794772684006295,
11.393917427895));
#59362=CARTESIAN_POINT('Ctrl Pts',(2.47740478277498,-0.636309800099556,
11.3249090921007));
#59363=CARTESIAN_POINT('Ctrl Pts',(2.46904555195898,-0.319434907279348,
11.2492951852861));
#59364=CARTESIAN_POINT('Ctrl Pts',(2.46993104457879,-0.158333333334417,
11.2008819504006));
#59365=CARTESIAN_POINT('Ctrl Pts',(2.49648908044561,0.158333333334419,11.1843719645541));
#59366=CARTESIAN_POINT('Ctrl Pts',(2.52295468317368,0.319434907279354,11.2158070281581));
#59367=CARTESIAN_POINT('Ctrl Pts',(2.58379531574759,0.636309800099564,11.2587449425823));
#59368=CARTESIAN_POINT('Ctrl Pts',(2.62718132427679,0.794772684006285,11.3104481557108));
#59369=CARTESIAN_POINT('Ctrl Pts',(2.69780711715852,1.0684760419525,11.3323479241051));
#59370=CARTESIAN_POINT('Ctrl Pts',(2.72949516865402,1.18514270862003,11.3323668908108));
#59371=CARTESIAN_POINT('Ctrl Pts',(2.76229998285004,1.30000000000911,11.3229252259507));
#59372=CARTESIAN_POINT('Ctrl Pts',(2.56131666944869,-1.30000000000913,11.4558130511715));
#59373=CARTESIAN_POINT('Ctrl Pts',(2.54071115869131,-1.18514270862008,11.4571454949206));
#59374=CARTESIAN_POINT('Ctrl Pts',(2.52354787125624,-1.06847604195257,11.4477619682194));
#59375=CARTESIAN_POINT('Ctrl Pts',(2.49184946826631,-0.794772684006371,
11.4013281089084));
#59376=CARTESIAN_POINT('Ctrl Pts',(2.4777522540972,-0.636309800099617,11.3319951009902));
#59377=CARTESIAN_POINT('Ctrl Pts',(2.46963844675668,-0.319434907279378,
11.2563237702013));
#59378=CARTESIAN_POINT('Ctrl Pts',(2.47048528287712,-0.158333333334432,
11.2076216623077));
#59379=CARTESIAN_POINT('Ctrl Pts',(2.49715360110744,0.158333333334434,11.1910694940594));
#59380=CARTESIAN_POINT('Ctrl Pts',(2.5237174938095,0.319434907279384,11.222768031268));
#59381=CARTESIAN_POINT('Ctrl Pts',(2.58464050828157,0.636309800099625,11.2656432613921));
#59382=CARTESIAN_POINT('Ctrl Pts',(2.62809396689711,0.794772684006361,11.3174935285109));
#59383=CARTESIAN_POINT('Ctrl Pts',(2.69861118974356,1.0684760419526,11.3384452605758));
#59384=CARTESIAN_POINT('Ctrl Pts',(2.73020709155904,1.18514270862015,11.3378226912375));
#59385=CARTESIAN_POINT('Ctrl Pts',(2.76287460234039,1.30000000000923,11.327508324088));
#59386=CARTESIAN_POINT('Ctrl Pts',(2.56128874706338,-1.30000000000925,11.460606417697));
#59387=CARTESIAN_POINT('Ctrl Pts',(2.54059919774736,-1.18514270862019,11.4628963272545));
#59388=CARTESIAN_POINT('Ctrl Pts',(2.52341514362887,-1.06847604195267,11.4541987306546));
#59389=CARTESIAN_POINT('Ctrl Pts',(2.49181493613513,-0.794772684006444,
11.4087222052943));
#59390=CARTESIAN_POINT('Ctrl Pts',(2.47803662716417,-0.636309800099675,
11.3391034991509));
#59391=CARTESIAN_POINT('Ctrl Pts',(2.47015524119871,-0.319434907279407,
11.2633795288095));
#59392=CARTESIAN_POINT('Ctrl Pts',(2.47104744026839,-0.158333333334447,
11.2143570172613));
#59393=CARTESIAN_POINT('Ctrl Pts',(2.49782482983666,0.158333333334448,11.1977641059529));
#59394=CARTESIAN_POINT('Ctrl Pts',(2.52442978411062,0.319434907279414,11.2297487364126));
#59395=CARTESIAN_POINT('Ctrl Pts',(2.58538867760488,0.636309800099683,11.2725805125511));
#59396=CARTESIAN_POINT('Ctrl Pts',(2.62885836607784,0.794772684006434,11.3245997575365));
#59397=CARTESIAN_POINT('Ctrl Pts',(2.69929693074833,1.0684760419527,11.344590867485));
#59398=CARTESIAN_POINT('Ctrl Pts',(2.7308347615203,1.18514270862026,11.3433123840418));
#59399=CARTESIAN_POINT('Ctrl Pts',(2.76342017842444,1.30000000000935,11.3321020064024));
#59400=CARTESIAN_POINT('Ctrl Pts',(2.56130713243344,-1.30000000000936,11.4641865202654));
#59401=CARTESIAN_POINT('Ctrl Pts',(2.54059650491898,-1.18514270862029,11.467178976126));
#59402=CARTESIAN_POINT('Ctrl Pts',(2.52341374472244,-1.06847604195276,11.4589895513125));
#59403=CARTESIAN_POINT('Ctrl Pts',(2.49186821052087,-0.79477268400651,11.4142379604201));
#59404=CARTESIAN_POINT('Ctrl Pts',(2.4781866708489,-0.636309800099728,11.3444578235712));
#59405=CARTESIAN_POINT('Ctrl Pts',(2.47046333705133,-0.319434907279434,
11.2686998715368));
#59406=CARTESIAN_POINT('Ctrl Pts',(2.47149975376307,-0.15833333333446,11.21939479967));
#59407=CARTESIAN_POINT('Ctrl Pts',(2.49836072670033,0.158333333334462,11.2027714476665));
#59408=CARTESIAN_POINT('Ctrl Pts',(2.52492852326674,0.319434907279441,11.2349976571573));
#59409=CARTESIAN_POINT('Ctrl Pts',(2.58585179782396,0.636309800099737,11.2778228799129));
#59410=CARTESIAN_POINT('Ctrl Pts',(2.6292601226087,0.794772684006501,11.3300004655705));
#59411=CARTESIAN_POINT('Ctrl Pts',(2.69966785275523,1.06847604195279,11.3492592714812));
#59412=CARTESIAN_POINT('Ctrl Pts',(2.73120098151679,1.18514270862035,11.3474724099805));
#59413=CARTESIAN_POINT('Ctrl Pts',(2.76379034152299,1.30000000000946,11.3355622635095));
#59414=CARTESIAN_POINT('Ctrl Pts',(2.56133053553565,-1.30000000000937,11.4663697219108));
#59415=CARTESIAN_POINT('Ctrl Pts',(2.54062092754015,-1.1851427086203,11.4697863261517));
#59416=CARTESIAN_POINT('Ctrl Pts',(2.52344453798962,-1.06847604195277,11.461905362338));
#59417=CARTESIAN_POINT('Ctrl Pts',(2.49192608342873,-0.794772684006519,
11.4175991170701));
#59418=CARTESIAN_POINT('Ctrl Pts',(2.47825706367865,-0.636309800099735,
11.3477377234317));
#59419=CARTESIAN_POINT('Ctrl Pts',(2.47062360734013,-0.319434907279438,
11.2719613563287));
#59420=CARTESIAN_POINT('Ctrl Pts',(2.47178145129884,-0.158333333334462,
11.2224707868178));
#59421=CARTESIAN_POINT('Ctrl Pts',(2.49869442133726,0.158333333334463,11.2058287322166));
#59422=CARTESIAN_POINT('Ctrl Pts',(2.52522064186388,0.319434907279444,11.238210140243));
#59423=CARTESIAN_POINT('Ctrl Pts',(2.58610321650479,0.636309800099743,11.2810393034797));
#59424=CARTESIAN_POINT('Ctrl Pts',(2.62945008104189,0.794772684006509,11.333323903885));
#59425=CARTESIAN_POINT('Ctrl Pts',(2.69984688561952,1.0684760419528,11.352131918274));
#59426=CARTESIAN_POINT('Ctrl Pts',(2.73138883622815,1.18514270862037,11.3500294681154));
#59427=CARTESIAN_POINT('Ctrl Pts',(2.76400056920245,1.30000000000948,11.3376832752746));
#59428=CARTESIAN_POINT('Ctrl Pts',(2.56134006102012,-1.30000000000938,11.467163217126));
#59429=CARTESIAN_POINT('Ctrl Pts',(2.54063196431958,-1.18514270862031,11.4707336261399));
#59430=CARTESIAN_POINT('Ctrl Pts',(2.52345832930351,-1.06847604195277,11.4629646624051));
#59431=CARTESIAN_POINT('Ctrl Pts',(2.49194911040026,-0.794772684006521,
11.418820582519));
#59432=CARTESIAN_POINT('Ctrl Pts',(2.47828069101631,-0.636309800099737,
11.348931118347));
#59433=CARTESIAN_POINT('Ctrl Pts',(2.47067921082616,-0.319434907279439,
11.2731483113593));
#59434=CARTESIAN_POINT('Ctrl Pts',(2.47188381244264,-0.158333333334462,
11.2235892926567));
#59435=CARTESIAN_POINT('Ctrl Pts',(2.49881575706648,0.158333333334464,11.2069404358377));
#59436=CARTESIAN_POINT('Ctrl Pts',(2.52532549432616,0.319434907279445,11.2393788263393));
#59437=CARTESIAN_POINT('Ctrl Pts',(2.586191725793,0.636309800099745,11.2822100750807));
#59438=CARTESIAN_POINT('Ctrl Pts',(2.62951411036498,0.794772684006511,11.3345344993265));
#59439=CARTESIAN_POINT('Ctrl Pts',(2.69990758027193,1.0684760419528,11.3531783372742));
#59440=CARTESIAN_POINT('Ctrl Pts',(2.73145372198533,1.18514270862037,11.3509607217599));
#59441=CARTESIAN_POINT('Ctrl Pts',(2.76407528062454,1.30000000000948,11.3384552641061));
#59442=CARTESIAN_POINT('Ctrl Pts',(2.56135024134104,-1.30000000000938,11.4679564555889));
#59443=CARTESIAN_POINT('Ctrl Pts',(2.54064438626549,-1.18514270862031,11.4716803923896));
#59444=CARTESIAN_POINT('Ctrl Pts',(2.52347378436581,-1.06847604195277,11.4640233214816));
#59445=CARTESIAN_POINT('Ctrl Pts',(2.49197340107165,-0.794772684006522,
11.4200415513229));
#59446=CARTESIAN_POINT('Ctrl Pts',(2.47830304739703,-0.636309800099738,
11.3501249648034));
#59447=CARTESIAN_POINT('Ctrl Pts',(2.47073306099399,-0.319434907279439,
11.2743358940396));
#59448=CARTESIAN_POINT('Ctrl Pts',(2.47198603717078,-0.158333333334462,
11.2247078081228));
#59449=CARTESIAN_POINT('Ctrl Pts',(2.49893699854064,0.158333333334464,11.2080521484978));
#59450=CARTESIAN_POINT('Ctrl Pts',(2.5254294386272,0.319434907279445,11.2405478475419));
#59451=CARTESIAN_POINT('Ctrl Pts',(2.58627834539166,0.636309800099746,11.2833815979748));
#59452=CARTESIAN_POINT('Ctrl Pts',(2.62957484156349,0.794772684006513,11.3357464466506));
#59453=CARTESIAN_POINT('Ctrl Pts',(2.69996537414403,1.0684760419528,11.3542259534225));
#59454=CARTESIAN_POINT('Ctrl Pts',(2.73151633698734,1.18514270862037,11.3518929137309));
#59455=CARTESIAN_POINT('Ctrl Pts',(2.76414880934613,1.30000000000948,11.3392277405993));
#59456=CARTESIAN_POINT('Ctrl Pts',(2.56136125091565,-1.30000000000939,11.46874936247));
#59457=CARTESIAN_POINT('Ctrl Pts',(2.54065855362631,-1.18514270862031,11.4726264753955));
#59458=CARTESIAN_POINT('Ctrl Pts',(2.523491321396,-1.06847604195278,11.4650811647543));
#59459=CARTESIAN_POINT('Ctrl Pts',(2.49199921220471,-0.794772684006527,
11.4212619042518));
#59460=CARTESIAN_POINT('Ctrl Pts',(2.47832365766506,-0.636309800099742,
11.3513194187444));
#59461=CARTESIAN_POINT('Ctrl Pts',(2.47078446722792,-0.319434907279441,
11.275524343034));
#59462=CARTESIAN_POINT('Ctrl Pts',(2.47208778158329,-0.158333333334463,
11.2258264444291));
#59463=CARTESIAN_POINT('Ctrl Pts',(2.49905780903537,0.158333333334465,11.2091639849313));
#59464=CARTESIAN_POINT('Ctrl Pts',(2.52553203339442,0.319434907279447,11.2417173591179));
#59465=CARTESIAN_POINT('Ctrl Pts',(2.58636238554639,0.63630980009975,11.2845541361013));
#59466=CARTESIAN_POINT('Ctrl Pts',(2.62963112657045,0.794772684006517,11.3369602049926));
#59467=CARTESIAN_POINT('Ctrl Pts',(2.70001921062227,1.06847604195281,11.3552751988756));
#59468=CARTESIAN_POINT('Ctrl Pts',(2.73157579789778,1.18514270862038,11.3528264099193));
#59469=CARTESIAN_POINT('Ctrl Pts',(2.76422057899831,1.30000000000949,11.3400009497923));
#59470=CARTESIAN_POINT('Ctrl Pts',(2.56137065250099,-1.30000000000939,11.4693934098164));
#59471=CARTESIAN_POINT('Ctrl Pts',(2.54067104000972,-1.18514270862032,11.4733947758321));
#59472=CARTESIAN_POINT('Ctrl Pts',(2.52350671901196,-1.06847604195278,11.4659402001361));
#59473=CARTESIAN_POINT('Ctrl Pts',(2.49202093437909,-0.794772684006528,
11.4222531218883));
#59474=CARTESIAN_POINT('Ctrl Pts',(2.47833920790945,-0.636309800099742,
11.3522903276923));
#59475=CARTESIAN_POINT('Ctrl Pts',(2.4708244777701,-0.319434907279441,11.2764905873951));
#59476=CARTESIAN_POINT('Ctrl Pts',(2.47216961473139,-0.158333333334463,
11.2267356190202));
#59477=CARTESIAN_POINT('Ctrl Pts',(2.49915516214719,0.158333333334465,11.2100676389615));
#59478=CARTESIAN_POINT('Ctrl Pts',(2.52561430177766,0.319434907279448,11.2426679916367));
#59479=CARTESIAN_POINT('Ctrl Pts',(2.58642895659811,0.636309800099751,11.2855074984505));
#59480=CARTESIAN_POINT('Ctrl Pts',(2.62967401306659,0.794772684006518,11.3379475363054));
#59481=CARTESIAN_POINT('Ctrl Pts',(2.70006034491809,1.06847604195281,11.3561287847828));
#59482=CARTESIAN_POINT('Ctrl Pts',(2.73162193854099,1.18514270862038,11.3535857786671));
#59483=CARTESIAN_POINT('Ctrl Pts',(2.76427749079888,1.30000000000949,11.3406297776516));
#59484=CARTESIAN_POINT('Ctrl Pts',(2.56137504094225,-1.30000000000939,11.4696906405867));
#59485=CARTESIAN_POINT('Ctrl Pts',(2.54067693502122,-1.18514270862032,11.473749321531));
#59486=CARTESIAN_POINT('Ctrl Pts',(2.52351398448711,-1.06847604195278,11.4663366124304));
#59487=CARTESIAN_POINT('Ctrl Pts',(2.49203105146606,-0.794772684006529,
11.4227105656534));
#59488=CARTESIAN_POINT('Ctrl Pts',(2.47834615136286,-0.636309800099743,
11.3527385214951));
#59489=CARTESIAN_POINT('Ctrl Pts',(2.47084263239626,-0.319434907279442,
11.2769366585471));
#59490=CARTESIAN_POINT('Ctrl Pts',(2.47220725302156,-0.158333333334464,
11.2271552820576));
#59491=CARTESIAN_POINT('Ctrl Pts',(2.49919997574841,0.158333333334465,11.2104847522061));
#59492=CARTESIAN_POINT('Ctrl Pts',(2.52565207601259,0.319434907279448,11.2431068189532));
#59493=CARTESIAN_POINT('Ctrl Pts',(2.58645940270579,0.636309800099751,11.2859476223562));
#59494=CARTESIAN_POINT('Ctrl Pts',(2.62969341506726,0.794772684006519,11.3384033860378));
#59495=CARTESIAN_POINT('Ctrl Pts',(2.70007896751934,1.06847604195281,11.3565228972491));
#59496=CARTESIAN_POINT('Ctrl Pts',(2.73164292102903,1.18514270862038,11.3539363877475));
#59497=CARTESIAN_POINT('Ctrl Pts',(2.76430353043367,1.30000000000949,11.3409201037351));
#59498=CARTESIAN_POINT('Ctrl Pts',(2.56137726536325,-1.30000000000939,11.4698392430645));
#59499=CARTESIAN_POINT('Ctrl Pts',(2.54067991505903,-1.18514270862032,11.47392657979));
#59500=CARTESIAN_POINT('Ctrl Pts',(2.52351764709741,-1.06847604195278,11.4665348044257));
#59501=CARTESIAN_POINT('Ctrl Pts',(2.49203612220835,-0.794772684006528,
11.4229392792989));
#59502=CARTESIAN_POINT('Ctrl Pts',(2.47834961582534,-0.636309800099743,
11.3529626174887));
#59503=CARTESIAN_POINT('Ctrl Pts',(2.47085165080681,-0.319434907279441,
11.2771597134595));
#59504=CARTESIAN_POINT('Ctrl Pts',(2.47222594584845,-0.158333333334463,
11.2273651600113));
#59505=CARTESIAN_POINT('Ctrl Pts',(2.49922224671243,0.158333333334465,11.210693359286));
#59506=CARTESIAN_POINT('Ctrl Pts',(2.52567090780485,0.319434907279448,11.2433262507377));
#59507=CARTESIAN_POINT('Ctrl Pts',(2.58647455662111,0.636309800099751,11.2861677092373));
#59508=CARTESIAN_POINT('Ctrl Pts',(2.62970293393306,0.794772684006518,11.3386313825405));
#59509=CARTESIAN_POINT('Ctrl Pts',(2.70008810179692,1.06847604195281,11.3567200251167));
#59510=CARTESIAN_POINT('Ctrl Pts',(2.73165326189538,1.18514270862038,11.3541117541788));
#59511=CARTESIAN_POINT('Ctrl Pts',(2.76431645095154,1.30000000000949,11.341065309182));
#59512=CARTESIAN_POINT('Ctrl Pts',(2.56137945448883,-1.30000000000939,11.4699878598848));
#59513=CARTESIAN_POINT('Ctrl Pts',(2.54068290101624,-1.18514270862032,11.4741038375641));
#59514=CARTESIAN_POINT('Ctrl Pts',(2.52352133537992,-1.06847604195278,11.4667329890265));
#59515=CARTESIAN_POINT('Ctrl Pts',(2.49204121467428,-0.79477268400653,11.423167987879));
#59516=CARTESIAN_POINT('Ctrl Pts',(2.47835295767272,-0.636309800099744,
11.3531867634054));
#59517=CARTESIAN_POINT('Ctrl Pts',(2.47086060422438,-0.319434907279442,
11.2773827955655));
#59518=CARTESIAN_POINT('Ctrl Pts',(2.47224480791073,-0.158333333334464,
11.2275749735584));
#59519=CARTESIAN_POINT('Ctrl Pts',(2.49924471338305,0.158333333334466,11.2109018927394));
#59520=CARTESIAN_POINT('Ctrl Pts',(2.52568973349682,0.319434907279448,11.2435456904092));
#59521=CARTESIAN_POINT('Ctrl Pts',(2.58648968861374,0.636309800099752,11.2863878097201));
#59522=CARTESIAN_POINT('Ctrl Pts',(2.62971259824551,0.79477268400652,11.3388593240486));
#59523=CARTESIAN_POINT('Ctrl Pts',(2.70009738605776,1.06847604195281,11.3569170940394));
#59524=CARTESIAN_POINT('Ctrl Pts',(2.73166372477225,1.18514270862038,11.3542870718402));
#59525=CARTESIAN_POINT('Ctrl Pts',(2.76432943557074,1.30000000000949,11.3412104879192));
#59526=CARTESIAN_POINT('Ctrl Pts',(2.56157722268406,-1.30000000000894,11.4827649103601));
#59527=CARTESIAN_POINT('Ctrl Pts',(2.54094502819204,-1.1851427086199,11.4893453425908));
#59528=CARTESIAN_POINT('Ctrl Pts',(2.52384113867237,-1.06847604195241,11.4837750560872));
#59529=CARTESIAN_POINT('Ctrl Pts',(2.49247882258168,-0.79477268400625,11.4428359889128));
#59530=CARTESIAN_POINT('Ctrl Pts',(2.47865230654726,-0.63630980009952,11.3724576776822));
#59531=CARTESIAN_POINT('Ctrl Pts',(2.47162642797473,-0.31943490727933,11.2965685612173));
#59532=CARTESIAN_POINT('Ctrl Pts',(2.47382416304614,-0.158333333334408,
11.2456348906483));
#59533=CARTESIAN_POINT('Ctrl Pts',(2.50112935392846,0.15833333333441,11.2288534986333));
#59534=CARTESIAN_POINT('Ctrl Pts',(2.52729875131117,0.319434907279336,11.2624201131549));
#59535=CARTESIAN_POINT('Ctrl Pts',(2.58778023915259,0.636309800099529,11.3053196978508));
#59536=CARTESIAN_POINT('Ctrl Pts',(2.63049321521687,0.794772684006241,11.3584818961727));
#59537=CARTESIAN_POINT('Ctrl Pts',(2.70084575128737,1.06847604195244,11.3738850860774));
#59538=CARTESIAN_POINT('Ctrl Pts',(2.73252152503143,1.18514270861997,11.3693815185187));
#59539=CARTESIAN_POINT('Ctrl Pts',(2.76542006647301,1.30000000000904,11.353706913236));
#59540=CARTESIAN_POINT('Ctrl Pts',(2.56100445263162,-1.30000000000382,11.5021321526777));
#59541=CARTESIAN_POINT('Ctrl Pts',(2.53988697929534,-1.18514270861524,11.5125879114081));
#59542=CARTESIAN_POINT('Ctrl Pts',(2.52257778342055,-1.06847604194821,11.5098011038562));
#59543=CARTESIAN_POINT('Ctrl Pts',(2.49138796103636,-0.794772684003123,
11.4727700436339));
#59544=CARTESIAN_POINT('Ctrl Pts',(2.47874734569991,-0.636309800097017,
11.401291801289));
#59545=CARTESIAN_POINT('Ctrl Pts',(2.47260853930848,-0.319434907278073,
11.3252255099555));
#59546=CARTESIAN_POINT('Ctrl Pts',(2.4750472889405,-0.158333333333785,11.2730089588781));
#59547=CARTESIAN_POINT('Ctrl Pts',(2.50290453090846,0.158333333333787,11.2560331856762));
#59548=CARTESIAN_POINT('Ctrl Pts',(2.52919053511972,0.31943490727808,11.2907603607314));
#59549=CARTESIAN_POINT('Ctrl Pts',(2.59030547838485,0.636309800097026,11.3332943963133));
#59550=CARTESIAN_POINT('Ctrl Pts',(2.63427592232645,0.794772684003113,11.386638886161));
#59551=CARTESIAN_POINT('Ctrl Pts',(2.70398322000805,1.06847604194824,11.3983679306146));
#59552=CARTESIAN_POINT('Ctrl Pts',(2.73493078676626,1.18514270861531,11.3914654578382));
#59553=CARTESIAN_POINT('Ctrl Pts',(2.76665221402625,1.30000000000392,11.3725834435454));
#59554=CARTESIAN_POINT('Ctrl Pts',(2.56105038800803,-1.30000000000269,11.5275512529855));
#59555=CARTESIAN_POINT('Ctrl Pts',(2.53937103043282,-1.18514270861421,11.543123480386));
#59556=CARTESIAN_POINT('Ctrl Pts',(2.52180787412611,-1.06847604194728,11.5440280334857));
#59557=CARTESIAN_POINT('Ctrl Pts',(2.49074271793371,-0.794772684002436,
11.5122324702082));
#59558=CARTESIAN_POINT('Ctrl Pts',(2.47924052020287,-0.636309800096463,
11.4394727690071));
#59559=CARTESIAN_POINT('Ctrl Pts',(2.47425825925016,-0.319434907277794,
11.363172367664));
#59560=CARTESIAN_POINT('Ctrl Pts',(2.47759035916085,-0.158333333333648,
11.3090055592548));
#59561=CARTESIAN_POINT('Ctrl Pts',(2.50587326386845,0.158333333333649,11.2918877855756));
#59562=CARTESIAN_POINT('Ctrl Pts',(2.53186766187087,0.319434907277803,11.3283374655647));
#59563=CARTESIAN_POINT('Ctrl Pts',(2.59233443905784,0.636309800096473,11.370991036896));
#59564=CARTESIAN_POINT('Ctrl Pts',(2.63483846985725,0.794772684002421,11.4258929157626));
#59565=CARTESIAN_POINT('Ctrl Pts',(2.70491060050181,1.0684760419473,11.4321819710538));
#59566=CARTESIAN_POINT('Ctrl Pts',(2.73644526408019,1.18514270861427,11.4214123261886));
#59567=CARTESIAN_POINT('Ctrl Pts',(2.76918296230924,1.30000000000279,11.3971507374553));
#59568=CARTESIAN_POINT('Ctrl Pts',(2.56038193620446,-1.3000000000001,11.5405164392947));
#59569=CARTESIAN_POINT('Ctrl Pts',(2.53863428981172,-1.18514270861185,11.5585564843419));
#59570=CARTESIAN_POINT('Ctrl Pts',(2.52104861549718,-1.06847604194515,11.5612588970542));
#59571=CARTESIAN_POINT('Ctrl Pts',(2.49003717792876,-0.794772684000851,
11.5320690120589));
#59572=CARTESIAN_POINT('Ctrl Pts',(2.47864981464921,-0.636309800095197,
11.4588263413895));
#59573=CARTESIAN_POINT('Ctrl Pts',(2.47402470093622,-0.319434907277159,
11.3825030046764));
#59574=CARTESIAN_POINT('Ctrl Pts',(2.47762464049648,-0.158333333333332,
11.3274655474548));
#59575=CARTESIAN_POINT('Ctrl Pts',(2.50647930782813,0.158333333333334,11.3101501710681));
#59576=CARTESIAN_POINT('Ctrl Pts',(2.53302516600472,0.319434907277167,11.3471799051407));
#59577=CARTESIAN_POINT('Ctrl Pts',(2.59379521979637,0.636309800095206,11.3896433274067));
#59578=CARTESIAN_POINT('Ctrl Pts',(2.63621560063971,0.79477268400084,11.4450389031251));
#59579=CARTESIAN_POINT('Ctrl Pts',(2.70595672826436,1.06847604194518,11.4488497372808));
#59580=CARTESIAN_POINT('Ctrl Pts',(2.73726147277651,1.18514270861191,11.436384457426));
#59581=CARTESIAN_POINT('Ctrl Pts',(2.76968261181557,1.3000000000002,11.4098043288156));
#59582=CARTESIAN_POINT('Ctrl Pts',(2.56007871299431,-1.3000000000001,11.5469848467937));
#59583=CARTESIAN_POINT('Ctrl Pts',(2.53830479690493,-1.18514270861185,11.566255317647));
#59584=CARTESIAN_POINT('Ctrl Pts',(2.52071187691434,-1.06847604194515,11.5698548993192));
#59585=CARTESIAN_POINT('Ctrl Pts',(2.48972764967806,-0.794772684000851,
11.5419677641169));
#59586=CARTESIAN_POINT('Ctrl Pts',(2.47833749752908,-0.636309800095197,
11.4685085686384));
#59587=CARTESIAN_POINT('Ctrl Pts',(2.47397094455174,-0.319434907277159,
11.3921419562768));
#59588=CARTESIAN_POINT('Ctrl Pts',(2.47794645705588,-0.158333333333332,
11.3365725980395));
#59589=CARTESIAN_POINT('Ctrl Pts',(2.50702387179274,0.158333333333334,11.31918253943));
#59590=CARTESIAN_POINT('Ctrl Pts',(2.53348691515875,0.319434907277167,11.3566435139838));
#59591=CARTESIAN_POINT('Ctrl Pts',(2.5943095218286,0.636309800095206,11.3990510055383));
#59592=CARTESIAN_POINT('Ctrl Pts',(2.636842707518,0.79477268400084,11.4546353160117));
#59593=CARTESIAN_POINT('Ctrl Pts',(2.70652295950979,1.06847604194518,11.4571620595879));
#59594=CARTESIAN_POINT('Ctrl Pts',(2.73776084593925,1.18514270861191,11.4438270002045));
#59595=CARTESIAN_POINT('Ctrl Pts',(2.77007461961871,1.3000000000002,11.4160631477685));
#59596=CARTESIAN_POINT('',(2.73386551409056,1.2,11.3265578089815));
#59597=CARTESIAN_POINT('Ctrl Pts',(2.73386551409056,1.2,11.3265578089815));
#59598=CARTESIAN_POINT('Ctrl Pts',(2.73584462812093,1.21680977180052,11.3050825247105));
#59599=CARTESIAN_POINT('Ctrl Pts',(2.738942467519,1.23315185137663,11.2833531581086));
#59600=CARTESIAN_POINT('Ctrl Pts',(2.74170316331882,1.2586271482025,11.2507580722637));
#59601=CARTESIAN_POINT('Ctrl Pts',(2.74277442651819,1.2672419954071,11.2396242820028));
#59602=CARTESIAN_POINT('Ctrl Pts',(2.7446650447868,1.28369101331277,11.2184347711517));
#59603=CARTESIAN_POINT('Ctrl Pts',(2.7455088379524,1.29283848095844,11.2067731878531));
#59604=CARTESIAN_POINT('Ctrl Pts',(2.74612652659282,1.3,11.1976604533081));
#59605=CARTESIAN_POINT('',(2.60194863185246,0.653834841400135,11.4109812771984));
#59606=CARTESIAN_POINT('Ctrl Pts',(2.60194863188356,0.653834841395383,11.4109812772131));
#59607=CARTESIAN_POINT('Ctrl Pts',(2.61465202379657,0.712710396428781,11.4031319017273));
#59608=CARTESIAN_POINT('Ctrl Pts',(2.6275775914059,0.767437746451103,11.3950673517918));
#59609=CARTESIAN_POINT('Ctrl Pts',(2.65479253142727,0.881623511218933,11.3778990266176));
#59610=CARTESIAN_POINT('Ctrl Pts',(2.66791954153367,0.939267186110352,11.3695399452405));
#59611=CARTESIAN_POINT('Ctrl Pts',(2.69220097159631,1.03693057340345,11.3538721025205));
#59612=CARTESIAN_POINT('Ctrl Pts',(2.69334780775769,1.04076945910191,11.3531565955888));
#59613=CARTESIAN_POINT('Ctrl Pts',(2.71798212515219,1.13794123504627,11.337051941875));
#59614=CARTESIAN_POINT('Ctrl Pts',(2.72508909283384,1.16622167032162,11.3323722326541));
#59615=CARTESIAN_POINT('Ctrl Pts',(2.73386551409056,1.2,11.3265578089815));
#59616=CARTESIAN_POINT('',(2.48224831221779,-0.653834841531101,11.4826327552677));
#59617=CARTESIAN_POINT('Ctrl Pts',(2.48224831221779,-0.653834841531095,
11.4826327552677));
#59618=CARTESIAN_POINT('Ctrl Pts',(2.47847738061633,-0.575759531786473,
11.4411122856413));
#59619=CARTESIAN_POINT('Ctrl Pts',(2.47624817611948,-0.493700405580143,
11.4060576739905));
#59620=CARTESIAN_POINT('Ctrl Pts',(2.47524680930892,-0.338117536422364,
11.3554159398901));
#59621=CARTESIAN_POINT('Ctrl Pts',(2.47616672898253,-0.265668500424853,
11.3375148853909));
#59622=CARTESIAN_POINT('Ctrl Pts',(2.48166898014515,-0.129739059380434,
11.3137074236253));
#59623=CARTESIAN_POINT('Ctrl Pts',(2.48564176829179,-0.0666644104608011,
11.306467035274));
#59624=CARTESIAN_POINT('Ctrl Pts',(2.49684517723276,0.0595020246954211,
11.2993228621924));
#59625=CARTESIAN_POINT('Ctrl Pts',(2.50413753009899,0.122723937005544,11.2993588371747));
#59626=CARTESIAN_POINT('Ctrl Pts',(2.52290455712779,0.260104219793123,11.3079494537664));
#59627=CARTESIAN_POINT('Ctrl Pts',(2.5349515325394,0.333974009178121,11.3180297306754));
#59628=CARTESIAN_POINT('Ctrl Pts',(2.56422889724993,0.491511647282905,11.3520776397861));
#59629=CARTESIAN_POINT('Ctrl Pts',(2.58242354484658,0.574911057590937,11.3781128894232));
#59630=CARTESIAN_POINT('Ctrl Pts',(2.60194863188389,0.653834841414069,11.4109812771463));
#59631=CARTESIAN_POINT('',(2.54449880327374,-1.2,11.4459422794167));
#59632=CARTESIAN_POINT('Ctrl Pts',(2.54449880327374,-1.2,11.4459422794167));
#59633=CARTESIAN_POINT('Ctrl Pts',(2.53869459902857,-1.16426922222959,11.4494206099695));
#59634=CARTESIAN_POINT('Ctrl Pts',(2.52319531495474,-1.06850390950927,11.4586966913891));
#59635=CARTESIAN_POINT('Ctrl Pts',(2.49047921518896,-0.779246466377113,
11.4778788224293));
#59636=CARTESIAN_POINT('Ctrl Pts',(2.48693835700297,-0.726323271199487,
11.4799143676736));
#59637=CARTESIAN_POINT('Ctrl Pts',(2.48224831221779,-0.653834841531102,
11.4826327552677));
#59638=CARTESIAN_POINT('Ctrl Pts',(2.55649102449442,-1.30000000000134,11.3215110871701));
#59639=CARTESIAN_POINT('Ctrl Pts',(2.55495837329733,-1.28299097848429,11.3424771749858));
#59640=CARTESIAN_POINT('Ctrl Pts',(2.55369848352248,-1.2750263530914,11.3526315204527));
#59641=CARTESIAN_POINT('Ctrl Pts',(2.54995094158512,-1.23879982679597,11.3973438043548));
#59642=CARTESIAN_POINT('Ctrl Pts',(2.54791533845649,-1.21869813962824,11.4220961802047));
#59643=CARTESIAN_POINT('Ctrl Pts',(2.54449880327374,-1.2,11.4459422794167));
#59644=CARTESIAN_POINT('Origin',(0.,1.25,7.2));
#59645=CARTESIAN_POINT('Origin',(0.,1.2,7.2));
#59646=CARTESIAN_POINT('Origin',(0.,0.92691742076555,7.2));
#59647=CARTESIAN_POINT('Origin',(0.,0.653834841531101,7.2));
#59648=CARTESIAN_POINT('Origin',(0.,0.,7.2));
#59649=CARTESIAN_POINT('Origin',(0.,-0.653834841531101,7.2));
#59650=CARTESIAN_POINT('Origin',(0.,-0.926917420765551,7.2));
#59651=CARTESIAN_POINT('Origin',(0.,-1.2,7.2));
#59652=CARTESIAN_POINT('Origin',(0.,-1.25,7.2));
#59653=CARTESIAN_POINT('Ctrl Pts',(2.2661804801183,-1.3000000000017,11.7069865648569));
#59654=CARTESIAN_POINT('Ctrl Pts',(2.30638156847542,-1.18514270861294,11.6928839421778));
#59655=CARTESIAN_POINT('Ctrl Pts',(2.33354901187765,-1.0684760419457,11.6724986686618));
#59656=CARTESIAN_POINT('Ctrl Pts',(2.36620091374758,-0.794772684000851,
11.6108904285065));
#59657=CARTESIAN_POINT('Ctrl Pts',(2.33933008166883,-0.636309800095197,
11.5462634539553));
#59658=CARTESIAN_POINT('Ctrl Pts',(2.33301542000619,-0.319434907277159,
11.4723857856765));
#59659=CARTESIAN_POINT('Ctrl Pts',(2.31380478607559,-0.158333333333332,
11.4307376305842));
#59660=CARTESIAN_POINT('Ctrl Pts',(2.34340372597314,0.158333333333334,11.4142508800506));
#59661=CARTESIAN_POINT('Ctrl Pts',(2.3935159581309,0.319434907277167,11.438592664348));
#59662=CARTESIAN_POINT('Ctrl Pts',(2.45746810794752,0.636309800095206,11.4805575163326));
#59663=CARTESIAN_POINT('Ctrl Pts',(2.51539056129685,0.79477268400084,11.5271512751816));
#59664=CARTESIAN_POINT('Ctrl Pts',(2.524049415203,1.06847604194524,11.5679279706864));
#59665=CARTESIAN_POINT('Ctrl Pts',(2.51213562603731,1.18514270861203,11.5813640954902));
#59666=CARTESIAN_POINT('Ctrl Pts',(2.48455995069209,1.30000000000038,11.5905856245393));
#59667=CARTESIAN_POINT('Ctrl Pts',(2.25573189552087,-1.3000000000017,11.7000487685172));
#59668=CARTESIAN_POINT('Ctrl Pts',(2.29399007944011,-1.18514270861294,11.6845764597768));
#59669=CARTESIAN_POINT('Ctrl Pts',(2.31971787859578,-1.0684760419457,11.6632056051479));
#59670=CARTESIAN_POINT('Ctrl Pts',(2.35020654597517,-0.794772684000851,
11.6002078347277));
#59671=CARTESIAN_POINT('Ctrl Pts',(2.32354980721585,-0.636309800095197,
11.535964978615));
#59672=CARTESIAN_POINT('Ctrl Pts',(2.31708571783412,-0.319434907277159,
11.4621224038657));
#59673=CARTESIAN_POINT('Ctrl Pts',(2.2987048291419,-0.158333333333332,11.4207620498046));
#59674=CARTESIAN_POINT('Ctrl Pts',(2.32795166823,0.158333333333334,11.404586426871));
#59675=CARTESIAN_POINT('Ctrl Pts',(2.37676704786356,0.319434907277167,11.4290468215792));
#59676=CARTESIAN_POINT('Ctrl Pts',(2.44038568131415,0.636309800095206,11.4714162382288));
#59677=CARTESIAN_POINT('Ctrl Pts',(2.49793589154107,0.79477268400084,11.5177886417626));
#59678=CARTESIAN_POINT('Ctrl Pts',(2.50882396394658,1.06847604194524,11.5599152167389));
#59679=CARTESIAN_POINT('Ctrl Pts',(2.49847136268361,1.18514270861203,11.5742359606339));
#59680=CARTESIAN_POINT('Ctrl Pts',(2.47305311705618,1.30000000000038,11.5846424150601));
#59681=CARTESIAN_POINT('Ctrl Pts',(2.23530773828075,-1.30000000000279,11.6858870354544));
#59682=CARTESIAN_POINT('Ctrl Pts',(2.26834048320191,-1.18514270861393,11.6686655879137));
#59683=CARTESIAN_POINT('Ctrl Pts',(2.290425030513,-1.06847604194659,11.6458802525827));
#59684=CARTESIAN_POINT('Ctrl Pts',(2.31615222614137,-0.794772684001515,
11.58038787593));
#59685=CARTESIAN_POINT('Ctrl Pts',(2.29209956838144,-0.636309800095726,
11.5152335524785));
#59686=CARTESIAN_POINT('Ctrl Pts',(2.28591671441847,-0.319434907277423,
11.4410086031402));
#59687=CARTESIAN_POINT('Ctrl Pts',(2.26841145191158,-0.158333333333464,
11.400860557849));
#59688=CARTESIAN_POINT('Ctrl Pts',(2.29717109254721,0.158333333333466,11.3851123134352));
#59689=CARTESIAN_POINT('Ctrl Pts',(2.34426015135361,0.319434907277433,11.4090637091879));
#59690=CARTESIAN_POINT('Ctrl Pts',(2.40734557678233,0.636309800095736,11.4521239875194));
#59691=CARTESIAN_POINT('Ctrl Pts',(2.46336241513653,0.794772684001498,11.4987150878894));
#59692=CARTESIAN_POINT('Ctrl Pts',(2.47873912392656,1.06847604194613,11.543542198105));
#59693=CARTESIAN_POINT('Ctrl Pts',(2.47166857906692,1.18514270861302,11.5595159461311));
#59694=CARTESIAN_POINT('Ctrl Pts',(2.45087148187566,1.30000000000147,11.5720594471789));
#59695=CARTESIAN_POINT('Ctrl Pts',(2.21458925500902,-1.3000000000039,11.6716678043255));
#59696=CARTESIAN_POINT('Ctrl Pts',(2.24450821073624,-1.18514270861494,11.6510794388257));
#59697=CARTESIAN_POINT('Ctrl Pts',(2.26417301394859,-1.06847604194751,11.6259439271504));
#59698=CARTESIAN_POINT('Ctrl Pts',(2.28591349965399,-0.794772684002193,
11.5573710495198));
#59699=CARTESIAN_POINT('Ctrl Pts',(2.26124918157428,-0.636309800096272,
11.4937848894172));
#59700=CARTESIAN_POINT('Ctrl Pts',(2.25440606220613,-0.319434907277698,
11.4199013384659));
#59701=CARTESIAN_POINT('Ctrl Pts',(2.23856260174892,-0.1583333333336,11.380351465671));
#59702=CARTESIAN_POINT('Ctrl Pts',(2.26679504521323,0.158333333333602,11.3650566116884));
#59703=CARTESIAN_POINT('Ctrl Pts',(2.3119341972642,0.319434907277706,11.3886645054107));
#59704=CARTESIAN_POINT('Ctrl Pts',(2.37411901128249,0.636309800096281,11.4327116872793));
#59705=CARTESIAN_POINT('Ctrl Pts',(2.42815247031914,0.794772684002181,11.4798788903475));
#59706=CARTESIAN_POINT('Ctrl Pts',(2.44792960651189,1.06847604194704,11.5275204633));
#59707=CARTESIAN_POINT('Ctrl Pts',(2.44420720743149,1.18514270861403,11.545122958669));
#59708=CARTESIAN_POINT('Ctrl Pts',(2.42820161982799,1.30000000000257,11.5597056777701));
#59709=CARTESIAN_POINT('Ctrl Pts',(2.20422090175705,-1.30000000000403,11.6644270944969));
#59710=CARTESIAN_POINT('Ctrl Pts',(2.23177075940266,-1.18514270861506,11.6427215001599));
#59711=CARTESIAN_POINT('Ctrl Pts',(2.24975521241107,-1.06847604194762,11.6167302669627));
#59712=CARTESIAN_POINT('Ctrl Pts',(2.26920489837338,-0.794772684002276,
11.5467846356428));
#59713=CARTESIAN_POINT('Ctrl Pts',(2.2453879086411,-0.636309800096337,11.4831102051312));
#59714=CARTESIAN_POINT('Ctrl Pts',(2.23874366496151,-0.319434907277732,
11.4089868433271));
#59715=CARTESIAN_POINT('Ctrl Pts',(2.22383100673436,-0.158333333333616,
11.3696723109777));
#59716=CARTESIAN_POINT('Ctrl Pts',(2.25180953322925,0.158333333333618,11.3545940342089));
#59717=CARTESIAN_POINT('Ctrl Pts',(2.29556217988666,0.31943490727774,11.3783403252151));
#59718=CARTESIAN_POINT('Ctrl Pts',(2.3574419315806,0.636309800096347,11.422748345473));
#59719=CARTESIAN_POINT('Ctrl Pts',(2.4112044664916,0.794772684002265,11.4695896170442));
#59720=CARTESIAN_POINT('Ctrl Pts',(2.43321311783985,1.06847604194715,11.5186576826337));
#59721=CARTESIAN_POINT('Ctrl Pts',(2.43103091988541,1.18514270861416,11.5372194632602));
#59722=CARTESIAN_POINT('Ctrl Pts',(2.41713979430878,1.30000000000271,11.5531032770706));
#59723=CARTESIAN_POINT('Ctrl Pts',(2.20398271305387,-1.30000000000403,11.6642592255014));
#59724=CARTESIAN_POINT('Ctrl Pts',(2.23147772863584,-1.18514270861506,11.6425279411832));
#59725=CARTESIAN_POINT('Ctrl Pts',(2.24942324895868,-1.06847604194762,11.6165170527948));
#59726=CARTESIAN_POINT('Ctrl Pts',(2.26881974647487,-0.794772684002275,
11.5465399556231));
#59727=CARTESIAN_POINT('Ctrl Pts',(2.24502184968262,-0.636309800096337,
11.4828638696009));
#59728=CARTESIAN_POINT('Ctrl Pts',(2.23838253278702,-0.319434907277731,
11.4087346991213));
#59729=CARTESIAN_POINT('Ctrl Pts',(2.22349255559444,-0.158333333333616,
11.3694246448445));
#59730=CARTESIAN_POINT('Ctrl Pts',(2.25146532055883,0.158333333333618,11.3543512781286));
#59731=CARTESIAN_POINT('Ctrl Pts',(2.29518505465604,0.319434907277739,11.3781014732845));
#59732=CARTESIAN_POINT('Ctrl Pts',(2.3570572488014,0.636309800096346,11.422518231083));
#59733=CARTESIAN_POINT('Ctrl Pts',(2.41081342436635,0.794772684002264,11.469352080062));
#59734=CARTESIAN_POINT('Ctrl Pts',(2.43287351260473,1.06847604194715,11.5184531279471));
#59735=CARTESIAN_POINT('Ctrl Pts',(2.43072689081419,1.18514270861416,11.5370370274423));
#59736=CARTESIAN_POINT('Ctrl Pts',(2.41688465244154,1.30000000000271,11.5529508021763));
#59737=CARTESIAN_POINT('Ctrl Pts',(2.20374429237847,-1.30000000000403,11.6640915148277));
#59738=CARTESIAN_POINT('Ctrl Pts',(2.23118465586839,-1.18514270861506,11.6423344085549));
#59739=CARTESIAN_POINT('Ctrl Pts',(2.24909137662577,-1.06847604194762,11.6163037719359));
#59740=CARTESIAN_POINT('Ctrl Pts',(2.26843486189156,-0.794772684002275,
11.5462950839186));
#59741=CARTESIAN_POINT('Ctrl Pts',(2.24465608947658,-0.636309800096337,
11.4826173038171));
#59742=CARTESIAN_POINT('Ctrl Pts',(2.23802145507188,-0.319434907277731,
11.4084825157905));
#59743=CARTESIAN_POINT('Ctrl Pts',(2.22315358796243,-0.158333333333616,
11.3691773918339));
#59744=CARTESIAN_POINT('Ctrl Pts',(2.25112054657791,0.158333333333618,11.3541089715631));
#59745=CARTESIAN_POINT('Ctrl Pts',(2.29480790079592,0.31943490727774,11.3778626514247));
#59746=CARTESIAN_POINT('Ctrl Pts',(2.35667267705616,0.636309800096346,11.4222880370731));
#59747=CARTESIAN_POINT('Ctrl Pts',(2.41042225638184,0.794772684002264,11.469114651762));
#59748=CARTESIAN_POINT('Ctrl Pts',(2.43253374250881,1.06847604194715,11.5182487095283));
#59749=CARTESIAN_POINT('Ctrl Pts',(2.43042270360374,1.18514270861416,11.5368547201871));
#59750=CARTESIAN_POINT('Ctrl Pts',(2.41662938276054,1.30000000000271,11.5527984284941));
#59751=CARTESIAN_POINT('Ctrl Pts',(2.20326815095482,-1.30000000000403,11.6637555811632));
#59752=CARTESIAN_POINT('Ctrl Pts',(2.23059929868076,-1.18514270861506,11.6419467453765));
#59753=CARTESIAN_POINT('Ctrl Pts',(2.24842844762722,-1.06847604194762,11.6158765783256));
#59754=CARTESIAN_POINT('Ctrl Pts',(2.26766583035358,-0.794772684002275,
11.5458047494221));
#59755=CARTESIAN_POINT('Ctrl Pts',(2.24392490420093,-0.636309800096337,
11.4821238977744));
#59756=CARTESIAN_POINT('Ctrl Pts',(2.23729963343724,-0.319434907277731,
11.4079778659707));
#59757=CARTESIAN_POINT('Ctrl Pts',(2.22247638038832,-0.158333333333616,
11.3686822890953));
#59758=CARTESIAN_POINT('Ctrl Pts',(2.25043176433982,0.158333333333618,11.3536237233659));
#59759=CARTESIAN_POINT('Ctrl Pts',(2.2940541909032,0.319434907277739,11.3773844944774));
#59760=CARTESIAN_POINT('Ctrl Pts',(2.35590382733677,0.636309800096346,11.4218273788027));
#59761=CARTESIAN_POINT('Ctrl Pts',(2.40963980116502,0.794772684002264,11.4686398671136));
#59762=CARTESIAN_POINT('Ctrl Pts',(2.4318539817315,1.06847604194715,11.5178400351151));
#59763=CARTESIAN_POINT('Ctrl Pts',(2.42981415266791,1.18514270861415,11.5364902367237));
#59764=CARTESIAN_POINT('Ctrl Pts',(2.41611879889003,1.30000000000271,11.5524937102589));
#59765=CARTESIAN_POINT('Ctrl Pts',(2.2022382209217,-1.30000000000403,11.6630264246427));
#59766=CARTESIAN_POINT('Ctrl Pts',(2.22933390480984,-1.18514270861506,11.6411045997646));
#59767=CARTESIAN_POINT('Ctrl Pts',(2.24699565887793,-1.06847604194761,11.6149482520847));
#59768=CARTESIAN_POINT('Ctrl Pts',(2.26600357886143,-0.794772684002273,
11.544739261599));
#59769=CARTESIAN_POINT('Ctrl Pts',(2.24234313065998,-0.636309800096335,
11.4810528947618));
#59770=CARTESIAN_POINT('Ctrl Pts',(2.23573710080049,-0.319434907277731,
11.4068832834797));
#59771=CARTESIAN_POINT('Ctrl Pts',(2.22100969320709,-0.158333333333616,
11.3676090343005));
#59772=CARTESIAN_POINT('Ctrl Pts',(2.24893997869284,0.158333333333618,11.3525718078456));
#59773=CARTESIAN_POINT('Ctrl Pts',(2.29242331970258,0.319434907277739,11.3763466484417));
#59774=CARTESIAN_POINT('Ctrl Pts',(2.35423954466323,0.636309800096345,11.4208279438684));
#59775=CARTESIAN_POINT('Ctrl Pts',(2.40794337957116,0.794772684002263,11.4676120015508));
#59776=CARTESIAN_POINT('Ctrl Pts',(2.43037953301274,1.06847604194715,11.5169558556867));
#59777=CARTESIAN_POINT('Ctrl Pts',(2.4284942213846,1.18514270861415,11.5357016246912));
#59778=CARTESIAN_POINT('Ctrl Pts',(2.41501181864488,1.30000000000271,11.5518340366149));
#59779=CARTESIAN_POINT('Ctrl Pts',(2.20097659874509,-1.30000000000402,11.6621244262188));
#59780=CARTESIAN_POINT('Ctrl Pts',(2.22778734368446,-1.18514270861505,11.640059792093));
#59781=CARTESIAN_POINT('Ctrl Pts',(2.24524586504824,-1.06847604194761,11.6137952097305));
#59782=CARTESIAN_POINT('Ctrl Pts',(2.26397303459823,-0.794772684002269,
11.5434160496375));
#59783=CARTESIAN_POINT('Ctrl Pts',(2.2404050642365,-0.636309800096332,11.4797278359943));
#59784=CARTESIAN_POINT('Ctrl Pts',(2.23381838546602,-0.319434907277729,
11.405532456724));
#59785=CARTESIAN_POINT('Ctrl Pts',(2.21920578066758,-0.158333333333615,
11.3662869368743));
#59786=CARTESIAN_POINT('Ctrl Pts',(2.24710526181061,0.158333333333617,11.3512758015688));
#59787=CARTESIAN_POINT('Ctrl Pts',(2.29042401540504,0.319434907277737,11.3750625946385));
#59788=CARTESIAN_POINT('Ctrl Pts',(2.35219680450747,0.636309800096341,11.4195930837349));
#59789=CARTESIAN_POINT('Ctrl Pts',(2.40585019176021,0.794772684002258,11.4663511106323));
#59790=CARTESIAN_POINT('Ctrl Pts',(2.42855770162894,1.06847604194714,11.5158733572356));
#59791=CARTESIAN_POINT('Ctrl Pts',(2.4268637067064,1.18514270861415,11.5347358290338));
#59792=CARTESIAN_POINT('Ctrl Pts',(2.41364647723532,1.3000000000027,11.5510244270556));
#59793=CARTESIAN_POINT('Ctrl Pts',(2.19972111476395,-1.30000000000402,11.6612176268975));
#59794=CARTESIAN_POINT('Ctrl Pts',(2.22625418374014,-1.18514270861505,11.6390046508609));
#59795=CARTESIAN_POINT('Ctrl Pts',(2.24351370352598,-1.0684760419476,11.6126285984401));
#59796=CARTESIAN_POINT('Ctrl Pts',(2.26196289318945,-0.794772684002267,
11.542077101569));
#59797=CARTESIAN_POINT('Ctrl Pts',(2.23847840133977,-0.63630980009633,11.4783937795508));
#59798=CARTESIAN_POINT('Ctrl Pts',(2.23190425369703,-0.319434907277728,
11.4041778067659));
#59799=CARTESIAN_POINT('Ctrl Pts',(2.2174001040939,-0.158333333333614,11.3649660215187));
#59800=CARTESIAN_POINT('Ctrl Pts',(2.24526898456281,0.158333333333616,11.3499806797437));
#59801=CARTESIAN_POINT('Ctrl Pts',(2.28843442810971,0.319434907277736,11.3737702808472));
#59802=CARTESIAN_POINT('Ctrl Pts',(2.35016138944899,0.63630980009634,11.4183520078683));
#59803=CARTESIAN_POINT('Ctrl Pts',(2.40374838610745,0.794772684002256,11.4650971761613));
#59804=CARTESIAN_POINT('Ctrl Pts',(2.4267250436441,1.06847604194714,11.5147996835543));
#59805=CARTESIAN_POINT('Ctrl Pts',(2.42522425508426,1.18514270861414,11.533777318534));
#59806=CARTESIAN_POINT('Ctrl Pts',(2.41227693428602,1.3000000000027,11.5502182147024));
#59807=CARTESIAN_POINT('Ctrl Pts',(2.19846958455996,-1.30000000000402,11.6603077003021));
#59808=CARTESIAN_POINT('Ctrl Pts',(2.22473048776691,-1.18514270861504,11.6379422093842));
#59809=CARTESIAN_POINT('Ctrl Pts',(2.24179423622381,-1.0684760419476,11.6114522353677));
#59810=CARTESIAN_POINT('Ctrl Pts',(2.2599676413933,-0.794772684002265,11.5407267150302));
#59811=CARTESIAN_POINT('Ctrl Pts',(2.23656002147746,-0.636309800096329,
11.4770532238972));
#59812=CARTESIAN_POINT('Ctrl Pts',(2.22999320980567,-0.319434907277727,
11.402820611383));
#59813=CARTESIAN_POINT('Ctrl Pts',(2.21559242099688,-0.158333333333614,
11.3636465782712));
#59814=CARTESIAN_POINT('Ctrl Pts',(2.24343082185128,0.158333333333616,11.3486868387618));
#59815=CARTESIAN_POINT('Ctrl Pts',(2.28645160784339,0.319434907277736,11.372472245126));
#59816=CARTESIAN_POINT('Ctrl Pts',(2.34813118217902,0.636309800096338,11.41710655782));
#59817=CARTESIAN_POINT('Ctrl Pts',(2.40164008353647,0.794772684002254,11.463848543502));
#59818=CARTESIAN_POINT('Ctrl Pts',(2.42488430650129,1.06847604194714,11.5137326365625));
#59819=CARTESIAN_POINT('Ctrl Pts',(2.42357811786405,1.18514270861414,11.5328242879174));
#59820=CARTESIAN_POINT('Ctrl Pts',(2.41090417775146,1.30000000000269,11.5494146151291));
#59821=CARTESIAN_POINT('Ctrl Pts',(2.196289457676,-1.30000000000401,11.6587073086812));
#59822=CARTESIAN_POINT('Ctrl Pts',(2.22208944260743,-1.18514270861504,11.6360632937767));
#59823=CARTESIAN_POINT('Ctrl Pts',(2.23881963717771,-1.0684760419476,11.6093671057776));
#59824=CARTESIAN_POINT('Ctrl Pts',(2.25651670335936,-0.794772684002261,
11.5383322404626));
#59825=CARTESIAN_POINT('Ctrl Pts',(2.23322556856686,-0.636309800096326,
11.474689429772));
#59826=CARTESIAN_POINT('Ctrl Pts',(2.226657040534,-0.319434907277726,11.400438793734));
#59827=CARTESIAN_POINT('Ctrl Pts',(2.21242235554669,-0.158333333333613,
11.3613424939));
#59828=CARTESIAN_POINT('Ctrl Pts',(2.24020775659807,0.158333333333615,11.3464270281605));
#59829=CARTESIAN_POINT('Ctrl Pts',(2.28299994815951,0.319434907277734,11.3701852165769));
#59830=CARTESIAN_POINT('Ctrl Pts',(2.34459261416236,0.636309800096335,11.4149150216674));
#59831=CARTESIAN_POINT('Ctrl Pts',(2.39793244491085,0.79477268400225,11.4616782436047));
#59832=CARTESIAN_POINT('Ctrl Pts',(2.42164060809001,1.06847604194713,11.5118837130961));
#59833=CARTESIAN_POINT('Ctrl Pts',(2.42067884707763,1.18514270861413,11.53117169741));
#59834=CARTESIAN_POINT('Ctrl Pts',(2.40849293968664,1.30000000000269,11.548015578591));
#59835=CARTESIAN_POINT('Ctrl Pts',(2.19381875820583,-1.30000000000399,11.656861363637));
#59836=CARTESIAN_POINT('Ctrl Pts',(2.21912960775502,-1.18514270861502,11.6338706984122));
#59837=CARTESIAN_POINT('Ctrl Pts',(2.23550094426406,-1.06847604194758,11.60692200114));
#59838=CARTESIAN_POINT('Ctrl Pts',(2.25266994320834,-0.794772684002247,
11.5355212735421));
#59839=CARTESIAN_POINT('Ctrl Pts',(2.22946984941338,-0.636309800096315,
11.4719449319254));
#59840=CARTESIAN_POINT('Ctrl Pts',(2.22286379687592,-0.31943490727772,11.3977008907338));
#59841=CARTESIAN_POINT('Ctrl Pts',(2.20878069664508,-0.158333333333611,
11.3587236376341));
#59842=CARTESIAN_POINT('Ctrl Pts',(2.23650590193875,0.158333333333613,11.3438578368234));
#59843=CARTESIAN_POINT('Ctrl Pts',(2.27909738250193,0.319434907277728,11.3675359022546));
#59844=CARTESIAN_POINT('Ctrl Pts',(2.34058241077827,0.636309800096324,11.4123821553926));
#59845=CARTESIAN_POINT('Ctrl Pts',(2.39365232488814,0.794772684002237,11.459233165597));
#59846=CARTESIAN_POINT('Ctrl Pts',(2.41788040073657,1.06847604194712,11.5098144836929));
#59847=CARTESIAN_POINT('Ctrl Pts',(2.41732125518124,1.18514270861411,11.5293193830973));
#59848=CARTESIAN_POINT('Ctrl Pts',(2.40571552777447,1.30000000000266,11.546434403525));
#59849=CARTESIAN_POINT('Ctrl Pts',(2.19136056145869,-1.30000000000398,11.6550049970701));
#59850=CARTESIAN_POINT('Ctrl Pts',(2.21620612079724,-1.18514270861501,11.6316495906278));
#59851=CARTESIAN_POINT('Ctrl Pts',(2.23223326356462,-1.06847604194757,11.6044372461332));
#59852=CARTESIAN_POINT('Ctrl Pts',(2.24888686317861,-0.794772684002242,
11.5326609880614));
#59853=CARTESIAN_POINT('Ctrl Pts',(2.22575506717335,-0.636309800096311,
11.4691681493286));
#59854=CARTESIAN_POINT('Ctrl Pts',(2.21909151598682,-0.319434907277718,
11.3949460381804));
#59855=CARTESIAN_POINT('Ctrl Pts',(2.20513628823617,-0.15833333333361,11.3561066828364));
#59856=CARTESIAN_POINT('Ctrl Pts',(2.23280061172639,0.158333333333612,11.3412905160417));
#59857=CARTESIAN_POINT('Ctrl Pts',(2.27522625937924,0.319434907277726,11.3648597398984));
#59858=CARTESIAN_POINT('Ctrl Pts',(2.33659808526763,0.63630980009632,11.4098270794775));
#59859=CARTESIAN_POINT('Ctrl Pts',(2.38935396916815,0.794772684002232,11.4568025472316));
#59860=CARTESIAN_POINT('Ctrl Pts',(2.41409391815274,1.06847604194711,11.5077664944603));
#59861=CARTESIAN_POINT('Ctrl Pts',(2.41394125332881,1.18514270861411,11.527485158495));
#59862=CARTESIAN_POINT('Ctrl Pts',(2.40292691647096,1.30000000000265,11.5448620822094));
#59863=CARTESIAN_POINT('Ctrl Pts',(2.18890613509595,-1.30000000000397,11.6531452736484));
#59864=CARTESIAN_POINT('Ctrl Pts',(2.21329486975642,-1.185142708615,11.629418650736));
#59865=CARTESIAN_POINT('Ctrl Pts',(2.22898346622039,-1.06847604194757,11.6019383403953));
#59866=CARTESIAN_POINT('Ctrl Pts',(2.24512820285448,-0.794772684002238,
11.529781557209));
#59867=CARTESIAN_POINT('Ctrl Pts',(2.22206011856169,-0.636309800096307,
11.4663757108842));
#59868=CARTESIAN_POINT('Ctrl Pts',(2.21533413273925,-0.319434907277716,
11.3921793633731));
#59869=CARTESIAN_POINT('Ctrl Pts',(2.20149883179455,-0.158333333333609,
11.3534842563929));
#59870=CARTESIAN_POINT('Ctrl Pts',(2.22910075916764,0.158333333333611,11.3387185888212));
#59871=CARTESIAN_POINT('Ctrl Pts',(2.27136895221501,0.319434907277724,11.3621717074321));
#59872=CARTESIAN_POINT('Ctrl Pts',(2.33262546136905,0.636309800096317,11.4072616844316));
#59873=CARTESIAN_POINT('Ctrl Pts',(2.38505696532997,0.794772684002227,11.4543702890334));
#59874=CARTESIAN_POINT('Ctrl Pts',(2.41030485625289,1.0684760419471,11.5057201840077));
#59875=CARTESIAN_POINT('Ctrl Pts',(2.41055832334208,1.1851427086141,11.5256529414547));
#59876=CARTESIAN_POINT('Ctrl Pts',(2.4001363810665,1.30000000000265,11.5432909895155));
#59877=CARTESIAN_POINT('Ctrl Pts',(2.1858362201203,-1.30000000000395,11.6508213457672));
#59878=CARTESIAN_POINT('Ctrl Pts',(2.20965543231636,-1.18514270861498,11.6266293618945));
#59879=CARTESIAN_POINT('Ctrl Pts',(2.22492307718425,-1.06847604194755,11.5988122794044));
#59880=CARTESIAN_POINT('Ctrl Pts',(2.24043855984763,-0.794772684002225,
11.5261745510593));
#59881=CARTESIAN_POINT('Ctrl Pts',(2.21745805066438,-0.636309800096297,
11.462871622945));
#59882=CARTESIAN_POINT('Ctrl Pts',(2.21066095291805,-0.319434907277711,
11.3887023331593));
#59883=CARTESIAN_POINT('Ctrl Pts',(2.19697882939341,-0.158333333333606,
11.3501853121502));
#59884=CARTESIAN_POINT('Ctrl Pts',(2.22450100165638,0.158333333333608,11.3354837726768));
#59885=CARTESIAN_POINT('Ctrl Pts',(2.26656305125532,0.319434907277719,11.3587981689194));
#59886=CARTESIAN_POINT('Ctrl Pts',(2.3276736494858,0.636309800096306,11.4040421560062));
#59887=CARTESIAN_POINT('Ctrl Pts',(2.3797099125093,0.794772684002214,11.4513087737755));
#59888=CARTESIAN_POINT('Ctrl Pts',(2.40558757945241,1.06847604194709,11.5031454341553));
#59889=CARTESIAN_POINT('Ctrl Pts',(2.40634353421008,1.18514270861408,11.5233501989616));
#59890=CARTESIAN_POINT('Ctrl Pts',(2.39665396056781,1.30000000000263,11.5413215590332));
#59891=CARTESIAN_POINT('Ctrl Pts',(2.18274681931169,-1.30000000000394,11.6485118513956));
#59892=CARTESIAN_POINT('Ctrl Pts',(2.20596545257011,-1.18514270861498,11.6238773181772));
#59893=CARTESIAN_POINT('Ctrl Pts',(2.2207965192823,-1.06847604194754,11.5957348565602));
#59894=CARTESIAN_POINT('Ctrl Pts',(2.2356822936834,-0.79477268400222,11.5226161239857));
#59895=CARTESIAN_POINT('Ctrl Pts',(2.21284515572733,-0.636309800096293,
11.4593748350266));
#59896=CARTESIAN_POINT('Ctrl Pts',(2.20602242295296,-0.319434907277709,
11.3851980449969));
#59897=CARTESIAN_POINT('Ctrl Pts',(2.1925330202892,-0.158333333333605,11.3468283024874));
#59898=CARTESIAN_POINT('Ctrl Pts',(2.21996847361036,0.158333333333607,11.3321960418809));
#59899=CARTESIAN_POINT('Ctrl Pts',(2.2617470425695,0.319434907277717,11.355432011693));
#59900=CARTESIAN_POINT('Ctrl Pts',(2.32271486648178,0.636309800096302,11.4008254844439));
#59901=CARTESIAN_POINT('Ctrl Pts',(2.37444872503291,0.794772684002209,11.4481734012841));
#59902=CARTESIAN_POINT('Ctrl Pts',(2.40095716721983,1.06847604194708,11.5004963520746));
#59903=CARTESIAN_POINT('Ctrl Pts',(2.40219792525709,1.18514270861407,11.5209881575624));
#59904=CARTESIAN_POINT('Ctrl Pts',(2.39320491894349,1.30000000000262,11.5393231018971));
#59905=CARTESIAN_POINT('Ctrl Pts',(2.18025660829921,-1.30000000000394,11.646678211753));
#59906=CARTESIAN_POINT('Ctrl Pts',(2.20296867079828,-1.18514270861497,11.6217090029632));
#59907=CARTESIAN_POINT('Ctrl Pts',(2.21743567570788,-1.06847604194754,11.5933171726611));
#59908=CARTESIAN_POINT('Ctrl Pts',(2.23180961871364,-0.794772684002217,
11.5198194245105));
#59909=CARTESIAN_POINT('Ctrl Pts',(2.20911846574213,-0.63630980009629,11.4566041124908));
#59910=CARTESIAN_POINT('Ctrl Pts',(2.20231019257562,-0.319434907277708,
11.3823947825735));
#59911=CARTESIAN_POINT('Ctrl Pts',(2.18901523160592,-0.158333333333604,
11.3441120092495));
#59912=CARTESIAN_POINT('Ctrl Pts',(2.2163859784749,0.158333333333606,11.3295317990621));
#59913=CARTESIAN_POINT('Ctrl Pts',(2.2578893782394,0.319434907277716,11.3527429855684));
#59914=CARTESIAN_POINT('Ctrl Pts',(2.31874357388177,0.636309800096299,11.3982543759599));
#59915=CARTESIAN_POINT('Ctrl Pts',(2.37028507707526,0.794772684002206,11.4456257258716));
#59916=CARTESIAN_POINT('Ctrl Pts',(2.39730020603818,1.06847604194707,11.4983361946587));
#59917=CARTESIAN_POINT('Ctrl Pts',(2.3989204728418,1.18514270861407,11.5190648878959));
#59918=CARTESIAN_POINT('Ctrl Pts',(2.39046715813017,1.30000000000261,11.5377058655478));
#59919=CARTESIAN_POINT('Ctrl Pts',(2.17775975093903,-1.30000000000393,11.6448494909324));
#59920=CARTESIAN_POINT('Ctrl Pts',(2.1999539175159,-1.18514270861497,11.6195538847476));
#59921=CARTESIAN_POINT('Ctrl Pts',(2.21405164558089,-1.06847604194753,11.5909164716912));
#59922=CARTESIAN_POINT('Ctrl Pts',(2.22791582500244,-0.794772684002214,
11.5170380762368));
#59923=CARTESIAN_POINT('Ctrl Pts',(2.20539661759653,-0.636309800096288,
11.4538297129487));
#59924=CARTESIAN_POINT('Ctrl Pts',(2.19861822688681,-0.319434907277707,
11.3795761410745));
#59925=CARTESIAN_POINT('Ctrl Pts',(2.18552618106875,-0.158333333333604,
11.3413733749366));
#59926=CARTESIAN_POINT('Ctrl Pts',(2.21282429868796,0.158333333333606,11.3268511133002));
#59927=CARTESIAN_POINT('Ctrl Pts',(2.25401998840293,0.319434907277715,11.3500629397051));
#59928=CARTESIAN_POINT('Ctrl Pts',(2.31476188014544,0.636309800096297,11.3956903738005));
#59929=CARTESIAN_POINT('Ctrl Pts',(2.3661513861697,0.794772684002203,11.4430519749583));
#59930=CARTESIAN_POINT('Ctrl Pts',(2.39367608711183,1.06847604194707,11.4961478266809));
#59931=CARTESIAN_POINT('Ctrl Pts',(2.39566977940424,1.18514270861406,11.5171186416964));
#59932=CARTESIAN_POINT('Ctrl Pts',(2.38774274084191,1.30000000000261,11.5360770449118));
#59933=CARTESIAN_POINT('Ctrl Pts',(2.16579089614802,-1.30000000000387,11.6362433191586));
#59934=CARTESIAN_POINT('Ctrl Pts',(2.18540265690836,-1.18514270861491,11.6094888559996));
#59935=CARTESIAN_POINT('Ctrl Pts',(2.19766263552379,-1.06847604194748,11.5797471743966));
#59936=CARTESIAN_POINT('Ctrl Pts',(2.209001551252,-0.794772684002177,11.5041368678941));
#59937=CARTESIAN_POINT('Ctrl Pts',(2.18729931429024,-0.636309800096258,
11.440958509013));
#59938=CARTESIAN_POINT('Ctrl Pts',(2.1808226017509,-0.319434907277691,11.3663741715338));
#59939=CARTESIAN_POINT('Ctrl Pts',(2.16898780467268,-0.158333333333596,
11.3283326797682));
#59940=CARTESIAN_POINT('Ctrl Pts',(2.19607948758469,0.158333333333598,11.3139831473216));
#59941=CARTESIAN_POINT('Ctrl Pts',(2.23573338242787,0.3194349072777,11.3372605965225));
#59942=CARTESIAN_POINT('Ctrl Pts',(2.29591221071323,0.636309800096267,11.3834602968739));
#59943=CARTESIAN_POINT('Ctrl Pts',(2.3465312248773,0.794772684002165,11.4308060021429));
#59944=CARTESIAN_POINT('Ctrl Pts',(2.37647426338148,1.06847604194702,11.4857343454214));
#59945=CARTESIAN_POINT('Ctrl Pts',(2.38025268270869,1.18514270861401,11.5078485077896));
#59946=CARTESIAN_POINT('Ctrl Pts',(2.37484828949358,1.30000000000255,11.5283003880162));
#59947=CARTESIAN_POINT('Ctrl Pts',(2.14717526900777,-1.30000000000332,11.6224242908445));
#59948=CARTESIAN_POINT('Ctrl Pts',(2.16302496616783,-1.18514270861441,11.5931207467066));
#59949=CARTESIAN_POINT('Ctrl Pts',(2.17265618912359,-1.06847604194703,11.5614273824515));
#59950=CARTESIAN_POINT('Ctrl Pts',(2.18054032145746,-0.794772684001842,
11.4826884082334));
#59951=CARTESIAN_POINT('Ctrl Pts',(2.16070647808883,-0.63630980009599,11.4191546062562));
#59952=CARTESIAN_POINT('Ctrl Pts',(2.15432666181657,-0.319434907277558,
11.3443408313766));
#59953=CARTESIAN_POINT('Ctrl Pts',(2.14331228751259,-0.15833333333353,11.3074176251932));
#59954=CARTESIAN_POINT('Ctrl Pts',(2.16930606692612,0.158333333333532,11.2939081140232));
#59955=CARTESIAN_POINT('Ctrl Pts',(2.20631618296266,0.319434907277567,11.3174363365325));
#59956=CARTESIAN_POINT('Ctrl Pts',(2.26563945918351,0.636309800096001,11.364498925613));
#59957=CARTESIAN_POINT('Ctrl Pts',(2.31572832178763,0.794772684001833,11.4112877513487));
#59958=CARTESIAN_POINT('Ctrl Pts',(2.34953065051007,1.06847604194657,11.4690816213842));
#59959=CARTESIAN_POINT('Ctrl Pts',(2.35601714912541,1.18514270861351,11.493090142667));
#59960=CARTESIAN_POINT('Ctrl Pts',(2.35435837075185,1.300000000002,11.5160903603682));
#59961=CARTESIAN_POINT('Ctrl Pts',(2.12785423414619,-1.30000000000305,11.6072652710164));
#59962=CARTESIAN_POINT('Ctrl Pts',(2.14022095354043,-1.18514270861416,11.5748523654447));
#59963=CARTESIAN_POINT('Ctrl Pts',(2.1471949550396,-1.06847604194681,11.5409647164221));
#59964=CARTESIAN_POINT('Ctrl Pts',(2.15084803649971,-0.794772684001673,
11.4592705155861));
#59965=CARTESIAN_POINT('Ctrl Pts',(2.130612959672,-0.636309800095855,11.3970814063584));
#59966=CARTESIAN_POINT('Ctrl Pts',(2.12394752489425,-0.319434907277489,
11.322298665619));
#59967=CARTESIAN_POINT('Ctrl Pts',(2.11485403559682,-0.158333333333496,
11.2858356831044));
#59968=CARTESIAN_POINT('Ctrl Pts',(2.14111401956761,0.158333333333498,11.272141734391));
#59969=CARTESIAN_POINT('Ctrl Pts',(2.177089544414,0.319434907277498,11.2945546004707));
#59970=CARTESIAN_POINT('Ctrl Pts',(2.23597760148315,0.636309800095864,11.3421692416818));
#59971=CARTESIAN_POINT('Ctrl Pts',(2.28393046254491,0.794772684001663,11.3895527718085));
#59972=CARTESIAN_POINT('Ctrl Pts',(2.3216167171952,1.06847604194634,11.4506061376397));
#59973=CARTESIAN_POINT('Ctrl Pts',(2.33109765843318,1.18514270861326,11.4765734373573));
#59974=CARTESIAN_POINT('Ctrl Pts',(2.33374655768437,1.30000000000172,11.5020802969744));
#59975=CARTESIAN_POINT('Ctrl Pts',(2.10820023776197,-1.30000000000293,11.5923398545344));
#59976=CARTESIAN_POINT('Ctrl Pts',(2.11650951602755,-1.18514270861406,11.5572139196954));
#59977=CARTESIAN_POINT('Ctrl Pts',(2.1207230502368,-1.06847604194671,11.5211951992743));
#59978=CARTESIAN_POINT('Ctrl Pts',(2.12099516905386,-0.794772684001603,
11.4359222362857));
#59979=CARTESIAN_POINT('Ctrl Pts',(2.10348361829659,-0.6363098000958,11.3728458265936));
#59980=CARTESIAN_POINT('Ctrl Pts',(2.0970554529222,-0.319434907277462,11.2977193417764));
#59981=CARTESIAN_POINT('Ctrl Pts',(2.08824332842965,-0.158333333333482,
11.2628850822701));
#59982=CARTESIAN_POINT('Ctrl Pts',(2.11335652669121,0.158333333333484,11.2500334513889));
#59983=CARTESIAN_POINT('Ctrl Pts',(2.14718474037035,0.319434907277469,11.2721570984063));
#59984=CARTESIAN_POINT('Ctrl Pts',(2.20496448658686,0.636309800095809,11.3208184921549));
#59985=CARTESIAN_POINT('Ctrl Pts',(2.25147409348881,0.794772684001595,11.3682791264201));
#59986=CARTESIAN_POINT('Ctrl Pts',(2.2928104914806,1.06847604194625,11.432774068759));
#59987=CARTESIAN_POINT('Ctrl Pts',(2.30506520593544,1.18514270861315,11.4608706729831));
#59988=CARTESIAN_POINT('Ctrl Pts',(2.31168163981896,1.30000000000161,11.4891464106659));
#59989=CARTESIAN_POINT('Ctrl Pts',(2.09127259383845,-1.30000000000273,11.5790458884984));
#59990=CARTESIAN_POINT('Ctrl Pts',(2.09686929881197,-1.18514270861387,11.5409596357206));
#59991=CARTESIAN_POINT('Ctrl Pts',(2.09901345333544,-1.06847604194655,11.5028365731315));
#59992=CARTESIAN_POINT('Ctrl Pts',(2.09599079700133,-0.794772684001478,
11.4146796340307));
#59993=CARTESIAN_POINT('Ctrl Pts',(2.07807450668747,-0.636309800095701,
11.3528061731806));
#59994=CARTESIAN_POINT('Ctrl Pts',(2.07160690915555,-0.319434907277413,
11.2775500345261));
#59995=CARTESIAN_POINT('Ctrl Pts',(2.06472793802358,-0.158333333333458,
11.2429443190537));
#59996=CARTESIAN_POINT('Ctrl Pts',(2.09005130262075,0.15833333333346,11.2299402401507));
#59997=CARTESIAN_POINT('Ctrl Pts',(2.12265513190828,0.319434907277418,11.2513067596518));
#59998=CARTESIAN_POINT('Ctrl Pts',(2.17988678631191,0.636309800095708,11.3005534424449));
#59999=CARTESIAN_POINT('Ctrl Pts',(2.22464331497208,0.794772684001471,11.3484204259832));
#60000=CARTESIAN_POINT('Ctrl Pts',(2.26918865414128,1.06847604194609,11.4159190371282));
#60001=CARTESIAN_POINT('Ctrl Pts',(2.28393376959161,1.18514270861297,11.445840624386));
#60002=CARTESIAN_POINT('Ctrl Pts',(2.2941419737334,1.30000000000141,11.4764661512069));
#60003=CARTESIAN_POINT('Ctrl Pts',(2.07532697621282,-1.3000000000026,11.5651096373288));
#60004=CARTESIAN_POINT('Ctrl Pts',(2.07757854621287,-1.18514270861376,11.5244753995875));
#60005=CARTESIAN_POINT('Ctrl Pts',(2.07740481777085,-1.06847604194644,11.4843999320093));
#60006=CARTESIAN_POINT('Ctrl Pts',(2.07140054573513,-0.7947726840014,11.3931084556919));
#60007=CARTESIAN_POINT('Ctrl Pts',(2.05524052391013,-0.636309800095639,
11.3309321974488));
#60008=CARTESIAN_POINT('Ctrl Pts',(2.04907147176573,-0.319434907277382,
11.2553117316264));
#60009=CARTESIAN_POINT('Ctrl Pts',(2.04330560685149,-0.158333333333442,
11.2215124938134));
#60010=CARTESIAN_POINT('Ctrl Pts',(2.06743297899763,0.158333333333444,11.2093599746065));
#60011=CARTESIAN_POINT('Ctrl Pts',(2.09706149851041,0.319434907277387,11.2312251157515));
#60012=CARTESIAN_POINT('Ctrl Pts',(2.15291548107219,0.636309800095646,11.281646863975));
#60013=CARTESIAN_POINT('Ctrl Pts',(2.19674656650228,0.794772684001394,11.3293153036376));
#60014=CARTESIAN_POINT('Ctrl Pts',(2.24466047260869,1.06847604194598,11.3997083221982));
#60015=CARTESIAN_POINT('Ctrl Pts',(2.26192153729684,1.18514270861285,11.4314426906725));
#60016=CARTESIAN_POINT('Ctrl Pts',(2.27570351210487,1.30000000000128,11.4644408982047));
#60017=CARTESIAN_POINT('Ctrl Pts',(2.06703609102509,-1.30000000000259,11.558339409599));
#60018=CARTESIAN_POINT('Ctrl Pts',(2.06772789851115,-1.18514270861374,11.5163550766524));
#60019=CARTESIAN_POINT('Ctrl Pts',(2.06646378438015,-1.06847604194643,11.4752581383681));
#60020=CARTESIAN_POINT('Ctrl Pts',(2.0590248576362,-0.794772684001393,11.3823660487101));
#60021=CARTESIAN_POINT('Ctrl Pts',(2.0436160167612,-0.636309800095632,11.3201326163491));
#60022=CARTESIAN_POINT('Ctrl Pts',(2.03752310066315,-0.319434907277378,
11.244382528723));
#60023=CARTESIAN_POINT('Ctrl Pts',(2.0320493381238,-0.15833333333344,11.2111742109098));
#60024=CARTESIAN_POINT('Ctrl Pts',(2.05600239402219,0.158333333333442,11.199134702077));
#60025=CARTESIAN_POINT('Ctrl Pts',(2.08515449655414,0.319434907277383,11.2205112381063));
#60026=CARTESIAN_POINT('Ctrl Pts',(2.14059763935983,0.636309800095639,11.2713145880716));
#60027=CARTESIAN_POINT('Ctrl Pts',(2.18336041648741,0.794772684001385,11.3193186717382));
#60028=CARTESIAN_POINT('Ctrl Pts',(2.2327241535391,1.06847604194597,11.391334482169));
#60029=CARTESIAN_POINT('Ctrl Pts',(2.2511801808519,1.18514270861284,11.4240258251324));
#60030=CARTESIAN_POINT('Ctrl Pts',(2.26672450281456,1.30000000000127,11.4582355351724));
#60031=CARTESIAN_POINT('Ctrl Pts',(2.06279202116117,-1.30000000000259,11.5550170835906));
#60032=CARTESIAN_POINT('Ctrl Pts',(2.06275384366667,-1.18514270861374,11.5123250243607));
#60033=CARTESIAN_POINT('Ctrl Pts',(2.0609667907251,-1.06847604194643,11.4707029801893));
#60034=CARTESIAN_POINT('Ctrl Pts',(2.05279808878728,-0.79477268400139,11.3770196805328));
#60035=CARTESIAN_POINT('Ctrl Pts',(2.0375888362941,-0.63630980009563,11.3148756573714));
#60036=CARTESIAN_POINT('Ctrl Pts',(2.0315723503544,-0.319434907277377,11.2390344487862));
#60037=CARTESIAN_POINT('Ctrl Pts',(2.02645821684465,-0.15833333333344,11.2059761441961));
#60038=CARTESIAN_POINT('Ctrl Pts',(2.0503854531006,0.158333333333442,11.1939534624214));
#60039=CARTESIAN_POINT('Ctrl Pts',(2.07918299434904,0.319434907277382,11.215170594379));
#60040=CARTESIAN_POINT('Ctrl Pts',(2.13443419885736,0.636309800095637,11.2661527447975));
#60041=CARTESIAN_POINT('Ctrl Pts',(2.17683124436735,0.794772684001383,11.314194270533));
#60042=CARTESIAN_POINT('Ctrl Pts',(2.22683467051598,1.06847604194597,11.3870841418656));
#60043=CARTESIAN_POINT('Ctrl Pts',(2.24579847958093,1.18514270861284,11.4203214029125));
#60044=CARTESIAN_POINT('Ctrl Pts',(2.26208146734064,1.30000000000126,11.4552446005424));
#60045=CARTESIAN_POINT('Ctrl Pts',(2.06041334439403,-1.30000000000258,11.5530881430361));
#60046=CARTESIAN_POINT('Ctrl Pts',(2.05994859131143,-1.18514270861374,11.5099973689643));
#60047=CARTESIAN_POINT('Ctrl Pts',(2.05785557660839,-1.06847604194643,11.4680796159551));
#60048=CARTESIAN_POINT('Ctrl Pts',(2.04925868386235,-0.79477268400139,11.3739511342031));
#60049=CARTESIAN_POINT('Ctrl Pts',(2.03416509416363,-0.63630980009563,11.3118575049429));
#60050=CARTESIAN_POINT('Ctrl Pts',(2.02818749776246,-0.319434907277377,
11.2359674132999));
#60051=CARTESIAN_POINT('Ctrl Pts',(2.02327194124969,-0.15833333333344,11.2029996999416));
#60052=CARTESIAN_POINT('Ctrl Pts',(2.04718860755012,0.158333333333442,11.1909831628903));
#60053=CARTESIAN_POINT('Ctrl Pts',(2.07580107504722,0.319434907277382,11.2120960888184));
#60054=CARTESIAN_POINT('Ctrl Pts',(2.13094282440124,0.636309800095637,11.2631798873757));
#60055=CARTESIAN_POINT('Ctrl Pts',(2.17310855833032,0.794772684001382,11.3112589742065));
#60056=CARTESIAN_POINT('Ctrl Pts',(2.22348049294071,1.06847604194597,11.3846460506045));
#60057=CARTESIAN_POINT('Ctrl Pts',(2.2427407163222,1.18514270861284,11.4181907026243));
#60058=CARTESIAN_POINT('Ctrl Pts',(2.25945701905647,1.30000000000126,11.4535134605503));
#60059=CARTESIAN_POINT('Ctrl Pts',(2.05008175662492,-1.30000000000257,11.5441639496957));
#60060=CARTESIAN_POINT('Ctrl Pts',(2.04771030887034,-1.18514270861372,11.4992670371596));
#60061=CARTESIAN_POINT('Ctrl Pts',(2.04423529821295,-1.06847604194641,11.4560198397657));
#60062=CARTESIAN_POINT('Ctrl Pts',(2.03365787734839,-0.794772684001376,
11.3599213342163));
#60063=CARTESIAN_POINT('Ctrl Pts',(2.01895341088084,-0.63630980009562,11.2981450873994));
#60064=CARTESIAN_POINT('Ctrl Pts',(2.01310653757849,-0.319434907277372,
11.222064419379));
#60065=CARTESIAN_POINT('Ctrl Pts',(2.00918074438003,-0.158333333333437,
11.1894381952052));
#60066=CARTESIAN_POINT('Ctrl Pts',(2.03298765738055,0.158333333333439,11.1774913875267));
#60067=CARTESIAN_POINT('Ctrl Pts',(2.06058997240673,0.319434907277377,11.1982575640768));
#60068=CARTESIAN_POINT('Ctrl Pts',(2.11519541076701,0.636309800095627,11.2498267210703));
#60069=CARTESIAN_POINT('Ctrl Pts',(2.15641126259881,0.79477268400137,11.2980101206211));
#60070=CARTESIAN_POINT('Ctrl Pts',(2.20851609507492,1.06847604194595,11.3735793773766));
#60071=CARTESIAN_POINT('Ctrl Pts',(2.22914556343519,1.18514270861282,11.408481012808));
#60072=CARTESIAN_POINT('Ctrl Pts',(2.24785024885114,1.30000000000124,11.4455731525382));
#60073=CARTESIAN_POINT('Ctrl Pts',(2.02156140521162,-1.30000000000232,11.5201193794798));
#60074=CARTESIAN_POINT('Ctrl Pts',(2.01404955018037,-1.1851427086135,11.4702923408371));
#60075=CARTESIAN_POINT('Ctrl Pts',(2.0069663174992,-1.06847604194621,11.4233369281064));
#60076=CARTESIAN_POINT('Ctrl Pts',(1.99159283638421,-0.794772684001226,
11.3214945616243));
#60077=CARTESIAN_POINT('Ctrl Pts',(1.97899458630368,-0.636309800095498,
11.2598662087087));
#60078=CARTESIAN_POINT('Ctrl Pts',(1.97382404237879,-0.319434907277311,
11.1830580850164));
#60079=CARTESIAN_POINT('Ctrl Pts',(1.9721734549569,-0.158333333333407,11.1516538828691));
#60080=CARTESIAN_POINT('Ctrl Pts',(1.99518066312744,0.158333333333409,11.140241072183));
#60081=CARTESIAN_POINT('Ctrl Pts',(2.01959671087466,0.319434907277317,11.1603570980484));
#60082=CARTESIAN_POINT('Ctrl Pts',(2.07212370422326,0.636309800095506,11.2136642768154));
#60083=CARTESIAN_POINT('Ctrl Pts',(2.11003874386777,0.794772684001218,11.2626377884138));
#60084=CARTESIAN_POINT('Ctrl Pts',(2.16716226267848,1.06847604194575,11.3438957364248));
#60085=CARTESIAN_POINT('Ctrl Pts',(2.19191591882493,1.18514270861259,11.3821875190118));
#60086=CARTESIAN_POINT('Ctrl Pts',(2.21669657645966,1.30000000000099,11.4235975293956));
#60087=CARTESIAN_POINT('Ctrl Pts',(1.98618970204284,-1.30000000000202,11.4873857546929));
#60088=CARTESIAN_POINT('Ctrl Pts',(1.97258910993661,-1.18514270861323,11.43064141872));
#60089=CARTESIAN_POINT('Ctrl Pts',(1.96126776052509,-1.06847604194597,11.3784887101778));
#60090=CARTESIAN_POINT('Ctrl Pts',(1.94037868514204,-0.794772684001049,
11.2686130982488));
#60091=CARTESIAN_POINT('Ctrl Pts',(1.93083613120932,-0.636309800095354,
11.2070608321537));
#60092=CARTESIAN_POINT('Ctrl Pts',(1.92609493733045,-0.319434907277237,
11.1296040666681));
#60093=CARTESIAN_POINT('Ctrl Pts',(1.92608674948616,-0.158333333333371,
11.1006567592145));
#60094=CARTESIAN_POINT('Ctrl Pts',(1.94760007049155,0.158333333333373,11.0901609205059));
#60095=CARTESIAN_POINT('Ctrl Pts',(1.9681369910674,0.319434907277246,11.1091527146429));
#60096=CARTESIAN_POINT('Ctrl Pts',(2.01870480624482,0.636309800095363,11.1641296084854));
#60097=CARTESIAN_POINT('Ctrl Pts',(2.0541842077594,0.794772684001037,11.2127661066329));
#60098=CARTESIAN_POINT('Ctrl Pts',(2.11720864062985,1.0684760419455,11.3019861247598));
#60099=CARTESIAN_POINT('Ctrl Pts',(2.14648289278499,1.18514270861232,11.3453784510037));
#60100=CARTESIAN_POINT('Ctrl Pts',(2.17775045539106,1.3000000000007,11.3935430635718));
#60101=CARTESIAN_POINT('Ctrl Pts',(1.95657107896372,-1.30000000000192,11.4578927873015));
#60102=CARTESIAN_POINT('Ctrl Pts',(1.93806150394524,-1.18514270861314,11.394863359753));
#60103=CARTESIAN_POINT('Ctrl Pts',(1.92340308449501,-1.06847604194589,11.337959254602));
#60104=CARTESIAN_POINT('Ctrl Pts',(1.89843614294196,-0.79477268400099,11.220650108181));
#60105=CARTESIAN_POINT('Ctrl Pts',(1.89156991148624,-0.636309800095305,
11.1592104192819));
#60106=CARTESIAN_POINT('Ctrl Pts',(1.8883872827842,-0.319434907277212,11.0804848377892));
#60107=CARTESIAN_POINT('Ctrl Pts',(1.89152698230331,-0.158333333333359,
11.0526443347744));
#60108=CARTESIAN_POINT('Ctrl Pts',(1.91208041730841,0.158333333333361,11.0426727723083));
#60109=CARTESIAN_POINT('Ctrl Pts',(1.92853344745413,0.31943490727722,11.0609832641629));
#60110=CARTESIAN_POINT('Ctrl Pts',(1.97553883097018,0.636309800095313,11.1184980826711));
#60111=CARTESIAN_POINT('Ctrl Pts',(2.00639081156863,0.794772684000975,11.1684223167876));
#60112=CARTESIAN_POINT('Ctrl Pts',(2.07320017460509,1.06847604194542,11.2654468820485));
#60113=CARTESIAN_POINT('Ctrl Pts',(2.10619712120972,1.18514270861223,11.3134355555938));
#60114=CARTESIAN_POINT('Ctrl Pts',(2.14327171669138,1.3000000000006,11.3674145634973));
#60115=CARTESIAN_POINT('Ctrl Pts',(1.93919233834441,-1.30000000000188,11.4412683292781));
#60116=CARTESIAN_POINT('Ctrl Pts',(1.9180392072829,-1.1851427086131,11.3744922842501));
#60117=CARTESIAN_POINT('Ctrl Pts',(1.9016915027463,-1.06847604194585,11.3147015044614));
#60118=CARTESIAN_POINT('Ctrl Pts',(1.87502653151455,-0.794772684000963,
11.1927102021457));
#60119=CARTESIAN_POINT('Ctrl Pts',(1.87077154762912,-0.636309800095285,
11.1307075350712));
#60120=CARTESIAN_POINT('Ctrl Pts',(1.86832967967525,-0.319434907277203,
11.0513547758013));
#60121=CARTESIAN_POINT('Ctrl Pts',(1.87173814123926,-0.158333333333354,
11.0250975637534));
#60122=CARTESIAN_POINT('Ctrl Pts',(1.89154572095382,0.158333333333356,11.0155265525274));
#60123=CARTESIAN_POINT('Ctrl Pts',(1.9065535778102,0.319434907277211,11.032871367099));
#60124=CARTESIAN_POINT('Ctrl Pts',(1.95217595853164,0.636309800095294,11.0913871168503));
#60125=CARTESIAN_POINT('Ctrl Pts',(1.98078372227384,0.794772684000952,11.1417282263698));
#60126=CARTESIAN_POINT('Ctrl Pts',(2.04993983042539,1.06847604194539,11.2431289591996));
#60127=CARTESIAN_POINT('Ctrl Pts',(2.08504196414533,1.18514270861219,11.2937958862347));
#60128=CARTESIAN_POINT('Ctrl Pts',(2.12531111485276,1.30000000000056,11.3512371203305));
#60129=CARTESIAN_POINT('Ctrl Pts',(1.92704926329494,-1.30000000000182,11.4283111506925));
#60130=CARTESIAN_POINT('Ctrl Pts',(1.90399556245151,-1.18514270861305,11.3587746878215));
#60131=CARTESIAN_POINT('Ctrl Pts',(1.8864011954364,-1.0684760419458,11.296885098931));
#60132=CARTESIAN_POINT('Ctrl Pts',(1.85836684116995,-0.794772684000927,
11.1715735762711));
#60133=CARTESIAN_POINT('Ctrl Pts',(1.85548565900223,-0.636309800095255,
11.1095352181817));
#60134=CARTESIAN_POINT('Ctrl Pts',(1.85390906783529,-0.319434907277188,
11.0295476705844));
#60135=CARTESIAN_POINT('Ctrl Pts',(1.85864937632493,-0.158333333333347,
11.0037448778369));
#60136=CARTESIAN_POINT('Ctrl Pts',(1.87802031518014,0.158333333333349,10.9943852668516));
#60137=CARTESIAN_POINT('Ctrl Pts',(1.89121780193844,0.319434907277195,11.011465514906));
#60138=CARTESIAN_POINT('Ctrl Pts',(1.93517081113783,0.636309800095263,11.0710905506731));
#60139=CARTESIAN_POINT('Ctrl Pts',(1.9619143550451,0.794772684000913,11.1218360551467));
#60140=CARTESIAN_POINT('Ctrl Pts',(2.03209926506429,1.06847604194534,11.2268812699618));
#60141=CARTESIAN_POINT('Ctrl Pts',(2.06840033622108,1.18514270861214,11.2797402876574));
#60142=CARTESIAN_POINT('Ctrl Pts',(2.11062203159456,1.3000000000005,11.3399881418638));
#60143=CARTESIAN_POINT('Ctrl Pts',(1.914880110088,-1.30000000000179,11.4152490614093));
#60144=CARTESIAN_POINT('Ctrl Pts',(1.88981935390603,-1.18514270861302,11.3428017862381));
#60145=CARTESIAN_POINT('Ctrl Pts',(1.87101009618621,-1.06847604194578,11.278635514902));
#60146=CARTESIAN_POINT('Ctrl Pts',(1.84199916012994,-0.794772684000909,
11.1495293671655));
#60147=CARTESIAN_POINT('Ctrl Pts',(1.84221824671498,-0.636309800095243,
11.0864611756966));
#60148=CARTESIAN_POINT('Ctrl Pts',(1.84038936278642,-0.319434907277182,
11.0064566878396));
#60149=CARTESIAN_POINT('Ctrl Pts',(1.84277700745507,-0.158333333333344,
10.983313889559));
#60150=CARTESIAN_POINT('Ctrl Pts',(1.86114349767242,0.158333333333346,10.9744875571855));
#60151=CARTESIAN_POINT('Ctrl Pts',(1.87507451244635,0.31943490727719,10.9897506965998));
#60152=CARTESIAN_POINT('Ctrl Pts',(1.91848589835599,0.636309800095253,11.0498482751571));
#60153=CARTESIAN_POINT('Ctrl Pts',(1.9430051609863,0.794772684000899,11.1012117979008));
#60154=CARTESIAN_POINT('Ctrl Pts',(2.01469293575375,1.06847604194532,11.2098347414939));
#60155=CARTESIAN_POINT('Ctrl Pts',(2.05246100102385,1.18514270861212,11.2648637130279));
#60156=CARTESIAN_POINT('Ctrl Pts',(2.09696615016107,1.30000000000047,11.3279028086911));
#60157=CARTESIAN_POINT('Ctrl Pts',(1.90480129625303,-1.30000000000176,11.4044692218274));
#60158=CARTESIAN_POINT('Ctrl Pts',(1.87895670415632,-1.18514270861299,11.3293601806111));
#60159=CARTESIAN_POINT('Ctrl Pts',(1.85940829677877,-1.06847604194575,11.263351254962));
#60160=CARTESIAN_POINT('Ctrl Pts',(1.8287930113399,-0.794772684000891,11.1318805191049));
#60161=CARTESIAN_POINT('Ctrl Pts',(1.82780080485016,-0.636309800095226,
11.0701491495695));
#60162=CARTESIAN_POINT('Ctrl Pts',(1.82522869434448,-0.319434907277173,
10.9905363761722));
#60163=CARTESIAN_POINT('Ctrl Pts',(1.82789637381727,-0.15833333333334,10.9683131199583));
#60164=CARTESIAN_POINT('Ctrl Pts',(1.84678133526567,0.158333333333342,10.9591666172288));
#60165=CARTESIAN_POINT('Ctrl Pts',(1.86174136838708,0.319434907277182,10.9727236463819));
#60166=CARTESIAN_POINT('Ctrl Pts',(1.9053417109919,0.636309800095236,11.0327273653333));
#60167=CARTESIAN_POINT('Ctrl Pts',(1.92819293348889,0.794772684000877,11.0844005483245));
#60168=CARTESIAN_POINT('Ctrl Pts',(2.00107046142142,1.06847604194529,11.1956723375267));
#60169=CARTESIAN_POINT('Ctrl Pts',(2.03992079422669,1.18514270861209,11.2523804603006));
#60170=CARTESIAN_POINT('Ctrl Pts',(2.08607547837377,1.30000000000044,11.3176312713287));
#60171=CARTESIAN_POINT('Ctrl Pts',(1.89327770970022,-1.30000000000175,11.3910324012902));
#60172=CARTESIAN_POINT('Ctrl Pts',(1.86630585421885,-1.18514270861298,11.3123850522012));
#60173=CARTESIAN_POINT('Ctrl Pts',(1.8455645163665,-1.06847604194574,11.2439803084536));
#60174=CARTESIAN_POINT('Ctrl Pts',(1.81204161877102,-0.79477268400088,11.10961413344));
#60175=CARTESIAN_POINT('Ctrl Pts',(1.80841575954142,-0.636309800095219,
11.050011281481));
#60176=CARTESIAN_POINT('Ctrl Pts',(1.8038742456901,-0.31943490727717,10.9713236115184));
#60177=CARTESIAN_POINT('Ctrl Pts',(1.80677796494244,-0.158333333333338,
10.9504155263368));
#60178=CARTESIAN_POINT('Ctrl Pts',(1.82555990331626,0.15833333333334,10.9413025549763));
#60179=CARTESIAN_POINT('Ctrl Pts',(1.84045534302504,0.319434907277178,10.9533997001063));
#60180=CARTESIAN_POINT('Ctrl Pts',(1.88525616390058,0.636309800095228,11.012909687534));
#60181=CARTESIAN_POINT('Ctrl Pts',(1.90913975376704,0.794772684000867,11.0633947089013));
#60182=CARTESIAN_POINT('Ctrl Pts',(1.98480688961782,1.06847604194528,11.1776920503212));
#60183=CARTESIAN_POINT('Ctrl Pts',(2.02516002756491,1.18514270861207,11.2366557310892));
#60184=CARTESIAN_POINT('Ctrl Pts',(2.073112804093,1.30000000000043,11.3051080086584));
#60185=CARTESIAN_POINT('Ctrl Pts',(1.88533826855979,-1.3000000000017,11.3819390151657));
#60186=CARTESIAN_POINT('Ctrl Pts',(1.85877864422648,-1.18514270861294,11.3001911079613));
#60187=CARTESIAN_POINT('Ctrl Pts',(1.837718248409,-1.0684760419457,11.2299700072838));
#60188=CARTESIAN_POINT('Ctrl Pts',(1.80176883894143,-0.794772684000851,
11.0943744460428));
#60189=CARTESIAN_POINT('Ctrl Pts',(1.79303694377367,-0.636309800095197,
11.0389207988312));
#60190=CARTESIAN_POINT('Ctrl Pts',(1.78572104870416,-0.319434907277159,
10.9623346432985));
#60191=CARTESIAN_POINT('Ctrl Pts',(1.78936170987159,-0.158333333333332,
10.9422136296668));
#60192=CARTESIAN_POINT('Ctrl Pts',(1.8080248988652,0.158333333333334,10.9332122433578));
#60193=CARTESIAN_POINT('Ctrl Pts',(1.82221963518582,0.319434907277167,10.9446174247407));
#60194=CARTESIAN_POINT('Ctrl Pts',(1.869237254135,0.636309800095206,11.0022867514235));
#60195=CARTESIAN_POINT('Ctrl Pts',(1.89712646388558,0.79477268400084,11.0489532910959));
#60196=CARTESIAN_POINT('Ctrl Pts',(1.97527792161974,1.06847604194524,11.1644588769458));
#60197=CARTESIAN_POINT('Ctrl Pts',(2.0162566695385,1.18514270861203,11.2251351015703));
#60198=CARTESIAN_POINT('Ctrl Pts',(2.06438529511981,1.30000000000038,11.2964894626088));
#60199=CARTESIAN_POINT('Ctrl Pts',(1.87799128879424,-1.3000000000017,11.3774649241137));
#60200=CARTESIAN_POINT('Ctrl Pts',(1.85162982048174,-1.18514270861294,11.2958715822796));
#60201=CARTESIAN_POINT('Ctrl Pts',(1.83046672246868,-1.0684760419457,11.2259796900101));
#60202=CARTESIAN_POINT('Ctrl Pts',(1.79358500771746,-0.794772684000851,
11.0915481264036));
#60203=CARTESIAN_POINT('Ctrl Pts',(1.78288365918825,-0.636309800095197,
11.0377389598563));
#60204=CARTESIAN_POINT('Ctrl Pts',(1.77431562872862,-0.319434907277159,
10.9622827219367));
#60205=CARTESIAN_POINT('Ctrl Pts',(1.77794490963746,-0.158333333333332,
10.9421106139582));
#60206=CARTESIAN_POINT('Ctrl Pts',(1.79644754730033,0.158333333333334,10.9332833264162));
#60207=CARTESIAN_POINT('Ctrl Pts',(1.8102831109525,0.319434907277167,10.9450989989837));
#60208=CARTESIAN_POINT('Ctrl Pts',(1.85865359192218,0.636309800095206,11.0016155958775));
#60209=CARTESIAN_POINT('Ctrl Pts',(1.8893645694356,0.79477268400084,11.0459682230072));
#60210=CARTESIAN_POINT('Ctrl Pts',(1.96832072991246,1.06847604194524,11.1603953244879));
#60211=CARTESIAN_POINT('Ctrl Pts',(2.00914338193007,1.18514270861203,11.2209304357419));
#60212=CARTESIAN_POINT('Ctrl Pts',(2.05661148970894,1.30000000000038,11.292469405961));
#60213=CARTESIAN_POINT('Ctrl Pts',(1.87799128879385,-1.3,11.3774649241125));
#60214=CARTESIAN_POINT('Ctrl Pts',(1.85162982048153,-1.18514270861178,11.2958715822789));
#60215=CARTESIAN_POINT('Ctrl Pts',(1.8304667224686,-1.06847604194512,11.2259796900098));
#60216=CARTESIAN_POINT('Ctrl Pts',(1.79358500771746,-0.794772684000851,
11.0915481264036));
#60217=CARTESIAN_POINT('Ctrl Pts',(1.78288365918825,-0.636309800095197,
11.0377389598563));
#60218=CARTESIAN_POINT('Ctrl Pts',(1.77431562872862,-0.319434907277159,
10.9622827219367));
#60219=CARTESIAN_POINT('Ctrl Pts',(1.77794490963746,-0.158333333333332,
10.9421106139582));
#60220=CARTESIAN_POINT('Ctrl Pts',(1.79644754730033,0.158333333333334,10.9332833264162));
#60221=CARTESIAN_POINT('Ctrl Pts',(1.8102831109525,0.319434907277167,10.9450989989837));
#60222=CARTESIAN_POINT('Ctrl Pts',(1.85865359192218,0.636309800095206,11.0016155958775));
#60223=CARTESIAN_POINT('Ctrl Pts',(1.8893645694356,0.79477268400084,11.0459682230072));
#60224=CARTESIAN_POINT('Ctrl Pts',(1.96832072991242,1.06847604194511,11.1603953244878));
#60225=CARTESIAN_POINT('Ctrl Pts',(2.00914338192998,1.18514270861177,11.2209304357418));
#60226=CARTESIAN_POINT('Ctrl Pts',(2.05661148970878,1.3,11.2924694059607));
#60227=CARTESIAN_POINT('',(2.2068264837238,-1.2,11.6308483240498));
#60228=CARTESIAN_POINT('Ctrl Pts',(2.2068264837238,-1.2,11.6308483240498));
#60229=CARTESIAN_POINT('Ctrl Pts',(2.18724117329495,-1.21681996775978,11.6218122533617));
#60230=CARTESIAN_POINT('Ctrl Pts',(2.16689868522774,-1.23318534441601,11.6135926611327));
#60231=CARTESIAN_POINT('Ctrl Pts',(2.12884789480307,-1.2658888355048,11.5957608209235));
#60232=CARTESIAN_POINT('Ctrl Pts',(2.11003562568207,-1.28160650336713,11.5873866307135));
#60233=CARTESIAN_POINT('Ctrl Pts',(2.09094241353359,-1.2984242831365,11.5778701597891));
#60234=CARTESIAN_POINT('Ctrl Pts',(2.09005049051658,-1.29921222705947,11.5774229103209));
#60235=CARTESIAN_POINT('Ctrl Pts',(2.08916175672605,-1.30000000000272,11.5769742007701));
#60236=CARTESIAN_POINT('',(2.34584242549889,-0.653834841417007,11.5588442636176));
#60237=CARTESIAN_POINT('Ctrl Pts',(2.34584242550886,-0.653834841416324,
11.5588442636418));
#60238=CARTESIAN_POINT('Ctrl Pts',(2.33152214904514,-0.717927032198887,
11.5665511487796));
#60239=CARTESIAN_POINT('Ctrl Pts',(2.31982760984721,-0.763778390313212,
11.5727769806235));
#60240=CARTESIAN_POINT('Ctrl Pts',(2.2739524493678,-0.949540773186723,11.5969165862991));
#60241=CARTESIAN_POINT('Ctrl Pts',(2.24889659026364,-1.04883931167899,11.6098949041864));
#60242=CARTESIAN_POINT('Ctrl Pts',(2.2068264837238,-1.2,11.6308483240498));
#60243=CARTESIAN_POINT('',(2.46774460503139,0.653834841531101,11.491006474516));
#60244=CARTESIAN_POINT('Ctrl Pts',(2.46774460503136,0.6538348415311,11.491006474516));
#60245=CARTESIAN_POINT('Ctrl Pts',(2.43368778115467,0.575795030619156,11.4669914411289));
#60246=CARTESIAN_POINT('Ctrl Pts',(2.40474750894542,0.493918313629019,11.447426688817));
#60247=CARTESIAN_POINT('Ctrl Pts',(2.3613754176558,0.338197324327257,11.4211796538803));
#60248=CARTESIAN_POINT('Ctrl Pts',(2.34543349869105,0.265711097259163,11.4130062283616));
#60249=CARTESIAN_POINT('Ctrl Pts',(2.3220968049692,0.129740576115995,11.4058460663461));
#60250=CARTESIAN_POINT('Ctrl Pts',(2.3138153758775,0.0666412396508463,11.4056782828097));
#60251=CARTESIAN_POINT('Ctrl Pts',(2.30198027918302,-0.0595498475940219,
11.4118386452963));
#60252=CARTESIAN_POINT('Ctrl Pts',(2.29832871714705,-0.122796020472284,
11.4181987058642));
#60253=CARTESIAN_POINT('Ctrl Pts',(2.29622270118133,-0.260148735050006,
11.4388365912281));
#60254=CARTESIAN_POINT('Ctrl Pts',(2.29883477760314,-0.333948670529117,
11.4543476372232));
#60255=CARTESIAN_POINT('Ctrl Pts',(2.31349450820435,-0.491142050749671,
11.4967086246876));
#60256=CARTESIAN_POINT('Ctrl Pts',(2.32698040039238,-0.574253995386567,
11.5252254122324));
#60257=CARTESIAN_POINT('Ctrl Pts',(2.34584242545894,-0.653834841428697,
11.5588442636123));
#60258=CARTESIAN_POINT('',(2.40489628334222,1.2,11.5265429463218));
#60259=CARTESIAN_POINT('Ctrl Pts',(2.40489628334222,1.2,11.5265429463218));
#60260=CARTESIAN_POINT('Ctrl Pts',(2.41582048848703,1.1340365096965,11.5204707587399));
#60261=CARTESIAN_POINT('Ctrl Pts',(2.43005844632245,1.038218713922,11.5125009027098));
#60262=CARTESIAN_POINT('Ctrl Pts',(2.45771077440481,0.795149709173985,11.496781434669));
#60263=CARTESIAN_POINT('Ctrl Pts',(2.46206175224414,0.741496517834653,11.4942746656479));
#60264=CARTESIAN_POINT('Ctrl Pts',(2.46774460503137,0.653834841531098,11.491006474516));
#60265=CARTESIAN_POINT('Ctrl Pts',(2.29116136298904,1.3000000000003,11.4747022830536));
#60266=CARTESIAN_POINT('Ctrl Pts',(2.30969599627212,1.28317246189965,11.4838602831997));
#60267=CARTESIAN_POINT('Ctrl Pts',(2.32883998949747,1.26664026084675,11.492301893308));
#60268=CARTESIAN_POINT('Ctrl Pts',(2.36390070845054,1.23528691103208,11.5088851378804));
#60269=CARTESIAN_POINT('Ctrl Pts',(2.38633959798998,1.21551346690462,11.5191086603475));
#60270=CARTESIAN_POINT('Ctrl Pts',(2.40489628334222,1.2,11.5265429463218));
#60271=CARTESIAN_POINT('Ctrl Pts',(1.87799128879384,-1.3,11.3774649241125));
#60272=CARTESIAN_POINT('Ctrl Pts',(1.85162982048153,-1.18514270861178,11.2958715822789));
#60273=CARTESIAN_POINT('Ctrl Pts',(1.8304667224686,-1.06847604194512,11.2259796900098));
#60274=CARTESIAN_POINT('Ctrl Pts',(1.79358500771746,-0.794772684000851,
11.0915481264036));
#60275=CARTESIAN_POINT('Ctrl Pts',(1.78288365918825,-0.636309800095197,
11.0377389598563));
#60276=CARTESIAN_POINT('Ctrl Pts',(1.77431562872862,-0.319434907277159,
10.9622827219367));
#60277=CARTESIAN_POINT('Ctrl Pts',(1.77794490963746,-0.158333333333332,
10.9421106139582));
#60278=CARTESIAN_POINT('Ctrl Pts',(1.79644754730034,0.158333333333334,10.9332833264162));
#60279=CARTESIAN_POINT('Ctrl Pts',(1.8102831109525,0.319434907277167,10.9450989989837));
#60280=CARTESIAN_POINT('Ctrl Pts',(1.85865359192218,0.636309800095206,11.0016155958775));
#60281=CARTESIAN_POINT('Ctrl Pts',(1.8893645694356,0.79477268400084,11.0459682230072));
#60282=CARTESIAN_POINT('Ctrl Pts',(1.96832072991242,1.06847604194511,11.1603953244878));
#60283=CARTESIAN_POINT('Ctrl Pts',(2.00914338192998,1.18514270861178,11.2209304357418));
#60284=CARTESIAN_POINT('Ctrl Pts',(2.05661148970878,1.3,11.2924694059607));
#60285=CARTESIAN_POINT('Ctrl Pts',(1.80704611563284,-1.3,11.407228856645));
#60286=CARTESIAN_POINT('Ctrl Pts',(1.78233798615881,-1.18514270861178,11.3251184310253));
#60287=CARTESIAN_POINT('Ctrl Pts',(1.76233903122006,-1.06847604194512,11.2549094900764));
#60288=CARTESIAN_POINT('Ctrl Pts',(1.72701657977795,-0.794772684000851,
11.1202076017071));
#60289=CARTESIAN_POINT('Ctrl Pts',(1.71574542397769,-0.636309800095197,
11.0668346892391));
#60290=CARTESIAN_POINT('Ctrl Pts',(1.70682212124656,-0.319434907277159,
10.9919427781636));
#60291=CARTESIAN_POINT('Ctrl Pts',(1.70940065624172,-0.158333333333332,
10.9724320209495));
#60292=CARTESIAN_POINT('Ctrl Pts',(1.72804929275646,0.158333333333334,10.9639326521977));
#60293=CARTESIAN_POINT('Ctrl Pts',(1.74307942205737,0.319434907277167,10.9754099984146));
#60294=CARTESIAN_POINT('Ctrl Pts',(1.79210700315155,0.636309800095206,11.0320401849215));
#60295=CARTESIAN_POINT('Ctrl Pts',(1.82352345611137,0.79477268400084,11.0762612736829));
#60296=CARTESIAN_POINT('Ctrl Pts',(1.90123537533585,1.06847604194511,11.1916662510505));
#60297=CARTESIAN_POINT('Ctrl Pts',(1.9410434505065,1.18514270861178,11.2528543422308));
#60298=CARTESIAN_POINT('Ctrl Pts',(1.98702099052593,1.3,11.3252759860648));
#60299=CARTESIAN_POINT('Ctrl Pts',(1.73610094247183,-1.3,11.4369927891775));
#60300=CARTESIAN_POINT('Ctrl Pts',(1.71304615183608,-1.18514270861178,11.3543652797717));
#60301=CARTESIAN_POINT('Ctrl Pts',(1.69421133997152,-1.06847604194512,11.283839290143));
#60302=CARTESIAN_POINT('Ctrl Pts',(1.66044815183843,-0.794772684000851,
11.1488670770106));
#60303=CARTESIAN_POINT('Ctrl Pts',(1.64860718876712,-0.636309800095197,
11.0959304186219));
#60304=CARTESIAN_POINT('Ctrl Pts',(1.63932861376449,-0.319434907277159,
11.0216028343905));
#60305=CARTESIAN_POINT('Ctrl Pts',(1.64085640284598,-0.158333333333332,
11.0027534279408));
#60306=CARTESIAN_POINT('Ctrl Pts',(1.65965103821258,0.158333333333334,10.9945819779792));
#60307=CARTESIAN_POINT('Ctrl Pts',(1.67587573316224,0.319434907277167,11.0057209978454));
#60308=CARTESIAN_POINT('Ctrl Pts',(1.72556041438091,0.636309800095206,11.0624647739656));
#60309=CARTESIAN_POINT('Ctrl Pts',(1.75768234278715,0.79477268400084,11.1065543243585));
#60310=CARTESIAN_POINT('Ctrl Pts',(1.83415002075929,1.06847604194511,11.2229371776131));
#60311=CARTESIAN_POINT('Ctrl Pts',(1.87294351908302,1.18514270861178,11.2847782487198));
#60312=CARTESIAN_POINT('Ctrl Pts',(1.91743049134307,1.3,11.3580825661689));
#60313=CARTESIAN_POINT('Ctrl Pts',(1.66515576931082,-1.3,11.46675672171));
#60314=CARTESIAN_POINT('Ctrl Pts',(1.64375431751336,-1.18514270861178,11.3836121285181));
#60315=CARTESIAN_POINT('Ctrl Pts',(1.62608364872297,-1.06847604194512,11.3127690902096));
#60316=CARTESIAN_POINT('Ctrl Pts',(1.59387972389892,-0.794772684000851,
11.1775265523141));
#60317=CARTESIAN_POINT('Ctrl Pts',(1.58146895355656,-0.636309800095197,
11.1250261480047));
#60318=CARTESIAN_POINT('Ctrl Pts',(1.57183510628243,-0.319434907277159,
11.0512628906174));
#60319=CARTESIAN_POINT('Ctrl Pts',(1.57231214945024,-0.158333333333332,
11.0330748349321));
#60320=CARTESIAN_POINT('Ctrl Pts',(1.59125278366871,0.158333333333334,11.0252313037607));
#60321=CARTESIAN_POINT('Ctrl Pts',(1.60867204426711,0.319434907277167,11.0360319972763));
#60322=CARTESIAN_POINT('Ctrl Pts',(1.65901382561028,0.636309800095206,11.0928893630096));
#60323=CARTESIAN_POINT('Ctrl Pts',(1.69184122946292,0.79477268400084,11.1368473750342));
#60324=CARTESIAN_POINT('Ctrl Pts',(1.76706466618273,1.06847604194511,11.2542081041758));
#60325=CARTESIAN_POINT('Ctrl Pts',(1.80484358765954,1.18514270861178,11.3167021552088));
#60326=CARTESIAN_POINT('Ctrl Pts',(1.84783999216022,1.3,11.390889146273));
#60327=CARTESIAN_POINT('Ctrl Pts',(1.66515576931082,-1.3,11.46675672171));
#60328=CARTESIAN_POINT('Ctrl Pts',(1.64375431751336,-1.18514270861178,11.3836121285181));
#60329=CARTESIAN_POINT('Ctrl Pts',(1.62608364872297,-1.06847604194512,11.3127690902096));
#60330=CARTESIAN_POINT('Ctrl Pts',(1.59387972389892,-0.794772684000851,
11.1775265523141));
#60331=CARTESIAN_POINT('Ctrl Pts',(1.58146895355656,-0.636309800095197,
11.1250261480047));
#60332=CARTESIAN_POINT('Ctrl Pts',(1.57183510628243,-0.319434907277159,
11.0512628906174));
#60333=CARTESIAN_POINT('Ctrl Pts',(1.57231214945024,-0.158333333333332,
11.0330748349321));
#60334=CARTESIAN_POINT('Ctrl Pts',(1.59125278366871,0.158333333333334,11.0252313037607));
#60335=CARTESIAN_POINT('Ctrl Pts',(1.6086720442671,0.319434907277167,11.0360319972763));
#60336=CARTESIAN_POINT('Ctrl Pts',(1.65901382561028,0.636309800095206,11.0928893630096));
#60337=CARTESIAN_POINT('Ctrl Pts',(1.69184122946292,0.79477268400084,11.1368473750342));
#60338=CARTESIAN_POINT('Ctrl Pts',(1.76706466618273,1.06847604194511,11.2542081041758));
#60339=CARTESIAN_POINT('Ctrl Pts',(1.80484358765954,1.18514270861178,11.3167021552088));
#60340=CARTESIAN_POINT('Ctrl Pts',(1.84783999216022,1.3,11.390889146273));
#60341=CARTESIAN_POINT('Ctrl Pts',(1.66515576931083,-1.30000000000005,11.46675672171));
#60342=CARTESIAN_POINT('Ctrl Pts',(1.64375431751336,-1.18514270861182,11.3836121285181));
#60343=CARTESIAN_POINT('Ctrl Pts',(1.62608364872297,-1.06847604194513,11.3127690902096));
#60344=CARTESIAN_POINT('Ctrl Pts',(1.59387972389892,-0.794772684000851,
11.1775265523141));
#60345=CARTESIAN_POINT('Ctrl Pts',(1.58146895355655,-0.636309800095197,
11.1250261480047));
#60346=CARTESIAN_POINT('Ctrl Pts',(1.57183510628243,-0.319434907277159,
11.0512628906174));
#60347=CARTESIAN_POINT('Ctrl Pts',(1.57231214945024,-0.158333333333332,
11.0330748349321));
#60348=CARTESIAN_POINT('Ctrl Pts',(1.5912527836687,0.158333333333334,11.0252313037607));
#60349=CARTESIAN_POINT('Ctrl Pts',(1.6086720442671,0.319434907277167,11.0360319972763));
#60350=CARTESIAN_POINT('Ctrl Pts',(1.65901382561028,0.636309800095206,11.0928893630096));
#60351=CARTESIAN_POINT('Ctrl Pts',(1.69184122946292,0.79477268400084,11.1368473750342));
#60352=CARTESIAN_POINT('Ctrl Pts',(1.76706466618285,1.06847604194556,11.254208104176));
#60353=CARTESIAN_POINT('Ctrl Pts',(1.80484358765983,1.18514270861267,11.3167021552093));
#60354=CARTESIAN_POINT('Ctrl Pts',(1.84783999216071,1.30000000000132,11.3908891462739));
#60355=CARTESIAN_POINT('Ctrl Pts',(1.66294156245547,-1.30000000000005,11.4752237278628));
#60356=CARTESIAN_POINT('Ctrl Pts',(1.64211927469555,-1.18514270861182,11.391711801944));
#60357=CARTESIAN_POINT('Ctrl Pts',(1.62444818678087,-1.06847604194513,11.3206583385042));
#60358=CARTESIAN_POINT('Ctrl Pts',(1.59090434064678,-0.794772684000851,
11.1852921643951));
#60359=CARTESIAN_POINT('Ctrl Pts',(1.57488586700129,-0.636309800095197,
11.1333404325032));
#60360=CARTESIAN_POINT('Ctrl Pts',(1.56349013315575,-0.319434907277159,
11.0598112207211));
#60361=CARTESIAN_POINT('Ctrl Pts',(1.56451256412487,-0.158333333333332,
11.041630919885));
#60362=CARTESIAN_POINT('Ctrl Pts',(1.5836900087521,0.158333333333334,11.0337845706398));
#60363=CARTESIAN_POINT('Ctrl Pts',(1.60107891375656,0.319434907277167,11.044542618244));
#60364=CARTESIAN_POINT('Ctrl Pts',(1.65309822965178,0.636309800095206,11.1012255285261));
#60365=CARTESIAN_POINT('Ctrl Pts',(1.68846554231891,0.79477268400084,11.1448203238114));
#60366=CARTESIAN_POINT('Ctrl Pts',(1.7651778318562,1.06847604194556,11.2622670815464));
#60367=CARTESIAN_POINT('Ctrl Pts',(1.80327012403914,1.18514270861267,11.3249050933935));
#60368=CARTESIAN_POINT('Ctrl Pts',(1.84624880073474,1.30000000000132,11.3993427674954));
#60369=CARTESIAN_POINT('Ctrl Pts',(1.66352992364858,-1.30000000000005,11.487474413773));
#60370=CARTESIAN_POINT('Ctrl Pts',(1.64473762368632,-1.18514270861181,11.4060420060404));
#60371=CARTESIAN_POINT('Ctrl Pts',(1.62791338132392,-1.06847604194513,11.3366047299185));
#60372=CARTESIAN_POINT('Ctrl Pts',(1.59359262255284,-0.794772684000851,
11.2039018848358));
#60373=CARTESIAN_POINT('Ctrl Pts',(1.57205079459115,-0.636309800095196,
11.1523732203483));
#60374=CARTESIAN_POINT('Ctrl Pts',(1.55780491322402,-0.319434907277158,
11.0792600320647));
#60375=CARTESIAN_POINT('Ctrl Pts',(1.55879634907134,-0.158333333333332,
11.0600902727381));
#60376=CARTESIAN_POINT('Ctrl Pts',(1.57813469347016,0.158333333333334,11.0522311225344));
#60377=CARTESIAN_POINT('Ctrl Pts',(1.59559909903037,0.319434907277167,11.0640703860129));
#60378=CARTESIAN_POINT('Ctrl Pts',(1.65103339058184,0.636309800095205,11.1200982203511));
#60379=CARTESIAN_POINT('Ctrl Pts',(1.69291229251351,0.794772684000838,11.1626715245407));
#60380=CARTESIAN_POINT('Ctrl Pts',(1.77033498791918,1.06847604194556,11.2774862822592));
#60381=CARTESIAN_POINT('Ctrl Pts',(1.80728926966501,1.18514270861267,11.3386684002332));
#60382=CARTESIAN_POINT('Ctrl Pts',(1.8476844171091,1.30000000000132,11.4113335818709));
#60383=CARTESIAN_POINT('Ctrl Pts',(1.66410716288398,-1.30000000000005,11.5054993221241));
#60384=CARTESIAN_POINT('Ctrl Pts',(1.64649300104017,-1.18514270861181,11.4275420236061));
#60385=CARTESIAN_POINT('Ctrl Pts',(1.63034498930106,-1.06847604194513,11.3607271826284));
#60386=CARTESIAN_POINT('Ctrl Pts',(1.59642695182921,-0.794772684000851,
11.2321128396658));
#60387=CARTESIAN_POINT('Ctrl Pts',(1.57333448035651,-0.636309800095196,
11.1805501678138));
#60388=CARTESIAN_POINT('Ctrl Pts',(1.55795451949656,-0.319434907277159,
11.1079876496958));
#60389=CARTESIAN_POINT('Ctrl Pts',(1.55794686674891,-0.158333333333332,
11.0877806504958));
#60390=CARTESIAN_POINT('Ctrl Pts',(1.57736811047979,0.158333333333334,11.0798704180037));
#60391=CARTESIAN_POINT('Ctrl Pts',(1.59558105644426,0.319434907277167,11.0927852508965));
#60392=CARTESIAN_POINT('Ctrl Pts',(1.65299749605388,0.636309800095206,11.1479762386669));
#60393=CARTESIAN_POINT('Ctrl Pts',(1.69824705110065,0.79477268400084,11.1900093036634));
#60394=CARTESIAN_POINT('Ctrl Pts',(1.77547688951519,1.06847604194556,11.3007258083824));
#60395=CARTESIAN_POINT('Ctrl Pts',(1.81145476612715,1.18514270861267,11.3594189182278));
#60396=CARTESIAN_POINT('Ctrl Pts',(1.8499805839489,1.30000000000132,11.4288800654763));
#60397=CARTESIAN_POINT('Ctrl Pts',(1.66462615833063,-1.30000000000005,11.5204313880076));
#60398=CARTESIAN_POINT('Ctrl Pts',(1.64753050462642,-1.18514270861181,11.4451970340025));
#60399=CARTESIAN_POINT('Ctrl Pts',(1.63187981906843,-1.06847604194513,11.3803258984653));
#60400=CARTESIAN_POINT('Ctrl Pts',(1.59906177000319,-0.794772684000852,
11.2544017057635));
#60401=CARTESIAN_POINT('Ctrl Pts',(1.57725211952697,-0.636309800095197,
11.2018237808047));
#60402=CARTESIAN_POINT('Ctrl Pts',(1.56158886062262,-0.319434907277159,
11.1293666304791));
#60403=CARTESIAN_POINT('Ctrl Pts',(1.55954130633869,-0.158333333333332,
11.1088058076973));
#60404=CARTESIAN_POINT('Ctrl Pts',(1.57840295787679,0.158333333333334,11.1010602390785));
#60405=CARTESIAN_POINT('Ctrl Pts',(1.5972639021225,0.319434907277166,11.114757650731));
#60406=CARTESIAN_POINT('Ctrl Pts',(1.65551914847726,0.636309800095205,11.169640744191));
#60407=CARTESIAN_POINT('Ctrl Pts',(1.7025183349984,0.794772684000841,11.2116827099241));
#60408=CARTESIAN_POINT('Ctrl Pts',(1.77903235823731,1.06847604194556,11.3196178795441));
#60409=CARTESIAN_POINT('Ctrl Pts',(1.81412006596867,1.18514270861267,11.3765231624912));
#60410=CARTESIAN_POINT('Ctrl Pts',(1.85117539589519,1.30000000000132,11.443612592849));
#60411=CARTESIAN_POINT('Ctrl Pts',(1.66400832169345,-1.30000000000005,11.5417962198323));
#60412=CARTESIAN_POINT('Ctrl Pts',(1.64758473327318,-1.18514270861181,11.4706865804745));
#60413=CARTESIAN_POINT('Ctrl Pts',(1.63272474774337,-1.06847604194513,11.4087476415573));
#60414=CARTESIAN_POINT('Ctrl Pts',(1.6020074439142,-0.79477268400085,11.2868424544265));
#60415=CARTESIAN_POINT('Ctrl Pts',(1.58263872436519,-0.636309800095197,
11.2327733254491));
#60416=CARTESIAN_POINT('Ctrl Pts',(1.56806146471367,-0.31943490727716,11.1601365165436));
#60417=CARTESIAN_POINT('Ctrl Pts',(1.5641448387696,-0.158333333333333,11.1387133277057));
#60418=CARTESIAN_POINT('Ctrl Pts',(1.58417746458293,0.158333333333335,11.1305334738137));
#60419=CARTESIAN_POINT('Ctrl Pts',(1.60670357041116,0.319434907277167,11.1444007366524));
#60420=CARTESIAN_POINT('Ctrl Pts',(1.66498469223539,0.636309800095207,11.199104875956));
#60421=CARTESIAN_POINT('Ctrl Pts',(1.7088475093535,0.794772684000842,11.2429825724483));
#60422=CARTESIAN_POINT('Ctrl Pts',(1.7829276416763,1.06847604194556,11.3471161791167));
#60423=CARTESIAN_POINT('Ctrl Pts',(1.81703219785438,1.18514270861267,11.4011998294516));
#60424=CARTESIAN_POINT('Ctrl Pts',(1.85317476586736,1.30000000000132,11.4642915503249));
#60425=CARTESIAN_POINT('Ctrl Pts',(1.66297539345541,-1.30000000000005,11.5661771710961));
#60426=CARTESIAN_POINT('Ctrl Pts',(1.64748790809536,-1.18514270861181,11.4995551871625));
#60427=CARTESIAN_POINT('Ctrl Pts',(1.63358502843746,-1.06847604194513,11.4408160710686));
#60428=CARTESIAN_POINT('Ctrl Pts',(1.60512735133741,-0.794772684000852,
11.323327963844));
#60429=CARTESIAN_POINT('Ctrl Pts',(1.58727693515927,-0.636309800095197,
11.2679265316481));
#60430=CARTESIAN_POINT('Ctrl Pts',(1.57496440665297,-0.319434907277159,
11.1947206572407));
#60431=CARTESIAN_POINT('Ctrl Pts',(1.57249846469125,-0.158333333333333,
11.1712285313312));
#60432=CARTESIAN_POINT('Ctrl Pts',(1.59315812681989,0.158333333333335,11.1628098713027));
#60433=CARTESIAN_POINT('Ctrl Pts',(1.61504264595899,0.319434907277168,11.1784122730249));
#60434=CARTESIAN_POINT('Ctrl Pts',(1.67196541936092,0.636309800095208,11.2333925388939));
#60435=CARTESIAN_POINT('Ctrl Pts',(1.71458559513429,0.794772684000841,11.278566366693));
#60436=CARTESIAN_POINT('Ctrl Pts',(1.78651169444565,1.06847604194556,11.3783610653472));
#60437=CARTESIAN_POINT('Ctrl Pts',(1.81958498585978,1.18514270861267,11.4293319290012));
#60438=CARTESIAN_POINT('Ctrl Pts',(1.85459742542072,1.30000000000132,11.4880762290198));
#60439=CARTESIAN_POINT('Ctrl Pts',(1.66253954923371,-1.30000000000004,11.5904501135859));
#60440=CARTESIAN_POINT('Ctrl Pts',(1.64716745471438,-1.18514270861181,11.5285960424193));
#60441=CARTESIAN_POINT('Ctrl Pts',(1.63366347314043,-1.06847604194513,11.4732599425887));
#60442=CARTESIAN_POINT('Ctrl Pts',(1.60678228886089,-0.794772684000851,
11.360480299733));
#60443=CARTESIAN_POINT('Ctrl Pts',(1.59123488997867,-0.636309800095198,
11.303586068394));
#60444=CARTESIAN_POINT('Ctrl Pts',(1.58077906844529,-0.31943490727716,11.2299960490128));
#60445=CARTESIAN_POINT('Ctrl Pts',(1.57850031280611,-0.158333333333333,
11.2048184941379));
#60446=CARTESIAN_POINT('Ctrl Pts',(1.60000105270369,0.158333333333335,11.1960984995114));
#60447=CARTESIAN_POINT('Ctrl Pts',(1.62296696905983,0.319434907277167,11.2129066633604));
#60448=CARTESIAN_POINT('Ctrl Pts',(1.67887545187121,0.636309800095208,11.2680205272578));
#60449=CARTESIAN_POINT('Ctrl Pts',(1.71900525567967,0.794772684000844,11.3148611545452));
#60450=CARTESIAN_POINT('Ctrl Pts',(1.78876603729209,1.06847604194556,11.4102050857618));
#60451=CARTESIAN_POINT('Ctrl Pts',(1.82100896742402,1.18514270861267,11.4579322183308));
#60452=CARTESIAN_POINT('Ctrl Pts',(1.85529797021952,1.30000000000131,11.512115628486));
#60453=CARTESIAN_POINT('Ctrl Pts',(1.66047989040796,-1.30000000000004,11.6120422433131));
#60454=CARTESIAN_POINT('Ctrl Pts',(1.6454766653493,-1.18514270861181,11.554246150656));
#60455=CARTESIAN_POINT('Ctrl Pts',(1.63249668632829,-1.06847604194513,11.5018119048232));
#60456=CARTESIAN_POINT('Ctrl Pts',(1.60718444124979,-0.794772684000848,
11.3930652463123));
#60457=CARTESIAN_POINT('Ctrl Pts',(1.59326532192798,-0.636309800095197,
11.3349913012082));
#60458=CARTESIAN_POINT('Ctrl Pts',(1.58467614588915,-0.31943490727716,11.2610090519529));
#60459=CARTESIAN_POINT('Ctrl Pts',(1.58342008565865,-0.158333333333332,
11.2341227576192));
#60460=CARTESIAN_POINT('Ctrl Pts',(1.60539226152046,0.158333333333335,11.2252470755727));
#60461=CARTESIAN_POINT('Ctrl Pts',(1.62765787597471,0.319434907277167,11.2436246555957));
#60462=CARTESIAN_POINT('Ctrl Pts',(1.6829635831606,0.636309800095207,11.2987802927372));
#60463=CARTESIAN_POINT('Ctrl Pts',(1.72303227090909,0.794772684000842,11.3464031280536));
#60464=CARTESIAN_POINT('Ctrl Pts',(1.79157743098819,1.06847604194556,11.4376927581495));
#60465=CARTESIAN_POINT('Ctrl Pts',(1.82309787132108,1.18514270861267,11.4826159445079));
#60466=CARTESIAN_POINT('Ctrl Pts',(1.85646809203706,1.30000000000131,11.5329464189705));
#60467=CARTESIAN_POINT('Ctrl Pts',(1.65917440129577,-1.30000000000004,11.6304388748568));
#60468=CARTESIAN_POINT('Ctrl Pts',(1.64420105650356,-1.18514270861181,11.5762004678021));
#60469=CARTESIAN_POINT('Ctrl Pts',(1.63143500502946,-1.06847604194513,11.5263218385257));
#60470=CARTESIAN_POINT('Ctrl Pts',(1.60704216141674,-0.794772684000848,
11.4211641855496));
#60471=CARTESIAN_POINT('Ctrl Pts',(1.59424465224217,-0.636309800095196,
11.362178575418));
#60472=CARTESIAN_POINT('Ctrl Pts',(1.58736265267558,-0.319434907277159,
11.2878467698504));
#60473=CARTESIAN_POINT('Ctrl Pts',(1.58756458885484,-0.158333333333332,
11.259339331069));
#60474=CARTESIAN_POINT('Ctrl Pts',(1.61015009976414,0.158333333333334,11.2502671569896));
#60475=CARTESIAN_POINT('Ctrl Pts',(1.63190827410841,0.319434907277167,11.2699434288937));
#60476=CARTESIAN_POINT('Ctrl Pts',(1.68606922874198,0.636309800095207,11.3253049547619));
#60477=CARTESIAN_POINT('Ctrl Pts',(1.72461091140695,0.794772684000842,11.374034284718));
#60478=CARTESIAN_POINT('Ctrl Pts',(1.7920431619667,1.06847604194556,11.4618498796299));
#60479=CARTESIAN_POINT('Ctrl Pts',(1.82324641542261,1.18514270861266,11.5042689079887));
#60480=CARTESIAN_POINT('Ctrl Pts',(1.8564639996782,1.30000000000131,11.5510948475572));
#60481=CARTESIAN_POINT('Ctrl Pts',(1.65825661873328,-1.30000000000005,11.6457250585537));
#60482=CARTESIAN_POINT('Ctrl Pts',(1.64381244552155,-1.18514270861181,11.5943362651268));
#60483=CARTESIAN_POINT('Ctrl Pts',(1.63149135558789,-1.06847604194513,11.5465257061246));
#60484=CARTESIAN_POINT('Ctrl Pts',(1.60793192010925,-0.794772684000851,
11.4443401877041));
#60485=CARTESIAN_POINT('Ctrl Pts',(1.59534912366149,-0.636309800095197,
11.3847350317333));
#60486=CARTESIAN_POINT('Ctrl Pts',(1.58905040871725,-0.319434907277159,
11.3103362650791));
#60487=CARTESIAN_POINT('Ctrl Pts',(1.58958601175429,-0.158333333333333,
11.2807547785508));
#60488=CARTESIAN_POINT('Ctrl Pts',(1.61247567219755,0.158333333333335,11.2715894287578));
#60489=CARTESIAN_POINT('Ctrl Pts',(1.63424089574764,0.319434907277168,11.2922306293025));
#60490=CARTESIAN_POINT('Ctrl Pts',(1.68836361307204,0.636309800095207,11.3475017995811));
#60491=CARTESIAN_POINT('Ctrl Pts',(1.72701439575528,0.794772684000843,11.3967473603989));
#60492=CARTESIAN_POINT('Ctrl Pts',(1.79381277498766,1.06847604194556,11.4815812537823));
#60493=CARTESIAN_POINT('Ctrl Pts',(1.82458463182755,1.18514270861266,11.5219615759282));
#60494=CARTESIAN_POINT('Ctrl Pts',(1.85721380226146,1.30000000000131,11.5660007711799));
#60495=CARTESIAN_POINT('Ctrl Pts',(1.65692536543948,-1.30000000000004,11.6580787419226));
#60496=CARTESIAN_POINT('Ctrl Pts',(1.64220899771378,-1.18514270861181,11.6091207818142));
#60497=CARTESIAN_POINT('Ctrl Pts',(1.62982954970193,-1.06847604194513,11.5630568054575));
#60498=CARTESIAN_POINT('Ctrl Pts',(1.6066293003326,-0.794772684000852,11.463325486413));
#60499=CARTESIAN_POINT('Ctrl Pts',(1.59503084689484,-0.636309800095197,
11.4030703960431));
#60500=CARTESIAN_POINT('Ctrl Pts',(1.58976206576291,-0.319434907277159,
11.3284945702936));
#60501=CARTESIAN_POINT('Ctrl Pts',(1.59087843016237,-0.158333333333333,
11.2979672191158));
#60502=CARTESIAN_POINT('Ctrl Pts',(1.61436971205319,0.158333333333335,11.2886305261183));
#60503=CARTESIAN_POINT('Ctrl Pts',(1.63641500674446,0.319434907277168,11.3099564531826));
#60504=CARTESIAN_POINT('Ctrl Pts',(1.6902052555697,0.636309800095208,11.3652385745838));
#60505=CARTESIAN_POINT('Ctrl Pts',(1.72785782392614,0.794772684000843,11.415205044039));
#60506=CARTESIAN_POINT('Ctrl Pts',(1.79409927768552,1.06847604194556,11.4976721140785));
#60507=CARTESIAN_POINT('Ctrl Pts',(1.82473409501747,1.18514270861266,11.5363655582635));
#60508=CARTESIAN_POINT('Ctrl Pts',(1.85733025883666,1.30000000000131,11.5780555077196));
#60509=CARTESIAN_POINT('Ctrl Pts',(1.65574912520358,-1.30000000000004,11.6703942470278));
#60510=CARTESIAN_POINT('Ctrl Pts',(1.6407031272259,-1.18514270861181,11.6238751238318));
#60511=CARTESIAN_POINT('Ctrl Pts',(1.62825119945876,-1.06847604194513,11.5795576353598));
#60512=CARTESIAN_POINT('Ctrl Pts',(1.60547757644532,-0.794772684000851,
11.4822615879543));
#60513=CARTESIAN_POINT('Ctrl Pts',(1.59514663822623,-0.636309800095197,
11.421295595551));
#60514=CARTESIAN_POINT('Ctrl Pts',(1.59093997819171,-0.319434907277159,
11.3465383751006));
#60515=CARTESIAN_POINT('Ctrl Pts',(1.5926049519623,-0.158333333333333,11.3150659952534));
#60516=CARTESIAN_POINT('Ctrl Pts',(1.61628845463705,0.158333333333335,11.3056729345733));
#60517=CARTESIAN_POINT('Ctrl Pts',(1.63790215909678,0.319434907277169,11.327890922621));
#60518=CARTESIAN_POINT('Ctrl Pts',(1.69117500705595,0.636309800095208,11.3832326962634));
#60519=CARTESIAN_POINT('Ctrl Pts',(1.72848079306108,0.794772684000844,11.4337256827248));
#60520=CARTESIAN_POINT('Ctrl Pts',(1.79407775002516,1.06847604194556,11.5138447056087));
#60521=CARTESIAN_POINT('Ctrl Pts',(1.82441011941276,1.18514270861266,11.5508964676374));
#60522=CARTESIAN_POINT('Ctrl Pts',(1.85668036612498,1.30000000000131,11.5903194353906));
#60523=CARTESIAN_POINT('Ctrl Pts',(1.65199738732143,-1.30000000000004,11.704362262037));
#60524=CARTESIAN_POINT('Ctrl Pts',(1.6378062771533,-1.18514270861181,11.6641808214006));
#60525=CARTESIAN_POINT('Ctrl Pts',(1.62616635359825,-1.06847604194513,11.6244530030084));
#60526=CARTESIAN_POINT('Ctrl Pts',(1.60516955306668,-0.79477268400085,11.5337217531304));
#60527=CARTESIAN_POINT('Ctrl Pts',(1.59592366447477,-0.636309800095196,
11.471274853242));
#60528=CARTESIAN_POINT('Ctrl Pts',(1.59311075487144,-0.319434907277158,
11.3963705904157));
#60529=CARTESIAN_POINT('Ctrl Pts',(1.59515399903155,-0.158333333333332,
11.3626387070737));
#60530=CARTESIAN_POINT('Ctrl Pts',(1.61956472506171,0.158333333333334,11.3530266873265));
#60531=CARTESIAN_POINT('Ctrl Pts',(1.64148739776061,0.319434907277168,11.377265724066));
#60532=CARTESIAN_POINT('Ctrl Pts',(1.69492924291113,0.636309800095207,11.4323482476407));
#60533=CARTESIAN_POINT('Ctrl Pts',(1.73248328685883,0.794772684000842,11.4840051515948));
#60534=CARTESIAN_POINT('Ctrl Pts',(1.79698535281222,1.06847604194556,11.5574998117437));
#60535=CARTESIAN_POINT('Ctrl Pts',(1.82653771960054,1.18514270861266,11.5900247156801));
#60536=CARTESIAN_POINT('Ctrl Pts',(1.85772189886299,1.3000000000013,11.62326140842));
#60537=CARTESIAN_POINT('Ctrl Pts',(1.64649643543192,-1.30000000000004,11.7416097712608));
#60538=CARTESIAN_POINT('Ctrl Pts',(1.63060661304912,-1.1851427086118,11.7088267957282));
#60539=CARTESIAN_POINT('Ctrl Pts',(1.61824802687329,-1.06847604194512,11.6744099857127));
#60540=CARTESIAN_POINT('Ctrl Pts',(1.59785508253992,-0.794772684000845,
11.5911257850145));
#60541=CARTESIAN_POINT('Ctrl Pts',(1.5926968241364,-0.636309800095194,11.5266070008333));
#60542=CARTESIAN_POINT('Ctrl Pts',(1.59311422876906,-0.319434907277159,
11.4512484604098));
#60543=CARTESIAN_POINT('Ctrl Pts',(1.59670845495764,-0.158333333333332,
11.4147734770359));
#60544=CARTESIAN_POINT('Ctrl Pts',(1.62223794910294,0.158333333333334,11.4048930759665));
#60545=CARTESIAN_POINT('Ctrl Pts',(1.64405960030171,0.319434907277165,11.4314759978575));
#60546=CARTESIAN_POINT('Ctrl Pts',(1.69587536621376,0.636309800095204,11.4867326241377));
#60547=CARTESIAN_POINT('Ctrl Pts',(1.73004745102725,0.79477268400084,11.5405226830685));
#60548=CARTESIAN_POINT('Ctrl Pts',(1.79369763209872,1.06847604194556,11.606703417957));
#60549=CARTESIAN_POINT('Ctrl Pts',(1.82351106461192,1.18514270861266,11.6340200566103));
#60550=CARTESIAN_POINT('Ctrl Pts',(1.85558612472409,1.3000000000013,11.6600061460216));
#60551=CARTESIAN_POINT('Ctrl Pts',(1.64172822170271,-1.30000000000004,11.7786863448143));
#60552=CARTESIAN_POINT('Ctrl Pts',(1.62575513936202,-1.1851427086118,11.7529906415876));
#60553=CARTESIAN_POINT('Ctrl Pts',(1.6134054477271,-1.06847604194512,11.7237453000575));
#60554=CARTESIAN_POINT('Ctrl Pts',(1.59324594689023,-0.794772684000844,
11.6479823360285));
#60555=CARTESIAN_POINT('Ctrl Pts',(1.58810131644293,-0.636309800095194,
11.5821626800989));
#60556=CARTESIAN_POINT('Ctrl Pts',(1.58994436496101,-0.319434907277158,
11.5067370957953));
#60557=CARTESIAN_POINT('Ctrl Pts',(1.59579155076718,-0.158333333333332,
11.4674554470401));
#60558=CARTESIAN_POINT('Ctrl Pts',(1.62204300194924,0.158333333333334,11.4574151571969));
#60559=CARTESIAN_POINT('Ctrl Pts',(1.64236886504219,0.319434907277165,11.4866258555787));
#60560=CARTESIAN_POINT('Ctrl Pts',(1.69415783221999,0.636309800095203,11.5416625456892));
#60561=CARTESIAN_POINT('Ctrl Pts',(1.72953400768076,0.794772684000838,11.5964997079218));
#60562=CARTESIAN_POINT('Ctrl Pts',(1.79311454461587,1.06847604194556,11.6551995377656));
#60563=CARTESIAN_POINT('Ctrl Pts',(1.82265133069952,1.18514270861266,11.6774486937642));
#60564=CARTESIAN_POINT('Ctrl Pts',(1.85420324431865,1.30000000000131,11.6965380244651));
#60565=CARTESIAN_POINT('Ctrl Pts',(1.63779021696461,-1.30000000000003,11.8035075973253));
#60566=CARTESIAN_POINT('Ctrl Pts',(1.62058710253557,-1.1851427086118,11.7827369798234));
#60567=CARTESIAN_POINT('Ctrl Pts',(1.60761419841532,-1.06847604194512,11.7570469303984));
#60568=CARTESIAN_POINT('Ctrl Pts',(1.58741682674095,-0.794772684000843,
11.6863329050787));
#60569=CARTESIAN_POINT('Ctrl Pts',(1.58451908111622,-0.636309800095193,
11.6192608085749));
#60570=CARTESIAN_POINT('Ctrl Pts',(1.58800279136641,-0.319434907277159,
11.5436880101914));
#60571=CARTESIAN_POINT('Ctrl Pts',(1.5945687098384,-0.158333333333331,11.502703946869));
#60572=CARTESIAN_POINT('Ctrl Pts',(1.62157218186044,0.158333333333334,11.4925040044064));
#60573=CARTESIAN_POINT('Ctrl Pts',(1.64210579695489,0.319434907277164,11.5231920863286));
#60574=CARTESIAN_POINT('Ctrl Pts',(1.69343054444979,0.636309800095202,11.5781839607371));
#60575=CARTESIAN_POINT('Ctrl Pts',(1.72737668125019,0.794772684000839,11.6342229988072));
#60576=CARTESIAN_POINT('Ctrl Pts',(1.7906744665107,1.06847604194556,11.6879901617425));
#60577=CARTESIAN_POINT('Ctrl Pts',(1.8203501553843,1.18514270861266,11.7067887653584));
#60578=CARTESIAN_POINT('Ctrl Pts',(1.85230226730626,1.30000000000131,11.7211121600253));
#60579=CARTESIAN_POINT('Ctrl Pts',(1.63206766705696,-1.30000000000004,11.8346752939481));
#60580=CARTESIAN_POINT('Ctrl Pts',(1.61435973387503,-1.18514270861181,11.8198546331378));
#60581=CARTESIAN_POINT('Ctrl Pts',(1.60115205248425,-1.06847604194513,11.7984963698485));
#60582=CARTESIAN_POINT('Ctrl Pts',(1.58103614819377,-0.794772684000846,
11.7340513393747));
#60583=CARTESIAN_POINT('Ctrl Pts',(1.57905152455074,-0.636309800095194,
11.6657577606432));
#60584=CARTESIAN_POINT('Ctrl Pts',(1.58365486389055,-0.319434907277158,
11.5901827399508));
#60585=CARTESIAN_POINT('Ctrl Pts',(1.59110326196349,-0.158333333333332,
11.5470991950029));
#60586=CARTESIAN_POINT('Ctrl Pts',(1.61887637191083,0.158333333333334,11.536748396219));
#60587=CARTESIAN_POINT('Ctrl Pts',(1.63951288335966,0.319434907277167,11.5693233003321));
#60588=CARTESIAN_POINT('Ctrl Pts',(1.69084625596948,0.636309800095205,11.6241360020771));
#60589=CARTESIAN_POINT('Ctrl Pts',(1.72416805543662,0.794772684000839,11.6814128995574));
#60590=CARTESIAN_POINT('Ctrl Pts',(1.78767359202545,1.06847604194556,11.7289080614217));
#60591=CARTESIAN_POINT('Ctrl Pts',(1.81760534753292,1.18514270861266,11.7433876662583));
#60592=CARTESIAN_POINT('Ctrl Pts',(1.84997966487054,1.30000000000131,11.7517879802295));
#60593=CARTESIAN_POINT('Ctrl Pts',(1.62757496106193,-1.30000000000004,11.8610434436437));
#60594=CARTESIAN_POINT('Ctrl Pts',(1.60890493030257,-1.18514270861181,11.8513624255336));
#60595=CARTESIAN_POINT('Ctrl Pts',(1.59508081426732,-1.06847604194513,11.8337526333206));
#60596=CARTESIAN_POINT('Ctrl Pts',(1.57433937315554,-0.794772684000849,
11.7747534361581));
#60597=CARTESIAN_POINT('Ctrl Pts',(1.57280459694369,-0.636309800095195,
11.7054903069103));
#60598=CARTESIAN_POINT('Ctrl Pts',(1.57862731462552,-0.319434907277158,
11.6298804413981));
#60599=CARTESIAN_POINT('Ctrl Pts',(1.58783877253507,-0.158333333333332,
11.5848469494164));
#60600=CARTESIAN_POINT('Ctrl Pts',(1.616612712653,0.158333333333334,11.5743201399577));
#60601=CARTESIAN_POINT('Ctrl Pts',(1.63696911563611,0.319434907277164,11.6085667153463));
#60602=CARTESIAN_POINT('Ctrl Pts',(1.68813968272809,0.636309800095203,11.6632640474509));
#60603=CARTESIAN_POINT('Ctrl Pts',(1.72074210362639,0.794772684000839,11.721627553831));
#60604=CARTESIAN_POINT('Ctrl Pts',(1.7845030729319,1.06847604194556,11.7637824585709));
#60605=CARTESIAN_POINT('Ctrl Pts',(1.81475743751615,1.18514270861266,11.7745746641525));
#60606=CARTESIAN_POINT('Ctrl Pts',(1.84766640564899,1.30000000000131,11.7779117790467));
#60607=CARTESIAN_POINT('Ctrl Pts',(1.62446161102719,-1.30000000000004,11.8766283155242));
#60608=CARTESIAN_POINT('Ctrl Pts',(1.60517405537136,-1.18514270861181,11.8699722209449));
#60609=CARTESIAN_POINT('Ctrl Pts',(1.5909861623095,-1.06847604194513,11.8545628836417));
#60610=CARTESIAN_POINT('Ctrl Pts',(1.56999053183438,-0.794772684000848,
11.7987424900714));
#60611=CARTESIAN_POINT('Ctrl Pts',(1.56902003450696,-0.636309800095197,
11.7288624901258));
#60612=CARTESIAN_POINT('Ctrl Pts',(1.5757349176515,-0.31943490727716,11.6532066521009));
#60613=CARTESIAN_POINT('Ctrl Pts',(1.5861166141376,-0.158333333333332,11.6070056598578));
#60614=CARTESIAN_POINT('Ctrl Pts',(1.61521019215178,0.158333333333334,11.5964305482167));
#60615=CARTESIAN_POINT('Ctrl Pts',(1.63483676436541,0.319434907277165,11.6317671668772));
#60616=CARTESIAN_POINT('Ctrl Pts',(1.68552024576209,0.636309800095204,11.6864714696696));
#60617=CARTESIAN_POINT('Ctrl Pts',(1.7174936154201,0.794772684000843,11.7455132932636));
#60618=CARTESIAN_POINT('Ctrl Pts',(1.7816632929437,1.06847604194556,11.7844768543231));
#60619=CARTESIAN_POINT('Ctrl Pts',(1.81235488861359,1.18514270861267,11.7930523385357));
#60620=CARTESIAN_POINT('Ctrl Pts',(1.84596140427423,1.30000000000131,11.7933374251206));
#60621=CARTESIAN_POINT('Ctrl Pts',(1.62325910326905,-1.30000000000004,11.8828532156717));
#60622=CARTESIAN_POINT('Ctrl Pts',(1.60375087733459,-1.18514270861181,11.8774021306647));
#60623=CARTESIAN_POINT('Ctrl Pts',(1.5894276312557,-1.06847604194513,11.8628709907803));
#60624=CARTESIAN_POINT('Ctrl Pts',(1.56831640817595,-0.794772684000848,
11.8083244074774));
#60625=CARTESIAN_POINT('Ctrl Pts',(1.5674992324408,-0.636309800095196,11.7382106430618));
#60626=CARTESIAN_POINT('Ctrl Pts',(1.57451847326436,-0.31943490727716,11.662546109776));
#60627=CARTESIAN_POINT('Ctrl Pts',(1.58531440897992,-0.158333333333332,
11.6158888448209));
#60628=CARTESIAN_POINT('Ctrl Pts',(1.6145903331477,0.158333333333334,11.6052837860805));
#60629=CARTESIAN_POINT('Ctrl Pts',(1.63407113660023,0.319434907277164,11.6410280219121));
#60630=CARTESIAN_POINT('Ctrl Pts',(1.6846462572754,0.636309800095204,11.6957181276293));
#60631=CARTESIAN_POINT('Ctrl Pts',(1.71638682467756,0.794772684000842,11.7550267856039));
#60632=CARTESIAN_POINT('Ctrl Pts',(1.78067425165386,1.06847604194556,11.7927235360901));
#60633=CARTESIAN_POINT('Ctrl Pts',(1.81149866824387,1.18514270861266,11.8004212359001));
#60634=CARTESIAN_POINT('Ctrl Pts',(1.84531985636975,1.30000000000131,11.799499109037));
#60635=CARTESIAN_POINT('Ctrl Pts',(1.61932560970724,-1.30000000000004,11.9000572296304));
#60636=CARTESIAN_POINT('Ctrl Pts',(1.59863734714343,-1.18514270861181,11.8979988143724));
#60637=CARTESIAN_POINT('Ctrl Pts',(1.58368072051496,-1.06847604194513,11.8859178751391));
#60638=CARTESIAN_POINT('Ctrl Pts',(1.56236914656071,-0.794772684000847,
11.8348544533447));
#60639=CARTESIAN_POINT('Ctrl Pts',(1.56359939056409,-0.636309800095195,
11.7638599559));
#60640=CARTESIAN_POINT('Ctrl Pts',(1.57168045445783,-0.319434907277159,
11.6881522006818));
#60641=CARTESIAN_POINT('Ctrl Pts',(1.58250539610576,-0.158333333333332,
11.6404302732981));
#60642=CARTESIAN_POINT('Ctrl Pts',(1.61222232235546,0.158333333333334,11.629751579368));
#60643=CARTESIAN_POINT('Ctrl Pts',(1.63182988702215,0.319434907277165,11.6665211023994));
#60644=CARTESIAN_POINT('Ctrl Pts',(1.68282247714058,0.636309800095204,11.7210346553957));
#60645=CARTESIAN_POINT('Ctrl Pts',(1.71492005119327,0.79477268400084,11.7808809201514));
#60646=CARTESIAN_POINT('Ctrl Pts',(1.77944618880968,1.06847604194556,11.8151101249152));
#60647=CARTESIAN_POINT('Ctrl Pts',(1.81031592086132,1.18514270861266,11.8204561758092));
#60648=CARTESIAN_POINT('Ctrl Pts',(1.84412441091943,1.30000000000131,11.816331723172));
#60649=CARTESIAN_POINT('Ctrl Pts',(1.61514176393842,-1.30000000000004,11.9218149414855));
#60650=CARTESIAN_POINT('Ctrl Pts',(1.59369237945656,-1.18514270861181,11.9239622185499));
#60651=CARTESIAN_POINT('Ctrl Pts',(1.57817340785515,-1.06847604194512,11.9149610364403));
#60652=CARTESIAN_POINT('Ctrl Pts',(1.55602191902508,-0.794772684000845,
11.8684113341534));
#60653=CARTESIAN_POINT('Ctrl Pts',(1.5570312496809,-0.636309800095196,11.7967058631063));
#60654=CARTESIAN_POINT('Ctrl Pts',(1.56568570948374,-0.31943490727716,11.7210616480371));
#60655=CARTESIAN_POINT('Ctrl Pts',(1.57799472897679,-0.158333333333332,
11.6717765646414));
#60656=CARTESIAN_POINT('Ctrl Pts',(1.60825236528344,0.158333333333334,11.6610301361501));
#60657=CARTESIAN_POINT('Ctrl Pts',(1.62744678734947,0.319434907277165,11.6992035717281));
#60658=CARTESIAN_POINT('Ctrl Pts',(1.6778873384829,0.636309800095204,11.7537020112002));
#60659=CARTESIAN_POINT('Ctrl Pts',(1.70847024371082,0.794772684000842,11.814605530805));
#60660=CARTESIAN_POINT('Ctrl Pts',(1.77391916968909,1.06847604194556,11.8443178419405));
#60661=CARTESIAN_POINT('Ctrl Pts',(1.80574027615595,1.18514270861267,11.8465100349315));
#60662=CARTESIAN_POINT('Ctrl Pts',(1.84105207415533,1.30000000000131,11.8380330623724));
#60663=CARTESIAN_POINT('Ctrl Pts',(1.60783404495285,-1.30000000000004,11.9530476574059));
#60664=CARTESIAN_POINT('Ctrl Pts',(1.58426159374155,-1.18514270861181,11.9613249468198));
#60665=CARTESIAN_POINT('Ctrl Pts',(1.56744492513183,-1.06847604194513,11.9567777659226));
#60666=CARTESIAN_POINT('Ctrl Pts',(1.54420226577969,-0.794772684000849,
11.9166457764448));
#60667=CARTESIAN_POINT('Ctrl Pts',(1.54733643364015,-0.636309800095195,
11.8436015159348));
#60668=CARTESIAN_POINT('Ctrl Pts',(1.55773531862725,-0.319434907277158,
11.7679317466498));
#60669=CARTESIAN_POINT('Ctrl Pts',(1.57160625154768,-0.158333333333332,
11.7165083827316));
#60670=CARTESIAN_POINT('Ctrl Pts',(1.60266798886658,0.158333333333334,11.7056600071616));
#60671=CARTESIAN_POINT('Ctrl Pts',(1.62083885672664,0.319434907277168,11.7459022467507));
#60672=CARTESIAN_POINT('Ctrl Pts',(1.67171417543449,0.636309800095206,11.8001524413723));
#60673=CARTESIAN_POINT('Ctrl Pts',(1.7034077465642,0.794772684000839,11.8619602905416));
#60674=CARTESIAN_POINT('Ctrl Pts',(1.76966641057741,1.06847604194556,11.8853447403049));
#60675=CARTESIAN_POINT('Ctrl Pts',(1.8017577243743,1.18514270861266,11.8832530437335));
#60676=CARTESIAN_POINT('Ctrl Pts',(1.83725943144218,1.30000000000131,11.8689473887673));
#60677=CARTESIAN_POINT('Ctrl Pts',(1.60362879054004,-1.30000000000005,11.9717350649118));
#60678=CARTESIAN_POINT('Ctrl Pts',(1.57888716168168,-1.18514270861182,11.9836612254861));
#60679=CARTESIAN_POINT('Ctrl Pts',(1.56131753260336,-1.06847604194513,11.981772259511));
#60680=CARTESIAN_POINT('Ctrl Pts',(1.53729692888577,-0.794772684000851,
11.9454926641869));
#60681=CARTESIAN_POINT('Ctrl Pts',(1.54134412420084,-0.636309800095197,
11.8716953287081));
#60682=CARTESIAN_POINT('Ctrl Pts',(1.55242668622773,-0.319434907277159,
11.796066796982));
#60683=CARTESIAN_POINT('Ctrl Pts',(1.56691293504717,-0.158333333333332,
11.7434227014676));
#60684=CARTESIAN_POINT('Ctrl Pts',(1.59850372070212,0.158333333333334,11.7325116687194));
#60685=CARTESIAN_POINT('Ctrl Pts',(1.6169412386113,0.319434907277167,11.7738468098411));
#60686=CARTESIAN_POINT('Ctrl Pts',(1.66749164588227,0.636309800095206,11.8280608912181));
#60687=CARTESIAN_POINT('Ctrl Pts',(1.69739655218748,0.79477268400084,11.8908575699105));
#60688=CARTESIAN_POINT('Ctrl Pts',(1.76461391978401,1.06847604194556,11.9103538108361));
#60689=CARTESIAN_POINT('Ctrl Pts',(1.79771081767218,1.18514270861267,11.9055342229517));
#60690=CARTESIAN_POINT('Ctrl Pts',(1.83480870566485,1.30000000000132,11.8874558468933));
#60691=CARTESIAN_POINT('Ctrl Pts',(1.600345881349,-1.30000000000005,11.9842630921627));
#60692=CARTESIAN_POINT('Ctrl Pts',(1.57504122138965,-1.18514270861182,11.9985854052829));
#60693=CARTESIAN_POINT('Ctrl Pts',(1.55708435379925,-1.06847604194513,11.9984485537176));
#60694=CARTESIAN_POINT('Ctrl Pts',(1.53257526769946,-0.794772684000851,
11.9647288362548));
#60695=CARTESIAN_POINT('Ctrl Pts',(1.53670704324099,-0.636309800095197,
11.8905067546537));
#60696=CARTESIAN_POINT('Ctrl Pts',(1.54831342142086,-0.319434907277159,
11.8149010785834));
#60697=CARTESIAN_POINT('Ctrl Pts',(1.56375557866725,-0.158333333333332,
11.7613725996759));
#60698=CARTESIAN_POINT('Ctrl Pts',(1.59581317861656,0.158333333333334,11.7504080900329));
#60699=CARTESIAN_POINT('Ctrl Pts',(1.61390936643398,0.319434907277167,11.7925524285043));
#60700=CARTESIAN_POINT('Ctrl Pts',(1.66458583994602,0.636309800095206,11.8466789456142));
#60701=CARTESIAN_POINT('Ctrl Pts',(1.69463294550622,0.79477268400084,11.9098917520947));
#60702=CARTESIAN_POINT('Ctrl Pts',(1.76226517728142,1.06847604194556,11.9268506192697));
#60703=CARTESIAN_POINT('Ctrl Pts',(1.79559295568807,1.18514270861267,11.9203016847132));
#60704=CARTESIAN_POINT('Ctrl Pts',(1.83297302538702,1.30000000000132,11.899862950388));
#60705=CARTESIAN_POINT('',(1.81631379076882,1.2,11.8047262908302));
#60706=CARTESIAN_POINT('Ctrl Pts',(1.81631379076882,1.2,11.8047262908302));
#60707=CARTESIAN_POINT('Ctrl Pts',(1.81954172329026,1.20865297781299,11.7941512478302));
#60708=CARTESIAN_POINT('Ctrl Pts',(1.82334800037714,1.21707870846838,11.783575657389));
#60709=CARTESIAN_POINT('Ctrl Pts',(1.83010849452505,1.23366298102073,11.7630163352366));
#60710=CARTESIAN_POINT('Ctrl Pts',(1.83359564288739,1.24271606614613,11.7518564645226));
#60711=CARTESIAN_POINT('Ctrl Pts',(1.84611908787067,1.27553627908762,11.7113941521115));
#60712=CARTESIAN_POINT('Ctrl Pts',(1.84915634495443,1.28315372901467,11.701886753377));
#60713=CARTESIAN_POINT('Ctrl Pts',(1.85479302522287,1.30000000000131,11.6813215498971));
#60714=CARTESIAN_POINT('',(1.66957759488823,0.653834841417358,11.8599367650635));
#60715=CARTESIAN_POINT('Ctrl Pts',(1.66957759489952,0.653834841416676,11.859936765087));
#60716=CARTESIAN_POINT('Ctrl Pts',(1.68494198314014,0.71815705809227,11.8544319611253));
#60717=CARTESIAN_POINT('Ctrl Pts',(1.69640604766083,0.760168978913057,11.850270842599));
#60718=CARTESIAN_POINT('Ctrl Pts',(1.74570835223144,0.949887649636558,11.8320857710676));
#60719=CARTESIAN_POINT('Ctrl Pts',(1.78038525555478,1.07519041108246,11.8188981416352));
#60720=CARTESIAN_POINT('Ctrl Pts',(1.81631379076882,1.2,11.8047262908302));
#60721=CARTESIAN_POINT('',(1.53759581372214,-0.653834841531101,11.9051353980119));
#60722=CARTESIAN_POINT('Ctrl Pts',(1.53759581372214,-0.653834841531122,
11.9051353980119));
#60723=CARTESIAN_POINT('Ctrl Pts',(1.54252926752756,-0.57592707476385,11.8638270643046));
#60724=CARTESIAN_POINT('Ctrl Pts',(1.54744292193318,-0.493582421500596,
11.8290212458167));
#60725=CARTESIAN_POINT('Ctrl Pts',(1.55695050923341,-0.338052012707416,
11.7793054455627));
#60726=CARTESIAN_POINT('Ctrl Pts',(1.5615223834955,-0.265565628467728,11.7620037496986));
#60727=CARTESIAN_POINT('Ctrl Pts',(1.571794384339,-0.129646434571565,11.7398984122046));
#60728=CARTESIAN_POINT('Ctrl Pts',(1.57720257787791,-0.0665942542479303,
11.7336412316907));
#60729=CARTESIAN_POINT('Ctrl Pts',(1.58968469190397,0.0595028577922644,
11.7289735009213));
#60730=CARTESIAN_POINT('Ctrl Pts',(1.59684561072502,0.122699779224089,11.7305123643919));
#60731=CARTESIAN_POINT('Ctrl Pts',(1.61358182914933,0.260014810575644,11.7427412035281));
#60732=CARTESIAN_POINT('Ctrl Pts',(1.62336779242219,0.333833648164222,11.755055690296));
#60733=CARTESIAN_POINT('Ctrl Pts',(1.64505548717876,0.49116691886655,11.7943182041769));
#60734=CARTESIAN_POINT('Ctrl Pts',(1.65719828911254,0.574146030768171,11.823374616898));
#60735=CARTESIAN_POINT('Ctrl Pts',(1.66957759491099,0.653834841429009,11.8599367650304));
#60736=CARTESIAN_POINT('',(1.60613120890469,-1.2,11.8821835226508));
#60737=CARTESIAN_POINT('Ctrl Pts',(1.60613120890469,-1.2,11.8821835226508));
#60738=CARTESIAN_POINT('Ctrl Pts',(1.58809120755403,-1.09919977191309,11.8883717912306));
#60739=CARTESIAN_POINT('Ctrl Pts',(1.57551018723902,-1.0108368422167,11.8925996120367));
#60740=CARTESIAN_POINT('Ctrl Pts',(1.54791748959699,-0.787234072051788,
11.9017710545491));
#60741=CARTESIAN_POINT('Ctrl Pts',(1.5438100803565,-0.741256752224837,11.9031046317205));
#60742=CARTESIAN_POINT('Ctrl Pts',(1.53759581372215,-0.6538348415311,11.9051353980119));
#60743=CARTESIAN_POINT('Ctrl Pts',(1.64376583932815,-1.3,11.7629523189989));
#60744=CARTESIAN_POINT('Ctrl Pts',(1.63817081442155,-1.28288489407424,11.7831596690008));
#60745=CARTESIAN_POINT('Ctrl Pts',(1.63165744768168,-1.26605460703988,11.8033441571198));
#60746=CARTESIAN_POINT('Ctrl Pts',(1.62182860196257,-1.23991764288754,11.834504145476));
#60747=CARTESIAN_POINT('Ctrl Pts',(1.61939946340474,-1.23326875145929,11.8423946820282));
#60748=CARTESIAN_POINT('Ctrl Pts',(1.61100387997911,-1.21129319797848,11.8685758706849));
#60749=CARTESIAN_POINT('Ctrl Pts',(1.60993145974154,-1.20847825033892,11.8719167228947));
#60750=CARTESIAN_POINT('Ctrl Pts',(1.60613120890469,-1.2,11.8821835226508));
#60751=CARTESIAN_POINT('Origin',(0.,1.25,7.2));
#60752=CARTESIAN_POINT('Origin',(0.,1.2,7.2));
#60753=CARTESIAN_POINT('Origin',(0.,1.25,7.2));
#60754=CARTESIAN_POINT('',(1.45281637513429,1.20000000016485,11.9320000612277));
#60755=CARTESIAN_POINT('Ctrl Pts',(1.35226619967441,1.30000000000266,11.8576685289093));
#60756=CARTESIAN_POINT('Ctrl Pts',(1.35823284506601,1.2940797865347,11.862100905817));
#60757=CARTESIAN_POINT('Ctrl Pts',(1.3636491659162,1.28792143437105,11.8669357058832));
#60758=CARTESIAN_POINT('Ctrl Pts',(1.37478082571786,1.27683526110006,11.8752248429408));
#60759=CARTESIAN_POINT('Ctrl Pts',(1.38017594642871,1.27167604393436,11.8790171853508));
#60760=CARTESIAN_POINT('Ctrl Pts',(1.39340497014156,1.25863370373997,11.8886989987441));
#60761=CARTESIAN_POINT('Ctrl Pts',(1.39774281353032,1.25431389636448,11.8919151916413));
#60762=CARTESIAN_POINT('Ctrl Pts',(1.4116468894559,1.24027168164373,11.9024179757432));
#60763=CARTESIAN_POINT('Ctrl Pts',(1.43151180765357,1.21992450679007,11.9176985644207));
#60764=CARTESIAN_POINT('Ctrl Pts',(1.45281637515628,1.20000000013438,11.9320000611525));
#60765=CARTESIAN_POINT('Origin',(0.,1.2,7.2));
#60766=CARTESIAN_POINT('Origin',(0.,0.92691742076555,7.2));
#60767=CARTESIAN_POINT('Origin',(0.,0.653834841531101,7.2));
#60768=CARTESIAN_POINT('Origin',(0.,0.,7.2));
#60769=CARTESIAN_POINT('Origin',(0.,-0.653834841531101,7.2));
#60770=CARTESIAN_POINT('Origin',(0.,-0.926917420765551,7.2));
#60771=CARTESIAN_POINT('Origin',(0.,-1.2,7.2));
#60772=CARTESIAN_POINT('Origin',(0.,-1.25,7.2));
#60773=CARTESIAN_POINT('Ctrl Pts',(1.27960380226576,-1.30000000000011,12.0796635102738));
#60774=CARTESIAN_POINT('Ctrl Pts',(1.32185850051503,-1.18514270861186,12.0742273399892));
#60775=CARTESIAN_POINT('Ctrl Pts',(1.35267060678129,-1.06847604194516,12.0599359627022));
#60776=CARTESIAN_POINT('Ctrl Pts',(1.39741805963368,-0.794772684000851,
12.0064627225352));
#60777=CARTESIAN_POINT('Ctrl Pts',(1.38457112325749,-0.636309800095197,
11.9376612423041));
#60778=CARTESIAN_POINT('Ctrl Pts',(1.39375448302828,-0.319434907277159,
11.864085086346));
#60779=CARTESIAN_POINT('Ctrl Pts',(1.38362278588515,-0.158333333333333,
11.8193529279854));
#60780=CARTESIAN_POINT('Ctrl Pts',(1.41600270610974,0.158333333333334,11.8093804181475));
#60781=CARTESIAN_POINT('Ctrl Pts',(1.45995892423146,0.319434907277167,11.8436091949742));
#60782=CARTESIAN_POINT('Ctrl Pts',(1.51378858280534,0.636309800095206,11.8979534138578));
#60783=CARTESIAN_POINT('Ctrl Pts',(1.56075790439375,0.79477268400084,11.9555717424973));
#60784=CARTESIAN_POINT('Ctrl Pts',(1.56074958985878,1.06847604194602,11.9972576463276));
#60785=CARTESIAN_POINT('Ctrl Pts',(1.54630261814452,1.18514270861357,12.0079231435181));
#60786=CARTESIAN_POINT('Ctrl Pts',(1.51741227377009,1.30000000000265,12.011209854746));
#60787=CARTESIAN_POINT('Ctrl Pts',(1.27082599327824,-1.30000000000011,12.0707049385394));
#60788=CARTESIAN_POINT('Ctrl Pts',(1.31146501795804,-1.18514270861186,12.0635250605734));
#60789=CARTESIAN_POINT('Ctrl Pts',(1.34107385349426,-1.06847604194515,12.047970320616));
#60790=CARTESIAN_POINT('Ctrl Pts',(1.3839942433067,-0.794772684000847,11.9926881530137));
#60791=CARTESIAN_POINT('Ctrl Pts',(1.37127685908325,-0.636309800095196,
11.9243069098157));
#60792=CARTESIAN_POINT('Ctrl Pts',(1.38030676013406,-0.31943490727716,11.8507340127396));
#60793=CARTESIAN_POINT('Ctrl Pts',(1.37092683910606,-0.158333333333332,
11.8064558800024));
#60794=CARTESIAN_POINT('Ctrl Pts',(1.40289766570327,0.158333333333334,11.7967144930055));
#60795=CARTESIAN_POINT('Ctrl Pts',(1.44556071014891,0.319434907277165,11.8307896575199));
#60796=CARTESIAN_POINT('Ctrl Pts',(1.49898002676598,0.636309800095204,11.8854602584084));
#60797=CARTESIAN_POINT('Ctrl Pts',(1.54563126199516,0.79477268400084,11.9427846751805));
#60798=CARTESIAN_POINT('Ctrl Pts',(1.54752279646355,1.06847604194602,11.9862544409645));
#60799=CARTESIAN_POINT('Ctrl Pts',(1.53441897429966,1.18514270861357,11.9981098154132));
#60800=CARTESIAN_POINT('Ctrl Pts',(1.50739255478879,1.30000000000265,12.0030041134162));
#60801=CARTESIAN_POINT('Ctrl Pts',(1.25383737212069,-1.30000000000012,12.052589623136));
#60802=CARTESIAN_POINT('Ctrl Pts',(1.28972360254438,-1.18514270861186,12.0426154229797));
#60803=CARTESIAN_POINT('Ctrl Pts',(1.31605876757647,-1.06847604194516,12.0249219047458));
#60804=CARTESIAN_POINT('Ctrl Pts',(1.35483339539366,-0.79477268400085,11.9662131690461));
#60805=CARTESIAN_POINT('Ctrl Pts',(1.34485222586452,-0.636309800095198,
11.897481087427));
#60806=CARTESIAN_POINT('Ctrl Pts',(1.35423307167692,-0.31943490727716,11.8235941605412));
#60807=CARTESIAN_POINT('Ctrl Pts',(1.34545823241125,-0.158333333333333,
11.7806840788868));
#60808=CARTESIAN_POINT('Ctrl Pts',(1.37685655019847,0.158333333333334,11.771262559764));
#60809=CARTESIAN_POINT('Ctrl Pts',(1.41792802988074,0.319434907277167,11.8044845269271));
#60810=CARTESIAN_POINT('Ctrl Pts',(1.47067347813237,0.636309800095207,11.8597235333016));
#60811=CARTESIAN_POINT('Ctrl Pts',(1.51577191090823,0.794772684000843,11.9169468970452));
#60812=CARTESIAN_POINT('Ctrl Pts',(1.52149737687582,1.06847604194602,11.9639876772803));
#60813=CARTESIAN_POINT('Ctrl Pts',(1.51126569030078,1.18514270861357,11.9781387732636));
#60814=CARTESIAN_POINT('Ctrl Pts',(1.48832397508273,1.30000000000265,11.9860787544988));
#60815=CARTESIAN_POINT('Ctrl Pts',(1.2365731147009,-1.30000000000012,12.034356720118));
#60816=CARTESIAN_POINT('Ctrl Pts',(1.27010978630414,-1.18514270861187,12.0204441753879));
#60817=CARTESIAN_POINT('Ctrl Pts',(1.29456342074366,-1.06847604194516,11.9999506330389));
#60818=CARTESIAN_POINT('Ctrl Pts',(1.33007257532821,-0.794772684000856,
11.9374030294705));
#60819=CARTESIAN_POINT('Ctrl Pts',(1.31916493506146,-0.6363098000952,11.8700777360443));
#60820=CARTESIAN_POINT('Ctrl Pts',(1.32782448681212,-0.31943490727716,11.7963893863368));
#60821=CARTESIAN_POINT('Ctrl Pts',(1.32055135829017,-0.158333333333333,
11.754410128018));
#60822=CARTESIAN_POINT('Ctrl Pts',(1.35133196538818,0.158333333333335,11.7453259482025));
#60823=CARTESIAN_POINT('Ctrl Pts',(1.39055802938108,0.319434907277168,11.7778105062921));
#60824=CARTESIAN_POINT('Ctrl Pts',(1.44220840952662,0.636309800095208,11.8338312363221));
#60825=CARTESIAN_POINT('Ctrl Pts',(1.48524012839578,0.794772684000845,11.8912092691164));
#60826=CARTESIAN_POINT('Ctrl Pts',(1.49468958829248,1.06847604194603,11.9419141249711));
#60827=CARTESIAN_POINT('Ctrl Pts',(1.48739966201705,1.18514270861358,11.9583509797162));
#60828=CARTESIAN_POINT('Ctrl Pts',(1.46872948841386,1.30000000000266,11.9692764359068));
#60829=CARTESIAN_POINT('Ctrl Pts',(1.2279422538807,-1.30000000000012,12.0251164943471));
#60830=CARTESIAN_POINT('Ctrl Pts',(1.25939336556772,-1.18514270861187,12.0096188855853));
#60831=CARTESIAN_POINT('Ctrl Pts',(1.28238085235411,-1.06847604194516,11.9879392005477));
#60832=CARTESIAN_POINT('Ctrl Pts',(1.3159338787988,-0.794772684000856,11.9235729581872));
#60833=CARTESIAN_POINT('Ctrl Pts',(1.30587319655974,-0.636309800095201,
11.85633747634));
#60834=CARTESIAN_POINT('Ctrl Pts',(1.31477662826182,-0.319434907277161,
11.782456120855));
#60835=CARTESIAN_POINT('Ctrl Pts',(1.30836512397911,-0.158333333333333,
11.7409006005277));
#60836=CARTESIAN_POINT('Ctrl Pts',(1.33885141222359,0.158333333333335,11.7319758825528));
#60837=CARTESIAN_POINT('Ctrl Pts',(1.37669134199997,0.319434907277169,11.7643080243584));
#60838=CARTESIAN_POINT('Ctrl Pts',(1.42796721862588,0.636309800095209,11.8206187219591));
#60839=CARTESIAN_POINT('Ctrl Pts',(1.47080084715812,0.794772684000844,11.8776220530351));
#60840=CARTESIAN_POINT('Ctrl Pts',(1.48213706696437,1.06847604194603,11.9301857284284));
#60841=CARTESIAN_POINT('Ctrl Pts',(1.47615489814238,1.18514270861358,11.9478807037177));
#60842=CARTESIAN_POINT('Ctrl Pts',(1.45928353099258,1.30000000000266,11.9605177868944));
#60843=CARTESIAN_POINT('Ctrl Pts',(1.2277441157689,-1.30000000000012,12.0249027924082));
#60844=CARTESIAN_POINT('Ctrl Pts',(1.25914693044367,-1.18514270861187,12.0093686494923));
#60845=CARTESIAN_POINT('Ctrl Pts',(1.28210042632704,-1.06847604194516,11.9876616416957));
#60846=CARTESIAN_POINT('Ctrl Pts',(1.31560797696017,-0.794772684000856,
11.9232535584614));
#60847=CARTESIAN_POINT('Ctrl Pts',(1.30556631666563,-0.636309800095201,
11.8560204271351));
#60848=CARTESIAN_POINT('Ctrl Pts',(1.3144757803299,-0.319434907277161,11.7821344120641));
#60849=CARTESIAN_POINT('Ctrl Pts',(1.30808552937375,-0.158333333333333,
11.7405879874874));
#60850=CARTESIAN_POINT('Ctrl Pts',(1.33856517060333,0.158333333333335,11.7316668701696));
#60851=CARTESIAN_POINT('Ctrl Pts',(1.37637210730414,0.319434907277169,11.7639959828845));
#60852=CARTESIAN_POINT('Ctrl Pts',(1.42763878600979,0.636309800095209,11.8203136512801));
#60853=CARTESIAN_POINT('Ctrl Pts',(1.47046774593146,0.794772684000844,11.8773083954233));
#60854=CARTESIAN_POINT('Ctrl Pts',(1.48184741511707,1.06847604194603,11.9299150314142));
#60855=CARTESIAN_POINT('Ctrl Pts',(1.47589543953387,1.18514270861358,11.9476390432925));
#60856=CARTESIAN_POINT('Ctrl Pts',(1.4590656512353,1.30000000000266,11.9603156035967));
#60857=CARTESIAN_POINT('Ctrl Pts',(1.22754580284173,-1.30000000000012,12.0246891655378));
#60858=CARTESIAN_POINT('Ctrl Pts',(1.25890052554179,-1.18514270861187,12.00911840385));
#60859=CARTESIAN_POINT('Ctrl Pts',(1.28182017328752,-1.06847604194516,11.9873840137994));
#60860=CARTESIAN_POINT('Ctrl Pts',(1.3152824340645,-0.794772684000856,11.9229340102849));
#60861=CARTESIAN_POINT('Ctrl Pts',(1.30525983172521,-0.636309800095201,
11.8557031978233));
#60862=CARTESIAN_POINT('Ctrl Pts',(1.31417504098312,-0.319434907277161,
11.7818126625729));
#60863=CARTESIAN_POINT('Ctrl Pts',(1.307805392372,-0.158333333333333,11.7402756575975));
#60864=CARTESIAN_POINT('Ctrl Pts',(1.33827832071744,0.158333333333335,11.7313581736543));
#60865=CARTESIAN_POINT('Ctrl Pts',(1.37605285408983,0.319434907277169,11.7636839655362));
#60866=CARTESIAN_POINT('Ctrl Pts',(1.42731047763198,0.636309800095209,11.8200085332043));
#60867=CARTESIAN_POINT('Ctrl Pts',(1.47013448595545,0.794772684000844,11.8769948315385));
#60868=CARTESIAN_POINT('Ctrl Pts',(1.4815575698706,1.06847604194603,11.929644439847));
#60869=CARTESIAN_POINT('Ctrl Pts',(1.47563580573477,1.18514270861358,11.9473974756357));
#60870=CARTESIAN_POINT('Ctrl Pts',(1.45884764770319,1.30000000000266,11.9601134826365));
#60871=CARTESIAN_POINT('Ctrl Pts',(1.22714990870516,-1.30000000000012,12.0242615781458));
#60872=CARTESIAN_POINT('Ctrl Pts',(1.25840855833041,-1.18514270861187,12.0086175096358));
#60873=CARTESIAN_POINT('Ctrl Pts',(1.28126054876466,-1.06847604194516,11.9868283246064));
#60874=CARTESIAN_POINT('Ctrl Pts',(1.31463215371521,-0.794772684000856,
11.9222944997908));
#60875=CARTESIAN_POINT('Ctrl Pts',(1.30464720806962,-0.636309800095201,
11.8550685521741));
#60876=CARTESIAN_POINT('Ctrl Pts',(1.31357391352614,-0.319434907277161,
11.7811689659258));
#60877=CARTESIAN_POINT('Ctrl Pts',(1.30724591853039,-0.158333333333334,
11.7396505754641));
#60878=CARTESIAN_POINT('Ctrl Pts',(1.33770547706531,0.158333333333335,11.7307403238344));
#60879=CARTESIAN_POINT('Ctrl Pts',(1.37541502963884,0.319434907277169,11.7630595516123));
#60880=CARTESIAN_POINT('Ctrl Pts',(1.42665420609279,0.63630980009521,11.8193980878653));
#60881=CARTESIAN_POINT('Ctrl Pts',(1.46946784062387,0.794772684000844,11.876367741162));
#60882=CARTESIAN_POINT('Ctrl Pts',(1.4809776294413,1.06847604194603,11.9291033667068));
#60883=CARTESIAN_POINT('Ctrl Pts',(1.47511633151914,1.18514270861358,11.9469144330437));
#60884=CARTESIAN_POINT('Ctrl Pts',(1.45841157457544,1.30000000000266,11.9597092674665));
#60885=CARTESIAN_POINT('Ctrl Pts',(1.22629415633927,-1.30000000000012,12.0233341953758));
#60886=CARTESIAN_POINT('Ctrl Pts',(1.25734596825504,-1.18514270861187,12.0075306576544));
#60887=CARTESIAN_POINT('Ctrl Pts',(1.28005213212735,-1.06847604194516,11.9856223762587));
#60888=CARTESIAN_POINT('Ctrl Pts',(1.31322779650329,-0.794772684000856,
11.9209066843603));
#60889=CARTESIAN_POINT('Ctrl Pts',(1.30332272510325,-0.636309800095201,
11.8536920688135));
#60890=CARTESIAN_POINT('Ctrl Pts',(1.3122731506626,-0.319434907277161,11.7797734197834));
#60891=CARTESIAN_POINT('Ctrl Pts',(1.30603447327239,-0.158333333333333,
11.7382958186757));
#60892=CARTESIAN_POINT('Ctrl Pts',(1.33646502740032,0.158333333333335,11.7294012299134));
#60893=CARTESIAN_POINT('Ctrl Pts',(1.37403557863277,0.319434907277169,11.7617053160632));
#60894=CARTESIAN_POINT('Ctrl Pts',(1.42523407739856,0.636309800095209,11.8180744807929));
#60895=CARTESIAN_POINT('Ctrl Pts',(1.46802220160723,0.794772684000844,11.875009634575));
#60896=CARTESIAN_POINT('Ctrl Pts',(1.47971924795819,1.06847604194603,11.9279319497901));
#60897=CARTESIAN_POINT('Ctrl Pts',(1.4739892254602,1.18514270861358,11.9458686175773));
#60898=CARTESIAN_POINT('Ctrl Pts',(1.45746596251714,1.30000000000266,11.9588338438603));
#60899=CARTESIAN_POINT('Ctrl Pts',(1.22524790954672,-1.30000000000012,12.0221894989965));
#60900=CARTESIAN_POINT('Ctrl Pts',(1.25605069328636,-1.18514270861187,12.0061870364817));
#60901=CARTESIAN_POINT('Ctrl Pts',(1.2785805568903,-1.06847604194516,11.9841306379267));
#60902=CARTESIAN_POINT('Ctrl Pts',(1.31151694839366,-0.794772684000856,
11.9191901415583));
#60903=CARTESIAN_POINT('Ctrl Pts',(1.30170267453756,-0.636309800095201,
11.8519929619082));
#60904=CARTESIAN_POINT('Ctrl Pts',(1.31067734237213,-0.319434907277161,
11.7780531506376));
#60905=CARTESIAN_POINT('Ctrl Pts',(1.30454497855561,-0.158333333333333,
11.7366275268995));
#60906=CARTESIAN_POINT('Ctrl Pts',(1.33493994462557,0.158333333333335,11.727752068216));
#60907=CARTESIAN_POINT('Ctrl Pts',(1.37234701512126,0.319434907277168,11.7600336232914));
#60908=CARTESIAN_POINT('Ctrl Pts',(1.42349273638346,0.636309800095209,11.8164419034647));
#60909=CARTESIAN_POINT('Ctrl Pts',(1.46623680485781,0.794772684000844,11.8733411702764));
#60910=CARTESIAN_POINT('Ctrl Pts',(1.47816221397479,1.06847604194603,11.9264943787167));
#60911=CARTESIAN_POINT('Ctrl Pts',(1.47259511058383,1.18514270861358,11.9445849484738));
#60912=CARTESIAN_POINT('Ctrl Pts',(1.4562988360751,1.30000000000266,11.9577580335746));
#60913=CARTESIAN_POINT('Ctrl Pts',(1.22368876170903,-1.30000000000012,12.0204674403452));
#60914=CARTESIAN_POINT('Ctrl Pts',(1.25413034507549,-1.18514270861187,12.0041607583451));
#60915=CARTESIAN_POINT('Ctrl Pts',(1.27640296468573,-1.06847604194516,11.981878763065));
#60916=CARTESIAN_POINT('Ctrl Pts',(1.30898523113519,-0.794772684000856,
11.9165987274361));
#60917=CARTESIAN_POINT('Ctrl Pts',(1.29929200326749,-0.636309800095201,
11.8494347124025));
#60918=CARTESIAN_POINT('Ctrl Pts',(1.3082915033771,-0.319434907277161,11.7754685822411));
#60919=CARTESIAN_POINT('Ctrl Pts',(1.3023077506762,-0.158333333333333,11.7341262772798));
#60920=CARTESIAN_POINT('Ctrl Pts',(1.33264970510214,0.158333333333335,11.7252791534609));
#60921=CARTESIAN_POINT('Ctrl Pts',(1.36983080131772,0.319434907277169,11.7575170945062));
#60922=CARTESIAN_POINT('Ctrl Pts',(1.42089331169685,0.636309800095209,11.8139862500183));
#60923=CARTESIAN_POINT('Ctrl Pts',(1.46354419012881,0.794772684000844,11.8708458353556));
#60924=CARTESIAN_POINT('Ctrl Pts',(1.47580830789673,1.06847604194603,11.9243474423368));
#60925=CARTESIAN_POINT('Ctrl Pts',(1.47048874147005,1.18514270861358,11.9426672444924));
#60926=CARTESIAN_POINT('Ctrl Pts',(1.45454092646529,1.30000000000266,11.9561479855713));
#60927=CARTESIAN_POINT('Ctrl Pts',(1.22162818486884,-1.30000000000012,12.0181623433247));
#60928=CARTESIAN_POINT('Ctrl Pts',(1.251613764737,-1.18514270861187,12.0014380578494));
#60929=CARTESIAN_POINT('Ctrl Pts',(1.27355839427798,-1.06847604194516,11.9788482316104));
#60930=CARTESIAN_POINT('Ctrl Pts',(1.30567867468334,-0.794772684000856,
11.9131106413578));
#60931=CARTESIAN_POINT('Ctrl Pts',(1.29611619437512,-0.6363098000952,11.8460049698049));
#60932=CARTESIAN_POINT('Ctrl Pts',(1.3051245076517,-0.319434907277161,11.7720152250008));
#60933=CARTESIAN_POINT('Ctrl Pts',(1.29931487976112,-0.158333333333333,
11.7307958743874));
#60934=CARTESIAN_POINT('Ctrl Pts',(1.32958673997488,0.158333333333335,11.7219859083677));
#60935=CARTESIAN_POINT('Ctrl Pts',(1.3665072480433,0.319434907277169,11.7541449844838));
#60936=CARTESIAN_POINT('Ctrl Pts',(1.4174515111205,0.636309800095209,11.81069932319));
#60937=CARTESIAN_POINT('Ctrl Pts',(1.45992304453503,0.794772684000844,11.8675347589428));
#60938=CARTESIAN_POINT('Ctrl Pts',(1.47263148167845,1.06847604194603,11.9215047324072));
#60939=CARTESIAN_POINT('Ctrl Pts',(1.46764862113243,1.18514270861358,11.940126701114));
#60940=CARTESIAN_POINT('Ctrl Pts',(1.45218188849499,1.30000000000266,11.9540090367993));
#60941=CARTESIAN_POINT('Ctrl Pts',(1.21883413279385,-1.30000000000012,12.0149728629311));
#60942=CARTESIAN_POINT('Ctrl Pts',(1.24826042730895,-1.18514270861187,11.9976427476694));
#60943=CARTESIAN_POINT('Ctrl Pts',(1.26979427796863,-1.06847604194516,11.9746108564949));
#60944=CARTESIAN_POINT('Ctrl Pts',(1.30130865664055,-0.794772684000856,
11.9082303373725));
#60945=CARTESIAN_POINT('Ctrl Pts',(1.29185020172849,-0.636309800095201,
11.8412398015522));
#60946=CARTESIAN_POINT('Ctrl Pts',(1.30080646926028,-0.319434907277161,
11.767248042859));
#60947=CARTESIAN_POINT('Ctrl Pts',(1.29516702066596,-0.158333333333333,
11.7262319896314));
#60948=CARTESIAN_POINT('Ctrl Pts',(1.32534343698007,0.158333333333335,11.7174717384533));
#60949=CARTESIAN_POINT('Ctrl Pts',(1.36201587657113,0.319434907277169,11.7494661513915));
#60950=CARTESIAN_POINT('Ctrl Pts',(1.41278201534404,0.636309800095209,11.8061463399929));
#60951=CARTESIAN_POINT('Ctrl Pts',(1.45486644089265,0.794772684000844,11.8630221677633));
#60952=CARTESIAN_POINT('Ctrl Pts',(1.46816687496799,1.06847604194603,11.9176461708665));
#60953=CARTESIAN_POINT('Ctrl Pts',(1.46366343298579,1.18514270861358,11.9366750131029));
#60954=CARTESIAN_POINT('Ctrl Pts',(1.4488992839398,1.30000000000266,11.951087990651));
#60955=CARTESIAN_POINT('Ctrl Pts',(1.21581476102868,-1.30000000000012,12.0114782862877));
#60956=CARTESIAN_POINT('Ctrl Pts',(1.24468676622456,-1.18514270861187,11.9934610959788));
#60957=CARTESIAN_POINT('Ctrl Pts',(1.26580677376303,-1.06847604194516,11.9699308744671));
#60958=CARTESIAN_POINT('Ctrl Pts',(1.29668955084951,-0.794772684000855,
11.902835150614));
#60959=CARTESIAN_POINT('Ctrl Pts',(1.28729091458771,-0.6363098000952,11.8359950228554));
#60960=CARTESIAN_POINT('Ctrl Pts',(1.29614317182758,-0.31943490727716,11.7620236248868));
#60961=CARTESIAN_POINT('Ctrl Pts',(1.29063333737263,-0.158333333333333,
11.7212572543137));
#60962=CARTESIAN_POINT('Ctrl Pts',(1.32070432401616,0.158333333333335,11.7125508945433));
#60963=CARTESIAN_POINT('Ctrl Pts',(1.35718925414493,0.319434907277168,11.7443225736727));
#60964=CARTESIAN_POINT('Ctrl Pts',(1.40774782651833,0.636309800095208,11.8011470545255));
#60965=CARTESIAN_POINT('Ctrl Pts',(1.44930440815035,0.794772684000843,11.8581223765224));
#60966=CARTESIAN_POINT('Ctrl Pts',(1.46323198337746,1.06847604194603,11.9134697715173));
#60967=CARTESIAN_POINT('Ctrl Pts',(1.45926115161887,1.18514270861358,11.9329374893995));
#60968=CARTESIAN_POINT('Ctrl Pts',(1.44529075685338,1.30000000000266,11.9479150886937));
#60969=CARTESIAN_POINT('Ctrl Pts',(1.2127914376561,-1.30000000000012,12.0079846421543));
#60970=CARTESIAN_POINT('Ctrl Pts',(1.24110915570597,-1.18514270861187,11.9892800327384));
#60971=CARTESIAN_POINT('Ctrl Pts',(1.26181830932371,-1.06847604194516,11.9652498645401));
#60972=CARTESIAN_POINT('Ctrl Pts',(1.29208329110632,-0.794772684000854,
11.8974322626217));
#60973=CARTESIAN_POINT('Ctrl Pts',(1.28276751986128,-0.6363098000952,11.830732122404));
#60974=CARTESIAN_POINT('Ctrl Pts',(1.29153147513043,-0.31943490727716,11.7567738149627));
#60975=CARTESIAN_POINT('Ctrl Pts',(1.28615636910397,-0.158333333333333,
11.7162549003776));
#60976=CARTESIAN_POINT('Ctrl Pts',(1.31611486034211,0.158333333333335,11.7076052631193));
#60977=CARTESIAN_POINT('Ctrl Pts',(1.35238550590869,0.319434907277168,11.7391661228376));
#60978=CARTESIAN_POINT('Ctrl Pts',(1.40273614028725,0.636309800095208,11.7961339664401));
#60979=CARTESIAN_POINT('Ctrl Pts',(1.44380164635047,0.794772684000843,11.8531898499142));
#60980=CARTESIAN_POINT('Ctrl Pts',(1.45834763245817,1.06847604194603,11.9092653490168));
#60981=CARTESIAN_POINT('Ctrl Pts',(1.45489660611559,1.18514270861358,11.9291787884017));
#60982=CARTESIAN_POINT('Ctrl Pts',(1.44169813502628,1.30000000000266,11.9447326614119));
#60983=CARTESIAN_POINT('Ctrl Pts',(1.20872858075993,-1.30000000000012,12.0033407550191));
#60984=CARTESIAN_POINT('Ctrl Pts',(1.23625742321363,-1.18514270861187,11.9837420038142));
#60985=CARTESIAN_POINT('Ctrl Pts',(1.25639293334808,-1.06847604194516,11.9590567469262));
#60986=CARTESIAN_POINT('Ctrl Pts',(1.28582991316517,-0.794772684000855,
11.8902780195665));
#60987=CARTESIAN_POINT('Ctrl Pts',(1.27670502214909,-0.6363098000952,11.8237279150921));
#60988=CARTESIAN_POINT('Ctrl Pts',(1.28542646124839,-0.31943490727716,11.7497516876065));
#60989=CARTESIAN_POINT('Ctrl Pts',(1.28030515900938,-0.158333333333333,
11.709527140093));
#60990=CARTESIAN_POINT('Ctrl Pts',(1.31011045946272,0.158333333333335,11.7009544754783));
#60991=CARTESIAN_POINT('Ctrl Pts',(1.34597814359557,0.319434907277168,11.7322909617147));
#60992=CARTESIAN_POINT('Ctrl Pts',(1.39605104033275,0.636309800095208,11.7894477289245));
#60993=CARTESIAN_POINT('Ctrl Pts',(1.43658852574654,0.794772684000842,11.846544440666));
#60994=CARTESIAN_POINT('Ctrl Pts',(1.45195911272829,1.06847604194603,11.9035912069717));
#60995=CARTESIAN_POINT('Ctrl Pts',(1.44917663141501,1.18514270861358,11.9241123932074));
#60996=CARTESIAN_POINT('Ctrl Pts',(1.43695831122038,1.30000000000266,11.940461334336));
#60997=CARTESIAN_POINT('Ctrl Pts',(1.20145510658949,-1.30000000000012,11.9952901443843));
#60998=CARTESIAN_POINT('Ctrl Pts',(1.22737142220384,-1.18514270861187,11.9742330751038));
#60999=CARTESIAN_POINT('Ctrl Pts',(1.24637839959851,-1.06847604194516,11.9484584103413));
#61000=CARTESIAN_POINT('Ctrl Pts',(1.27432636621717,-0.794772684000854,
11.8780151892209));
#61001=CARTESIAN_POINT('Ctrl Pts',(1.26588617433029,-0.6363098000952,11.8115668131939));
#61002=CARTESIAN_POINT('Ctrl Pts',(1.27484109981736,-0.31943490727716,11.737414026359));
#61003=CARTESIAN_POINT('Ctrl Pts',(1.27046109361697,-0.158333333333333,
11.6975606099016));
#61004=CARTESIAN_POINT('Ctrl Pts',(1.29998168292981,0.158333333333335,11.6891312863438));
#61005=CARTESIAN_POINT('Ctrl Pts',(1.33464292223727,0.319434907277168,11.7203220298716));
#61006=CARTESIAN_POINT('Ctrl Pts',(1.38426993498686,0.636309800095208,11.7777802074196));
#61007=CARTESIAN_POINT('Ctrl Pts',(1.42450022186561,0.794772684000843,11.8346246185139));
#61008=CARTESIAN_POINT('Ctrl Pts',(1.44133915951881,1.06847604194603,11.8933588537356));
#61009=CARTESIAN_POINT('Ctrl Pts',(1.43961940851332,1.18514270861358,11.9150013498131));
#61010=CARTESIAN_POINT('Ctrl Pts',(1.42889095433638,1.30000000000266,11.9328624678583));
#61011=CARTESIAN_POINT('Ctrl Pts',(1.19312358840273,-1.30000000000012,11.986092224098));
#61012=CARTESIAN_POINT('Ctrl Pts',(1.21718649562038,-1.18514270861187,11.9633706907938));
#61013=CARTESIAN_POINT('Ctrl Pts',(1.23487329811423,-1.06847604194516,11.936363193005));
#61014=CARTESIAN_POINT('Ctrl Pts',(1.26100327266032,-0.794772684000852,
11.8640690349175));
#61015=CARTESIAN_POINT('Ctrl Pts',(1.25309742420552,-0.636309800095199,
11.7978514797918));
#61016=CARTESIAN_POINT('Ctrl Pts',(1.26234630009569,-0.31943490727716,11.723487627083));
#61017=CARTESIAN_POINT('Ctrl Pts',(1.25905343060208,-0.158333333333333,
11.6839559230984));
#61018=CARTESIAN_POINT('Ctrl Pts',(1.28845759211167,0.158333333333335,11.6755922274868));
#61019=CARTESIAN_POINT('Ctrl Pts',(1.32200304010692,0.319434907277168,11.7064777237483));
#61020=CARTESIAN_POINT('Ctrl Pts',(1.37092015971712,0.636309800095208,11.7643807875321));
#61021=CARTESIAN_POINT('Ctrl Pts',(1.40998322857041,0.794772684000842,11.8213481979597));
#61022=CARTESIAN_POINT('Ctrl Pts',(1.42851014512994,1.06847604194602,11.8820088745646));
#61023=CARTESIAN_POINT('Ctrl Pts',(1.42818966260314,1.18514270861358,11.9048416990058));
#61024=CARTESIAN_POINT('Ctrl Pts',(1.41952908186081,1.30000000000266,11.9242495886853));
#61025=CARTESIAN_POINT('Ctrl Pts',(1.18504714964652,-1.30000000000012,11.976770901141));
#61026=CARTESIAN_POINT('Ctrl Pts',(1.20752489221823,-1.18514270861186,11.9522592293794));
#61027=CARTESIAN_POINT('Ctrl Pts',(1.22409981608184,-1.06847604194516,11.9239215647813));
#61028=CARTESIAN_POINT('Ctrl Pts',(1.24875451393843,-0.79477268400085,11.84961708179));
#61029=CARTESIAN_POINT('Ctrl Pts',(1.24163979516002,-0.636309800095198,
11.7835146474624));
#61030=CARTESIAN_POINT('Ctrl Pts',(1.25083536704097,-0.31943490727716,11.7090985716443));
#61031=CARTESIAN_POINT('Ctrl Pts',(1.24776341731568,-0.158333333333333,
11.6702844395716));
#61032=CARTESIAN_POINT('Ctrl Pts',(1.27660485154415,0.158333333333334,11.662190750739));
#61033=CARTESIAN_POINT('Ctrl Pts',(1.30897301991081,0.319434907277167,11.6928095556046));
#61034=CARTESIAN_POINT('Ctrl Pts',(1.35759900979757,0.636309800095207,11.7509464000865));
#61035=CARTESIAN_POINT('Ctrl Pts',(1.39673351914396,0.794772684000841,11.8074159111043));
#61036=CARTESIAN_POINT('Ctrl Pts',(1.41683529369696,1.06847604194602,11.8700590369959));
#61037=CARTESIAN_POINT('Ctrl Pts',(1.4175582816801,1.18514270861358,11.8942602030662));
#61038=CARTESIAN_POINT('Ctrl Pts',(1.4103029442865,1.30000000000266,11.9155466471649));
#61039=CARTESIAN_POINT('Ctrl Pts',(1.173082577549,-1.30000000000012,11.9627193030931));
#61040=CARTESIAN_POINT('Ctrl Pts',(1.19325401770505,-1.18514270861186,11.9354877943743));
#61041=CARTESIAN_POINT('Ctrl Pts',(1.20817392342902,-1.06847604194516,11.9051476176419));
#61042=CARTESIAN_POINT('Ctrl Pts',(1.23050979526431,-0.794772684000851,
11.8278740948604));
#61043=CARTESIAN_POINT('Ctrl Pts',(1.22411878218085,-0.636309800095198,
11.7621572297401));
#61044=CARTESIAN_POINT('Ctrl Pts',(1.23331463099599,-0.31943490727716,11.687624974606));
#61045=CARTESIAN_POINT('Ctrl Pts',(1.23109745274161,-0.158333333333333,
11.6496486423212));
#61046=CARTESIAN_POINT('Ctrl Pts',(1.25933044141261,0.158333333333335,11.6418461038297));
#61047=CARTESIAN_POINT('Ctrl Pts',(1.28996838723369,0.319434907277169,11.672035062822));
#61048=CARTESIAN_POINT('Ctrl Pts',(1.33789861140877,0.636309800095208,11.7306432184318));
#61049=CARTESIAN_POINT('Ctrl Pts',(1.37628250493933,0.79477268400084,11.7867795523974));
#61050=CARTESIAN_POINT('Ctrl Pts',(1.39902063264288,1.06847604194602,11.8522725395376));
#61051=CARTESIAN_POINT('Ctrl Pts',(1.4016799951753,1.18514270861358,11.878353102107));
#61052=CARTESIAN_POINT('Ctrl Pts',(1.39715622728792,1.30000000000266,11.9021647398668));
#61053=CARTESIAN_POINT('Ctrl Pts',(1.15913005914174,-1.30000000000013,11.9463091067294));
#61054=CARTESIAN_POINT('Ctrl Pts',(1.17670119651856,-1.18514270861187,11.9158671500722));
#61055=CARTESIAN_POINT('Ctrl Pts',(1.18968778798641,-1.06847604194516,11.8831932196852));
#61056=CARTESIAN_POINT('Ctrl Pts',(1.20909819405085,-0.794772684000851,
11.8025535982731));
#61057=CARTESIAN_POINT('Ctrl Pts',(1.20291285503855,-0.636309800095199,
11.7375618676765));
#61058=CARTESIAN_POINT('Ctrl Pts',(1.21193377854271,-0.31943490727716,11.6629739236331));
#61059=CARTESIAN_POINT('Ctrl Pts',(1.21073094722639,-0.158333333333333,
11.6259876804447));
#61060=CARTESIAN_POINT('Ctrl Pts',(1.23896402942151,0.158333333333335,11.6181923045527));
#61061=CARTESIAN_POINT('Ctrl Pts',(1.26892852413936,0.319434907277168,11.6472300289417));
#61062=CARTESIAN_POINT('Ctrl Pts',(1.3163396743589,0.636309800095208,11.7062512946545));
#61063=CARTESIAN_POINT('Ctrl Pts',(1.3530093507216,0.794772684000842,11.7624106275473));
#61064=CARTESIAN_POINT('Ctrl Pts',(1.37814864427987,1.06847604194603,11.8315494906404));
#61065=CARTESIAN_POINT('Ctrl Pts',(1.38276042254293,1.18514270861358,11.8599659305594));
#61066=CARTESIAN_POINT('Ctrl Pts',(1.38110211039027,1.30000000000266,11.8868711584118));
#61067=CARTESIAN_POINT('Ctrl Pts',(1.14519361629814,-1.30000000000012,11.9298776634644));
#61068=CARTESIAN_POINT('Ctrl Pts',(1.15988682778115,-1.18514270861187,11.8963267159581));
#61069=CARTESIAN_POINT('Ctrl Pts',(1.17096728411276,-1.06847604194516,11.8612936567873));
#61070=CARTESIAN_POINT('Ctrl Pts',(1.18821916774755,-0.794772684000851,
11.7769363073234));
#61071=CARTESIAN_POINT('Ctrl Pts',(1.18437105667397,-0.636309800095198,
11.7117553462717));
#61072=CARTESIAN_POINT('Ctrl Pts',(1.19382220937109,-0.319434907277159,
11.6368413175492));
#61073=CARTESIAN_POINT('Ctrl Pts',(1.19296893064302,-0.158333333333333,
11.6011157302902));
#61074=CARTESIAN_POINT('Ctrl Pts',(1.22009217020531,0.158333333333334,11.5938150571528));
#61075=CARTESIAN_POINT('Ctrl Pts',(1.24804529143141,0.319434907277168,11.6223032872997));
#61076=CARTESIAN_POINT('Ctrl Pts',(1.29388988291989,0.636309800095208,11.6822174003226));
#61077=CARTESIAN_POINT('Ctrl Pts',(1.3285254716536,0.794772684000839,11.7385634639138));
#61078=CARTESIAN_POINT('Ctrl Pts',(1.35638827104748,1.06847604194602,11.8112107840679));
#61079=CARTESIAN_POINT('Ctrl Pts',(1.36332864649763,1.18514270861358,11.8417941355254));
#61080=CARTESIAN_POINT('Ctrl Pts',(1.36514862395873,1.30000000000266,11.8715145053942));
#61081=CARTESIAN_POINT('Ctrl Pts',(1.13751282886348,-1.30000000000012,11.9203535763013));
#61082=CARTESIAN_POINT('Ctrl Pts',(1.15107565576836,-1.18514270861187,11.8848081665791));
#61083=CARTESIAN_POINT('Ctrl Pts',(1.16125632286343,-1.06847604194516,11.8483479199077));
#61084=CARTESIAN_POINT('Ctrl Pts',(1.17696223472908,-0.794772684000853,
11.7620039998844));
#61085=CARTESIAN_POINT('Ctrl Pts',(1.17261396792746,-0.636309800095199,
11.697502731694));
#61086=CARTESIAN_POINT('Ctrl Pts',(1.18193573939001,-0.31943490727716,11.6225658847503));
#61087=CARTESIAN_POINT('Ctrl Pts',(1.18202816633933,-0.158333333333333,
11.5872503591164));
#61088=CARTESIAN_POINT('Ctrl Pts',(1.20932211372468,0.158333333333335,11.579872933071));
#61089=CARTESIAN_POINT('Ctrl Pts',(1.23678302590977,0.319434907277168,11.6077476966413));
#61090=CARTESIAN_POINT('Ctrl Pts',(1.28252869772572,0.636309800095208,11.6677862688316));
#61091=CARTESIAN_POINT('Ctrl Pts',(1.31664043959854,0.794772684000841,11.7238947651359));
#61092=CARTESIAN_POINT('Ctrl Pts',(1.34583653283923,1.06847604194602,11.7986518965237));
#61093=CARTESIAN_POINT('Ctrl Pts',(1.35375920212431,1.18514270861358,11.8306470269596));
#61094=CARTESIAN_POINT('Ctrl Pts',(1.35696663375241,1.30000000000266,11.8622776956782));
#61095=CARTESIAN_POINT('Ctrl Pts',(1.1259503820225,-1.30000000000012,11.9060906586386));
#61096=CARTESIAN_POINT('Ctrl Pts',(1.13752129822288,-1.18514270861187,11.8676764365745));
#61097=CARTESIAN_POINT('Ctrl Pts',(1.14627996941706,-1.06847604194516,11.8291030294281));
#61098=CARTESIAN_POINT('Ctrl Pts',(1.16001740348972,-0.794772684000853,
11.7396229929514));
#61099=CARTESIAN_POINT('Ctrl Pts',(1.15622634367563,-0.636309800095199,
11.6755780491627));
#61100=CARTESIAN_POINT('Ctrl Pts',(1.16583292808979,-0.31943490727716,11.6004014894004));
#61101=CARTESIAN_POINT('Ctrl Pts',(1.16739699622653,-0.158333333333333,
11.5656741781615));
#61102=CARTESIAN_POINT('Ctrl Pts',(1.19388648139649,0.158333333333335,11.5586551791307));
#61103=CARTESIAN_POINT('Ctrl Pts',(1.21868580967463,0.319434907277168,11.5864612973334));
#61104=CARTESIAN_POINT('Ctrl Pts',(1.26329323296083,0.636309800095208,11.6471414376856));
#61105=CARTESIAN_POINT('Ctrl Pts',(1.29710575820313,0.794772684000841,11.7027114515257));
#61106=CARTESIAN_POINT('Ctrl Pts',(1.32847580086383,1.06847604194602,11.7805544638185));
#61107=CARTESIAN_POINT('Ctrl Pts',(1.33798892842302,1.18514270861358,11.8146061751362));
#61108=CARTESIAN_POINT('Ctrl Pts',(1.34343625444816,1.30000000000266,11.8490142421176));
#61109=CARTESIAN_POINT('Ctrl Pts',(1.10885180968865,-1.30000000000012,11.8845870085044));
#61110=CARTESIAN_POINT('Ctrl Pts',(1.11709245468514,-1.18514270861186,11.8420002941912));
#61111=CARTESIAN_POINT('Ctrl Pts',(1.12356110285849,-1.06847604194516,11.8003158606242));
#61112=CARTESIAN_POINT('Ctrl Pts',(1.13441130703938,-0.794772684000849,
11.7061009291664));
#61113=CARTESIAN_POINT('Ctrl Pts',(1.13255043658639,-0.636309800095197,
11.6423045232017));
#61114=CARTESIAN_POINT('Ctrl Pts',(1.14245569830209,-0.319434907277159,
11.5668278190085));
#61115=CARTESIAN_POINT('Ctrl Pts',(1.1445785018066,-0.158333333333333,11.5336865077498));
#61116=CARTESIAN_POINT('Ctrl Pts',(1.17055816770753,0.158333333333334,11.5268703358465));
#61117=CARTESIAN_POINT('Ctrl Pts',(1.19430857035661,0.319434907277168,11.5532479824523));
#61118=CARTESIAN_POINT('Ctrl Pts',(1.23753886832307,0.636309800095207,11.6147336817711));
#61119=CARTESIAN_POINT('Ctrl Pts',(1.26836862766871,0.794772684000839,11.6706300949674));
#61120=CARTESIAN_POINT('Ctrl Pts',(1.30243416626119,1.06847604194602,11.7533592151628));
#61121=CARTESIAN_POINT('Ctrl Pts',(1.31442308574661,1.18514270861358,11.7904591111974));
#61122=CARTESIAN_POINT('Ctrl Pts',(1.3236552153133,1.30000000000266,11.8288485325497));
#61123=CARTESIAN_POINT('Ctrl Pts',(1.08716165682342,-1.30000000000012,11.8554460453488));
#61124=CARTESIAN_POINT('Ctrl Pts',(1.09163461330749,-1.18514270861186,11.8070094617491));
#61125=CARTESIAN_POINT('Ctrl Pts',(1.09539864499635,-1.06847604194516,11.7610253698515));
#61126=CARTESIAN_POINT('Ctrl Pts',(1.10245655309274,-0.794772684000854,
11.6604586649336));
#61127=CARTESIAN_POINT('Ctrl Pts',(1.10147273423353,-0.6363098000952,11.5976855395406));
#61128=CARTESIAN_POINT('Ctrl Pts',(1.11195971100687,-0.319434907277161,
11.521728456344));
#61129=CARTESIAN_POINT('Ctrl Pts',(1.11670449593826,-0.158333333333333,
11.4899360422753));
#61130=CARTESIAN_POINT('Ctrl Pts',(1.14205338335703,0.158333333333334,11.4833662346199));
#61131=CARTESIAN_POINT('Ctrl Pts',(1.16250208920525,0.319434907277166,11.5086383759976));
#61132=CARTESIAN_POINT('Ctrl Pts',(1.20396550268856,0.636309800095206,11.5711123348862));
#61133=CARTESIAN_POINT('Ctrl Pts',(1.23302071493999,0.794772684000843,11.6264001209399));
#61134=CARTESIAN_POINT('Ctrl Pts',(1.27061175970696,1.06847604194603,11.7156785368982));
#61135=CARTESIAN_POINT('Ctrl Pts',(1.28542248019329,1.18514270861358,11.7570763750097));
#61136=CARTESIAN_POINT('Ctrl Pts',(1.29877215077176,1.30000000000266,11.8012267330557));
#61137=CARTESIAN_POINT('Ctrl Pts',(1.06841695418305,-1.30000000000012,11.8313959298598));
#61138=CARTESIAN_POINT('Ctrl Pts',(1.06988891972052,-1.18514270861186,11.7780452189972));
#61139=CARTESIAN_POINT('Ctrl Pts',(1.07167056824593,-1.06847604194516,11.7283836920636));
#61140=CARTESIAN_POINT('Ctrl Pts',(1.07650196241119,-0.79477268400085,11.6221783829878));
#61141=CARTESIAN_POINT('Ctrl Pts',(1.07780198175782,-0.636309800095199,
11.5596463462105));
#61142=CARTESIAN_POINT('Ctrl Pts',(1.08914618742764,-0.319434907277161,
11.4831627993829));
#61143=CARTESIAN_POINT('Ctrl Pts',(1.0950312567616,-0.158333333333333,11.4529425339032));
#61144=CARTESIAN_POINT('Ctrl Pts',(1.11950704521747,0.158333333333335,11.4466974187544));
#61145=CARTESIAN_POINT('Ctrl Pts',(1.13785291367085,0.319434907277167,11.4707104453756));
#61146=CARTESIAN_POINT('Ctrl Pts',(1.17686286995234,0.636309800095208,11.5343959910323));
#61147=CARTESIAN_POINT('Ctrl Pts',(1.20210874432592,0.794772684000843,11.5902004428271));
#61148=CARTESIAN_POINT('Ctrl Pts',(1.24225934619864,1.06847604194603,11.685077607433));
#61149=CARTESIAN_POINT('Ctrl Pts',(1.2597239735542,1.18514270861358,11.7299119855198));
#61150=CARTESIAN_POINT('Ctrl Pts',(1.27727352044097,1.30000000000266,11.7785119326807));
#61151=CARTESIAN_POINT('Ctrl Pts',(1.05531692441144,-1.30000000000012,11.8114079524742));
#61152=CARTESIAN_POINT('Ctrl Pts',(1.0546407111963,-1.18514270861186,11.7539943304867));
#61153=CARTESIAN_POINT('Ctrl Pts',(1.05493059994745,-1.06847604194516,11.7013319032987));
#61154=CARTESIAN_POINT('Ctrl Pts',(1.05783218976483,-0.794772684000854,
11.5906473718717));
#61155=CARTESIAN_POINT('Ctrl Pts',(1.06027950848901,-0.636309800095201,
11.5286058085701));
#61156=CARTESIAN_POINT('Ctrl Pts',(1.07171063351252,-0.319434907277162,
11.4519220537149));
#61157=CARTESIAN_POINT('Ctrl Pts',(1.07811630542711,-0.158333333333333,
11.423080293972));
#61158=CARTESIAN_POINT('Ctrl Pts',(1.10178790521326,0.158333333333335,11.4171187681031));
#61159=CARTESIAN_POINT('Ctrl Pts',(1.11847728742668,0.319434907277166,11.4401420173214));
#61160=CARTESIAN_POINT('Ctrl Pts',(1.15643788874875,0.636309800095207,11.5043912612665));
#61161=CARTESIAN_POINT('Ctrl Pts',(1.18059788257868,0.794772684000845,11.5597062750224));
#61162=CARTESIAN_POINT('Ctrl Pts',(1.2227287743895,1.06847604194603,11.6591153862637));
#61163=CARTESIAN_POINT('Ctrl Pts',(1.24180134488315,1.18514270861358,11.7069489676139));
#61164=CARTESIAN_POINT('Ctrl Pts',(1.26170958390887,1.30000000000266,11.7595856095285));
#61165=CARTESIAN_POINT('Ctrl Pts',(1.0397243972048,-1.30000000000012,11.7892518976244));
#61166=CARTESIAN_POINT('Ctrl Pts',(1.03645879285365,-1.18514270861186,11.7273595872148));
#61167=CARTESIAN_POINT('Ctrl Pts',(1.03505188828116,-1.06847604194516,11.6713483817551));
#61168=CARTESIAN_POINT('Ctrl Pts',(1.0360956255887,-0.794772684000855,11.5555378210857));
#61169=CARTESIAN_POINT('Ctrl Pts',(1.04032196354068,-0.636309800095198,
11.4938500836594));
#61170=CARTESIAN_POINT('Ctrl Pts',(1.0531486514601,-0.319434907277158,11.416480256983));
#61171=CARTESIAN_POINT('Ctrl Pts',(1.06190772064469,-0.158333333333333,
11.38857937633));
#61172=CARTESIAN_POINT('Ctrl Pts',(1.0849067419774,0.158333333333334,11.3828389576133));
#61173=CARTESIAN_POINT('Ctrl Pts',(1.09837768607963,0.319434907277168,11.4051781230188));
#61174=CARTESIAN_POINT('Ctrl Pts',(1.13396476264952,0.636309800095207,11.4704911239939));
#61175=CARTESIAN_POINT('Ctrl Pts',(1.15604748076304,0.79477268400084,11.5256381923072));
#61176=CARTESIAN_POINT('Ctrl Pts',(1.19990113065527,1.06847604194602,11.6303206238347));
#61177=CARTESIAN_POINT('Ctrl Pts',(1.22073684896087,1.18514270861357,11.6815257532195));
#61178=CARTESIAN_POINT('Ctrl Pts',(1.24342566547151,1.30000000000265,11.738622866247));
#61179=CARTESIAN_POINT('Ctrl Pts',(1.02334846451551,-1.30000000000012,11.7642300009282));
#61180=CARTESIAN_POINT('Ctrl Pts',(1.01762825135153,-1.18514270861186,11.6971517312257));
#61181=CARTESIAN_POINT('Ctrl Pts',(1.01469621959795,-1.06847604194516,11.6372540829325));
#61182=CARTESIAN_POINT('Ctrl Pts',(1.01436389652807,-0.794772684000856,
11.5154672048252));
#61183=CARTESIAN_POINT('Ctrl Pts',(1.0215444001965,-0.636309800095199,11.4538984689758));
#61184=CARTESIAN_POINT('Ctrl Pts',(1.03490484456462,-0.319434907277159,
11.3761250793631));
#61185=CARTESIAN_POINT('Ctrl Pts',(1.04325944749601,-0.158333333333333,
11.3503042370641));
#61186=CARTESIAN_POINT('Ctrl Pts',(1.0650830312482,0.158333333333334,11.3449301805328));
#61187=CARTESIAN_POINT('Ctrl Pts',(1.07733643050619,0.319434907277167,11.365653493038));
#61188=CARTESIAN_POINT('Ctrl Pts',(1.11090510700976,0.636309800095207,11.4319170513878));
#61189=CARTESIAN_POINT('Ctrl Pts',(1.12960436174885,0.794772684000841,11.4872553750911));
#61190=CARTESIAN_POINT('Ctrl Pts',(1.17546572258528,1.06847604194602,11.5977926535385));
#61191=CARTESIAN_POINT('Ctrl Pts',(1.19846922681292,1.18514270861357,11.6526905755081));
#61192=CARTESIAN_POINT('Ctrl Pts',(1.22462455149293,1.30000000000266,11.714638927417));
#61193=CARTESIAN_POINT('Ctrl Pts',(1.00703467199694,-1.30000000000012,11.739219370099));
#61194=CARTESIAN_POINT('Ctrl Pts',(0.999134719940811,-1.18514270861186,
11.6669388808963));
#61195=CARTESIAN_POINT('Ctrl Pts',(0.994917017441277,-1.06847604194516,
11.603134999775));
#61196=CARTESIAN_POINT('Ctrl Pts',(0.993680014026088,-0.794772684000856,
11.4753179308695));
#61197=CARTESIAN_POINT('Ctrl Pts',(1.00356933560391,-0.636309800095199,
11.4139753193718));
#61198=CARTESIAN_POINT('Ctrl Pts',(1.0186375465584,-0.31943490727716,11.3354321895726));
#61199=CARTESIAN_POINT('Ctrl Pts',(1.02865194271522,-0.158333333333333,
11.3109890627905));
#61200=CARTESIAN_POINT('Ctrl Pts',(1.04965946900603,0.158333333333334,11.3058310424178));
#61201=CARTESIAN_POINT('Ctrl Pts',(1.05908788074018,0.319434907277167,11.3254614994301));
#61202=CARTESIAN_POINT('Ctrl Pts',(1.08999770696503,0.636309800095207,11.3927946588076));
#61203=CARTESIAN_POINT('Ctrl Pts',(1.10608353727842,0.794772684000843,11.4479350054623));
#61204=CARTESIAN_POINT('Ctrl Pts',(1.15295974013333,1.06847604194602,11.5645997130572));
#61205=CARTESIAN_POINT('Ctrl Pts',(1.17739635454459,1.18514270861357,11.6234322688973));
#61206=CARTESIAN_POINT('Ctrl Pts',(1.20597861208563,1.30000000000265,11.6905975515131));
#61207=CARTESIAN_POINT('Ctrl Pts',(0.996639789377811,-1.30000000000012,
11.7212674543398));
#61208=CARTESIAN_POINT('Ctrl Pts',(0.987178980341047,-1.18514270861186,
11.6452064782541));
#61209=CARTESIAN_POINT('Ctrl Pts',(0.982115189660983,-1.06847604194516,
11.5785418109598));
#61210=CARTESIAN_POINT('Ctrl Pts',(0.980574812206666,-0.794772684000854,
11.4462404463224));
#61211=CARTESIAN_POINT('Ctrl Pts',(0.993894584228217,-0.636309800095199,
11.38460189545));
#61212=CARTESIAN_POINT('Ctrl Pts',(1.00877894511221,-0.31943490727716,11.3059524142012));
#61213=CARTESIAN_POINT('Ctrl Pts',(1.01600681948604,-0.158333333333333,
11.2837759476425));
#61214=CARTESIAN_POINT('Ctrl Pts',(1.03581728561432,0.158333333333335,11.2789554106594));
#61215=CARTESIAN_POINT('Ctrl Pts',(1.04621763664454,0.319434907277168,11.2968028614693));
#61216=CARTESIAN_POINT('Ctrl Pts',(1.07613083609169,0.636309800095208,11.3646320626102));
#61217=CARTESIAN_POINT('Ctrl Pts',(1.08939609589899,0.794772684000843,11.4199880656248));
#61218=CARTESIAN_POINT('Ctrl Pts',(1.13689333586009,1.06847604194602,11.5411468399775));
#61219=CARTESIAN_POINT('Ctrl Pts',(1.16238177307412,1.18514270861357,11.6028236320556));
#61220=CARTESIAN_POINT('Ctrl Pts',(1.19279885226912,1.30000000000265,11.6737320721692));
#61221=CARTESIAN_POINT('Ctrl Pts',(0.988936150867084,-1.30000000000012,
11.7086498444924));
#61222=CARTESIAN_POINT('Ctrl Pts',(0.979260374531466,-1.18514270861186,
11.6298092175276));
#61223=CARTESIAN_POINT('Ctrl Pts',(0.97386258527909,-1.06847604194516,11.5611758706455));
#61224=CARTESIAN_POINT('Ctrl Pts',(0.971275618252736,-0.794772684000855,
11.4261999682441));
#61225=CARTESIAN_POINT('Ctrl Pts',(0.98322860322658,-0.636309800095198,
11.365581526662));
#61226=CARTESIAN_POINT('Ctrl Pts',(0.997261739605961,-0.319434907277158,
11.2871729392513));
#61227=CARTESIAN_POINT('Ctrl Pts',(1.00439654953326,-0.158333333333333,
11.2660209705762));
#61228=CARTESIAN_POINT('Ctrl Pts',(1.02475591643617,0.158333333333334,11.2610046392375));
#61229=CARTESIAN_POINT('Ctrl Pts',(1.03661944501925,0.319434907277167,11.2773588457922));
#61230=CARTESIAN_POINT('Ctrl Pts',(1.06682918993637,0.636309800095207,11.3451043176933));
#61231=CARTESIAN_POINT('Ctrl Pts',(1.07845024126375,0.79477268400084,11.4003959078489));
#61232=CARTESIAN_POINT('Ctrl Pts',(1.12663667854303,1.06847604194602,11.5243786857344));
#61233=CARTESIAN_POINT('Ctrl Pts',(1.15286519959577,1.18514270861357,11.5879206634263));
#61234=CARTESIAN_POINT('Ctrl Pts',(1.18446411848644,1.30000000000265,11.6613370682779));
#61235=CARTESIAN_POINT('Ctrl Pts',(0.980511229803926,-1.30000000000012,
11.6930945208311));
#61236=CARTESIAN_POINT('Ctrl Pts',(0.970473519190732,-1.18514270861186,
11.6105616290021));
#61237=CARTESIAN_POINT('Ctrl Pts',(0.96440575931758,-1.06847604194516,11.5393409241277));
#61238=CARTESIAN_POINT('Ctrl Pts',(0.959559400554817,-0.794772684000853,
11.4009402630753));
#61239=CARTESIAN_POINT('Ctrl Pts',(0.968435802254349,-0.636309800095197,
11.3418765139652));
#61240=CARTESIAN_POINT('Ctrl Pts',(0.980362066338188,-0.319434907277159,
11.2639606380389));
#61241=CARTESIAN_POINT('Ctrl Pts',(0.987534292221185,-0.158333333333333,
11.2441157359081));
#61242=CARTESIAN_POINT('Ctrl Pts',(1.00779765629327,0.158333333333334,11.2391069268715));
#61243=CARTESIAN_POINT('Ctrl Pts',(1.01985751736349,0.319434907277167,11.2540357236247));
#61244=CARTESIAN_POINT('Ctrl Pts',(1.05130690412056,0.636309800095206,11.321560185511));
#61245=CARTESIAN_POINT('Ctrl Pts',(1.06416712157485,0.794772684000839,11.3759106179189));
#61246=CARTESIAN_POINT('Ctrl Pts',(1.11442040326315,1.06847604194602,11.5034399801553));
#61247=CARTESIAN_POINT('Ctrl Pts',(1.14163565378195,1.18514270861357,11.5695028885468));
#61248=CARTESIAN_POINT('Ctrl Pts',(1.17431337124421,1.30000000000266,11.6464259698462));
#61249=CARTESIAN_POINT('Ctrl Pts',(0.974665092423404,-1.30000000000011,
11.682537481278));
#61250=CARTESIAN_POINT('Ctrl Pts',(0.96568220521313,-1.18514270861186,11.5970539055789));
#61251=CARTESIAN_POINT('Ctrl Pts',(0.959681817346747,-1.06847604194516,
11.523988601927));
#61252=CARTESIAN_POINT('Ctrl Pts',(0.952709891133254,-0.794772684000851,
11.3838818265229));
#61253=CARTESIAN_POINT('Ctrl Pts',(0.955698270378833,-0.636309800095197,
11.3278245114625));
#61254=CARTESIAN_POINT('Ctrl Pts',(0.964465402259398,-0.319434907277159,
11.2513908870651));
#61255=CARTESIAN_POINT('Ctrl Pts',(0.972209900210545,-0.158333333333333,
11.2324665018759));
#61256=CARTESIAN_POINT('Ctrl Pts',(0.992336747193892,0.158333333333334,
11.2275421126342));
#61257=CARTESIAN_POINT('Ctrl Pts',(1.00385002392356,0.319434907277167,11.2416493150689));
#61258=CARTESIAN_POINT('Ctrl Pts',(1.03785006787198,0.636309800095206,11.3078339412536));
#61259=CARTESIAN_POINT('Ctrl Pts',(1.05542731230797,0.79477268400084,11.3592791978235));
#61260=CARTESIAN_POINT('Ctrl Pts',(1.10785601153169,1.06847604194602,11.4885093112117));
#61261=CARTESIAN_POINT('Ctrl Pts',(1.13532397903559,1.18514270861357,11.5563795755177));
#61262=CARTESIAN_POINT('Ctrl Pts',(1.16756547282411,1.30000000000265,11.6361811764914));
#61263=CARTESIAN_POINT('Ctrl Pts',(0.96840887762859,-1.30000000000011,11.6766336368645));
#61264=CARTESIAN_POINT('Ctrl Pts',(0.959587680307159,-1.18514270861186,
11.5913424478649));
#61265=CARTESIAN_POINT('Ctrl Pts',(0.953418388257846,-1.06847604194516,
11.5185778056402));
#61266=CARTESIAN_POINT('Ctrl Pts',(0.945292521151707,-0.794772684000851,
11.3794157545617));
#61267=CARTESIAN_POINT('Ctrl Pts',(0.946012577561581,-0.636309800095197,
11.3245575119393));
#61268=CARTESIAN_POINT('Ctrl Pts',(0.953320013133084,-0.319434907277159,
11.248968780158));
#61269=CARTESIAN_POINT('Ctrl Pts',(0.961064002623636,-0.158333333333333,
11.2299920510673));
#61270=CARTESIAN_POINT('Ctrl Pts',(0.980997609539021,0.158333333333334,
11.2252045756181));
#61271=CARTESIAN_POINT('Ctrl Pts',(0.992074216468527,0.319434907277167,
11.2396386228234));
#61272=CARTESIAN_POINT('Ctrl Pts',(1.0276372251559,0.636309800095206,11.3049769849608));
#61273=CARTESIAN_POINT('Ctrl Pts',(1.04845566442809,0.79477268400084,11.3547455720355));
#61274=CARTESIAN_POINT('Ctrl Pts',(1.10189571121762,1.06847604194602,11.4830880756333));
#61275=CARTESIAN_POINT('Ctrl Pts',(1.12924033300978,1.18514270861357,11.5507878560718));
#61276=CARTESIAN_POINT('Ctrl Pts',(1.16079736048771,1.30000000000265,11.6306327026994));
#61277=CARTESIAN_POINT('Ctrl Pts',(0.968408877628581,-1.3,11.6766336368644));
#61278=CARTESIAN_POINT('Ctrl Pts',(0.959587680307155,-1.18514270861178,
11.5913424478648));
#61279=CARTESIAN_POINT('Ctrl Pts',(0.953418388257844,-1.06847604194512,
11.5185778056402));
#61280=CARTESIAN_POINT('Ctrl Pts',(0.945292521151707,-0.794772684000851,
11.3794157545617));
#61281=CARTESIAN_POINT('Ctrl Pts',(0.946012577561581,-0.636309800095197,
11.3245575119393));
#61282=CARTESIAN_POINT('Ctrl Pts',(0.953320013133084,-0.319434907277159,
11.248968780158));
#61283=CARTESIAN_POINT('Ctrl Pts',(0.961064002623637,-0.158333333333332,
11.2299920510673));
#61284=CARTESIAN_POINT('Ctrl Pts',(0.980997609539021,0.158333333333334,
11.2252045756181));
#61285=CARTESIAN_POINT('Ctrl Pts',(0.992074216468527,0.319434907277167,
11.2396386228234));
#61286=CARTESIAN_POINT('Ctrl Pts',(1.0276372251559,0.636309800095206,11.3049769849608));
#61287=CARTESIAN_POINT('Ctrl Pts',(1.04845566442809,0.79477268400084,11.3547455720355));
#61288=CARTESIAN_POINT('Ctrl Pts',(1.10189571121744,1.06847604194511,11.4830880756329));
#61289=CARTESIAN_POINT('Ctrl Pts',(1.12924033300936,1.18514270861178,11.5507878560707));
#61290=CARTESIAN_POINT('Ctrl Pts',(1.16079736048698,1.3,11.6306327026976));
#61291=CARTESIAN_POINT('',(1.23747338465645,-1.2,11.992823762905));
#61292=CARTESIAN_POINT('Ctrl Pts',(1.23747338465645,-1.2,11.992823762905));
#61293=CARTESIAN_POINT('Ctrl Pts',(1.22202142463578,-1.21504261691669,11.9812774246274));
#61294=CARTESIAN_POINT('Ctrl Pts',(1.22101763652485,-1.21547066370301,11.9810846963363));
#61295=CARTESIAN_POINT('Ctrl Pts',(1.20114420805669,-1.23406682102662,11.9669384589505));
#61296=CARTESIAN_POINT('Ctrl Pts',(1.19879977037005,-1.23640407488411,11.9651259639072));
#61297=CARTESIAN_POINT('Ctrl Pts',(1.16489618114301,-1.2694151087703,11.939553996061));
#61298=CARTESIAN_POINT('Ctrl Pts',(1.15239439192118,-1.28140639977682,11.9302651952717));
#61299=CARTESIAN_POINT('Ctrl Pts',(1.13369207118163,-1.30000000000012,11.91563805733));
#61300=CARTESIAN_POINT('',(1.38832545964766,-0.653834841418303,11.9513211234181));
#61301=CARTESIAN_POINT('Ctrl Pts',(1.38832545965232,-0.653834841417626,
11.9513211234436));
#61302=CARTESIAN_POINT('Ctrl Pts',(1.3726639062272,-0.718140327968288,11.9558973945044));
#61303=CARTESIAN_POINT('Ctrl Pts',(1.36006904497293,-0.763507044235833,
11.9595163718063));
#61304=CARTESIAN_POINT('Ctrl Pts',(1.310095733821,-0.949792418009667,11.9736128203625));
#61305=CARTESIAN_POINT('Ctrl Pts',(1.28314643916662,-1.04824234463106,11.9810313014776));
#61306=CARTESIAN_POINT('Ctrl Pts',(1.23747338465645,-1.2,11.992823762905));
#61307=CARTESIAN_POINT('',(1.52166805320867,0.653834841531101,11.9103106411196));
#61308=CARTESIAN_POINT('Ctrl Pts',(1.5216680532087,0.653834841531103,11.9103106411196));
#61309=CARTESIAN_POINT('Ctrl Pts',(1.49334701587912,0.575791054272758,11.8797380243135));
#61310=CARTESIAN_POINT('Ctrl Pts',(1.46910678427171,0.493913072109036,11.8545837028923));
#61311=CARTESIAN_POINT('Ctrl Pts',(1.43214296547969,0.338189409403288,11.8198918513023));
#61312=CARTESIAN_POINT('Ctrl Pts',(1.41825074992248,0.26570323421117,11.8085823585735));
#61313=CARTESIAN_POINT('Ctrl Pts',(1.39691398424971,0.129735728132282,11.7967274120108));
#61314=CARTESIAN_POINT('Ctrl Pts',(1.38884807661025,0.066638383369331,11.7948419035998));
#61315=CARTESIAN_POINT('Ctrl Pts',(1.37599207798182,-0.0595481201416573,
11.7984066861682));
#61316=CARTESIAN_POINT('Ctrl Pts',(1.3710999037416,-0.1227920732973,11.8038677116978));
#61317=CARTESIAN_POINT('Ctrl Pts',(1.3647527081023,-0.260144682905592,11.823615105641));
#61318=CARTESIAN_POINT('Ctrl Pts',(1.36408444680164,-0.333946167126978,
11.8393299926389));
#61319=CARTESIAN_POINT('Ctrl Pts',(1.36961150358366,-0.491143170270118,
11.8838155733034));
#61320=CARTESIAN_POINT('Ctrl Pts',(1.37686564932431,-0.574255514599531,
11.9145159732068));
#61321=CARTESIAN_POINT('Ctrl Pts',(1.3883254596101,-0.653834841429858,11.9513211234048));
#61322=CARTESIAN_POINT('Ctrl Pts',(1.45281637526615,1.20000000018694,11.9320000612594));
#61323=CARTESIAN_POINT('Ctrl Pts',(1.46460429832537,1.13482355934137,11.9283809388103));
#61324=CARTESIAN_POINT('Ctrl Pts',(1.48025049117954,1.03875021853169,11.9235272221373));
#61325=CARTESIAN_POINT('Ctrl Pts',(1.51065417803845,0.795063418652971,11.9138728568002));
#61326=CARTESIAN_POINT('Ctrl Pts',(1.51542476738704,0.741568492646493,11.912327537521));
#61327=CARTESIAN_POINT('Ctrl Pts',(1.5216680532087,0.653834841531106,11.9103106411195));
#61328=CARTESIAN_POINT('Ctrl Pts',(0.968408877628581,-1.3,11.6766336368644));
#61329=CARTESIAN_POINT('Ctrl Pts',(0.959587680307155,-1.18514270861178,
11.5913424478648));
#61330=CARTESIAN_POINT('Ctrl Pts',(0.953418388257845,-1.06847604194512,
11.5185778056402));
#61331=CARTESIAN_POINT('Ctrl Pts',(0.945292521151707,-0.794772684000851,
11.3794157545617));
#61332=CARTESIAN_POINT('Ctrl Pts',(0.946012577561581,-0.636309800095197,
11.3245575119393));
#61333=CARTESIAN_POINT('Ctrl Pts',(0.953320013133084,-0.319434907277159,
11.248968780158));
#61334=CARTESIAN_POINT('Ctrl Pts',(0.961064002623636,-0.158333333333332,
11.2299920510673));
#61335=CARTESIAN_POINT('Ctrl Pts',(0.980997609539021,0.158333333333334,
11.2252045756181));
#61336=CARTESIAN_POINT('Ctrl Pts',(0.992074216468527,0.319434907277167,
11.2396386228234));
#61337=CARTESIAN_POINT('Ctrl Pts',(1.0276372251559,0.636309800095206,11.3049769849608));
#61338=CARTESIAN_POINT('Ctrl Pts',(1.04845566442809,0.79477268400084,11.3547455720355));
#61339=CARTESIAN_POINT('Ctrl Pts',(1.10189571121744,1.06847604194511,11.4830880756329));
#61340=CARTESIAN_POINT('Ctrl Pts',(1.12924033300936,1.18514270861178,11.5507878560707));
#61341=CARTESIAN_POINT('Ctrl Pts',(1.16079736048698,1.3,11.6306327026976));
#61342=CARTESIAN_POINT('Ctrl Pts',(0.892825757179277,-1.3,11.6909968251522));
#61343=CARTESIAN_POINT('Ctrl Pts',(0.885729277039985,-1.18514270861178,
11.6055436003612));
#61344=CARTESIAN_POINT('Ctrl Pts',(0.880764606872679,-1.06847604194512,
11.5327108766861));
#61345=CARTESIAN_POINT('Ctrl Pts',(0.874220133109747,-0.794772684000851,
11.3936085971602));
#61346=CARTESIAN_POINT('Ctrl Pts',(0.874292131581309,-0.636309800095197,
11.3390586058255));
#61347=CARTESIAN_POINT('Ctrl Pts',(0.881134728284516,-0.319434907277159,
11.2639480037341));
#61348=CARTESIAN_POINT('Ctrl Pts',(0.88771343062497,-0.158333333333332,
11.2453997109473));
#61349=CARTESIAN_POINT('Ctrl Pts',(0.907721667816888,0.158333333333334,
11.2409633433442));
#61350=CARTESIAN_POINT('Ctrl Pts',(0.920037078273241,0.319434907277167,
11.2553148216052));
#61351=CARTESIAN_POINT('Ctrl Pts',(0.956219211262304,0.636309800095206,
11.3209009099481));
#61352=CARTESIAN_POINT('Ctrl Pts',(0.977755058014351,0.79477268400084,11.3706875096762));
#61353=CARTESIAN_POINT('Ctrl Pts',(1.02977474137891,1.06847604194511,11.4997278279237));
#61354=CARTESIAN_POINT('Ctrl Pts',(1.0559911951017,1.18514270861178,11.5678553767222));
#61355=CARTESIAN_POINT('Ctrl Pts',(1.08590670913801,1.3,11.6482537019647));
#61356=CARTESIAN_POINT('Ctrl Pts',(0.817242636729973,-1.3,11.70536001344));
#61357=CARTESIAN_POINT('Ctrl Pts',(0.811870873772815,-1.18514270861178,
11.6197447528576));
#61358=CARTESIAN_POINT('Ctrl Pts',(0.808110825487514,-1.06847604194512,
11.5468439477319));
#61359=CARTESIAN_POINT('Ctrl Pts',(0.803147745067786,-0.794772684000851,
11.4078014397586));
#61360=CARTESIAN_POINT('Ctrl Pts',(0.802571685601037,-0.636309800095197,
11.3535596997118));
#61361=CARTESIAN_POINT('Ctrl Pts',(0.808949443435948,-0.319434907277159,
11.2789272273103));
#61362=CARTESIAN_POINT('Ctrl Pts',(0.814362858626305,-0.158333333333332,
11.2608073708274));
#61363=CARTESIAN_POINT('Ctrl Pts',(0.834445726094754,0.158333333333334,
11.2567221110703));
#61364=CARTESIAN_POINT('Ctrl Pts',(0.847999940077955,0.319434907277167,
11.270991020387));
#61365=CARTESIAN_POINT('Ctrl Pts',(0.884801197368705,0.636309800095206,
11.3368248349354));
#61366=CARTESIAN_POINT('Ctrl Pts',(0.907054451600615,0.79477268400084,11.3866294473169));
#61367=CARTESIAN_POINT('Ctrl Pts',(0.957653771540387,1.06847604194511,11.5163675802146));
#61368=CARTESIAN_POINT('Ctrl Pts',(0.982742057194051,1.18514270861178,11.5849228973736));
#61369=CARTESIAN_POINT('Ctrl Pts',(1.01101605778904,1.3,11.6658747012318));
#61370=CARTESIAN_POINT('Ctrl Pts',(0.741659516280668,-1.3,11.7197232017278));
#61371=CARTESIAN_POINT('Ctrl Pts',(0.738012470505645,-1.18514270861178,
11.633945905354));
#61372=CARTESIAN_POINT('Ctrl Pts',(0.735457044102349,-1.06847604194512,
11.5609770187778));
#61373=CARTESIAN_POINT('Ctrl Pts',(0.732075357025825,-0.794772684000851,
11.421994282357));
#61374=CARTESIAN_POINT('Ctrl Pts',(0.730851239620764,-0.636309800095197,
11.368060793598));
#61375=CARTESIAN_POINT('Ctrl Pts',(0.73676415858738,-0.319434907277159,
11.2939064508864));
#61376=CARTESIAN_POINT('Ctrl Pts',(0.741012286627639,-0.158333333333332,
11.2762150307074));
#61377=CARTESIAN_POINT('Ctrl Pts',(0.76116978437262,0.158333333333334,11.2724808787964));
#61378=CARTESIAN_POINT('Ctrl Pts',(0.775962801882669,0.319434907277167,
11.2866672191688));
#61379=CARTESIAN_POINT('Ctrl Pts',(0.813383183475107,0.636309800095206,
11.3527487599227));
#61380=CARTESIAN_POINT('Ctrl Pts',(0.836353845186878,0.79477268400084,11.4025713849577));
#61381=CARTESIAN_POINT('Ctrl Pts',(0.885532801701863,1.06847604194511,11.5330073325055));
#61382=CARTESIAN_POINT('Ctrl Pts',(0.909492919286399,1.18514270861178,11.6019904180251));
#61383=CARTESIAN_POINT('Ctrl Pts',(0.936125406440074,1.3,11.683495700499));
#61384=CARTESIAN_POINT('Ctrl Pts',(0.741659516280668,-1.3,11.7197232017278));
#61385=CARTESIAN_POINT('Ctrl Pts',(0.738012470505645,-1.18514270861178,
11.633945905354));
#61386=CARTESIAN_POINT('Ctrl Pts',(0.735457044102348,-1.06847604194512,
11.5609770187778));
#61387=CARTESIAN_POINT('Ctrl Pts',(0.732075357025825,-0.794772684000851,
11.421994282357));
#61388=CARTESIAN_POINT('Ctrl Pts',(0.730851239620765,-0.636309800095197,
11.368060793598));
#61389=CARTESIAN_POINT('Ctrl Pts',(0.736764158587381,-0.319434907277159,
11.2939064508864));
#61390=CARTESIAN_POINT('Ctrl Pts',(0.741012286627639,-0.158333333333332,
11.2762150307074));
#61391=CARTESIAN_POINT('Ctrl Pts',(0.76116978437262,0.158333333333334,11.2724808787964));
#61392=CARTESIAN_POINT('Ctrl Pts',(0.775962801882669,0.319434907277167,
11.2866672191688));
#61393=CARTESIAN_POINT('Ctrl Pts',(0.813383183475106,0.636309800095206,
11.3527487599227));
#61394=CARTESIAN_POINT('Ctrl Pts',(0.836353845186878,0.79477268400084,11.4025713849577));
#61395=CARTESIAN_POINT('Ctrl Pts',(0.885532801701862,1.06847604194511,11.5330073325055));
#61396=CARTESIAN_POINT('Ctrl Pts',(0.909492919286399,1.18514270861178,11.6019904180251));
#61397=CARTESIAN_POINT('Ctrl Pts',(0.936125406440073,1.3,11.683495700499));
#61398=CARTESIAN_POINT('Ctrl Pts',(0.741659516280677,-1.30000000000028,
11.719723201728));
#61399=CARTESIAN_POINT('Ctrl Pts',(0.738012470505649,-1.18514270861197,
11.6339459053541));
#61400=CARTESIAN_POINT('Ctrl Pts',(0.735457044102349,-1.06847604194521,
11.5609770187778));
#61401=CARTESIAN_POINT('Ctrl Pts',(0.732075357025825,-0.794772684000851,
11.421994282357));
#61402=CARTESIAN_POINT('Ctrl Pts',(0.730851239620765,-0.636309800095197,
11.368060793598));
#61403=CARTESIAN_POINT('Ctrl Pts',(0.736764158587381,-0.319434907277159,
11.2939064508864));
#61404=CARTESIAN_POINT('Ctrl Pts',(0.741012286627639,-0.158333333333332,
11.2762150307074));
#61405=CARTESIAN_POINT('Ctrl Pts',(0.76116978437262,0.158333333333334,11.2724808787964));
#61406=CARTESIAN_POINT('Ctrl Pts',(0.77596280188267,0.319434907277167,11.2866672191688));
#61407=CARTESIAN_POINT('Ctrl Pts',(0.813383183475107,0.636309800095206,
11.3527487599227));
#61408=CARTESIAN_POINT('Ctrl Pts',(0.836353845186879,0.79477268400084,11.4025713849577));
#61409=CARTESIAN_POINT('Ctrl Pts',(0.885532801702161,1.06847604194677,11.5330073325063));
#61410=CARTESIAN_POINT('Ctrl Pts',(0.90949291928707,1.18514270861505,11.601990418027));
#61411=CARTESIAN_POINT('Ctrl Pts',(0.936125406441193,1.30000000000483,11.6834957005024));
#61412=CARTESIAN_POINT('Ctrl Pts',(0.739042042488344,-1.30000000000028,
11.7249376165698));
#61413=CARTESIAN_POINT('Ctrl Pts',(0.735823583834715,-1.18514270861197,
11.6390010597618));
#61414=CARTESIAN_POINT('Ctrl Pts',(0.733297050684359,-1.06847604194521,
11.5658948972));
#61415=CARTESIAN_POINT('Ctrl Pts',(0.729058740007599,-0.794772684000851,
11.4266458142653));
#61416=CARTESIAN_POINT('Ctrl Pts',(0.725405994775785,-0.636309800095197,
11.3725700581163));
#61417=CARTESIAN_POINT('Ctrl Pts',(0.73013754978232,-0.319434907277159,
11.2983241249589));
#61418=CARTESIAN_POINT('Ctrl Pts',(0.734740249452905,-0.158333333333332,
11.2807133567046));
#61419=CARTESIAN_POINT('Ctrl Pts',(0.755052561493668,0.158333333333334,
11.2770101909005));
#61420=CARTESIAN_POINT('Ctrl Pts',(0.769831695225161,0.319434907277167,
11.2911645144203));
#61421=CARTESIAN_POINT('Ctrl Pts',(0.808370175300976,0.636309800095206,
11.3573648124169));
#61422=CARTESIAN_POINT('Ctrl Pts',(0.833047452158995,0.79477268400084,11.4073026355546));
#61423=CARTESIAN_POINT('Ctrl Pts',(0.883185362981537,1.06847604194677,11.5380010488157));
#61424=CARTESIAN_POINT('Ctrl Pts',(0.907329875011758,1.18514270861505,11.607121446575));
#61425=CARTESIAN_POINT('Ctrl Pts',(0.933916055269645,1.30000000000483,11.6887877418462));
#61426=CARTESIAN_POINT('Ctrl Pts',(0.736513353027043,-1.30000000000024,
11.7335029101657));
#61427=CARTESIAN_POINT('Ctrl Pts',(0.734197104083671,-1.18514270861194,
11.6485493198283));
#61428=CARTESIAN_POINT('Ctrl Pts',(0.731891266475708,-1.06847604194518,
11.5761286952239));
#61429=CARTESIAN_POINT('Ctrl Pts',(0.726588372587658,-0.79477268400083,
11.4377762227459));
#61430=CARTESIAN_POINT('Ctrl Pts',(0.719179900276991,-0.636309800095178,
11.3832624369924));
#61431=CARTESIAN_POINT('Ctrl Pts',(0.722022671202612,-0.319434907277149,
11.3088658603034));
#61432=CARTESIAN_POINT('Ctrl Pts',(0.726936954002692,-0.158333333333327,
11.2908872748991));
#61433=CARTESIAN_POINT('Ctrl Pts',(0.747449048780318,0.15833333333333,11.2872075458618));
#61434=CARTESIAN_POINT('Ctrl Pts',(0.762206183434706,0.319434907277157,
11.3017933991775));
#61435=CARTESIAN_POINT('Ctrl Pts',(0.802857471827774,0.636309800095187,
11.3681100406464));
#61436=CARTESIAN_POINT('Ctrl Pts',(0.831207002399099,0.794772684000817,
11.4183174781789));
#61437=CARTESIAN_POINT('Ctrl Pts',(0.882448094814532,1.06847604194674,11.5481255882124));
#61438=CARTESIAN_POINT('Ctrl Pts',(0.906391184552781,1.18514270861501,11.6166006607166));
#61439=CARTESIAN_POINT('Ctrl Pts',(0.932096993792065,1.30000000000479,11.6973616847556));
#61440=CARTESIAN_POINT('Ctrl Pts',(0.734690372091587,-1.30000000000024,
11.7455625251118));
#61441=CARTESIAN_POINT('Ctrl Pts',(0.733386866582579,-1.18514270861193,
11.6632066715271));
#61442=CARTESIAN_POINT('Ctrl Pts',(0.731407157793679,-1.06847604194518,
11.5926822187035));
#61443=CARTESIAN_POINT('Ctrl Pts',(0.725271469601385,-0.794772684000829,
11.4570895269343));
#61444=CARTESIAN_POINT('Ctrl Pts',(0.714394232863423,-0.636309800095177,
11.4020845254731));
#61445=CARTESIAN_POINT('Ctrl Pts',(0.7152493773471,-0.319434907277149,11.3277048294426));
#61446=CARTESIAN_POINT('Ctrl Pts',(0.71994876732749,-0.158333333333327,
11.3087599499422));
#61447=CARTESIAN_POINT('Ctrl Pts',(0.740554013134365,0.158333333333329,
11.3050802735153));
#61448=CARTESIAN_POINT('Ctrl Pts',(0.755401586135559,0.319434907277157,
11.3206828608572));
#61449=CARTESIAN_POINT('Ctrl Pts',(0.798673489649781,0.636309800095186,
11.3868800934896));
#61450=CARTESIAN_POINT('Ctrl Pts',(0.831837381161029,0.794772684000816,
11.437299798421));
#61451=CARTESIAN_POINT('Ctrl Pts',(0.883912658960803,1.06847604194674,11.5643693378906));
#61452=CARTESIAN_POINT('Ctrl Pts',(0.907206670173654,1.18514270861501,11.6310263922609));
#61453=CARTESIAN_POINT('Ctrl Pts',(0.931253234418874,1.30000000000479,11.7093368057551));
#61454=CARTESIAN_POINT('Ctrl Pts',(0.732507359893536,-1.3000000000002,11.7573468723062));
#61455=CARTESIAN_POINT('Ctrl Pts',(0.731446973883555,-1.18514270861191,
11.6773389107016));
#61456=CARTESIAN_POINT('Ctrl Pts',(0.729521126215045,-1.06847604194515,
11.6085578501234));
#61457=CARTESIAN_POINT('Ctrl Pts',(0.723072643270074,-0.794772684000809,
11.4755962278889));
#61458=CARTESIAN_POINT('Ctrl Pts',(0.711265049464907,-0.636309800095161,
11.4203598204888));
#61459=CARTESIAN_POINT('Ctrl Pts',(0.711336217967816,-0.31943490727714,
11.3461817951623));
#61460=CARTESIAN_POINT('Ctrl Pts',(0.715519917280257,-0.158333333333323,
11.3264634689159));
#61461=CARTESIAN_POINT('Ctrl Pts',(0.736192836746224,0.158333333333325,
11.3227634990918));
#61462=CARTESIAN_POINT('Ctrl Pts',(0.751417880673255,0.319434907277149,
11.3391299261724));
#61463=CARTESIAN_POINT('Ctrl Pts',(0.796030996572588,0.63630980009517,11.405062384505));
#61464=CARTESIAN_POINT('Ctrl Pts',(0.831284152871013,0.794772684000795,
11.4556021487431));
#61465=CARTESIAN_POINT('Ctrl Pts',(0.88380018897958,1.06847604194671,11.5800628855438));
#61466=CARTESIAN_POINT('Ctrl Pts',(0.90684379510631,1.18514270861498,11.6450189495381));
#61467=CARTESIAN_POINT('Ctrl Pts',(0.930198761239113,1.30000000000475,11.72105663629));
#61468=CARTESIAN_POINT('Ctrl Pts',(0.729739714965373,-1.30000000000017,
11.772078421086));
#61469=CARTESIAN_POINT('Ctrl Pts',(0.728627363429549,-1.18514270861187,
11.6948641909879));
#61470=CARTESIAN_POINT('Ctrl Pts',(0.72679940596954,-1.06847604194513,11.6281040130364));
#61471=CARTESIAN_POINT('Ctrl Pts',(0.720923265713938,-0.794772684000789,
11.4980255984249));
#61472=CARTESIAN_POINT('Ctrl Pts',(0.710628506046623,-0.636309800095146,
11.4420613460075));
#61473=CARTESIAN_POINT('Ctrl Pts',(0.710519142033698,-0.319434907277133,
11.3679189145324));
#61474=CARTESIAN_POINT('Ctrl Pts',(0.712895820440734,-0.15833333333332,
11.3474097803368));
#61475=CARTESIAN_POINT('Ctrl Pts',(0.733068591135251,0.158333333333322,
11.3437410226042));
#61476=CARTESIAN_POINT('Ctrl Pts',(0.748783293766575,0.319434907277142,
11.3610032250158));
#61477=CARTESIAN_POINT('Ctrl Pts',(0.794222780061106,0.636309800095155,
11.4268134320641));
#61478=CARTESIAN_POINT('Ctrl Pts',(0.830997222534945,0.794772684000776,
11.4777581767203));
#61479=CARTESIAN_POINT('Ctrl Pts',(0.883398438514725,1.06847604194668,11.5993299343026));
#61480=CARTESIAN_POINT('Ctrl Pts',(0.905989964443896,1.18514270861495,11.6623326059402));
#61481=CARTESIAN_POINT('Ctrl Pts',(0.92849047156083,1.30000000000472,11.7357140400351));
#61482=CARTESIAN_POINT('Ctrl Pts',(0.726871111169889,-1.30000000000014,
11.7854327933036));
#61483=CARTESIAN_POINT('Ctrl Pts',(0.725662375630626,-1.18514270861184,
11.7109232510307));
#61484=CARTESIAN_POINT('Ctrl Pts',(0.723931742859821,-1.0684760419451,11.6461298391096));
#61485=CARTESIAN_POINT('Ctrl Pts',(0.718727947937321,-0.79477268400077,
11.5188903005118));
#61486=CARTESIAN_POINT('Ctrl Pts',(0.70996917089403,-0.636309800095129,
11.4623191156996));
#61487=CARTESIAN_POINT('Ctrl Pts',(0.710300254588474,-0.319434907277125,
11.3882293156305));
#61488=CARTESIAN_POINT('Ctrl Pts',(0.711401496061413,-0.158333333333315,
11.3669370146061));
#61489=CARTESIAN_POINT('Ctrl Pts',(0.732257858090713,0.158333333333317,
11.3631717685982));
#61490=CARTESIAN_POINT('Ctrl Pts',(0.750292771558832,0.319434907277133,
11.3810603770313));
#61491=CARTESIAN_POINT('Ctrl Pts',(0.795948533589905,0.636309800095138,
11.4467441838119));
#61492=CARTESIAN_POINT('Ctrl Pts',(0.830900527909714,0.794772684000756,
11.498364921461));
#61493=CARTESIAN_POINT('Ctrl Pts',(0.882259193644855,1.06847604194666,11.617186409127));
#61494=CARTESIAN_POINT('Ctrl Pts',(0.90450231688194,1.18514270861492,11.6782740666674));
#61495=CARTESIAN_POINT('Ctrl Pts',(0.926757299985315,1.30000000000469,11.7490159625073));
#61496=CARTESIAN_POINT('Ctrl Pts',(0.724391632493098,-1.30000000000012,
11.7943012189908));
#61497=CARTESIAN_POINT('Ctrl Pts',(0.723101127419453,-1.18514270861183,
11.7215140260944));
#61498=CARTESIAN_POINT('Ctrl Pts',(0.72144951393426,-1.06847604194509,11.6579705374978));
#61499=CARTESIAN_POINT('Ctrl Pts',(0.716799723709153,-0.79477268400076,
11.5325271731377));
#61500=CARTESIAN_POINT('Ctrl Pts',(0.70905911646003,-0.636309800095122,
11.4755695176922));
#61501=CARTESIAN_POINT('Ctrl Pts',(0.710251122888309,-0.319434907277121,
11.4014618232877));
#61502=CARTESIAN_POINT('Ctrl Pts',(0.711503517432686,-0.158333333333314,
11.3795871437005));
#61503=CARTESIAN_POINT('Ctrl Pts',(0.732900309736102,0.158333333333316,
11.3757416690285));
#61504=CARTESIAN_POINT('Ctrl Pts',(0.751632512409751,0.31943490727713,11.3940739107996));
#61505=CARTESIAN_POINT('Ctrl Pts',(0.796900770990882,0.636309800095131,
11.4597313859243));
#61506=CARTESIAN_POINT('Ctrl Pts',(0.83033283835543,0.794772684000747,11.5118499896394));
#61507=CARTESIAN_POINT('Ctrl Pts',(0.881120250462187,1.06847604194664,11.6289323109164));
#61508=CARTESIAN_POINT('Ctrl Pts',(0.903323722379641,1.18514270861491,11.6887900188793));
#61509=CARTESIAN_POINT('Ctrl Pts',(0.925746677372449,1.30000000000468,11.7578248362514));
#61510=CARTESIAN_POINT('Ctrl Pts',(0.722742798682041,-1.30000000000012,
11.8002248077556));
#61511=CARTESIAN_POINT('Ctrl Pts',(0.721419566753041,-1.18514270861183,
11.7286007197735));
#61512=CARTESIAN_POINT('Ctrl Pts',(0.719837963986194,-1.06847604194509,
11.6659004086064));
#61513=CARTESIAN_POINT('Ctrl Pts',(0.715587256873898,-0.79477268400076,
11.5416658562942));
#61514=CARTESIAN_POINT('Ctrl Pts',(0.708530478596676,-0.636309800095122,
11.4844419155667));
#61515=CARTESIAN_POINT('Ctrl Pts',(0.710307727169727,-0.319434907277121,
11.4103142310288));
#61516=CARTESIAN_POINT('Ctrl Pts',(0.711734427886754,-0.158333333333314,
11.3880287945659));
#61517=CARTESIAN_POINT('Ctrl Pts',(0.73334722574718,0.158333333333316,11.3841478302049));
#61518=CARTESIAN_POINT('Ctrl Pts',(0.752177487683406,0.319434907277129,
11.4028351922547));
#61519=CARTESIAN_POINT('Ctrl Pts',(0.797185690872596,0.636309800095131,
11.468481405373));
#61520=CARTESIAN_POINT('Ctrl Pts',(0.83004512865742,0.794772684000747,11.5208842267609));
#61521=CARTESIAN_POINT('Ctrl Pts',(0.880500610743032,1.06847604194664,11.6367846006553));
#61522=CARTESIAN_POINT('Ctrl Pts',(0.902624193344047,1.18514270861491,11.6958162840945));
#61523=CARTESIAN_POINT('Ctrl Pts',(0.925031049910914,1.30000000000467,11.7637106736459));
#61524=CARTESIAN_POINT('Ctrl Pts',(0.71994117055138,-1.30000000000009,11.8105870027124));
#61525=CARTESIAN_POINT('Ctrl Pts',(0.718688939033695,-1.18514270861181,
11.740999718903));
#61526=CARTESIAN_POINT('Ctrl Pts',(0.717294270598105,-1.06847604194506,
11.6797778294328));
#61527=CARTESIAN_POINT('Ctrl Pts',(0.71374324973466,-0.794772684000742,
11.557668751774));
#61528=CARTESIAN_POINT('Ctrl Pts',(0.707595361315513,-0.636309800095109,
11.4999959843807));
#61529=CARTESIAN_POINT('Ctrl Pts',(0.71031903400796,-0.319434907277115,
11.4258370640626));
#61530=CARTESIAN_POINT('Ctrl Pts',(0.712311439868488,-0.15833333333331,
11.4027989395063));
#61531=CARTESIAN_POINT('Ctrl Pts',(0.734014976729677,0.158333333333312,
11.3988955011669));
#61532=CARTESIAN_POINT('Ctrl Pts',(0.752221442724715,0.319434907277122,
11.4183153622965));
#61533=CARTESIAN_POINT('Ctrl Pts',(0.796771206188982,0.636309800095118,
11.4839423790098));
#61534=CARTESIAN_POINT('Ctrl Pts',(0.829569489541166,0.794772684000731,
11.5367202862584));
#61535=CARTESIAN_POINT('Ctrl Pts',(0.879553043281544,1.06847604194662,11.6505216761042));
#61536=CARTESIAN_POINT('Ctrl Pts',(0.901425593708693,1.18514270861488,11.7081115434555));
#61537=CARTESIAN_POINT('Ctrl Pts',(0.923534666221812,1.30000000000465,11.7740308732505));
#61538=CARTESIAN_POINT('Ctrl Pts',(0.715773049841682,-1.30000000000009,
11.8312567595427));
#61539=CARTESIAN_POINT('Ctrl Pts',(0.713894702046613,-1.1851427086118,11.7657401096002));
#61540=CARTESIAN_POINT('Ctrl Pts',(0.712263951197079,-1.06847604194506,
11.7074819432039));
#61541=CARTESIAN_POINT('Ctrl Pts',(0.709068588979851,-0.794772684000739,
11.5896624733687));
#61542=CARTESIAN_POINT('Ctrl Pts',(0.704527181281509,-0.636309800095106,
11.531156225655));
#61543=CARTESIAN_POINT('Ctrl Pts',(0.708833282403318,-0.319434907277113,
11.4569945983025));
#61544=CARTESIAN_POINT('Ctrl Pts',(0.711666493724411,-0.15833333333331,
11.4325322881426));
#61545=CARTESIAN_POINT('Ctrl Pts',(0.734429330765286,0.158333333333312,
11.4284919162156));
#61546=CARTESIAN_POINT('Ctrl Pts',(0.753655173885053,0.319434907277122,
11.4490887889334));
#61547=CARTESIAN_POINT('Ctrl Pts',(0.797148887319053,0.636309800095116,
11.5146641406369));
#61548=CARTESIAN_POINT('Ctrl Pts',(0.826817146073029,0.794772684000727,
11.5684948467983));
#61549=CARTESIAN_POINT('Ctrl Pts',(0.875521263709609,1.06847604194662,11.6781493133238));
#61550=CARTESIAN_POINT('Ctrl Pts',(0.897270371507951,1.18514270861487,11.7328314345891));
#61551=CARTESIAN_POINT('Ctrl Pts',(0.919686379245016,1.30000000000464,11.7947303216591));
#61552=CARTESIAN_POINT('Ctrl Pts',(0.708106339592663,-1.29999999999985,
11.8549337471632));
#61553=CARTESIAN_POINT('Ctrl Pts',(0.705716356639382,-1.18514270861158,
11.7940699885983));
#61554=CARTESIAN_POINT('Ctrl Pts',(0.704096117869523,-1.06847604194486,
11.7391945926482));
#61555=CARTESIAN_POINT('Ctrl Pts',(0.702131305233996,-0.794772684000595,
11.6262557658256));
#61556=CARTESIAN_POINT('Ctrl Pts',(0.700490171305661,-0.636309800094987,
11.5667529657947));
#61557=CARTESIAN_POINT('Ctrl Pts',(0.707123085947054,-0.319434907277052,
11.4925747952514));
#61558=CARTESIAN_POINT('Ctrl Pts',(0.710920992338189,-0.15833333333328,
11.466458146152));
#61559=CARTESIAN_POINT('Ctrl Pts',(0.734037344146519,0.158333333333282,
11.4623676047482));
#61560=CARTESIAN_POINT('Ctrl Pts',(0.752190621505164,0.319434907277065,
11.4845724982227));
#61561=CARTESIAN_POINT('Ctrl Pts',(0.795017414505158,0.636309800094999,
11.5500543566967));
#61562=CARTESIAN_POINT('Ctrl Pts',(0.824547896991247,0.794772684000577,
11.6047319280489));
#61563=CARTESIAN_POINT('Ctrl Pts',(0.872754551306088,1.06847604194641,11.7095502432165));
#61564=CARTESIAN_POINT('Ctrl Pts',(0.894271436335858,1.18514270861465,11.7609185955138));
#61565=CARTESIAN_POINT('Ctrl Pts',(0.91643833197493,1.3000000000044,11.8182833353734));
#61566=CARTESIAN_POINT('Ctrl Pts',(0.701392717589504,-1.29999999999977,
11.8785605604878));
#61567=CARTESIAN_POINT('Ctrl Pts',(0.698072695455552,-1.18514270861151,
11.8223399017));
#61568=CARTESIAN_POINT('Ctrl Pts',(0.696020255650023,-1.06847604194479,
11.7708544676842));
#61569=CARTESIAN_POINT('Ctrl Pts',(0.694207077867708,-0.794772684000542,
11.6628521319838));
#61570=CARTESIAN_POINT('Ctrl Pts',(0.694147020817013,-0.636309800094947,
11.6024830083094));
#61571=CARTESIAN_POINT('Ctrl Pts',(0.703048255663917,-0.319434907277033,
11.5283287199599));
#61572=CARTESIAN_POINT('Ctrl Pts',(0.7092636804318,-0.158333333333271,11.5005012358133));
#61573=CARTESIAN_POINT('Ctrl Pts',(0.733194250079355,0.158333333333273,
11.4963283081617));
#61574=CARTESIAN_POINT('Ctrl Pts',(0.75018486417955,0.319434907277045,11.5200944460579));
#61575=CARTESIAN_POINT('Ctrl Pts',(0.791504293676369,0.636309800094959,
11.585521497962));
#61576=CARTESIAN_POINT('Ctrl Pts',(0.819005278050289,0.794772684000529,
11.6411952916285));
#61577=CARTESIAN_POINT('Ctrl Pts',(0.866710872109081,1.06847604194635,11.7411747899911));
#61578=CARTESIAN_POINT('Ctrl Pts',(0.88844359663303,1.18514270861458,11.7891948061993));
#61579=CARTESIAN_POINT('Ctrl Pts',(0.91125906167919,1.30000000000432,11.8419574183797));
#61580=CARTESIAN_POINT('Ctrl Pts',(0.696379212651574,-1.29999999999974,
11.8962766909092));
#61581=CARTESIAN_POINT('Ctrl Pts',(0.692999191360036,-1.18514270861148,
11.8435384540665));
#61582=CARTESIAN_POINT('Ctrl Pts',(0.690970633093636,-1.06847604194477,
11.7945953930707));
#61583=CARTESIAN_POINT('Ctrl Pts',(0.689406407633882,-0.794772684000527,
11.6902947465732));
#61584=CARTESIAN_POINT('Ctrl Pts',(0.689712119805148,-0.636309800094934,
11.629249227579));
#61585=CARTESIAN_POINT('Ctrl Pts',(0.699298112195223,-0.319434907277026,
11.5551617154664));
#61586=CARTESIAN_POINT('Ctrl Pts',(0.706099181263705,-0.158333333333267,
11.5261610928535));
#61587=CARTESIAN_POINT('Ctrl Pts',(0.730556960302764,0.158333333333269,
11.5219451899244));
#61588=CARTESIAN_POINT('Ctrl Pts',(0.747648646203372,0.319434907277038,
11.5468243597819));
#61589=CARTESIAN_POINT('Ctrl Pts',(0.789032302044774,0.636309800094946,
11.61213199298));
#61590=CARTESIAN_POINT('Ctrl Pts',(0.816252297706209,0.794772684000512,
11.668461565255));
#61591=CARTESIAN_POINT('Ctrl Pts',(0.863996819850258,1.06847604194633,11.7647786583432));
#61592=CARTESIAN_POINT('Ctrl Pts',(0.885803182416638,1.18514270861455,11.8102911655351));
#61593=CARTESIAN_POINT('Ctrl Pts',(0.908749073021981,1.30000000000429,11.8596240792207));
#61594=CARTESIAN_POINT('Ctrl Pts',(0.690660095299648,-1.29999999999966,
11.9139835115398));
#61595=CARTESIAN_POINT('Ctrl Pts',(0.685682722076107,-1.18514270861141,
11.8647239191065));
#61596=CARTESIAN_POINT('Ctrl Pts',(0.682768533441947,-1.0684760419447,11.8183239634083));
#61597=CARTESIAN_POINT('Ctrl Pts',(0.680802543855727,-0.794772684000474,
11.7177371163932));
#61598=CARTESIAN_POINT('Ctrl Pts',(0.683350742237752,-0.636309800094896,
11.6560556065026));
#61599=CARTESIAN_POINT('Ctrl Pts',(0.694836451094066,-0.319434907277008,
11.5820281070802));
#61600=CARTESIAN_POINT('Ctrl Pts',(0.703081913914877,-0.158333333333258,
11.5517991314348));
#61601=CARTESIAN_POINT('Ctrl Pts',(0.728231769052573,0.15833333333326,11.5475366605752));
#61602=CARTESIAN_POINT('Ctrl Pts',(0.744790141058607,0.31943490727702,11.5735538840847));
#61603=CARTESIAN_POINT('Ctrl Pts',(0.785237694727035,0.636309800094909,
11.6387957268862));
#61604=CARTESIAN_POINT('Ctrl Pts',(0.810856804125816,0.794772684000465,
11.6958543568564));
#61605=CARTESIAN_POINT('Ctrl Pts',(0.858356073086245,1.06847604194626,11.7885319067558));
#61606=CARTESIAN_POINT('Ctrl Pts',(0.880405649972082,1.18514270861449,11.8315323060639));
#61607=CARTESIAN_POINT('Ctrl Pts',(0.903944130232002,1.30000000000422,11.87741642737));
#61608=CARTESIAN_POINT('Ctrl Pts',(0.684774161766043,-1.29999999999961,
11.9316792283627));
#61609=CARTESIAN_POINT('Ctrl Pts',(0.679670728815399,-1.18514270861137,
11.8858988962828));
#61610=CARTESIAN_POINT('Ctrl Pts',(0.676779668951229,-1.06847604194467,
11.8420404620596));
#61611=CARTESIAN_POINT('Ctrl Pts',(0.675211766723929,-0.794772684000448,
11.7451586736775));
#61612=CARTESIAN_POINT('Ctrl Pts',(0.678635652890764,-0.636309800094872,
11.682807341107));
#61613=CARTESIAN_POINT('Ctrl Pts',(0.690797413702307,-0.319434907276995,
11.6088645835443));
#61614=CARTESIAN_POINT('Ctrl Pts',(0.699162179082554,-0.158333333333252,
11.5774811768116));
#61615=CARTESIAN_POINT('Ctrl Pts',(0.724632526989099,0.158333333333254,
11.5731918390187));
#61616=CARTESIAN_POINT('Ctrl Pts',(0.741230482084265,0.319434907277007,
11.6003317903806));
#61617=CARTESIAN_POINT('Ctrl Pts',(0.781983986559276,0.636309800094885,
11.6654440165117));
#61618=CARTESIAN_POINT('Ctrl Pts',(0.807937356793683,0.794772684000434,
11.7231212970555));
#61619=CARTESIAN_POINT('Ctrl Pts',(0.855587165199985,1.06847604194622,11.812130964535));
#61620=CARTESIAN_POINT('Ctrl Pts',(0.877639911931404,1.18514270861444,11.8526284951903));
#61621=CARTESIAN_POINT('Ctrl Pts',(0.901119568934406,1.30000000000417,11.895094569582));
#61622=CARTESIAN_POINT('Ctrl Pts',(0.678549186698821,-1.29999999999946,
11.9493585018483));
#61623=CARTESIAN_POINT('Ctrl Pts',(0.672432041213187,-1.18514270861122,
11.9070486740622));
#61624=CARTESIAN_POINT('Ctrl Pts',(0.668959648382607,-1.06847604194454,
11.865729892223));
#61625=CARTESIAN_POINT('Ctrl Pts',(0.667047634008289,-0.79477268400035,
11.7725647547759));
#61626=CARTESIAN_POINT('Ctrl Pts',(0.671674453970411,-0.636309800094796,
11.7095875503082));
#61627=CARTESIAN_POINT('Ctrl Pts',(0.685080552577213,-0.319434907276958,
11.6357386986211));
#61628=CARTESIAN_POINT('Ctrl Pts',(0.694640062897662,-0.158333333333233,
11.6031714292693));
#61629=CARTESIAN_POINT('Ctrl Pts',(0.720646467007646,0.158333333333235,
11.5988554570619));
#61630=CARTESIAN_POINT('Ctrl Pts',(0.736905994278727,0.319434907276967,
11.6271197806948));
#61631=CARTESIAN_POINT('Ctrl Pts',(0.776854720427988,0.636309800094807,
11.6921507737362));
#61632=CARTESIAN_POINT('Ctrl Pts',(0.801120572561274,0.79477268400034,11.7505397288079));
#61633=CARTESIAN_POINT('Ctrl Pts',(0.84893651173128,1.0684760419461,11.8358910768284));
#61634=CARTESIAN_POINT('Ctrl Pts',(0.871504994914518,1.1851427086143,11.8738691384865));
#61635=CARTESIAN_POINT('Ctrl Pts',(0.895944212969302,1.30000000000401,11.9128798258235));
#61636=CARTESIAN_POINT('Ctrl Pts',(0.674222718308865,-1.29999999999937,
11.9640876094412));
#61637=CARTESIAN_POINT('Ctrl Pts',(0.666986355018664,-1.18514270861114,
11.9246619613613));
#61638=CARTESIAN_POINT('Ctrl Pts',(0.662836854551111,-1.06847604194446,
11.8854538539057));
#61639=CARTESIAN_POINT('Ctrl Pts',(0.660381949011449,-0.794772684000296,
11.7953778444889));
#61640=CARTESIAN_POINT('Ctrl Pts',(0.66609150822191,-0.636309800094752,
11.7318822817835));
#61641=CARTESIAN_POINT('Ctrl Pts',(0.68063358116873,-0.319434907276936,
11.6581096922817));
#61642=CARTESIAN_POINT('Ctrl Pts',(0.691415225026868,-0.158333333333222,
11.624551409228));
#61643=CARTESIAN_POINT('Ctrl Pts',(0.717918159526262,0.158333333333224,
11.6202170472644));
#61644=CARTESIAN_POINT('Ctrl Pts',(0.733451120016153,0.319434907276946,
11.6494425495418));
#61645=CARTESIAN_POINT('Ctrl Pts',(0.773277231328102,0.636309800094764,
11.7143831350432));
#61646=CARTESIAN_POINT('Ctrl Pts',(0.797580730757561,0.794772684000285,
11.7733006957295));
#61647=CARTESIAN_POINT('Ctrl Pts',(0.845788720600292,1.06847604194602,11.8555845497542));
#61648=CARTESIAN_POINT('Ctrl Pts',(0.868618068406382,1.18514270861422,11.8914654749949));
#61649=CARTESIAN_POINT('Ctrl Pts',(0.893409311497553,1.30000000000392,11.9276096939862));
#61650=CARTESIAN_POINT('Ctrl Pts',(0.667369721617846,-1.2999999999993,11.9817468175657));
#61651=CARTESIAN_POINT('Ctrl Pts',(0.659742133214706,-1.18514270861108,
11.9457950770222));
#61652=CARTESIAN_POINT('Ctrl Pts',(0.655434396033206,-1.06847604194441,
11.9091279977393));
#61653=CARTESIAN_POINT('Ctrl Pts',(0.653152181840017,-0.794772684000256,
11.8227671337809));
#61654=CARTESIAN_POINT('Ctrl Pts',(0.659921427366295,-0.636309800094721,
11.7586271846953));
#61655=CARTESIAN_POINT('Ctrl Pts',(0.675123639591609,-0.319434907276921,
11.684961005829));
#61656=CARTESIAN_POINT('Ctrl Pts',(0.686172569068147,-0.158333333333214,
11.6502500215863));
#61657=CARTESIAN_POINT('Ctrl Pts',(0.712534168854585,0.158333333333216,
11.6459109667399));
#61658=CARTESIAN_POINT('Ctrl Pts',(0.727362482686232,0.319434907276929,
11.6762765482347));
#61659=CARTESIAN_POINT('Ctrl Pts',(0.766843550399096,0.636309800094731,
11.7411173150198));
#61660=CARTESIAN_POINT('Ctrl Pts',(0.790971787147075,0.794772684000247,
11.8006841259155));
#61661=CARTESIAN_POINT('Ctrl Pts',(0.839696979707915,1.06847604194597,11.8793011898733));
#61662=CARTESIAN_POINT('Ctrl Pts',(0.862932260753159,1.18514270861416,11.9126710725441));
#61663=CARTESIAN_POINT('Ctrl Pts',(0.888311492430216,1.30000000000386,11.9453804239475));
#61664=CARTESIAN_POINT('Ctrl Pts',(0.662335531550092,-1.29999999999911,
11.99643968074));
#61665=CARTESIAN_POINT('Ctrl Pts',(0.652920552658503,-1.18514270861091,
11.9633444972165));
#61666=CARTESIAN_POINT('Ctrl Pts',(0.647516901475013,-1.06847604194426,
11.9287737920991));
#61667=CARTESIAN_POINT('Ctrl Pts',(0.644300355713498,-0.794772684000144,
11.8454997973729));
#61668=CARTESIAN_POINT('Ctrl Pts',(0.652833902539925,-0.63630980009463,
11.7808905622974));
#61669=CARTESIAN_POINT('Ctrl Pts',(0.66948372337528,-0.319434907276874,
11.7073339904357));
#61670=CARTESIAN_POINT('Ctrl Pts',(0.681622795171332,-0.158333333333192,
11.6716547229497));
#61671=CARTESIAN_POINT('Ctrl Pts',(0.709092228259606,0.158333333333194,
11.6672915509916));
#61672=CARTESIAN_POINT('Ctrl Pts',(0.724480061053731,0.319434907276885,
11.6985662875476));
#61673=CARTESIAN_POINT('Ctrl Pts',(0.76366643224308,0.636309800094642,11.7633196375378));
#61674=CARTESIAN_POINT('Ctrl Pts',(0.785832472357193,0.794772684000132,
11.823476606662));
#61675=CARTESIAN_POINT('Ctrl Pts',(0.834828940803699,1.06847604194582,11.8990326400059));
#61676=CARTESIAN_POINT('Ctrl Pts',(0.858651545639185,1.18514270861399,11.9302973597015));
#61677=CARTESIAN_POINT('Ctrl Pts',(0.885087999617585,1.30000000000367,11.9601213918847));
#61678=CARTESIAN_POINT('Ctrl Pts',(0.654500613520237,-1.29999999999899,
12.0170141288364));
#61679=CARTESIAN_POINT('Ctrl Pts',(0.644565540455188,-1.1851427086108,11.9879631922512));
#61680=CARTESIAN_POINT('Ctrl Pts',(0.63877654301765,-1.06847604194416,11.9563506643837));
#61681=CARTESIAN_POINT('Ctrl Pts',(0.634981064971107,-0.794772684000068,
11.8774016126389));
#61682=CARTESIAN_POINT('Ctrl Pts',(0.643084042498312,-0.636309800094567,
11.8120386328918));
#61683=CARTESIAN_POINT('Ctrl Pts',(0.660652874351986,-0.319434907276841,
11.7386122902342));
#61684=CARTESIAN_POINT('Ctrl Pts',(0.675025400252646,-0.158333333333176,
11.7016017791411));
#61685=CARTESIAN_POINT('Ctrl Pts',(0.702984679232211,0.158333333333178,
11.6972430066232));
#61686=CARTESIAN_POINT('Ctrl Pts',(0.716772423379789,0.319434907276852,
11.7298538736244));
#61687=CARTESIAN_POINT('Ctrl Pts',(0.755745225337548,0.636309800094577,
11.7944849629586));
#61688=CARTESIAN_POINT('Ctrl Pts',(0.778484066973515,0.794772684000052,
11.8553751368386));
#61689=CARTESIAN_POINT('Ctrl Pts',(0.828258808440125,1.06847604194571,11.9266539771194));
#61690=CARTESIAN_POINT('Ctrl Pts',(0.852499600637966,1.18514270861387,11.9549949065323));
#61691=CARTESIAN_POINT('Ctrl Pts',(0.879435543788526,1.30000000000354,11.9808227965415));
#61692=CARTESIAN_POINT('Ctrl Pts',(0.648585099106898,-1.29999999999886,
12.0346262810387));
#61693=CARTESIAN_POINT('Ctrl Pts',(0.63671231292895,-1.18514270861068,12.0089949224276));
#61694=CARTESIAN_POINT('Ctrl Pts',(0.629749814138102,-1.06847604194405,
11.9798926459143));
#61695=CARTESIAN_POINT('Ctrl Pts',(0.625008795251963,-0.794772683999986,
11.9046420505691));
#61696=CARTESIAN_POINT('Ctrl Pts',(0.635421531598707,-0.636309800094504,
11.8387169067579));
#61697=CARTESIAN_POINT('Ctrl Pts',(0.654077321348798,-0.319434907276811,
11.7654365401314));
#61698=CARTESIAN_POINT('Ctrl Pts',(0.668786882007543,-0.15833333333316,
11.7272830225411));
#61699=CARTESIAN_POINT('Ctrl Pts',(0.696966209368503,0.158333333333162,
11.722917458364));
#61700=CARTESIAN_POINT('Ctrl Pts',(0.710403034558743,0.319434907276821,
11.7566401387454));
#61701=CARTESIAN_POINT('Ctrl Pts',(0.749213605152048,0.636309800094515,
11.8211611219402));
#61702=CARTESIAN_POINT('Ctrl Pts',(0.771463328588758,0.794772683999976,
11.8827097085051));
#61703=CARTESIAN_POINT('Ctrl Pts',(0.821963976608028,1.0684760419456,11.9503235628632));
#61704=CARTESIAN_POINT('Ctrl Pts',(0.846789883164354,1.18514270861375,11.976153865767));
#61705=CARTESIAN_POINT('Ctrl Pts',(0.874581836982727,1.30000000000341,11.9985469393629));
#61706=CARTESIAN_POINT('Ctrl Pts',(0.639457684724997,-1.29999999999865,
12.055133698939));
#61707=CARTESIAN_POINT('Ctrl Pts',(0.62674097457832,-1.18514270861049,12.0335190159486));
#61708=CARTESIAN_POINT('Ctrl Pts',(0.619210639483942,-1.06847604194388,
12.0073589062376));
#61709=CARTESIAN_POINT('Ctrl Pts',(0.613795622879141,-0.794772683999862,
11.9364229744589));
#61710=CARTESIAN_POINT('Ctrl Pts',(0.624369194200539,-0.636309800094403,
11.8697763172489));
#61711=CARTESIAN_POINT('Ctrl Pts',(0.644000269036368,-0.31943490727676,
11.7966569147437));
#61712=CARTESIAN_POINT('Ctrl Pts',(0.660203030149533,-0.158333333333135,
11.7572028730154));
#61713=CARTESIAN_POINT('Ctrl Pts',(0.689570015141949,0.158333333333137,
11.7528497218579));
#61714=CARTESIAN_POINT('Ctrl Pts',(0.703522155079055,0.319434907276769,
11.7878781852481));
#61715=CARTESIAN_POINT('Ctrl Pts',(0.742104585901675,0.636309800094413,
11.8522780612349));
#61716=CARTESIAN_POINT('Ctrl Pts',(0.762340533905654,0.794772683999849,
11.914587337957));
#61717=CARTESIAN_POINT('Ctrl Pts',(0.813454919682806,1.06847604194544,11.9779296921709));
#61718=CARTESIAN_POINT('Ctrl Pts',(0.839095253705589,1.18514270861357,12.0008344718056));
#61719=CARTESIAN_POINT('Ctrl Pts',(0.86825039812271,1.30000000000321,12.0192254730012));
#61720=CARTESIAN_POINT('Ctrl Pts',(0.634180702243894,-1.29999999999847,
12.0697751580724));
#61721=CARTESIAN_POINT('Ctrl Pts',(0.619712411140887,-1.18514270861032,
12.05099069487));
#61722=CARTESIAN_POINT('Ctrl Pts',(0.611114313461518,-1.06847604194372,
12.0269109747433));
#61723=CARTESIAN_POINT('Ctrl Pts',(0.604812308915402,-0.794772683999744,
11.9590489013119));
#61724=CARTESIAN_POINT('Ctrl Pts',(0.617553440481668,-0.636309800094312,
11.8919593671572));
#61725=CARTESIAN_POINT('Ctrl Pts',(0.637867983997188,-0.319434907276715,
11.8189734347907));
#61726=CARTESIAN_POINT('Ctrl Pts',(0.654017685311995,-0.158333333333112,
11.77856682571));
#61727=CARTESIAN_POINT('Ctrl Pts',(0.683031161223074,0.158333333333114,
11.7742147812699));
#61728=CARTESIAN_POINT('Ctrl Pts',(0.695951979822126,0.319434907276722,
11.8101765875292));
#61729=CARTESIAN_POINT('Ctrl Pts',(0.734619603171526,0.636309800094321,
11.8744866608729));
#61730=CARTESIAN_POINT('Ctrl Pts',(0.755655244379573,0.794772683999735,
11.9373347308432));
#61731=CARTESIAN_POINT('Ctrl Pts',(0.807961459846468,1.06847604194528,11.9976281313998));
#61732=CARTESIAN_POINT('Ctrl Pts',(0.834216491313751,1.1851427086134,12.0184458455809));
#61733=CARTESIAN_POINT('Ctrl Pts',(0.864085131708817,1.30000000000302,12.0339824949326));
#61734=CARTESIAN_POINT('Ctrl Pts',(0.63020141310794,-1.2999999999984,12.0800255317113));
#61735=CARTESIAN_POINT('Ctrl Pts',(0.615033907744602,-1.18514270861026,
12.0632398912468));
#61736=CARTESIAN_POINT('Ctrl Pts',(0.605937831805631,-1.06847604194367,
12.0406238643243));
#61737=CARTESIAN_POINT('Ctrl Pts',(0.598950293278431,-0.794772683999704,
11.9749069587294));
#61738=CARTESIAN_POINT('Ctrl Pts',(0.611717138522065,-0.636309800094279,
11.9074519874911));
#61739=CARTESIAN_POINT('Ctrl Pts',(0.632489467969168,-0.319434907276699,
11.8345501240997));
#61740=CARTESIAN_POINT('Ctrl Pts',(0.649593654306062,-0.158333333333104,
11.7935078738823));
#61741=CARTESIAN_POINT('Ctrl Pts',(0.679139447618656,0.158333333333106,
11.7891681687253));
#61742=CARTESIAN_POINT('Ctrl Pts',(0.691964698903671,0.319434907276706,
11.8257791539708));
#61743=CARTESIAN_POINT('Ctrl Pts',(0.73059356723184,0.636309800094288,11.8900278511768));
#61744=CARTESIAN_POINT('Ctrl Pts',(0.751111017380349,0.794772683999695,
11.9532534353523));
#61745=CARTESIAN_POINT('Ctrl Pts',(0.80386579375481,1.06847604194523,12.0114142945674));
#61746=CARTESIAN_POINT('Ctrl Pts',(0.830518240483384,1.18514270861334,12.0307719737918));
#61747=CARTESIAN_POINT('Ctrl Pts',(0.860987546004967,1.30000000000295,12.0443116513584));
#61748=CARTESIAN_POINT('Ctrl Pts',(0.627856112644543,-1.29999999999838,
12.0858800499617));
#61749=CARTESIAN_POINT('Ctrl Pts',(0.612387208051074,-1.18514270861024,
12.0702385265224));
#61750=CARTESIAN_POINT('Ctrl Pts',(0.603066085512306,-1.06847604194365,
12.0484598929655));
#61751=CARTESIAN_POINT('Ctrl Pts',(0.595735034169528,-0.794772683999692,
11.9839689405519));
#61752=CARTESIAN_POINT('Ctrl Pts',(0.60841018552264,-0.63630980009427,11.9163008622495));
#61753=CARTESIAN_POINT('Ctrl Pts',(0.629369647417197,-0.319434907276694,
11.8434463136223));
#61754=CARTESIAN_POINT('Ctrl Pts',(0.64696106719286,-0.158333333333102,
11.8020427839178));
#61755=CARTESIAN_POINT('Ctrl Pts',(0.676787204160346,0.158333333333104,
11.7977112676138));
#61756=CARTESIAN_POINT('Ctrl Pts',(0.689594301071588,0.319434907276702,
11.8346940175172));
#61757=CARTESIAN_POINT('Ctrl Pts',(0.728222636350922,0.63630980009428,11.8989074026291));
#61758=CARTESIAN_POINT('Ctrl Pts',(0.748448052983879,0.794772683999683,
11.9623467578494));
#61759=CARTESIAN_POINT('Ctrl Pts',(0.801484476416064,1.06847604194521,12.0192889798408));
#61760=CARTESIAN_POINT('Ctrl Pts',(0.828377630920278,1.18514270861332,12.0378127284722));
#61761=CARTESIAN_POINT('Ctrl Pts',(0.859206437417904,1.30000000000294,12.050212047752));
#61762=CARTESIAN_POINT('Ctrl Pts',(0.624161576291421,-1.29999999999834,
12.0946516707519));
#61763=CARTESIAN_POINT('Ctrl Pts',(0.608111877397449,-1.18514270861021,
12.0807179966861));
#61764=CARTESIAN_POINT('Ctrl Pts',(0.598390121382353,-1.06847604194362,
12.0601912051343));
#61765=CARTESIAN_POINT('Ctrl Pts',(0.59054973410769,-0.794772683999669,
11.9975387899378));
#61766=CARTESIAN_POINT('Ctrl Pts',(0.603378336192844,-0.636309800094251,
11.9295685320289));
#61767=CARTESIAN_POINT('Ctrl Pts',(0.624724051565348,-0.319434907276684,
11.8567909971145));
#61768=CARTESIAN_POINT('Ctrl Pts',(0.64299874908432,-0.158333333333097,
11.814841382019));
#61769=CARTESIAN_POINT('Ctrl Pts',(0.673200200924868,0.158333333333099,
11.8105216849394));
#61770=CARTESIAN_POINT('Ctrl Pts',(0.685901221470102,0.319434907276692,
11.8480620242187));
#61771=CARTESIAN_POINT('Ctrl Pts',(0.724496564371522,0.63630980009426,11.9122231126468));
#61772=CARTESIAN_POINT('Ctrl Pts',(0.744303193228928,0.794772683999659,
11.9759842154236));
#61773=CARTESIAN_POINT('Ctrl Pts',(0.797802730050058,1.06847604194518,12.0310995623443));
#61774=CARTESIAN_POINT('Ctrl Pts',(0.825082932547686,1.18514270861328,12.0483728427296));
#61775=CARTESIAN_POINT('Ctrl Pts',(0.856485370406105,1.30000000000289,12.0590620120429));
#61776=CARTESIAN_POINT('Ctrl Pts',(0.619749336779534,-1.29999999999813,
12.104870548424));
#61777=CARTESIAN_POINT('Ctrl Pts',(0.602682915760704,-1.18514270861001,
12.0929135692186));
#61778=CARTESIAN_POINT('Ctrl Pts',(0.592312141089411,-1.06847604194344,
12.0738387098464));
#61779=CARTESIAN_POINT('Ctrl Pts',(0.583821859454634,-0.794772683999537,
12.0133282416719));
#61780=CARTESIAN_POINT('Ctrl Pts',(0.597458428936834,-0.636309800094145,
11.9450334137923));
#61781=CARTESIAN_POINT('Ctrl Pts',(0.619488733694328,-0.319434907276631,
11.8723573671982));
#61782=CARTESIAN_POINT('Ctrl Pts',(0.638601914260369,-0.158333333333071,
11.8297699041693));
#61783=CARTESIAN_POINT('Ctrl Pts',(0.668949937282336,0.158333333333073,
11.8254615373418));
#61784=CARTESIAN_POINT('Ctrl Pts',(0.68092804808564,0.319434907276639,11.8636444166396));
#61785=CARTESIAN_POINT('Ctrl Pts',(0.719200496987211,0.636309800094155,
11.9277406171235));
#61786=CARTESIAN_POINT('Ctrl Pts',(0.738593692950098,0.794772683999528,
11.9918766932466));
#61787=CARTESIAN_POINT('Ctrl Pts',(0.792873086952508,1.068476041945,12.0448646804517));
#61788=CARTESIAN_POINT('Ctrl Pts',(0.820774824770173,1.18514270861309,12.0606821506067));
#61789=CARTESIAN_POINT('Ctrl Pts',(0.853082761991445,1.30000000000268,12.069380554654));
#61790=CARTESIAN_POINT('Ctrl Pts',(0.615467141218366,-1.29999999999805,
12.1150930403923));
#61791=CARTESIAN_POINT('Ctrl Pts',(0.597625820552847,-1.18514270860994,
12.1051224765165));
#61792=CARTESIAN_POINT('Ctrl Pts',(0.586724619994118,-1.06847604194338,
12.0875038092771));
#61793=CARTESIAN_POINT('Ctrl Pts',(0.577573731738714,-0.794772683999492,
12.0291325145843));
#61794=CARTESIAN_POINT('Ctrl Pts',(0.591441124832637,-0.636309800094109,
11.9604851530946));
#61795=CARTESIAN_POINT('Ctrl Pts',(0.614019250197833,-0.319434907276613,
11.8879041059066));
#61796=CARTESIAN_POINT('Ctrl Pts',(0.634168133697368,-0.158333333333062,
11.8446920128823));
#61797=CARTESIAN_POINT('Ctrl Pts',(0.664825533059683,0.158333333333064,
11.8403984497482));
#61798=CARTESIAN_POINT('Ctrl Pts',(0.676259290560238,0.319434907276621,
11.8792215022969));
#61799=CARTESIAN_POINT('Ctrl Pts',(0.714243429693531,0.636309800094118,
11.9432513509972));
#61800=CARTESIAN_POINT('Ctrl Pts',(0.73306672545194,0.794772683999482,12.007759507101));
#61801=CARTESIAN_POINT('Ctrl Pts',(0.78803548171108,1.06847604194494,12.058621077946));
#61802=CARTESIAN_POINT('Ctrl Pts',(0.816526615288474,1.18514270861302,12.0729840605242));
#61803=CARTESIAN_POINT('Ctrl Pts',(0.849714944651654,1.30000000000261,12.0796939362685));
#61804=CARTESIAN_POINT('Ctrl Pts',(0.612875854852303,-1.29999999999804,
12.120923162107));
#61805=CARTESIAN_POINT('Ctrl Pts',(0.594468444044198,-1.18514270860993,
12.1120779219025));
#61806=CARTESIAN_POINT('Ctrl Pts',(0.583206793009732,-1.06847604194337,
12.0952865642195));
#61807=CARTESIAN_POINT('Ctrl Pts',(0.573698260816,-0.794772683999482,12.0381380478815));
#61808=CARTESIAN_POINT('Ctrl Pts',(0.588052060272601,-0.636309800094101,
11.9693126236165));
#61809=CARTESIAN_POINT('Ctrl Pts',(0.61095813111931,-0.319434907276609,
11.8967910853841));
#61810=CARTESIAN_POINT('Ctrl Pts',(0.631389225007648,-0.15833333333306,
11.853210394178));
#61811=CARTESIAN_POINT('Ctrl Pts',(0.662219798857672,0.158333333333062,
11.8489248608128));
#61812=CARTESIAN_POINT('Ctrl Pts',(0.673542143115433,0.319434907276617,
11.8881199204326));
#61813=CARTESIAN_POINT('Ctrl Pts',(0.71155592320357,0.63630980009411,11.952116028638));
#61814=CARTESIAN_POINT('Ctrl Pts',(0.730260496834435,0.794772683999472,
12.0168389022997));
#61815=CARTESIAN_POINT('Ctrl Pts',(0.78559404428569,1.06847604194493,12.0664856050893));
#61816=CARTESIAN_POINT('Ctrl Pts',(0.814343552157919,1.185142708613,12.080016779632));
#61817=CARTESIAN_POINT('Ctrl Pts',(0.847890725520545,1.30000000000259,12.0855889106711));
#61818=CARTESIAN_POINT('Ctrl Pts',(0.610887521890204,-1.29999999999802,
12.1252916341884));
#61819=CARTESIAN_POINT('Ctrl Pts',(0.592006378682212,-1.18514270860991,
12.1172867448402));
#61820=CARTESIAN_POINT('Ctrl Pts',(0.580449617324699,-1.06847604194335,
12.1011139887057));
#61821=CARTESIAN_POINT('Ctrl Pts',(0.57067197397883,-0.794772683999469,
12.0448822804338));
#61822=CARTESIAN_POINT('Ctrl Pts',(0.585512953505324,-0.636309800094091,
11.9759310928786));
#61823=CARTESIAN_POINT('Ctrl Pts',(0.608669395392358,-0.319434907276604,
11.9034560993797));
#61824=CARTESIAN_POINT('Ctrl Pts',(0.62920984988828,-0.158333333333057,
11.8595955660245));
#61825=CARTESIAN_POINT('Ctrl Pts',(0.660165216176782,0.158333333333059,
11.8553160338946));
#61826=CARTESIAN_POINT('Ctrl Pts',(0.671462899317354,0.319434907276612,
11.8947918593629));
#61827=CARTESIAN_POINT('Ctrl Pts',(0.709562168025446,0.6363098000941,11.9587639894938));
#61828=CARTESIAN_POINT('Ctrl Pts',(0.728249453803018,0.794772683999459,
12.023648584504));
#61829=CARTESIAN_POINT('Ctrl Pts',(0.783854550106997,1.06847604194491,12.0723844674039));
#61830=CARTESIAN_POINT('Ctrl Pts',(0.812776317227144,1.18514270861299,12.0852917383376));
#61831=CARTESIAN_POINT('Ctrl Pts',(0.846550465649136,1.30000000000257,12.0900103223398));
#61832=CARTESIAN_POINT('Ctrl Pts',(0.608881776228894,-1.29999999999798,
12.1296579890848));
#61833=CARTESIAN_POINT('Ctrl Pts',(0.589506189731673,-1.18514270860988,
12.12249184714));
#61834=CARTESIAN_POINT('Ctrl Pts',(0.577641880738069,-1.06847604194333,
12.1069367182218));
#61835=CARTESIAN_POINT('Ctrl Pts',(0.567585507175229,-0.794772683999451,
12.0516210205087));
#61836=CARTESIAN_POINT('Ctrl Pts',(0.582946263395987,-0.636309800094076,
11.982545953206));
#61837=CARTESIAN_POINT('Ctrl Pts',(0.606351309519338,-0.319434907276596,
11.9101183918654));
#61838=CARTESIAN_POINT('Ctrl Pts',(0.626975530392277,-0.158333333333053,
11.8659782356395));
#61839=CARTESIAN_POINT('Ctrl Pts',(0.658049576929821,0.158333333333055,
11.8617050272318));
#61840=CARTESIAN_POINT('Ctrl Pts',(0.66932884207984,0.319434907276604,11.9014615037808));
#61841=CARTESIAN_POINT('Ctrl Pts',(0.707529882837701,0.636309800094085,
11.9654098692974));
#61842=CARTESIAN_POINT('Ctrl Pts',(0.726221780561683,0.794772683999441,
12.0304562908449));
#61843=CARTESIAN_POINT('Ctrl Pts',(0.782113312648036,1.06847604194489,12.0782818608322));
#61844=CARTESIAN_POINT('Ctrl Pts',(0.811211199795286,1.18514270861296,12.0905655177454));
#61845=CARTESIAN_POINT('Ctrl Pts',(0.845213600834787,1.30000000000254,12.0944309144363));
#61846=CARTESIAN_POINT('Ctrl Pts',(0.606906390042853,-1.29999999999795,
12.1340256154503));
#61847=CARTESIAN_POINT('Ctrl Pts',(0.58706541570433,-1.18514270860985,12.1277000610048));
#61848=CARTESIAN_POINT('Ctrl Pts',(0.574903502850208,-1.0684760419433,12.1127631645127));
#61849=CARTESIAN_POINT('Ctrl Pts',(0.564547219394806,-0.794772683999432,
12.0583620226792));
#61850=CARTESIAN_POINT('Ctrl Pts',(0.580312530161547,-0.636309800094061,
11.9891555586623));
#61851=CARTESIAN_POINT('Ctrl Pts',(0.603951989620995,-0.319434907276589,
11.9167744619309));
#61852=CARTESIAN_POINT('Ctrl Pts',(0.624751753109886,-0.158333333333049,
11.8723601588131));
#61853=CARTESIAN_POINT('Ctrl Pts',(0.655942851254485,0.158333333333052,
11.8680941065743));
#61854=CARTESIAN_POINT('Ctrl Pts',(0.667141013668526,0.319434907276596,
11.9081285729616));
#61855=CARTESIAN_POINT('Ctrl Pts',(0.705392125245831,0.63630980009407,11.9720517992652));
#61856=CARTESIAN_POINT('Ctrl Pts',(0.724031221176676,0.794772683999421,
12.0372592228598));
#61857=CARTESIAN_POINT('Ctrl Pts',(0.780241753093799,1.06847604194486,12.0841751634707));
#61858=CARTESIAN_POINT('Ctrl Pts',(0.809553287601487,1.18514270861293,12.0958359487701));
#61859=CARTESIAN_POINT('Ctrl Pts',(0.843844900155231,1.30000000000251,12.0988493470852));
#61860=CARTESIAN_POINT('Ctrl Pts',(0.605306250790031,-1.29999999999793,
12.1376678988936));
#61861=CARTESIAN_POINT('Ctrl Pts',(0.58512674498234,-1.18514270860983,12.1320459852867));
#61862=CARTESIAN_POINT('Ctrl Pts',(0.572736658115396,-1.06847604194328,
12.1176255286028));
#61863=CARTESIAN_POINT('Ctrl Pts',(0.562108194845417,-0.794772683999416,
12.0639849942102));
#61864=CARTESIAN_POINT('Ctrl Pts',(0.578043239721755,-0.636309800094048,
11.9946583851704));
#61865=CARTESIAN_POINT('Ctrl Pts',(0.601859231195697,-0.319434907276582,
11.9223142599912));
#61866=CARTESIAN_POINT('Ctrl Pts',(0.622935554994119,-0.158333333333046,
11.8776783729586));
#61867=CARTESIAN_POINT('Ctrl Pts',(0.654225922229719,0.158333333333048,
11.8734192056745));
#61868=CARTESIAN_POINT('Ctrl Pts',(0.665275576234766,0.31943490727659,11.9136820531298));
#61869=CARTESIAN_POINT('Ctrl Pts',(0.703493731277744,0.636309800094057,
11.9775825108839));
#61870=CARTESIAN_POINT('Ctrl Pts',(0.722000803806554,0.794772683999405,
12.0429229622622));
#61871=CARTESIAN_POINT('Ctrl Pts',(0.778511064718178,1.06847604194484,12.0890815767378));
#61872=CARTESIAN_POINT('Ctrl Pts',(0.808047250965803,1.1851427086129,12.1002241597667));
#61873=CARTESIAN_POINT('Ctrl Pts',(0.842658425423753,1.30000000000248,12.102528971963));
#61874=CARTESIAN_POINT('Ctrl Pts',(0.604285083056295,-1.29999999999792,
12.1400363911309));
#61875=CARTESIAN_POINT('Ctrl Pts',(0.583906288881377,-1.18514270860982,
12.1348731089851));
#61876=CARTESIAN_POINT('Ctrl Pts',(0.571376200341018,-1.06847604194327,
12.1207888249669));
#61877=CARTESIAN_POINT('Ctrl Pts',(0.560561269321183,-0.794772683999411,
12.0676420123679));
#61878=CARTESIAN_POINT('Ctrl Pts',(0.576537005022671,-0.636309800094044,
11.9982329662929));
#61879=CARTESIAN_POINT('Ctrl Pts',(0.600457349747139,-0.31943490727658,
11.9259120320742));
#61880=CARTESIAN_POINT('Ctrl Pts',(0.621762735057343,-0.158333333333045,
11.8811346916932));
#61881=CARTESIAN_POINT('Ctrl Pts',(0.653118547739335,0.158333333333047,
11.8768803927112));
#61882=CARTESIAN_POINT('Ctrl Pts',(0.664043720438682,0.319434907276588,
11.9172906141691));
#61883=CARTESIAN_POINT('Ctrl Pts',(0.70221111520551,0.636309800094053,11.9811756537776));
#61884=CARTESIAN_POINT('Ctrl Pts',(0.720594222382496,0.794772683999401,
12.0466020212848));
#61885=CARTESIAN_POINT('Ctrl Pts',(0.777311411198164,1.06847604194483,12.092268747927));
#61886=CARTESIAN_POINT('Ctrl Pts',(0.807011834517717,1.1851427086129,12.1030749121673));
#61887=CARTESIAN_POINT('Ctrl Pts',(0.841861911697297,1.30000000000247,12.1049198068032));
#61888=CARTESIAN_POINT('Ctrl Pts',(0.603815899220733,-1.29999999999792,
12.1411296230263));
#61889=CARTESIAN_POINT('Ctrl Pts',(0.583347471311102,-1.18514270860982,
12.1361781416372));
#61890=CARTESIAN_POINT('Ctrl Pts',(0.570753626107481,-1.06847604194327,
12.1222490532589));
#61891=CARTESIAN_POINT('Ctrl Pts',(0.559851185652774,-0.794772683999409,
12.0693300044916));
#61892=CARTESIAN_POINT('Ctrl Pts',(0.575837369233593,-0.636309800094043,
11.9998824067175));
#61893=CARTESIAN_POINT('Ctrl Pts',(0.599803987165821,-0.31943490727658,
11.9275720589377));
#61894=CARTESIAN_POINT('Ctrl Pts',(0.621219922477897,-0.158333333333045,
11.8827297039398));
#61895=CARTESIAN_POINT('Ctrl Pts',(0.652606018081053,0.158333333333047,
11.8784777079958));
#61896=CARTESIAN_POINT('Ctrl Pts',(0.663471519768857,0.319434907276587,
11.9189558690088));
#61897=CARTESIAN_POINT('Ctrl Pts',(0.701612372747973,0.636309800094052,
11.9828337465353));
#61898=CARTESIAN_POINT('Ctrl Pts',(0.719933452155873,0.794772683999399,
12.0482996836085));
#61899=CARTESIAN_POINT('Ctrl Pts',(0.77674737768157,1.06847604194483,12.093739461978));
#61900=CARTESIAN_POINT('Ctrl Pts',(0.806525649454242,1.1851427086129,12.1043904270862));
#61901=CARTESIAN_POINT('Ctrl Pts',(0.841489549802737,1.30000000000247,12.1060231609561));
#61902=CARTESIAN_POINT('Ctrl Pts',(0.603581710836913,-1.29999999999792,
12.1416762537866));
#61903=CARTESIAN_POINT('Ctrl Pts',(0.583068922644597,-1.18514270860982,
12.1368306966218));
#61904=CARTESIAN_POINT('Ctrl Pts',(0.570443366248212,-1.06847604194327,
12.1229792133864));
#61905=CARTESIAN_POINT('Ctrl Pts',(0.559496888522581,-0.79477268399941,
12.0701740252806));
#61906=CARTESIAN_POINT('Ctrl Pts',(0.575486671213716,-0.636309800094043,
12.0007070539529));
#61907=CARTESIAN_POINT('Ctrl Pts',(0.599476059838051,-0.31943490727658,
11.9284019768101));
#61908=CARTESIAN_POINT('Ctrl Pts',(0.620948214103655,-0.158333333333045,
11.8835271674347));
#61909=CARTESIAN_POINT('Ctrl Pts',(0.652349472132746,0.158333333333047,
11.8792763341935));
#61910=CARTESIAN_POINT('Ctrl Pts',(0.663184708296504,0.319434907276587,
11.9197884496198));
#61911=CARTESIAN_POINT('Ctrl Pts',(0.701311694856169,0.636309800094052,
11.9836627377277));
#61912=CARTESIAN_POINT('Ctrl Pts',(0.719600847373781,0.794772683999399,
12.049148444006));
#61913=CARTESIAN_POINT('Ctrl Pts',(0.776463368826196,1.06847604194483,12.0944747635993));
#61914=CARTESIAN_POINT('Ctrl Pts',(0.806280949610835,1.1851427086129,12.1050481430266));
#61915=CARTESIAN_POINT('Ctrl Pts',(0.841302432607243,1.30000000000247,12.1065748176348));
#61916=CARTESIAN_POINT('Ctrl Pts',(0.603386782454753,-1.29999999999792,
12.1421317832905));
#61917=CARTESIAN_POINT('Ctrl Pts',(0.582837263443985,-1.18514270860982,
12.1373745060256));
#61918=CARTESIAN_POINT('Ctrl Pts',(0.570185353761598,-1.06847604194327,
12.1235876951198));
#61919=CARTESIAN_POINT('Ctrl Pts',(0.559201968849319,-0.794772683999408,
12.0708773748228));
#61920=CARTESIAN_POINT('Ctrl Pts',(0.575193834867384,-0.636309800094042,
12.0013942059284));
#61921=CARTESIAN_POINT('Ctrl Pts',(0.599201878836009,-0.319434907276579,
11.9290935048279));
#61922=CARTESIAN_POINT('Ctrl Pts',(0.620721225877243,-0.158333333333045,
11.8841916730529));
#61923=CARTESIAN_POINT('Ctrl Pts',(0.652135121329545,0.158333333333047,
11.8799418160112));
#61924=CARTESIAN_POINT('Ctrl Pts',(0.662945093381664,0.319434907276587,
11.9204822267212));
#61925=CARTESIAN_POINT('Ctrl Pts',(0.701060240529716,0.636309800094051,
11.9843535229102));
#61926=CARTESIAN_POINT('Ctrl Pts',(0.719322187748478,0.794772683999398,
12.0498556904397));
#61927=CARTESIAN_POINT('Ctrl Pts',(0.776225303499505,1.06847604194483,12.0950874746472));
#61928=CARTESIAN_POINT('Ctrl Pts',(0.806075850100194,1.18514270861289,12.105596210833));
#61929=CARTESIAN_POINT('Ctrl Pts',(0.841145692960999,1.30000000000247,12.1070345198236));
#61930=CARTESIAN_POINT('Ctrl Pts',(0.603250458156735,-1.29999999999792,
12.1424506569694));
#61931=CARTESIAN_POINT('Ctrl Pts',(0.582675401104163,-1.18514270860982,
12.1377551837426));
#61932=CARTESIAN_POINT('Ctrl Pts',(0.570005106414889,-1.06847604194327,
12.1240136455603));
#61933=CARTESIAN_POINT('Ctrl Pts',(0.558995773400406,-0.794772683999409,
12.0713697236677));
#61934=CARTESIAN_POINT('Ctrl Pts',(0.574988458255701,-0.636309800094042,
12.0018751789434));
#61935=CARTESIAN_POINT('Ctrl Pts',(0.599009439913919,-0.319434907276579,
11.929577533758));
#61936=CARTESIAN_POINT('Ctrl Pts',(0.620562232944649,-0.158333333333045,
11.8846568094334));
#61937=CARTESIAN_POINT('Ctrl Pts',(0.651984994328979,0.158333333333047,
11.8804076406294));
#61938=CARTESIAN_POINT('Ctrl Pts',(0.662777078632811,0.319434907276587,
11.9209678497561));
#61939=CARTESIAN_POINT('Ctrl Pts',(0.700883715604501,0.636309800094051,
11.9848370486251));
#61940=CARTESIAN_POINT('Ctrl Pts',(0.719126316881295,0.794772683999399,
12.0503507353582));
#61941=CARTESIAN_POINT('Ctrl Pts',(0.776057933517928,1.06847604194483,12.095516351444));
#61942=CARTESIAN_POINT('Ctrl Pts',(0.805931692314347,1.18514270861289,12.1059798427101));
#61943=CARTESIAN_POINT('Ctrl Pts',(0.841035622589297,1.30000000000247,12.1073563035896));
#61944=CARTESIAN_POINT('Ctrl Pts',(0.603172548320683,-1.29999999999791,
12.1426328672716));
#61945=CARTESIAN_POINT('Ctrl Pts',(0.582582836069079,-1.18514270860982,
12.1379727059308));
#61946=CARTESIAN_POINT('Ctrl Pts',(0.569902001416967,-1.06847604194327,
12.1242570353342));
#61947=CARTESIAN_POINT('Ctrl Pts',(0.558877825998678,-0.794772683999409,
12.0716510545165));
#61948=CARTESIAN_POINT('Ctrl Pts',(0.574871154895082,-0.636309800094042,
12.0021500208177));
#61949=CARTESIAN_POINT('Ctrl Pts',(0.598899431395806,-0.319434907276579,
11.9298541192445));
#61950=CARTESIAN_POINT('Ctrl Pts',(0.620471004332286,-0.158333333333045,
11.8849225841299));
#61951=CARTESIAN_POINT('Ctrl Pts',(0.651898805737524,0.158333333333047,
11.8806738081012));
#61952=CARTESIAN_POINT('Ctrl Pts',(0.662680942569796,0.319434907276587,
11.9212453435713));
#61953=CARTESIAN_POINT('Ctrl Pts',(0.700782825985886,0.636309800094051,
11.985113348793));
#61954=CARTESIAN_POINT('Ctrl Pts',(0.719014349215731,0.794772683999398,
12.0506336128885));
#61955=CARTESIAN_POINT('Ctrl Pts',(0.775962198276967,1.06847604194483,12.0957614210369));
#61956=CARTESIAN_POINT('Ctrl Pts',(0.805849179745395,1.18514270861289,12.1061990601445));
#61957=CARTESIAN_POINT('Ctrl Pts',(0.840972528949222,1.30000000000247,12.107540182362));
#61958=CARTESIAN_POINT('Ctrl Pts',(0.600643530861967,-1.29999999999796,
12.1485549289069));
#61959=CARTESIAN_POINT('Ctrl Pts',(0.579584823952958,-1.18514270860986,
12.1450428386672));
#61960=CARTESIAN_POINT('Ctrl Pts',(0.56656473266857,-1.06847604194331,12.1321680482343));
#61961=CARTESIAN_POINT('Ctrl Pts',(0.55505652735372,-0.794772683999437,
12.0807949962933));
#61962=CARTESIAN_POINT('Ctrl Pts',(0.571046633027255,-0.636309800094064,
12.0110815971801));
#61963=CARTESIAN_POINT('Ctrl Pts',(0.595315222693786,-0.31943490727659,
11.938842369259));
#61964=CARTESIAN_POINT('Ctrl Pts',(0.61752567296301,-0.15833333333305,11.8935608790396));
#61965=CARTESIAN_POINT('Ctrl Pts',(0.649119349189772,0.158333333333052,
11.8893250071093));
#61966=CARTESIAN_POINT('Ctrl Pts',(0.659557679761414,0.319434907276598,
11.9302636958771));
#61967=CARTESIAN_POINT('Ctrl Pts',(0.697493961619743,0.636309800094073,
11.9940925654044));
#61968=CARTESIAN_POINT('Ctrl Pts',(0.715360551785109,0.794772683999426,
12.0598268264269));
#61969=CARTESIAN_POINT('Ctrl Pts',(0.772840883424242,1.06847604194487,12.1037258900667));
#61970=CARTESIAN_POINT('Ctrl Pts',(0.803162869925518,1.18514270861294,12.1133233314549));
#61971=CARTESIAN_POINT('Ctrl Pts',(0.838925737217494,1.30000000000251,12.1135159362019));
#61972=CARTESIAN_POINT('Ctrl Pts',(0.595485031953642,-1.29999999999867,
12.1602434858869));
#61973=CARTESIAN_POINT('Ctrl Pts',(0.573241290581446,-1.18514270861051,
12.1589798784746));
#61974=CARTESIAN_POINT('Ctrl Pts',(0.559414705256469,-1.06847604194389,
12.1477561964616));
#61975=CARTESIAN_POINT('Ctrl Pts',(0.546917841472229,-0.794772683999873,
12.0988174808883));
#61976=CARTESIAN_POINT('Ctrl Pts',(0.56360172731629,-0.636309800094413,
12.0287328666738));
#61977=CARTESIAN_POINT('Ctrl Pts',(0.588134026213673,-0.319434907276765,
11.9566036793466));
#61978=CARTESIAN_POINT('Ctrl Pts',(0.610582825305128,-0.158333333333137,
11.9105839829202));
#61979=CARTESIAN_POINT('Ctrl Pts',(0.642469543617756,0.158333333333139,
11.9063714642218));
#61980=CARTESIAN_POINT('Ctrl Pts',(0.653078416052506,0.319434907276774,
11.9480710018856));
#61981=CARTESIAN_POINT('Ctrl Pts',(0.691111919053413,0.636309800094423,
12.0118388469959));
#61982=CARTESIAN_POINT('Ctrl Pts',(0.708360915710318,0.794772683999862,
12.0779886723153));
#61983=CARTESIAN_POINT('Ctrl Pts',(0.766684612953707,1.06847604194545,12.119467236768));
#61984=CARTESIAN_POINT('Ctrl Pts',(0.797667728588445,1.18514270861359,12.1274091500634));
#61985=CARTESIAN_POINT('Ctrl Pts',(0.834387792427035,1.30000000000323,12.1253384430347));
#61986=CARTESIAN_POINT('Ctrl Pts',(0.587185078806851,-1.29999999999891,
12.1776573032884));
#61987=CARTESIAN_POINT('Ctrl Pts',(0.562993490899537,-1.18514270861072,
12.1797310055913));
#61988=CARTESIAN_POINT('Ctrl Pts',(0.547883421785488,-1.06847604194409,
12.1709617431183));
#61989=CARTESIAN_POINT('Ctrl Pts',(0.533956264537119,-0.794772684000015,
12.1256535747606));
#61990=CARTESIAN_POINT('Ctrl Pts',(0.551875880532105,-0.636309800094528,
12.0550347186061));
#61991=CARTESIAN_POINT('Ctrl Pts',(0.577514735286172,-0.319434907276823,
11.9831127855141));
#61992=CARTESIAN_POINT('Ctrl Pts',(0.601418710125038,-0.158333333333166,
11.9360515158364));
#61993=CARTESIAN_POINT('Ctrl Pts',(0.633873956312172,0.158333333333168,
11.9318854240732));
#61994=CARTESIAN_POINT('Ctrl Pts',(0.643459387532714,0.31943490727683,11.9746628061304));
#61995=CARTESIAN_POINT('Ctrl Pts',(0.681823023208725,0.636309800094536,
12.038338651949));
#61996=CARTESIAN_POINT('Ctrl Pts',(0.699858850607088,0.794772684000005,
12.105164341511));
#61997=CARTESIAN_POINT('Ctrl Pts',(0.759403760308767,1.06847604194565,12.1430273132517));
#61998=CARTESIAN_POINT('Ctrl Pts',(0.790999049044779,1.1851427086138,12.1484856809274));
#61999=CARTESIAN_POINT('Ctrl Pts',(0.8284148414631,1.30000000000346,12.1430129387736));
#62000=CARTESIAN_POINT('Ctrl Pts',(0.579506951612649,-1.2999999999997,12.1950893665228));
#62001=CARTESIAN_POINT('Ctrl Pts',(0.553345502078091,-1.18514270861144,
12.2004957811793));
#62002=CARTESIAN_POINT('Ctrl Pts',(0.536920448834634,-1.06847604194474,
12.1941774992085));
#62003=CARTESIAN_POINT('Ctrl Pts',(0.521468313213451,-0.794772684000499,
12.1524946091617));
#62004=CARTESIAN_POINT('Ctrl Pts',(0.540639835639615,-0.636309800094918,
12.0813512164322));
#62005=CARTESIAN_POINT('Ctrl Pts',(0.567046541242541,-0.319434907277021,
12.009617450558));
#62006=CARTESIAN_POINT('Ctrl Pts',(0.591913503988528,-0.158333333333263,
11.9614795037667));
#62007=CARTESIAN_POINT('Ctrl Pts',(0.624684878793728,0.158333333333265,
11.9573439230541));
#62008=CARTESIAN_POINT('Ctrl Pts',(0.633791842433493,0.319434907277025,
12.0012228555678));
#62009=CARTESIAN_POINT('Ctrl Pts',(0.671688556708476,0.636309800094926,
12.0647841665863));
#62010=CARTESIAN_POINT('Ctrl Pts',(0.688016865714616,0.794772684000495,
12.1322217064504));
#62011=CARTESIAN_POINT('Ctrl Pts',(0.749472591398532,1.0684760419463,12.1664696953007));
#62012=CARTESIAN_POINT('Ctrl Pts',(0.782693584574102,1.18514270861453,12.1694595734739));
#62013=CARTESIAN_POINT('Ctrl Pts',(0.822533664435534,1.30000000000426,12.1606146444599));
#62014=CARTESIAN_POINT('Ctrl Pts',(0.573578201915757,-1.30000000000028,
12.2066602306644));
#62015=CARTESIAN_POINT('Ctrl Pts',(0.546373190975778,-1.18514270861197,
12.2142950671844));
#62016=CARTESIAN_POINT('Ctrl Pts',(0.529208707811323,-1.06847604194521,
12.2096111059055));
#62017=CARTESIAN_POINT('Ctrl Pts',(0.512750945720502,-0.794772684000851,
12.1703313310453));
#62018=CARTESIAN_POINT('Ctrl Pts',(0.532138549719906,-0.636309800095197,
12.0987891640359));
#62019=CARTESIAN_POINT('Ctrl Pts',(0.558956795859338,-0.319434907277159,
12.0271831232441));
#62020=CARTESIAN_POINT('Ctrl Pts',(0.584631254886148,-0.158333333333332,
11.9783681315311));
#62021=CARTESIAN_POINT('Ctrl Pts',(0.618034103223892,0.158333333333334,
11.9742859986132));
#62022=CARTESIAN_POINT('Ctrl Pts',(0.627223601649686,0.319434907277167,
12.0189115172152));
#62023=CARTESIAN_POINT('Ctrl Pts',(0.665468378425724,0.636309800095206,
12.0824211914211));
#62024=CARTESIAN_POINT('Ctrl Pts',(0.681689914147691,0.79477268400084,12.1502814912943));
#62025=CARTESIAN_POINT('Ctrl Pts',(0.743851598608587,1.06847604194677,12.1821291336617));
#62026=CARTESIAN_POINT('Ctrl Pts',(0.777519991844039,1.18514270861505,12.1834743205671));
#62027=CARTESIAN_POINT('Ctrl Pts',(0.817949288429029,1.30000000000483,12.1723790300684));
#62028=CARTESIAN_POINT('Ctrl Pts',(0.57067025537727,-1.30000000000028,12.2124460829627));
#62029=CARTESIAN_POINT('Ctrl Pts',(0.542940786613358,-1.18514270861197,
12.2211942845405));
#62030=CARTESIAN_POINT('Ctrl Pts',(0.525404772703435,-1.06847604194521,
12.2173269808077));
#62031=CARTESIAN_POINT('Ctrl Pts',(0.508441992410329,-0.794772684000851,
12.1792483945427));
#62032=CARTESIAN_POINT('Ctrl Pts',(0.52791511722475,-0.636309800095197,
12.107507287942));
#62033=CARTESIAN_POINT('Ctrl Pts',(0.554987172141785,-0.319434907277159,
12.0359668790037));
#62034=CARTESIAN_POINT('Ctrl Pts',(0.581221077759065,-0.158333333333332,
11.9868187308123));
#62035=CARTESIAN_POINT('Ctrl Pts',(0.614857791973618,0.158333333333334,
11.9827589718209));
#62036=CARTESIAN_POINT('Ctrl Pts',(0.623796233999667,0.319434907277167,
12.0277447643876));
#62037=CARTESIAN_POINT('Ctrl Pts',(0.662111769288738,0.636309800095206,
12.0912247185273));
#62038=CARTESIAN_POINT('Ctrl Pts',(0.678359592024736,0.79477268400084,12.1593033180431));
#62039=CARTESIAN_POINT('Ctrl Pts',(0.74098795051949,1.06847604194677,12.1899531249437));
#62040=CARTESIAN_POINT('Ctrl Pts',(0.774949037062868,1.18514270861505,12.1904765350795));
#62041=CARTESIAN_POINT('Ctrl Pts',(0.81576171436643,1.30000000000483,12.178256189631));
#62042=CARTESIAN_POINT('',(0.819125420164991,1.2,12.0817551706368));
#62043=CARTESIAN_POINT('Ctrl Pts',(0.819125420164991,1.2,12.0817551706368));
#62044=CARTESIAN_POINT('Ctrl Pts',(0.830644422591068,1.2183776817245,12.061187766347));
#62045=CARTESIAN_POINT('Ctrl Pts',(0.843273624387522,1.23628901120912,12.0408328984551));
#62046=CARTESIAN_POINT('Ctrl Pts',(0.866362035602099,1.27375689806004,11.9986871795306));
#62047=CARTESIAN_POINT('Ctrl Pts',(0.875510184622732,1.2880705970965,11.9824605692077));
#62048=CARTESIAN_POINT('Ctrl Pts',(0.882649956912143,1.30000000000362,11.969007134984));
#62049=CARTESIAN_POINT('',(0.664237960863694,0.65383484145594,12.1052306705389));
#62050=CARTESIAN_POINT('Ctrl Pts',(0.664237960894242,0.653834841448649,
12.1052306705503));
#62051=CARTESIAN_POINT('Ctrl Pts',(0.678771402050763,0.711663049082454,
12.1032626360241));
#62052=CARTESIAN_POINT('Ctrl Pts',(0.694178908180175,0.767421706161028,
12.1011084974005));
#62053=CARTESIAN_POINT('Ctrl Pts',(0.744496374024038,0.949876651320734,
12.0938180273354));
#62054=CARTESIAN_POINT('Ctrl Pts',(0.780817741461556,1.07527000774591,12.0881829394037));
#62055=CARTESIAN_POINT('Ctrl Pts',(0.81912542016499,1.2,12.0817551706368));
#62056=CARTESIAN_POINT('',(0.525742999963518,-0.653834841531101,12.1220010461183));
#62057=CARTESIAN_POINT('Ctrl Pts',(0.525742999963527,-0.653834841531115,
12.1220010461183));
#62058=CARTESIAN_POINT('Ctrl Pts',(0.539190022298025,-0.575736048549707,
12.0825245635937));
#62059=CARTESIAN_POINT('Ctrl Pts',(0.55145350222942,-0.493707176825078,
12.0495991382559));
#62060=CARTESIAN_POINT('Ctrl Pts',(0.571106258772745,-0.338050175537241,
12.0029165481558));
#62061=CARTESIAN_POINT('Ctrl Pts',(0.579194577471218,-0.265591481216425,
11.9869422768981));
#62062=CARTESIAN_POINT('Ctrl Pts',(0.593836166316479,-0.129668288621025,
11.9674504522924));
#62063=CARTESIAN_POINT('Ctrl Pts',(0.600389101024186,-0.0666199245840123,
11.9624587608477));
#62064=CARTESIAN_POINT('Ctrl Pts',(0.613515992006829,0.0594914647288782,
11.9604922996646));
#62065=CARTESIAN_POINT('Ctrl Pts',(0.62016841052224,0.122683940931368,11.9634887161708));
#62066=CARTESIAN_POINT('Ctrl Pts',(0.633865216238478,0.26005354284401,11.9789549475266));
#62067=CARTESIAN_POINT('Ctrl Pts',(0.640796190912842,0.333934236185787,
11.9930603476798));
#62068=CARTESIAN_POINT('Ctrl Pts',(0.653731520036761,0.491651609165574,
12.0361172105966));
#62069=CARTESIAN_POINT('Ctrl Pts',(0.659778232475277,0.575076596064635,
12.0673420839221));
#62070=CARTESIAN_POINT('Ctrl Pts',(0.664237960911195,0.653834841464539,
12.1052306705154));
#62071=CARTESIAN_POINT('',(0.597524573714823,-1.2,12.1138034539252));
#62072=CARTESIAN_POINT('Ctrl Pts',(0.597524573714823,-1.2,12.1138034539252));
#62073=CARTESIAN_POINT('Ctrl Pts',(0.58514630377234,-1.1341651966939,12.1153086668504));
#62074=CARTESIAN_POINT('Ctrl Pts',(0.569018766055164,-1.03862960183204,
12.1172216138762));
#62075=CARTESIAN_POINT('Ctrl Pts',(0.533638828669213,-0.766812999705298,
12.1211801707249));
#62076=CARTESIAN_POINT('Ctrl Pts',(0.530556512233154,-0.718567421671387,
12.121486891335));
#62077=CARTESIAN_POINT('Ctrl Pts',(0.525742999963529,-0.6538348415311,12.1220010461183));
#62078=CARTESIAN_POINT('Ctrl Pts',(0.65906282859866,-1.29999999999906,12.005011570014));
#62079=CARTESIAN_POINT('Ctrl Pts',(0.648887062337683,-1.28291444576899,
12.0236528169717));
#62080=CARTESIAN_POINT('Ctrl Pts',(0.638372322676667,-1.26592287187928,
12.0421942540332));
#62081=CARTESIAN_POINT('Ctrl Pts',(0.623146285770558,-1.24020469105829,
12.0700941915526));
#62082=CARTESIAN_POINT('Ctrl Pts',(0.610885738061428,-1.21949365620403,
12.0925414675189));
#62083=CARTESIAN_POINT('Ctrl Pts',(0.597524573714824,-1.2,12.1138034539252));
#62084=CARTESIAN_POINT('Origin',(0.,1.25,7.2));
#62085=CARTESIAN_POINT('',(0.437314692285883,1.2,12.1306445684019));
#62086=CARTESIAN_POINT('Ctrl Pts',(0.354270609538459,1.3,12.0370437599031));
#62087=CARTESIAN_POINT('Ctrl Pts',(0.367581476408574,1.28316120465979,12.0529527556245));
#62088=CARTESIAN_POINT('Ctrl Pts',(0.381406074582236,1.26649040416743,12.0686092762383));
#62089=CARTESIAN_POINT('Ctrl Pts',(0.413005097135395,1.22892242797915,12.1037420910764));
#62090=CARTESIAN_POINT('Ctrl Pts',(0.422615951166165,1.21634758534866,12.1155364885164));
#62091=CARTESIAN_POINT('Ctrl Pts',(0.437314692285883,1.2,12.1306445684019));
#62092=CARTESIAN_POINT('Origin',(0.,1.2,7.2));
#62093=CARTESIAN_POINT('Origin',(0.,0.92691742076555,7.2));
#62094=CARTESIAN_POINT('Origin',(0.,0.653834841531101,7.2));
#62095=CARTESIAN_POINT('Origin',(0.,0.92691742076555,7.2));
#62096=CARTESIAN_POINT('',(0.509087305687289,0.653834841531101,12.123751630128));
#62097=CARTESIAN_POINT('Ctrl Pts',(0.437314692285884,1.2,12.1306445684019));
#62098=CARTESIAN_POINT('Ctrl Pts',(0.447918386563704,1.14399458640636,12.1297040927225));
#62099=CARTESIAN_POINT('Ctrl Pts',(0.463097499149716,1.06151801688422,12.1283363573917));
#62100=CARTESIAN_POINT('Ctrl Pts',(0.497285011036078,0.797206845778639,
12.124974622511));
#62101=CARTESIAN_POINT('Ctrl Pts',(0.502682930763357,0.739930875460911,
12.1244138052781));
#62102=CARTESIAN_POINT('Ctrl Pts',(0.509087305687304,0.653834841531103,
12.123751630128));
#62103=CARTESIAN_POINT('Origin',(0.,0.653834841531101,7.2));
#62104=CARTESIAN_POINT('Origin',(0.,-1.25,7.2));
#62105=CARTESIAN_POINT('Origin',(0.,-1.2,7.2));
#62106=CARTESIAN_POINT('Origin',(0.,0.,7.2));
#62107=CARTESIAN_POINT('Origin',(0.,-0.653834841531101,7.2));
#62108=CARTESIAN_POINT('Origin',(0.,-0.926917420765551,7.2));
#62109=CARTESIAN_POINT('Ctrl Pts',(0.237102298033322,-1.30000000000024,
12.2390757450685));
#62110=CARTESIAN_POINT('Ctrl Pts',(0.279563873101034,-1.18514270861194,
12.2425436139055));
#62111=CARTESIAN_POINT('Ctrl Pts',(0.31267400533481,-1.0684760419452,12.2349707346125));
#62112=CARTESIAN_POINT('Ctrl Pts',(0.367561330757959,-0.794772684000851,
12.1919695316219));
#62113=CARTESIAN_POINT('Ctrl Pts',(0.369299762850422,-0.636309800095197,
12.1220005005432));
#62114=CARTESIAN_POINT('Ctrl Pts',(0.393579787165998,-0.319434907277159,
12.0519414879789));
#62115=CARTESIAN_POINT('Ctrl Pts',(0.392969830592779,-0.158333333333332,
12.0060803363189));
#62116=CARTESIAN_POINT('Ctrl Pts',(0.426715573254505,0.158333333333334,
12.0030579137102));
#62117=CARTESIAN_POINT('Ctrl Pts',(0.462594679682929,0.319434907277167,
12.0456777212709));
#62118=CARTESIAN_POINT('Ctrl Pts',(0.503949232631026,0.636309800095206,
12.1100262039159));
#62119=CARTESIAN_POINT('Ctrl Pts',(0.537912637721293,0.794772684000841,
12.1761509049009));
#62120=CARTESIAN_POINT('Ctrl Pts',(0.52923751813028,1.0684760419452,12.2169241430278));
#62121=CARTESIAN_POINT('Ctrl Pts',(0.512888765856004,1.18514270861195,12.224352879199));
#62122=CARTESIAN_POINT('Ctrl Pts',(0.483946399133541,1.30000000000025,12.2215611275538));
#62123=CARTESIAN_POINT('Ctrl Pts',(0.230378897029079,-1.30000000000024,
12.2284879305123));
#62124=CARTESIAN_POINT('Ctrl Pts',(0.271622642083581,-1.18514270861194,
12.2299142784407));
#62125=CARTESIAN_POINT('Ctrl Pts',(0.303818465808643,-1.0684760419452,12.2208554699308));
#62126=CARTESIAN_POINT('Ctrl Pts',(0.357294751064532,-0.794772684000851,
12.1757050011437));
#62127=CARTESIAN_POINT('Ctrl Pts',(0.359072532092265,-0.636309800095197,
12.1061739593177));
#62128=CARTESIAN_POINT('Ctrl Pts',(0.383201773569423,-0.319434907277159,
12.0360862285591));
#62129=CARTESIAN_POINT('Ctrl Pts',(0.383232767764448,-0.158333333333332,
11.9908254840166));
#62130=CARTESIAN_POINT('Ctrl Pts',(0.416530303335429,0.158333333333334,
11.9879440783124));
#62131=CARTESIAN_POINT('Ctrl Pts',(0.451176432830853,0.319434907277167,
12.0301447644328));
#62132=CARTESIAN_POINT('Ctrl Pts',(0.492061752143941,0.636309800095206,
12.0947271819628));
#62133=CARTESIAN_POINT('Ctrl Pts',(0.525775129538419,0.794772684000841,
12.1604982598871));
#62134=CARTESIAN_POINT('Ctrl Pts',(0.518587456936806,1.0684760419452,12.2034113791225));
#62135=CARTESIAN_POINT('Ctrl Pts',(0.503305113780037,1.18514270861195,12.2122832473731));
#62136=CARTESIAN_POINT('Ctrl Pts',(0.475851704606219,1.30000000000025,12.211451484645));
#62137=CARTESIAN_POINT('Ctrl Pts',(0.217480409460025,-1.30000000000027,
12.2072321589895));
#62138=CARTESIAN_POINT('Ctrl Pts',(0.255006220628721,-1.18514270861197,
12.2048581625234));
#62139=CARTESIAN_POINT('Ctrl Pts',(0.284649067387247,-1.06847604194522,
12.1929812542131));
#62140=CARTESIAN_POINT('Ctrl Pts',(0.334918748661489,-0.794772684000867,
12.1435895926376));
#62141=CARTESIAN_POINT('Ctrl Pts',(0.338932835191999,-0.63630980009521,
12.0744056487988));
#62142=CARTESIAN_POINT('Ctrl Pts',(0.363309405263975,-0.319434907277166,
12.0041227783375));
#62143=CARTESIAN_POINT('Ctrl Pts',(0.363778637604756,-0.158333333333336,
11.9602912653471));
#62144=CARTESIAN_POINT('Ctrl Pts',(0.396376781294448,0.158333333333338,
11.9576271363067));
#62145=CARTESIAN_POINT('Ctrl Pts',(0.429467212561655,0.319434907277176,
11.9987176860391));
#62146=CARTESIAN_POINT('Ctrl Pts',(0.469532167199508,0.636309800095223,
12.0637304232381));
#62147=CARTESIAN_POINT('Ctrl Pts',(0.501908584033921,0.794772684000859,
12.1290339635959));
#62148=CARTESIAN_POINT('Ctrl Pts',(0.497690845494853,1.06847604194522,12.1762437320941));
#62149=CARTESIAN_POINT('Ctrl Pts',(0.484688916619089,1.18514270861197,12.1879700590222));
#62150=CARTESIAN_POINT('Ctrl Pts',(0.460510761598508,1.30000000000028,12.1909873533899));
#62151=CARTESIAN_POINT('Ctrl Pts',(0.204221446243486,-1.3000000000003,12.1855696400446));
#62152=CARTESIAN_POINT('Ctrl Pts',(0.239925501229051,-1.185142708612,12.1788788856711));
#62153=CARTESIAN_POINT('Ctrl Pts',(0.268098011735459,-1.06847604194524,
12.163880376218));
#62154=CARTESIAN_POINT('Ctrl Pts',(0.31578277246951,-0.794772684000884,
12.1100382427449));
#62155=CARTESIAN_POINT('Ctrl Pts',(0.318975050902126,-0.636309800095224,
12.0419589490921));
#62156=CARTESIAN_POINT('Ctrl Pts',(0.342761455244345,-0.319434907277172,
11.9716803997706));
#62157=CARTESIAN_POINT('Ctrl Pts',(0.344489810553044,-0.158333333333339,
11.9290947507789));
#62158=CARTESIAN_POINT('Ctrl Pts',(0.376548640812749,0.158333333333341,
11.9265957252551));
#62159=CARTESIAN_POINT('Ctrl Pts',(0.408153655753568,0.319434907277179,
11.9665148817081));
#62160=CARTESIAN_POINT('Ctrl Pts',(0.447072634148667,0.636309800095232,
12.0320442142247));
#62161=CARTESIAN_POINT('Ctrl Pts',(0.477304696940038,0.794772684000872,
12.0970886036103));
#62162=CARTESIAN_POINT('Ctrl Pts',(0.476004865794366,1.06847604194524,12.1487086624893));
#62163=CARTESIAN_POINT('Ctrl Pts',(0.465438337761383,1.185142708612,12.1633146761431));
#62164=CARTESIAN_POINT('Ctrl Pts',(0.444867930434888,1.30000000000031,12.1701822926736));
#62165=CARTESIAN_POINT('Ctrl Pts',(0.197352232389149,-1.3000000000003,12.174247236372));
#62166=CARTESIAN_POINT('Ctrl Pts',(0.231242228234118,-1.185142708612,12.1654874086266));
#62167=CARTESIAN_POINT('Ctrl Pts',(0.258160357660685,-1.06847604194525,
12.1489595156624));
#62168=CARTESIAN_POINT('Ctrl Pts',(0.30424021544578,-0.794772684000887,
12.09283099187));
#62169=CARTESIAN_POINT('Ctrl Pts',(0.308345084562613,-0.636309800095226,
12.0250112049144));
#62170=CARTESIAN_POINT('Ctrl Pts',(0.332424732837815,-0.319434907277173,
11.9545881433762));
#62171=CARTESIAN_POINT('Ctrl Pts',(0.334882470599985,-0.158333333333339,
11.9126391673332));
#62172=CARTESIAN_POINT('Ctrl Pts',(0.366609291628401,0.158333333333342,
11.9102385945571));
#62173=CARTESIAN_POINT('Ctrl Pts',(0.39687726031105,0.319434907277181,11.9496881813109));
#62174=CARTESIAN_POINT('Ctrl Pts',(0.435388204392732,0.636309800095236,
12.0154227310738));
#62175=CARTESIAN_POINT('Ctrl Pts',(0.465524583282553,0.794772684000877,
12.0800332353211));
#62176=CARTESIAN_POINT('Ctrl Pts',(0.465750995849449,1.06847604194524,12.1339656762935));
#62177=CARTESIAN_POINT('Ctrl Pts',(0.45624019572631,1.185142708612,12.1501459091373));
#62178=CARTESIAN_POINT('Ctrl Pts',(0.437120589869235,1.30000000000031,12.1591610195218));
#62179=CARTESIAN_POINT('Ctrl Pts',(0.196563250283277,-1.3000000000003,12.1729109480967));
#62180=CARTESIAN_POINT('Ctrl Pts',(0.230245887700426,-1.185142708612,12.1639059355002));
#62181=CARTESIAN_POINT('Ctrl Pts',(0.25701921103806,-1.06847604194525,12.1471972339629));
#62182=CARTESIAN_POINT('Ctrl Pts',(0.302909046205741,-0.794772684000887,
12.0907997282765));
#62183=CARTESIAN_POINT('Ctrl Pts',(0.307103184371951,-0.636309800095226,
12.023015057334));
#62184=CARTESIAN_POINT('Ctrl Pts',(0.33121687505589,-0.319434907277173,
11.9525749339417));
#62185=CARTESIAN_POINT('Ctrl Pts',(0.333776829383913,-0.158333333333339,
11.9106965890592));
#62186=CARTESIAN_POINT('Ctrl Pts',(0.365464948756233,0.158333333333342,
11.9083073734864));
#62187=CARTESIAN_POINT('Ctrl Pts',(0.395565754534697,0.319434907277181,
11.9477040904735));
#62188=CARTESIAN_POINT('Ctrl Pts',(0.434017282248823,0.636309800095235,
12.0134657910199));
#62189=CARTESIAN_POINT('Ctrl Pts',(0.464130379642697,0.794772684000877,
12.0780286470565));
#62190=CARTESIAN_POINT('Ctrl Pts',(0.464534180971738,1.06847604194524,12.1322338543628));
#62191=CARTESIAN_POINT('Ctrl Pts',(0.455149630347196,1.185142708612,12.1485988036637));
#62192=CARTESIAN_POINT('Ctrl Pts',(0.436205738465085,1.30000000000031,12.1578652765235));
#62193=CARTESIAN_POINT('Ctrl Pts',(0.195186075930414,-1.3000000000003,12.1705714112126));
#62194=CARTESIAN_POINT('Ctrl Pts',(0.228514698020356,-1.185142708612,12.1611353971354));
#62195=CARTESIAN_POINT('Ctrl Pts',(0.255040140543214,-1.06847604194525,
12.144109066136));
#62196=CARTESIAN_POINT('Ctrl Pts',(0.300602513396229,-0.794772684000888,
12.087239684894));
#62197=CARTESIAN_POINT('Ctrl Pts',(0.304947137552805,-0.636309800095226,
12.0195174794346));
#62198=CARTESIAN_POINT('Ctrl Pts',(0.329109272365874,-0.319434907277173,
11.9490501487589));
#62199=CARTESIAN_POINT('Ctrl Pts',(0.331829184804893,-0.158333333333339,
11.9073002608922));
#62200=CARTESIAN_POINT('Ctrl Pts',(0.363449794366847,0.158333333333342,
11.9049307792051));
#62201=CARTESIAN_POINT('Ctrl Pts',(0.393281919043544,0.319434907277181,
11.9442287386361));
#62202=CARTESIAN_POINT('Ctrl Pts',(0.431631438286729,0.636309800095235,
12.0100375438143));
#62203=CARTESIAN_POINT('Ctrl Pts',(0.461684190827631,0.794772684000876,
12.0745224001291));
#62204=CARTESIAN_POINT('Ctrl Pts',(0.462394759484056,1.06847604194524,12.1292059131272));
#62205=CARTESIAN_POINT('Ctrl Pts',(0.453232364716767,1.185142708612,12.1458937410935));
#62206=CARTESIAN_POINT('Ctrl Pts',(0.434599996339987,1.30000000000031,12.155598930473));
#62207=CARTESIAN_POINT('Ctrl Pts',(0.192488897548456,-1.3000000000003,12.1658782086319));
#62208=CARTESIAN_POINT('Ctrl Pts',(0.225171863855822,-1.185142708612,12.1555653405062));
#62209=CARTESIAN_POINT('Ctrl Pts',(0.251237527370526,-1.06847604194524,
12.1378951147785));
#62210=CARTESIAN_POINT('Ctrl Pts',(0.296167131269672,-0.794772684000886,
12.080076390536));
#62211=CARTESIAN_POINT('Ctrl Pts',(0.300730177358066,-0.636309800095225,
12.0124981823844));
#62212=CARTESIAN_POINT('Ctrl Pts',(0.324933733863143,-0.319434907277173,
11.9419893998123));
#62213=CARTESIAN_POINT('Ctrl Pts',(0.327930015438478,-0.158333333333339,
11.9005074513403));
#62214=CARTESIAN_POINT('Ctrl Pts',(0.35941891215817,0.158333333333342,11.8981758248249));
#62215=CARTESIAN_POINT('Ctrl Pts',(0.388804632316006,0.319434907277181,
11.9372517493087));
#62216=CARTESIAN_POINT('Ctrl Pts',(0.42692250054638,0.636309800095235,12.0031627188469));
#62217=CARTESIAN_POINT('Ctrl Pts',(0.456708971916004,0.794772684000877,
12.0675320420977));
#62218=CARTESIAN_POINT('Ctrl Pts',(0.458013159641032,1.06847604194524,12.1231779190637));
#62219=CARTESIAN_POINT('Ctrl Pts',(0.449313071918081,1.185142708612,12.1405066173595));
#62220=CARTESIAN_POINT('Ctrl Pts',(0.431348361930932,1.30000000000031,12.1510769756955));
#62221=CARTESIAN_POINT('Ctrl Pts',(0.189515797580747,-1.30000000000029,
12.160485154833));
#62222=CARTESIAN_POINT('Ctrl Pts',(0.221664788052325,-1.18514270861199,
12.1491237299431));
#62223=CARTESIAN_POINT('Ctrl Pts',(0.247325613607149,-1.06847604194524,
12.1306901654602));
#62224=CARTESIAN_POINT('Ctrl Pts',(0.29161829515871,-0.794772684000884,
12.0717668866466));
#62225=CARTESIAN_POINT('Ctrl Pts',(0.296199973908871,-0.636309800095224,
12.0044049429406));
#62226=CARTESIAN_POINT('Ctrl Pts',(0.320254171005224,-0.319434907277172,
11.9338955794758));
#62227=CARTESIAN_POINT('Ctrl Pts',(0.323354127894758,-0.158333333333339,
11.8927739101461));
#62228=CARTESIAN_POINT('Ctrl Pts',(0.354696758613631,0.158333333333341,
11.8904824344401));
#62229=CARTESIAN_POINT('Ctrl Pts',(0.383904433670636,0.31943490727718,11.9292162073965));
#62230=CARTESIAN_POINT('Ctrl Pts',(0.421727280585961,0.636309800095234,
11.9952544017964));
#62231=CARTESIAN_POINT('Ctrl Pts',(0.450818647748768,0.794772684000874,
12.0596015040265));
#62232=CARTESIAN_POINT('Ctrl Pts',(0.452745866745147,1.06847604194524,12.1163624018534));
#62233=CARTESIAN_POINT('Ctrl Pts',(0.444616828462124,1.185142708612,12.1344110765862));
#62234=CARTESIAN_POINT('Ctrl Pts',(0.427524530203049,1.30000000000031,12.1459387365809));
#62235=CARTESIAN_POINT('Ctrl Pts',(0.186537501569236,-1.30000000000029,
12.1550913385809));
#62236=CARTESIAN_POINT('Ctrl Pts',(0.218151414965836,-1.18514270861199,
12.1426802740476));
#62237=CARTESIAN_POINT('Ctrl Pts',(0.24341279621573,-1.06847604194524,12.1234812599331));
#62238=CARTESIAN_POINT('Ctrl Pts',(0.28709602034639,-0.794772684000885,
12.0634461751218));
#62239=CARTESIAN_POINT('Ctrl Pts',(0.291744047657623,-0.636309800095224,
11.9962907032332));
#62240=CARTESIAN_POINT('Ctrl Pts',(0.315682053496503,-0.319434907277172,
11.9257734385231));
#62241=CARTESIAN_POINT('Ctrl Pts',(0.318895369098061,-0.158333333333339,
11.8850103867684));
#62242=CARTESIAN_POINT('Ctrl Pts',(0.350082585755415,0.158333333333341,
11.8827600112108));
#62243=CARTESIAN_POINT('Ctrl Pts',(0.379079998488632,0.31943490727718,11.9211565710733));
#62244=CARTESIAN_POINT('Ctrl Pts',(0.416583287835046,0.636309800095234,
11.987326503418));
#62245=CARTESIAN_POINT('Ctrl Pts',(0.444979632628529,0.794772684000875,
12.0516512681616));
#62246=CARTESIAN_POINT('Ctrl Pts',(0.447509768154567,1.06847604194524,12.1095336326909));
#62247=CARTESIAN_POINT('Ctrl Pts',(0.439941051572146,1.185142708612,12.1283060702387));
#62248=CARTESIAN_POINT('Ctrl Pts',(0.423708416488844,1.30000000000031,12.1407958144826));
#62249=CARTESIAN_POINT('Ctrl Pts',(0.183538689402441,-1.30000000000029,
12.1497018523168));
#62250=CARTESIAN_POINT('Ctrl Pts',(0.214582539874455,-1.18514270861199,
12.1362489176074));
#62251=CARTESIAN_POINT('Ctrl Pts',(0.23942873327211,-1.06847604194524,12.1162878162494));
#62252=CARTESIAN_POINT('Ctrl Pts',(0.282510582805826,-0.794772684000885,
12.0551385119952));
#62253=CARTESIAN_POINT('Ctrl Pts',(0.287300547318078,-0.636309800095224,
11.9881719462936));
#62254=CARTESIAN_POINT('Ctrl Pts',(0.311186548055135,-0.319434907277173,
11.9176313249842));
#62255=CARTESIAN_POINT('Ctrl Pts',(0.314572598923691,-0.158333333333339,
11.8772123082057));
#62256=CARTESIAN_POINT('Ctrl Pts',(0.345584121560986,0.158333333333341,
11.8750077977819));
#62257=CARTESIAN_POINT('Ctrl Pts',(0.374223456744635,0.31943490727718,11.9131042924092));
#62258=CARTESIAN_POINT('Ctrl Pts',(0.411440527940432,0.636309800095233,
11.9793948661069));
#62259=CARTESIAN_POINT('Ctrl Pts',(0.439379615769516,0.794772684000875,
12.0436318337386));
#62260=CARTESIAN_POINT('Ctrl Pts',(0.442514805388562,1.06847604194524,12.1026355646076));
#62261=CARTESIAN_POINT('Ctrl Pts',(0.435458341800622,1.185142708612,12.122145507241));
#62262=CARTESIAN_POINT('Ctrl Pts',(0.419988307208882,1.30000000000031,12.1356248637183));
#62263=CARTESIAN_POINT('Ctrl Pts',(0.174871610951366,-1.30000000000029,
12.1349776486484));
#62264=CARTESIAN_POINT('Ctrl Pts',(0.203767783462163,-1.18514270861199,
12.11878748013));
#62265=CARTESIAN_POINT('Ctrl Pts',(0.227142824975559,-1.06847604194524,
12.0968033580528));
#62266=CARTESIAN_POINT('Ctrl Pts',(0.268388929930062,-0.794772684000881,
12.0326304463486));
#62267=CARTESIAN_POINT('Ctrl Pts',(0.274297728470185,-0.636309800095219,
11.9660269653453));
#62268=CARTESIAN_POINT('Ctrl Pts',(0.298739555434465,-0.319434907277169,
11.8952612685211));
#62269=CARTESIAN_POINT('Ctrl Pts',(0.303310176945395,-0.158333333333338,
11.8556154250831));
#62270=CARTESIAN_POINT('Ctrl Pts',(0.333952127921591,0.15833333333334,11.8535106333163));
#62271=CARTESIAN_POINT('Ctrl Pts',(0.360878601011834,0.31943490727718,11.8909619677454));
#62272=CARTESIAN_POINT('Ctrl Pts',(0.397110355900687,0.636309800095231,
11.9576231028531));
#62273=CARTESIAN_POINT('Ctrl Pts',(0.424086307390311,0.794772684000868,
12.0215240402449));
#62274=CARTESIAN_POINT('Ctrl Pts',(0.428914422170458,1.06847604194523,12.0836039242876));
#62275=CARTESIAN_POINT('Ctrl Pts',(0.423248054611277,1.18514270861199,12.1051515713865));
#62276=CARTESIAN_POINT('Ctrl Pts',(0.409825407503875,1.3000000000003,12.1213747840685));
#62277=CARTESIAN_POINT('Ctrl Pts',(0.15989854583247,-1.30000000000028,12.1079962375592));
#62278=CARTESIAN_POINT('Ctrl Pts',(0.186097547729273,-1.18514270861198,
12.0865642185193));
#62279=CARTESIAN_POINT('Ctrl Pts',(0.207480269930789,-1.06847604194523,
12.0607499545607));
#62280=CARTESIAN_POINT('Ctrl Pts',(0.245752066225641,-0.794772684000871,
11.9909899782638));
#62281=CARTESIAN_POINT('Ctrl Pts',(0.251980650996533,-0.636309800095216,
11.9253969188526));
#62282=CARTESIAN_POINT('Ctrl Pts',(0.276297595609869,-0.319434907277169,
11.854478854774));
#62283=CARTESIAN_POINT('Ctrl Pts',(0.282316170182864,-0.158333333333337,
11.8164342936643));
#62284=CARTESIAN_POINT('Ctrl Pts',(0.312123312753905,0.15833333333334,11.8145536268061));
#62285=CARTESIAN_POINT('Ctrl Pts',(0.336365846919138,0.31943490727718,11.8507265227037));
#62286=CARTESIAN_POINT('Ctrl Pts',(0.371839209141617,0.636309800095229,
11.9177954680997));
#62287=CARTESIAN_POINT('Ctrl Pts',(0.398845696192265,0.794772684000865,
11.9806162688803));
#62288=CARTESIAN_POINT('Ctrl Pts',(0.406726498838685,1.06847604194523,12.0483032401435));
#62289=CARTESIAN_POINT('Ctrl Pts',(0.403122927646196,1.18514270861198,12.0736823929196));
#62290=CARTESIAN_POINT('Ctrl Pts',(0.392504477808099,1.30000000000029,12.0951415166614));
#62291=CARTESIAN_POINT('Ctrl Pts',(0.142368228275982,-1.30000000000025,
12.0755162243303));
#62292=CARTESIAN_POINT('Ctrl Pts',(0.164577244832849,-1.18514270861196,
12.0479100423271));
#62293=CARTESIAN_POINT('Ctrl Pts',(0.183321623936367,-1.06847604194521,
12.0175268289581));
#62294=CARTESIAN_POINT('Ctrl Pts',(0.218620883850096,-0.794772684000863,
11.9409200299361));
#62295=CARTESIAN_POINT('Ctrl Pts',(0.228261751117289,-0.636309800095203,
11.8759733523308));
#62296=CARTESIAN_POINT('Ctrl Pts',(0.25292606159555,-0.31943490727716,11.8047686637498));
#62297=CARTESIAN_POINT('Ctrl Pts',(0.258749364371646,-0.158333333333334,
11.7690234910886));
#62298=CARTESIAN_POINT('Ctrl Pts',(0.28707569305352,0.158333333333336,11.7674589260075));
#62299=CARTESIAN_POINT('Ctrl Pts',(0.309534439982334,0.319434907277173,
11.8017008235096));
#62300=CARTESIAN_POINT('Ctrl Pts',(0.34265901455359,0.636309800095215,11.8695937625149));
#62301=CARTESIAN_POINT('Ctrl Pts',(0.365625602803515,0.794772684000848,
11.9321516222108));
#62302=CARTESIAN_POINT('Ctrl Pts',(0.37682644013388,1.0684760419452,12.0066766111699));
#62303=CARTESIAN_POINT('Ctrl Pts',(0.376407879371129,1.18514270861196,12.0364913873925));
#62304=CARTESIAN_POINT('Ctrl Pts',(0.370722330397239,1.30000000000026,12.0638618335402));
#62305=CARTESIAN_POINT('Ctrl Pts',(0.127980957799861,-1.30000000000026,
12.0483368524573));
#62306=CARTESIAN_POINT('Ctrl Pts',(0.148161195722953,-1.18514270861197,
12.0153280736421));
#62307=CARTESIAN_POINT('Ctrl Pts',(0.165386717646749,-1.06847604194522,
11.9810000168413));
#62308=CARTESIAN_POINT('Ctrl Pts',(0.198355134197284,-0.794772684000868,
11.89864754226));
#62309=CARTESIAN_POINT('Ctrl Pts',(0.20788127579913,-0.636309800095204,
11.8348054186726));
#62310=CARTESIAN_POINT('Ctrl Pts',(0.232736015668612,-0.31943490727716,
11.7633758451342));
#62311=CARTESIAN_POINT('Ctrl Pts',(0.240404384429822,-0.158333333333334,
11.729168768354));
#62312=CARTESIAN_POINT('Ctrl Pts',(0.268447431824777,0.158333333333337,
11.7276671885862));
#62313=CARTESIAN_POINT('Ctrl Pts',(0.288975462966633,0.319434907277174,
11.760380825881));
#62314=CARTESIAN_POINT('Ctrl Pts',(0.320930023456981,0.636309800095217,
11.8287352083804));
#62315=CARTESIAN_POINT('Ctrl Pts',(0.342399008811111,0.794772684000848,
11.8905569992644));
#62316=CARTESIAN_POINT('Ctrl Pts',(0.355891004113073,1.06847604194521,11.9709049018606));
#62317=CARTESIAN_POINT('Ctrl Pts',(0.357375294527153,1.18514270861196,12.0046200308278));
#62318=CARTESIAN_POINT('Ctrl Pts',(0.354503690516788,1.30000000000027,12.0372706589114));
#62319=CARTESIAN_POINT('Ctrl Pts',(0.120462273527673,-1.30000000000026,
12.0318473446919));
#62320=CARTESIAN_POINT('Ctrl Pts',(0.138892560461965,-1.18514270861196,
11.9956795717989));
#62321=CARTESIAN_POINT('Ctrl Pts',(0.154959724777024,-1.06847604194521,
11.9590188344525));
#62322=CARTESIAN_POINT('Ctrl Pts',(0.186618802578527,-0.794772684000862,
11.8731863507222));
#62323=CARTESIAN_POINT('Ctrl Pts',(0.197532813745976,-0.636309800095202,
11.8097426426205));
#62324=CARTESIAN_POINT('Ctrl Pts',(0.222728594550386,-0.31943490727716,
11.7381357037543));
#62325=CARTESIAN_POINT('Ctrl Pts',(0.231038606336704,-0.158333333333334,
11.7049345709295));
#62326=CARTESIAN_POINT('Ctrl Pts',(0.25791364597085,0.158333333333336,11.7036669633902));
#62327=CARTESIAN_POINT('Ctrl Pts',(0.276036279865896,0.319434907277173,
11.735710844867));
#62328=CARTESIAN_POINT('Ctrl Pts',(0.306484144357572,0.636309800095215,
11.8045109708308));
#62329=CARTESIAN_POINT('Ctrl Pts',(0.327090231868471,0.794772684000847,
11.8659070582392));
#62330=CARTESIAN_POINT('Ctrl Pts',(0.342261698133297,1.0684760419452,11.9496835149717));
#62331=CARTESIAN_POINT('Ctrl Pts',(0.34515937151465,1.18514270861195,11.9856764880079));
#62332=CARTESIAN_POINT('Ctrl Pts',(0.344387552689541,1.30000000000026,12.0213987101844));
#62333=CARTESIAN_POINT('Ctrl Pts',(0.114879864456069,-1.30000000000026,
12.0209362197056));
#62334=CARTESIAN_POINT('Ctrl Pts',(0.132339498666072,-1.18514270861196,
11.9826291753253));
#62335=CARTESIAN_POINT('Ctrl Pts',(0.147764458409392,-1.06847604194521,
11.9443917057748));
#62336=CARTESIAN_POINT('Ctrl Pts',(0.17869869611581,-0.794772684000861,
11.8562162335089));
#62337=CARTESIAN_POINT('Ctrl Pts',(0.190404690486681,-0.636309800095203,
11.793063869767));
#62338=CARTESIAN_POINT('Ctrl Pts',(0.215752348972689,-0.31943490727716,
11.7213549202783));
#62339=CARTESIAN_POINT('Ctrl Pts',(0.224125089103901,-0.158333333333334,
11.6889015783789));
#62340=CARTESIAN_POINT('Ctrl Pts',(0.250752042061645,0.158333333333336,
11.6876746256021));
#62341=CARTESIAN_POINT('Ctrl Pts',(0.26854110742805,0.319434907277173,11.7190001728044));
#62342=CARTESIAN_POINT('Ctrl Pts',(0.298378106797284,0.636309800095215,
11.7880079299611));
#62343=CARTESIAN_POINT('Ctrl Pts',(0.317784368782244,0.794772684000847,
11.8492406110604));
#62344=CARTESIAN_POINT('Ctrl Pts',(0.333705235052286,1.0684760419452,11.9353877720829));
#62345=CARTESIAN_POINT('Ctrl Pts',(0.337385718999905,1.18514270861196,11.9729402953774));
#62346=CARTESIAN_POINT('Ctrl Pts',(0.337855133813078,1.30000000000026,12.0107554280267));
#62347=CARTESIAN_POINT('Ctrl Pts',(0.10918826148896,-1.30000000000026,12.010040768441));
#62348=CARTESIAN_POINT('Ctrl Pts',(0.125741996817306,-1.18514270861196,
11.9695834866496));
#62349=CARTESIAN_POINT('Ctrl Pts',(0.140526383380073,-1.06847604194521,
11.9297694514619));
#62350=CARTESIAN_POINT('Ctrl Pts',(0.17059372434096,-0.794772684000861,
11.8392770937437));
#62351=CARTESIAN_POINT('Ctrl Pts',(0.182555816696012,-0.636309800095203,
11.7765124961274));
#62352=CARTESIAN_POINT('Ctrl Pts',(0.20815294648653,-0.319434907277161,
11.704682908112));
#62353=CARTESIAN_POINT('Ctrl Pts',(0.217220431067991,-0.158333333333334,
11.6728605536538));
#62354=CARTESIAN_POINT('Ctrl Pts',(0.243858388181379,0.158333333333336,
11.6716291151367));
#62355=CARTESIAN_POINT('Ctrl Pts',(0.261104508940357,0.319434907277172,
11.7022838198051));
#62356=CARTESIAN_POINT('Ctrl Pts',(0.290427661000645,0.636309800095215,
11.7714751231832));
#62357=CARTESIAN_POINT('Ctrl Pts',(0.309093235239651,0.794772684000848,
11.8324306450287));
#62358=CARTESIAN_POINT('Ctrl Pts',(0.325460045223944,1.06847604194521,11.9210137645983));
#62359=CARTESIAN_POINT('Ctrl Pts',(0.329626402260167,1.18514270861196,11.9601929260328));
#62360=CARTESIAN_POINT('Ctrl Pts',(0.330874530740492,1.30000000000026,12.0002068987681));
#62361=CARTESIAN_POINT('Ctrl Pts',(0.103562192797037,-1.30000000000025,
11.9961742881129));
#62362=CARTESIAN_POINT('Ctrl Pts',(0.119158940804234,-1.18514270861196,
11.9529910346458));
#62363=CARTESIAN_POINT('Ctrl Pts',(0.133244708046977,-1.06847604194521,
11.9111830414882));
#62364=CARTESIAN_POINT('Ctrl Pts',(0.162294980389235,-0.794772684000857,
11.8177753400688));
#62365=CARTESIAN_POINT('Ctrl Pts',(0.174380721365818,-0.636309800095201,
11.7555311234643));
#62366=CARTESIAN_POINT('Ctrl Pts',(0.200082511825562,-0.31943490727716,
11.6835887744683));
#62367=CARTESIAN_POINT('Ctrl Pts',(0.209999887910456,-0.158333333333334,
11.65256476212));
#62368=CARTESIAN_POINT('Ctrl Pts',(0.236184727887872,0.158333333333336,
11.6514091690308));
#62369=CARTESIAN_POINT('Ctrl Pts',(0.252155158378876,0.319434907277171,
11.681322438965));
#62370=CARTESIAN_POINT('Ctrl Pts',(0.28039503723386,0.636309800095213,11.7508195704479));
#62371=CARTESIAN_POINT('Ctrl Pts',(0.29776887209576,0.794772684000846,11.8115163260757));
#62372=CARTESIAN_POINT('Ctrl Pts',(0.315300187630474,1.0684760419452,11.9030078072475));
#62373=CARTESIAN_POINT('Ctrl Pts',(0.320585012528572,1.18514270861195,11.9441064816108));
#62374=CARTESIAN_POINT('Ctrl Pts',(0.323566005429051,1.30000000000026,11.9867005582316));
#62375=CARTESIAN_POINT('Ctrl Pts',(0.094794633655618,-1.30000000000025,
11.9798529787367));
#62376=CARTESIAN_POINT('Ctrl Pts',(0.108885876876833,-1.18514270861196,
11.9334650249093));
#62377=CARTESIAN_POINT('Ctrl Pts',(0.122024990313988,-1.06847604194521,
11.8892865355057));
#62378=CARTESIAN_POINT('Ctrl Pts',(0.150179360550364,-0.79477268400086,
11.7923296919279));
#62379=CARTESIAN_POINT('Ctrl Pts',(0.163754820774804,-0.636309800095203,
11.7304776935039));
#62380=CARTESIAN_POINT('Ctrl Pts',(0.190187546892998,-0.319434907277161,
11.6582959379707));
#62381=CARTESIAN_POINT('Ctrl Pts',(0.200831056815098,-0.158333333333334,
11.6282797031472));
#62382=CARTESIAN_POINT('Ctrl Pts',(0.226557352250275,0.158333333333336,
11.627199545701));
#62383=CARTESIAN_POINT('Ctrl Pts',(0.241067094049417,0.319434907277171,
11.6562114221743));
#62384=CARTESIAN_POINT('Ctrl Pts',(0.268204228162709,0.636309800095214,
11.7260385774622));
#62385=CARTESIAN_POINT('Ctrl Pts',(0.284499538638445,0.794772684000848,
11.7863238456839));
#62386=CARTESIAN_POINT('Ctrl Pts',(0.303104086580015,1.06847604194521,11.8813850994134));
#62387=CARTESIAN_POINT('Ctrl Pts',(0.309408290174266,1.18514270861196,11.92486252824));
#62388=CARTESIAN_POINT('Ctrl Pts',(0.313963477925306,1.30000000000026,11.9706688915202));
#62389=CARTESIAN_POINT('Ctrl Pts',(0.0830130309313852,-1.30000000000024,
11.9521871509239));
#62390=CARTESIAN_POINT('Ctrl Pts',(0.0957161656842548,-1.18514270861195,
11.9002711856679));
#62391=CARTESIAN_POINT('Ctrl Pts',(0.107860818724359,-1.06847604194521,
11.8520460684592));
#62392=CARTESIAN_POINT('Ctrl Pts',(0.13462719229614,-0.794772684000858,
11.7491629976463));
#62393=CARTESIAN_POINT('Ctrl Pts',(0.148671537687174,-0.636309800095198,
11.6883128523622));
#62394=CARTESIAN_POINT('Ctrl Pts',(0.175072801269439,-0.319434907277158,
11.6159447109649));
#62395=CARTESIAN_POINT('Ctrl Pts',(0.186253878137799,-0.158333333333333,
11.5877234799558));
#62396=CARTESIAN_POINT('Ctrl Pts',(0.211375734943978,0.158333333333335,
11.5867225045778));
#62397=CARTESIAN_POINT('Ctrl Pts',(0.225013277830667,0.319434907277169,
11.6139407036506));
#62398=CARTESIAN_POINT('Ctrl Pts',(0.250401099768228,0.636309800095208,
11.6842741193368));
#62399=CARTESIAN_POINT('Ctrl Pts',(0.263796170364388,0.79477268400084,11.7440370831602));
#62400=CARTESIAN_POINT('Ctrl Pts',(0.283344363081088,1.0684760419452,11.8451960582538));
#62401=CARTESIAN_POINT('Ctrl Pts',(0.291000962720118,1.18514270861195,11.8927073822637));
#62402=CARTESIAN_POINT('Ctrl Pts',(0.297852473703045,1.30000000000026,11.9439420582748));
#62403=CARTESIAN_POINT('Ctrl Pts',(0.0682437123209798,-1.30000000000025,
11.9190458604761));
#62404=CARTESIAN_POINT('Ctrl Pts',(0.078446405555705,-1.18514270861195,
11.8605989204779));
#62405=CARTESIAN_POINT('Ctrl Pts',(0.0890788816669909,-1.06847604194521,
11.8075487239736));
#62406=CARTESIAN_POINT('Ctrl Pts',(0.114634912926241,-0.794772684000859,
11.6974597144792));
#62407=CARTESIAN_POINT('Ctrl Pts',(0.131740333363184,-0.636309800095201,
11.6374429325233));
#62408=CARTESIAN_POINT('Ctrl Pts',(0.1594292559344,-0.31943490727716,11.5646392296698));
#62409=CARTESIAN_POINT('Ctrl Pts',(0.171645869628339,-0.158333333333333,
11.5385002879484));
#62410=CARTESIAN_POINT('Ctrl Pts',(0.195246818017136,0.158333333333336,
11.5377061193558));
#62411=CARTESIAN_POINT('Ctrl Pts',(0.205343216370943,0.319434907277171,
11.563161128943));
#62412=CARTESIAN_POINT('Ctrl Pts',(0.228351159935257,0.636309800095212,
11.6341226238268));
#62413=CARTESIAN_POINT('Ctrl Pts',(0.240273808775317,0.794772684000846,
11.6929087520959));
#62414=CARTESIAN_POINT('Ctrl Pts',(0.261870995302839,1.0684760419452,11.8012335718407));
#62415=CARTESIAN_POINT('Ctrl Pts',(0.271386990239266,1.18514270861195,11.8535526181072));
#62416=CARTESIAN_POINT('Ctrl Pts',(0.281070358318985,1.30000000000026,11.9113009100027));
#62417=CARTESIAN_POINT('Ctrl Pts',(0.0556483962276951,-1.30000000000024,
11.8855803936001));
#62418=CARTESIAN_POINT('Ctrl Pts',(0.0644266534852743,-1.18514270861195,
11.8204697935768));
#62419=CARTESIAN_POINT('Ctrl Pts',(0.0742122621370922,-1.0684760419452,
11.7625226330136));
#62420=CARTESIAN_POINT('Ctrl Pts',(0.0991461589677387,-0.794772684000853,
11.6452020780171));
#62421=CARTESIAN_POINT('Ctrl Pts',(0.117818837276392,-0.636309800095197,
11.5862860789068));
#62422=CARTESIAN_POINT('Ctrl Pts',(0.146885729055631,-0.319434907277159,
11.5130795221398));
#62423=CARTESIAN_POINT('Ctrl Pts',(0.161014727437592,-0.158333333333332,
11.4889316353716));
#62424=CARTESIAN_POINT('Ctrl Pts',(0.183847560566396,0.158333333333335,
11.4881825033546));
#62425=CARTESIAN_POINT('Ctrl Pts',(0.191540343583512,0.319434907277169,
11.5115859798794));
#62426=CARTESIAN_POINT('Ctrl Pts',(0.211041728444421,0.636309800095208,
11.5832569907542));
#62427=CARTESIAN_POINT('Ctrl Pts',(0.218742224588253,0.794772684000841,
11.6414480623763));
#62428=CARTESIAN_POINT('Ctrl Pts',(0.240246692293113,1.0684760419452,11.7572633594441));
#62429=CARTESIAN_POINT('Ctrl Pts',(0.250868610018655,1.18514270861195,11.814519967009));
#62430=CARTESIAN_POINT('Ctrl Pts',(0.262803958219365,1.30000000000025,11.8789010314179));
#62431=CARTESIAN_POINT('Ctrl Pts',(0.0464357783185983,-1.30000000000024,
11.86333871748));
#62432=CARTESIAN_POINT('Ctrl Pts',(0.0542499946932897,-1.18514270861195,
11.793739927263));
#62433=CARTESIAN_POINT('Ctrl Pts',(0.0636295362538139,-1.0684760419452,
11.7324730561432));
#62434=CARTESIAN_POINT('Ctrl Pts',(0.0889143679509853,-0.794772684000858,
11.6101827273706));
#62435=CARTESIAN_POINT('Ctrl Pts',(0.110340899142229,-0.636309800095199,
11.5517926056029));
#62436=CARTESIAN_POINT('Ctrl Pts',(0.140424748904,-0.319434907277159,11.4783003446474));
#62437=CARTESIAN_POINT('Ctrl Pts',(0.154212363334051,-0.158333333333333,
11.4556985708264));
#62438=CARTESIAN_POINT('Ctrl Pts',(0.17615831927619,0.158333333333335,11.455019647929));
#62439=CARTESIAN_POINT('Ctrl Pts',(0.182754644700643,0.319434907277169,
11.4769817094759));
#62440=CARTESIAN_POINT('Ctrl Pts',(0.200554841333362,0.636309800095209,
11.549011184157));
#62441=CARTESIAN_POINT('Ctrl Pts',(0.206119407133801,0.794772684000844,
11.606659084153));
#62442=CARTESIAN_POINT('Ctrl Pts',(0.228088731804076,1.0684760419452,11.7274091082837));
#62443=CARTESIAN_POINT('Ctrl Pts',(0.23959717134933,1.18514270861195,11.7879587027551));
#62444=CARTESIAN_POINT('Ctrl Pts',(0.253104343833782,1.30000000000025,11.8567896804811));
#62445=CARTESIAN_POINT('Ctrl Pts',(0.0406518797623858,-1.30000000000024,
11.8465564726809));
#62446=CARTESIAN_POINT('Ctrl Pts',(0.0478819400995714,-1.18514270861195,
11.773657943409));
#62447=CARTESIAN_POINT('Ctrl Pts',(0.0569887955685448,-1.0684760419452,
11.7099645477952));
#62448=CARTESIAN_POINT('Ctrl Pts',(0.0823632257280734,-0.794772684000853,
11.5840857623383));
#62449=CARTESIAN_POINT('Ctrl Pts',(0.104982086020124,-0.636309800095198,
11.5262348933961));
#62450=CARTESIAN_POINT('Ctrl Pts',(0.136074315850756,-0.319434907277159,
11.4525214372116));
#62451=CARTESIAN_POINT('Ctrl Pts',(0.150878273702948,-0.158333333333333,
11.4308793229505));
#62452=CARTESIAN_POINT('Ctrl Pts',(0.172369064798244,0.158333333333335,
11.4302102994935));
#62453=CARTESIAN_POINT('Ctrl Pts',(0.177494189085355,0.319434907277169,
11.4511811093708));
#62454=CARTESIAN_POINT('Ctrl Pts',(0.193358242024117,0.636309800095208,
11.5235364590285));
#62455=CARTESIAN_POINT('Ctrl Pts',(0.197067540665844,0.794772684000842,
11.580789800071));
#62456=CARTESIAN_POINT('Ctrl Pts',(0.218448911255057,1.0684760419452,11.7052970606092));
#62457=CARTESIAN_POINT('Ctrl Pts',(0.230124991373547,1.18514270861195,11.7683449680977));
#62458=CARTESIAN_POINT('Ctrl Pts',(0.244221948540316,1.30000000000025,11.8405462034364));
#62459=CARTESIAN_POINT('Ctrl Pts',(0.034830413167812,-1.30000000000025,
11.829676335823));
#62460=CARTESIAN_POINT('Ctrl Pts',(0.0413983638315718,-1.18514270861195,
11.7533037192462));
#62461=CARTESIAN_POINT('Ctrl Pts',(0.050314467195016,-1.06847604194521,
11.6870370189958));
#62462=CARTESIAN_POINT('Ctrl Pts',(0.0763371521075432,-0.794772684000857,
11.5572943732051));
#62463=CARTESIAN_POINT('Ctrl Pts',(0.102225806674094,-0.6363098000952,11.4997609588548));
#62464=CARTESIAN_POINT('Ctrl Pts',(0.13310772074771,-0.31943490727716,11.4259272518795));
#62465=CARTESIAN_POINT('Ctrl Pts',(0.144692433467357,-0.158333333333333,
11.4057563231153));
#62466=CARTESIAN_POINT('Ctrl Pts',(0.165044457335305,0.158333333333335,
11.4051666385386));
#62467=CARTESIAN_POINT('Ctrl Pts',(0.171551107388644,0.319434907277168,
11.4247803349145));
#62468=CARTESIAN_POINT('Ctrl Pts',(0.186729604417125,0.636309800095209,
11.4973467940944));
#62469=CARTESIAN_POINT('Ctrl Pts',(0.188181266030554,0.794772684000846,
11.5542555919596));
#62470=CARTESIAN_POINT('Ctrl Pts',(0.209496799931565,1.0684760419452,11.6826400382386));
#62471=CARTESIAN_POINT('Ctrl Pts',(0.221636035209642,1.18514270861195,11.7482662320662));
#62472=CARTESIAN_POINT('Ctrl Pts',(0.236687800958419,1.30000000000025,11.82394575004));
#62473=CARTESIAN_POINT('Ctrl Pts',(0.0300137202382451,-1.30000000000024,
11.815727424252));
#62474=CARTESIAN_POINT('Ctrl Pts',(0.0369536379353412,-1.18514270861195,
11.7366024621951));
#62475=CARTESIAN_POINT('Ctrl Pts',(0.0459456534800434,-1.0684760419452,
11.6683507799072));
#62476=CARTESIAN_POINT('Ctrl Pts',(0.0714597647835856,-0.794772684000853,
11.5357951915782));
#62477=CARTESIAN_POINT('Ctrl Pts',(0.0956780461528079,-0.636309800095197,
11.4789939209136));
#62478=CARTESIAN_POINT('Ctrl Pts',(0.12571304728649,-0.319434907277159,
11.4052172446615));
#62479=CARTESIAN_POINT('Ctrl Pts',(0.137179957999219,-0.158333333333332,
11.3860007057705));
#62480=CARTESIAN_POINT('Ctrl Pts',(0.158144120393544,0.158333333333335,
11.385327828888));
#62481=CARTESIAN_POINT('Ctrl Pts',(0.166297992339798,0.319434907277168,
11.4037986346615));
#62482=CARTESIAN_POINT('Ctrl Pts',(0.181701848327912,0.636309800095208,
11.4763531120574));
#62483=CARTESIAN_POINT('Ctrl Pts',(0.181519653365159,0.794772684000841,
11.5328622516889));
#62484=CARTESIAN_POINT('Ctrl Pts',(0.202836953204498,1.0684760419452,11.6641532144601));
#62485=CARTESIAN_POINT('Ctrl Pts',(0.215272326681509,1.18514270861195,11.7317564899875));
#62486=CARTESIAN_POINT('Ctrl Pts',(0.230915604418885,1.30000000000025,11.8101320480683));
#62487=CARTESIAN_POINT('Ctrl Pts',(0.0249486472265458,-1.30000000000024,
11.7987654117141));
#62488=CARTESIAN_POINT('Ctrl Pts',(0.0322960695121722,-1.18514270861195,
11.7159494251139));
#62489=CARTESIAN_POINT('Ctrl Pts',(0.0411713710709376,-1.0684760419452,
11.6450237733314));
#62490=CARTESIAN_POINT('Ctrl Pts',(0.0652047999418275,-0.794772684000854,
11.5086403811676));
#62491=CARTESIAN_POINT('Ctrl Pts',(0.0861507442337192,-0.636309800095198,
11.4527126715445));
#62492=CARTESIAN_POINT('Ctrl Pts',(0.11401151949034,-0.319434907277159,
11.378979926875));
#62493=CARTESIAN_POINT('Ctrl Pts',(0.12516253329486,-0.158333333333333,
11.3610604540291));
#62494=CARTESIAN_POINT('Ctrl Pts',(0.146020139137245,0.158333333333335,
11.3603760542832));
#62495=CARTESIAN_POINT('Ctrl Pts',(0.154705006362177,0.319434907277168,
11.3774873687404));
#62496=CARTESIAN_POINT('Ctrl Pts',(0.171410852286353,0.636309800095208,
11.4500781278508));
#62497=CARTESIAN_POINT('Ctrl Pts',(0.1726664600724,0.794772684000841,11.505919375511));
#62498=CARTESIAN_POINT('Ctrl Pts',(0.195303874973743,1.0684760419452,11.6411090107818));
#62499=CARTESIAN_POINT('Ctrl Pts',(0.208193542904413,1.18514270861195,11.7113846754377));
#62500=CARTESIAN_POINT('Ctrl Pts',(0.224173980653852,1.30000000000026,11.7934174209105));
#62501=CARTESIAN_POINT('Ctrl Pts',(0.0213943747864571,-1.30000000000024,
11.7872275498583));
#62502=CARTESIAN_POINT('Ctrl Pts',(0.0303808199748146,-1.18514270861194,
11.7017443481177));
#62503=CARTESIAN_POINT('Ctrl Pts',(0.0397026858022263,-1.0684760419452,
11.6290281458668));
#62504=CARTESIAN_POINT('Ctrl Pts',(0.0620129494732972,-0.794772684000851,
11.4905334946914));
#62505=CARTESIAN_POINT('Ctrl Pts',(0.0765909966193375,-0.636309800095197,
11.4363224854433));
#62506=CARTESIAN_POINT('Ctrl Pts',(0.101057989717432,-0.319434907277159,
11.3633819083365));
#62507=CARTESIAN_POINT('Ctrl Pts',(0.112567852729614,-0.158333333333332,
11.3464812380319));
#62508=CARTESIAN_POINT('Ctrl Pts',(0.133278717910193,0.158333333333334,
11.3458490652972));
#62509=CARTESIAN_POINT('Ctrl Pts',(0.141607349608986,0.319434907277167,
11.3620417363435));
#62510=CARTESIAN_POINT('Ctrl Pts',(0.161103853485779,0.636309800095206,
11.4338490762767));
#62511=CARTESIAN_POINT('Ctrl Pts',(0.167600922680342,0.79477268400084,11.4878246451703));
#62512=CARTESIAN_POINT('Ctrl Pts',(0.192015477656447,1.0684760419452,11.6251313100261));
#62513=CARTESIAN_POINT('Ctrl Pts',(0.204772182759206,1.18514270861195,11.6972293577846));
#62514=CARTESIAN_POINT('Ctrl Pts',(0.219717436763987,1.30000000000025,11.781990485799));
#62515=CARTESIAN_POINT('Ctrl Pts',(0.0165023515695648,-1.30000000000024,
11.780151978414));
#62516=CARTESIAN_POINT('Ctrl Pts',(0.0256069538907778,-1.18514270861194,
11.6948905764801));
#62517=CARTESIAN_POINT('Ctrl Pts',(0.0347010954711953,-1.0684760419452,
11.6224333483287));
#62518=CARTESIAN_POINT('Ctrl Pts',(0.0556862153948441,-0.794772684000851,
11.4846228591836));
#62519=CARTESIAN_POINT('Ctrl Pts',(0.0677962068234778,-0.636309800095197,
11.4311131089277));
#62520=CARTESIAN_POINT('Ctrl Pts',(0.0906597384266766,-0.319434907277159,
11.3586954735785));
#62521=CARTESIAN_POINT('Ctrl Pts',(0.102179986998412,-0.158333333333332,
11.3417434974973));
#62522=CARTESIAN_POINT('Ctrl Pts',(0.12267336889205,0.158333333333334,11.341205069791));
#62523=CARTESIAN_POINT('Ctrl Pts',(0.130506918224618,0.319434907277167,
11.357626654509));
#62524=CARTESIAN_POINT('Ctrl Pts',(0.151708180499798,0.636309800095206,
11.4289311819364));
#62525=CARTESIAN_POINT('Ctrl Pts',(0.161724215836605,0.79477268400084,11.4819406028846));
#62526=CARTESIAN_POINT('Ctrl Pts',(0.187312562460002,1.0684760419452,11.618589325336));
#62527=CARTESIAN_POINT('Ctrl Pts',(0.199984062839927,1.18514270861195,11.690494969693));
#62528=CARTESIAN_POINT('Ctrl Pts',(0.214250816488192,1.30000000000025,11.7751560897922));
#62529=CARTESIAN_POINT('Ctrl Pts',(0.0165023515695838,-1.3,11.7801519784138));
#62530=CARTESIAN_POINT('Ctrl Pts',(0.0256069538907905,-1.18514270861178,
11.69489057648));
#62531=CARTESIAN_POINT('Ctrl Pts',(0.0347010954712016,-1.06847604194512,
11.6224333483286));
#62532=CARTESIAN_POINT('Ctrl Pts',(0.0556862153948441,-0.794772684000851,
11.4846228591836));
#62533=CARTESIAN_POINT('Ctrl Pts',(0.0677962068234778,-0.636309800095197,
11.4311131089277));
#62534=CARTESIAN_POINT('Ctrl Pts',(0.0906597384266766,-0.319434907277159,
11.3586954735785));
#62535=CARTESIAN_POINT('Ctrl Pts',(0.102179986998412,-0.158333333333332,
11.3417434974973));
#62536=CARTESIAN_POINT('Ctrl Pts',(0.12267336889205,0.158333333333334,11.341205069791));
#62537=CARTESIAN_POINT('Ctrl Pts',(0.130506918224618,0.319434907277167,
11.357626654509));
#62538=CARTESIAN_POINT('Ctrl Pts',(0.151708180499798,0.636309800095206,
11.4289311819364));
#62539=CARTESIAN_POINT('Ctrl Pts',(0.161724215836605,0.79477268400084,11.4819406028846));
#62540=CARTESIAN_POINT('Ctrl Pts',(0.187312562459994,1.06847604194511,11.6185893253359));
#62541=CARTESIAN_POINT('Ctrl Pts',(0.199984062839908,1.18514270861178,11.6904949696929));
#62542=CARTESIAN_POINT('Ctrl Pts',(0.214250816488161,1.3,11.775156089792));
#62543=CARTESIAN_POINT('',(0.213846491495602,-1.2,12.1453786182733));
#62544=CARTESIAN_POINT('Ctrl Pts',(0.213846491495599,-1.2,12.1453786182733));
#62545=CARTESIAN_POINT('Ctrl Pts',(0.195932239642712,-1.22117287959761,
12.1249605953279));
#62546=CARTESIAN_POINT('Ctrl Pts',(0.17709346156536,-1.24191631337165,12.1049180269287));
#62547=CARTESIAN_POINT('Ctrl Pts',(0.149359662911878,-1.27453035159476,
12.0731904402628));
#62548=CARTESIAN_POINT('Ctrl Pts',(0.135822023537843,-1.29050619980739,
12.0576008960751));
#62549=CARTESIAN_POINT('Ctrl Pts',(0.12821877836405,-1.30000000000026,12.0483048527163));
#62550=CARTESIAN_POINT('',(0.370132012244428,-0.653834841366415,12.1361424506532));
#62551=CARTESIAN_POINT('Ctrl Pts',(0.370132012242185,-0.653834841365131,
12.136142450691));
#62552=CARTESIAN_POINT('Ctrl Pts',(0.354420225940763,-0.715934737885519,
12.1373205842513));
#62553=CARTESIAN_POINT('Ctrl Pts',(0.332824972003976,-0.793120943268795,
12.1388328601562));
#62554=CARTESIAN_POINT('Ctrl Pts',(0.306961911531932,-0.886126995183554,
12.1404786488211));
#62555=CARTESIAN_POINT('Ctrl Pts',(0.300477517120967,-0.909338780067549,
12.1408773304724));
#62556=CARTESIAN_POINT('Ctrl Pts',(0.267922703219645,-1.02407623900668,
12.1428079516095));
#62557=CARTESIAN_POINT('Ctrl Pts',(0.241155291200104,-1.11212798593213,
12.1441977398301));
#62558=CARTESIAN_POINT('Ctrl Pts',(0.2138464914956,-1.2,12.1453786182733));
#62559=CARTESIAN_POINT('Ctrl Pts',(0.509087305687303,0.653834841531096,
12.123751630128));
#62560=CARTESIAN_POINT('Ctrl Pts',(0.487797291982429,0.575994836847891,
12.0880522833113));
#62561=CARTESIAN_POINT('Ctrl Pts',(0.469153198145619,0.493638162905769,
12.0582419843226));
#62562=CARTESIAN_POINT('Ctrl Pts',(0.440252074501338,0.338128653655767,
12.0166877772658));
#62563=CARTESIAN_POINT('Ctrl Pts',(0.429043836054997,0.265646903379949,
12.0027380309224));
#62564=CARTESIAN_POINT('Ctrl Pts',(0.41067468427847,0.129700315862073,11.9867102146548));
#62565=CARTESIAN_POINT('Ctrl Pts',(0.40318577277248,0.0666145002772442,
11.9831901735331));
#62566=CARTESIAN_POINT('Ctrl Pts',(0.389879396129507,-0.0595448625857636,
11.9840041603447));
#62567=CARTESIAN_POINT('Ctrl Pts',(0.383960588584499,-0.122774529296895,
11.9883274493114));
#62568=CARTESIAN_POINT('Ctrl Pts',(0.373635521614742,-0.260111751750111,
12.0063195248107));
#62569=CARTESIAN_POINT('Ctrl Pts',(0.369700559967849,-0.333922237377205,
12.0215526341913));
#62570=CARTESIAN_POINT('Ctrl Pts',(0.365867536509685,-0.491193347292214,
12.0662344420976));
#62571=CARTESIAN_POINT('Ctrl Pts',(0.366579815351903,-0.57435183090168,
12.0978053593006));
#62572=CARTESIAN_POINT('Ctrl Pts',(0.370132012193589,-0.653834841383324,
12.1361424506229));
#62573=CARTESIAN_POINT('Ctrl Pts',(0.0165023515695837,-1.3,11.7801519784138));
#62574=CARTESIAN_POINT('Ctrl Pts',(0.0256069538907904,-1.18514270861178,
11.69489057648));
#62575=CARTESIAN_POINT('Ctrl Pts',(0.0347010954712016,-1.06847604194512,
11.6224333483286));
#62576=CARTESIAN_POINT('Ctrl Pts',(0.0556862153948441,-0.794772684000851,
11.4846228591836));
#62577=CARTESIAN_POINT('Ctrl Pts',(0.0677962068234778,-0.636309800095196,
11.4311131089277));
#62578=CARTESIAN_POINT('Ctrl Pts',(0.0906597384266765,-0.319434907277159,
11.3586954735785));
#62579=CARTESIAN_POINT('Ctrl Pts',(0.102179986998412,-0.158333333333332,
11.3417434974973));
#62580=CARTESIAN_POINT('Ctrl Pts',(0.12267336889205,0.158333333333334,11.341205069791));
#62581=CARTESIAN_POINT('Ctrl Pts',(0.130506918224618,0.319434907277167,
11.357626654509));
#62582=CARTESIAN_POINT('Ctrl Pts',(0.151708180499798,0.636309800095206,
11.4289311819363));
#62583=CARTESIAN_POINT('Ctrl Pts',(0.161724215836605,0.79477268400084,11.4819406028846));
#62584=CARTESIAN_POINT('Ctrl Pts',(0.187312562459994,1.06847604194511,11.6185893253359));
#62585=CARTESIAN_POINT('Ctrl Pts',(0.199984062839908,1.18514270861178,11.6904949696929));
#62586=CARTESIAN_POINT('Ctrl Pts',(0.214250816488161,1.3,11.775156089792));
#62587=CARTESIAN_POINT('Ctrl Pts',(-0.0604153711163311,-1.3,11.7784866822066));
#62588=CARTESIAN_POINT('Ctrl Pts',(-0.0495900516861092,-1.18514270861178,
11.6934253742177));
#62589=CARTESIAN_POINT('Ctrl Pts',(-0.0393034571725303,-1.06847604194512,
11.6211520073311));
#62590=CARTESIAN_POINT('Ctrl Pts',(-0.0167839283489728,-0.794772684000851,
11.4837287737506));
#62591=CARTESIAN_POINT('Ctrl Pts',(-0.00537192228428078,-0.636309800095196,
11.4303857999306));
#62592=CARTESIAN_POINT('Ctrl Pts',(0.0169375195429119,-0.319434907277159,
11.3583392005554));
#62593=CARTESIAN_POINT('Ctrl Pts',(0.0272288683682581,-0.158333333333332,
11.3415640215952));
#62594=CARTESIAN_POINT('Ctrl Pts',(0.0477222502618957,0.158333333333334,
11.3413845456931));
#62595=CARTESIAN_POINT('Ctrl Pts',(0.0567846993408533,0.319434907277167,
11.3579829275322));
#62596=CARTESIAN_POINT('Ctrl Pts',(0.0785400513920397,0.636309800095206,
11.4296584909335));
#62597=CARTESIAN_POINT('Ctrl Pts',(0.0892540720927883,0.79477268400084,
11.4828346883176));
#62598=CARTESIAN_POINT('Ctrl Pts',(0.113308009816262,1.06847604194511,11.6198706663335));
#62599=CARTESIAN_POINT('Ctrl Pts',(0.124787057263008,1.18514270861178,11.6919601719553));
#62600=CARTESIAN_POINT('Ctrl Pts',(0.137333093802246,1.3,11.7768213859993));
#62601=CARTESIAN_POINT('Ctrl Pts',(-0.137333093802246,-1.3,11.7768213859993));
#62602=CARTESIAN_POINT('Ctrl Pts',(-0.124787057263009,-1.18514270861178,
11.6919601719553));
#62603=CARTESIAN_POINT('Ctrl Pts',(-0.113308009816262,-1.06847604194512,
11.6198706663335));
#62604=CARTESIAN_POINT('Ctrl Pts',(-0.0892540720927895,-0.794772684000851,
11.4828346883176));
#62605=CARTESIAN_POINT('Ctrl Pts',(-0.0785400513920391,-0.636309800095196,
11.4296584909335));
#62606=CARTESIAN_POINT('Ctrl Pts',(-0.0567846993408526,-0.319434907277159,
11.3579829275322));
#62607=CARTESIAN_POINT('Ctrl Pts',(-0.0477222502618955,-0.158333333333332,
11.3413845456931));
#62608=CARTESIAN_POINT('Ctrl Pts',(-0.027228868368258,0.158333333333334,
11.3415640215952));
#62609=CARTESIAN_POINT('Ctrl Pts',(-0.0169375195429113,0.319434907277167,
11.3583392005554));
#62610=CARTESIAN_POINT('Ctrl Pts',(0.00537192228428136,0.636309800095206,
11.4303857999306));
#62611=CARTESIAN_POINT('Ctrl Pts',(0.0167839283489716,0.79477268400084,
11.4837287737506));
#62612=CARTESIAN_POINT('Ctrl Pts',(0.03930345717253,1.06847604194511,11.6211520073311));
#62613=CARTESIAN_POINT('Ctrl Pts',(0.0495900516861087,1.18514270861178,
11.6934253742177));
#62614=CARTESIAN_POINT('Ctrl Pts',(0.0604153711163312,1.3,11.7784866822066));
#62615=CARTESIAN_POINT('Ctrl Pts',(-0.214250816488161,-1.3,11.775156089792));
#62616=CARTESIAN_POINT('Ctrl Pts',(-0.199984062839908,-1.18514270861178,
11.6904949696929));
#62617=CARTESIAN_POINT('Ctrl Pts',(-0.187312562459994,-1.06847604194512,
11.6185893253359));
#62618=CARTESIAN_POINT('Ctrl Pts',(-0.161724215836606,-0.794772684000851,
11.4819406028846));
#62619=CARTESIAN_POINT('Ctrl Pts',(-0.151708180499798,-0.636309800095196,
11.4289311819363));
#62620=CARTESIAN_POINT('Ctrl Pts',(-0.130506918224617,-0.319434907277159,
11.357626654509));
#62621=CARTESIAN_POINT('Ctrl Pts',(-0.122673368892049,-0.158333333333332,
11.341205069791));
#62622=CARTESIAN_POINT('Ctrl Pts',(-0.102179986998412,0.158333333333334,
11.3417434974973));
#62623=CARTESIAN_POINT('Ctrl Pts',(-0.0906597384266759,0.319434907277167,
11.3586954735785));
#62624=CARTESIAN_POINT('Ctrl Pts',(-0.0677962068234772,0.636309800095206,
11.4311131089277));
#62625=CARTESIAN_POINT('Ctrl Pts',(-0.055686215394845,0.79477268400084,
11.4846228591836));
#62626=CARTESIAN_POINT('Ctrl Pts',(-0.0347010954712021,1.06847604194511,
11.6224333483286));
#62627=CARTESIAN_POINT('Ctrl Pts',(-0.0256069538907909,1.18514270861178,
11.69489057648));
#62628=CARTESIAN_POINT('Ctrl Pts',(-0.0165023515695837,1.3,11.7801519784138));
#62629=CARTESIAN_POINT('Ctrl Pts',(-0.214250816488161,-1.3,11.775156089792));
#62630=CARTESIAN_POINT('Ctrl Pts',(-0.199984062839908,-1.18514270861178,
11.6904949696929));
#62631=CARTESIAN_POINT('Ctrl Pts',(-0.187312562459994,-1.06847604194512,
11.6185893253359));
#62632=CARTESIAN_POINT('Ctrl Pts',(-0.161724215836606,-0.794772684000851,
11.4819406028846));
#62633=CARTESIAN_POINT('Ctrl Pts',(-0.151708180499798,-0.636309800095197,
11.4289311819364));
#62634=CARTESIAN_POINT('Ctrl Pts',(-0.130506918224617,-0.319434907277159,
11.357626654509));
#62635=CARTESIAN_POINT('Ctrl Pts',(-0.122673368892049,-0.158333333333332,
11.341205069791));
#62636=CARTESIAN_POINT('Ctrl Pts',(-0.102179986998412,0.158333333333334,
11.3417434974973));
#62637=CARTESIAN_POINT('Ctrl Pts',(-0.0906597384266759,0.319434907277167,
11.3586954735785));
#62638=CARTESIAN_POINT('Ctrl Pts',(-0.0677962068234772,0.636309800095206,
11.4311131089277));
#62639=CARTESIAN_POINT('Ctrl Pts',(-0.055686215394845,0.79477268400084,
11.4846228591836));
#62640=CARTESIAN_POINT('Ctrl Pts',(-0.0347010954712021,1.06847604194511,
11.6224333483286));
#62641=CARTESIAN_POINT('Ctrl Pts',(-0.025606953890791,1.18514270861178,
11.69489057648));
#62642=CARTESIAN_POINT('Ctrl Pts',(-0.0165023515695838,1.3,11.7801519784138));
#62643=CARTESIAN_POINT('Ctrl Pts',(-0.214250816488491,-1.30000000000266,
11.775156089794));
#62644=CARTESIAN_POINT('Ctrl Pts',(-0.199984062840104,-1.18514270861358,
11.690494969694));
#62645=CARTESIAN_POINT('Ctrl Pts',(-0.18731256246008,-1.06847604194603,
11.6185893253364));
#62646=CARTESIAN_POINT('Ctrl Pts',(-0.161724215836606,-0.794772684000851,
11.4819406028846));
#62647=CARTESIAN_POINT('Ctrl Pts',(-0.151708180499798,-0.636309800095197,
11.4289311819364));
#62648=CARTESIAN_POINT('Ctrl Pts',(-0.130506918224617,-0.319434907277159,
11.357626654509));
#62649=CARTESIAN_POINT('Ctrl Pts',(-0.122673368892049,-0.158333333333332,
11.341205069791));
#62650=CARTESIAN_POINT('Ctrl Pts',(-0.102179986998412,0.158333333333334,
11.3417434974973));
#62651=CARTESIAN_POINT('Ctrl Pts',(-0.0906597384266759,0.319434907277167,
11.3586954735785));
#62652=CARTESIAN_POINT('Ctrl Pts',(-0.0677962068234772,0.636309800095206,
11.4311131089277));
#62653=CARTESIAN_POINT('Ctrl Pts',(-0.055686215394845,0.79477268400084,
11.4846228591836));
#62654=CARTESIAN_POINT('Ctrl Pts',(-0.0347010954709978,1.06847604194777,
11.62243334833));
#62655=CARTESIAN_POINT('Ctrl Pts',(-0.0256069538903818,1.18514270861702,
11.6948905764833));
#62656=CARTESIAN_POINT('Ctrl Pts',(-0.0165023515689693,1.30000000000775,
11.7801519784196));
#62657=CARTESIAN_POINT('Ctrl Pts',(-0.219717436762998,-1.30000000000266,
11.7819904857412));
#62658=CARTESIAN_POINT('Ctrl Pts',(-0.204772182758638,-1.18514270861358,
11.6972293577337));
#62659=CARTESIAN_POINT('Ctrl Pts',(-0.192015477656179,-1.06847604194603,
11.6251313099799));
#62660=CARTESIAN_POINT('Ctrl Pts',(-0.167600922680588,-0.794772684000851,
11.4878246451312));
#62661=CARTESIAN_POINT('Ctrl Pts',(-0.161103853486099,-0.636309800095197,
11.4338490762469));
#62662=CARTESIAN_POINT('Ctrl Pts',(-0.141607349608946,-0.319434907277159,
11.3620417362896));
#62663=CARTESIAN_POINT('Ctrl Pts',(-0.133278717909188,-0.158333333333332,
11.3458490651824));
#62664=CARTESIAN_POINT('Ctrl Pts',(-0.112567852728384,0.158333333333334,
11.3464812379208));
#62665=CARTESIAN_POINT('Ctrl Pts',(-0.10105798971678,0.319434907277167,
11.363381908291));
#62666=CARTESIAN_POINT('Ctrl Pts',(-0.0765909966189224,0.636309800095206,
11.4363224854275));
#62667=CARTESIAN_POINT('Ctrl Pts',(-0.0620129494727472,0.79477268400084,
11.4905334946661));
#62668=CARTESIAN_POINT('Ctrl Pts',(-0.0397026858016881,1.06847604194777,
11.6290281458399));
#62669=CARTESIAN_POINT('Ctrl Pts',(-0.030380819974229,1.18514270861702,
11.7017443480897));
#62670=CARTESIAN_POINT('Ctrl Pts',(-0.0213943747858902,1.30000000000775,
11.7872275498281));
#62671=CARTESIAN_POINT('Ctrl Pts',(-0.224217870079186,-1.30000000000266,
11.793407741607));
#62672=CARTESIAN_POINT('Ctrl Pts',(-0.208244333473234,-1.18514270861359,
11.7113717526455));
#62673=CARTESIAN_POINT('Ctrl Pts',(-0.195355471940572,-1.06847604194604,
11.6410945205255));
#62674=CARTESIAN_POINT('Ctrl Pts',(-0.172705839898739,-0.794772684000856,
11.5059051360521));
#62675=CARTESIAN_POINT('Ctrl Pts',(-0.17141959502437,-0.636309800095198,
11.4500701232598));
#62676=CARTESIAN_POINT('Ctrl Pts',(-0.154685054000868,-0.319434907277159,
11.3774846305103));
#62677=CARTESIAN_POINT('Ctrl Pts',(-0.145979289299972,-0.158333333333332,
11.3603771369061));
#62678=CARTESIAN_POINT('Ctrl Pts',(-0.125122661406262,0.158333333333334,
11.3610623482316));
#62679=CARTESIAN_POINT('Ctrl Pts',(-0.114003801242036,0.319434907277166,
11.3789777248218));
#62680=CARTESIAN_POINT('Ctrl Pts',(-0.0861527771105432,0.636309800095206,
11.4527090703651));
#62681=CARTESIAN_POINT('Ctrl Pts',(-0.0651925831004888,0.794772684000841,
11.5086371330806));
#62682=CARTESIAN_POINT('Ctrl Pts',(-0.0411580507325554,1.06847604194777,
11.6450217831126));
#62683=CARTESIAN_POINT('Ctrl Pts',(-0.0322838315682777,1.18514270861703,
11.71594832617));
#62684=CARTESIAN_POINT('Ctrl Pts',(-0.0249390517347361,1.30000000000775,
11.7987655508345));
#62685=CARTESIAN_POINT('Ctrl Pts',(-0.230940212073702,-1.30000000000266,
11.8101274281025));
#62686=CARTESIAN_POINT('Ctrl Pts',(-0.215296597918111,-1.18514270861359,
11.7317529065375));
#62687=CARTESIAN_POINT('Ctrl Pts',(-0.202859343717702,-1.06847604194603,
11.6641508310356));
#62688=CARTESIAN_POINT('Ctrl Pts',(-0.181534131377252,-0.794772684000852,
11.5328630183039));
#62689=CARTESIAN_POINT('Ctrl Pts',(-0.181705445881087,-0.636309800095196,
11.4763566179852));
#62690=CARTESIAN_POINT('Ctrl Pts',(-0.166289710338157,-0.319434907277158,
11.4038054324094));
#62691=CARTESIAN_POINT('Ctrl Pts',(-0.158119436476584,-0.158333333333332,
11.3853366219702));
#62692=CARTESIAN_POINT('Ctrl Pts',(-0.137170837613514,0.158333333333334,
11.3860097881351));
#62693=CARTESIAN_POINT('Ctrl Pts',(-0.125758787670006,0.319434907277168,
11.4052233409097));
#62694=CARTESIAN_POINT('Ctrl Pts',(-0.0957207317599793,0.636309800095206,
11.4789999219884));
#62695=CARTESIAN_POINT('Ctrl Pts',(-0.0714304791785025,0.794772684000838,
11.5358058689093));
#62696=CARTESIAN_POINT('Ctrl Pts',(-0.0459133378491548,1.06847604194777,
11.6683582509209));
#62697=CARTESIAN_POINT('Ctrl Pts',(-0.0369336206498608,1.18514270861702,
11.7366069404878));
#62698=CARTESIAN_POINT('Ctrl Pts',(-0.0300196112296146,1.30000000000775,
11.8157273049977));
#62699=CARTESIAN_POINT('Ctrl Pts',(-0.236830809019557,-1.30000000000266,
11.823913013989));
#62700=CARTESIAN_POINT('Ctrl Pts',(-0.221807828841873,-1.18514270861359,
11.7482186534331));
#62701=CARTESIAN_POINT('Ctrl Pts',(-0.209674709327399,-1.06847604194603,
11.6825842381735));
#62702=CARTESIAN_POINT('Ctrl Pts',(-0.188320932273469,-0.794772684000854,
11.5541960949243));
#62703=CARTESIAN_POINT('Ctrl Pts',(-0.186759959728292,-0.636309800095198,
11.4973087358865));
#62704=CARTESIAN_POINT('Ctrl Pts',(-0.17148164451981,-0.31943490727716,
11.4247589069605));
#62705=CARTESIAN_POINT('Ctrl Pts',(-0.164914018978241,-0.158333333333333,
11.4051578558322));
#62706=CARTESIAN_POINT('Ctrl Pts',(-0.144542563833041,0.158333333333335,
11.4057504239017));
#62707=CARTESIAN_POINT('Ctrl Pts',(-0.133007072754958,0.319434907277168,
11.4259090530163));
#62708=CARTESIAN_POINT('Ctrl Pts',(-0.102169758375363,0.636309800095207,
11.4997371727135));
#62709=CARTESIAN_POINT('Ctrl Pts',(-0.0763311114729764,0.794772684000843,
11.5572650096014));
#62710=CARTESIAN_POINT('Ctrl Pts',(-0.0503084407492601,1.06847604194778,
11.6870176439549));
#62711=CARTESIAN_POINT('Ctrl Pts',(-0.0413782275088885,1.18514270861702,
11.7532925032257));
#62712=CARTESIAN_POINT('Ctrl Pts',(-0.0347820509496016,1.30000000000775,
11.8296771141638));
#62713=CARTESIAN_POINT('Ctrl Pts',(-0.242947140261799,-1.30000000000266,
11.8377863890196));
#62714=CARTESIAN_POINT('Ctrl Pts',(-0.228673177411667,-1.18514270861359,
11.7650169188838));
#62715=CARTESIAN_POINT('Ctrl Pts',(-0.216911379186633,-1.06847604194603,
11.701547333098));
#62716=CARTESIAN_POINT('Ctrl Pts',(-0.19554287518801,-0.794772684000852,
11.5764044861699));
#62717=CARTESIAN_POINT('Ctrl Pts',(-0.192246096408202,-0.636309800095196,
11.519203297661));
#62718=CARTESIAN_POINT('Ctrl Pts',(-0.176523859962701,-0.319434907277158,
11.4468119320853));
#62719=CARTESIAN_POINT('Ctrl Pts',(-0.171159810408635,-0.158333333333333,
11.4260654238642));
#62720=CARTESIAN_POINT('Ctrl Pts',(-0.149913038564751,0.158333333333334,
11.4267203975001));
#62721=CARTESIAN_POINT('Ctrl Pts',(-0.135766465861496,0.319434907277169,
11.4481164809824));
#62722=CARTESIAN_POINT('Ctrl Pts',(-0.104674146178431,0.636309800095208,
11.5218529767954));
#62723=CARTESIAN_POINT('Ctrl Pts',(-0.0812829026006441,0.79477268400084,
11.579666864191));
#62724=CARTESIAN_POINT('Ctrl Pts',(-0.0557924094028948,1.06847604194777,
11.7061748677036));
#62725=CARTESIAN_POINT('Ctrl Pts',(-0.0467597412619023,1.18514270861702,
11.7702841191655));
#62726=CARTESIAN_POINT('Ctrl Pts',(-0.0397282949695003,1.30000000000775,
11.8437419949516));
#62727=CARTESIAN_POINT('Ctrl Pts',(-0.250450467575642,-1.30000000000266,
11.8513121660939));
#62728=CARTESIAN_POINT('Ctrl Pts',(-0.236823957280526,-1.18514270861359,
11.7813326284548));
#62729=CARTESIAN_POINT('Ctrl Pts',(-0.22527978638569,-1.06847604194603,
11.7199380521404));
#62730=CARTESIAN_POINT('Ctrl Pts',(-0.20342106280045,-0.794772684000851,
11.5979372769874));
#62731=CARTESIAN_POINT('Ctrl Pts',(-0.198182879193841,-0.636309800095198,
11.5404728242816));
#62732=CARTESIAN_POINT('Ctrl Pts',(-0.180833769426929,-0.31943490727716,
11.4683672228574));
#62733=CARTESIAN_POINT('Ctrl Pts',(-0.174706384337292,-0.158333333333333,
11.4467454432747));
#62734=CARTESIAN_POINT('Ctrl Pts',(-0.152838862898622,0.158333333333335,
11.4474283582768));
#62735=CARTESIAN_POINT('Ctrl Pts',(-0.138654662265025,0.319434907277169,
11.4697025037864));
#62736=CARTESIAN_POINT('Ctrl Pts',(-0.108291876353905,0.636309800095209,
11.5432613801654));
#62737=CARTESIAN_POINT('Ctrl Pts',(-0.0866786973629504,0.794772684000843,
11.6014545180862));
#62738=CARTESIAN_POINT('Ctrl Pts',(-0.0613805082616765,1.06847604194778,
11.7249531277311));
#62739=CARTESIAN_POINT('Ctrl Pts',(-0.0520560587818162,1.18514270861703,
11.7870408114846));
#62740=CARTESIAN_POINT('Ctrl Pts',(-0.0443578084938825,1.30000000000775,
11.8577582069501));
#62741=CARTESIAN_POINT('Ctrl Pts',(-0.260323420711465,-1.30000000000266,
11.873400837634));
#62742=CARTESIAN_POINT('Ctrl Pts',(-0.247802116813471,-1.18514270861359,
11.8079670508444));
#62743=CARTESIAN_POINT('Ctrl Pts',(-0.236836054686001,-1.06847604194603,
11.7499259468651));
#62744=CARTESIAN_POINT('Ctrl Pts',(-0.215095177033385,-0.794772684000849,
11.6329179617837));
#62745=CARTESIAN_POINT('Ctrl Pts',(-0.208135190489906,-0.636309800095196,
11.5748097817095));
#62746=CARTESIAN_POINT('Ctrl Pts',(-0.189098646525768,-0.319434907277158,
11.5030319137751));
#62747=CARTESIAN_POINT('Ctrl Pts',(-0.181564680695925,-0.158333333333333,
11.4799869089716));
#62748=CARTESIAN_POINT('Ctrl Pts',(-0.159079342990061,0.158333333333334,
11.4807109001114));
#62749=CARTESIAN_POINT('Ctrl Pts',(-0.145397680171436,0.319434907277169,
11.5044627691746));
#62750=CARTESIAN_POINT('Ctrl Pts',(-0.11604690429894,0.636309800095208,
11.5777502411529));
#62751=CARTESIAN_POINT('Ctrl Pts',(-0.0961679003060289,0.794772684000839,
11.6365852973473));
#62752=CARTESIAN_POINT('Ctrl Pts',(-0.0711454710836636,1.06847604194777,
11.7551190889297));
#62753=CARTESIAN_POINT('Ctrl Pts',(-0.0615643462518385,1.18514270861702,
11.8138663524707));
#62754=CARTESIAN_POINT('Ctrl Pts',(-0.0532333790263047,1.30000000000775,
11.8800519932859));
#62755=CARTESIAN_POINT('Ctrl Pts',(-0.276239090050472,-1.30000000000266,
11.9032333655254));
#62756=CARTESIAN_POINT('Ctrl Pts',(-0.266429290422055,-1.18514270861359,
11.8437129298302));
#62757=CARTESIAN_POINT('Ctrl Pts',(-0.256910355903995,-1.06847604194603,
11.7900873376451));
#62758=CARTESIAN_POINT('Ctrl Pts',(-0.235591669503331,-0.794772684000857,
11.6798197597031));
#62759=CARTESIAN_POINT('Ctrl Pts',(-0.224279524630662,-0.636309800095201,
11.621290618903));
#62760=CARTESIAN_POINT('Ctrl Pts',(-0.201942143076302,-0.319434907277161,
11.5502056857409));
#62761=CARTESIAN_POINT('Ctrl Pts',(-0.192515727923751,-0.158333333333333,
11.5252832663945));
#62762=CARTESIAN_POINT('Ctrl Pts',(-0.168732153072857,0.158333333333335,
11.5261075273927));
#62763=CARTESIAN_POINT('Ctrl Pts',(-0.15525846429931,0.319434907277169,
11.5517979296741));
#62764=CARTESIAN_POINT('Ctrl Pts',(-0.127350849694823,0.63630980009521,
11.6246764575031));
#62765=CARTESIAN_POINT('Ctrl Pts',(-0.110979158576652,0.794772684000847,
11.6842968419898));
#62766=CARTESIAN_POINT('Ctrl Pts',(-0.0858860639788656,1.06847604194778,
11.7961802575163));
#62767=CARTESIAN_POINT('Ctrl Pts',(-0.0754350815714248,1.18514270861703,
11.8504719847924));
#62768=CARTESIAN_POINT('Ctrl Pts',(-0.0653949876172695,1.30000000000775,
11.9106252544515));
#62769=CARTESIAN_POINT('Ctrl Pts',(-0.29517793742003,-1.30000000000266,
11.9384674305417));
#62770=CARTESIAN_POINT('Ctrl Pts',(-0.287639116641684,-1.18514270861359,
11.8861840873237));
#62771=CARTESIAN_POINT('Ctrl Pts',(-0.279540159415899,-1.06847604194604,
11.8378938566315));
#62772=CARTESIAN_POINT('Ctrl Pts',(-0.259535920785081,-0.794772684000854,
11.7355586520591));
#62773=CARTESIAN_POINT('Ctrl Pts',(-0.246694283457694,-0.636309800095197,
11.6759025600909));
#62774=CARTESIAN_POINT('Ctrl Pts',(-0.221681184675174,-0.319434907277158,
11.6054673769956));
#62775=CARTESIAN_POINT('Ctrl Pts',(-0.208422081944555,-0.158333333333332,
11.5785818413453));
#62776=CARTESIAN_POINT('Ctrl Pts',(-0.183440518011101,0.158333333333334,
11.5795669581184));
#62777=CARTESIAN_POINT('Ctrl Pts',(-0.17205280598463,0.319434907277167,
11.607442706844));
#62778=CARTESIAN_POINT('Ctrl Pts',(-0.145498397797482,0.636309800095206,
11.6798741210746));
#62779=CARTESIAN_POINT('Ctrl Pts',(-0.131176827593208,0.794772684000839,
11.7405507697081));
#62780=CARTESIAN_POINT('Ctrl Pts',(-0.104598028284302,1.06847604194777,
11.8446411509602));
#62781=CARTESIAN_POINT('Ctrl Pts',(-0.0926448526882476,1.18514270861703,
11.8936822166786));
#62782=CARTESIAN_POINT('Ctrl Pts',(-0.0802434788755316,1.30000000000775,
11.9467074789994));
#62783=CARTESIAN_POINT('Ctrl Pts',(-0.309070134152884,-1.30000000000266,
11.9626521575258));
#62784=CARTESIAN_POINT('Ctrl Pts',(-0.304257903017002,-1.18514270861359,
11.9151094210709));
#62785=CARTESIAN_POINT('Ctrl Pts',(-0.297805472165891,-1.06847604194604,
11.870356610646));
#62786=CARTESIAN_POINT('Ctrl Pts',(-0.279109876632523,-0.794772684000858,
11.7734139530484));
#62787=CARTESIAN_POINT('Ctrl Pts',(-0.263186794327446,-0.636309800095199,
11.7134052465165));
#62788=CARTESIAN_POINT('Ctrl Pts',(-0.236216413283395,-0.319434907277159,
11.6435063095043));
#62789=CARTESIAN_POINT('Ctrl Pts',(-0.221758045974766,-0.158333333333333,
11.6150838982541));
#62790=CARTESIAN_POINT('Ctrl Pts',(-0.19597593177251,0.158333333333335,
11.6161785319858));
#62791=CARTESIAN_POINT('Ctrl Pts',(-0.185020774202201,0.319434907277168,
11.6456538669924));
#62792=CARTESIAN_POINT('Ctrl Pts',(-0.158724055077794,0.636309800095208,
11.7178674543161));
#62793=CARTESIAN_POINT('Ctrl Pts',(-0.145416493623235,0.794772684000842,
11.7793663528091));
#62794=CARTESIAN_POINT('Ctrl Pts',(-0.117930848075837,1.06847604194778,
11.8780739513503));
#62795=CARTESIAN_POINT('Ctrl Pts',(-0.105163024546976,1.18514270861703,
11.9234613046999));
#62796=CARTESIAN_POINT('Ctrl Pts',(-0.09152489500333,1.30000000000776,11.971509149467));
#62797=CARTESIAN_POINT('Ctrl Pts',(-0.318947568796887,-1.30000000000267,
11.9786313169475));
#62798=CARTESIAN_POINT('Ctrl Pts',(-0.315273910384892,-1.18514270861359,
11.9343985878693));
#62799=CARTESIAN_POINT('Ctrl Pts',(-0.309537129818828,-1.06847604194604,
11.89209096527));
#62800=CARTESIAN_POINT('Ctrl Pts',(-0.2915177941702,-0.794772684000857,
11.7987992745377));
#62801=CARTESIAN_POINT('Ctrl Pts',(-0.274625041771405,-0.6363098000952,
11.7383363870941));
#62802=CARTESIAN_POINT('Ctrl Pts',(-0.246787850417295,-0.31943490727716,
11.6687157402135));
#62803=CARTESIAN_POINT('Ctrl Pts',(-0.231396951287163,-0.158333333333333,
11.6392967488708));
#62804=CARTESIAN_POINT('Ctrl Pts',(-0.205226404564591,0.158333333333335,
11.6404513861524));
#62805=CARTESIAN_POINT('Ctrl Pts',(-0.19470126514578,0.319434907277169,
11.670989837913));
#62806=CARTESIAN_POINT('Ctrl Pts',(-0.16871252234342,0.636309800095209,
11.7430340505382));
#62807=CARTESIAN_POINT('Ctrl Pts',(-0.156409891339114,0.794772684000843,
11.8050042227834));
#62808=CARTESIAN_POINT('Ctrl Pts',(-0.127831439852261,1.06847604194778,
11.9001890837079));
#62809=CARTESIAN_POINT('Ctrl Pts',(-0.114124307099296,1.18514270861703,
11.9432009124148));
#62810=CARTESIAN_POINT('Ctrl Pts',(-0.0990805943061879,1.30000000000776,
11.9880225704805));
#62811=CARTESIAN_POINT('Ctrl Pts',(-0.325037630289391,-1.30000000000267,
11.9893873191805));
#62812=CARTESIAN_POINT('Ctrl Pts',(-0.322785150534061,-1.18514270861359,
11.9472150763738));
#62813=CARTESIAN_POINT('Ctrl Pts',(-0.317960794414666,-1.06847604194604,
11.9064425391265));
#62814=CARTESIAN_POINT('Ctrl Pts',(-0.300874017766708,-0.794772684000856,
11.8154834214201));
#62815=CARTESIAN_POINT('Ctrl Pts',(-0.28289635081279,-0.636309800095199,
11.7548283828312));
#62816=CARTESIAN_POINT('Ctrl Pts',(-0.254121503986549,-0.31943490727716,
11.6854673897822));
#62817=CARTESIAN_POINT('Ctrl Pts',(-0.237602570414715,-0.158333333333333,
11.6554698969414));
#62818=CARTESIAN_POINT('Ctrl Pts',(-0.211105296395253,0.158333333333335,
11.6566798966747));
#62819=CARTESIAN_POINT('Ctrl Pts',(-0.20125636216096,0.319434907277169,
11.6878608173297));
#62820=CARTESIAN_POINT('Ctrl Pts',(-0.175794578537588,0.636309800095209,
11.7597406177987));
#62821=CARTESIAN_POINT('Ctrl Pts',(-0.164323991831707,0.794772684000842,
11.82199900382));
#62822=CARTESIAN_POINT('Ctrl Pts',(-0.135233099564808,1.06847604194778,
11.9148039470579));
#62823=CARTESIAN_POINT('Ctrl Pts',(-0.120977627755776,1.18514270861703,
11.9562217008324));
#62824=CARTESIAN_POINT('Ctrl Pts',(-0.105059053476416,1.30000000000776,
11.9988853872153));
#62825=CARTESIAN_POINT('Ctrl Pts',(-0.3326990773971,-1.30000000000267,12.0028153799187));
#62826=CARTESIAN_POINT('Ctrl Pts',(-0.33185156874756,-1.18514270861359,
11.9632961021561));
#62827=CARTESIAN_POINT('Ctrl Pts',(-0.327940416842498,-1.06847604194604,
11.9244888658819));
#62828=CARTESIAN_POINT('Ctrl Pts',(-0.311827244718624,-0.794772684000857,
11.8364813450097));
#62829=CARTESIAN_POINT('Ctrl Pts',(-0.292912661410954,-0.6363098000952,
11.7754878653476));
#62830=CARTESIAN_POINT('Ctrl Pts',(-0.263172738621346,-0.31943490727716,
11.7064116664776));
#62831=CARTESIAN_POINT('Ctrl Pts',(-0.245372626632432,-0.158333333333333,
11.6756830038836));
#62832=CARTESIAN_POINT('Ctrl Pts',(-0.21843054828428,0.158333333333335,
11.6769697718535));
#62833=CARTESIAN_POINT('Ctrl Pts',(-0.209429046196659,0.319434907277169,
11.7089467663506));
#62834=CARTESIAN_POINT('Ctrl Pts',(-0.184003779677574,0.63630980009521,
11.7807223104256));
#62835=CARTESIAN_POINT('Ctrl Pts',(-0.172594457528252,0.794772684000843,
11.843509730546));
#62836=CARTESIAN_POINT('Ctrl Pts',(-0.14234409618874,1.06847604194778,11.9334185969874));
#62837=CARTESIAN_POINT('Ctrl Pts',(-0.127315850771895,1.18514270861703,
11.972852455381));
#62838=CARTESIAN_POINT('Ctrl Pts',(-0.110353620475885,1.30000000000776,
12.0128019553371));
#62839=CARTESIAN_POINT('Ctrl Pts',(-0.342890406495062,-1.30000000000267,
12.0187005673102));
#62840=CARTESIAN_POINT('Ctrl Pts',(-0.343404801620718,-1.18514270861359,
11.9824364379119));
#62841=CARTESIAN_POINT('Ctrl Pts',(-0.340328286663603,-1.06847604194604,
11.9460455915638));
#62842=CARTESIAN_POINT('Ctrl Pts',(-0.324925201007721,-0.794772684000854,
11.8616827150327));
#62843=CARTESIAN_POINT('Ctrl Pts',(-0.30440917001716,-0.636309800095197,
11.8003810198176));
#62844=CARTESIAN_POINT('Ctrl Pts',(-0.27406327984717,-0.319434907277158,
11.7315459342188));
#62845=CARTESIAN_POINT('Ctrl Pts',(-0.256131817511993,-0.158333333333333,
11.6996667708295));
#62846=CARTESIAN_POINT('Ctrl Pts',(-0.229344633515742,0.158333333333334,
11.7009131340153));
#62847=CARTESIAN_POINT('Ctrl Pts',(-0.220929192197765,0.319434907277169,
11.7339227857933));
#62848=CARTESIAN_POINT('Ctrl Pts',(-0.195814697950992,0.636309800095208,
11.8055326520784));
#62849=CARTESIAN_POINT('Ctrl Pts',(-0.185004960135747,0.794772684000838,
11.86886708947));
#62850=CARTESIAN_POINT('Ctrl Pts',(-0.153575863981641,1.06847604194777,
11.9552861106441));
#62851=CARTESIAN_POINT('Ctrl Pts',(-0.137630621387517,1.18514270861703,
11.9923508536253));
#62852=CARTESIAN_POINT('Ctrl Pts',(-0.119344627361765,1.30000000000776,
12.0290727474613));
#62853=CARTESIAN_POINT('Ctrl Pts',(-0.35278967854841,-1.30000000000267,
12.03461531483));
#62854=CARTESIAN_POINT('Ctrl Pts',(-0.355844257705039,-1.18514270861359,
12.0013185840351));
#62855=CARTESIAN_POINT('Ctrl Pts',(-0.354443939977227,-1.06847604194604,
11.967144126374));
#62856=CARTESIAN_POINT('Ctrl Pts',(-0.340917222891307,-0.794772684000859,
11.8861665679506));
#62857=CARTESIAN_POINT('Ctrl Pts',(-0.318967482009493,-0.636309800095201,
11.8245812730303));
#62858=CARTESIAN_POINT('Ctrl Pts',(-0.286878403158749,-0.319434907277161,
11.7562488211688));
#62859=CARTESIAN_POINT('Ctrl Pts',(-0.266663621926033,-0.158333333333333,
11.7236716820602));
#62860=CARTESIAN_POINT('Ctrl Pts',(-0.238406038584845,0.158333333333335,
11.7252091998553));
#62861=CARTESIAN_POINT('Ctrl Pts',(-0.23001997737375,0.319434907277169,
11.7593411259456));
#62862=CARTESIAN_POINT('Ctrl Pts',(-0.205249587648581,0.63630980009521,
11.8307702147613));
#62863=CARTESIAN_POINT('Ctrl Pts',(-0.196579192702014,0.794772684000844,
11.8943575162252));
#62864=CARTESIAN_POINT('Ctrl Pts',(-0.163974351536508,1.06847604194778,
11.9772659406248));
#62865=CARTESIAN_POINT('Ctrl Pts',(-0.146811779920227,1.18514270861703,
12.0120066261991));
#62866=CARTESIAN_POINT('Ctrl Pts',(-0.126600064299955,1.30000000000777,
12.0456000124843));
#62867=CARTESIAN_POINT('Ctrl Pts',(-0.362458227405669,-1.30000000000267,
12.0505988729736));
#62868=CARTESIAN_POINT('Ctrl Pts',(-0.366646738676606,-1.18514270861359,
12.0206060978921));
#62869=CARTESIAN_POINT('Ctrl Pts',(-0.36606713314898,-1.06847604194604,
11.9888494879981));
#62870=CARTESIAN_POINT('Ctrl Pts',(-0.353712824767352,-0.794772684000856,
11.9114105549845));
#62871=CARTESIAN_POINT('Ctrl Pts',(-0.331642810172518,-0.636309800095202,
11.8491847076909));
#62872=CARTESIAN_POINT('Ctrl Pts',(-0.2992336617953,-0.319434907277162,
11.7810309769482));
#62873=CARTESIAN_POINT('Ctrl Pts',(-0.277779816053976,-0.158333333333334,
11.7475495932847));
#62874=CARTESIAN_POINT('Ctrl Pts',(-0.249752596286747,0.158333333333336,
11.7490435296266));
#62875=CARTESIAN_POINT('Ctrl Pts',(-0.243245132670091,0.319434907277169,
11.7839537572776));
#62876=CARTESIAN_POINT('Ctrl Pts',(-0.21843059765032,0.636309800095211,
11.8552831172205));
#62877=CARTESIAN_POINT('Ctrl Pts',(-0.20843821376195,0.794772684000847,
11.9197789423395));
#62878=CARTESIAN_POINT('Ctrl Pts',(-0.174222980806344,1.06847604194778,
11.999286491599));
#62879=CARTESIAN_POINT('Ctrl Pts',(-0.156269703867267,1.18514270861703,
12.0316394533571));
#62880=CARTESIAN_POINT('Ctrl Pts',(-0.135173656536452,1.30000000000776,
12.0619295048437));
#62881=CARTESIAN_POINT('Ctrl Pts',(-0.375985236281673,-1.30000000000266,
12.0717119172313));
#62882=CARTESIAN_POINT('Ctrl Pts',(-0.383369052387185,-1.18514270861359,
12.0457045367987));
#62883=CARTESIAN_POINT('Ctrl Pts',(-0.384870749705919,-1.06847604194604,
12.0169282275241));
#62884=CARTESIAN_POINT('Ctrl Pts',(-0.374751099814466,-0.794772684000857,
11.9440524168714));
#62885=CARTESIAN_POINT('Ctrl Pts',(-0.350303398133014,-0.636309800095203,
11.881548963167));
#62886=CARTESIAN_POINT('Ctrl Pts',(-0.316274483201399,-0.319434907277163,
11.8139400195225));
#62887=CARTESIAN_POINT('Ctrl Pts',(-0.293277812625114,-0.158333333333334,
11.7792453136778));
#62888=CARTESIAN_POINT('Ctrl Pts',(-0.26415322173086,0.158333333333336,
11.7809700651923));
#62889=CARTESIAN_POINT('Ctrl Pts',(-0.257612583060493,0.319434907277169,
11.8173973229585));
#62890=CARTESIAN_POINT('Ctrl Pts',(-0.233157480947777,0.636309800095211,
11.8885035723848));
#62891=CARTESIAN_POINT('Ctrl Pts',(-0.22547365179888,0.794772684000849,
11.9534155283702));
#62892=CARTESIAN_POINT('Ctrl Pts',(-0.189605353394397,1.06847604194778,
12.0282785934395));
#62893=CARTESIAN_POINT('Ctrl Pts',(-0.170088629217099,1.18514270861703,
12.0575394195504));
#62894=CARTESIAN_POINT('Ctrl Pts',(-0.146581238190558,1.30000000000776,
12.0836556248532));
#62895=CARTESIAN_POINT('Ctrl Pts',(-0.388002912938967,-1.30000000000267,
12.0886184370541));
#62896=CARTESIAN_POINT('Ctrl Pts',(-0.397056775472148,-1.18514270861359,
12.0660581729704));
#62897=CARTESIAN_POINT('Ctrl Pts',(-0.399691866065676,-1.06847604194604,
12.0398281403293));
#62898=CARTESIAN_POINT('Ctrl Pts',(-0.390950805233306,-0.794772684000856,
11.9707536181264));
#62899=CARTESIAN_POINT('Ctrl Pts',(-0.365574569069799,-0.6363098000952,
11.9077858528155));
#62900=CARTESIAN_POINT('Ctrl Pts',(-0.331012395793997,-0.319434907277161,
11.8404456471227));
#62901=CARTESIAN_POINT('Ctrl Pts',(-0.307244324656631,-0.158333333333333,
11.8046648039295));
#62902=CARTESIAN_POINT('Ctrl Pts',(-0.277878312564256,0.158333333333335,
11.8064520917464));
#62903=CARTESIAN_POINT('Ctrl Pts',(-0.271921220308894,0.31943490727717,
11.8440078854625));
#62904=CARTESIAN_POINT('Ctrl Pts',(-0.247398506714636,0.636309800095211,
11.9150137979284));
#62905=CARTESIAN_POINT('Ctrl Pts',(-0.240133095739699,0.794772684000846,
11.980543623939));
#62906=CARTESIAN_POINT('Ctrl Pts',(-0.202402311331478,1.06847604194778,
12.0517514903152));
#62907=CARTESIAN_POINT('Ctrl Pts',(-0.181594603253596,1.18514270861703,
12.0785149889845));
#62908=CARTESIAN_POINT('Ctrl Pts',(-0.156311445605007,1.30000000000775,
12.1012187394798));
#62909=CARTESIAN_POINT('Ctrl Pts',(-0.398046289221613,-1.30000000000267,
12.1044479065164));
#62910=CARTESIAN_POINT('Ctrl Pts',(-0.409380371236153,-1.18514270861359,
12.0848926609609));
#62911=CARTESIAN_POINT('Ctrl Pts',(-0.413583277518684,-1.06847604194604,
12.0608879172386));
#62912=CARTESIAN_POINT('Ctrl Pts',(-0.406818389292128,-0.794772684000856,
11.9951529262238));
#62913=CARTESIAN_POINT('Ctrl Pts',(-0.380431605342912,-0.636309800095201,
11.9317906969053));
#62914=CARTESIAN_POINT('Ctrl Pts',(-0.345050833649757,-0.319434907277161,
11.8647783468055));
#62915=CARTESIAN_POINT('Ctrl Pts',(-0.31985344599858,-0.158333333333334,
11.8281735574692));
#62916=CARTESIAN_POINT('Ctrl Pts',(-0.28998327846249,0.158333333333336,
11.8300842442891));
#62917=CARTESIAN_POINT('Ctrl Pts',(-0.28483235918426,0.319434907277171,
11.8686067719113));
#62918=CARTESIAN_POINT('Ctrl Pts',(-0.26034368584684,0.636309800095212,
11.9394966901605));
#62919=CARTESIAN_POINT('Ctrl Pts',(-0.253528051313759,0.794772684000847,
12.0055925283148));
#62920=CARTESIAN_POINT('Ctrl Pts',(-0.214078183372511,1.06847604194778,
12.0734284420653));
#62921=CARTESIAN_POINT('Ctrl Pts',(-0.192057012409329,1.18514270861703,
12.0978912232342));
#62922=CARTESIAN_POINT('Ctrl Pts',(-0.165091056553272,1.30000000000776,
12.1174531320774));
#62923=CARTESIAN_POINT('Ctrl Pts',(-0.405212661371279,-1.30000000000267,
12.1148940485206));
#62924=CARTESIAN_POINT('Ctrl Pts',(-0.417447748107665,-1.18514270861359,
12.0974907272638));
#62925=CARTESIAN_POINT('Ctrl Pts',(-0.422345660903717,-1.06847604194604,
12.0750525418653));
#62926=CARTESIAN_POINT('Ctrl Pts',(-0.416710479687932,-0.794772684000857,
12.011584301463));
#62927=CARTESIAN_POINT('Ctrl Pts',(-0.390689544578296,-0.6363098000952,
11.9476998442955));
#62928=CARTESIAN_POINT('Ctrl Pts',(-0.355023316128746,-0.319434907277161,
11.8808422569316));
#62929=CARTESIAN_POINT('Ctrl Pts',(-0.328684331227664,-0.158333333333334,
11.8437431505064));
#62930=CARTESIAN_POINT('Ctrl Pts',(-0.298123930914947,0.158333333333335,
11.8458196167914));
#62931=CARTESIAN_POINT('Ctrl Pts',(-0.292918278048133,0.31943490727717,
11.88511715802));
#62932=CARTESIAN_POINT('Ctrl Pts',(-0.268339992311274,0.636309800095211,
11.9559559166057));
#62933=CARTESIAN_POINT('Ctrl Pts',(-0.262312628808647,0.794772684000846,
12.0223207693886));
#62934=CARTESIAN_POINT('Ctrl Pts',(-0.221903226169962,1.06847604194778,
12.0878687935682));
#62935=CARTESIAN_POINT('Ctrl Pts',(-0.199111159992541,1.18514270861703,
12.1107901379001));
#62936=CARTESIAN_POINT('Ctrl Pts',(-0.171018760724269,1.30000000000775,
12.12825951569));
#62937=CARTESIAN_POINT('Ctrl Pts',(-0.41534867580558,-1.30000000000267,
12.129153621754));
#62938=CARTESIAN_POINT('Ctrl Pts',(-0.429894776557093,-1.1851427086136,
12.1144297574352));
#62939=CARTESIAN_POINT('Ctrl Pts',(-0.436318583411802,-1.06847604194604,
12.0939970326791));
#62940=CARTESIAN_POINT('Ctrl Pts',(-0.432394738563412,-0.79477268400086,
12.0336047412763));
#62941=CARTESIAN_POINT('Ctrl Pts',(-0.404819836431124,-0.636309800095204,
11.9695374830877));
#62942=CARTESIAN_POINT('Ctrl Pts',(-0.368076777863108,-0.319434907277163,
11.903074296202));
#62943=CARTESIAN_POINT('Ctrl Pts',(-0.340280761436702,-0.158333333333334,
11.8652579327567));
#62944=CARTESIAN_POINT('Ctrl Pts',(-0.309565682256709,0.158333333333336,
11.8673854677189));
#62945=CARTESIAN_POINT('Ctrl Pts',(-0.305791634384979,0.31943490727717,
11.9074118717088));
#62946=CARTESIAN_POINT('Ctrl Pts',(-0.281711831347124,0.636309800095213,
11.9780406361937));
#62947=CARTESIAN_POINT('Ctrl Pts',(-0.276359383968067,0.79477268400085,
12.0448633886902));
#62948=CARTESIAN_POINT('Ctrl Pts',(-0.234015232478537,1.06847604194778,
12.1074058962497));
#62949=CARTESIAN_POINT('Ctrl Pts',(-0.20977922135297,1.18514270861703,12.1282961333338));
#62950=CARTESIAN_POINT('Ctrl Pts',(-0.179636413276436,1.30000000000776,
12.1430042734075));
#62951=CARTESIAN_POINT('Ctrl Pts',(-0.424476296754516,-1.30000000000268,
12.1421342910495));
#62952=CARTESIAN_POINT('Ctrl Pts',(-0.440665495397502,-1.1851427086136,
12.1299569524641));
#62953=CARTESIAN_POINT('Ctrl Pts',(-0.448240048525547,-1.06847604194604,
12.111403173544));
#62954=CARTESIAN_POINT('Ctrl Pts',(-0.445837227042061,-0.794772684000862,
12.0538093797921));
#62955=CARTESIAN_POINT('Ctrl Pts',(-0.417803733610112,-0.636309800095205,
11.9893325638084));
#62956=CARTESIAN_POINT('Ctrl Pts',(-0.380369801383896,-0.319434907277163,
11.9231559217953));
#62957=CARTESIAN_POINT('Ctrl Pts',(-0.351121243067043,-0.158333333333334,
11.8847308731295));
#62958=CARTESIAN_POINT('Ctrl Pts',(-0.319894625120041,0.158333333333336,
11.8869907516665));
#62959=CARTESIAN_POINT('Ctrl Pts',(-0.316797578034367,0.319434907277171,
11.9278148839816));
#62960=CARTESIAN_POINT('Ctrl Pts',(-0.292904434770781,0.636309800095215,
11.9983111850674));
#62961=CARTESIAN_POINT('Ctrl Pts',(-0.288335254952031,0.794772684000851,
12.0655099666861));
#62962=CARTESIAN_POINT('Ctrl Pts',(-0.24449397264818,1.06847604194779,12.1252672188602));
#62963=CARTESIAN_POINT('Ctrl Pts',(-0.219109615872915,1.18514270861704,
12.1442784384785));
#62964=CARTESIAN_POINT('Ctrl Pts',(-0.187318168952349,1.30000000000776,
12.1564341774732));
#62965=CARTESIAN_POINT('Ctrl Pts',(-0.431265933106911,-1.30000000000268,
12.151098725605));
#62966=CARTESIAN_POINT('Ctrl Pts',(-0.449096337968213,-1.1851427086136,
12.1405654754374));
#62967=CARTESIAN_POINT('Ctrl Pts',(-0.457725079498785,-1.06847604194604,
12.1232568494019));
#62968=CARTESIAN_POINT('Ctrl Pts',(-0.456401515527817,-0.794772684000862,
12.0676179870174));
#62969=CARTESIAN_POINT('Ctrl Pts',(-0.426858480497729,-0.636309800095204,
12.0031829395948));
#62970=CARTESIAN_POINT('Ctrl Pts',(-0.38885614998925,-0.319434907277163,
11.9372443662456));
#62971=CARTESIAN_POINT('Ctrl Pts',(-0.359466334516699,-0.158333333333334,
11.8981754071227));
#62972=CARTESIAN_POINT('Ctrl Pts',(-0.327998948950437,0.158333333333336,
11.9005014725806));
#62973=CARTESIAN_POINT('Ctrl Pts',(-0.325009471962342,0.319434907277171,
11.9419757366776));
#62974=CARTESIAN_POINT('Ctrl Pts',(-0.30077249248368,0.636309800095215,
12.0124909326934));
#62975=CARTESIAN_POINT('Ctrl Pts',(-0.29612913799147,0.794772684000851,
12.0800924747781));
#62976=CARTESIAN_POINT('Ctrl Pts',(-0.251185627287519,1.06847604194779,
12.1379133478779));
#62977=CARTESIAN_POINT('Ctrl Pts',(-0.225129779128529,1.18514270861704,
12.1555798121165));
#62978=CARTESIAN_POINT('Ctrl Pts',(-0.192472463273335,1.30000000000776,
12.165884227103));
#62979=CARTESIAN_POINT('Ctrl Pts',(-0.434502644741001,-1.30000000000268,
12.1556249880944));
#62980=CARTESIAN_POINT('Ctrl Pts',(-0.452983313731051,-1.1851427086136,
12.1459617586608));
#62981=CARTESIAN_POINT('Ctrl Pts',(-0.462066356594455,-1.06847604194604,
12.1292962264643));
#62982=CARTESIAN_POINT('Ctrl Pts',(-0.461339606324205,-0.794772684000861,
12.0746187929737));
#62983=CARTESIAN_POINT('Ctrl Pts',(-0.431579525689312,-0.636309800095204,
12.010054557842));
#62984=CARTESIAN_POINT('Ctrl Pts',(-0.393350922373833,-0.319434907277162,
11.9442162999102));
#62985=CARTESIAN_POINT('Ctrl Pts',(-0.363480148592282,-0.158333333333334,
11.9049342616725));
#62986=CARTESIAN_POINT('Ctrl Pts',(-0.331875952022848,0.158333333333336,
11.9072995234825));
#62987=CARTESIAN_POINT('Ctrl Pts',(-0.329176263507277,0.319434907277171,
11.9490383339075));
#62988=CARTESIAN_POINT('Ctrl Pts',(-0.304997607702349,0.636309800095214,
12.0195080597917));
#62989=CARTESIAN_POINT('Ctrl Pts',(-0.30059676410946,0.79477268400085,12.0872480075864));
#62990=CARTESIAN_POINT('Ctrl Pts',(-0.255019206798925,1.06847604194779,
12.1441198649727));
#62991=CARTESIAN_POINT('Ctrl Pts',(-0.228496396831367,1.18514270861704,
12.1611441312157));
#62992=CARTESIAN_POINT('Ctrl Pts',(-0.195179612641289,1.30000000000776,
12.1705749439487));
#62993=CARTESIAN_POINT('Ctrl Pts',(-0.436112354604507,-1.30000000000268,
12.1578902342253));
#62994=CARTESIAN_POINT('Ctrl Pts',(-0.45490880513389,-1.1851427086136,12.1486645668709));
#62995=CARTESIAN_POINT('Ctrl Pts',(-0.46421605190099,-1.06847604194604,
12.132321362437));
#62996=CARTESIAN_POINT('Ctrl Pts',(-0.463795694841754,-0.794772684000861,
12.0781223562358));
#62997=CARTESIAN_POINT('Ctrl Pts',(-0.433965073693174,-0.636309800095204,
12.0134829209234));
#62998=CARTESIAN_POINT('Ctrl Pts',(-0.395631299550042,-0.319434907277163,
11.9476926447746));
#62999=CARTESIAN_POINT('Ctrl Pts',(-0.36549533649341,-0.158333333333334,
11.9083108979011));
#63000=CARTESIAN_POINT('Ctrl Pts',(-0.333823806975698,0.158333333333336,
11.9106958437498));
#63001=CARTESIAN_POINT('Ctrl Pts',(-0.331283738001294,0.319434907277172,
11.9525632339281));
#63002=CARTESIAN_POINT('Ctrl Pts',(-0.30715098623571,0.636309800095215,
12.0230063595812));
#63003=CARTESIAN_POINT('Ctrl Pts',(-0.302895353172418,0.794772684000851,
12.0908100086447));
#63004=CARTESIAN_POINT('Ctrl Pts',(-0.256990821320803,1.06847604194779,
12.1472098458578));
#63005=CARTESIAN_POINT('Ctrl Pts',(-0.230221724585517,1.18514270861704,
12.1639160882153));
#63006=CARTESIAN_POINT('Ctrl Pts',(-0.196553902023217,1.30000000000776,
12.1729151732204));
#63007=CARTESIAN_POINT('Ctrl Pts',(-0.437025956946848,-1.30000000000268,
12.1591863243717));
#63008=CARTESIAN_POINT('Ctrl Pts',(-0.455997165561016,-1.1851427086136,
12.1502122862774));
#63009=CARTESIAN_POINT('Ctrl Pts',(-0.465430235748078,-1.06847604194604,
12.1340539182948));
#63010=CARTESIAN_POINT('Ctrl Pts',(-0.465187507094752,-0.794772684000861,
12.0801276165228));
#63011=CARTESIAN_POINT('Ctrl Pts',(-0.435335675416772,-0.636309800095204,
12.0154399566702));
#63012=CARTESIAN_POINT('Ctrl Pts',(-0.396944310444561,-0.319434907277162,
11.9496763405232));
#63013=CARTESIAN_POINT('Ctrl Pts',(-0.36664263106812,-0.158333333333334,
11.9102413513394));
#63014=CARTESIAN_POINT('Ctrl Pts',(-0.334932443849119,0.158333333333336,
11.9126376435904));
#63015=CARTESIAN_POINT('Ctrl Pts',(-0.332492095751833,0.319434907277172,
11.954576306481));
#63016=CARTESIAN_POINT('Ctrl Pts',(-0.308393876872099,0.636309800095215,
12.0250022691105));
#63017=CARTESIAN_POINT('Ctrl Pts',(-0.304231219116808,0.79477268400085,
12.092840125262));
#63018=CARTESIAN_POINT('Ctrl Pts',(-0.25813661299071,1.06847604194779,12.1489710072257));
#63019=CARTESIAN_POINT('Ctrl Pts',(-0.231221908265117,1.18514270861704,
12.1654966449073));
#63020=CARTESIAN_POINT('Ctrl Pts',(-0.19734514583268,1.30000000000776,12.1742509413223));
#63021=CARTESIAN_POINT('Ctrl Pts',(-0.444794417751137,-1.30000000000268,
12.1702019182047));
#63022=CARTESIAN_POINT('Ctrl Pts',(-0.46522928698987,-1.1851427086136,12.1633718897678));
#63023=CARTESIAN_POINT('Ctrl Pts',(-0.475723958401096,-1.06847604194604,
12.1487861342615));
#63024=CARTESIAN_POINT('Ctrl Pts',(-0.477004903301544,-0.794772684000861,
12.0971728401138));
#63025=CARTESIAN_POINT('Ctrl Pts',(-0.447039629478921,-0.636309800095204,
12.0320561788573));
#63026=CARTESIAN_POINT('Ctrl Pts',(-0.40819871638579,-0.319434907277163,
11.9665085734518));
#63027=CARTESIAN_POINT('Ctrl Pts',(-0.376500881569381,-0.158333333333334,
11.9266191611378));
#63028=CARTESIAN_POINT('Ctrl Pts',(-0.344452505120339,0.158333333333336,
11.9291155053812));
#63029=CARTESIAN_POINT('Ctrl Pts',(-0.342808124805955,0.319434907277171,
11.9716738798763));
#63030=CARTESIAN_POINT('Ctrl Pts',(-0.319004258867317,0.636309800095214,
12.041954748453));
#63031=CARTESIAN_POINT('Ctrl Pts',(-0.315687596474742,0.79477268400085,
12.1100686400152));
#63032=CARTESIAN_POINT('Ctrl Pts',(-0.267989187339546,1.06847604194779,
12.1639125004961));
#63033=CARTESIAN_POINT('Ctrl Pts',(-0.239833641747303,1.18514270861704,
12.1789051904198));
#63034=CARTESIAN_POINT('Ctrl Pts',(-0.204169424477457,1.30000000000776,
12.1855835581765));
#63035=CARTESIAN_POINT('Ctrl Pts',(-0.460499827063455,-1.30000000000266,
12.1909882378324));
#63036=CARTESIAN_POINT('Ctrl Pts',(-0.484682298294522,-1.18514270861358,
12.1879667082804));
#63037=CARTESIAN_POINT('Ctrl Pts',(-0.497681648841877,-1.06847604194603,
12.1762391098647));
#63038=CARTESIAN_POINT('Ctrl Pts',(-0.501877503162414,-0.794772684000854,
12.1290332507087));
#63039=CARTESIAN_POINT('Ctrl Pts',(-0.46943057625706,-0.636309800095199,
12.0637512065799));
#63040=CARTESIAN_POINT('Ctrl Pts',(-0.429385621777131,-0.319434907277161,
11.9987349348556));
#63041=CARTESIAN_POINT('Ctrl Pts',(-0.396387340540971,-0.158333333333332,
11.9576216144592));
#63042=CARTESIAN_POINT('Ctrl Pts',(-0.363836289262359,0.158333333333334,
11.9602735413555));
#63043=CARTESIAN_POINT('Ctrl Pts',(-0.363378403513772,0.319434907277162,
12.0041009411279));
#63044=CARTESIAN_POINT('Ctrl Pts',(-0.338962865815543,0.636309800095203,
12.0743923968692));
#63045=CARTESIAN_POINT('Ctrl Pts',(-0.334838814901272,0.794772684000845,
12.1436020444614));
#63046=CARTESIAN_POINT('Ctrl Pts',(-0.284554381841157,1.06847604194778,
12.1929991429715));
#63047=CARTESIAN_POINT('Ctrl Pts',(-0.254927105241685,1.18514270861703,
12.2048737624313));
#63048=CARTESIAN_POINT('Ctrl Pts',(-0.217438819892861,1.30000000000775,
12.2072408277485));
#63049=CARTESIAN_POINT('Ctrl Pts',(-0.475851704605936,-1.30000000000266,
12.211451484628));
#63050=CARTESIAN_POINT('Ctrl Pts',(-0.503305113781325,-1.18514270861358,
12.2122832473818));
#63051=CARTESIAN_POINT('Ctrl Pts',(-0.518587456938927,-1.06847604194603,
12.2034113791443));
#63052=CARTESIAN_POINT('Ctrl Pts',(-0.525775129540728,-0.794772684000851,
12.1604982599099));
#63053=CARTESIAN_POINT('Ctrl Pts',(-0.492061752143856,-0.636309800095197,
12.0947271819335));
#63054=CARTESIAN_POINT('Ctrl Pts',(-0.451176432830116,-0.319434907277159,
12.0301447643824));
#63055=CARTESIAN_POINT('Ctrl Pts',(-0.41653030333555,-0.158333333333332,
11.9879440782691));
#63056=CARTESIAN_POINT('Ctrl Pts',(-0.38323276776461,0.158333333333334,
11.9908254839733));
#63057=CARTESIAN_POINT('Ctrl Pts',(-0.383201773569385,0.319434907277167,
12.0360862285271));
#63058=CARTESIAN_POINT('Ctrl Pts',(-0.359072532091704,0.636309800095206,
12.1061739592688));
#63059=CARTESIAN_POINT('Ctrl Pts',(-0.357294751063013,0.79477268400084,
12.1757050010453));
#63060=CARTESIAN_POINT('Ctrl Pts',(-0.303818465806733,1.06847604194777,
12.2208554698369));
#63061=CARTESIAN_POINT('Ctrl Pts',(-0.271622642081085,1.18514270861702,
12.2299142783607));
#63062=CARTESIAN_POINT('Ctrl Pts',(-0.230378897025869,1.30000000000775,
12.2284879304579));
#63063=CARTESIAN_POINT('Ctrl Pts',(-0.483946399133603,-1.30000000000266,
12.2215611275524));
#63064=CARTESIAN_POINT('Ctrl Pts',(-0.512888765856687,-1.18514270861358,
12.2243528792004));
#63065=CARTESIAN_POINT('Ctrl Pts',(-0.529237518131319,-1.06847604194603,
12.2169241430307));
#63066=CARTESIAN_POINT('Ctrl Pts',(-0.537912637722502,-0.794772684000851,
12.1761509049044));
#63067=CARTESIAN_POINT('Ctrl Pts',(-0.503949232631998,-0.636309800095197,
12.1100262039146));
#63068=CARTESIAN_POINT('Ctrl Pts',(-0.462594679683807,-0.319434907277159,
12.0456777212677));
#63069=CARTESIAN_POINT('Ctrl Pts',(-0.426715573255357,-0.158333333333332,
12.0030579137075));
#63070=CARTESIAN_POINT('Ctrl Pts',(-0.392969830593602,0.158333333333334,
12.0060803363164));
#63071=CARTESIAN_POINT('Ctrl Pts',(-0.393579787166861,0.319434907277167,
12.0519414879776));
#63072=CARTESIAN_POINT('Ctrl Pts',(-0.369299762851234,0.636309800095206,
12.1220005005405));
#63073=CARTESIAN_POINT('Ctrl Pts',(-0.367561330758702,0.79477268400084,
12.1919695316153));
#63074=CARTESIAN_POINT('Ctrl Pts',(-0.312674005334915,1.06847604194777,
12.2349707346061));
#63075=CARTESIAN_POINT('Ctrl Pts',(-0.279563873100157,1.18514270861702,
12.2425436138999));
#63076=CARTESIAN_POINT('Ctrl Pts',(-0.237102298031049,1.30000000000775,
12.239075745064));
#63077=CARTESIAN_POINT('Origin',(0.,-0.926917420765551,7.2));
#63078=CARTESIAN_POINT('Origin',(0.,-0.653834841531101,7.2));
#63079=CARTESIAN_POINT('Origin',(0.,-1.2,7.2));
#63080=CARTESIAN_POINT('Origin',(0.,0.,7.2));
#63081=CARTESIAN_POINT('Origin',(0.,-1.25,7.2));
#63082=CARTESIAN_POINT('',(0.,0.,0.));
#63083=CARTESIAN_POINT('Origin',(0.4,0.,8.78));
#63084=CARTESIAN_POINT('',(0.4,-5.55,8.78));
#63085=CARTESIAN_POINT('',(0.4,-5.55,8.48937969582276));
#63086=CARTESIAN_POINT('',(0.4,-5.55,9.075));
#63087=CARTESIAN_POINT('',(0.4,5.55,8.78));
#63088=CARTESIAN_POINT('',(0.4,0.,8.78));
#63089=CARTESIAN_POINT('',(0.4,5.55,8.48937969582276));
#63090=CARTESIAN_POINT('',(0.4,5.55,8.665));
#63091=CARTESIAN_POINT('',(0.4,5.45,8.3842719282327));
#63092=CARTESIAN_POINT('Ctrl Pts',(0.4,5.45,8.3842719282327));
#63093=CARTESIAN_POINT('Ctrl Pts',(0.4,5.49787545330696,8.43480450880564));
#63094=CARTESIAN_POINT('Ctrl Pts',(0.4,5.55,8.48937969582276));
#63095=CARTESIAN_POINT('',(0.4,-5.45,8.3842719282327));
#63096=CARTESIAN_POINT('',(0.4,0.,8.3842719282327));
#63097=CARTESIAN_POINT('Ctrl Pts',(0.4,-5.55,8.48937969582276));
#63098=CARTESIAN_POINT('Ctrl Pts',(0.4,-5.49787545330696,8.43480450880564));
#63099=CARTESIAN_POINT('Ctrl Pts',(0.4,-5.45,8.3842719282327));
#63100=CARTESIAN_POINT('Origin',(-0.4,0.,8.78));
#63101=CARTESIAN_POINT('',(-0.4,-5.55,8.78));
#63102=CARTESIAN_POINT('',(-0.2,-5.55,8.78));
#63103=CARTESIAN_POINT('',(-0.4,5.55,8.78));
#63104=CARTESIAN_POINT('',(-0.4,0.,8.78));
#63105=CARTESIAN_POINT('',(-0.2,5.55,8.78));
#63106=CARTESIAN_POINT('Origin',(-0.4,0.,7.2));
#63107=CARTESIAN_POINT('',(-0.4,-5.55,8.48937969582276));
#63108=CARTESIAN_POINT('',(-0.4,-5.55,8.285));
#63109=CARTESIAN_POINT('',(-0.4,-5.45,8.3842719282327));
#63110=CARTESIAN_POINT('Ctrl Pts',(-0.4,-5.45,8.3842719282327));
#63111=CARTESIAN_POINT('Ctrl Pts',(-0.4,-5.49787545330696,8.43480450880564));
#63112=CARTESIAN_POINT('Ctrl Pts',(-0.4,-5.55,8.48937969582276));
#63113=CARTESIAN_POINT('',(-0.4,5.45,8.3842719282327));
#63114=CARTESIAN_POINT('',(-0.4,0.,8.3842719282327));
#63115=CARTESIAN_POINT('',(-0.4,5.55,8.48937969582276));
#63116=CARTESIAN_POINT('Ctrl Pts',(-0.4,5.55,8.48937969582276));
#63117=CARTESIAN_POINT('Ctrl Pts',(-0.4,5.49787545330696,8.43480450880564));
#63118=CARTESIAN_POINT('Ctrl Pts',(-0.4,5.45,8.3842719282327));
#63119=CARTESIAN_POINT('',(-0.4,5.55,7.875));
#63120=CARTESIAN_POINT('Origin',(0.,-5.55,9.37));
#63121=CARTESIAN_POINT('',(-2.65748355414976E-16,-5.55,5.03));
#63122=CARTESIAN_POINT('Origin',(0.,-5.55,7.2));
#63123=CARTESIAN_POINT('Origin',(0.,-5.55,7.2));
#63124=CARTESIAN_POINT('Origin',(0.,-5.5,7.2));
#63125=CARTESIAN_POINT('Origin',(0.,-5.45,7.2));
#63126=CARTESIAN_POINT('Origin',(0.,-5.51,7.2));
#63127=CARTESIAN_POINT('',(-2.75545529808154E-16,-5.47,4.95));
#63128=CARTESIAN_POINT('Origin',(0.,-5.47,7.2));
#63129=CARTESIAN_POINT('',(-2.70646942611565E-16,-5.51,4.99));
#63130=CARTESIAN_POINT('Origin',(0.,-4.335,7.2));
#63131=CARTESIAN_POINT('',(-2.75545529808154E-16,-3.2,4.95));
#63132=CARTESIAN_POINT('Origin',(0.,-3.2,7.2));
#63133=CARTESIAN_POINT('',(-2.75545529808154E-16,-4.335,4.95));
#63134=CARTESIAN_POINT('Origin',(0.,-3.2,9.75));
#63135=CARTESIAN_POINT('',(-3.12284933782575E-16,-3.2,4.65));
#63136=CARTESIAN_POINT('Origin',(0.,-3.2,7.2));
#63137=CARTESIAN_POINT('Origin',(0.,-3.175,7.2));
#63138=CARTESIAN_POINT('',(-3.18408167778312E-16,-3.15,4.6));
#63139=CARTESIAN_POINT('Origin',(0.,-3.15,7.2));
#63140=CARTESIAN_POINT('',(-3.15346550780443E-16,-3.175,4.625));
#63141=CARTESIAN_POINT('Origin',(0.,-2.225,7.2));
#63142=CARTESIAN_POINT('',(-3.18408167778312E-16,-1.3,4.6));
#63143=CARTESIAN_POINT('Origin',(0.,-1.3,7.2));
#63144=CARTESIAN_POINT('',(-3.18408167778312E-16,-2.225,4.6));
#63145=CARTESIAN_POINT('Origin',(0.,-1.3,10.5));
#63146=CARTESIAN_POINT('',(-4.04133443718627E-16,-1.3,3.9));
#63147=CARTESIAN_POINT('Origin',(0.,-1.3,7.2));
#63148=CARTESIAN_POINT('Origin',(0.,0.,7.2));
#63149=CARTESIAN_POINT('',(-4.04133443718627E-16,1.3,3.9));
#63150=CARTESIAN_POINT('Origin',(0.,1.3,7.2));
#63151=CARTESIAN_POINT('',(-4.04133443718627E-16,0.,3.9));
#63152=CARTESIAN_POINT('Origin',(0.,1.3,9.8));
#63153=CARTESIAN_POINT('',(-3.18408167778312E-16,1.3,4.6));
#63154=CARTESIAN_POINT('Origin',(0.,1.3,7.2));
#63155=CARTESIAN_POINT('Origin',(0.,2.225,7.2));
#63156=CARTESIAN_POINT('',(-3.18408167778312E-16,3.15,4.6));
#63157=CARTESIAN_POINT('Origin',(0.,3.15,7.2));
#63158=CARTESIAN_POINT('',(-3.18408167778312E-16,2.225,4.6));
#63159=CARTESIAN_POINT('Origin',(0.,3.175,7.2));
#63160=CARTESIAN_POINT('',(-3.12284933782575E-16,3.2,4.65));
#63161=CARTESIAN_POINT('',(3.15346550780443E-16,3.175,4.625));
#63162=CARTESIAN_POINT('Origin',(0.,3.2,7.2));
#63163=CARTESIAN_POINT('Origin',(0.,3.2,9.45));
#63164=CARTESIAN_POINT('',(-2.75545529808154E-16,3.2,4.95));
#63165=CARTESIAN_POINT('Origin',(0.,3.2,7.2));
#63166=CARTESIAN_POINT('Origin',(0.,4.335,7.2));
#63167=CARTESIAN_POINT('',(-2.75545529808154E-16,5.47,4.95));
#63168=CARTESIAN_POINT('Origin',(0.,5.47,7.2));
#63169=CARTESIAN_POINT('',(-2.75545529808154E-16,4.335,4.95));
#63170=CARTESIAN_POINT('Origin',(0.,5.51,7.2));
#63171=CARTESIAN_POINT('',(-2.65748355414976E-16,5.55,5.03));
#63172=CARTESIAN_POINT('',(2.70646942611565E-16,5.51,4.99));
#63173=CARTESIAN_POINT('Origin',(0.,5.55,7.2));
#63174=CARTESIAN_POINT('Origin',(0.,5.55,8.55));
#63175=CARTESIAN_POINT('Origin',(0.,5.55,7.2));
#63176=CARTESIAN_POINT('Origin',(0.,5.5,7.2));
#63177=CARTESIAN_POINT('Origin',(0.,5.45,7.2));
#63178=CARTESIAN_POINT('Origin',(0.,0.,7.2));
#63179=CARTESIAN_POINT('',(0.,0.,0.));
#63180=CARTESIAN_POINT('Origin',(2.55,0.,0.));
#63181=CARTESIAN_POINT('',(-2.55,-3.12284933782575E-16,-1.17961196366423E-16));
#63182=CARTESIAN_POINT('Origin',(0.,0.,0.));
#63183=CARTESIAN_POINT('',(-1.6,-1.95943487863577E-16,-2.77555756156289E-17));
#63184=CARTESIAN_POINT('Origin',(0.,0.,0.));
#63185=CARTESIAN_POINT('Origin',(0.,0.,0.025));
#63186=CARTESIAN_POINT('',(-2.6,-3.18408167778312E-16,0.0499999999999999));
#63187=CARTESIAN_POINT('Origin',(0.,0.,0.05));
#63188=CARTESIAN_POINT('',(-2.575,-3.15346550780443E-16,0.025));
#63189=CARTESIAN_POINT('Origin',(0.,0.,0.355));
#63190=CARTESIAN_POINT('',(-2.6,-3.18408167778312E-16,0.66));
#63191=CARTESIAN_POINT('Origin',(0.,0.,0.66));
#63192=CARTESIAN_POINT('',(-2.6,-3.18408167778312E-16,0.355));
#63193=CARTESIAN_POINT('Origin',(0.,0.,0.68));
#63194=CARTESIAN_POINT('',(-2.56,-3.13509580581722E-16,0.7));
#63195=CARTESIAN_POINT('',(-2.58,3.15958874180017E-16,0.68));
#63196=CARTESIAN_POINT('Origin',(0.,0.,0.7));
#63197=CARTESIAN_POINT('Origin',(1.7,0.,0.7));
#63198=CARTESIAN_POINT('',(-1.7,-2.0818995585505E-16,0.7));
#63199=CARTESIAN_POINT('Origin',(0.,0.,0.7));
#63200=CARTESIAN_POINT('Origin',(0.,0.,0.625));
#63201=CARTESIAN_POINT('',(-1.7,-2.0818995585505E-16,0.55));
#63202=CARTESIAN_POINT('Origin',(0.,0.,0.55));
#63203=CARTESIAN_POINT('',(-1.7,-2.0818995585505E-16,0.625));
#63204=CARTESIAN_POINT('Origin',(1.4,0.,0.55));
#63205=CARTESIAN_POINT('',(-1.4,-1.71450551880629E-16,0.55));
#63206=CARTESIAN_POINT('Origin',(0.,0.,0.55));
#63207=CARTESIAN_POINT('Origin',(0.,0.,0.475));
#63208=CARTESIAN_POINT('',(-1.25,-1.53080849893419E-16,0.4));
#63209=CARTESIAN_POINT('Origin',(0.,0.,0.4));
#63210=CARTESIAN_POINT('',(-1.325,-1.62265700887024E-16,0.475));
#63211=CARTESIAN_POINT('Origin',(0.,0.,0.35));
#63212=CARTESIAN_POINT('',(-1.25,-1.53080849893419E-16,0.3));
#63213=CARTESIAN_POINT('Origin',(0.,0.,0.3));
#63214=CARTESIAN_POINT('',(-1.25,-1.53080849893419E-16,0.35));
#63215=CARTESIAN_POINT('Origin',(0.,0.,0.25));
#63216=CARTESIAN_POINT('',(-1.45,-1.77573785876366E-16,0.2));
#63217=CARTESIAN_POINT('',(-1.35,1.65327317884893E-16,0.25));
#63218=CARTESIAN_POINT('Origin',(0.,0.,0.2));
#63219=CARTESIAN_POINT('Origin',(0.,0.,0.1));
#63220=CARTESIAN_POINT('',(-1.525,1.86758636869971E-16,0.1));
#63221=CARTESIAN_POINT('',(0.,0.,0.));
#63222=CARTESIAN_POINT('Origin',(0.,0.,0.62));
#63223=CARTESIAN_POINT('',(-1.,-1.22464679914735E-16,0.6));
#63224=CARTESIAN_POINT('Origin',(0.,0.,0.6));
#63225=CARTESIAN_POINT('',(-1.,-1.22464679914735E-16,0.59));
#63226=CARTESIAN_POINT('',(-1.,-1.22464679914735E-16,0.62));
#63227=CARTESIAN_POINT('Origin',(0.,0.,0.59));
#63228=CARTESIAN_POINT('Origin',(1.12,0.,0.59));
#63229=CARTESIAN_POINT('',(-1.12,-1.37160441504504E-16,0.59));
#63230=CARTESIAN_POINT('Origin',(0.,0.,0.59));
#63231=CARTESIAN_POINT('Origin',(0.,0.,0.62));
#63232=CARTESIAN_POINT('',(-1.12,1.37160441504504E-16,0.6));
#63233=CARTESIAN_POINT('',(-1.12,-1.37160441504504E-16,0.62));
#63234=CARTESIAN_POINT('Origin',(0.,0.,0.6));
#63235=CARTESIAN_POINT('Origin',(0.,0.,0.6));
#63236=CARTESIAN_POINT('',(-2.56,-3.13509580581722E-16,0.6));
#63237=CARTESIAN_POINT('Origin',(0.,0.,0.6));
#63238=CARTESIAN_POINT('Origin',(0.,0.,0.26));
#63239=CARTESIAN_POINT('',(-2.52,-3.08610993385133E-16,0.));
#63240=CARTESIAN_POINT('Origin',(0.,0.,0.));
#63241=CARTESIAN_POINT('',(-2.52,-3.08610993385133E-16,0.52));
#63242=CARTESIAN_POINT('',(-2.52,-3.08610993385133E-16,0.26));
#63243=CARTESIAN_POINT('Origin',(0.,0.,0.52));
#63244=CARTESIAN_POINT('Origin',(2.6,0.,0.));
#63245=CARTESIAN_POINT('',(-2.6,-3.18408167778312E-16,0.));
#63246=CARTESIAN_POINT('Origin',(0.,0.,0.));
#63247=CARTESIAN_POINT('Origin',(0.,0.,0.28));
#63248=CARTESIAN_POINT('',(-2.6,-3.18408167778312E-16,0.56));
#63249=CARTESIAN_POINT('Origin',(0.,0.,0.56));
#63250=CARTESIAN_POINT('',(-2.6,-3.18408167778312E-16,0.28));
#63251=CARTESIAN_POINT('Origin',(0.,0.,0.58));
#63252=CARTESIAN_POINT('',(-2.58,3.15958874180017E-16,0.58));
#63253=CARTESIAN_POINT('Origin',(0.,0.,0.6));
#63254=CARTESIAN_POINT('Origin',(2.52,0.,0.52));
#63255=CARTESIAN_POINT('',(0.,0.,0.));
#63256=CARTESIAN_POINT('Origin',(0.,0.,-0.920658989190502));
#63257=CARTESIAN_POINT('',(-0.00922985932074701,0.43710256198851,-0.675612757771509));
#63258=CARTESIAN_POINT('',(-0.00922985932074692,0.43710256198851,-0.695322262895625));
#63259=CARTESIAN_POINT('',(-0.00922985932074702,0.43710256198851,-0.920658989190502));
#63260=CARTESIAN_POINT('',(-0.253836275241718,-0.35596486536091,-0.73578659827137));
#63261=CARTESIAN_POINT('Ctrl Pts',(-0.253836275241718,-0.35596486536091,
-0.73578659827137));
#63262=CARTESIAN_POINT('Ctrl Pts',(-0.23609314335769,-0.368617379546539,
-0.734988690310258));
#63263=CARTESIAN_POINT('Ctrl Pts',(-0.217340678724491,-0.379983145122343,
-0.734190782349146));
#63264=CARTESIAN_POINT('Ctrl Pts',(-0.197795612701048,-0.389898365726528,
-0.733392874388034));
#63265=CARTESIAN_POINT('Ctrl Pts',(-0.178285302760331,-0.399795954554633,
-0.732596385309573));
#63266=CARTESIAN_POINT('Ctrl Pts',(-0.157985814170068,-0.408247724716953,
-0.731799896231113));
#63267=CARTESIAN_POINT('Ctrl Pts',(-0.13714195136672,-0.415133623277287,
-0.731003407152653));
#63268=CARTESIAN_POINT('Ctrl Pts',(-0.115855204867377,-0.422165831196564,
-0.730189994530307));
#63269=CARTESIAN_POINT('Ctrl Pts',(-0.0940013712333268,-0.427564424236376,
-0.729376581907962));
#63270=CARTESIAN_POINT('Ctrl Pts',(-0.0718621610207865,-0.431253602667181,
-0.728563169285616));
#63271=CARTESIAN_POINT('Ctrl Pts',(-0.0501929304701205,-0.434864465800608,
-0.727767024098989));
#63272=CARTESIAN_POINT('Ctrl Pts',(-0.0282511020507067,-0.436837780034281,
-0.726970878912363));
#63273=CARTESIAN_POINT('Ctrl Pts',(-0.00630957656052663,-0.437154468401762,
-0.726174733725736));
#63274=CARTESIAN_POINT('Ctrl Pts',(0.0163457770492143,-0.43748145965643,
-0.725352687385531));
#63275=CARTESIAN_POINT('Ctrl Pts',(0.0389999615898507,-0.436042033330408,
-0.724530641045326));
#63276=CARTESIAN_POINT('Ctrl Pts',(0.061355526823022,-0.432873352527352,
-0.723708594705121));
#63277=CARTESIAN_POINT('Ctrl Pts',(0.0837110920561935,-0.429704671724297,
-0.722886548364916));
#63278=CARTESIAN_POINT('Ctrl Pts',(0.10576721131509,-0.424806998274031,
-0.722064502024711));
#63279=CARTESIAN_POINT('Ctrl Pts',(0.127242103991421,-0.41827417679297,
-0.721242455684506));
#63280=CARTESIAN_POINT('Ctrl Pts',(0.148546925876914,-0.411793092106706,
-0.720426919554772));
#63281=CARTESIAN_POINT('Ctrl Pts',(0.169414363182626,-0.403662168059158,
-0.719611383425039));
#63282=CARTESIAN_POINT('Ctrl Pts',(0.189574309742103,-0.393961192360117,
-0.718795847295306));
#63283=CARTESIAN_POINT('Ctrl Pts',(0.209698695316446,-0.38427732862373,
-0.717981749724356));
#63284=CARTESIAN_POINT('Ctrl Pts',(0.229117409464745,-0.373029168092783,
-0.717167652153405));
#63285=CARTESIAN_POINT('Ctrl Pts',(0.247578773794493,-0.360345099545443,
-0.716353554582455));
#63286=CARTESIAN_POINT('Ctrl Pts',(0.266020771766867,-0.347674336851346,
-0.715540311016886));
#63287=CARTESIAN_POINT('Ctrl Pts',(0.283506814660605,-0.333571035915543,
-0.714727067451318));
#63288=CARTESIAN_POINT('Ctrl Pts',(0.299812669558214,-0.318207798729662,
-0.713913823885749));
#63289=CARTESIAN_POINT('Ctrl Pts',(0.316126157215975,-0.302837370022371,
-0.713100199641393));
#63290=CARTESIAN_POINT('Ctrl Pts',(0.33125782248679,-0.286206301894547,
-0.712286575397036));
#63291=CARTESIAN_POINT('Ctrl Pts',(0.345018414943263,-0.268525852293663,
-0.71147295115268));
#63292=CARTESIAN_POINT('Ctrl Pts',(0.358782327805654,-0.250841136432466,
-0.710659130582274));
#63293=CARTESIAN_POINT('Ctrl Pts',(0.371174096206649,-0.232107115550857,
-0.709845310011867));
#63294=CARTESIAN_POINT('Ctrl Pts',(0.3820467077514,-0.21256564420507,-0.709031489441461));
#63295=CARTESIAN_POINT('Ctrl Pts',(0.392942211323343,-0.192983028752224,
-0.708215955391037));
#63296=CARTESIAN_POINT('Ctrl Pts',(0.402311867170909,-0.172590213434354,
-0.707400421340613));
#63297=CARTESIAN_POINT('Ctrl Pts',(0.410055556767824,-0.151651839302494,
-0.706584887290189));
#63298=CARTESIAN_POINT('Ctrl Pts',(0.413741612735028,-0.141685011739698,
-0.706196686792816));
#63299=CARTESIAN_POINT('Ctrl Pts',(0.417059976950239,-0.131594818230247,
-0.705808486295443));
#63300=CARTESIAN_POINT('Ctrl Pts',(0.420003875212337,-0.121410810089629,
-0.70542028579807));
#63301=CARTESIAN_POINT('Ctrl Pts',(0.42618277750005,-0.100035753754183,
-0.704605497810254));
#63302=CARTESIAN_POINT('Ctrl Pts',(0.430742949574895,-0.0781284216398137,
-0.703790709822439));
#63303=CARTESIAN_POINT('Ctrl Pts',(0.433604087624001,-0.0559583344619706,
-0.702975921834623));
#63304=CARTESIAN_POINT('Ctrl Pts',(0.436460231986423,-0.0338269418410514,
-0.702162555936848));
#63305=CARTESIAN_POINT('Ctrl Pts',(0.437623085351083,-0.0114343978593403,
-0.701349190039073));
#63306=CARTESIAN_POINT('Ctrl Pts',(0.437063135300412,0.010938727593921,
-0.700535824141298));
#63307=CARTESIAN_POINT('Ctrl Pts',(0.436503760081961,0.0332888852961096,
-0.699723293226793));
#63308=CARTESIAN_POINT('Ctrl Pts',(0.434225084143321,0.0556189534824457,
-0.698910762312289));
#63309=CARTESIAN_POINT('Ctrl Pts',(0.430249624151161,0.0776472853214116,
-0.698098231397785));
#63310=CARTESIAN_POINT('Ctrl Pts',(0.426272118272563,0.0996869535756465,
-0.697285282331424));
#63311=CARTESIAN_POINT('Ctrl Pts',(0.420596193643256,0.121423869876721,
-0.696472333265063));
#63312=CARTESIAN_POINT('Ctrl Pts',(0.413295843054221,0.142584662969411,
-0.695659384198702));
#63313=CARTESIAN_POINT('Ctrl Pts',(0.405993543982359,0.163751103933591,
-0.69484621815409));
#63314=CARTESIAN_POINT('Ctrl Pts',(0.397066218842823,0.1843404517338,-0.694033052109479));
#63315=CARTESIAN_POINT('Ctrl Pts',(0.386636516520684,0.204098123687483,
-0.693219886064868));
#63316=CARTESIAN_POINT('Ctrl Pts',(0.376184292898921,0.223898459222176,
-0.692404964116246));
#63317=CARTESIAN_POINT('Ctrl Pts',(0.364223591037297,0.242862925444445,
-0.691590042167625));
#63318=CARTESIAN_POINT('Ctrl Pts',(0.350921694804399,0.260763885757994,
-0.690775120219003));
#63319=CARTESIAN_POINT('Ctrl Pts',(0.344517650348058,0.269382096549297,
-0.690382785449881));
#63320=CARTESIAN_POINT('Ctrl Pts',(0.337803352917797,0.277754285510053,
-0.689990450680759));
#63321=CARTESIAN_POINT('Ctrl Pts',(0.330800617403977,0.285857991886089,
-0.689598115911637));
#63322=CARTESIAN_POINT('Ctrl Pts',(0.316290891250969,0.302648938810849,
-0.688785195011078));
#63323=CARTESIAN_POINT('Ctrl Pts',(0.300456998910622,0.318381474757695,
-0.68797227411052));
#63324=CARTESIAN_POINT('Ctrl Pts',(0.283479247888115,0.33284133760215,-0.687159353209962));
#63325=CARTESIAN_POINT('Ctrl Pts',(0.266533027410502,0.347274346044395,
-0.686347942040517));
#63326=CARTESIAN_POINT('Ctrl Pts',(0.248447668655544,0.36043887033087,-0.685536530871072));
#63327=CARTESIAN_POINT('Ctrl Pts',(0.229440609456682,0.372157018920974,
-0.684725119701626));
#63328=CARTESIAN_POINT('Ctrl Pts',(0.210445091826676,0.383868051953779,
-0.683914201241642));
#63329=CARTESIAN_POINT('Ctrl Pts',(0.190529570065128,0.394134040634215,
-0.683103282781657));
#63330=CARTESIAN_POINT('Ctrl Pts',(0.169941306080854,0.402819801508731,
-0.682292364321672));
#63331=CARTESIAN_POINT('Ctrl Pts',(0.14936201662218,0.411501776217333,-0.681481799345035));
#63332=CARTESIAN_POINT('Ctrl Pts',(0.128111228261427,0.418604612966437,
-0.680671234368398));
#63333=CARTESIAN_POINT('Ctrl Pts',(0.106456800455306,0.42404102353053,-0.679860669391761));
#63334=CARTESIAN_POINT('Ctrl Pts',(0.0847714872781761,0.42948518796181,
-0.679048948319002));
#63335=CARTESIAN_POINT('Ctrl Pts',(0.0626820859558504,0.433258018369173,
-0.678237227246242));
#63336=CARTESIAN_POINT('Ctrl Pts',(0.0404683503361822,0.435323043981212,
-0.677425506173482));
#63337=CARTESIAN_POINT('Ctrl Pts',(0.0239323278453153,0.43686025998799,
-0.676821256706158));
#63338=CARTESIAN_POINT('Ctrl Pts',(0.00732768865856914,0.437452191233075,
-0.676217007238833));
#63339=CARTESIAN_POINT('Ctrl Pts',(-0.00922985932074701,0.43710256198851,
-0.675612757771509));
#63340=CARTESIAN_POINT('',(0.253835875722688,-0.355965150255044,-0.7358));
#63341=CARTESIAN_POINT('Origin',(0.,0.,-0.7358));
#63342=CARTESIAN_POINT('Ctrl Pts',(0.253835875722687,-0.355965150255045,
-0.7358));
#63343=CARTESIAN_POINT('Ctrl Pts',(0.274914182552133,-0.340934379773804,
-0.734857571584884));
#63344=CARTESIAN_POINT('Ctrl Pts',(0.294627512029226,-0.3240474366386,-0.733915143169768));
#63345=CARTESIAN_POINT('Ctrl Pts',(0.312694699597163,-0.305558283873699,
-0.732972714754652));
#63346=CARTESIAN_POINT('Ctrl Pts',(0.330744485056812,-0.287086939649135,
-0.732031194075799));
#63347=CARTESIAN_POINT('Ctrl Pts',(0.347151135572132,-0.26701667183279,
-0.731089673396946));
#63348=CARTESIAN_POINT('Ctrl Pts',(0.361671991886951,-0.245636337467659,
-0.730148152718094));
#63349=CARTESIAN_POINT('Ctrl Pts',(0.373286559043319,-0.228535188339421,
-0.729395073497657));
#63350=CARTESIAN_POINT('Ctrl Pts',(0.383695334702161,-0.210596615772003,
-0.72864199427722));
#63351=CARTESIAN_POINT('Ctrl Pts',(0.392792712220016,-0.191983658749498,
-0.727888915056783));
#63352=CARTESIAN_POINT('Ctrl Pts',(0.402665549171227,-0.171784135370104,
-0.72707164344855));
#63353=CARTESIAN_POINT('Ctrl Pts',(0.410982336608168,-0.150808835824164,
-0.726254371840317));
#63354=CARTESIAN_POINT('Ctrl Pts',(0.417635754569863,-0.129322142361088,
-0.725437100232084));
#63355=CARTESIAN_POINT('Ctrl Pts',(0.424288360024729,-0.107838072825331,
-0.724619928428007));
#63356=CARTESIAN_POINT('Ctrl Pts',(0.429277804386253,-0.0858434103456964,
-0.72380275662393));
#63357=CARTESIAN_POINT('Ctrl Pts',(0.432546731640961,-0.0636173321251568,
-0.722985584819852));
#63358=CARTESIAN_POINT('Ctrl Pts',(0.435819780852261,-0.0413632279124443,
-0.722167382602296));
#63359=CARTESIAN_POINT('Ctrl Pts',(0.437367913469084,-0.018877827071933,
-0.72134918038474));
#63360=CARTESIAN_POINT('Ctrl Pts',(0.437185553804755,0.00355408841049547,
-0.720530978167183));
#63361=CARTESIAN_POINT('Ctrl Pts',(0.437144458872794,0.00860914290346409,
-0.720346595482644));
#63362=CARTESIAN_POINT('Ctrl Pts',(0.43701569380716,0.0136614873623527,
-0.720162212798104));
#63363=CARTESIAN_POINT('Ctrl Pts',(0.436799559222696,0.0187078877177015,
-0.719977830113565));
#63364=CARTESIAN_POINT('Ctrl Pts',(0.435833468478675,0.041264577041772,
-0.719153665830307));
#63365=CARTESIAN_POINT('Ctrl Pts',(0.433113968332593,0.0637884349248981,
-0.718329501547049));
#63366=CARTESIAN_POINT('Ctrl Pts',(0.428659807839924,0.0859919132397912,
-0.717505337263792));
#63367=CARTESIAN_POINT('Ctrl Pts',(0.424211114992684,0.108168135970398,
-0.716682184672431));
#63368=CARTESIAN_POINT('Ctrl Pts',(0.418032095436736,0.130024080115696,
-0.71585903208107));
#63369=CARTESIAN_POINT('Ctrl Pts',(0.410192983832772,0.151279727704565,
-0.715035879489709));
#63370=CARTESIAN_POINT('Ctrl Pts',(0.402358358148486,0.172523211781469,
-0.714213197946165));
#63371=CARTESIAN_POINT('Ctrl Pts',(0.392865756473906,0.193166431332994,
-0.713390516402621));
#63372=CARTESIAN_POINT('Ctrl Pts',(0.381834617237782,0.212946390152255,
-0.712567834859076));
#63373=CARTESIAN_POINT('Ctrl Pts',(0.370792523466517,0.232745991571373,
-0.711744336346978));
#63374=CARTESIAN_POINT('Ctrl Pts',(0.358209175667509,0.251680014588842,
-0.710920837834879));
#63375=CARTESIAN_POINT('Ctrl Pts',(0.344249629493799,0.26951072816009,-0.71009733932278));
#63376=CARTESIAN_POINT('Ctrl Pts',(0.330282425057853,0.287351223731319,
-0.709273389036141));
#63377=CARTESIAN_POINT('Ctrl Pts',(0.314937976448905,0.304086685582767,
-0.708449438749502));
#63378=CARTESIAN_POINT('Ctrl Pts',(0.298420829956647,0.319513455503811,
-0.707625488462862));
#63379=CARTESIAN_POINT('Ctrl Pts',(0.281864984291512,0.334976369878523,
-0.706799607685711));
#63380=CARTESIAN_POINT('Ctrl Pts',(0.264131494784984,0.349124036809449,
-0.70597372690856));
#63381=CARTESIAN_POINT('Ctrl Pts',(0.245458067100449,0.361793003380817,
-0.705147846131409));
#63382=CARTESIAN_POINT('Ctrl Pts',(0.237980187223299,0.366866362797672,
-0.70481711749665));
#63383=CARTESIAN_POINT('Ctrl Pts',(0.230351882816712,0.371703090974448,
-0.70448638886189));
#63384=CARTESIAN_POINT('Ctrl Pts',(0.222589516841263,0.376294760782519,
-0.704155660227131));
#63385=CARTESIAN_POINT('Ctrl Pts',(0.203657935596137,0.387493352848033,
-0.703349048423612));
#63386=CARTESIAN_POINT('Ctrl Pts',(0.183815030407178,0.3972974216862,-0.702542436620092));
#63387=CARTESIAN_POINT('Ctrl Pts',(0.1632943380843,0.405559858898302,-0.701735824816572));
#63388=CARTESIAN_POINT('Ctrl Pts',(0.142813510323876,0.413806245070843,
-0.700930779979026));
#63389=CARTESIAN_POINT('Ctrl Pts',(0.121658149897246,0.420516609879964,
-0.70012573514148));
#63390=CARTESIAN_POINT('Ctrl Pts',(0.100086214106577,0.425589696475152,
-0.699320690303934));
#63391=CARTESIAN_POINT('Ctrl Pts',(0.0785346546054127,0.430657991164684,
-0.698516405890804));
#63392=CARTESIAN_POINT('Ctrl Pts',(0.0565679968628827,0.434091867394654,
-0.697712121477673));
#63393=CARTESIAN_POINT('Ctrl Pts',(0.0344593539473663,0.435839870738704,
-0.696907837064543));
#63394=CARTESIAN_POINT('Ctrl Pts',(0.0199309555581142,0.436988547709296,
-0.69637931234157));
#63395=CARTESIAN_POINT('Ctrl Pts',(0.00534155190377906,0.437410251961992,
-0.695850787618598));
#63396=CARTESIAN_POINT('Ctrl Pts',(-0.00922985932074692,0.43710256198851,
-0.695322262895625));
#63397=CARTESIAN_POINT('Origin',(0.,0.,-0.920658989190502));
#63398=CARTESIAN_POINT('',(-0.0092298593207472,0.43710256198851,-0.57559571443739));
#63399=CARTESIAN_POINT('',(-0.00922985932074836,0.43710256198851,-0.595330810493319));
#63400=CARTESIAN_POINT('',(-0.00922985932074702,0.43710256198851,-0.920658989190502));
#63401=CARTESIAN_POINT('',(-0.437199981330587,0.000127767500978009,-0.650941010811321));
#63402=CARTESIAN_POINT('Ctrl Pts',(-0.437199981330602,0.000127767450639139,
-0.650941010809498));
#63403=CARTESIAN_POINT('Ctrl Pts',(-0.437206707008506,-0.0228864371799604,
-0.650107475569003));
#63404=CARTESIAN_POINT('Ctrl Pts',(-0.435391893778402,-0.0458841048713647,
-0.649273940328508));
#63405=CARTESIAN_POINT('Ctrl Pts',(-0.431789350475714,-0.0685696493775565,
-0.648440405088013));
#63406=CARTESIAN_POINT('Ctrl Pts',(-0.428183198960036,-0.0912779151307892,
-0.647606035000459));
#63407=CARTESIAN_POINT('Ctrl Pts',(-0.422785904167437,-0.113672790754695,
-0.646771664912904));
#63408=CARTESIAN_POINT('Ctrl Pts',(-0.415682208654229,-0.135470075693277,
-0.64593729482535));
#63409=CARTESIAN_POINT('Ctrl Pts',(-0.408557536979716,-0.157331724787675,
-0.645100460966437));
#63410=CARTESIAN_POINT('Ctrl Pts',(-0.399716654157924,-0.178591646120379,
-0.644263627107525));
#63411=CARTESIAN_POINT('Ctrl Pts',(-0.389292783329051,-0.198984845774547,
-0.643426793248612));
#63412=CARTESIAN_POINT('Ctrl Pts',(-0.383915028511627,-0.209505853707524,
-0.642995064249852));
#63413=CARTESIAN_POINT('Ctrl Pts',(-0.378116695543855,-0.219796585034483,
-0.642563335251093));
#63414=CARTESIAN_POINT('Ctrl Pts',(-0.371920583669806,-0.229823670327299,
-0.642131606252333));
#63415=CARTESIAN_POINT('Ctrl Pts',(-0.360242219712324,-0.248722611124779,
-0.64131788815282));
#63416=CARTESIAN_POINT('Ctrl Pts',(-0.347086172853866,-0.266783349012772,
-0.640504170053308));
#63417=CARTESIAN_POINT('Ctrl Pts',(-0.332597230391415,-0.283765611616278,
-0.639690451953796));
#63418=CARTESIAN_POINT('Ctrl Pts',(-0.318134186922218,-0.300717518415296,
-0.63887818837587));
#63419=CARTESIAN_POINT('Ctrl Pts',(-0.302343394083982,-0.316594201814829,
-0.638065924797943));
#63420=CARTESIAN_POINT('Ctrl Pts',(-0.28541202189861,-0.331185473346503,
-0.637253661220017));
#63421=CARTESIAN_POINT('Ctrl Pts',(-0.268498651128944,-0.345761231454833,
-0.636442261239805));
#63422=CARTESIAN_POINT('Ctrl Pts',(-0.250447629667843,-0.35905380475023,
-0.635630861259594));
#63423=CARTESIAN_POINT('Ctrl Pts',(-0.231481955973139,-0.370890744099728,
-0.634819461279382));
#63424=CARTESIAN_POINT('Ctrl Pts',(-0.212507201857559,-0.382733350761281,
-0.634007672815564));
#63425=CARTESIAN_POINT('Ctrl Pts',(-0.192617517962916,-0.393118536251465,
-0.633195884351746));
#63426=CARTESIAN_POINT('Ctrl Pts',(-0.172064415822184,-0.401917500001892,
-0.632384095887928));
#63427=CARTESIAN_POINT('Ctrl Pts',(-0.151506287174457,-0.410718615644161,
-0.63157210889153));
#63428=CARTESIAN_POINT('Ctrl Pts',(-0.130285087484214,-0.417932484591169,
-0.630760121895132));
#63429=CARTESIAN_POINT('Ctrl Pts',(-0.108671147300701,-0.423478950768925,
-0.629948134898734));
#63430=CARTESIAN_POINT('Ctrl Pts',(-0.0870107368529557,-0.429037341924109,
-0.629134402119293));
#63431=CARTESIAN_POINT('Ctrl Pts',(-0.0649566050649743,-0.432921042028621,
-0.628320669339852));
#63432=CARTESIAN_POINT('Ctrl Pts',(-0.0427891354973138,-0.435101057092938,
-0.62750693656041));
#63433=CARTESIAN_POINT('Ctrl Pts',(-0.0319151525429824,-0.43617043700467,
-0.627107769828907));
#63434=CARTESIAN_POINT('Ctrl Pts',(-0.0210139566724641,-0.436830661251386,
-0.626708603097403));
#63435=CARTESIAN_POINT('Ctrl Pts',(-0.010118573979996,-0.437082891978869,
-0.6263094363659));
#63436=CARTESIAN_POINT('Ctrl Pts',(0.0120971323446054,-0.4375971909187,
-0.625495534630464));
#63437=CARTESIAN_POINT('Ctrl Pts',(0.0344155954638143,-0.436414896660635,
-0.624681632895029));
#63438=CARTESIAN_POINT('Ctrl Pts',(0.0565563354687885,-0.433526493905899,
-0.623867731159593));
#63439=CARTESIAN_POINT('Ctrl Pts',(0.0786576030299037,-0.4306432405868,
-0.623055280445693));
#63440=CARTESIAN_POINT('Ctrl Pts',(0.100581067681182,-0.426059952861661,
-0.622242829731793));
#63441=CARTESIAN_POINT('Ctrl Pts',(0.122048384613809,-0.419819046510708,
-0.621430379017893));
#63442=CARTESIAN_POINT('Ctrl Pts',(0.143492958568617,-0.413584751921958,
-0.620618789033288));
#63443=CARTESIAN_POINT('Ctrl Pts',(0.16448165293897,-0.405696497122655,
-0.619807199048683));
#63444=CARTESIAN_POINT('Ctrl Pts',(0.184748243534716,-0.396247304736369,
-0.618995609064078));
#63445=CARTESIAN_POINT('Ctrl Pts',(0.205024587099967,-0.386793565078811,
-0.618183628514896));
#63446=CARTESIAN_POINT('Ctrl Pts',(0.224577476372314,-0.375777672622639,
-0.617371647965715));
#63447=CARTESIAN_POINT('Ctrl Pts',(0.243161744224629,-0.363340344781083,
-0.616559667416533));
#63448=CARTESIAN_POINT('Ctrl Pts',(0.261750589070784,-0.350899953834034,
-0.615747486890145));
#63449=CARTESIAN_POINT('Ctrl Pts',(0.279369760744317,-0.337037854520489,
-0.614935306363757));
#63450=CARTESIAN_POINT('Ctrl Pts',(0.295804617117614,-0.321937056723673,
-0.614123125837369));
#63451=CARTESIAN_POINT('Ctrl Pts',(0.312274784376428,-0.30680381431462,
-0.613309200311637));
#63452=CARTESIAN_POINT('Ctrl Pts',(0.327555062329663,-0.290427079341062,
-0.612495274785905));
#63453=CARTESIAN_POINT('Ctrl Pts',(0.341468220043877,-0.273026179514101,
-0.611681349260173));
#63454=CARTESIAN_POINT('Ctrl Pts',(0.348272062052594,-0.264516754431455,
-0.611283321666603));
#63455=CARTESIAN_POINT('Ctrl Pts',(0.354749601097303,-0.255762890076055,
-0.610885294073034));
#63456=CARTESIAN_POINT('Ctrl Pts',(0.360883951753957,-0.246792652577924,
-0.610487266479464));
#63457=CARTESIAN_POINT('Ctrl Pts',(0.373427041870483,-0.228450939884396,
-0.609673407563592));
#63458=CARTESIAN_POINT('Ctrl Pts',(0.384604105896927,-0.209098124000313,
-0.608859548647719));
#63459=CARTESIAN_POINT('Ctrl Pts',(0.394254240566668,-0.188964107161121,
-0.608045689731846));
#63460=CARTESIAN_POINT('Ctrl Pts',(0.403887166674859,-0.168865994221708,
-0.607233282126419));
#63461=CARTESIAN_POINT('Ctrl Pts',(0.411998212385938,-0.147990059600682,
-0.606420874520992));
#63462=CARTESIAN_POINT('Ctrl Pts',(0.418471169710053,-0.126592733288683,
-0.605608466915565));
#63463=CARTESIAN_POINT('Ctrl Pts',(0.424937267919239,-0.105218080804583,
-0.604796920183593));
#63464=CARTESIAN_POINT('Ctrl Pts',(0.429768491061065,-0.0833238068245529,
-0.603985373451621));
#63465=CARTESIAN_POINT('Ctrl Pts',(0.432897661814507,-0.061183775590699,
-0.603173826719649));
#63466=CARTESIAN_POINT('Ctrl Pts',(0.436028339652899,-0.0390330811778364,
-0.602361889126978));
#63467=CARTESIAN_POINT('Ctrl Pts',(0.437455208865004,-0.0166370989373022,
-0.601549951534307));
#63468=CARTESIAN_POINT('Ctrl Pts',(0.437162554732755,0.0057219524230085,
-0.600738013941636));
#63469=CARTESIAN_POINT('Ctrl Pts',(0.43686982848041,0.028086513826494,-0.599925876259475));
#63470=CARTESIAN_POINT('Ctrl Pts',(0.434856776168184,0.0504134114387393,
-0.599113738577314));
#63471=CARTESIAN_POINT('Ctrl Pts',(0.431159779498312,0.072422955911557,
-0.598301600895153));
#63472=CARTESIAN_POINT('Ctrl Pts',(0.427454835427866,0.0944798141046644,
-0.597487717367903));
#63473=CARTESIAN_POINT('Ctrl Pts',(0.422058885916212,0.11621725989166,-0.596673833840652));
#63474=CARTESIAN_POINT('Ctrl Pts',(0.415059155108187,0.137367164056328,
-0.595859950313402));
#63475=CARTESIAN_POINT('Ctrl Pts',(0.411633745076104,0.147717146918554,
-0.595461665739945));
#63476=CARTESIAN_POINT('Ctrl Pts',(0.40782501804362,0.157926696114878,-0.595063381166487));
#63477=CARTESIAN_POINT('Ctrl Pts',(0.403647325398977,0.16796629631641,-0.59466509659303));
#63478=CARTESIAN_POINT('Ctrl Pts',(0.395110849896879,0.188480682716078,
-0.593851263026661));
#63479=CARTESIAN_POINT('Ctrl Pts',(0.384982079822358,0.208401318098998,
-0.593037429460293));
#63480=CARTESIAN_POINT('Ctrl Pts',(0.373365985328546,0.227467977965348,
-0.592223595893924));
#63481=CARTESIAN_POINT('Ctrl Pts',(0.361770617011629,0.246500617880724,
-0.591411214421326));
#63482=CARTESIAN_POINT('Ctrl Pts',(0.348693512632148,0.264681673595572,
-0.590598832948729));
#63483=CARTESIAN_POINT('Ctrl Pts',(0.334286251145077,0.281773920538027,
-0.589786451476131));
#63484=CARTESIAN_POINT('Ctrl Pts',(0.319894269219178,0.298848040369167,
-0.588974931571321));
#63485=CARTESIAN_POINT('Ctrl Pts',(0.304175368342171,0.314835081589508,
-0.588163411666511));
#63486=CARTESIAN_POINT('Ctrl Pts',(0.287322477414341,0.329529412909508,
-0.587351891761701));
#63487=CARTESIAN_POINT('Ctrl Pts',(0.270461484632071,0.34423080837856,-0.586539981727021));
#63488=CARTESIAN_POINT('Ctrl Pts',(0.252465939804094,0.357637768087622,
-0.585728071692341));
#63489=CARTESIAN_POINT('Ctrl Pts',(0.233563836147,0.369583244268862,-0.584916161657661));
#63490=CARTESIAN_POINT('Ctrl Pts',(0.214657084771853,0.381531657647269,
-0.584104051987587));
#63491=CARTESIAN_POINT('Ctrl Pts',(0.194843952325113,0.392017516588651,
-0.583291942317512));
#63492=CARTESIAN_POINT('Ctrl Pts',(0.174378718070393,0.400918823060388,
-0.582479832647437));
#63493=CARTESIAN_POINT('Ctrl Pts',(0.153869495105059,0.409839262320423,
-0.581665977399627));
#63494=CARTESIAN_POINT('Ctrl Pts',(0.132706047056115,0.417168108345919,
-0.580852122151817));
#63495=CARTESIAN_POINT('Ctrl Pts',(0.111160684757035,0.422832286095027,
-0.580038266904007));
#63496=CARTESIAN_POINT('Ctrl Pts',(0.100612520042174,0.42560535062012,-0.579639820171537));
#63497=CARTESIAN_POINT('Ctrl Pts',(0.0899729993074902,0.427980190290949,
-0.579241373439067));
#63498=CARTESIAN_POINT('Ctrl Pts',(0.0792747311758675,0.429952738096868,
-0.578842926706597));
#63499=CARTESIAN_POINT('Ctrl Pts',(0.0574208879911633,0.433982152007093,
-0.578029001284114));
#63500=CARTESIAN_POINT('Ctrl Pts',(0.0351965747481254,0.436352639203792,
-0.577215075861632));
#63501=CARTESIAN_POINT('Ctrl Pts',(0.0128772540754298,0.437010316042398,
-0.576401150439149));
#63502=CARTESIAN_POINT('Ctrl Pts',(0.00551507898827925,0.437227255084029,
-0.576132671771896));
#63503=CARTESIAN_POINT('Ctrl Pts',(-0.00185733207176875,0.437258240301254,
-0.575864193104643));
#63504=CARTESIAN_POINT('Ctrl Pts',(-0.0092298593207472,0.43710256198851,
-0.57559571443739));
#63505=CARTESIAN_POINT('Ctrl Pts',(-0.00922985932074701,0.43710256198851,
-0.675612757771509));
#63506=CARTESIAN_POINT('Ctrl Pts',(-0.0260072006138585,0.436748291587515,
-0.675000487189407));
#63507=CARTESIAN_POINT('Ctrl Pts',(-0.0427360189425501,0.435427294772284,
-0.674388216607305));
#63508=CARTESIAN_POINT('Ctrl Pts',(-0.0592984893725335,0.433159934848706,
-0.673775946025203));
#63509=CARTESIAN_POINT('Ctrl Pts',(-0.0813219580013637,0.430144978211756,
-0.672961796830837));
#63510=CARTESIAN_POINT('Ctrl Pts',(-0.103177495193642,0.425437540065905,
-0.672147647636471));
#63511=CARTESIAN_POINT('Ctrl Pts',(-0.12458652359729,0.419072831543566,
-0.671333498442105));
#63512=CARTESIAN_POINT('Ctrl Pts',(-0.14595746363186,0.412719446345326,
-0.670520797684091));
#63513=CARTESIAN_POINT('Ctrl Pts',(-0.166882778259061,0.404714791959317,
-0.669708096926077));
#63514=CARTESIAN_POINT('Ctrl Pts',(-0.187094255225339,0.395145010928489,
-0.668895396168062));
#63515=CARTESIAN_POINT('Ctrl Pts',(-0.20728436950885,0.385585344754514,
-0.668083554400636));
#63516=CARTESIAN_POINT('Ctrl Pts',(-0.226761489326628,0.374464115613459,
-0.66727171263321));
#63517=CARTESIAN_POINT('Ctrl Pts',(-0.245277409181012,0.361915504704414,
-0.666459870865784));
#63518=CARTESIAN_POINT('Ctrl Pts',(-0.263802228239114,0.349360862626204,
-0.665647638907358));
#63519=CARTESIAN_POINT('Ctrl Pts',(-0.281364322202039,0.33537785401944,
-0.664835406948932));
#63520=CARTESIAN_POINT('Ctrl Pts',(-0.297743847746859,0.320144406680634,
-0.664023174990506));
#63521=CARTESIAN_POINT('Ctrl Pts',(-0.314127408365929,0.304907206602414,
-0.663210742939821));
#63522=CARTESIAN_POINT('Ctrl Pts',(-0.329327318663427,0.288419464249492,
-0.662398310889137));
#63523=CARTESIAN_POINT('Ctrl Pts',(-0.343160581830907,0.270896022631329,
-0.661585878838452));
#63524=CARTESIAN_POINT('Ctrl Pts',(-0.357023492965347,0.253335024117745,
-0.660771705553013));
#63525=CARTESIAN_POINT('Ctrl Pts',(-0.369513504192179,0.234734485300197,
-0.659957532267574));
#63526=CARTESIAN_POINT('Ctrl Pts',(-0.380490314154753,0.215339176264835,
-0.659143358982135));
#63527=CARTESIAN_POINT('Ctrl Pts',(-0.385836360686416,0.205893059865574,
-0.658746831367679));
#63528=CARTESIAN_POINT('Ctrl Pts',(-0.390824175469108,0.196258797900248,
-0.658350303753223));
#63529=CARTESIAN_POINT('Ctrl Pts',(-0.395441669118987,0.18646642143933,
-0.657953776138767));
#63530=CARTESIAN_POINT('Ctrl Pts',(-0.405679523518418,0.164754875732289,
-0.657074599622247));
#63531=CARTESIAN_POINT('Ctrl Pts',(-0.414145038150763,0.142156655082225,
-0.656195423105727));
#63532=CARTESIAN_POINT('Ctrl Pts',(-0.420702760698338,0.118966495875085,
-0.655316246589207));
#63533=CARTESIAN_POINT('Ctrl Pts',(-0.427225743179071,0.095899188416417,
-0.65444172758156));
#63534=CARTESIAN_POINT('Ctrl Pts',(-0.431860855423825,0.0722466731816281,
-0.653567208573913));
#63535=CARTESIAN_POINT('Ctrl Pts',(-0.434521538858847,0.0483205160127569,
-0.652692689566266));
#63536=CARTESIAN_POINT('Ctrl Pts',(-0.436298005924746,0.0323456617085848,
-0.652108796647951));
#63537=CARTESIAN_POINT('Ctrl Pts',(-0.437195269979398,0.016249258772824,
-0.651524903729636));
#63538=CARTESIAN_POINT('Ctrl Pts',(-0.437199981330587,0.0001277675009783,
-0.650941010811321));
#63539=CARTESIAN_POINT('',(-0.437199929076795,0.000249028602953033,-0.670658989188628));
#63540=CARTESIAN_POINT('Ctrl Pts',(-0.00922985932074692,0.43710256198851,
-0.695322262895625));
#63541=CARTESIAN_POINT('Ctrl Pts',(-0.0314070055045328,0.436634269287409,
-0.694517867915448));
#63542=CARTESIAN_POINT('Ctrl Pts',(-0.0535419143035678,0.43447398832484,
-0.693713472935271));
#63543=CARTESIAN_POINT('Ctrl Pts',(-0.0753586276524695,0.43065637953981,
-0.692909077955093));
#63544=CARTESIAN_POINT('Ctrl Pts',(-0.0972255992166277,0.426829976295182,
-0.692102829925127));
#63545=CARTESIAN_POINT('Ctrl Pts',(-0.118772195023262,0.421338777062112,
-0.691296581895161));
#63546=CARTESIAN_POINT('Ctrl Pts',(-0.139733376290776,0.414268540382178,
-0.690490333865195));
#63547=CARTESIAN_POINT('Ctrl Pts',(-0.158424889903764,0.407963865876317,
-0.689771386023696));
#63548=CARTESIAN_POINT('Ctrl Pts',(-0.176650775880943,0.400404465031996,
-0.689052438182196));
#63549=CARTESIAN_POINT('Ctrl Pts',(-0.194238339255865,0.391682661810711,
-0.688333490340697));
#63550=CARTESIAN_POINT('Ctrl Pts',(-0.214188832527874,0.381789064114617,
-0.687517950190592));
#63551=CARTESIAN_POINT('Ctrl Pts',(-0.233436790932398,0.370339900816165,
-0.686702410040488));
#63552=CARTESIAN_POINT('Ctrl Pts',(-0.251728887762749,0.357458259193615,
-0.685886869890383));
#63553=CARTESIAN_POINT('Ctrl Pts',(-0.269988720408491,0.344599338621977,
-0.685072768216042));
#63554=CARTESIAN_POINT('Ctrl Pts',(-0.28729543149376,0.330313317168977,
-0.684258666541701));
#63555=CARTESIAN_POINT('Ctrl Pts',(-0.303421857626618,0.31476819457247,
-0.68344456486736));
#63556=CARTESIAN_POINT('Ctrl Pts',(-0.319531368230129,0.299239377757251,
-0.682631317130566));
#63557=CARTESIAN_POINT('Ctrl Pts',(-0.334462523180116,0.282454554403131,
-0.681818069393772));
#63558=CARTESIAN_POINT('Ctrl Pts',(-0.34802249643644,0.264620826795905,
-0.681004821656977));
#63559=CARTESIAN_POINT('Ctrl Pts',(-0.361588817911958,0.246778750174284,
-0.680191193191195));
#63560=CARTESIAN_POINT('Ctrl Pts',(-0.373782229810875,0.227887344095649,
-0.679377564725412));
#63561=CARTESIAN_POINT('Ctrl Pts',(-0.384450764797267,0.208186093307877,
-0.67856393625963));
#63562=CARTESIAN_POINT('Ctrl Pts',(-0.395121874506069,0.188480087860543,
-0.677750111434418));
#63563=CARTESIAN_POINT('Ctrl Pts',(-0.404267062659073,0.167964489125426,
-0.676936286609206));
#63564=CARTESIAN_POINT('Ctrl Pts',(-0.411781053241527,0.146902022420722,
-0.676122461783995));
#63565=CARTESIAN_POINT('Ctrl Pts',(-0.419310864121166,0.125795209841608,
-0.675306923495018));
#63566=CARTESIAN_POINT('Ctrl Pts',(-0.425202425782493,0.104139916643362,
-0.674491385206042));
#63567=CARTESIAN_POINT('Ctrl Pts',(-0.429400462770177,0.0822136398218577,
-0.673675846917065));
#63568=CARTESIAN_POINT('Ctrl Pts',(-0.431398621626343,0.0717772896081326,
-0.673287671429464));
#63569=CARTESIAN_POINT('Ctrl Pts',(-0.433013865462819,0.0612796736223055,
-0.672899495941863));
#63570=CARTESIAN_POINT('Ctrl Pts',(-0.434244367921488,0.0507510485454944,
-0.672511320454263));
#63571=CARTESIAN_POINT('Ctrl Pts',(-0.436201642613934,0.0340038967914236,
-0.671893876699676));
#63572=CARTESIAN_POINT('Ctrl Pts',(-0.437190307036958,0.017141683576328,
-0.671276432945089));
#63573=CARTESIAN_POINT('Ctrl Pts',(-0.437199929076766,0.000249028654235785,
-0.670658989190502));
#63574=CARTESIAN_POINT('Ctrl Pts',(-0.437199929076795,0.000249028602953033,
-0.670658989188628));
#63575=CARTESIAN_POINT('Ctrl Pts',(-0.437212452159017,-0.0217367617606223,
-0.669855386142677));
#63576=CARTESIAN_POINT('Ctrl Pts',(-0.4355622610073,-0.0437851949110618,
-0.669051783096727));
#63577=CARTESIAN_POINT('Ctrl Pts',(-0.43224731193602,-0.0656208909120047,
-0.668248180050776));
#63578=CARTESIAN_POINT('Ctrl Pts',(-0.428937309510904,-0.0874240031659445,
-0.66744577616048));
#63579=CARTESIAN_POINT('Ctrl Pts',(-0.423967539716265,-0.109014281124924,
-0.666643372270185));
#63580=CARTESIAN_POINT('Ctrl Pts',(-0.417387828497506,-0.130120100761322,
-0.665840968379889));
#63581=CARTESIAN_POINT('Ctrl Pts',(-0.410807504084803,-0.151227887347385,
-0.665038489709837));
#63582=CARTESIAN_POINT('Ctrl Pts',(-0.402617116897674,-0.171850412733853,
-0.664236011039784));
#63583=CARTESIAN_POINT('Ctrl Pts',(-0.392916898071436,-0.191729369711374,
-0.663433532369732));
#63584=CARTESIAN_POINT('Ctrl Pts',(-0.383217301367585,-0.211607051754341,
-0.662631105166554));
#63585=CARTESIAN_POINT('Ctrl Pts',(-0.372008404123178,-0.230740607532142,
-0.661828677963376));
#63586=CARTESIAN_POINT('Ctrl Pts',(-0.359436913400565,-0.248895450511001,
-0.661026250760198));
#63587=CARTESIAN_POINT('Ctrl Pts',(-0.346837793311001,-0.26709019383499,
-0.660222059998812));
#63588=CARTESIAN_POINT('Ctrl Pts',(-0.33287054764678,-0.284301343360384,
-0.659417869237426));
#63589=CARTESIAN_POINT('Ctrl Pts',(-0.317723540675403,-0.300325809248366,
-0.65861367847604));
#63590=CARTESIAN_POINT('Ctrl Pts',(-0.305640653943371,-0.313108651867483,
-0.657972169173303));
#63591=CARTESIAN_POINT('Ctrl Pts',(-0.292807951576093,-0.32513693237376,
-0.657330659870565));
#63592=CARTESIAN_POINT('Ctrl Pts',(-0.279336207285159,-0.336325918269085,
-0.656689150567827));
#63593=CARTESIAN_POINT('Ctrl Pts',(-0.262265604125063,-0.350503944058331,
-0.655876267655708));
#63594=CARTESIAN_POINT('Ctrl Pts',(-0.244062841964013,-0.363420492111987,
-0.655063384743588));
#63595=CARTESIAN_POINT('Ctrl Pts',(-0.224940951780152,-0.374893862596121,
-0.654250501831469));
#63596=CARTESIAN_POINT('Ctrl Pts',(-0.205853665365587,-0.386346470390926,
-0.65343908994614));
#63597=CARTESIAN_POINT('Ctrl Pts',(-0.185851131125435,-0.396360670469547,
-0.652627678060812));
#63598=CARTESIAN_POINT('Ctrl Pts',(-0.165177059889714,-0.404796713037779,
-0.651816266175484));
#63599=CARTESIAN_POINT('Ctrl Pts',(-0.144525341083946,-0.413223634710158,
-0.651005731573934));
#63600=CARTESIAN_POINT('Ctrl Pts',(-0.123204176561203,-0.420075489728682,
-0.650195196972384));
#63601=CARTESIAN_POINT('Ctrl Pts',(-0.101479296768336,-0.425259676347763,
-0.649384662370834));
#63602=CARTESIAN_POINT('Ctrl Pts',(-0.0797442867957068,-0.43044628032164,
-0.648573749821912));
#63603=CARTESIAN_POINT('Ctrl Pts',(-0.0576058788370304,-0.43396347684704,
-0.64776283727299));
#63604=CARTESIAN_POINT('Ctrl Pts',(-0.0353429899867632,-0.435769105213754,
-0.646951924724069));
#63605=CARTESIAN_POINT('Ctrl Pts',(-0.0130748491733914,-0.437575159540172,
-0.6461408208755));
#63606=CARTESIAN_POINT('Ctrl Pts',(0.00931711353290146,-0.437668815182892,
-0.64532971702693));
#63607=CARTESIAN_POINT('Ctrl Pts',(0.0315515946571501,-0.43606001522106,
-0.644518613178361));
#63608=CARTESIAN_POINT('Ctrl Pts',(0.0538340014276071,-0.434447747547192,
-0.643705761023822));
#63609=CARTESIAN_POINT('Ctrl Pts',(0.0759575371609294,-0.431125798174385,
-0.642892908869284));
#63610=CARTESIAN_POINT('Ctrl Pts',(0.0976476401346384,-0.426155814668926,
-0.642080056714745));
#63611=CARTESIAN_POINT('Ctrl Pts',(0.10843752524531,-0.423683463519149,
-0.641675698036961));
#63612=CARTESIAN_POINT('Ctrl Pts',(0.119120351997259,-0.420804075188136,
-0.641271339359178));
#63613=CARTESIAN_POINT('Ctrl Pts',(0.129663922009771,-0.417529768195088,
-0.640866980681394));
#63614=CARTESIAN_POINT('Ctrl Pts',(0.150892702491631,-0.410937167747313,
-0.640052831242787));
#63615=CARTESIAN_POINT('Ctrl Pts',(0.171677745929381,-0.402702679274393,
-0.63923868180418));
#63616=CARTESIAN_POINT('Ctrl Pts',(0.191750046405751,-0.392906807911739,
-0.638424532365573));
#63617=CARTESIAN_POINT('Ctrl Pts',(0.211786636880584,-0.383128364077228,
-0.63761183135475));
#63618=CARTESIAN_POINT('Ctrl Pts',(0.231112341796989,-0.37179431180374,
-0.636799130343927));
#63619=CARTESIAN_POINT('Ctrl Pts',(0.249476747912302,-0.359033692362015,
-0.635986429333104));
#63620=CARTESIAN_POINT('Ctrl Pts',(0.267821743800063,-0.346286560235126,
-0.635174587305221));
#63621=CARTESIAN_POINT('Ctrl Pts',(0.285206858144772,-0.332116237615206,
-0.634362745277338));
#63622=CARTESIAN_POINT('Ctrl Pts',(0.301409305687097,-0.31669586426921,
-0.633550903249455));
#63623=CARTESIAN_POINT('Ctrl Pts',(0.317619540685347,-0.301268079359162,
-0.632738671022252));
#63624=CARTESIAN_POINT('Ctrl Pts',(0.332645442649692,-0.284589522910896,
-0.631926438795049));
#63625=CARTESIAN_POINT('Ctrl Pts',(0.346299390938616,-0.266871826605102,
-0.631114206567846));
#63626=CARTESIAN_POINT('Ctrl Pts',(0.359956702944012,-0.249149765458776,
-0.630301774243289));
#63627=CARTESIAN_POINT('Ctrl Pts',(0.3722409770448,-0.230388640070999,-0.629489341918732));
#63628=CARTESIAN_POINT('Ctrl Pts',(0.383007003794254,-0.21083044145604,
-0.628676909594176));
#63629=CARTESIAN_POINT('Ctrl Pts',(0.393796104733718,-0.191230324907786,
-0.627862736031345));
#63630=CARTESIAN_POINT('Ctrl Pts',(0.40306015939866,-0.170830373667132,
-0.627048562468515));
#63631=CARTESIAN_POINT('Ctrl Pts',(0.410700990773741,-0.149895083900265,
-0.626234388905685));
#63632=CARTESIAN_POINT('Ctrl Pts',(0.414422296306332,-0.139698993211769,
-0.625837862868776));
#63633=CARTESIAN_POINT('Ctrl Pts',(0.417759328118468,-0.12937617521928,
-0.625441336831868));
#63634=CARTESIAN_POINT('Ctrl Pts',(0.420705095541896,-0.118958238828105,
-0.625044810794959));
#63635=CARTESIAN_POINT('Ctrl Pts',(0.426751840268641,-0.0975734541923914,
-0.624230866115));
#63636=CARTESIAN_POINT('Ctrl Pts',(0.431181153288528,-0.0756655031661115,
-0.623416921435041));
#63637=CARTESIAN_POINT('Ctrl Pts',(0.433913816065184,-0.053503646864019,
-0.622602976755082));
#63638=CARTESIAN_POINT('Ctrl Pts',(0.436641616652187,-0.0313812228509463,
-0.621790480315805));
#63639=CARTESIAN_POINT('Ctrl Pts',(0.437678617813652,-0.00900648565784756,
-0.620977983876527));
#63640=CARTESIAN_POINT('Ctrl Pts',(0.436996422614475,0.0133404131176973,
-0.620165487437249));
#63641=CARTESIAN_POINT('Ctrl Pts',(0.436314947907121,0.0356637104990086,
-0.6193538491058));
#63642=CARTESIAN_POINT('Ctrl Pts',(0.43391787560429,0.0579585155943608,
-0.61854221077435));
#63643=CARTESIAN_POINT('Ctrl Pts',(0.429828839422716,0.0799437852526436,
-0.617730572442901));
#63644=CARTESIAN_POINT('Ctrl Pts',(0.425737818513836,0.101939726072318,
-0.61691854016024));
#63645=CARTESIAN_POINT('Ctrl Pts',(0.419953305726717,0.123625124627191,
-0.616106507877578));
#63646=CARTESIAN_POINT('Ctrl Pts',(0.412550375838212,0.144727424477014,
-0.615294475594917));
#63647=CARTESIAN_POINT('Ctrl Pts',(0.405145604587074,0.165834973192759,
-0.614482241331969));
#63648=CARTESIAN_POINT('Ctrl Pts',(0.396121881367468,0.186358470157252,
-0.613670007069021));
#63649=CARTESIAN_POINT('Ctrl Pts',(0.385602853630614,0.20604436238812,-0.612857772806072));
#63650=CARTESIAN_POINT('Ctrl Pts',(0.375061197452133,0.225772602740353,
-0.612043791271792));
#63651=CARTESIAN_POINT('Ctrl Pts',(0.363018194278841,0.244659033216597,
-0.611229809737512));
#63652=CARTESIAN_POINT('Ctrl Pts',(0.349641998044345,0.262477262260102,
-0.610415828203231));
#63653=CARTESIAN_POINT('Ctrl Pts',(0.343106097360962,0.271183636878155,
-0.610018099104996));
#63654=CARTESIAN_POINT('Ctrl Pts',(0.336252519568758,0.279635469956066,
-0.609620370006761));
#63655=CARTESIAN_POINT('Ctrl Pts',(0.329104171259901,0.287809458599494,
-0.609222640908525));
#63656=CARTESIAN_POINT('Ctrl Pts',(0.314478583628286,0.304533515967566,
-0.608408883446165));
#63657=CARTESIAN_POINT('Ctrl Pts',(0.298532990971369,0.320187864219064,
-0.607595125983804));
#63658=CARTESIAN_POINT('Ctrl Pts',(0.281449718780217,0.334559256034767,
-0.606781368521444));
#63659=CARTESIAN_POINT('Ctrl Pts',(0.264397829962196,0.348904246424167,
-0.605969105998331));
#63660=CARTESIAN_POINT('Ctrl Pts',(0.246212916914089,0.361970461363107,
-0.605156843475219));
#63661=CARTESIAN_POINT('Ctrl Pts',(0.227114142122697,0.37358132507912,-0.604344580952106));
#63662=CARTESIAN_POINT('Ctrl Pts',(0.208026932940381,0.385185157626264,
-0.60353281030928));
#63663=CARTESIAN_POINT('Ctrl Pts',(0.188027547854929,0.395334982137295,
-0.602721039666453));
#63664=CARTESIAN_POINT('Ctrl Pts',(0.167364636428823,0.403897163239664,
-0.601909269023626));
#63665=CARTESIAN_POINT('Ctrl Pts',(0.146710493450358,0.412455710921982,
-0.601097842861218));
#63666=CARTESIAN_POINT('Ctrl Pts',(0.125394044635463,0.419427680505348,
-0.60028641669881));
#63667=CARTESIAN_POINT('Ctrl Pts',(0.103684190323387,0.424727475773564,
-0.599474990536402));
#63668=CARTESIAN_POINT('Ctrl Pts',(0.0819443642684749,0.430034587723808,
-0.598662444152001));
#63669=CARTESIAN_POINT('Ctrl Pts',(0.0598107485201382,0.433664759998317,
-0.5978498977676));
#63670=CARTESIAN_POINT('Ctrl Pts',(0.03756375015824,0.435583292464311,-0.597037351383199));
#63671=CARTESIAN_POINT('Ctrl Pts',(0.0219890854947838,0.436926417470108,
-0.596468504419906));
#63672=CARTESIAN_POINT('Ctrl Pts',(0.00635908031257408,0.437431738095647,
-0.595899657456613));
#63673=CARTESIAN_POINT('Ctrl Pts',(-0.00922985932074836,0.43710256198851,
-0.595330810493319));
#63674=CARTESIAN_POINT('Origin',(0.,0.,-0.920658989190502));
#63675=CARTESIAN_POINT('',(-0.00922985932074692,0.43710256198851,-0.475606184023132));
#63676=CARTESIAN_POINT('',(-0.00922985932074758,0.43710256198851,-0.495313704306577));
#63677=CARTESIAN_POINT('',(-0.00922985932074702,0.43710256198851,-0.920658989190502));
#63678=CARTESIAN_POINT('',(-0.437199823825855,-0.000392487759930489,-0.550941010807406));
#63679=CARTESIAN_POINT('Ctrl Pts',(-0.437199823825855,-0.000392487759930985,
-0.550941010807406));
#63680=CARTESIAN_POINT('Ctrl Pts',(-0.437173299123608,-0.0299388745087773,
-0.549865238956156));
#63681=CARTESIAN_POINT('Ctrl Pts',(-0.434147816830185,-0.0593528249596906,
-0.548789467104907));
#63682=CARTESIAN_POINT('Ctrl Pts',(-0.428225193397315,-0.0881307196148554,
-0.547713695253658));
#63683=CARTESIAN_POINT('Ctrl Pts',(-0.42727988992287,-0.0927239280322208,
-0.547541992480348));
#63684=CARTESIAN_POINT('Ctrl Pts',(-0.426260877065074,-0.0973009825016195,
-0.547370289707038));
#63685=CARTESIAN_POINT('Ctrl Pts',(-0.425168676443051,-0.101859886960786,
-0.547198586933727));
#63686=CARTESIAN_POINT('Ctrl Pts',(-0.419991785780037,-0.123468508538497,
-0.546384737842233));
#63687=CARTESIAN_POINT('Ctrl Pts',(-0.413148549881292,-0.144743242971641,
-0.545570888750738));
#63688=CARTESIAN_POINT('Ctrl Pts',(-0.404701375565575,-0.165410509385986,
-0.544757039659243));
#63689=CARTESIAN_POINT('Ctrl Pts',(-0.396269269375605,-0.186040909392995,
-0.543944642317172));
#63690=CARTESIAN_POINT('Ctrl Pts',(-0.386239120277342,-0.20606531629854,
-0.543132244975101));
#63691=CARTESIAN_POINT('Ctrl Pts',(-0.374722999789755,-0.225225472423896,
-0.54231984763303));
#63692=CARTESIAN_POINT('Ctrl Pts',(-0.363219088317679,-0.244365315576356,
-0.541508311568137));
#63693=CARTESIAN_POINT('Ctrl Pts',(-0.350232675903339,-0.262642102451221,
-0.540696775503244));
#63694=CARTESIAN_POINT('Ctrl Pts',(-0.335921668328666,-0.279822216321874,
-0.539885239438351));
#63695=CARTESIAN_POINT('Ctrl Pts',(-0.321603776659083,-0.29701059442786,
-0.539073312996242));
#63696=CARTESIAN_POINT('Ctrl Pts',(-0.305960460555495,-0.31310068390885,
-0.538261386554133));
#63697=CARTESIAN_POINT('Ctrl Pts',(-0.289190361932185,-0.327891406666189,
-0.537449460112023));
#63698=CARTESIAN_POINT('Ctrl Pts',(-0.272416136530548,-0.342685769117932,
-0.536637333871421));
#63699=CARTESIAN_POINT('Ctrl Pts',(-0.254515133900513,-0.356179678793403,
-0.535825207630818));
#63700=CARTESIAN_POINT('Ctrl Pts',(-0.235719089868977,-0.36821237169783,
-0.535013081390215));
#63701=CARTESIAN_POINT('Ctrl Pts',(-0.21688264590535,-0.380270927489969,
-0.534199209577782));
#63702=CARTESIAN_POINT('Ctrl Pts',(-0.197147948073415,-0.390861651227168,
-0.53338533776535));
#63703=CARTESIAN_POINT('Ctrl Pts',(-0.176772290129475,-0.399869225425489,
-0.532571465952917));
#63704=CARTESIAN_POINT('Ctrl Pts',(-0.16679942243077,-0.404277983464777,
-0.532173116317709));
#63705=CARTESIAN_POINT('Ctrl Pts',(-0.15667331020594,-0.408308216793835,
-0.531774766682501));
#63706=CARTESIAN_POINT('Ctrl Pts',(-0.146425481105729,-0.411950747642186,
-0.531376417047293));
#63707=CARTESIAN_POINT('Ctrl Pts',(-0.125488539703116,-0.419392660869208,
-0.53056256438752));
#63708=CARTESIAN_POINT('Ctrl Pts',(-0.103922955068954,-0.425255634331867,
-0.529748711727747));
#63709=CARTESIAN_POINT('Ctrl Pts',(-0.0819920957220178,-0.429442820686423,
-0.528934859067974));
#63710=CARTESIAN_POINT('Ctrl Pts',(-0.0601003545798103,-0.433622538331684,
-0.528122458082049));
#63711=CARTESIAN_POINT('Ctrl Pts',(-0.0378453166231203,-0.436132214901088,
-0.527310057096123));
#63712=CARTESIAN_POINT('Ctrl Pts',(-0.0155045831831506,-0.436924991160172,
-0.526497656110197));
#63713=CARTESIAN_POINT('Ctrl Pts',(0.00681246718488999,-0.437716927009195,
-0.525686116338208));
#63714=CARTESIAN_POINT('Ctrl Pts',(0.029214322223221,-0.436795522814159,
-0.524874576566219));
#63715=CARTESIAN_POINT('Ctrl Pts',(0.0514190471355656,-0.434165776624172,
-0.52406303679423));
#63716=CARTESIAN_POINT('Ctrl Pts',(0.0736344546586686,-0.431534765273052,
-0.523251106593467));
#63717=CARTESIAN_POINT('Ctrl Pts',(0.0956518298188783,-0.427193835658177,
-0.522439176392705));
#63718=CARTESIAN_POINT('Ctrl Pts',(0.11719430442358,-0.421199875368777,
-0.521627246191943));
#63719=CARTESIAN_POINT('Ctrl Pts',(0.138742081080045,-0.415204439840886,
-0.520815116158245));
#63720=CARTESIAN_POINT('Ctrl Pts',(0.15981404383523,-0.407555385787585,
-0.520002986124546));
#63721=CARTESIAN_POINT('Ctrl Pts',(0.180149075836899,-0.398359323318924,
-0.519190856090848));
#63722=CARTESIAN_POINT('Ctrl Pts',(0.200527815297379,-0.389143495131599,
-0.518376980491173));
#63723=CARTESIAN_POINT('Ctrl Pts',(0.220165830000383,-0.378374358729374,
-0.517563104891498));
#63724=CARTESIAN_POINT('Ctrl Pts',(0.238826165613217,-0.366204727739127,
-0.516749229291823));
#63725=CARTESIAN_POINT('Ctrl Pts',(0.247958915804214,-0.360248661242976,
-0.516350901914835));
#63726=CARTESIAN_POINT('Ctrl Pts',(0.256857931630922,-0.353957788076334,
-0.515952574537847));
#63727=CARTESIAN_POINT('Ctrl Pts',(0.265498334026349,-0.347353529749207,
-0.515554247160858));
#63728=CARTESIAN_POINT('Ctrl Pts',(0.283152162037289,-0.333859894231881,
-0.514740395828064));
#63729=CARTESIAN_POINT('Ctrl Pts',(0.299825141677166,-0.318978397252585,
-0.51392654449527));
#63730=CARTESIAN_POINT('Ctrl Pts',(0.315292491492751,-0.302877012677247,
-0.513112693162475));
#63731=CARTESIAN_POINT('Ctrl Pts',(0.330732251724026,-0.286804348633387,
-0.512300293521162));
#63732=CARTESIAN_POINT('Ctrl Pts',(0.344970120595746,-0.269516587985787,
-0.511487893879849));
#63733=CARTESIAN_POINT('Ctrl Pts',(0.357815460872545,-0.251220890772579,
-0.510675494238536));
#63734=CARTESIAN_POINT('Ctrl Pts',(0.370647183769643,-0.232944588877088,
-0.509863955824262));
#63735=CARTESIAN_POINT('Ctrl Pts',(0.382088876941243,-0.213663038361432,
-0.509052417409989));
#63736=CARTESIAN_POINT('Ctrl Pts',(0.391991011714252,-0.193615306045873,
-0.508240878995716));
#63737=CARTESIAN_POINT('Ctrl Pts',(0.401897910330637,-0.173557928915436,
-0.507428950156349));
#63738=CARTESIAN_POINT('Ctrl Pts',(0.410263437270949,-0.152734266903474,
-0.506617021316982));
#63739=CARTESIAN_POINT('Ctrl Pts',(0.416984324671081,-0.131407431215295,
-0.505805092477615));
#63740=CARTESIAN_POINT('Ctrl Pts',(0.423706866192026,-0.110075346642452,
-0.50499296380922));
#63741=CARTESIAN_POINT('Ctrl Pts',(0.428783777419164,-0.0882405335351049,
-0.504180835140825));
#63742=CARTESIAN_POINT('Ctrl Pts',(0.432162060346666,-0.0661800090429443,
-0.503368706472431));
#63743=CARTESIAN_POINT('Ctrl Pts',(0.4355476045219,-0.0440720678788024,
-0.502554832222752));
#63744=CARTESIAN_POINT('Ctrl Pts',(0.437227170701727,-0.0217381609663,-0.501740957973073));
#63745=CARTESIAN_POINT('Ctrl Pts',(0.437199666812554,0.000539758271596754,
-0.500927083723394));
#63746=CARTESIAN_POINT('Ctrl Pts',(0.437186205549979,0.0114432679023959,
-0.500528748240405));
#63747=CARTESIAN_POINT('Ctrl Pts',(0.436764624756656,0.0223333862276293,
-0.500130412757415));
#63748=CARTESIAN_POINT('Ctrl Pts',(0.435939317411843,0.0331775757778652,
-0.499732077274425));
#63749=CARTESIAN_POINT('Ctrl Pts',(0.434253107340928,0.0553336631378791,
-0.49891822615915));
#63750=CARTESIAN_POINT('Ctrl Pts',(0.430868685109664,0.0774242171171006,
-0.498104375043875));
#63751=CARTESIAN_POINT('Ctrl Pts',(0.425804304059114,0.0991692222654455,
-0.4972905239286));
#63752=CARTESIAN_POINT('Ctrl Pts',(0.42074895656677,0.120875439896079,-0.496478124515191));
#63753=CARTESIAN_POINT('Ctrl Pts',(0.414019704841125,0.142236630434071,
-0.495665725101782));
#63754=CARTESIAN_POINT('Ctrl Pts',(0.405686267894861,0.16298003571462,-0.494853325688373));
#63755=CARTESIAN_POINT('Ctrl Pts',(0.397361665348452,0.183701450604199,
-0.494041787511606));
#63756=CARTESIAN_POINT('Ctrl Pts',(0.387436493343025,0.203805709481093,
-0.49323024933484));
#63757=CARTESIAN_POINT('Ctrl Pts',(0.376029631492862,0.223037118523673,
-0.492418711158074));
#63758=CARTESIAN_POINT('Ctrl Pts',(0.364617282049137,0.242277779379574,
-0.491606782567911));
#63759=CARTESIAN_POINT('Ctrl Pts',(0.351722167742822,0.260644126579765,
-0.490794853977749));
#63760=CARTESIAN_POINT('Ctrl Pts',(0.337508546981797,0.277906136517775,
-0.489982925387587));
#63761=CARTESIAN_POINT('Ctrl Pts',(0.323291428136882,0.295172394772234,
-0.489170796975411));
#63762=CARTESIAN_POINT('Ctrl Pts',(0.30775563583115,0.311333242542577,-0.488358668563235));
#63763=CARTESIAN_POINT('Ctrl Pts',(0.291104494176897,0.326193214935585,
-0.487546540151059));
#63764=CARTESIAN_POINT('Ctrl Pts',(0.274417562854466,0.341085127089369,
-0.486732666164495));
#63765=CARTESIAN_POINT('Ctrl Pts',(0.256611061717959,0.354670141411213,
-0.485918792177932));
#63766=CARTESIAN_POINT('Ctrl Pts',(0.237920753444391,0.366793613740007,
-0.485104918191369));
#63767=CARTESIAN_POINT('Ctrl Pts',(0.228773096405688,0.37272724337087,-0.484706581256909));
#63768=CARTESIAN_POINT('Ctrl Pts',(0.219414145616143,0.378311447305482,
-0.484308244322449));
#63769=CARTESIAN_POINT('Ctrl Pts',(0.209873572367088,0.383532167649438,
-0.48390990738799));
#63770=CARTESIAN_POINT('Ctrl Pts',(0.190381206986412,0.394198632424477,
-0.483096064354828));
#63771=CARTESIAN_POINT('Ctrl Pts',(0.170017884048308,0.403405803602295,
-0.482282221321667));
#63772=CARTESIAN_POINT('Ctrl Pts',(0.149028282021272,0.411016314953297,
-0.481468378288506));
#63773=CARTESIAN_POINT('Ctrl Pts',(0.128075969059305,0.41861330585486,-0.480655981087704));
#63774=CARTESIAN_POINT('Ctrl Pts',(0.106500231687055,0.424618973788685,
-0.479843583886902));
#63775=CARTESIAN_POINT('Ctrl Pts',(0.0845677300764937,0.428943048701934,
-0.4790311866861));
#63776=CARTESIAN_POINT('Ctrl Pts',(0.0626556115000823,0.433263105023587,
-0.478219544488999));
#63777=CARTESIAN_POINT('Ctrl Pts',(0.0403880794136098,0.435904501921364,
-0.477407902291897));
#63778=CARTESIAN_POINT('Ctrl Pts',(0.0180444028609421,0.436827471120341,
-0.476596260094796));
#63779=CARTESIAN_POINT('Ctrl Pts',(0.00895914354067751,0.437202763633081,
-0.476266234737575));
#63780=CARTESIAN_POINT('Ctrl Pts',(-0.000138609858056261,0.437294532845896,
-0.475936209380354));
#63781=CARTESIAN_POINT('Ctrl Pts',(-0.00922985932074711,0.43710256198851,
-0.475606184023132));
#63782=CARTESIAN_POINT('Ctrl Pts',(-0.0092298593207472,0.43710256198851,
-0.57559571443739));
#63783=CARTESIAN_POINT('Ctrl Pts',(-0.0315292904518787,0.436631687118007,
-0.574783656190821));
#63784=CARTESIAN_POINT('Ctrl Pts',(-0.0538297205441489,0.434449229488396,
-0.573971597944252));
#63785=CARTESIAN_POINT('Ctrl Pts',(-0.0758498132990062,0.430570140421402,
-0.573159539697683));
#63786=CARTESIAN_POINT('Ctrl Pts',(-0.0987604173441071,0.42653417769141,
-0.572314641124557));
#63787=CARTESIAN_POINT('Ctrl Pts',(-0.121366684075482,0.42066129074851,
-0.57146974255143));
#63788=CARTESIAN_POINT('Ctrl Pts',(-0.1433594617347,0.41302772876786,-0.570624843978303));
#63789=CARTESIAN_POINT('Ctrl Pts',(-0.164494584018402,0.405691853853778,
-0.56981289403105));
#63790=CARTESIAN_POINT('Ctrl Pts',(-0.185062535112171,0.396730542173786,
-0.569000944083796));
#63791=CARTESIAN_POINT('Ctrl Pts',(-0.204806602463167,0.386261693140148,
-0.568188994136542));
#63792=CARTESIAN_POINT('Ctrl Pts',(-0.224560290384027,0.375787743015042,
-0.567376648555448));
#63793=CARTESIAN_POINT('Ctrl Pts',(-0.243488685069747,0.363805166334551,
-0.566564302974354));
#63794=CARTESIAN_POINT('Ctrl Pts',(-0.261361799646781,0.35047660362055,
-0.56575195739326));
#63795=CARTESIAN_POINT('Ctrl Pts',(-0.279271495348444,0.337120761172417,
-0.56493794917442));
#63796=CARTESIAN_POINT('Ctrl Pts',(-0.296121069562384,0.32241391337574,
-0.564123940955579));
#63797=CARTESIAN_POINT('Ctrl Pts',(-0.311714809764689,0.306557853224092,
-0.563309932736738));
#63798=CARTESIAN_POINT('Ctrl Pts',(-0.313561365287305,0.304680234701524,
-0.563213540764546));
#63799=CARTESIAN_POINT('Ctrl Pts',(-0.315390357015224,0.302786539933061,
-0.563117148792354));
#63800=CARTESIAN_POINT('Ctrl Pts',(-0.317201497937629,0.300877133903732,
-0.563020756820161));
#63801=CARTESIAN_POINT('Ctrl Pts',(-0.332303636588417,0.284955614910453,
-0.562216995549647));
#63802=CARTESIAN_POINT('Ctrl Pts',(-0.346252502632818,0.267842840736493,
-0.561413234279134));
#63803=CARTESIAN_POINT('Ctrl Pts',(-0.358854735651147,0.249734095991607,
-0.56060947300862));
#63804=CARTESIAN_POINT('Ctrl Pts',(-0.371487447422678,0.231581554884516,
-0.55980376782536));
#63805=CARTESIAN_POINT('Ctrl Pts',(-0.382766470990126,0.212428739913962,
-0.558998062642099));
#63806=CARTESIAN_POINT('Ctrl Pts',(-0.392536209756225,0.192507568760859,
-0.558192357458839));
#63807=CARTESIAN_POINT('Ctrl Pts',(-0.402256949762855,0.172686309457707,
-0.557390693177329));
#63808=CARTESIAN_POINT('Ctrl Pts',(-0.410483164408189,0.152105037054788,
-0.556589028895819));
#63809=CARTESIAN_POINT('Ctrl Pts',(-0.417106810099915,0.131018124579286,
-0.555787364614309));
#63810=CARTESIAN_POINT('Ctrl Pts',(-0.423780536920521,0.109771774774175,
-0.554979638980174));
#63811=CARTESIAN_POINT('Ctrl Pts',(-0.428827075457434,0.0880128079590822,
-0.554171913346038));
#63812=CARTESIAN_POINT('Ctrl Pts',(-0.432186891185448,0.0660176573914703,
-0.553364187711903));
#63813=CARTESIAN_POINT('Ctrl Pts',(-0.435546706913462,0.0440225068238584,
-0.552556462077768));
#63814=CARTESIAN_POINT('Ctrl Pts',(-0.43721973946023,0.021791931740694,
-0.551748736443633));
#63815=CARTESIAN_POINT('Ctrl Pts',(-0.437199823825906,-0.000392487702464365,
-0.550941010809498));
#63816=CARTESIAN_POINT('',(-0.43719997630689,0.00014393489640635,-0.57065898919245));
#63817=CARTESIAN_POINT('Ctrl Pts',(-0.00922985932074836,0.43710256198851,
-0.595330810493319));
#63818=CARTESIAN_POINT('Ctrl Pts',(-0.0268631581577466,0.436730217184842,
-0.59468736400291));
#63819=CARTESIAN_POINT('Ctrl Pts',(-0.0444436751027457,0.435289819211557,
-0.5940439175125));
#63820=CARTESIAN_POINT('Ctrl Pts',(-0.0618348607888011,0.432805140902034,
-0.593400471022091));
#63821=CARTESIAN_POINT('Ctrl Pts',(-0.0838331401374778,0.4296622472241,
-0.592586569319385));
#63822=CARTESIAN_POINT('Ctrl Pts',(-0.105654017097476,0.424828934836601,
-0.59177266761668));
#63823=CARTESIAN_POINT('Ctrl Pts',(-0.127019260290177,0.418341902653005,
-0.590958765913974));
#63824=CARTESIAN_POINT('Ctrl Pts',(-0.148346413599656,0.411866435528422,
-0.590146315232468));
#63825=CARTESIAN_POINT('Ctrl Pts',(-0.169218852447682,0.403743253256097,
-0.589333864550962));
#63826=CARTESIAN_POINT('Ctrl Pts',(-0.189368984193052,0.394059929231192,
-0.588521413869456));
#63827=CARTESIAN_POINT('Ctrl Pts',(-0.209497768427388,0.384386863941518,
-0.587709823916808));
#63828=CARTESIAN_POINT('Ctrl Pts',(-0.228905111152579,0.373157221535593,
-0.58689823396416));
#63829=CARTESIAN_POINT('Ctrl Pts',(-0.247343690691476,0.360506502958157,
-0.586086644011512));
#63830=CARTESIAN_POINT('Ctrl Pts',(-0.26579114352254,0.347849696410559,
-0.585274663493271));
#63831=CARTESIAN_POINT('Ctrl Pts',(-0.283268301333048,0.333770836892071,
-0.584462682975029));
#63832=CARTESIAN_POINT('Ctrl Pts',(-0.299556449929447,0.318449012097175,
-0.583650702456787));
#63833=CARTESIAN_POINT('Ctrl Pts',(-0.315848610034954,0.303123413783186,
-0.582838521960799));
#63834=CARTESIAN_POINT('Ctrl Pts',(-0.330950678613554,0.286554753730788,
-0.582026341464811));
#63835=CARTESIAN_POINT('Ctrl Pts',(-0.3446810005753,0.268958821834142,-0.581214160968823));
#63836=CARTESIAN_POINT('Ctrl Pts',(-0.358440822655247,0.251325084409538,
-0.580400235472194));
#63837=CARTESIAN_POINT('Ctrl Pts',(-0.370822612161444,0.232660262061621,
-0.579586309975564));
#63838=CARTESIAN_POINT('Ctrl Pts',(-0.381687584035801,0.21320982198978,
-0.578772384478935));
#63839=CARTESIAN_POINT('Ctrl Pts',(-0.38700079840824,0.20369812155143,-0.578374356697842));
#63840=CARTESIAN_POINT('Ctrl Pts',(-0.391951981037456,0.193998917752201,
-0.577976328916749));
#63841=CARTESIAN_POINT('Ctrl Pts',(-0.396529087440907,0.184142669724542,
-0.577578301135656));
#63842=CARTESIAN_POINT('Ctrl Pts',(-0.406675666486683,0.162293232352492,
-0.576695948839841));
#63843=CARTESIAN_POINT('Ctrl Pts',(-0.415031602930839,0.13956203722299,
-0.575813596544027));
#63844=CARTESIAN_POINT('Ctrl Pts',(-0.421462353738376,0.116246825252598,
-0.574931244248212));
#63845=CARTESIAN_POINT('Ctrl Pts',(-0.427857489738203,0.0930607376746569,
-0.574053778599118));
#63846=CARTESIAN_POINT('Ctrl Pts',(-0.432348472496993,0.0692975505394903,
-0.573176312950024));
#63847=CARTESIAN_POINT('Ctrl Pts',(-0.434849789863832,0.0452714065982187,
-0.57229884730093));
#63848=CARTESIAN_POINT('Ctrl Pts',(-0.436407991627485,0.0303042615412165,
-0.571752227931437));
#63849=CARTESIAN_POINT('Ctrl Pts',(-0.437195007874429,0.0152354700883076,
-0.571205608561943));
#63850=CARTESIAN_POINT('Ctrl Pts',(-0.437199976306891,0.000143934896406404,
-0.57065898919245));
#63851=CARTESIAN_POINT('Ctrl Pts',(-0.437199976306908,0.000143934842618929,
-0.570658989190502));
#63852=CARTESIAN_POINT('Ctrl Pts',(-0.437207536200571,-0.022819131431466,
-0.56982726089721));
#63853=CARTESIAN_POINT('Ctrl Pts',(-0.435401621291541,-0.0457679489929577,
-0.568995532603917));
#63854=CARTESIAN_POINT('Ctrl Pts',(-0.431814986033601,-0.0684080246520904,
-0.568163804310625));
#63855=CARTESIAN_POINT('Ctrl Pts',(-0.428225091115235,-0.0910686764092512,
-0.56733132011337));
#63856=CARTESIAN_POINT('Ctrl Pts',(-0.422851404212316,-0.113419377779202,
-0.566498835916116));
#63857=CARTESIAN_POINT('Ctrl Pts',(-0.415777657420984,-0.135176845611661,
-0.565666351718861));
#63858=CARTESIAN_POINT('Ctrl Pts',(-0.408683321630454,-0.156997641196864,
-0.564831444475238));
#63859=CARTESIAN_POINT('Ctrl Pts',(-0.399879295855431,-0.178221136303188,
-0.563996537231616));
#63860=CARTESIAN_POINT('Ctrl Pts',(-0.38949786065506,-0.198583122508261,
-0.563161629987993));
#63861=CARTESIAN_POINT('Ctrl Pts',(-0.383672425477592,-0.210009040835808,
-0.562693130408403));
#63862=CARTESIAN_POINT('Ctrl Pts',(-0.377351137911915,-0.221164130691169,
-0.562224630828812));
#63863=CARTESIAN_POINT('Ctrl Pts',(-0.370563342659814,-0.232005709146963,
-0.561756131249221));
#63864=CARTESIAN_POINT('Ctrl Pts',(-0.35877222017527,-0.250838684325242,
-0.560942297637313));
#63865=CARTESIAN_POINT('Ctrl Pts',(-0.345508001174671,-0.268824352225785,
-0.560128464025405));
#63866=CARTESIAN_POINT('Ctrl Pts',(-0.330916986010361,-0.285723272362996,
-0.559314630413496));
#63867=CARTESIAN_POINT('Ctrl Pts',(-0.316352005050509,-0.302592040386936,
-0.558502248894565));
#63868=CARTESIAN_POINT('Ctrl Pts',(-0.300465347420246,-0.318377337669999,
-0.557689867375634));
#63869=CARTESIAN_POINT('Ctrl Pts',(-0.283445509763087,-0.33287006923895,
-0.556877485856702));
#63870=CARTESIAN_POINT('Ctrl Pts',(-0.266443722409415,-0.347347430614106,
-0.556065965904917));
#63871=CARTESIAN_POINT('Ctrl Pts',(-0.248311664896186,-0.360534464973568,
-0.555254445953133));
#63872=CARTESIAN_POINT('Ctrl Pts',(-0.229273430822636,-0.372260035350047,
-0.554442926001348));
#63873=CARTESIAN_POINT('Ctrl Pts',(-0.210226044304049,-0.383991242679931,
-0.553631015919274));
#63874=CARTESIAN_POINT('Ctrl Pts',(-0.190272210438616,-0.394259191281616,
-0.552819105837201));
#63875=CARTESIAN_POINT('Ctrl Pts',(-0.169664271032002,-0.402936564654015,
-0.552007195755127));
#63876=CARTESIAN_POINT('Ctrl Pts',(-0.149051264462849,-0.411616071653674,
-0.551195086037357));
#63877=CARTESIAN_POINT('Ctrl Pts',(-0.127784503651842,-0.418703976275056,
-0.550382976319586));
#63878=CARTESIAN_POINT('Ctrl Pts',(-0.106134857200167,-0.424121718480792,
-0.549570866601815));
#63879=CARTESIAN_POINT('Ctrl Pts',(-0.0844386762296176,-0.429551105774012,
-0.548757011306578));
#63880=CARTESIAN_POINT('Ctrl Pts',(-0.062358672049308,-0.433303036707379,
-0.547943156011342));
#63881=CARTESIAN_POINT('Ctrl Pts',(-0.0401754613602373,-0.435350172050606,
-0.547129300716105));
#63882=CARTESIAN_POINT('Ctrl Pts',(-0.0293150275399613,-0.436352406498445,
-0.546730854264999));
#63883=CARTESIAN_POINT('Ctrl Pts',(-0.0184299106066175,-0.436946818404209,
-0.546332407813893));
#63884=CARTESIAN_POINT('Ctrl Pts',(-0.00755294417326473,-0.437134753862371,
-0.545933961362787));
#63885=CARTESIAN_POINT('Ctrl Pts',(0.0146641498154526,-0.43751862741419,
-0.545120101882027));
#63886=CARTESIAN_POINT('Ctrl Pts',(0.0369740900129726,-0.43620552516262,
-0.544306242401266));
#63887=CARTESIAN_POINT('Ctrl Pts',(0.0590963723883364,-0.433187556112291,
-0.543492382920506));
#63888=CARTESIAN_POINT('Ctrl Pts',(0.0811791982123437,-0.430174969809041,
-0.542679975011869));
#63889=CARTESIAN_POINT('Ctrl Pts',(0.103074322004255,-0.425463593101464,
-0.541867567103232));
#63890=CARTESIAN_POINT('Ctrl Pts',(0.124503674974381,-0.419097452769489,
-0.541055159194595));
#63891=CARTESIAN_POINT('Ctrl Pts',(0.145910313274123,-0.412738060414434,
-0.540243612421518));
#63892=CARTESIAN_POINT('Ctrl Pts',(0.16685147056835,-0.404727562698576,
-0.539432065648441));
#63893=CARTESIAN_POINT('Ctrl Pts',(0.187061492127124,-0.395160522020069,
-0.538620518875363));
#63894=CARTESIAN_POINT('Ctrl Pts',(0.207281237447412,-0.385588878297392,
-0.537808581638216));
#63895=CARTESIAN_POINT('Ctrl Pts',(0.226768489566447,-0.374459484778317,
-0.536996644401068));
#63896=CARTESIAN_POINT('Ctrl Pts',(0.24527892815776,-0.3619144752587,-0.53618470716392));
#63897=CARTESIAN_POINT('Ctrl Pts',(0.263793923186711,-0.349366377721841,
-0.535372570064334));
#63898=CARTESIAN_POINT('Ctrl Pts',(0.281331051587131,-0.33540239783538,
-0.534560432964749));
#63899=CARTESIAN_POINT('Ctrl Pts',(0.297676764826116,-0.320206782693086,
-0.533748295865163));
#63900=CARTESIAN_POINT('Ctrl Pts',(0.314057609401525,-0.304978508084671,
-0.532934413264402));
#63901=CARTESIAN_POINT('Ctrl Pts',(0.329241435602004,-0.288513835581878,
-0.532120530663641));
#63902=CARTESIAN_POINT('Ctrl Pts',(0.343052318357026,-0.271033110283356,
-0.53130664806288));
#63903=CARTESIAN_POINT('Ctrl Pts',(0.349810878789107,-0.262478657941508,
-0.530908362534038));
#63904=CARTESIAN_POINT('Ctrl Pts',(0.356241286735471,-0.253681362361846,
-0.530510077005196));
#63905=CARTESIAN_POINT('Ctrl Pts',(0.362326789425417,-0.244669445711289,
-0.530111791476353));
#63906=CARTESIAN_POINT('Ctrl Pts',(0.374761829137925,-0.226254608491577,
-0.52929793983247));
#63907=CARTESIAN_POINT('Ctrl Pts',(0.385824970639398,-0.206836713406551,
-0.528484088188586));
#63908=CARTESIAN_POINT('Ctrl Pts',(0.395356659951971,-0.186646595017487,
-0.527670236544703));
#63909=CARTESIAN_POINT('Ctrl Pts',(0.404871347717123,-0.166492489473992,
-0.526857836557169));
#63910=CARTESIAN_POINT('Ctrl Pts',(0.412859653188187,-0.145569510876561,
-0.526045436569635));
#63911=CARTESIAN_POINT('Ctrl Pts',(0.419206871783939,-0.124134760035713,
-0.525233036582102));
#63912=CARTESIAN_POINT('Ctrl Pts',(0.425547361943917,-0.102722731327747,
-0.524421497787712));
#63913=CARTESIAN_POINT('Ctrl Pts',(0.430249990105675,-0.0808006821067508,
-0.523609958993323));
#63914=CARTESIAN_POINT('Ctrl Pts',(0.433249183383256,-0.0586428605862762,
-0.522798420198933));
#63915=CARTESIAN_POINT('Ctrl Pts',(0.436249819722372,-0.0364743778322752,
-0.521986490932737));
#63916=CARTESIAN_POINT('Ctrl Pts',(0.437545269348742,-0.0140706027309854,
-0.521174561666541));
#63917=CARTESIAN_POINT('Ctrl Pts',(0.437121469958561,0.00828616324160506,
-0.520362632400345));
#63918=CARTESIAN_POINT('Ctrl Pts',(0.436697566250218,0.0306484323291283,
-0.519550503277869));
#63919=CARTESIAN_POINT('Ctrl Pts',(0.434553616100216,0.0529629546957005,
-0.518738374155393));
#63920=CARTESIAN_POINT('Ctrl Pts',(0.430727637927697,0.0749502630097212,
-0.517926245032917));
#63921=CARTESIAN_POINT('Ctrl Pts',(0.426893436074222,0.0969848315538128,
-0.517112370293897));
#63922=CARTESIAN_POINT('Ctrl Pts',(0.421370158290273,0.118690085595842,
-0.516298495554876));
#63923=CARTESIAN_POINT('Ctrl Pts',(0.414246596892501,0.139798415452329,
-0.515484620815855));
#63924=CARTESIAN_POINT('Ctrl Pts',(0.410760126576244,0.150129422846104,
-0.515086287740543));
#63925=CARTESIAN_POINT('Ctrl Pts',(0.406891073807587,0.160317716194181,
-0.514687954665231));
#63926=CARTESIAN_POINT('Ctrl Pts',(0.402653968465716,0.170333853589971,
-0.514289621589919));
#63927=CARTESIAN_POINT('Ctrl Pts',(0.393996981173336,0.190798195908118,
-0.513475772489442));
#63928=CARTESIAN_POINT('Ctrl Pts',(0.383751155681082,0.210659396133888,
-0.512661923388965));
#63929=CARTESIAN_POINT('Ctrl Pts',(0.372023001995696,0.22965784547041,-0.511848074288487));
#63930=CARTESIAN_POINT('Ctrl Pts',(0.360315769066053,0.248622405251188,
-0.511035676937254));
#63931=CARTESIAN_POINT('Ctrl Pts',(0.347131780986945,0.266726637689673,
-0.51022327958602));
#63932=CARTESIAN_POINT('Ctrl Pts',(0.332624019768573,0.283734209204664,
-0.509410882234786));
#63933=CARTESIAN_POINT('Ctrl Pts',(0.318131639202835,0.300723749850129,
-0.508599346160581));
#63934=CARTESIAN_POINT('Ctrl Pts',(0.302318712512743,0.316618378059953,
-0.507787810086375));
#63935=CARTESIAN_POINT('Ctrl Pts',(0.285379384357789,0.331213597220237,
-0.506976274012169));
#63936=CARTESIAN_POINT('Ctrl Pts',(0.268431907791513,0.345815837193151,
-0.506164347560631));
#63937=CARTESIAN_POINT('Ctrl Pts',(0.250357477215184,0.359116938197219,
-0.505352421109092));
#63938=CARTESIAN_POINT('Ctrl Pts',(0.23138507344878,0.370951193265506,-0.504540494657554));
#63939=CARTESIAN_POINT('Ctrl Pts',(0.212408000959996,0.382788360503076,
-0.503728368407443));
#63940=CARTESIAN_POINT('Ctrl Pts',(0.192533138946753,0.393157611381695,
-0.502916242157332));
#63941=CARTESIAN_POINT('Ctrl Pts',(0.172015488466205,0.401938442709494,
-0.502104115907221));
#63942=CARTESIAN_POINT('Ctrl Pts',(0.151453737659898,0.410738147422545,
-0.501290244085305));
#63943=CARTESIAN_POINT('Ctrl Pts',(0.130247116519065,0.417942379376124,
-0.500476372263389));
#63944=CARTESIAN_POINT('Ctrl Pts',(0.108668369482998,0.423479663589536,
-0.499662500441473));
#63945=CARTESIAN_POINT('Ctrl Pts',(0.0981066513195151,0.42618988745728,
-0.499264150862143));
#63946=CARTESIAN_POINT('Ctrl Pts',(0.087455965752906,0.428501551984591,
-0.498865801282813));
#63947=CARTESIAN_POINT('Ctrl Pts',(0.0767489199084235,0.430410784359419,
-0.498467451703484));
#63948=CARTESIAN_POINT('Ctrl Pts',(0.05487165141627,0.434311840718447,-0.497653520314069));
#63949=CARTESIAN_POINT('Ctrl Pts',(0.0326336448370843,0.436551803539617,
-0.496839588924654));
#63950=CARTESIAN_POINT('Ctrl Pts',(0.0103106826073552,0.437078402376702,
-0.496025657535238));
#63951=CARTESIAN_POINT('Ctrl Pts',(0.00380198288178817,0.437231942649321,
-0.495788339792351));
#63952=CARTESIAN_POINT('Ctrl Pts',(-0.00271386094603355,0.437240153834367,
-0.495551022049464));
#63953=CARTESIAN_POINT('Ctrl Pts',(-0.00922985932074758,0.43710256198851,
-0.495313704306577));
#63954=CARTESIAN_POINT('Origin',(0.,0.,-0.920658989190502));
#63955=CARTESIAN_POINT('',(-0.00922985932074681,0.43710256198851,-0.375613721612844));
#63956=CARTESIAN_POINT('',(-0.0092298593207473,0.43710256198851,-0.39532387974855));
#63957=CARTESIAN_POINT('',(-0.00922985932074702,0.43710256198851,-0.920658989190502));
#63958=CARTESIAN_POINT('',(-0.437199950177151,0.000208722535621865,-0.450941010807471));
#63959=CARTESIAN_POINT('Ctrl Pts',(-0.437199950177151,0.000208722535622156,
-0.450941010807471));
#63960=CARTESIAN_POINT('Ctrl Pts',(-0.437210447586036,-0.0217796393252642,
-0.450136498703844));
#63961=CARTESIAN_POINT('Ctrl Pts',(-0.435557844346497,-0.0438345863239729,
-0.449331986600217));
#63962=CARTESIAN_POINT('Ctrl Pts',(-0.432238247625148,-0.0656805701097482,
-0.44852747449659));
#63963=CARTESIAN_POINT('Ctrl Pts',(-0.428924107663845,-0.0874906434216002,
-0.447724284851645));
#63964=CARTESIAN_POINT('Ctrl Pts',(-0.423948466443405,-0.1090917095392,
-0.446921095206699));
#63965=CARTESIAN_POINT('Ctrl Pts',(-0.417359317587333,-0.130211520316123,
-0.446117905561754));
#63966=CARTESIAN_POINT('Ctrl Pts',(-0.410745398879746,-0.151410724439345,
-0.445311696575665));
#63967=CARTESIAN_POINT('Ctrl Pts',(-0.402505957615879,-0.172124316795769,
-0.444505487589576));
#63968=CARTESIAN_POINT('Ctrl Pts',(-0.39274073871354,-0.192089958495344,
-0.443699278603487));
#63969=CARTESIAN_POINT('Ctrl Pts',(-0.383014546323265,-0.211975807886681,
-0.442896291616315));
#63970=CARTESIAN_POINT('Ctrl Pts',(-0.371775107128368,-0.231119027356013,
-0.442093304629142));
#63971=CARTESIAN_POINT('Ctrl Pts',(-0.359167827505802,-0.24928359690273,
-0.44129031764197));
#63972=CARTESIAN_POINT('Ctrl Pts',(-0.346484667498001,-0.267557494914912,
-0.440482497656422));
#63973=CARTESIAN_POINT('Ctrl Pts',(-0.332417586681563,-0.28484031772645,
-0.439674677670875));
#63974=CARTESIAN_POINT('Ctrl Pts',(-0.317156271461288,-0.300924807007953,
-0.438866857685328));
#63975=CARTESIAN_POINT('Ctrl Pts',(-0.301894956241013,-0.317009296289457,
-0.438059037699781));
#63976=CARTESIAN_POINT('Ctrl Pts',(-0.285440002767781,-0.331894998055556,
-0.437251217714234));
#63977=CARTESIAN_POINT('Ctrl Pts',(-0.268014769370086,-0.34541558071329,
-0.436443397728686));
#63978=CARTESIAN_POINT('Ctrl Pts',(-0.250459433934599,-0.359037112111036,
-0.435629546315962));
#63979=CARTESIAN_POINT('Ctrl Pts',(-0.231812813534221,-0.371355830785756,
-0.434815694903237));
#63980=CARTESIAN_POINT('Ctrl Pts',(-0.212294725853223,-0.382197317330858,
-0.434001843490512));
#63981=CARTESIAN_POINT('Ctrl Pts',(-0.1928114532553,-0.393019465544209,
-0.433189443772493));
#63982=CARTESIAN_POINT('Ctrl Pts',(-0.172460390531698,-0.402369219853268,
-0.432377044054474));
#63983=CARTESIAN_POINT('Ctrl Pts',(-0.151490520190107,-0.410115181738656,
-0.431564644336455));
#63984=CARTESIAN_POINT('Ctrl Pts',(-0.13054288015175,-0.417852932076774,
-0.430753105848943));
#63985=CARTESIAN_POINT('Ctrl Pts',(-0.10897839299455,-0.423989992562469,
-0.429941567361431));
#63986=CARTESIAN_POINT('Ctrl Pts',(-0.0870663892354181,-0.428442859510468,
-0.429130028873919));
#63987=CARTESIAN_POINT('Ctrl Pts',(-0.0651438439397747,-0.432897868666,
-0.428318099967407));
#63988=CARTESIAN_POINT('Ctrl Pts',(-0.0428741455502252,-0.435666904852043,
-0.427506171060895));
#63989=CARTESIAN_POINT('Ctrl Pts',(-0.0205380549729165,-0.436717332261876,
-0.426694242154384));
#63990=CARTESIAN_POINT('Ctrl Pts',(0.00180353278951352,-0.437768018194743,
-0.425882113422236));
#63991=CARTESIAN_POINT('Ctrl Pts',(0.0242108292959832,-0.437099251179971,
-0.425069984690088));
#63992=CARTESIAN_POINT('Ctrl Pts',(0.0464024694007817,-0.434730549689701,
-0.42425785595794));
#63993=CARTESIAN_POINT('Ctrl Pts',(0.0686418078214144,-0.432356756954652,
-0.423443981650766));
#63994=CARTESIAN_POINT('Ctrl Pts',(0.0906638584377974,-0.428275858908475,
-0.422630107343592));
#63995=CARTESIAN_POINT('Ctrl Pts',(0.112195741892854,-0.422558818983952,
-0.421816233036417));
#63996=CARTESIAN_POINT('Ctrl Pts',(0.122734106495398,-0.419760724181995,
-0.421417897971696));
#63997=CARTESIAN_POINT('Ctrl Pts',(0.133155278346947,-0.416571469487715,
-0.421019562906974));
#63998=CARTESIAN_POINT('Ctrl Pts',(0.143428921514978,-0.413003613147694,
-0.420621227842253));
#63999=CARTESIAN_POINT('Ctrl Pts',(0.164419343064774,-0.405714007368978,
-0.4198073762426));
#64000=CARTESIAN_POINT('Ctrl Pts',(0.184912629682327,-0.396799260557487,
-0.418993524642946));
#64001=CARTESIAN_POINT('Ctrl Pts',(0.204642716959909,-0.386348545222143,
-0.418179673043293));
#64002=CARTESIAN_POINT('Ctrl Pts',(0.224337611028023,-0.375916471173517,
-0.417367273137665));
#64003=CARTESIAN_POINT('Ctrl Pts',(0.243271356699597,-0.363954149047342,
-0.416554873232037));
#64004=CARTESIAN_POINT('Ctrl Pts',(0.261198052034453,-0.350598656034799,
-0.415742473326409));
#64005=CARTESIAN_POINT('Ctrl Pts',(0.279105743162667,-0.337257321267503,
-0.41493093465122));
#64006=CARTESIAN_POINT('Ctrl Pts',(0.296007915887002,-0.322526150683547,
-0.41411939597603));
#64007=CARTESIAN_POINT('Ctrl Pts',(0.311687723668804,-0.306585392532259,
-0.413307857300841));
#64008=CARTESIAN_POINT('Ctrl Pts',(0.327375074729211,-0.290636965563753,
-0.412495928208727));
#64009=CARTESIAN_POINT('Ctrl Pts',(0.341838370981948,-0.273478285563776,
-0.411683999116614));
#64010=CARTESIAN_POINT('Ctrl Pts',(0.354897175683285,-0.255326917288459,
-0.4108720700245));
#64011=CARTESIAN_POINT('Ctrl Pts',(0.367959194300396,-0.237171081761341,
-0.410059941107688));
#64012=CARTESIAN_POINT('Ctrl Pts',(0.379615641078203,-0.218022670618517,
-0.409247812190875));
#64013=CARTESIAN_POINT('Ctrl Pts',(0.389729470148362,-0.198128191073044,
-0.408435683274062));
#64014=CARTESIAN_POINT('Ctrl Pts',(0.399865037643893,-0.178190950803033,
-0.407621808786534));
#64015=CARTESIAN_POINT('Ctrl Pts',(0.408451086733716,-0.157505099989189,
-0.406807934299006));
#64016=CARTESIAN_POINT('Ctrl Pts',(0.415398323941052,-0.136338081499503,
-0.405994059811478));
#64017=CARTESIAN_POINT('Ctrl Pts',(0.418798504796817,-0.125978324247186,
-0.405595725859591));
#64018=CARTESIAN_POINT('Ctrl Pts',(0.421806886383809,-0.115503537983901,
-0.405197391907705));
#64019=CARTESIAN_POINT('Ctrl Pts',(0.424417456202221,-0.104945999784821,
-0.404799057955819));
#64020=CARTESIAN_POINT('Ctrl Pts',(0.429751209670126,-0.0833754960638666,
-0.403985206863895));
#64021=CARTESIAN_POINT('Ctrl Pts',(0.433451576961043,-0.0613356638242659,
-0.403171355771971));
#64022=CARTESIAN_POINT('Ctrl Pts',(0.435448244719041,-0.0390981607125717,
-0.402357504680048));
#64023=CARTESIAN_POINT('Ctrl Pts',(0.437441350953927,-0.0169003233795044,
-0.401545105281558));
#64024=CARTESIAN_POINT('Ctrl Pts',(0.437736671263043,0.00549378516313112,
-0.400732705883068));
#64025=CARTESIAN_POINT('Ctrl Pts',(0.436315043346417,0.0278032902659854,
-0.399920306484578));
#64026=CARTESIAN_POINT('Ctrl Pts',(0.434894922503936,0.0500891449621915,
-0.399108768314342));
#64027=CARTESIAN_POINT('Ctrl Pts',(0.431761484426021,0.0722898620470738,
-0.398297230144107));
#64028=CARTESIAN_POINT('Ctrl Pts',(0.426947598401813,0.094125385624304,
-0.397485691973871));
#64029=CARTESIAN_POINT('Ctrl Pts',(0.422131396447059,0.11597141413576,-0.396673763377683));
#64030=CARTESIAN_POINT('Ctrl Pts',(0.415633267298273,0.137451195365861,
-0.395861834781494));
#64031=CARTESIAN_POINT('Ctrl Pts',(0.407537213848898,0.158294849342224,
-0.395049906185305));
#64032=CARTESIAN_POINT('Ctrl Pts',(0.399439167825586,0.179143633289868,
-0.394237777759932));
#64033=CARTESIAN_POINT('Ctrl Pts',(0.38974270292394,0.1993553229584,-0.393425649334559));
#64034=CARTESIAN_POINT('Ctrl Pts',(0.378579742042501,0.218680632235764,
-0.392613520909186));
#64035=CARTESIAN_POINT('Ctrl Pts',(0.367392787543437,0.238047479245474,
-0.391799646898648));
#64036=CARTESIAN_POINT('Ctrl Pts',(0.354733443520658,0.256523547104739,
-0.390985772888111));
#64037=CARTESIAN_POINT('Ctrl Pts',(0.340777218881838,0.273888165299561,
-0.390171898877574));
#64038=CARTESIAN_POINT('Ctrl Pts',(0.333946579630962,0.282386985409414,
-0.38977356194151));
#64039=CARTESIAN_POINT('Ctrl Pts',(0.326805888618687,0.290620077775586,
-0.389375225005447));
#64040=CARTESIAN_POINT('Ctrl Pts',(0.319378925732149,0.298564803347914,
-0.388976888069383));
#64041=CARTESIAN_POINT('Ctrl Pts',(0.304203718720093,0.314797933505676,
-0.388162982633519));
#64042=CARTESIAN_POINT('Ctrl Pts',(0.287744340900112,0.329917556773789,
-0.387349077197655));
#64043=CARTESIAN_POINT('Ctrl Pts',(0.270190222122802,0.343716574911992,
-0.386535171761791));
#64044=CARTESIAN_POINT('Ctrl Pts',(0.252668522721909,0.357490108685591,
-0.385722769466417));
#64045=CARTESIAN_POINT('Ctrl Pts',(0.234056618747682,0.369947398846978,
-0.384910367171043));
#64046=CARTESIAN_POINT('Ctrl Pts',(0.214579520855051,0.380919242398723,
-0.384097964875668));
#64047=CARTESIAN_POINT('Ctrl Pts',(0.195116095478011,0.391883383945638,
-0.383286132869724));
#64048=CARTESIAN_POINT('Ctrl Pts',(0.174789283585532,0.401363765400864,
-0.382474300863779));
#64049=CARTESIAN_POINT('Ctrl Pts',(0.153852054252127,0.409235122395916,
-0.381662468857834));
#64050=CARTESIAN_POINT('Ctrl Pts',(0.132923776607731,0.41710311400108,-0.380850983949757));
#64051=CARTESIAN_POINT('Ctrl Pts',(0.111386269345724,0.42336319726535,-0.380039499041679));
#64052=CARTESIAN_POINT('Ctrl Pts',(0.0895111269731423,0.427938778504587,
-0.379228014133602));
#64053=CARTESIAN_POINT('Ctrl Pts',(0.0676112186894509,0.432519539981572,
-0.378415610504047));
#64054=CARTESIAN_POINT('Ctrl Pts',(0.0453736167109743,0.435411863787432,
-0.377603206874493));
#64055=CARTESIAN_POINT('Ctrl Pts',(0.023079508171655,0.436590398775047,
-0.376790803244939));
#64056=CARTESIAN_POINT('Ctrl Pts',(0.0123122882369146,0.437159587060376,
-0.376398442700907));
#64057=CARTESIAN_POINT('Ctrl Pts',(0.00153195052704815,0.437329808405186,
-0.376006082156876));
#64058=CARTESIAN_POINT('Ctrl Pts',(-0.00922985932074681,0.43710256198851,
-0.375613721612844));
#64059=CARTESIAN_POINT('Ctrl Pts',(-0.00922985932074711,0.43710256198851,
-0.475606184023132));
#64060=CARTESIAN_POINT('Ctrl Pts',(-0.031596657038163,0.436630264604921,
-0.474794237278421));
#64061=CARTESIAN_POINT('Ctrl Pts',(-0.0539235984025056,0.43443692052174,
-0.47398229053371));
#64062=CARTESIAN_POINT('Ctrl Pts',(-0.0759302021839514,0.430555971270059,
-0.473170343788999));
#64063=CARTESIAN_POINT('Ctrl Pts',(-0.0988896108466164,0.426506991211468,
-0.472323242741092));
#64064=CARTESIAN_POINT('Ctrl Pts',(-0.121499442488184,0.420620914447263,
-0.471476141693185));
#64065=CARTESIAN_POINT('Ctrl Pts',(-0.143455413350369,0.412994412045096,
-0.470629040645277));
#64066=CARTESIAN_POINT('Ctrl Pts',(-0.165411384212554,0.405367909642929,
-0.46978193959737));
#64067=CARTESIAN_POINT('Ctrl Pts',(-0.186712719534122,0.39600139295843,
-0.468934838549463));
#64068=CARTESIAN_POINT('Ctrl Pts',(-0.207081768033953,0.385046726187786,
-0.468087737501556));
#64069=CARTESIAN_POINT('Ctrl Pts',(-0.226651309261429,0.374522041983556,
-0.467273886089646));
#64070=CARTESIAN_POINT('Ctrl Pts',(-0.24547239624558,0.362471566139285,
-0.466460034677735));
#64071=CARTESIAN_POINT('Ctrl Pts',(-0.263296463456217,0.349025518166579,
-0.465646183265825));
#64072=CARTESIAN_POINT('Ctrl Pts',(-0.281088737272656,0.335603454366427,
-0.464833783548326));
#64073=CARTESIAN_POINT('Ctrl Pts',(-0.297886923090229,0.320791141461004,
-0.464021383830827));
#64074=CARTESIAN_POINT('Ctrl Pts',(-0.313469956409651,0.30476290198863,
-0.463208984113328));
#64075=CARTESIAN_POINT('Ctrl Pts',(-0.329036470054283,0.28875165415698,
-0.462397445626044));
#64076=CARTESIAN_POINT('Ctrl Pts',(-0.343389872413706,0.271527529831524,
-0.461585907138759));
#64077=CARTESIAN_POINT('Ctrl Pts',(-0.356344630186733,0.253302871158383,
-0.460774368651475));
#64078=CARTESIAN_POINT('Ctrl Pts',(-0.369305620306502,0.235069444865338,
-0.459962439744753));
#64079=CARTESIAN_POINT('Ctrl Pts',(-0.380866191846791,0.215835095032773,
-0.459150510838031));
#64080=CARTESIAN_POINT('Ctrl Pts',(-0.390882676100084,0.195843237117948,
-0.458338581931309));
#64081=CARTESIAN_POINT('Ctrl Pts',(-0.400901625535766,0.175846458956176,
-0.457526453198701));
#64082=CARTESIAN_POINT('Ctrl Pts',(-0.409375438908169,0.15509245518468,
-0.456714324466092));
#64083=CARTESIAN_POINT('Ctrl Pts',(-0.416207877534535,0.133846339801273,
-0.455902195733484));
#64084=CARTESIAN_POINT('Ctrl Pts',(-0.423055001685896,0.112554558386221,
-0.455088321425474));
#64085=CARTESIAN_POINT('Ctrl Pts',(-0.428253534660455,0.090769249199721,
-0.454274447117464));
#64086=CARTESIAN_POINT('Ctrl Pts',(-0.431757704996032,0.0687686278513655,
-0.453460572809453));
#64087=CARTESIAN_POINT('Ctrl Pts',(-0.433472753503982,0.0580008485472618,
-0.453062237744676));
#64088=CARTESIAN_POINT('Ctrl Pts',(-0.434782720481834,0.0471815993014252,
-0.452663902679899));
#64089=CARTESIAN_POINT('Ctrl Pts',(-0.435686785767368,0.0363437024489768,
-0.452265567615122));
#64090=CARTESIAN_POINT('Ctrl Pts',(-0.436688861601316,0.0243308592390448,
-0.451824048679914));
#64091=CARTESIAN_POINT('Ctrl Pts',(-0.437194189162464,0.0122760091762199,
-0.451382529744706));
#64092=CARTESIAN_POINT('Ctrl Pts',(-0.437199950177124,0.00020872259101247,
-0.450941010809498));
#64093=CARTESIAN_POINT('',(-0.43719982366506,-0.000392666831192225,-0.470658989187641));
#64094=CARTESIAN_POINT('Ctrl Pts',(-0.00922985932074758,0.43710256198851,
-0.495313704306577));
#64095=CARTESIAN_POINT('Ctrl Pts',(-0.03152725504041,0.436631730097763,
-0.494501615763862));
#64096=CARTESIAN_POINT('Ctrl Pts',(-0.0538264166591165,0.434449611184395,
-0.493689527221147));
#64097=CARTESIAN_POINT('Ctrl Pts',(-0.0758460144531191,0.430570809613909,
-0.492877438678432));
#64098=CARTESIAN_POINT('Ctrl Pts',(-0.0989662333703342,0.426498131162421,
-0.492024758939984));
#64099=CARTESIAN_POINT('Ctrl Pts',(-0.121777335796485,0.420554526014737,
-0.491172079201535));
#64100=CARTESIAN_POINT('Ctrl Pts',(-0.143961542459546,0.412818258187145,
-0.490319399463087));
#64101=CARTESIAN_POINT('Ctrl Pts',(-0.165085803368755,0.405451623782063,
-0.489507460161377));
#64102=CARTESIAN_POINT('Ctrl Pts',(-0.185641063095161,0.396460216974159,
-0.488695520859668));
#64103=CARTESIAN_POINT('Ctrl Pts',(-0.205370664093565,0.385962084057189,
-0.487883581557959));
#64104=CARTESIAN_POINT('Ctrl Pts',(-0.225109510264207,0.375459031778341,
-0.487071261786381));
#64105=CARTESIAN_POINT('Ctrl Pts',(-0.244021317172783,0.363448221097851,
-0.486258942014804));
#64106=CARTESIAN_POINT('Ctrl Pts',(-0.261876166526046,0.35009243551614,
-0.485446622243226));
#64107=CARTESIAN_POINT('Ctrl Pts',(-0.27976768974906,0.336709217143978,
-0.48463263396642));
#64108=CARTESIAN_POINT('Ctrl Pts',(-0.296597391328691,0.321975988816443,
-0.483818645689614));
#64109=CARTESIAN_POINT('Ctrl Pts',(-0.3121696267946,0.306094697939903,-0.483004657412808));
#64110=CARTESIAN_POINT('Ctrl Pts',(-0.314461339323845,0.303757502784972,
-0.482884865547555));
#64111=CARTESIAN_POINT('Ctrl Pts',(-0.316725888252609,0.301395502024436,
-0.482765073682303));
#64112=CARTESIAN_POINT('Ctrl Pts',(-0.318962724860187,0.299009398096054,
-0.48264528181705));
#64113=CARTESIAN_POINT('Ctrl Pts',(-0.333977798397273,0.282992347127554,
-0.48184116243711));
#64114=CARTESIAN_POINT('Ctrl Pts',(-0.347831425387404,0.265789959998062,
-0.48103704305717));
#64115=CARTESIAN_POINT('Ctrl Pts',(-0.360331303178404,0.247598852884567,
-0.48023292367723));
#64116=CARTESIAN_POINT('Ctrl Pts',(-0.372811195416129,0.229436830802655,
-0.479430089971516));
#64117=CARTESIAN_POINT('Ctrl Pts',(-0.383941167054413,0.210289786234671,
-0.478627256265802));
#64118=CARTESIAN_POINT('Ctrl Pts',(-0.393568659859785,0.190387893460095,
-0.477824422560088));
#64119=CARTESIAN_POINT('Ctrl Pts',(-0.403186140154464,0.170506698484859,
-0.477022423794605));
#64120=CARTESIAN_POINT('Ctrl Pts',(-0.411303899013268,0.149872859957529,
-0.476220425029121));
#64121=CARTESIAN_POINT('Ctrl Pts',(-0.41781511838112,0.12874147292994,-0.475418426263638));
#64122=CARTESIAN_POINT('Ctrl Pts',(-0.424331811700911,0.107592320843235,
-0.474615753261511));
#64123=CARTESIAN_POINT('Ctrl Pts',(-0.429239034539328,0.0859454832553259,
-0.473813080259383));
#64124=CARTESIAN_POINT('Ctrl Pts',(-0.432479564362781,0.0640723529190212,
-0.473010407257255));
#64125=CARTESIAN_POINT('Ctrl Pts',(-0.435643924923276,0.0427133546250252,
-0.472226601235004));
#64126=CARTESIAN_POINT('Ctrl Pts',(-0.43721916236399,0.0211392701264403,
-0.471442795212753));
#64127=CARTESIAN_POINT('Ctrl Pts',(-0.437199823665131,-0.000392666752592153,
-0.470658989190502));
#64128=CARTESIAN_POINT('Ctrl Pts',(-0.43719982366506,-0.000392666831191846,
-0.470658989187641));
#64129=CARTESIAN_POINT('Ctrl Pts',(-0.437173552585976,-0.0296431922912459,
-0.469594210940398));
#64130=CARTESIAN_POINT('Ctrl Pts',(-0.434207981134181,-0.0587635782881525,
-0.468529432693157));
#64131=CARTESIAN_POINT('Ctrl Pts',(-0.428402952386622,-0.08726253713035,
-0.467464654445915));
#64132=CARTESIAN_POINT('Ctrl Pts',(-0.427237084359252,-0.0929861995568984,
-0.467250806940815));
#64133=CARTESIAN_POINT('Ctrl Pts',(-0.425956834269805,-0.0986848733356714,
-0.467036959435715));
#64134=CARTESIAN_POINT('Ctrl Pts',(-0.424563234051596,-0.104354685048875,
-0.466823111930615));
#64135=CARTESIAN_POINT('Ctrl Pts',(-0.419259533671851,-0.12593259680828,
-0.466009260813785));
#64136=CARTESIAN_POINT('Ctrl Pts',(-0.41229146880438,-0.147166837152214,
-0.465195409696954));
#64137=CARTESIAN_POINT('Ctrl Pts',(-0.40372305330094,-0.167784195421876,
-0.464381558580123));
#64138=CARTESIAN_POINT('Ctrl Pts',(-0.39516992165499,-0.188364777607852,
-0.463569159165125));
#64139=CARTESIAN_POINT('Ctrl Pts',(-0.385022325946846,-0.208329987179689,
-0.462756759750126));
#64140=CARTESIAN_POINT('Ctrl Pts',(-0.373393853815011,-0.227422228318109,
-0.461944360335128));
#64141=CARTESIAN_POINT('Ctrl Pts',(-0.361777709198173,-0.246494229489809,
-0.461132822156744));
#64142=CARTESIAN_POINT('Ctrl Pts',(-0.348684151388529,-0.264694477016946,
-0.46032128397836));
#64143=CARTESIAN_POINT('Ctrl Pts',(-0.334272456697672,-0.281790284951954,
-0.459509745799976));
#64144=CARTESIAN_POINT('Ctrl Pts',(-0.319853828853012,-0.298894317309442,
-0.458697817208173));
#64145=CARTESIAN_POINT('Ctrl Pts',(-0.304116244236127,-0.314892289514549,
-0.45788588861637));
#64146=CARTESIAN_POINT('Ctrl Pts',(-0.287259523413783,-0.329584293023933,
-0.457073960024566));
#64147=CARTESIAN_POINT('Ctrl Pts',(-0.270398654019511,-0.344279912351244,
-0.456261831610733));
#64148=CARTESIAN_POINT('Ctrl Pts',(-0.252418660021591,-0.35766847690647,
-0.4554497031969));
#64149=CARTESIAN_POINT('Ctrl Pts',(-0.233552218507466,-0.369590585959979,
-0.454637574783067));
#64150=CARTESIAN_POINT('Ctrl Pts',(-0.214645225799104,-0.381538320182898,
-0.453823700794849));
#64151=CARTESIAN_POINT('Ctrl Pts',(-0.194848612001848,-0.392012964846112,
-0.453009826806631));
#64152=CARTESIAN_POINT('Ctrl Pts',(-0.174420344756774,-0.400900715059138,
-0.452195952818412));
#64153=CARTESIAN_POINT('Ctrl Pts',(-0.164422073193806,-0.405250674805973,
-0.451797615893668));
#64154=CARTESIAN_POINT('Ctrl Pts',(-0.154272792737645,-0.409221240741445,
-0.451399278968925));
#64155=CARTESIAN_POINT('Ctrl Pts',(-0.144004081235465,-0.412803421240098,
-0.451000942044181));
#64156=CARTESIAN_POINT('Ctrl Pts',(-0.123023833918062,-0.420122258932769,
-0.450187090452869));
#64157=CARTESIAN_POINT('Ctrl Pts',(-0.101424225607706,-0.425858497932171,
-0.449373238861556));
#64158=CARTESIAN_POINT('Ctrl Pts',(-0.0794691881014299,-0.429916838635683,
-0.448559387270244));
#64159=CARTESIAN_POINT('Ctrl Pts',(-0.0575533124497425,-0.433967940355956,
-0.447746987370266));
#64160=CARTESIAN_POINT('Ctrl Pts',(-0.0352839517474037,-0.436346901387538,
-0.446934587470287));
#64161=CARTESIAN_POINT('Ctrl Pts',(-0.012938976963878,-0.43700849290961,
-0.446122187570308));
#64162=CARTESIAN_POINT('Ctrl Pts',(0.00938230983974245,-0.437669383076373,
-0.445310648898086));
#64163=CARTESIAN_POINT('Ctrl Pts',(0.0317783408244336,-0.436616469221204,
-0.444499110225864));
#64164=CARTESIAN_POINT('Ctrl Pts',(0.0539672160245315,-0.433856404348906,
-0.443687571553642));
#64165=CARTESIAN_POINT('Ctrl Pts',(0.0761667660106505,-0.431095011644455,
-0.442875642460473));
#64166=CARTESIAN_POINT('Ctrl Pts',(0.0981582487386274,-0.426624897012567,
-0.442063713367304));
#64167=CARTESIAN_POINT('Ctrl Pts',(0.119665135370166,-0.420504572361395,
-0.441251784274134));
#64168=CARTESIAN_POINT('Ctrl Pts',(0.141177315144382,-0.414382741413558,
-0.44043965535397));
#64169=CARTESIAN_POINT('Ctrl Pts',(0.162203982046089,-0.406610117993494,
-0.439627526433805));
#64170=CARTESIAN_POINT('Ctrl Pts',(0.182484650225093,-0.397294843198632,
-0.438815397513641));
#64171=CARTESIAN_POINT('Ctrl Pts',(0.202808909279719,-0.387959546332437,
-0.438001523019295));
#64172=CARTESIAN_POINT('Ctrl Pts',(0.222383338673432,-0.37707532065262,
-0.437187648524949));
#64173=CARTESIAN_POINT('Ctrl Pts',(0.240971885936293,-0.364796368112823,
-0.436373774030604));
#64174=CARTESIAN_POINT('Ctrl Pts',(0.250069664093788,-0.358786689968868,
-0.435975440072985));
#64175=CARTESIAN_POINT('Ctrl Pts',(0.258931738409619,-0.352443572121148,
-0.435577106115366));
#64176=CARTESIAN_POINT('Ctrl Pts',(0.267533354777696,-0.345788582925162,
-0.435178772157747));
#64177=CARTESIAN_POINT('Ctrl Pts',(0.28510764763195,-0.332191518830764,
-0.434364920745939));
#64178=CARTESIAN_POINT('Ctrl Pts',(0.301692959607839,-0.317212376336345,
-0.433551069334132));
#64179=CARTESIAN_POINT('Ctrl Pts',(0.317065499398493,-0.301020446300886,
-0.432737217922324));
#64180=CARTESIAN_POINT('Ctrl Pts',(0.332410618667629,-0.284857398361162,
-0.43192481820493));
#64181=CARTESIAN_POINT('Ctrl Pts',(0.346546732292667,-0.267486331847394,
-0.431112418487537));
#64182=CARTESIAN_POINT('Ctrl Pts',(0.3592844226865,-0.249115522629217,-0.430300018770144));
#64183=CARTESIAN_POINT('Ctrl Pts',(0.372008609772009,-0.230764188425222,
-0.429488480282968));
#64184=CARTESIAN_POINT('Ctrl Pts',(0.383336888246875,-0.211415784750808,
-0.428676941795792));
#64185=CARTESIAN_POINT('Ctrl Pts',(0.393121135724313,-0.191310252330675,
-0.427865403308615));
#64186=CARTESIAN_POINT('Ctrl Pts',(0.402910090261781,-0.17119504742952,
-0.427053474402004));
#64187=CARTESIAN_POINT('Ctrl Pts',(0.41115319997167,-0.150322621360285,
-0.426241545495393));
#64188=CARTESIAN_POINT('Ctrl Pts',(0.417748743659805,-0.128956687188586,
-0.425429616588782));
#64189=CARTESIAN_POINT('Ctrl Pts',(0.424345910593941,-0.107585494592584,
-0.424617487856286));
#64190=CARTESIAN_POINT('Ctrl Pts',(0.429294523396063,-0.0857212448492418,
-0.42380535912379));
#64191=CARTESIAN_POINT('Ctrl Pts',(0.432543211513634,-0.0636412615641114,
-0.422993230391294));
#64192=CARTESIAN_POINT('Ctrl Pts',(0.435798882305056,-0.0415138199461588,
-0.422179356083397));
#64193=CARTESIAN_POINT('Ctrl Pts',(0.437347277372875,-0.0191704335859931,
-0.4213654817755));
#64194=CARTESIAN_POINT('Ctrl Pts',(0.437188960185798,0.00310694249401093,
-0.420551607467603));
#64195=CARTESIAN_POINT('Ctrl Pts',(0.437111474895426,0.0140101740769806,
-0.420153272402173));
#64196=CARTESIAN_POINT('Ctrl Pts',(0.43662595656848,0.0248976182249839,
-0.419754937336743));
#64197=CARTESIAN_POINT('Ctrl Pts',(0.435736989139207,0.0357367639259372,
-0.419356602271314));
#64198=CARTESIAN_POINT('Ctrl Pts',(0.433920710848475,0.0578825753229286,
-0.418542750933284));
#64199=CARTESIAN_POINT('Ctrl Pts',(0.430406633419485,0.079952882377742,
-0.417728899595255));
#64200=CARTESIAN_POINT('Ctrl Pts',(0.425214654265534,0.101667781513332,
-0.416915048257226));
#64201=CARTESIAN_POINT('Ctrl Pts',(0.420031936227625,0.123343947018685,
-0.416102648614486));
#64202=CARTESIAN_POINT('Ctrl Pts',(0.413177367857804,0.14466526188217,-0.415290248971747));
#64203=CARTESIAN_POINT('Ctrl Pts',(0.404722268735889,0.165359381920938,
-0.414477849329007));
#64204=CARTESIAN_POINT('Ctrl Pts',(0.396276132926945,0.186031563970348,
-0.413666310917124));
#64205=CARTESIAN_POINT('Ctrl Pts',(0.386233078348518,0.206077201652903,
-0.412854772505241));
#64206=CARTESIAN_POINT('Ctrl Pts',(0.374713484125949,0.225241303526223,
-0.412043234093357));
#64207=CARTESIAN_POINT('Ctrl Pts',(0.363188347994157,0.244414624970205,
-0.411231305262148));
#64208=CARTESIAN_POINT('Ctrl Pts',(0.350185605792639,0.262704940483676,
-0.410419376430939));
#64209=CARTESIAN_POINT('Ctrl Pts',(0.335870863915565,0.279883194873526,
-0.40960744759973));
#64210=CARTESIAN_POINT('Ctrl Pts',(0.321552599003601,0.297065677044085,
-0.408795318942801));
#64211=CARTESIAN_POINT('Ctrl Pts',(0.305922173702576,0.313135023897119,
-0.407983190285872));
#64212=CARTESIAN_POINT('Ctrl Pts',(0.28918405650235,0.327896967757931,-0.407171061628943));
#64213=CARTESIAN_POINT('Ctrl Pts',(0.272409962661738,0.34269064070388,-0.406357187395717));
#64214=CARTESIAN_POINT('Ctrl Pts',(0.254523991886672,0.356170863517118,
-0.405543313162491));
#64215=CARTESIAN_POINT('Ctrl Pts',(0.235762810969417,0.368184379032841,
-0.404729438929265));
#64216=CARTESIAN_POINT('Ctrl Pts',(0.226580502015823,0.374064169413345,
-0.40433110341447));
#64217=CARTESIAN_POINT('Ctrl Pts',(0.217188956300894,0.379593301930375,
-0.403932767899674));
#64218=CARTESIAN_POINT('Ctrl Pts',(0.207617926817868,0.384757893309352,
-0.403534432384878));
#64219=CARTESIAN_POINT('Ctrl Pts',(0.188063231238235,0.395309737537622,
-0.402720587882132));
#64220=CARTESIAN_POINT('Ctrl Pts',(0.167646158475161,0.404397194139404,
-0.401906743379385));
#64221=CARTESIAN_POINT('Ctrl Pts',(0.14661219073182,0.411884335134048,-0.401092898876639));
#64222=CARTESIAN_POINT('Ctrl Pts',(0.125615611123411,0.419358167643997,
-0.40028050099245));
#64223=CARTESIAN_POINT('Ctrl Pts',(0.104004961028189,0.425237041178104,
-0.399468103108262));
#64224=CARTESIAN_POINT('Ctrl Pts',(0.0820474268363558,0.429432252805414,
-0.398655705224073));
#64225=CARTESIAN_POINT('Ctrl Pts',(0.0601107828488583,0.433623473145389,
-0.397844080248065));
#64226=CARTESIAN_POINT('Ctrl Pts',(0.0378286035179152,0.436134047399237,
-0.397032455272057));
#64227=CARTESIAN_POINT('Ctrl Pts',(0.0154803688227484,0.436925849751547,
-0.396220830296049));
#64228=CARTESIAN_POINT('Ctrl Pts',(0.00724780578029177,0.437217531079915,
-0.395921846780216));
#64229=CARTESIAN_POINT('Ctrl Pts',(-0.000993645708467723,0.437276477905706,
-0.395622863264383));
#64230=CARTESIAN_POINT('Ctrl Pts',(-0.0092298593207473,0.43710256198851,
-0.39532387974855));
#64231=CARTESIAN_POINT('Origin',(0.,0.,-0.920658989190502));
#64232=CARTESIAN_POINT('',(-0.00922985932074603,0.43710256198851,-0.275596058510812));
#64233=CARTESIAN_POINT('',(-0.00922985932074758,0.43710256198851,-0.295331813926952));
#64234=CARTESIAN_POINT('',(-0.00922985932074702,0.43710256198851,-0.920658989190502));
#64235=CARTESIAN_POINT('',(-0.437199947496373,0.000214264250231113,-0.350941010812191));
#64236=CARTESIAN_POINT('Ctrl Pts',(-0.437199947496409,0.000214264175926867,
-0.350941010809498));
#64237=CARTESIAN_POINT('Ctrl Pts',(-0.437211089295146,-0.022520258763288,
-0.350117162487918));
#64238=CARTESIAN_POINT('Ctrl Pts',(-0.43544457971145,-0.0452520109580569,
-0.349293314166337));
#64239=CARTESIAN_POINT('Ctrl Pts',(-0.431927926938213,-0.0676912544636132,
-0.348469465844757));
#64240=CARTESIAN_POINT('Ctrl Pts',(-0.428409577883707,-0.0901413216901649,
-0.347645220134362));
#64241=CARTESIAN_POINT('Ctrl Pts',(-0.423139546600431,-0.112297926406255,
-0.346820974423967));
#64242=CARTESIAN_POINT('Ctrl Pts',(-0.416196537937162,-0.133881596230103,
-0.345996728713572));
#64243=CARTESIAN_POINT('Ctrl Pts',(-0.409234442445989,-0.155524601107592,
-0.345170217092707));
#64244=CARTESIAN_POINT('Ctrl Pts',(-0.400590430497763,-0.176590881432304,
-0.344343705471842));
#64245=CARTESIAN_POINT('Ctrl Pts',(-0.390392136003001,-0.196819257561384,
-0.343517193850977));
#64246=CARTESIAN_POINT('Ctrl Pts',(-0.382138130313612,-0.213191125596992,
-0.342848255370678));
#64247=CARTESIAN_POINT('Ctrl Pts',(-0.372867007592829,-0.229014402602027,
-0.342179316890379));
#64248=CARTESIAN_POINT('Ctrl Pts',(-0.362667230495944,-0.244164534534403,
-0.341510378410081));
#64249=CARTESIAN_POINT('Ctrl Pts',(-0.350257857036033,-0.262596667249655,
-0.340696526563625));
#64250=CARTESIAN_POINT('Ctrl Pts',(-0.336404235292047,-0.280133047453723,
-0.33988267471717));
#64251=CARTESIAN_POINT('Ctrl Pts',(-0.321260540146733,-0.296539213839636,
-0.339068822870715));
#64252=CARTESIAN_POINT('Ctrl Pts',(-0.306143857926695,-0.312916115337265,
-0.338256422751787));
#64253=CARTESIAN_POINT('Ctrl Pts',(-0.289742109223225,-0.328166247186758,
-0.33744402263286));
#64254=CARTESIAN_POINT('Ctrl Pts',(-0.27225063444735,-0.342086877917022,
-0.336631622513932));
#64255=CARTESIAN_POINT('Ctrl Pts',(-0.254777703215119,-0.355992750725109,
-0.335820083658978));
#64256=CARTESIAN_POINT('Ctrl Pts',(-0.236217879135763,-0.368571455511955,
-0.335008544804023));
#64257=CARTESIAN_POINT('Ctrl Pts',(-0.21680082004648,-0.379659379480046,
-0.334197005949068));
#64258=CARTESIAN_POINT('Ctrl Pts',(-0.197374420979929,-0.390752636951906,
-0.333385076728383));
#64259=CARTESIAN_POINT('Ctrl Pts',(-0.177090575262683,-0.400353310004381,
-0.332573147507699));
#64260=CARTESIAN_POINT('Ctrl Pts',(-0.156205719281849,-0.408342519539222,
-0.331761218287014));
#64261=CARTESIAN_POINT('Ctrl Pts',(-0.135315724054299,-0.416333695021011,
-0.330949089270621));
#64262=CARTESIAN_POINT('Ctrl Pts',(-0.113825103464974,-0.422712391422751,
-0.330136960254228));
#64263=CARTESIAN_POINT('Ctrl Pts',(-0.0920071930443114,-0.427409073871984,
-0.329324831237835));
#64264=CARTESIAN_POINT('Ctrl Pts',(-0.0701423889445194,-0.43211585099644,
-0.328510956696011));
#64265=CARTESIAN_POINT('Ctrl Pts',(-0.0479495998776903,-0.435133293229205,
-0.327697082154186));
#64266=CARTESIAN_POINT('Ctrl Pts',(-0.0257102052507155,-0.436443381604036,
-0.326883207612362));
#64267=CARTESIAN_POINT('Ctrl Pts',(-0.0148256217155885,-0.437084575602048,
-0.32648487458279));
#64268=CARTESIAN_POINT('Ctrl Pts',(-0.00392990203914814,-0.437317587185639,
-0.326086541553219));
#64269=CARTESIAN_POINT('Ctrl Pts',(0.00694421185564129,-0.437144847758388,
-0.325688208523647));
#64270=CARTESIAN_POINT('Ctrl Pts',(0.0291618100177887,-0.436791912777334,
-0.324874348813205));
#64271=CARTESIAN_POINT('Ctrl Pts',(0.0514159432842557,-0.434739857967319,
-0.324060489102762));
#64272=CARTESIAN_POINT('Ctrl Pts',(0.0734260003306082,-0.430990095565373,
-0.32324662939232));
#64273=CARTESIAN_POINT('Ctrl Pts',(0.0953967989195519,-0.427247021464472,
-0.322434221330853));
#64274=CARTESIAN_POINT('Ctrl Pts',(0.117123678599569,-0.421812314603624,
-0.321621813269387));
#64275=CARTESIAN_POINT('Ctrl Pts',(0.138330183008807,-0.414739195722746,
-0.32080940520792));
#64276=CARTESIAN_POINT('Ctrl Pts',(0.159514206969538,-0.407673574866139,
-0.319997858358526));
#64277=CARTESIAN_POINT('Ctrl Pts',(0.180178266695892,-0.398973188936921,
-0.319186311509131));
#64278=CARTESIAN_POINT('Ctrl Pts',(0.200059988304416,-0.388741354990226,
-0.318374764659736));
#64279=CARTESIAN_POINT('Ctrl Pts',(0.219951272906357,-0.37850459959042,
-0.317562827460988));
#64280=CARTESIAN_POINT('Ctrl Pts',(0.239058822880429,-0.366735235436711,
-0.316750890262239));
#64281=CARTESIAN_POINT('Ctrl Pts',(0.257143164034255,-0.3535834175841,-0.315938953063491));
#64282=CARTESIAN_POINT('Ctrl Pts',(0.275231955281206,-0.340428363406001,
-0.315126816067796));
#64283=CARTESIAN_POINT('Ctrl Pts',(0.292296476518162,-0.325890624459326,
-0.314314679072101));
#64284=CARTESIAN_POINT('Ctrl Pts',(0.308129404466762,-0.310161425878458,
-0.313502542076406));
#64285=CARTESIAN_POINT('Ctrl Pts',(0.323996359718719,-0.294398422923984,
-0.312688659678217));
#64286=CARTESIAN_POINT('Ctrl Pts',(0.338625963946799,-0.277439386363242,
-0.311874777280029));
#64287=CARTESIAN_POINT('Ctrl Pts',(0.351849693310249,-0.25951037227341,
-0.31106089488184));
#64288=CARTESIAN_POINT('Ctrl Pts',(0.358320921275683,-0.250736543485635,
-0.310662609466964));
#64289=CARTESIAN_POINT('Ctrl Pts',(0.364456125959481,-0.241730884102552,
-0.310264324052088));
#64290=CARTESIAN_POINT('Ctrl Pts',(0.37023949937262,-0.232522156157885,
-0.309866038637212));
#64291=CARTESIAN_POINT('Ctrl Pts',(0.382056895684477,-0.213705597053647,
-0.309052206249676));
#64292=CARTESIAN_POINT('Ctrl Pts',(0.392469966357593,-0.193932044311778,
-0.308238373862141));
#64293=CARTESIAN_POINT('Ctrl Pts',(0.401326898651035,-0.173437482739868,
-0.307424541474605));
#64294=CARTESIAN_POINT('Ctrl Pts',(0.410168032450458,-0.152979478205733,
-0.306612160755173));
#64295=CARTESIAN_POINT('Ctrl Pts',(0.417458205930442,-0.131803645208973,
-0.305799780035741));
#64296=CARTESIAN_POINT('Ctrl Pts',(0.423091301325727,-0.110170734510135,
-0.304987399316309));
#64297=CARTESIAN_POINT('Ctrl Pts',(0.428718425496042,-0.0885607552490719,
-0.304175879741186));
#64298=CARTESIAN_POINT('Ctrl Pts',(0.432691752470204,-0.0664953421261078,
-0.303364360166062));
#64299=CARTESIAN_POINT('Ctrl Pts',(0.434954837451626,-0.0442507556707181,
-0.302552840590939));
#64300=CARTESIAN_POINT('Ctrl Pts',(0.437219012156079,-0.0219954579789519,
-0.301740930252066));
#64301=CARTESIAN_POINT('Ctrl Pts',(0.437771208707934,0.00043847537874489,
-0.300929019913194));
#64302=CARTESIAN_POINT('Ctrl Pts',(0.436606731545274,0.0227684424006747,
-0.300117109574321));
#64303=CARTESIAN_POINT('Ctrl Pts',(0.435441967537652,0.0451039099500344,
-0.29930499923806));
#64304=CARTESIAN_POINT('Ctrl Pts',(0.432559756713184,0.0673346474730818,
-0.2984928889018));
#64305=CARTESIAN_POINT('Ctrl Pts',(0.428007361644517,0.0891826125323723,
-0.297680778565539));
#64306=CARTESIAN_POINT('Ctrl Pts',(0.423445178452432,0.111077552991472,
-0.296866922107494));
#64307=CARTESIAN_POINT('Ctrl Pts',(0.417205834699874,0.132587387596294,
-0.296053065649448));
#64308=CARTESIAN_POINT('Ctrl Pts',(0.409386945720571,0.153447608888449,
-0.295239209191403));
#64309=CARTESIAN_POINT('Ctrl Pts',(0.405558983960924,0.163660329597941,
-0.294840762377861));
#64310=CARTESIAN_POINT('Ctrl Pts',(0.401353165163034,0.173717644055453,
-0.294442315564319));
#64311=CARTESIAN_POINT('Ctrl Pts',(0.396785001936018,0.183590583197054,
-0.294043868750778));
#64312=CARTESIAN_POINT('Ctrl Pts',(0.387454150385809,0.203756878689673,
-0.293230008150127));
#64313=CARTESIAN_POINT('Ctrl Pts',(0.376555297387723,0.223267664750025,
-0.292416147549476));
#64314=CARTESIAN_POINT('Ctrl Pts',(0.364203505370233,0.241867002040449,
-0.291602286948825));
#64315=CARTESIAN_POINT('Ctrl Pts',(0.351873748820917,0.260433158307072,
-0.290789878267));
#64316=CARTESIAN_POINT('Ctrl Pts',(0.338096543508109,0.278090473234571,
-0.289977469585175));
#64317=CARTESIAN_POINT('Ctrl Pts',(0.323032626525938,0.294607810826111,
-0.28916506090335));
#64318=CARTESIAN_POINT('Ctrl Pts',(0.307984683331389,0.311107633421845,
-0.288353513700233));
#64319=CARTESIAN_POINT('Ctrl Pts',(0.291653196375196,0.326469333806669,
-0.287541966497116));
#64320=CARTESIAN_POINT('Ctrl Pts',(0.274238987269211,0.340494960111831,
-0.286730419294));
#64321=CARTESIAN_POINT('Ctrl Pts',(0.256816410500093,0.354527325839693,
-0.28591848213613));
#64322=CARTESIAN_POINT('Ctrl Pts',(0.238310617794821,0.367221871584436,
-0.28510654497826));
#64323=CARTESIAN_POINT('Ctrl Pts',(0.218955961826285,0.378420568654409,
-0.28429460782039));
#64324=CARTESIAN_POINT('Ctrl Pts',(0.199596548531911,0.389622018336003,
-0.283482471090406));
#64325=CARTESIAN_POINT('Ctrl Pts',(0.17938849147353,0.399326556419703,-0.282670334360422));
#64326=CARTESIAN_POINT('Ctrl Pts',(0.158590651123122,0.407422195488101,
-0.281858197630437));
#64327=CARTESIAN_POINT('Ctrl Pts',(0.137748121701303,0.415535229948826,
-0.281044315832902));
#64328=CARTESIAN_POINT('Ctrl Pts',(0.1163139628022,0.42203224894274,-0.280230434035367));
#64329=CARTESIAN_POINT('Ctrl Pts',(0.0945631436825621,0.426850854347126,
-0.279416552237832));
#64330=CARTESIAN_POINT('Ctrl Pts',(0.0839190756782834,0.429208906396934,
-0.279018267780003));
#64331=CARTESIAN_POINT('Ctrl Pts',(0.0731993284726913,0.431165798971983,
-0.278619983322173));
#64332=CARTESIAN_POINT('Ctrl Pts',(0.0624366031354644,0.432718743052464,
-0.278221698864344));
#64333=CARTESIAN_POINT('Ctrl Pts',(0.0404381850287124,0.435892875264188,
-0.277407627357897));
#64334=CARTESIAN_POINT('Ctrl Pts',(0.0181342531020704,0.437394274199899,
-0.27659355585145));
#64335=CARTESIAN_POINT('Ctrl Pts',(-0.00419770291906552,0.437179847763141,
-0.275779484345003));
#64336=CARTESIAN_POINT('Ctrl Pts',(-0.00587497476798022,0.437163742974752,
-0.275718342400273));
#64337=CARTESIAN_POINT('Ctrl Pts',(-0.00755240007482553,0.437137983224171,
-0.275657200455542));
#64338=CARTESIAN_POINT('Ctrl Pts',(-0.00922985932074603,0.43710256198851,
-0.275596058510812));
#64339=CARTESIAN_POINT('Ctrl Pts',(-0.00922985932074681,0.43710256198851,
-0.375613721612844));
#64340=CARTESIAN_POINT('Ctrl Pts',(-0.0317120106057848,0.436627828798559,
-0.374794053802879));
#64341=CARTESIAN_POINT('Ctrl Pts',(-0.0541124227825446,0.43441512874084,
-0.373974385992914));
#64342=CARTESIAN_POINT('Ctrl Pts',(-0.0761493254630166,0.430517270538044,
-0.373154718182949));
#64343=CARTESIAN_POINT('Ctrl Pts',(-0.0980298880315945,0.426647065567484,
-0.372340865480442));
#64344=CARTESIAN_POINT('Ctrl Pts',(-0.11967720422635,0.42109345977911,-0.371527012777935));
#64345=CARTESIAN_POINT('Ctrl Pts',(-0.140814437977076,0.413902324295479,
-0.370713160075428));
#64346=CARTESIAN_POINT('Ctrl Pts',(-0.16191396871899,0.406724015818812,
-0.369900759062199));
#64347=CARTESIAN_POINT('Ctrl Pts',(-0.182504535270659,0.397914150857145,
-0.369088358048971));
#64348=CARTESIAN_POINT('Ctrl Pts',(-0.202321615710707,0.387569095538085,
-0.368275957035743));
#64349=CARTESIAN_POINT('Ctrl Pts',(-0.22211768799125,0.377235007050031,
-0.367464417251802));
#64350=CARTESIAN_POINT('Ctrl Pts',(-0.241141258078628,0.365369263937545,
-0.366652877467861));
#64351=CARTESIAN_POINT('Ctrl Pts',(-0.259149649006979,0.352115463192913,
-0.36584133768392));
#64352=CARTESIAN_POINT('Ctrl Pts',(-0.277166703195314,0.338855286469323,
-0.365029407494186));
#64353=CARTESIAN_POINT('Ctrl Pts',(-0.294167015236909,0.324206127234508,
-0.364217477304452));
#64354=CARTESIAN_POINT('Ctrl Pts',(-0.309937942529275,0.308354198578064,
-0.363405547114719));
#64355=CARTESIAN_POINT('Ctrl Pts',(-0.325712751120537,0.292498368687908,
-0.362593417105172));
#64356=CARTESIAN_POINT('Ctrl Pts',(-0.340257090489989,0.275439709384688,
-0.361781287095625));
#64357=CARTESIAN_POINT('Ctrl Pts',(-0.353396572576067,0.25739988828958,
-0.360969157086077));
#64358=CARTESIAN_POINT('Ctrl Pts',(-0.366564295920897,0.239321293424545,
-0.360155281530276));
#64359=CARTESIAN_POINT('Ctrl Pts',(-0.37832075156722,0.220257932975055,
-0.359341405974474));
#64360=CARTESIAN_POINT('Ctrl Pts',(-0.388535381537813,0.200459714888717,
-0.358527530418673));
#64361=CARTESIAN_POINT('Ctrl Pts',(-0.393534630752391,0.190770061273941,
-0.35812920304462));
#64362=CARTESIAN_POINT('Ctrl Pts',(-0.398165279852222,0.180904733858332,
-0.357730875670568));
#64363=CARTESIAN_POINT('Ctrl Pts',(-0.402416276549772,0.170894646984093,
-0.357332548296515));
#64364=CARTESIAN_POINT('Ctrl Pts',(-0.412033637771879,0.148248047096182,
-0.356431381225949));
#64365=CARTESIAN_POINT('Ctrl Pts',(-0.419751737952197,0.124749261219136,
-0.355530214155383));
#64366=CARTESIAN_POINT('Ctrl Pts',(-0.425441532179863,0.1007141633359,-0.354629047084817));
#64367=CARTESIAN_POINT('Ctrl Pts',(-0.43109173274687,0.0768463188666618,
-0.353734150979732));
#64368=CARTESIAN_POINT('Ctrl Pts',(-0.434741554040949,0.0524500065223676,
-0.352839254874646));
#64369=CARTESIAN_POINT('Ctrl Pts',(-0.436311747948595,0.0278549565076211,
-0.35194435876956));
#64370=CARTESIAN_POINT('Ctrl Pts',(-0.436898576162864,0.0186630540236529,
-0.351609909450437));
#64371=CARTESIAN_POINT('Ctrl Pts',(-0.437195424372157,0.00944356716727992,
-0.351275460131314));
#64372=CARTESIAN_POINT('Ctrl Pts',(-0.437199947496373,0.000214264250231167,
-0.350941010812191));
#64373=CARTESIAN_POINT('',(-0.437199956252192,0.000195583950560346,-0.37065898918853));
#64374=CARTESIAN_POINT('Ctrl Pts',(-0.0092298593207473,0.43710256198851,
-0.39532387974855));
#64375=CARTESIAN_POINT('Ctrl Pts',(-0.0315967145607968,0.436630263390273,
-0.394511938566279));
#64376=CARTESIAN_POINT('Ctrl Pts',(-0.0539244619775135,0.434436892463301,
-0.393699997384007));
#64377=CARTESIAN_POINT('Ctrl Pts',(-0.0759325594972625,0.430555555542133,
-0.392888056201736));
#64378=CARTESIAN_POINT('Ctrl Pts',(-0.0979513364331321,0.426672335204552,
-0.392075721025493));
#64379=CARTESIAN_POINT('Ctrl Pts',(-0.119649459095544,0.421099685297624,
-0.391263385849249));
#64380=CARTESIAN_POINT('Ctrl Pts',(-0.140758031335858,0.413921510209911,
-0.390451050673006));
#64381=CARTESIAN_POINT('Ctrl Pts',(-0.16190982507083,0.406728637232986,
-0.389637052175337));
#64382=CARTESIAN_POINT('Ctrl Pts',(-0.182469006676033,0.39792396999991,
-0.388823053677668));
#64383=CARTESIAN_POINT('Ctrl Pts',(-0.202187227238474,0.387639220334601,
-0.388009055179999));
#64384=CARTESIAN_POINT('Ctrl Pts',(-0.204583719604231,0.386389243239631,
-0.387910124286147));
#64385=CARTESIAN_POINT('Ctrl Pts',(-0.206967823593862,0.385117457043982,
-0.387811193392296));
#64386=CARTESIAN_POINT('Ctrl Pts',(-0.209339122541238,0.383824141728558,
-0.387712262498445));
#64387=CARTESIAN_POINT('Ctrl Pts',(-0.228846531848669,0.37318472772745,
-0.386898410899664));
#64388=CARTESIAN_POINT('Ctrl Pts',(-0.247596540127881,0.361023942572635,
-0.386084559300883));
#64389=CARTESIAN_POINT('Ctrl Pts',(-0.265341350695688,0.34747346317523,
-0.385270707702102));
#64390=CARTESIAN_POINT('Ctrl Pts',(-0.28305450925764,0.333947154216364,
-0.384458307797352));
#64391=CARTESIAN_POINT('Ctrl Pts',(-0.299765433088831,0.319036456730761,
-0.383645907892601));
#64392=CARTESIAN_POINT('Ctrl Pts',(-0.315254085039217,0.302916988407858,
-0.382833507987851));
#64393=CARTESIAN_POINT('Ctrl Pts',(-0.330726317368614,0.286814608438495,
-0.38202196931354));
#64394=CARTESIAN_POINT('Ctrl Pts',(-0.344978336906196,0.269506495667498,
-0.381210430639228));
#64395=CARTESIAN_POINT('Ctrl Pts',(-0.357825860337883,0.25120607809815,
-0.380398891964917));
#64396=CARTESIAN_POINT('Ctrl Pts',(-0.370679564486306,0.232896856520951,
-0.379586962873676));
#64397=CARTESIAN_POINT('Ctrl Pts',(-0.382126996289671,0.213594951382642,
-0.378775033782434));
#64398=CARTESIAN_POINT('Ctrl Pts',(-0.392025918765554,0.193544617636407,
-0.377963104691192));
#64399=CARTESIAN_POINT('Ctrl Pts',(-0.401927277475406,0.17348934928196,
-0.377150975775248));
#64400=CARTESIAN_POINT('Ctrl Pts',(-0.410279079762644,0.152685940947287,
-0.376338846859304));
#64401=CARTESIAN_POINT('Ctrl Pts',(-0.41698664526085,0.131400067253036,
-0.375526717943361));
#64402=CARTESIAN_POINT('Ctrl Pts',(-0.423708627842109,0.110068442203989,
-0.374712843456683));
#64403=CARTESIAN_POINT('Ctrl Pts',(-0.428779149029836,0.088252978039073,
-0.373898968970005));
#64404=CARTESIAN_POINT('Ctrl Pts',(-0.432154071737152,0.0662321544342359,
-0.373085094483327));
#64405=CARTESIAN_POINT('Ctrl Pts',(-0.433805857533288,0.0554545198617944,
-0.372686760526221));
#64406=CARTESIAN_POINT('Ctrl Pts',(-0.435052268808273,0.0446277950996431,
-0.372288426569115));
#64407=CARTESIAN_POINT('Ctrl Pts',(-0.435892678136593,0.033784806450657,
-0.371890092612009));
#64408=CARTESIAN_POINT('Ctrl Pts',(-0.43675847661306,0.0226142461816568,
-0.37147972480484));
#64409=CARTESIAN_POINT('Ctrl Pts',(-0.437194939423667,0.0114099837046195,
-0.371069356997671));
#64410=CARTESIAN_POINT('Ctrl Pts',(-0.437199956252168,0.000195584004442945,
-0.370658989190502));
#64411=CARTESIAN_POINT('Ctrl Pts',(-0.437199956252192,0.00019558395055889,
-0.37065898918853));
#64412=CARTESIAN_POINT('Ctrl Pts',(-0.437209797318043,-0.0218027116530455,
-0.36985400697195));
#64413=CARTESIAN_POINT('Ctrl Pts',(-0.43555503723887,-0.0438677724418389,
-0.369049024755369));
#64414=CARTESIAN_POINT('Ctrl Pts',(-0.432231672166008,-0.0657238280730574,
-0.368244042538789));
#64415=CARTESIAN_POINT('Ctrl Pts',(-0.428913828524319,-0.0875435721031573,
-0.367440397717833));
#64416=CARTESIAN_POINT('Ctrl Pts',(-0.423932935122254,-0.109154275283681,
-0.366636752896876));
#64417=CARTESIAN_POINT('Ctrl Pts',(-0.41733687497774,-0.130283432499356,
-0.36583310807592));
#64418=CARTESIAN_POINT('Ctrl Pts',(-0.410657747974787,-0.151678677754392,
-0.365019342630058));
#64419=CARTESIAN_POINT('Ctrl Pts',(-0.402322582880881,-0.172579399162873,
-0.364205577184196));
#64420=CARTESIAN_POINT('Ctrl Pts',(-0.392433908419011,-0.192716028194281,
-0.363391811738334));
#64421=CARTESIAN_POINT('Ctrl Pts',(-0.382671012325383,-0.212596530648642,
-0.362588396930498));
#64422=CARTESIAN_POINT('Ctrl Pts',(-0.371394308094424,-0.231731635324634,
-0.361784982122661));
#64423=CARTESIAN_POINT('Ctrl Pts',(-0.358749524065807,-0.249885211612367,
-0.360981567314825));
#64424=CARTESIAN_POINT('Ctrl Pts',(-0.345860380122883,-0.268389604990845,
-0.36016262654995));
#64425=CARTESIAN_POINT('Ctrl Pts',(-0.331550130208112,-0.28587345548614,
-0.359343685785075));
#64426=CARTESIAN_POINT('Ctrl Pts',(-0.316016681609745,-0.30212132818516,
-0.3585247450202));
#64427=CARTESIAN_POINT('Ctrl Pts',(-0.300483233011378,-0.31836920088418,
-0.357705804255325));
#64428=CARTESIAN_POINT('Ctrl Pts',(-0.283727222915686,-0.333380613157547,
-0.35688686349045));
#64429=CARTESIAN_POINT('Ctrl Pts',(-0.265981928594421,-0.346983362225327,
-0.356067922725575));
#64430=CARTESIAN_POINT('Ctrl Pts',(-0.248346914651699,-0.360501575286587,
-0.355254071371781));
#64431=CARTESIAN_POINT('Ctrl Pts',(-0.22962828453433,-0.372710590695404,
-0.354440220017987));
#64432=CARTESIAN_POINT('Ctrl Pts',(-0.210046876199587,-0.383437282744904,
-0.353626368664193));
#64433=CARTESIAN_POINT('Ctrl Pts',(-0.190500396005526,-0.394144841165067,
-0.352813969009587));
#64434=CARTESIAN_POINT('Ctrl Pts',(-0.170094786286069,-0.403374935974287,
-0.352001569354981));
#64435=CARTESIAN_POINT('Ctrl Pts',(-0.149079796723947,-0.410997632850539,
-0.351189169700375));
#64436=CARTESIAN_POINT('Ctrl Pts',(-0.128087085406607,-0.418612248813575,
-0.350377631280475));
#64437=CARTESIAN_POINT('Ctrl Pts',(-0.106486936500757,-0.424622580888818,
-0.349566092860576));
#64438=CARTESIAN_POINT('Ctrl Pts',(-0.0845491661335071,-0.428946708235567,
-0.348754554440676));
#64439=CARTESIAN_POINT('Ctrl Pts',(-0.0626008419783057,-0.433272915826677,
-0.347942625607154));
#64440=CARTESIAN_POINT('Ctrl Pts',(-0.0403152703163706,-0.43591114144486,
-0.347130696773632));
#64441=CARTESIAN_POINT('Ctrl Pts',(-0.01797339879321,-0.43683039836511,
-0.34631876794011));
#64442=CARTESIAN_POINT('Ctrl Pts',(0.00437397125136595,-0.437749881522174,
-0.345506639284112));
#64443=CARTESIAN_POINT('Ctrl Pts',(0.0267769527679093,-0.436949555850671,
-0.344694510628114));
#64444=CARTESIAN_POINT('Ctrl Pts',(0.0489543001086752,-0.434450591553136,
-0.343882381972117));
#64445=CARTESIAN_POINT('Ctrl Pts',(0.071179314951276,-0.431946256036789,
-0.343068507744676));
#64446=CARTESIAN_POINT('Ctrl Pts',(0.093177022140436,-0.427736120776913,
-0.342254633517235));
#64447=CARTESIAN_POINT('Ctrl Pts',(0.114674963735666,-0.421892750224774,
-0.341440759289794));
#64448=CARTESIAN_POINT('Ctrl Pts',(0.125196728244188,-0.419032822049172,
-0.341042423806243));
#64449=CARTESIAN_POINT('Ctrl Pts',(0.135599004985787,-0.415782428010782,
-0.340644088322692));
#64450=CARTESIAN_POINT('Ctrl Pts',(0.145851532189345,-0.41215430430607,
-0.340245752839141));
#64451=CARTESIAN_POINT('Ctrl Pts',(0.166798817261596,-0.404741562061054,
-0.339431900140907));
#64452=CARTESIAN_POINT('Ctrl Pts',(0.187239430905852,-0.395706621866752,
-0.338618047442673));
#64453=CARTESIAN_POINT('Ctrl Pts',(0.206907836438915,-0.385140217609337,
-0.337804194744438));
#64454=CARTESIAN_POINT('Ctrl Pts',(0.226541158947589,-0.374592660910136,
-0.336991793735514));
#64455=CARTESIAN_POINT('Ctrl Pts',(0.245404357843054,-0.362519348440181,
-0.33617939272659));
#64456=CARTESIAN_POINT('Ctrl Pts',(0.263252339930174,-0.349058799518488,
-0.335366991717666));
#64457=CARTESIAN_POINT('Ctrl Pts',(0.281081401305644,-0.335612520174361,
-0.334555451938048));
#64458=CARTESIAN_POINT('Ctrl Pts',(0.297896797365796,-0.320782330393067,
-0.33374391215843));
#64459=CARTESIAN_POINT('Ctrl Pts',(0.313482743356919,-0.304749749167116,
-0.332932372378813));
#64460=CARTESIAN_POINT('Ctrl Pts',(0.329076187247889,-0.288709455179399,
-0.332120442193377));
#64461=CARTESIAN_POINT('Ctrl Pts',(0.343438487359899,-0.271466114248043,
-0.331308512007942));
#64462=CARTESIAN_POINT('Ctrl Pts',(0.356390487247955,-0.25323834741043,
-0.330496581822506));
#64463=CARTESIAN_POINT('Ctrl Pts',(0.369345674683841,-0.235006094634032,
-0.32968445181725));
#64464=CARTESIAN_POINT('Ctrl Pts',(0.380889482304987,-0.215789534962041,
-0.328872321811993));
#64465=CARTESIAN_POINT('Ctrl Pts',(0.390886313736336,-0.195835976607004,
-0.328060191806737));
#64466=CARTESIAN_POINT('Ctrl Pts',(0.400904631792151,-0.175839531201396,
-0.327246316255148));
#64467=CARTESIAN_POINT('Ctrl Pts',(0.409369058235974,-0.155103585576575,
-0.326432440703559));
#64468=CARTESIAN_POINT('Ctrl Pts',(0.41619187118334,-0.133896102859307,
-0.32561856515197));
#64469=CARTESIAN_POINT('Ctrl Pts',(0.419531095878111,-0.1235167255336,-0.325220237752215));
#64470=CARTESIAN_POINT('Ctrl Pts',(0.422477865488116,-0.113024625635012,
-0.32482191035246));
#64471=CARTESIAN_POINT('Ctrl Pts',(0.425026357386873,-0.102452113333234,
-0.324423582952706));
#64472=CARTESIAN_POINT('Ctrl Pts',(0.430233348946519,-0.080850717485575,
-0.323609734021301));
#64473=CARTESIAN_POINT('Ctrl Pts',(0.43380423538123,-0.0587895925647821,
-0.322795885089896));
#64474=CARTESIAN_POINT('Ctrl Pts',(0.435670299321658,-0.0365408030696792,
-0.321982036158491));
#64475=CARTESIAN_POINT('Ctrl Pts',(0.437533034704557,-0.0143316994471554,
-0.321169638915277));
#64476=CARTESIAN_POINT('Ctrl Pts',(0.437696869278996,0.00806370382861299,
-0.320357241672064));
#64477=CARTESIAN_POINT('Ctrl Pts',(0.436144289949209,0.0303644256441752,
-0.319544844428851));
#64478=CARTESIAN_POINT('Ctrl Pts',(0.43459335649725,0.0526415066299919,
-0.318733308401928));
#64479=CARTESIAN_POINT('Ctrl Pts',(0.431329643147004,0.0748233933029086,
-0.317921772375005));
#64480=CARTESIAN_POINT('Ctrl Pts',(0.426387662689023,0.0966302287412781,
-0.317110236348082));
#64481=CARTESIAN_POINT('Ctrl Pts',(0.421443304411229,0.118447556476376,
-0.316298309852912));
#64482=CARTESIAN_POINT('Ctrl Pts',(0.41481920581988,0.139888770494463,-0.315486383357742));
#64483=CARTESIAN_POINT('Ctrl Pts',(0.406600952687178,0.160684489836074,
-0.314674456862573));
#64484=CARTESIAN_POINT('Ctrl Pts',(0.398380676684247,0.181485327910446,
-0.31386233051691));
#64485=CARTESIAN_POINT('Ctrl Pts',(0.388565757169535,0.201639701359637,
-0.313050204171248));
#64486=CARTESIAN_POINT('Ctrl Pts',(0.377289578154882,0.220899104153257,
-0.312238077825586));
#64487=CARTESIAN_POINT('Ctrl Pts',(0.365989161212073,0.240199904659756,
-0.31142420583009));
#64488=CARTESIAN_POINT('Ctrl Pts',(0.353221616938479,0.258601301089725,
-0.310610333834595));
#64489=CARTESIAN_POINT('Ctrl Pts',(0.339163746543061,0.275883658506397,
-0.309796461839099));
#64490=CARTESIAN_POINT('Ctrl Pts',(0.332283122866943,0.284342507128237,
-0.309398112248157));
#64491=CARTESIAN_POINT('Ctrl Pts',(0.325093993353602,0.292533795250246,
-0.308999762657214));
#64492=CARTESIAN_POINT('Ctrl Pts',(0.317620272842288,0.300435021726147,
-0.308601413066272));
#64493=CARTESIAN_POINT('Ctrl Pts',(0.302349949891085,0.316578825848198,
-0.307787504265165));
#64494=CARTESIAN_POINT('Ctrl Pts',(0.285802006571729,0.331601593610649,
-0.306973595464059));
#64495=CARTESIAN_POINT('Ctrl Pts',(0.268167087518553,0.345297340232758,
-0.306159686662952));
#64496=CARTESIAN_POINT('Ctrl Pts',(0.250564779980651,0.358967759885753,
-0.305347282989213));
#64497=CARTESIAN_POINT('Ctrl Pts',(0.231880012732739,0.371315552973588,
-0.304534879315474));
#64498=CARTESIAN_POINT('Ctrl Pts',(0.212338786939443,0.382172839905043,
-0.303722475641736));
#64499=CARTESIAN_POINT('Ctrl Pts',(0.192811611077644,0.393022320563789,
-0.302910656077514));
#64500=CARTESIAN_POINT('Ctrl Pts',(0.172429803304405,0.402383042990127,
-0.302098836513293));
#64501=CARTESIAN_POINT('Ctrl Pts',(0.151447051746655,0.410131235724915,
-0.301287016949071));
#64502=CARTESIAN_POINT('Ctrl Pts',(0.130473291938885,0.417876108122441,
-0.300475545274331));
#64503=CARTESIAN_POINT('Ctrl Pts',(0.108899770708046,0.42400957704949,-0.29966407359959));
#64504=CARTESIAN_POINT('Ctrl Pts',(0.0869985137521189,0.42845664728759,
-0.29885260192485));
#64505=CARTESIAN_POINT('Ctrl Pts',(0.0650733633028138,0.432908569121355,
-0.298040244963337));
#64506=CARTESIAN_POINT('Ctrl Pts',(0.0428204685794942,0.435670295902952,
-0.297227888001824));
#64507=CARTESIAN_POINT('Ctrl Pts',(0.0205211119096451,0.43671812873522,
-0.296415531040311));
#64508=CARTESIAN_POINT('Ctrl Pts',(0.010605030029012,0.437184079224994,
-0.296054292002525));
#64509=CARTESIAN_POINT('Ctrl Pts',(0.000679806771193227,0.437311814534476,
-0.295693052964738));
#64510=CARTESIAN_POINT('Ctrl Pts',(-0.00922985932074758,0.43710256198851,
-0.295331813926952));
#64511=CARTESIAN_POINT('Origin',(0.,0.,-0.920658989190502));
#64512=CARTESIAN_POINT('',(-0.00922985932074711,0.43710256198851,-0.175603427251549));
#64513=CARTESIAN_POINT('',(-0.00922985932074797,0.43710256198851,-0.195314102181071));
#64514=CARTESIAN_POINT('',(-0.00922985932074702,0.43710256198851,-0.920658989190502));
#64515=CARTESIAN_POINT('',(-0.437199828329094,-0.000387439040882649,-0.250941010806415));
#64516=CARTESIAN_POINT('Ctrl Pts',(-0.437199828329094,-0.00038743904088227,
-0.250941010806416));
#64517=CARTESIAN_POINT('Ctrl Pts',(-0.43717515196089,-0.028233120049581,
-0.249928536965401));
#64518=CARTESIAN_POINT('Ctrl Pts',(-0.434486254312535,-0.0559608307135708,
-0.248916063124386));
#64519=CARTESIAN_POINT('Ctrl Pts',(-0.429223229213364,-0.0831339852506318,
-0.247903589283372));
#64520=CARTESIAN_POINT('Ctrl Pts',(-0.426925233122178,-0.0949986071619341,
-0.247461512552739));
#64521=CARTESIAN_POINT('Ctrl Pts',(-0.42413710727963,-0.106757801910374,
-0.247019435822107));
#64522=CARTESIAN_POINT('Ctrl Pts',(-0.420869149183294,-0.118376514840278,
-0.246577359091474));
#64523=CARTESIAN_POINT('Ctrl Pts',(-0.414852133348964,-0.139769071786505,
-0.245763400463551));
#64524=CARTESIAN_POINT('Ctrl Pts',(-0.407182709648748,-0.160762817480468,
-0.244949441835628));
#64525=CARTESIAN_POINT('Ctrl Pts',(-0.397933943629819,-0.181086765135445,
-0.244135483207705));
#64526=CARTESIAN_POINT('Ctrl Pts',(-0.388701689625341,-0.201374428023709,
-0.243322977757059));
#64527=CARTESIAN_POINT('Ctrl Pts',(-0.377895932657817,-0.220993999659641,
-0.242510472306414));
#64528=CARTESIAN_POINT('Ctrl Pts',(-0.365638766296714,-0.239691744916292,
-0.241697966855769));
#64529=CARTESIAN_POINT('Ctrl Pts',(-0.353394619145413,-0.258369629965361,
-0.240886324425059));
#64530=CARTESIAN_POINT('Ctrl Pts',(-0.339702490091048,-0.276127022019479,
-0.24007468199435));
#64531=CARTESIAN_POINT('Ctrl Pts',(-0.324729310597089,-0.292736596344118,
-0.23926303956364));
#64532=CARTESIAN_POINT('Ctrl Pts',(-0.309748999178721,-0.309354082029776,
-0.238451010536853));
#64533=CARTESIAN_POINT('Ctrl Pts',(-0.29348688338928,-0.324822113908098,
-0.237638981510066));
#64534=CARTESIAN_POINT('Ctrl Pts',(-0.276149330728357,-0.338947469585304,
-0.236826952483278));
#64535=CARTESIAN_POINT('Ctrl Pts',(-0.258807555287566,-0.353076265671243,
-0.236014725676568));
#64536=CARTESIAN_POINT('Ctrl Pts',(-0.240390395703553,-0.365861307147297,
-0.235202498869858));
#64537=CARTESIAN_POINT('Ctrl Pts',(-0.221135719732469,-0.37715094253946,
-0.234390272063148));
#64538=CARTESIAN_POINT('Ctrl Pts',(-0.201839772608195,-0.388464776535246,
-0.233576304300786));
#64539=CARTESIAN_POINT('Ctrl Pts',(-0.181703366188955,-0.3982764850038,
-0.232762336538424));
#64540=CARTESIAN_POINT('Ctrl Pts',(-0.16098813901441,-0.406480822544775,
-0.231948368776062));
#64541=CARTESIAN_POINT('Ctrl Pts',(-0.15086612230538,-0.410489682354834,
-0.231550642252388));
#64542=CARTESIAN_POINT('Ctrl Pts',(-0.140606183717589,-0.414115518715765,
-0.231152915728714));
#64543=CARTESIAN_POINT('Ctrl Pts',(-0.130240030003468,-0.417350421809653,
-0.23075518920504));
#64544=CARTESIAN_POINT('Ctrl Pts',(-0.109020412341652,-0.423972299964116,
-0.229941039135587));
#64545=CARTESIAN_POINT('Ctrl Pts',(-0.0872341704118623,-0.428990553146929,
-0.229126889066133));
#64546=CARTESIAN_POINT('Ctrl Pts',(-0.0651484699482539,-0.432318767651141,
-0.228312738996679));
#64547=CARTESIAN_POINT('Ctrl Pts',(-0.0431020702402091,-0.435641059710425,
-0.227500037679685));
#64548=CARTESIAN_POINT('Ctrl Pts',(-0.0207579606770463,-0.437279122771291,
-0.226687336362691));
#64549=CARTESIAN_POINT('Ctrl Pts',(0.00160444992955381,-0.43719705596038,
-0.225874635045697));
#64550=CARTESIAN_POINT('Ctrl Pts',(0.0239432157696132,-0.43711507592234,
-0.225062793033778));
#64551=CARTESIAN_POINT('Ctrl Pts',(0.0462995328254728,-0.435316551808519,
-0.224250951021858));
#64552=CARTESIAN_POINT('Ctrl Pts',(0.0683917067825807,-0.43181757079045,
-0.223439109009938));
#64553=CARTESIAN_POINT('Ctrl Pts',(0.0904944859685637,-0.428316910105428,
-0.222626877277642));
#64554=CARTESIAN_POINT('Ctrl Pts',(0.112332159703595,-0.423114255294599,
-0.221814645545347));
#64555=CARTESIAN_POINT('Ctrl Pts',(0.133630135588047,-0.416277343681734,
-0.221002413813051));
#64556=CARTESIAN_POINT('Ctrl Pts',(0.154933351152798,-0.409438750067195,
-0.220189982257324));
#64557=CARTESIAN_POINT('Ctrl Pts',(0.175695933661859,-0.400965347569769,
-0.219377550701598));
#64558=CARTESIAN_POINT('Ctrl Pts',(0.195660974687255,-0.390973941566996,
-0.218565119145871));
#64559=CARTESIAN_POINT('Ctrl Pts',(0.215668795638291,-0.380961126562095,
-0.217750946759184));
#64560=CARTESIAN_POINT('Ctrl Pts',(0.234875045798112,-0.369424176900229,
-0.216936774372497));
#64561=CARTESIAN_POINT('Ctrl Pts',(0.253048763665302,-0.356525122827918,
-0.216122601985811));
#64562=CARTESIAN_POINT('Ctrl Pts',(0.261899935778643,-0.350242877855939,
-0.215726074430076));
#64563=CARTESIAN_POINT('Ctrl Pts',(0.270506665361262,-0.343638176717351,
-0.21532954687434));
#64564=CARTESIAN_POINT('Ctrl Pts',(0.278845254818156,-0.336733075098657,
-0.214933019318605));
#64565=CARTESIAN_POINT('Ctrl Pts',(0.295938302881246,-0.322578494823539,
-0.214120188251246));
#64566=CARTESIAN_POINT('Ctrl Pts',(0.312000410918705,-0.307078035278154,
-0.213307357183887));
#64567=CARTESIAN_POINT('Ctrl Pts',(0.326813749353737,-0.290407667311579,
-0.212494526116528));
#64568=CARTESIAN_POINT('Ctrl Pts',(0.341600620471756,-0.273767084657452,
-0.211683147352283));
#64569=CARTESIAN_POINT('Ctrl Pts',(0.355142637308786,-0.255961235444033,
-0.210871768588038));
#64570=CARTESIAN_POINT('Ctrl Pts',(0.367257567579701,-0.237203960876377,
-0.210060389823792));
#64571=CARTESIAN_POINT('Ctrl Pts',(0.379359676986439,-0.218466536564906,
-0.209249869717145));
#64572=CARTESIAN_POINT('Ctrl Pts',(0.390037287005823,-0.198780270088444,
-0.208439349610498));
#64573=CARTESIAN_POINT('Ctrl Pts',(0.39915046323598,-0.178389314978512,
-0.207628829503852));
#64574=CARTESIAN_POINT('Ctrl Pts',(0.408268202657258,-0.157988149616636,
-0.206817903549884));
#64575=CARTESIAN_POINT('Ctrl Pts',(0.415819633610496,-0.136882238240811,
-0.206006977595917));
#64576=CARTESIAN_POINT('Ctrl Pts',(0.421711976104694,-0.115337978176637,
-0.20519605164195));
#64577=CARTESIAN_POINT('Ctrl Pts',(0.427605824304418,-0.0937882127788037,
-0.204384918467223));
#64578=CARTESIAN_POINT('Ctrl Pts',(0.431839582023699,-0.0718005760780592,
-0.203573785292495));
#64579=CARTESIAN_POINT('Ctrl Pts',(0.434371248107624,-0.0496533867669199,
-0.202762652117767));
#64580=CARTESIAN_POINT('Ctrl Pts',(0.436908445724973,-0.0274578072203115,
-0.201949746667345));
#64581=CARTESIAN_POINT('Ctrl Pts',(0.43773609446431,-0.00510269711023237,
-0.201136841216923));
#64582=CARTESIAN_POINT('Ctrl Pts',(0.436864255439904,0.0171307419260887,
-0.200323935766501));
#64583=CARTESIAN_POINT('Ctrl Pts',(0.436430578105641,0.0281902819361774,
-0.199919573655058));
#64584=CARTESIAN_POINT('Ctrl Pts',(0.435577202005302,0.0392197681305007,
-0.199515211543615));
#64585=CARTESIAN_POINT('Ctrl Pts',(0.434310110882799,0.0501853323688408,
-0.199110849432172));
#64586=CARTESIAN_POINT('Ctrl Pts',(0.431756587431705,0.0722838420496241,
-0.198295952921602));
#64587=CARTESIAN_POINT('Ctrl Pts',(0.427504918281149,0.0942495724137049,
-0.197481056411031));
#64588=CARTESIAN_POINT('Ctrl Pts',(0.421584542938335,0.115802906507027,
-0.19666615990046));
#64589=CARTESIAN_POINT('Ctrl Pts',(0.41567478439003,0.137317589787553,-0.195852724714264));
#64590=CARTESIAN_POINT('Ctrl Pts',(0.408102393480184,0.158420649713672,
-0.195039289528069));
#64591=CARTESIAN_POINT('Ctrl Pts',(0.398947945800709,0.178841763974174,
-0.194225854341873));
#64592=CARTESIAN_POINT('Ctrl Pts',(0.389803334365754,0.199240936214769,
-0.193413293173169));
#64593=CARTESIAN_POINT('Ctrl Pts',(0.379080305967078,0.218958958286204,
-0.192600732004464));
#64594=CARTESIAN_POINT('Ctrl Pts',(0.366907889356692,0.237744486219592,
-0.19178817083576));
#64595=CARTESIAN_POINT('Ctrl Pts',(0.354730083304338,0.256538331606766,
-0.190975249898621));
#64596=CARTESIAN_POINT('Ctrl Pts',(0.341101978880221,0.274398248767588,
-0.190162328961482));
#64597=CARTESIAN_POINT('Ctrl Pts',(0.32619694664029,0.291100312611567,-0.189349408024344));
#64598=CARTESIAN_POINT('Ctrl Pts',(0.311288547867978,0.307806148875347,
-0.188536303476421));
#64599=CARTESIAN_POINT('Ctrl Pts',(0.295103144584151,0.3233530990482,-0.187723198928498));
#64600=CARTESIAN_POINT('Ctrl Pts',(0.277851824848643,0.337553260135758,
-0.186910094380575));
#64601=CARTESIAN_POINT('Ctrl Pts',(0.260564312822474,0.351783212356134,
-0.186095283985413));
#64602=CARTESIAN_POINT('Ctrl Pts',(0.242207000193842,0.364660317308267,
-0.185280473590252));
#64603=CARTESIAN_POINT('Ctrl Pts',(0.223021837114547,0.376038695043546,
-0.18446566319509));
#64604=CARTESIAN_POINT('Ctrl Pts',(0.213784259313793,0.381517337531054,
-0.184073335311972));
#64605=CARTESIAN_POINT('Ctrl Pts',(0.204355136177859,0.386649196640079,
-0.183681007428854));
#64606=CARTESIAN_POINT('Ctrl Pts',(0.19476325782855,0.391421912263493,-0.183288679545737));
#64607=CARTESIAN_POINT('Ctrl Pts',(0.17482500171414,0.401342766448193,-0.182473163175578));
#64608=CARTESIAN_POINT('Ctrl Pts',(0.15407180251471,0.409763693222663,-0.18165764680542));
#64609=CARTESIAN_POINT('Ctrl Pts',(0.132754872050416,0.416557299716231,
-0.180842130435262));
#64610=CARTESIAN_POINT('Ctrl Pts',(0.111475306657736,0.423338998135435,
-0.180028043531116));
#64611=CARTESIAN_POINT('Ctrl Pts',(0.0896346266806214,0.428498773999735,
-0.179213956626969));
#64612=CARTESIAN_POINT('Ctrl Pts',(0.0675039988359496,0.43195723184264,
-0.178399869722823));
#64613=CARTESIAN_POINT('Ctrl Pts',(0.0453962963714171,0.435412107028003,
-0.177586626140966));
#64614=CARTESIAN_POINT('Ctrl Pts',(0.0229999384184317,0.43716902774766,
-0.176773382559109));
#64615=CARTESIAN_POINT('Ctrl Pts',(0.000596477640129765,0.437199593108714,
-0.175960138977252));
#64616=CARTESIAN_POINT('Ctrl Pts',(-0.0026791203620098,0.437204062053784,
-0.175841235068684));
#64617=CARTESIAN_POINT('Ctrl Pts',(-0.00595486139123389,0.437171716856941,
-0.175722331160117));
#64618=CARTESIAN_POINT('Ctrl Pts',(-0.00922985932074711,0.43710256198851,
-0.175603427251549));
#64619=CARTESIAN_POINT('Ctrl Pts',(-0.00922985932074603,0.43710256198851,
-0.275596058510812));
#64620=CARTESIAN_POINT('Ctrl Pts',(-0.0315175128047482,0.436631935814847,
-0.274783692737513));
#64621=CARTESIAN_POINT('Ctrl Pts',(-0.053811199458999,0.434451425783461,
-0.273971326964214));
#64622=CARTESIAN_POINT('Ctrl Pts',(-0.0758295964441591,0.430573701360308,
-0.273158961190914));
#64623=CARTESIAN_POINT('Ctrl Pts',(-0.0978258595168454,0.42669987500535,
-0.272347412045317));
#64624=CARTESIAN_POINT('Ctrl Pts',(-0.119546676627676,0.421132319555819,
-0.271535862899719));
#64625=CARTESIAN_POINT('Ctrl Pts',(-0.14071744677465,0.413935309164637,
-0.270724313754122));
#64626=CARTESIAN_POINT('Ctrl Pts',(-0.161899378925678,0.406734504246444,
-0.269912336730143));
#64627=CARTESIAN_POINT('Ctrl Pts',(-0.182530002334501,0.39790274367376,
-0.269100359706165));
#64628=CARTESIAN_POINT('Ctrl Pts',(-0.202350636352501,0.387553944590605,
-0.268288382682186));
#64629=CARTESIAN_POINT('Ctrl Pts',(-0.222177114956752,0.377202093917437,
-0.267476166227433));
#64630=CARTESIAN_POINT('Ctrl Pts',(-0.241192510643821,0.365332675222146,
-0.26666394977268));
#64631=CARTESIAN_POINT('Ctrl Pts',(-0.259164041999417,0.352104869796662,
-0.265851733317928));
#64632=CARTESIAN_POINT('Ctrl Pts',(-0.277173773677142,0.338848947322146,
-0.265037790414293));
#64633=CARTESIAN_POINT('Ctrl Pts',(-0.29413466693318,0.324229339238528,
-0.264223847510659));
#64634=CARTESIAN_POINT('Ctrl Pts',(-0.309847353017181,0.308445226625809,
-0.263409904607024));
#64635=CARTESIAN_POINT('Ctrl Pts',(-0.31634892088569,0.301914104012707,
-0.263073112730652));
#64636=CARTESIAN_POINT('Ctrl Pts',(-0.322637237278018,0.295184021827159,
-0.262736320854281));
#64637=CARTESIAN_POINT('Ctrl Pts',(-0.328700221991952,0.288270713154218,
-0.262399528977909));
#64638=CARTESIAN_POINT('Ctrl Pts',(-0.343220359896925,0.2717141490118,-0.261592951900623));
#64639=CARTESIAN_POINT('Ctrl Pts',(-0.356531992844097,0.254005601113313,
-0.260786374823338));
#64640=CARTESIAN_POINT('Ctrl Pts',(-0.368448821091825,0.235349328097712,
-0.259979797746052));
#64641=CARTESIAN_POINT('Ctrl Pts',(-0.380344742409986,0.216725785719645,
-0.25917463573071));
#64642=CARTESIAN_POINT('Ctrl Pts',(-0.390850274299905,0.197158392385561,
-0.258369473715368));
#64643=CARTESIAN_POINT('Ctrl Pts',(-0.399820049116241,0.17688348799333,
-0.257564311700026));
#64644=CARTESIAN_POINT('Ctrl Pts',(-0.40878017178987,0.156630400901375,
-0.256760016098707));
#64645=CARTESIAN_POINT('Ctrl Pts',(-0.416207497594123,0.135671966911522,
-0.255955720497387));
#64646=CARTESIAN_POINT('Ctrl Pts',(-0.42200318132526,0.114267908668004,
-0.255151424896067));
#64647=CARTESIAN_POINT('Ctrl Pts',(-0.427801701475788,0.0928533752349068,
-0.254346735670846));
#64648=CARTESIAN_POINT('Ctrl Pts',(-0.43196677910013,0.0709934828957616,
-0.253542046445625));
#64649=CARTESIAN_POINT('Ctrl Pts',(-0.434449677398004,0.0489624122033488,
-0.252737357220404));
#64650=CARTESIAN_POINT('Ctrl Pts',(-0.436297241776996,0.0325687397451478,
-0.252138575083435));
#64651=CARTESIAN_POINT('Ctrl Pts',(-0.437214422054611,0.0160806372592578,
-0.251539792946467));
#64652=CARTESIAN_POINT('Ctrl Pts',(-0.437199828329169,-0.000387438956102599,
-0.250941010809498));
#64653=CARTESIAN_POINT('',(-0.437199941752427,0.000225680469443025,-0.270658989193252));
#64654=CARTESIAN_POINT('Ctrl Pts',(-0.00922985932074758,0.43710256198851,
-0.295331813926952));
#64655=CARTESIAN_POINT('Ctrl Pts',(-0.0325709355740933,0.436609691735741,
-0.294480957011248));
#64656=CARTESIAN_POINT('Ctrl Pts',(-0.0558246518002711,0.434243140628511,
-0.293630100095543));
#64657=CARTESIAN_POINT('Ctrl Pts',(-0.0786759310588921,0.430062713882541,
-0.292779243179838));
#64658=CARTESIAN_POINT('Ctrl Pts',(-0.100533583978425,0.426064061735552,
-0.291965383485719));
#64659=CARTESIAN_POINT('Ctrl Pts',(-0.122148097674547,0.420383379243374,
-0.2911515237916));
#64660=CARTESIAN_POINT('Ctrl Pts',(-0.143242906605044,0.413068165933104,
-0.29033766409748));
#64661=CARTESIAN_POINT('Ctrl Pts',(-0.164300089563836,0.405766000477875,
-0.289525256052529));
#64662=CARTESIAN_POINT('Ctrl Pts',(-0.184838721069643,0.39683527062798,
-0.288712848007577));
#64663=CARTESIAN_POINT('Ctrl Pts',(-0.204594846587949,0.386373897603932,
-0.287900439962625));
#64664=CARTESIAN_POINT('Ctrl Pts',(-0.224330029161878,0.375923614403804,
-0.287088893129882));
#64665=CARTESIAN_POINT('Ctrl Pts',(-0.243283710418694,0.363946217876189,
-0.286277346297139));
#64666=CARTESIAN_POINT('Ctrl Pts',(-0.261214058100043,0.350586730854017,
-0.285465799464396));
#64667=CARTESIAN_POINT('Ctrl Pts',(-0.279153030175122,0.337220817995707,
-0.284653862282312));
#64668=CARTESIAN_POINT('Ctrl Pts',(-0.296067100426924,0.322471899138628,
-0.283841925100227));
#64669=CARTESIAN_POINT('Ctrl Pts',(-0.311744720888325,0.306527435963341,
-0.283029987918142));
#64670=CARTESIAN_POINT('Ctrl Pts',(-0.32742619921006,0.290579049264572,
-0.28221785093914));
#64671=CARTESIAN_POINT('Ctrl Pts',(-0.341870143007703,0.273435064679692,
-0.281405713960137));
#64672=CARTESIAN_POINT('Ctrl Pts',(-0.354903466385701,0.255318173163239,
-0.280593576981134));
#64673=CARTESIAN_POINT('Ctrl Pts',(-0.367964800306894,0.237162345762387,
-0.279779694599423));
#64674=CARTESIAN_POINT('Ctrl Pts',(-0.379609082787468,0.21803004565943,
-0.278965812217711));
#64675=CARTESIAN_POINT('Ctrl Pts',(-0.389707223032687,0.198171946339918,
-0.278151929836));
#64676=CARTESIAN_POINT('Ctrl Pts',(-0.394648898968172,0.188454088482066,
-0.277753644321801));
#64677=CARTESIAN_POINT('Ctrl Pts',(-0.399221026801609,0.178562761786,-0.277355358807602));
#64678=CARTESIAN_POINT('Ctrl Pts',(-0.403412739191937,0.168528934778744,
-0.276957073293403));
#64679=CARTESIAN_POINT('Ctrl Pts',(-0.412935550646297,0.145733896890115,
-0.276052240732498));
#64680=CARTESIAN_POINT('Ctrl Pts',(-0.42053826809405,0.122091879741921,
-0.275147408171593));
#64681=CARTESIAN_POINT('Ctrl Pts',(-0.426092790488426,0.0979222849702084,
-0.274242575610688));
#64682=CARTESIAN_POINT('Ctrl Pts',(-0.431607015213754,0.0739280389075253,
-0.27334430754633));
#64683=CARTESIAN_POINT('Ctrl Pts',(-0.43510245696255,0.0494142356025085,
-0.272446039481973));
#64684=CARTESIAN_POINT('Ctrl Pts',(-0.436500945633631,0.024713649284278,
-0.271547771417616));
#64685=CARTESIAN_POINT('Ctrl Pts',(-0.436962185776802,0.0165670677599341,
-0.271251510676161));
#64686=CARTESIAN_POINT('Ctrl Pts',(-0.437195722049905,0.00840030763711254,
-0.270955249934706));
#64687=CARTESIAN_POINT('Ctrl Pts',(-0.437199941752427,0.000225680469444049,
-0.270658989193251));
#64688=CARTESIAN_POINT('Ctrl Pts',(-0.437199941752466,0.000225680393569806,
-0.270658989190502));
#64689=CARTESIAN_POINT('Ctrl Pts',(-0.437211658071991,-0.0224717907196608,
-0.269836398816264));
#64690=CARTESIAN_POINT('Ctrl Pts',(-0.435451497671837,-0.0451684701615349,
-0.269013808442026));
#64691=CARTESIAN_POINT('Ctrl Pts',(-0.431946071086998,-0.0675753777089434,
-0.268191218067787));
#64692=CARTESIAN_POINT('Ctrl Pts',(-0.428439190565981,-0.0899915789079819,
-0.267368286509994));
#64693=CARTESIAN_POINT('Ctrl Pts',(-0.42318574251998,-0.112117092405877,
-0.266545354952201));
#64694=CARTESIAN_POINT('Ctrl Pts',(-0.416263570354819,-0.133673033912822,
-0.265722423394408));
#64695=CARTESIAN_POINT('Ctrl Pts',(-0.40932251389466,-0.155287781925684,
-0.264897246806886));
#64696=CARTESIAN_POINT('Ctrl Pts',(-0.400703886039429,-0.176329206487253,
-0.264072070219364));
#64697=CARTESIAN_POINT('Ctrl Pts',(-0.390534527426051,-0.196536568831632,
-0.263246893631841));
#64698=CARTESIAN_POINT('Ctrl Pts',(-0.381858571956055,-0.213776414777793,
-0.262542896890217));
#64699=CARTESIAN_POINT('Ctrl Pts',(-0.372054857008198,-0.230409337630752,
-0.261838900148593));
#64700=CARTESIAN_POINT('Ctrl Pts',(-0.361227100237478,-0.246290117654004,
-0.261134903406969));
#64701=CARTESIAN_POINT('Ctrl Pts',(-0.348709593271618,-0.264649208901961,
-0.260321042853594));
#64702=CARTESIAN_POINT('Ctrl Pts',(-0.334753100380863,-0.2821040656358,
-0.25950718230022));
#64703=CARTESIAN_POINT('Ctrl Pts',(-0.319513172884127,-0.298421132551832,
-0.258693321746845));
#64704=CARTESIAN_POINT('Ctrl Pts',(-0.304300433255758,-0.314709089994243,
-0.257880913112031));
#64705=CARTESIAN_POINT('Ctrl Pts',(-0.287809246239468,-0.329862731700687,
-0.257068504477217));
#64706=CARTESIAN_POINT('Ctrl Pts',(-0.270236141695493,-0.343680473291011,
-0.256256095842403));
#64707=CARTESIAN_POINT('Ctrl Pts',(-0.25268167167555,-0.357483562545028,
-0.255444548685889));
#64708=CARTESIAN_POINT('Ctrl Pts',(-0.234048104169553,-0.369953102104183,
-0.254633001529375));
#64709=CARTESIAN_POINT('Ctrl Pts',(-0.214566056380477,-0.380926826896361,
-0.253821454372862));
#64710=CARTESIAN_POINT('Ctrl Pts',(-0.195074647287965,-0.391905824664393,
-0.253009517260463));
#64711=CARTESIAN_POINT('Ctrl Pts',(-0.174734557699403,-0.401387204353369,
-0.252197580148064));
#64712=CARTESIAN_POINT('Ctrl Pts',(-0.153802920495106,-0.40925359087878,
-0.251385643035665));
#64713=CARTESIAN_POINT('Ctrl Pts',(-0.132866138331588,-0.417121910948018,
-0.250573506350567));
#64714=CARTESIAN_POINT('Ctrl Pts',(-0.111338199713712,-0.4233742254396,
-0.249761369665469));
#64715=CARTESIAN_POINT('Ctrl Pts',(-0.0894928473206696,-0.427942601616665,
-0.248949232980371));
#64716=CARTESIAN_POINT('Ctrl Pts',(-0.0676005549841006,-0.432520794038206,
-0.248135351226142));
#64717=CARTESIAN_POINT('Ctrl Pts',(-0.0453901970621191,-0.435407725064112,
-0.247321469471912));
#64718=CARTESIAN_POINT('Ctrl Pts',(-0.0231432582016464,-0.436587024085476,
-0.246507587717683));
#64719=CARTESIAN_POINT('Ctrl Pts',(-0.012256398968934,-0.437164131008787,
-0.2461093029853));
#64720=CARTESIAN_POINT('Ctrl Pts',(-0.00136080249563929,-0.437333095328693,
-0.245711018252918));
#64721=CARTESIAN_POINT('Ctrl Pts',(0.00951081625659959,-0.437096538963801,
-0.245312733520535));
#64722=CARTESIAN_POINT('Ctrl Pts',(0.0317271789964791,-0.436613131466661,
-0.24449883098311));
#64723=CARTESIAN_POINT('Ctrl Pts',(0.053970050068627,-0.434430233866494,
-0.243684928445685));
#64724=CARTESIAN_POINT('Ctrl Pts',(0.0759588056466642,-0.430550925959674,
-0.24287102590826));
#64725=CARTESIAN_POINT('Ctrl Pts',(0.0979083516421918,-0.426678535499496,
-0.242058574693471));
#64726=CARTESIAN_POINT('Ctrl Pts',(0.119603975224661,-0.421115807505287,
-0.241246123478681));
#64727=CARTESIAN_POINT('Ctrl Pts',(0.140769515543163,-0.413917604715894,
-0.240433672263892));
#64728=CARTESIAN_POINT('Ctrl Pts',(0.161912624805773,-0.40672703051933,
-0.239622082077847));
#64729=CARTESIAN_POINT('Ctrl Pts',(0.182526083246665,-0.39790462540619,
-0.238810491891802));
#64730=CARTESIAN_POINT('Ctrl Pts',(0.202348109039612,-0.387555264147054,
-0.237998901705757));
#64731=CARTESIAN_POINT('Ctrl Pts',(0.222179662922132,-0.377200928136997,
-0.237186921402977));
#64732=CARTESIAN_POINT('Ctrl Pts',(0.241218381327371,-0.36531848427911,
-0.236374941100197));
#64733=CARTESIAN_POINT('Ctrl Pts',(0.259225658378425,-0.352059509228585,
-0.235562960797416));
#64734=CARTESIAN_POINT('Ctrl Pts',(0.277237364648469,-0.338797272890752,
-0.234750780773237));
#64735=CARTESIAN_POINT('Ctrl Pts',(0.294216567259407,-0.32415828071142,
-0.233938600749057));
#64736=CARTESIAN_POINT('Ctrl Pts',(0.309957052119384,-0.308334989648371,
-0.233126420724877));
#64737=CARTESIAN_POINT('Ctrl Pts',(0.325731348562761,-0.292477709128823,
-0.232312496085276));
#64738=CARTESIAN_POINT('Ctrl Pts',(0.340261144854378,-0.275431591742576,
-0.231498571445675));
#64739=CARTESIAN_POINT('Ctrl Pts',(0.353379229979316,-0.25742369708173,
-0.230684646806073));
#64740=CARTESIAN_POINT('Ctrl Pts',(0.359794272983742,-0.248617425619982,
-0.230286619082082));
#64741=CARTESIAN_POINT('Ctrl Pts',(0.365872369471393,-0.239581604847051,
-0.229888591358091));
#64742=CARTESIAN_POINT('Ctrl Pts',(0.371597910291157,-0.230345030480897,
-0.2294905636341));
#64743=CARTESIAN_POINT('Ctrl Pts',(0.383302953098264,-0.211462185741816,
-0.228676853332419));
#64744=CARTESIAN_POINT('Ctrl Pts',(0.393598548054935,-0.191630784443394,
-0.227863143030739));
#64745=CARTESIAN_POINT('Ctrl Pts',(0.402334272718512,-0.171087617892312,
-0.227049432729058));
#64746=CARTESIAN_POINT('Ctrl Pts',(0.411054413010577,-0.150581099971071,
-0.226237174071532));
#64747=CARTESIAN_POINT('Ctrl Pts',(0.418219878496133,-0.129365966855261,
-0.225424915414007));
#64748=CARTESIAN_POINT('Ctrl Pts',(0.42372608260923,-0.107703513947485,
-0.224612656756481));
#64749=CARTESIAN_POINT('Ctrl Pts',(0.429226451898634,-0.0860640163444657,
-0.223801258834584));
#64750=CARTESIAN_POINT('Ctrl Pts',(0.433070848035163,-0.0639788233525656,
-0.222989860912687));
#64751=CARTESIAN_POINT('Ctrl Pts',(0.435204446264768,-0.0417244526791764,
-0.22217846299079));
#64752=CARTESIAN_POINT('Ctrl Pts',(0.437339077286187,-0.0194593095315962,
-0.221366672302758));
#64753=CARTESIAN_POINT('Ctrl Pts',(0.437761169140678,0.00297446411620671,
-0.220554881614725));
#64754=CARTESIAN_POINT('Ctrl Pts',(0.436467682495792,0.0252943103632527,
-0.219743090926692));
#64755=CARTESIAN_POINT('Ctrl Pts',(0.435173875617286,0.0476196824231763,
-0.218931099260419));
#64756=CARTESIAN_POINT('Ctrl Pts',(0.4321637176653,0.0698303584049589,-0.218119107594145));
#64757=CARTESIAN_POINT('Ctrl Pts',(0.427486099801381,0.0916486468891051,
-0.217307115927871));
#64758=CARTESIAN_POINT('Ctrl Pts',(0.422798403889784,0.113513943435468,
-0.216493374804724));
#64759=CARTESIAN_POINT('Ctrl Pts',(0.416436272878416,0.13498447528246,-0.215679633681576));
#64760=CARTESIAN_POINT('Ctrl Pts',(0.40849886971943,0.155796384547101,-0.214865892558429));
#64761=CARTESIAN_POINT('Ctrl Pts',(0.40460531742823,0.166005297384021,-0.214466726288175));
#64762=CARTESIAN_POINT('Ctrl Pts',(0.400333460376828,0.17605603414868,-0.21406756001792));
#64763=CARTESIAN_POINT('Ctrl Pts',(0.395699074473075,0.185919559114021,
-0.213668393747666));
#64764=CARTESIAN_POINT('Ctrl Pts',(0.386248884447322,0.206032727758595,
-0.212854435397172));
#64765=CARTESIAN_POINT('Ctrl Pts',(0.375234272621707,0.225481003321121,
-0.212040477046679));
#64766=CARTESIAN_POINT('Ctrl Pts',(0.362771836476794,0.244009087247287,
-0.211226518696185));
#64767=CARTESIAN_POINT('Ctrl Pts',(0.350331649792709,0.262504092578487,
-0.210414013523402));
#64768=CARTESIAN_POINT('Ctrl Pts',(0.33644911834653,0.280081549310864,-0.209601508350619));
#64769=CARTESIAN_POINT('Ctrl Pts',(0.321286366746358,0.296511231731489,
-0.208789003177837));
#64770=CARTESIAN_POINT('Ctrl Pts',(0.306139720582353,0.312923463018676,
-0.207977361024547));
#64771=CARTESIAN_POINT('Ctrl Pts',(0.289716016086182,0.328189798415627,
-0.207165718871257));
#64772=CARTESIAN_POINT('Ctrl Pts',(0.272217266964286,0.342113430847861,
-0.206354076717967));
#64773=CARTESIAN_POINT('Ctrl Pts',(0.254710182870472,0.356043695359024,
-0.205542047964783));
#64774=CARTESIAN_POINT('Ctrl Pts',(0.236127579275898,0.368629519174213,
-0.204730019211599));
#64775=CARTESIAN_POINT('Ctrl Pts',(0.216704766697847,0.379714213706087,
-0.203917990458415));
#64776=CARTESIAN_POINT('Ctrl Pts',(0.197277223403594,0.390801608080931,
-0.203105763923496));
#64777=CARTESIAN_POINT('Ctrl Pts',(0.177009700324741,0.40038681807714,-0.202293537388577));
#64778=CARTESIAN_POINT('Ctrl Pts',(0.156161749713277,0.408359336769086,
-0.201481310853657));
#64779=CARTESIAN_POINT('Ctrl Pts',(0.135269112674117,0.416348944113376,
-0.200667343356137));
#64780=CARTESIAN_POINT('Ctrl Pts',(0.113794249235171,0.422718748466058,
-0.199853375858616));
#64781=CARTESIAN_POINT('Ctrl Pts',(0.0920125345055164,0.427407923995182,
-0.199039408361096));
#64782=CARTESIAN_POINT('Ctrl Pts',(0.0813693558875901,0.429699191388346,
-0.198641680194474));
#64783=CARTESIAN_POINT('Ctrl Pts',(0.0706530627684541,0.431589976052635,
-0.198243952027853));
#64784=CARTESIAN_POINT('Ctrl Pts',(0.0598962310386143,0.433077685302959,
-0.197846223861231));
#64785=CARTESIAN_POINT('Ctrl Pts',(0.0370685737600804,0.436234833964334,
-0.197002183301178));
#64786=CARTESIAN_POINT('Ctrl Pts',(0.0139233262192277,0.437591464740278,
-0.196158142741124));
#64787=CARTESIAN_POINT('Ctrl Pts',(-0.00922985932074797,0.43710256198851,
-0.195314102181071));
#64788=CARTESIAN_POINT('Origin',(0.,0.,-0.425));
#64789=CARTESIAN_POINT('',(-0.494199919830197,0.000281495695726044,-0.703567954531148));
#64790=CARTESIAN_POINT('',(0.217103634412858,0.443959065595836,-0.735793298822188));
#64791=CARTESIAN_POINT('Ctrl Pts',(-0.494199919830141,0.000281495793510342,
-0.70356795453431));
#64792=CARTESIAN_POINT('Ctrl Pts',(-0.494189043315793,0.0193765325329848,
-0.704185398288897));
#64793=CARTESIAN_POINT('Ctrl Pts',(-0.493071481655549,0.0384371587244305,
-0.704802842043484));
#64794=CARTESIAN_POINT('Ctrl Pts',(-0.490859027051234,0.0573677223037112,
-0.705420285798071));
#64795=CARTESIAN_POINT('Ctrl Pts',(-0.488025007900596,0.0816166174500458,
-0.706211193517275));
#64796=CARTESIAN_POINT('Ctrl Pts',(-0.483382241576563,0.105719856305908,
-0.707002101236479));
#64797=CARTESIAN_POINT('Ctrl Pts',(-0.476961436613325,0.129388670229479,
-0.707793008955683));
#64798=CARTESIAN_POINT('Ctrl Pts',(-0.470551610652628,0.153017012596962,
-0.708582564293386));
#64799=CARTESIAN_POINT('Ctrl Pts',(-0.462369911821056,0.176211732126128,
-0.709372119631088));
#64800=CARTESIAN_POINT('Ctrl Pts',(-0.452498206008631,0.198693265006569,
-0.71016167496879));
#64801=CARTESIAN_POINT('Ctrl Pts',(-0.442636742276802,0.221151472873474,
-0.710950411127968));
#64802=CARTESIAN_POINT('Ctrl Pts',(-0.431089005319465,0.242897323630535,
-0.711739147287145));
#64803=CARTESIAN_POINT('Ctrl Pts',(-0.417985469180945,0.263669845741953,
-0.712527883446322));
#64804=CARTESIAN_POINT('Ctrl Pts',(-0.404876010945428,0.284451755921562,
-0.713316976072028));
#64805=CARTESIAN_POINT('Ctrl Pts',(-0.390209699265885,0.304258863184272,
-0.714106068697735));
#64806=CARTESIAN_POINT('Ctrl Pts',(-0.374161764982923,0.322856955360828,
-0.714895161323441));
#64807=CARTESIAN_POINT('Ctrl Pts',(-0.358110975600725,0.341458356336999,
-0.715684394337169));
#64808=CARTESIAN_POINT('Ctrl Pts',(-0.340678545179392,0.358849808020938,
-0.716473627350897));
#64809=CARTESIAN_POINT('Ctrl Pts',(-0.322078167210184,0.374832354802155,
-0.717262860364625));
#64810=CARTESIAN_POINT('Ctrl Pts',(-0.303437753289581,0.39084930284485,
-0.718053792144616));
#64811=CARTESIAN_POINT('Ctrl Pts',(-0.283624920583873,0.405450867811287,
-0.718844723924608));
#64812=CARTESIAN_POINT('Ctrl Pts',(-0.262885493554465,0.418479219649704,
-0.719635655704599));
#64813=CARTESIAN_POINT('Ctrl Pts',(-0.248841251991481,0.427301706410154,
-0.720171255697901));
#64814=CARTESIAN_POINT('Ctrl Pts',(-0.234372743655487,0.435403667645454,
-0.720706855691203));
#64815=CARTESIAN_POINT('Ctrl Pts',(-0.219562184950262,0.442748333638724,
-0.721242455684505));
#64816=CARTESIAN_POINT('Ctrl Pts',(-0.198162636941886,0.453360528334189,
-0.722016335859998));
#64817=CARTESIAN_POINT('Ctrl Pts',(-0.175919859251839,0.462453061988652,
-0.722790216035492));
#64818=CARTESIAN_POINT('Ctrl Pts',(-0.153080630572819,0.469893562994247,
-0.723564096210985));
#64819=CARTESIAN_POINT('Ctrl Pts',(-0.130281663118874,0.477320947808841,
-0.724336612182618));
#64820=CARTESIAN_POINT('Ctrl Pts',(-0.106888989111418,0.483101796651286,
-0.725109128154251));
#64821=CARTESIAN_POINT('Ctrl Pts',(-0.0831705534104316,0.487151207578717,
-0.725881644125885));
#64822=CARTESIAN_POINT('Ctrl Pts',(-0.0594763804315271,0.491196476170071,
-0.726653369853989));
#64823=CARTESIAN_POINT('Ctrl Pts',(-0.0354578103524282,0.493513670289717,
-0.727425095582093));
#64824=CARTESIAN_POINT('Ctrl Pts',(-0.0113943297299146,0.494068628077118,
-0.728196821310198));
#64825=CARTESIAN_POINT('Ctrl Pts',(0.0126807155116891,0.494623852570552,
-0.728968917920397));
#64826=CARTESIAN_POINT('Ctrl Pts',(0.0367999923064215,0.49341511688943,
-0.729741014530596));
#64827=CARTESIAN_POINT('Ctrl Pts',(0.0606819164688182,0.490460339898825,
-0.730513111140794));
#64828=CARTESIAN_POINT('Ctrl Pts',(0.0845712378333966,0.487504647693741,
-0.731285446900682));
#64829=CARTESIAN_POINT('Ctrl Pts',(0.108222349062157,0.482801966413205,
-0.732057782660569));
#64830=CARTESIAN_POINT('Ctrl Pts',(0.131362496978341,0.476421593116449,
-0.732830118420457));
#64831=CARTESIAN_POINT('Ctrl Pts',(0.15454926048216,0.470028366623956,-0.733604010042711));
#64832=CARTESIAN_POINT('Ctrl Pts',(0.177222330691234,0.461950958188405,
-0.734377901664965));
#64833=CARTESIAN_POINT('Ctrl Pts',(0.199126837746785,0.452307575095715,
-0.735151793287219));
#64834=CARTESIAN_POINT('Ctrl Pts',(0.205179305608705,0.449642997157454,
-0.735365628465542));
#64835=CARTESIAN_POINT('Ctrl Pts',(0.211173242086841,0.44685912964959,-0.735579463643865));
#64836=CARTESIAN_POINT('Ctrl Pts',(0.217103634412858,0.443959065595836,
-0.735793298822188));
#64837=CARTESIAN_POINT('',(-0.21691713542861,0.4440502182833,-0.7358));
#64838=CARTESIAN_POINT('Origin',(0.,0.,-0.7358));
#64839=CARTESIAN_POINT('',(-0.494199978279375,0.000146521891872193,-0.71803204546284));
#64840=CARTESIAN_POINT('Ctrl Pts',(-0.21691713542861,0.444050218283299,
-0.7358));
#64841=CARTESIAN_POINT('Ctrl Pts',(-0.242422499554944,0.431590928102705,
-0.734885845562297));
#64842=CARTESIAN_POINT('Ctrl Pts',(-0.266820316362194,0.416946027148979,
-0.733971691124595));
#64843=CARTESIAN_POINT('Ctrl Pts',(-0.289781003824319,0.400325629734807,
-0.733057536686892));
#64844=CARTESIAN_POINT('Ctrl Pts',(-0.312720563515027,0.383720525937519,
-0.732144223428097));
#64845=CARTESIAN_POINT('Ctrl Pts',(-0.334225451338591,0.365143726777976,
-0.731230910169302));
#64846=CARTESIAN_POINT('Ctrl Pts',(-0.353998238105765,0.344846179358297,
-0.730317596910507));
#64847=CARTESIAN_POINT('Ctrl Pts',(-0.371524830782327,0.326854438985688,
-0.729508036292599));
#64848=CARTESIAN_POINT('Ctrl Pts',(-0.387690835626447,0.307511334928945,
-0.72869847567469));
#64849=CARTESIAN_POINT('Ctrl Pts',(-0.402311589169874,0.287017465007986,
-0.727888915056782));
#64850=CARTESIAN_POINT('Ctrl Pts',(-0.416625437140234,0.266953783782416,
-0.727096347999748));
#64851=CARTESIAN_POINT('Ctrl Pts',(-0.429443326069453,0.24580492972889,
-0.726303780942715));
#64852=CARTESIAN_POINT('Ctrl Pts',(-0.440610621559015,0.223821179000958,
-0.725511213885681));
#64853=CARTESIAN_POINT('Ctrl Pts',(-0.451776489915784,0.20184023770272,
-0.724718748115341));
#64854=CARTESIAN_POINT('Ctrl Pts',(-0.461291885577421,0.179025226576472,
-0.723926282345001));
#64855=CARTESIAN_POINT('Ctrl Pts',(-0.469048899800802,0.155649508819196,
-0.723133816574661));
#64856=CARTESIAN_POINT('Ctrl Pts',(-0.476815701348878,0.132244297015232,
-0.722340350919625));
#64857=CARTESIAN_POINT('Ctrl Pts',(-0.482819504926692,0.108277624151794,
-0.72154688526459));
#64858=CARTESIAN_POINT('Ctrl Pts',(-0.487002394070417,0.0840375402405484,
-0.720753419609555));
#64859=CARTESIAN_POINT('Ctrl Pts',(-0.488365278047467,0.0761395489647055,
-0.720494889777558));
#64860=CARTESIAN_POINT('Ctrl Pts',(-0.489535259913778,0.068212597425999,
-0.720236359945562));
#64861=CARTESIAN_POINT('Ctrl Pts',(-0.490511524358925,0.0602667775070422,
-0.719977830113566));
#64862=CARTESIAN_POINT('Ctrl Pts',(-0.492960758624551,0.0403324507877492,
-0.71932923523094));
#64863=CARTESIAN_POINT('Ctrl Pts',(-0.494194016840838,0.020253694832792,
-0.718680640348315));
#64864=CARTESIAN_POINT('Ctrl Pts',(-0.494199978279349,0.000146521980200406,
-0.718032045465689));
#64865=CARTESIAN_POINT('',(-0.493957328857296,0.000144449760132726,-0.618032048526421));
#64866=CARTESIAN_POINT('Ctrl Pts',(-0.494199978279375,0.000146521891871864,
-0.71803204546284));
#64867=CARTESIAN_POINT('Ctrl Pts',(-0.494207244096923,-0.0243601700993693,
-0.717241535770997));
#64868=CARTESIAN_POINT('Ctrl Pts',(-0.492387304238366,-0.0489116703554373,
-0.716451026079155));
#64869=CARTESIAN_POINT('Ctrl Pts',(-0.488746376918454,-0.0732162485318961,
-0.715660516387312));
#64870=CARTESIAN_POINT('Ctrl Pts',(-0.485109097541938,-0.0974964752951923,
-0.714870798728475));
#64871=CARTESIAN_POINT('Ctrl Pts',(-0.479654529871509,-0.121529589269361,
-0.714081081069639));
#64872=CARTESIAN_POINT('Ctrl Pts',(-0.472440669219862,-0.145029149025596,
-0.713291363410802));
#64873=CARTESIAN_POINT('Ctrl Pts',(-0.46522265817095,-0.168542228936054,
-0.71250119139858));
#64874=CARTESIAN_POINT('Ctrl Pts',(-0.456243513596847,-0.191520475939915,
-0.711711019386358));
#64875=CARTESIAN_POINT('Ctrl Pts',(-0.4456114552376,-0.213691532263279,
-0.710920847374135));
#64876=CARTESIAN_POINT('Ctrl Pts',(-0.43497729975056,-0.235866961732167,
-0.710130519503881));
#64877=CARTESIAN_POINT('Ctrl Pts',(-0.422689903369407,-0.257234273154619,
-0.709340191633627));
#64878=CARTESIAN_POINT('Ctrl Pts',(-0.408903840618506,-0.277545111878116,
-0.708549863763373));
#64879=CARTESIAN_POINT('Ctrl Pts',(-0.395084683632739,-0.297904707935681,
-0.707757638665707));
#64880=CARTESIAN_POINT('Ctrl Pts',(-0.379760090875259,-0.317202212976357,
-0.706965413568041));
#64881=CARTESIAN_POINT('Ctrl Pts',(-0.363126562901895,-0.335220433916336,
-0.706173188470374));
#64882=CARTESIAN_POINT('Ctrl Pts',(-0.349006580853906,-0.350515863521925,
-0.70550067905596));
#64883=CARTESIAN_POINT('Ctrl Pts',(-0.33394424513909,-0.364889857227316,
-0.704828169641546));
#64884=CARTESIAN_POINT('Ctrl Pts',(-0.318078815963211,-0.378232080653455,
-0.704155660227131));
#64885=CARTESIAN_POINT('Ctrl Pts',(-0.299623197393985,-0.393752554993512,
-0.703373356950046));
#64886=CARTESIAN_POINT('Ctrl Pts',(-0.279968336043869,-0.407969816740406,
-0.702591053672961));
#64887=CARTESIAN_POINT('Ctrl Pts',(-0.259326300085853,-0.420694081351024,
-0.701808750395877));
#64888=CARTESIAN_POINT('Ctrl Pts',(-0.238723919473107,-0.433393901420054,
-0.701027949998964));
#64889=CARTESIAN_POINT('Ctrl Pts',(-0.217138687657615,-0.444605994987196,
-0.700247149602051));
#64890=CARTESIAN_POINT('Ctrl Pts',(-0.194814530887546,-0.454181614065415,
-0.699466349205139));
#64891=CARTESIAN_POINT('Ctrl Pts',(-0.172517371391529,-0.463745653059551,
-0.698686493053625));
#64892=CARTESIAN_POINT('Ctrl Pts',(-0.149483692726507,-0.471676835437457,
-0.69790663690211));
#64893=CARTESIAN_POINT('Ctrl Pts',(-0.125980905571912,-0.477872840231877,
-0.697126780750596));
#64894=CARTESIAN_POINT('Ctrl Pts',(-0.102470164077595,-0.484070942017038,
-0.696346660662693));
#64895=CARTESIAN_POINT('Ctrl Pts',(-0.0784906736443169,-0.488532484068602,
-0.69556654057479));
#64896=CARTESIAN_POINT('Ctrl Pts',(-0.0543247696931755,-0.491205109295275,
-0.694786420486887));
#64897=CARTESIAN_POINT('Ctrl Pts',(-0.0301566133277679,-0.493877983627432,
-0.694006227686884));
#64898=CARTESIAN_POINT('Ctrl Pts',(-0.00580271548859992,-0.494761555682616,
-0.693226034886882));
#64899=CARTESIAN_POINT('Ctrl Pts',(0.0184502740422664,-0.493855472165456,
-0.692445842086879));
#64900=CARTESIAN_POINT('Ctrl Pts',(0.0427572233526025,-0.492947372729115,
-0.691663913458335));
#64901=CARTESIAN_POINT('Ctrl Pts',(0.0669621087722994,-0.490241731562058,
-0.690881984829792));
#64902=CARTESIAN_POINT('Ctrl Pts',(0.0907827585528636,-0.485790212694258,
-0.690100056201248));
#64903=CARTESIAN_POINT('Ctrl Pts',(0.108721627968127,-0.482437860159601,
-0.689511200914398));
#64904=CARTESIAN_POINT('Ctrl Pts',(0.126442657763115,-0.478096476634594,
-0.688922345627547));
#64905=CARTESIAN_POINT('Ctrl Pts',(0.143831307851241,-0.472806720427916,
-0.688333490340696));
#64906=CARTESIAN_POINT('Ctrl Pts',(0.16718711327821,-0.46570171135055,-0.687542561232651));
#64907=CARTESIAN_POINT('Ctrl Pts',(0.190077963261476,-0.45684287391047,
-0.686751632124605));
#64908=CARTESIAN_POINT('Ctrl Pts',(0.212225147621608,-0.446311692337302,
-0.685960703016559));
#64909=CARTESIAN_POINT('Ctrl Pts',(0.234334212618236,-0.435798636857817,
-0.685171135242473));
#64910=CARTESIAN_POINT('Ctrl Pts',(0.25570151426798,-0.423619198931231,
-0.684381567468386));
#64911=CARTESIAN_POINT('Ctrl Pts',(0.276066477637526,-0.409903573935151,
-0.6835919996943));
#64912=CARTESIAN_POINT('Ctrl Pts',(0.296410082892266,-0.396202333442886,
-0.682803259993354));
#64913=CARTESIAN_POINT('Ctrl Pts',(0.315752852412834,-0.380968466591575,
-0.682014520292407));
#64914=CARTESIAN_POINT('Ctrl Pts',(0.333861132976999,-0.364376706016335,
-0.681225780591461));
#64915=CARTESIAN_POINT('Ctrl Pts',(0.351977287474953,-0.347777730928168,
-0.680436697926744));
#64916=CARTESIAN_POINT('Ctrl Pts',(0.368857356774819,-0.329820133027349,
-0.679647615262028));
#64917=CARTESIAN_POINT('Ctrl Pts',(0.384301967368983,-0.310717939418259,
-0.678858532597311));
#64918=CARTESIAN_POINT('Ctrl Pts',(0.399749177407836,-0.291612530765616,
-0.678069317124018));
#64919=CARTESIAN_POINT('Ctrl Pts',(0.413760033322562,-0.271362696072906,
-0.677280101650725));
#64920=CARTESIAN_POINT('Ctrl Pts',(0.426176682147419,-0.250214059544658,
-0.676490886177432));
#64921=CARTESIAN_POINT('Ctrl Pts',(0.43861987187072,-0.229020217275132,
-0.675699983736261));
#64922=CARTESIAN_POINT('Ctrl Pts',(0.449461731410235,-0.206924351775776,
-0.674909081295089));
#64923=CARTESIAN_POINT('Ctrl Pts',(0.458590583438979,-0.18419640816557,
-0.674118178853917));
#64924=CARTESIAN_POINT('Ctrl Pts',(0.464772876727418,-0.168804460437752,
-0.673582559387366));
#64925=CARTESIAN_POINT('Ctrl Pts',(0.470170522976654,-0.153123089496478,
-0.673046939920814));
#64926=CARTESIAN_POINT('Ctrl Pts',(0.47476192847652,-0.137239758340124,
-0.672511320454262));
#64927=CARTESIAN_POINT('Ctrl Pts',(0.481535664504905,-0.113806957097083,
-0.671721116914586));
#64928=CARTESIAN_POINT('Ctrl Pts',(0.48658864117106,-0.0898083330886664,
-0.670930913374909));
#64929=CARTESIAN_POINT('Ctrl Pts',(0.489837288117429,-0.0655215321078692,
-0.670140709835232));
#64930=CARTESIAN_POINT('Ctrl Pts',(0.493080401942685,-0.0412760965981491,
-0.669351852176459));
#64931=CARTESIAN_POINT('Ctrl Pts',(0.494525145611274,-0.0167441303366198,
-0.668562994517687));
#64932=CARTESIAN_POINT('Ctrl Pts',(0.494138672924038,0.00778536581481629,
-0.667774136858914));
#64933=CARTESIAN_POINT('Ctrl Pts',(0.493752597210261,0.032289665984111,
-0.666986089491693));
#64934=CARTESIAN_POINT('Ctrl Pts',(0.491539024476357,0.0567908121559613,
-0.666198042124471));
#64935=CARTESIAN_POINT('Ctrl Pts',(0.487517124062875,0.0809981095178388,
-0.66540999475725));
#64936=CARTESIAN_POINT('Ctrl Pts',(0.483493290450566,0.105217042552913,
-0.664621568600877));
#64937=CARTESIAN_POINT('Ctrl Pts',(0.477659485504374,0.129141158390872,
-0.663833142444504));
#64938=CARTESIAN_POINT('Ctrl Pts',(0.470086507952698,0.152487097948771,
-0.663044716288131));
#64939=CARTESIAN_POINT('Ctrl Pts',(0.462512070366296,0.175837538494852,
-0.662256138126875));
#64940=CARTESIAN_POINT('Ctrl Pts',(0.453198031838177,0.198608930707294,
-0.661467559965618));
#64941=CARTESIAN_POINT('Ctrl Pts',(0.442264297449436,0.220535555413535,
-0.660678981804362));
#64942=CARTESIAN_POINT('Ctrl Pts',(0.431306593626934,0.242510248671639,
-0.659888674885911));
#64943=CARTESIAN_POINT('Ctrl Pts',(0.418722446922477,0.263635873164357,
-0.659098367967459));
#64944=CARTESIAN_POINT('Ctrl Pts',(0.404677297416772,0.283672213929136,
-0.658308061049007));
#64945=CARTESIAN_POINT('Ctrl Pts',(0.395086998081313,0.297353414363736,
-0.657768424221947));
#64946=CARTESIAN_POINT('Ctrl Pts',(0.384816459366048,0.310527325364656,
-0.657228787394887));
#64947=CARTESIAN_POINT('Ctrl Pts',(0.373928785729749,0.323126760270139,
-0.656689150567828));
#64948=CARTESIAN_POINT('Ctrl Pts',(0.358022972409093,0.341533287343491,
-0.655900794586661));
#64949=CARTESIAN_POINT('Ctrl Pts',(0.340709666072,0.358814795169719,-0.655112438605495));
#64950=CARTESIAN_POINT('Ctrl Pts',(0.322174116471729,0.374749888159638,
-0.654324082624329));
#64951=CARTESIAN_POINT('Ctrl Pts',(0.303671294869083,0.390656844746979,
-0.653537118633864));
#64952=CARTESIAN_POINT('Ctrl Pts',(0.283950999955547,0.405221616003787,
-0.652750154643398));
#64953=CARTESIAN_POINT('Ctrl Pts',(0.263235856531688,0.418258919613232,
-0.651963190652933));
#64954=CARTESIAN_POINT('Ctrl Pts',(0.242543096654239,0.431282135891278,
-0.651177077008741));
#64955=CARTESIAN_POINT('Ctrl Pts',(0.220858192931202,0.442780768411191,
-0.650390963364548));
#64956=CARTESIAN_POINT('Ctrl Pts',(0.198433747993738,0.452612071930431,
-0.649604849720356));
#64957=CARTESIAN_POINT('Ctrl Pts',(0.175999603359157,0.462447627981525,
-0.648818396042586));
#64958=CARTESIAN_POINT('Ctrl Pts',(0.152825906399773,0.470614113568941,
-0.648031942364815));
#64959=CARTESIAN_POINT('Ctrl Pts',(0.129187428819195,0.477015983207151,
-0.647245488687044));
#64960=CARTESIAN_POINT('Ctrl Pts',(0.105545124682946,0.483418889168894,
-0.646458907699519));
#64961=CARTESIAN_POINT('Ctrl Pts',(0.0814385687965266,0.488056453694102,
-0.645672326711994));
#64962=CARTESIAN_POINT('Ctrl Pts',(0.0571546618842482,0.490883880999262,
-0.644885745724469));
#64963=CARTESIAN_POINT('Ctrl Pts',(0.032817603107085,0.493717496889916,
-0.64409744309279));
#64964=CARTESIAN_POINT('Ctrl Pts',(0.0083031147787867,0.494733021134595,
-0.643309140461111));
#64965=CARTESIAN_POINT('Ctrl Pts',(-0.0160983489333721,0.493937732069154,
-0.642520837829432));
#64966=CARTESIAN_POINT('Ctrl Pts',(-0.0331630875930237,0.493381560512369,
-0.641969552113419));
#64967=CARTESIAN_POINT('Ctrl Pts',(-0.0501725070709088,0.49194089521943,
-0.641418266397407));
#64968=CARTESIAN_POINT('Ctrl Pts',(-0.067029536706112,0.489633210892566,
-0.640866980681394));
#64969=CARTESIAN_POINT('Ctrl Pts',(-0.0911731719304014,0.486328008860752,
-0.640077396660969));
#64970=CARTESIAN_POINT('Ctrl Pts',(-0.115138288037024,0.481223649190943,
-0.639287812640545));
#64971=CARTESIAN_POINT('Ctrl Pts',(-0.138637569592122,0.474355630616513,
-0.638498228620121));
#64972=CARTESIAN_POINT('Ctrl Pts',(-0.162096057117822,0.467499534710909,
-0.63771001529325));
#64973=CARTESIAN_POINT('Ctrl Pts',(-0.185089642614131,0.458885999687149,
-0.63692180196638));
#64974=CARTESIAN_POINT('Ctrl Pts',(-0.207341068124737,0.448601517461648,
-0.636133588639509));
#64975=CARTESIAN_POINT('Ctrl Pts',(-0.229568978728543,0.438327903692233,
-0.635346208282324));
#64976=CARTESIAN_POINT('Ctrl Pts',(-0.25105564894622,0.426387113204784,
-0.63455882792514));
#64977=CARTESIAN_POINT('Ctrl Pts',(-0.271543256460522,0.412913913389723,
-0.633771447567955));
#64978=CARTESIAN_POINT('Ctrl Pts',(-0.292040020441645,0.399434692036666,
-0.632983715309158));
#64979=CARTESIAN_POINT('Ctrl Pts',(-0.3115362382033,0.384422055600117,-0.632195983050361));
#64980=CARTESIAN_POINT('Ctrl Pts',(-0.329801650634823,0.368055038327892,
-0.631408250791564));
#64981=CARTESIAN_POINT('Ctrl Pts',(-0.348070214991009,0.351685196722759,
-0.630620382599744));
#64982=CARTESIAN_POINT('Ctrl Pts',(-0.365107052144935,0.333960991305438,
-0.629832514407923));
#64983=CARTESIAN_POINT('Ctrl Pts',(-0.380717878936952,0.315099248900642,
-0.629044646216103));
#64984=CARTESIAN_POINT('Ctrl Pts',(-0.396362675980733,0.296196462024162,
-0.628255063567951));
#64985=CARTESIAN_POINT('Ctrl Pts',(-0.410574852499632,0.27615175415103,
-0.627465480919799));
#64986=CARTESIAN_POINT('Ctrl Pts',(-0.423201864383091,0.255213287237706,
-0.626675898271647));
#64987=CARTESIAN_POINT('Ctrl Pts',(-0.431896652276968,0.240795344947433,
-0.626132202446085));
#64988=CARTESIAN_POINT('Ctrl Pts',(-0.439840744309758,0.22595425813607,
-0.625588506620522));
#64989=CARTESIAN_POINT('Ctrl Pts',(-0.446997421954708,0.210777002459577,
-0.625044810794959));
#64990=CARTESIAN_POINT('Ctrl Pts',(-0.458220859400495,0.186975318475107,
-0.624192161508451));
#64991=CARTESIAN_POINT('Ctrl Pts',(-0.467560202617464,0.162231059761754,
-0.623339512221943));
#64992=CARTESIAN_POINT('Ctrl Pts',(-0.474875071827669,0.13684774808767,
-0.622486862935434));
#64993=CARTESIAN_POINT('Ctrl Pts',(-0.482151827518084,0.111596694055384,
-0.621638656307369));
#64994=CARTESIAN_POINT('Ctrl Pts',(-0.487424918762182,0.0857136895848494,
-0.620790449679303));
#64995=CARTESIAN_POINT('Ctrl Pts',(-0.490602792428975,0.0595192410980851,
-0.619942243051237));
#64996=CARTESIAN_POINT('Ctrl Pts',(-0.492988355924927,0.0398556148313835,
-0.619305512022537));
#64997=CARTESIAN_POINT('Ctrl Pts',(-0.49419416568895,0.020016978509648,
-0.618668780993836));
#64998=CARTESIAN_POINT('Ctrl Pts',(-0.494199978855518,0.000144565574625915,
-0.618032049965136));
#64999=CARTESIAN_POINT('',(-0.494183370864054,-0.00044364358185519,-0.518032045465689));
#65000=CARTESIAN_POINT('Ctrl Pts',(-0.493441113705293,0.000144203375642127,
-0.618032045465689));
#65001=CARTESIAN_POINT('Ctrl Pts',(-0.49319563664091,-0.0913624936415018,
-0.615095577279967));
#65002=CARTESIAN_POINT('Ctrl Pts',(-0.42500180876295,-0.347559668173545,
-0.606885052465435));
#65003=CARTESIAN_POINT('Ctrl Pts',(-0.0134997172395283,-0.583292780708831,
-0.59340047102209));
#65004=CARTESIAN_POINT('Ctrl Pts',(0.481597770827401,-0.329343127216554,
-0.577578301135657));
#65005=CARTESIAN_POINT('Ctrl Pts',(0.538669550813453,0.224150668479914,
-0.561756131249221));
#65006=CARTESIAN_POINT('Ctrl Pts',(0.105791851363253,0.573773597596928,
-0.545933961362787));
#65007=CARTESIAN_POINT('Ctrl Pts',(-0.381589922382086,0.415101937259952,
-0.531359266101609));
#65008=CARTESIAN_POINT('Ctrl Pts',(-0.493051107525581,0.124562909647714,
-0.522058627469244));
#65009=CARTESIAN_POINT('Ctrl Pts',(-0.494183370864054,-0.00044364358185519,
-0.518032045465689));
#65010=CARTESIAN_POINT('',(-0.494856786895912,0.000236248404645519,-0.418032045465689));
#65011=CARTESIAN_POINT('Ctrl Pts',(-0.494183370864054,-0.00044364358185519,
-0.518032045465689));
#65012=CARTESIAN_POINT('Ctrl Pts',(-0.49453415715938,-0.0391719007009277,
-0.516784570840433));
#65013=CARTESIAN_POINT('Ctrl Pts',(-0.472722741173915,-0.241244450658913,
-0.510263039586364));
#65014=CARTESIAN_POINT('Ctrl Pts',(-0.195405102640593,-0.549749372943316,
-0.498467451703485));
#65015=CARTESIAN_POINT('Ctrl Pts',(0.354308135899791,-0.463544097374131,
-0.482645281817051));
#65016=CARTESIAN_POINT('Ctrl Pts',(0.581762127488868,0.0442755404655635,
-0.466823111930615));
#65017=CARTESIAN_POINT('Ctrl Pts',(0.280076793883528,0.511824640016281,
-0.451000942044181));
#65018=CARTESIAN_POINT('Ctrl Pts',(-0.276351126568424,0.513845803011739,
-0.435178772157748));
#65019=CARTESIAN_POINT('Ctrl Pts',(-0.488246889901193,0.190630286924777,
-0.424189139964916));
#65020=CARTESIAN_POINT('Ctrl Pts',(-0.494937727816466,0.0138949803393536,
-0.418473564400897));
#65021=CARTESIAN_POINT('Ctrl Pts',(-0.494856786895912,0.000236248404645519,
-0.418032045465689));
#65022=CARTESIAN_POINT('',(-0.493522771508053,0.000241867023412317,-0.318032045465689));
#65023=CARTESIAN_POINT('Ctrl Pts',(-0.494856786895912,0.000236248404645519,
-0.418032045465689));
#65024=CARTESIAN_POINT('Ctrl Pts',(-0.493970867814446,-0.149262066747403,
-0.413199507772085));
#65025=CARTESIAN_POINT('Ctrl Pts',(-0.34234445800717,-0.463474892665707,
-0.403092913449672));
#65026=CARTESIAN_POINT('Ctrl Pts',(0.191406249927459,-0.551154335841721,
-0.387712262498443));
#65027=CARTESIAN_POINT('Ctrl Pts',(0.566386150012029,-0.140050711081548,
-0.37189009261201));
#65028=CARTESIAN_POINT('Ctrl Pts',(0.426211974611545,0.398435501884038,
-0.356067922725576));
#65029=CARTESIAN_POINT('Ctrl Pts',(-0.101621460572443,0.574526295417654,
-0.34024575283914));
#65030=CARTESIAN_POINT('Ctrl Pts',(-0.450519577851589,0.296895367549325,
-0.327567127085845));
#65031=CARTESIAN_POINT('Ctrl Pts',(-0.493818787931586,0.0666086579641146,
-0.320162557961362));
#65032=CARTESIAN_POINT('Ctrl Pts',(-0.493522771508053,0.000241867023412317,
-0.318032045465689));
#65033=CARTESIAN_POINT('',(-0.494175246121693,-0.000437982247251857,-0.218032043771887));
#65034=CARTESIAN_POINT('Ctrl Pts',(-0.493522771508053,0.000241867023412317,
-0.318032045465689));
#65035=CARTESIAN_POINT('Ctrl Pts',(-0.493086003034083,-0.0976814902536105,
-0.31488850133255));
#65036=CARTESIAN_POINT('Ctrl Pts',(-0.417562805783599,-0.360516000773604,
-0.3064709005706));
#65037=CARTESIAN_POINT('Ctrl Pts',(0.00926706993024401,-0.583370379414318,
-0.292779243179837));
#65038=CARTESIAN_POINT('Ctrl Pts',(0.49408565294531,-0.310302150601255,
-0.276957073293404));
#65039=CARTESIAN_POINT('Ctrl Pts',(0.529510809583032,0.245003489134929,
-0.26113490340697));
#65040=CARTESIAN_POINT('Ctrl Pts',(0.0833216145626671,0.577460662606022,
-0.245312733520534));
#65041=CARTESIAN_POINT('Ctrl Pts',(-0.390666567691133,0.402424062808438,
-0.230945114206776));
#65042=CARTESIAN_POINT('Ctrl Pts',(-0.492979328796984,0.118255994136513,
-0.221851551521826));
#65043=CARTESIAN_POINT('Ctrl Pts',(-0.493995525633567,-0.000437770324621543,
-0.218032045465689));
#65044=CARTESIAN_POINT('',(-0.490426859062112,0.0609519147399937,-0.120013405629935));
#65045=CARTESIAN_POINT('Ctrl Pts',(-0.494199805894521,-0.000438011207620882,
-0.21803204354042));
#65046=CARTESIAN_POINT('Ctrl Pts',(-0.494172750277752,-0.0309643546498033,
-0.217050118877898));
#65047=CARTESIAN_POINT('Ctrl Pts',(-0.491313369343038,-0.0613653915007896,
-0.216068194215376));
#65048=CARTESIAN_POINT('Ctrl Pts',(-0.485713819065904,-0.0911906024128288,
-0.215086269552854));
#65049=CARTESIAN_POINT('Ctrl Pts',(-0.483018613360579,-0.105546233603582,
-0.214613644284458));
#65050=CARTESIAN_POINT('Ctrl Pts',(-0.479689296480285,-0.11976880665172,
-0.214141019016061));
#65051=CARTESIAN_POINT('Ctrl Pts',(-0.475740012640402,-0.133809866500606,
-0.213668393747665));
#65052=CARTESIAN_POINT('Ctrl Pts',(-0.46914374763369,-0.15726185311221,
-0.212878994543758));
#65053=CARTESIAN_POINT('Ctrl Pts',(-0.46079092504738,-0.180289888503342,
-0.21208959533985));
#65054=CARTESIAN_POINT('Ctrl Pts',(-0.450756093102774,-0.202614373948947,
-0.211300196135942));
#65055=CARTESIAN_POINT('Ctrl Pts',(-0.440738742206839,-0.224899969314599,
-0.210512172094666));
#65056=CARTESIAN_POINT('Ctrl Pts',(-0.429045431654185,-0.246483800410652,
-0.20972414805339));
#65057=CARTESIAN_POINT('Ctrl Pts',(-0.415799841100531,-0.267103223755861,
-0.208936124012114));
#65058=CARTESIAN_POINT('Ctrl Pts',(-0.402568315817015,-0.287700751681739,
-0.208148936760333));
#65059=CARTESIAN_POINT('Ctrl Pts',(-0.387788132945832,-0.307335309549207,
-0.207361749508551));
#65060=CARTESIAN_POINT('Ctrl Pts',(-0.3716281231461,-0.325770130746985,
-0.206574562256769));
#65061=CARTESIAN_POINT('Ctrl Pts',(-0.355460960498201,-0.344213111684677,
-0.205787026575069));
#65062=CARTESIAN_POINT('Ctrl Pts',(-0.337913191277882,-0.361454758624169,
-0.204999490893369));
#65063=CARTESIAN_POINT('Ctrl Pts',(-0.319193707533974,-0.377291686988616,
-0.204211955211669));
#65064=CARTESIAN_POINT('Ctrl Pts',(-0.300471045810742,-0.393131303965184,
-0.20342428583119));
#65065=CARTESIAN_POINT('Ctrl Pts',(-0.28057682017882,-0.407565299330699,
-0.202636616450712));
#65066=CARTESIAN_POINT('Ctrl Pts',(-0.259752412171317,-0.420431117272714,
-0.201848947070233));
#65067=CARTESIAN_POINT('Ctrl Pts',(-0.238882683742495,-0.433324935256292,
-0.201059563474966));
#65068=CARTESIAN_POINT('Ctrl Pts',(-0.217079341425805,-0.444643427712769,
-0.200270179879698));
#65069=CARTESIAN_POINT('Ctrl Pts',(-0.194609064591469,-0.454269690799236,
-0.19948079628443));
#65070=CARTESIAN_POINT('Ctrl Pts',(-0.179099370244633,-0.460914041435148,
-0.198935938810031));
#65071=CARTESIAN_POINT('Ctrl Pts',(-0.163272437722091,-0.466753171034724,
-0.198391081335632));
#65072=CARTESIAN_POINT('Ctrl Pts',(-0.147220088809954,-0.471762530783009,
-0.197846223861232));
#65073=CARTESIAN_POINT('Ctrl Pts',(-0.123957690090648,-0.479021887306522,
-0.197056638992124));
#65074=CARTESIAN_POINT('Ctrl Pts',(-0.100092955879836,-0.484576542004863,
-0.196267054123016));
#65075=CARTESIAN_POINT('Ctrl Pts',(-0.0759010851752448,-0.488336631095006,
-0.195477469253907));
#65076=CARTESIAN_POINT('Ctrl Pts',(-0.0517512198782043,-0.492090191377329,
-0.194689255375684));
#65077=CARTESIAN_POINT('Ctrl Pts',(-0.0272760151105899,-0.494055214548706,
-0.19390104149746));
#65078=CARTESIAN_POINT('Ctrl Pts',(-0.00276321768710077,-0.494192274957848,
-0.193112827619237));
#65079=CARTESIAN_POINT('Ctrl Pts',(0.0217236658700617,-0.494329190472671,
-0.192325447006541));
#65080=CARTESIAN_POINT('Ctrl Pts',(0.046247373601404,-0.492641948741059,
-0.191538066393845));
#65081=CARTESIAN_POINT('Ctrl Pts',(0.0705172555593016,-0.489143084044315,
-0.190750685781149));
#65082=CARTESIAN_POINT('Ctrl Pts',(0.0947979704728245,-0.485642657615789,
-0.189962953718073));
#65083=CARTESIAN_POINT('Ctrl Pts',(0.11882394383847,-0.48032906976862,-0.189175221654997));
#65084=CARTESIAN_POINT('Ctrl Pts',(0.142310683354916,-0.473266636689147,
-0.188387489591921));
#65085=CARTESIAN_POINT('Ctrl Pts',(0.165801468263671,-0.466202987165286,
-0.187599621848657));
#65086=CARTESIAN_POINT('Ctrl Pts',(0.1887521778002,-0.45739011747967,-0.186811754105393));
#65087=CARTESIAN_POINT('Ctrl Pts',(0.210894842896268,-0.446941836528825,
-0.186023886362129));
#65088=CARTESIAN_POINT('Ctrl Pts',(0.233085680856849,-0.436470824636584,
-0.185234304559338));
#65089=CARTESIAN_POINT('Ctrl Pts',(0.254464352083612,-0.424357627123245,
-0.184444722756548));
#65090=CARTESIAN_POINT('Ctrl Pts',(0.274787370646444,-0.410762146422007,
-0.183655140953757));
#65091=CARTESIAN_POINT('Ctrl Pts',(0.288781534322225,-0.401400476963514,
-0.183111445294104));
#65092=CARTESIAN_POINT('Ctrl Pts',(0.302275715266755,-0.391336939837268,
-0.18256774963445));
#65093=CARTESIAN_POINT('Ctrl Pts',(0.315199736804966,-0.380634688274834,
-0.182024053974797));
#65094=CARTESIAN_POINT('Ctrl Pts',(0.333938307202834,-0.365117467591981,
-0.181235748309775));
#65095=CARTESIAN_POINT('Ctrl Pts',(0.351580955646325,-0.348169540189685,
-0.180447442644754));
#65096=CARTESIAN_POINT('Ctrl Pts',(0.367902590472904,-0.329971701700808,
-0.179659136979733));
#65097=CARTESIAN_POINT('Ctrl Pts',(0.38419576896201,-0.311805590660732,
-0.178872205704732));
#65098=CARTESIAN_POINT('Ctrl Pts',(0.399172006415922,-0.292394370584428,
-0.178085274429732));
#65099=CARTESIAN_POINT('Ctrl Pts',(0.412641578489278,-0.27195692251141,
-0.177298343154732));
#65100=CARTESIAN_POINT('Ctrl Pts',(0.426096895277571,-0.251541104052655,
-0.176512244714627));
#65101=CARTESIAN_POINT('Ctrl Pts',(0.438048308175922,-0.230101776433988,
-0.175726146274522));
#65102=CARTESIAN_POINT('Ctrl Pts',(0.448348028550459,-0.207888636762371,
-0.174940047834417));
#65103=CARTESIAN_POINT('Ctrl Pts',(0.45865255445566,-0.185665133127465,
-0.174153582625116));
#65104=CARTESIAN_POINT('Ctrl Pts',(0.467303535332435,-0.162667718136668,
-0.173367117415816));
#65105=CARTESIAN_POINT('Ctrl Pts',(0.474199930407406,-0.139169199184342,
-0.172580652206515));
#65106=CARTESIAN_POINT('Ctrl Pts',(0.481097573071553,-0.115666429243265,
-0.171794044722088));
#65107=CARTESIAN_POINT('Ctrl Pts',(0.48623982790186,-0.0916630503429066,
-0.17100743723766));
#65108=CARTESIAN_POINT('Ctrl Pts',(0.489576155418217,-0.0674450001550752,
-0.170220829753233));
#65109=CARTESIAN_POINT('Ctrl Pts',(0.492919884988233,-0.0431732192390262,
-0.169432477083185));
#65110=CARTESIAN_POINT('Ctrl Pts',(0.494449629709502,-0.0186865116197863,
-0.168644124413136));
#65111=CARTESIAN_POINT('Ctrl Pts',(0.494166843308743,0.00572459380850489,
-0.167855771743088));
#65112=CARTESIAN_POINT('Ctrl Pts',(0.493969090469221,0.0227953065491065,
-0.167304475858179));
#65113=CARTESIAN_POINT('Ctrl Pts',(0.492886082646355,0.0398289838668983,
-0.166753179973271));
#65114=CARTESIAN_POINT('Ctrl Pts',(0.490933341258643,0.0567282508158417,
-0.166201884088363));
#65115=CARTESIAN_POINT('Ctrl Pts',(0.488133993899746,0.0809541511826329,
-0.165411575300368));
#65116=CARTESIAN_POINT('Ctrl Pts',(0.483529467227842,0.105038900077909,
-0.164621266512374));
#65117=CARTESIAN_POINT('Ctrl Pts',(0.477149307483064,0.128694127171494,
-0.163830957724379));
#65118=CARTESIAN_POINT('Ctrl Pts',(0.470780310953839,0.152307965270199,
-0.163042031721097));
#65119=CARTESIAN_POINT('Ctrl Pts',(0.462641976466881,0.175493099130243,
-0.162253105717814));
#65120=CARTESIAN_POINT('Ctrl Pts',(0.452815041473334,0.197970144757997,
-0.161464179714532));
#65121=CARTESIAN_POINT('Ctrl Pts',(0.442998656932671,0.220423058445223,
-0.160676100722716));
#65122=CARTESIAN_POINT('Ctrl Pts',(0.43149752188693,0.24216875149014,-0.159888021730901));
#65123=CARTESIAN_POINT('Ctrl Pts',(0.418441051031408,0.262946243197598,
-0.159099942739085));
#65124=CARTESIAN_POINT('Ctrl Pts',(0.405379232005872,0.283732245746872,
-0.158311540935655));
#65125=CARTESIAN_POINT('Ctrl Pts',(0.39076115327825,0.303548656609079,-0.157523139132226));
#65126=CARTESIAN_POINT('Ctrl Pts',(0.374761072967117,0.322161105952496,
-0.156734737328796));
#65127=CARTESIAN_POINT('Ctrl Pts',(0.358758544707163,0.340776402926834,
-0.155946214903018));
#65128=CARTESIAN_POINT('Ctrl Pts',(0.341374064153866,0.358186863061602,
-0.155157692477239));
#65129=CARTESIAN_POINT('Ctrl Pts',(0.322820463086095,0.374193250357191,
-0.154369170051461));
#65130=CARTESIAN_POINT('Ctrl Pts',(0.304227342540955,0.390233731522653,
-0.153578968059864));
#65131=CARTESIAN_POINT('Ctrl Pts',(0.284460677467843,0.40486374277383,-0.152788766068268));
#65132=CARTESIAN_POINT('Ctrl Pts',(0.263765544119174,0.417925086272069,
-0.151998564076671));
#65133=CARTESIAN_POINT('Ctrl Pts',(0.249633160085072,0.42684447418847,-0.151458947451757));
#65134=CARTESIAN_POINT('Ctrl Pts',(0.235068449819283,0.435033240514805,
-0.150919330826843));
#65135=CARTESIAN_POINT('Ctrl Pts',(0.220155539841901,0.442453588839463,
-0.150379714201929));
#65136=CARTESIAN_POINT('Ctrl Pts',(0.198298032359417,0.453329421877741,
-0.149588810586563));
#65137=CARTESIAN_POINT('Ctrl Pts',(0.175574231759261,0.462610811271088,
-0.148797906971198));
#65138=CARTESIAN_POINT('Ctrl Pts',(0.152242765825034,0.470165694467327,
-0.148007003355832));
#65139=CARTESIAN_POINT('Ctrl Pts',(0.128951195010208,0.477707659359674,
-0.14721745212845));
#65140=CARTESIAN_POINT('Ctrl Pts',(0.105054656046012,0.483528720307415,
-0.146427900901068));
#65141=CARTESIAN_POINT('Ctrl Pts',(0.0808320197756471,0.487544689827496,
-0.145638349673686));
#65142=CARTESIAN_POINT('Ctrl Pts',(0.0566345148620286,0.491556492717588,
-0.144849617617816));
#65143=CARTESIAN_POINT('Ctrl Pts',(0.0321122579899425,0.49376678450621,
-0.144060885561945));
#65144=CARTESIAN_POINT('Ctrl Pts',(0.00755510785655334,0.494142247075957,
-0.143272153506075));
#65145=CARTESIAN_POINT('Ctrl Pts',(-0.0170131427268601,0.494517879364236,
-0.142483064923461));
#65146=CARTESIAN_POINT('Ctrl Pts',(-0.0416156278715312,0.493056993651087,
-0.141693976340847));
#65147=CARTESIAN_POINT('Ctrl Pts',(-0.065960445619597,0.48977837805855,
-0.140904887758233));
#65148=CARTESIAN_POINT('Ctrl Pts',(-0.0903095954698473,0.486499179044198,
-0.14011565875919));
#65149=CARTESIAN_POINT('Ctrl Pts',(-0.114400305547835,0.48140172413962,
-0.139326429760147));
#65150=CARTESIAN_POINT('Ctrl Pts',(-0.137949186516829,0.474556279001074,
-0.138537200761103));
#65151=CARTESIAN_POINT('Ctrl Pts',(-0.161548758335482,0.467696098494388,
-0.13774627288352));
#65152=CARTESIAN_POINT('Ctrl Pts',(-0.184603518314131,0.459080642868388,
-0.136955345005936));
#65153=CARTESIAN_POINT('Ctrl Pts',(-0.206846964820815,0.448829559125083,
-0.136164417128352));
#65154=CARTESIAN_POINT('Ctrl Pts',(-0.221910449313245,0.441887422664734,
-0.135628792857399));
#65155=CARTESIAN_POINT('Ctrl Pts',(-0.23660225795376,0.434196191489723,
-0.135093168586447));
#65156=CARTESIAN_POINT('Ctrl Pts',(-0.250846662107074,0.425804640779946,
-0.134557544315494));
#65157=CARTESIAN_POINT('Ctrl Pts',(-0.271427480270615,0.413680231965847,
-0.133783655453187));
#65158=CARTESIAN_POINT('Ctrl Pts',(-0.291196252392501,0.400019231727095,
-0.13300976659088));
#65159=CARTESIAN_POINT('Ctrl Pts',(-0.309907271780441,0.384956001248979,
-0.132235877728573));
#65160=CARTESIAN_POINT('Ctrl Pts',(-0.328585302606954,0.369919328078811,
-0.131463353275106));
#65161=CARTESIAN_POINT('Ctrl Pts',(-0.346208685401953,0.35348572733314,
-0.13069082882164));
#65162=CARTESIAN_POINT('Ctrl Pts',(-0.362559905979217,0.335833224348547,
-0.129918304368173));
#65163=CARTESIAN_POINT('Ctrl Pts',(-0.378894395704946,0.318198783710141,
-0.129146570375081));
#65164=CARTESIAN_POINT('Ctrl Pts',(-0.393958795340787,0.299348422171846,
-0.128374836381989));
#65165=CARTESIAN_POINT('Ctrl Pts',(-0.407571780799048,0.279497555438849,
-0.127603102388897));
#65166=CARTESIAN_POINT('Ctrl Pts',(-0.421191283860761,0.259637184539559,
-0.126830998906235));
#65167=CARTESIAN_POINT('Ctrl Pts',(-0.433357563228689,0.238775938819434,
-0.126058895423573));
#65168=CARTESIAN_POINT('Ctrl Pts',(-0.443931768323362,0.217159446198623,
-0.125286791940911));
#65169=CARTESIAN_POINT('Ctrl Pts',(-0.454509246755392,0.195536262004101,
-0.124514449446886));
#65170=CARTESIAN_POINT('Ctrl Pts',(-0.463493389163292,0.173158031484789,
-0.123742106952861));
#65171=CARTESIAN_POINT('Ctrl Pts',(-0.470793200383583,0.150291059190437,
-0.122969764458837));
#65172=CARTESIAN_POINT('Ctrl Pts',(-0.478107688939874,0.12737810951043,
-0.12219586905749));
#65173=CARTESIAN_POINT('Ctrl Pts',(-0.483730932047285,0.103975162145308,
-0.121421973656143));
#65174=CARTESIAN_POINT('Ctrl Pts',(-0.487622669413537,0.0803602655173329,
-0.120648078254796));
#65175=CARTESIAN_POINT('Ctrl Pts',(-0.488686542371567,0.0739047297077928,
-0.120436520713176));
#65176=CARTESIAN_POINT('Ctrl Pts',(-0.489621320718089,0.0674333787202251,
-0.120224963171555));
#65177=CARTESIAN_POINT('Ctrl Pts',(-0.490426859062112,0.0609519147399937,
-0.120013405629935));
#65178=CARTESIAN_POINT('',(-0.253382212491109,0.424300712223195,-0.12));
#65179=CARTESIAN_POINT('Origin',(0.,0.,-0.12));
#65180=CARTESIAN_POINT('',(-0.49396390682824,-0.000458628609927681,-0.203567954534311));
#65181=CARTESIAN_POINT('Ctrl Pts',(-0.253382212491106,0.424300712223197,
-0.12));
#65182=CARTESIAN_POINT('Ctrl Pts',(-0.183080092417522,0.466283452798211,
-0.122637028314406));
#65183=CARTESIAN_POINT('Ctrl Pts',(-0.0218069960358891,0.513732009672345,
-0.127911084943216));
#65184=CARTESIAN_POINT('Ctrl Pts',(0.310758681059315,0.447140495242652,
-0.138459198200843));
#65185=CARTESIAN_POINT('Ctrl Pts',(0.579077760680187,0.0710394712093248,
-0.151644339772866));
#65186=CARTESIAN_POINT('Ctrl Pts',(0.374813391339547,-0.447521999574274,
-0.167466509659305));
#65187=CARTESIAN_POINT('Ctrl Pts',(-0.170557872637833,-0.557786202019076,
-0.183288679545736));
#65188=CARTESIAN_POINT('Ctrl Pts',(-0.467287313083341,-0.25627684446579,
-0.195322494504073));
#65189=CARTESIAN_POINT('Ctrl Pts',(-0.494353707556968,-0.0466364371496805,
-0.202082252833598));
#65190=CARTESIAN_POINT('Ctrl Pts',(-0.49396390682824,-0.000458628609927681,
-0.203567954534311));
#65191=CARTESIAN_POINT('',(-0.493537605131362,0.000254761609798343,-0.303567954534311));
#65192=CARTESIAN_POINT('Ctrl Pts',(-0.49396390682824,-0.000458628609927681,
-0.203567954534311));
#65193=CARTESIAN_POINT('Ctrl Pts',(-0.492969963352949,0.117289051470408,
-0.207356309462409));
#65194=CARTESIAN_POINT('Ctrl Pts',(-0.392003835461347,0.400544594774385,
-0.21641872101932));
#65195=CARTESIAN_POINT('Ctrl Pts',(0.0799333386512568,0.577918330084977,
-0.230755189205039));
#65196=CARTESIAN_POINT('Ctrl Pts',(0.5280611079658,0.248119757234704,-0.246577359091475));
#65197=CARTESIAN_POINT('Ctrl Pts',(0.495900283769359,-0.307401514562771,
-0.26239952897791));
#65198=CARTESIAN_POINT('Ctrl Pts',(0.0126918090925729,-0.583302937513682,
-0.278221698864343));
#65199=CARTESIAN_POINT('Ctrl Pts',(-0.416412681034692,-0.362461323671283,
-0.291944507383144));
#65200=CARTESIAN_POINT('Ctrl Pts',(-0.493071761030911,-0.0986317868095975,
-0.300393259273133));
#65201=CARTESIAN_POINT('Ctrl Pts',(-0.493537605131362,0.000254761609798343,
-0.303567954534311));
#65202=CARTESIAN_POINT('',(-0.494874876107118,0.000221385223355512,-0.403567954534311));
#65203=CARTESIAN_POINT('Ctrl Pts',(-0.493537605131362,0.000254761609798343,
-0.303567954534311));
#65204=CARTESIAN_POINT('Ctrl Pts',(-0.493845658354544,0.0656464236281961,
-0.305667315901945));
#65205=CARTESIAN_POINT('Ctrl Pts',(-0.451402068223567,0.294932643527596,
-0.313040733898388));
#65206=CARTESIAN_POINT('Ctrl Pts',(-0.104993157557767,0.57391933243674,
-0.325688208523647));
#65207=CARTESIAN_POINT('Ctrl Pts',(0.423865099612549,0.400931541670995,
-0.341510378410082));
#65208=CARTESIAN_POINT('Ctrl Pts',(0.567198827523238,-0.136722713111685,
-0.357332548296515));
#65209=CARTESIAN_POINT('Ctrl Pts',(0.194639240804606,-0.550020940519229,
-0.373154718182949));
#65210=CARTESIAN_POINT('Ctrl Pts',(-0.340699208879849,-0.465305939894536,
-0.388566520262216));
#65211=CARTESIAN_POINT('Ctrl Pts',(-0.494030155161132,-0.150226124138736,
-0.398704265712668));
#65212=CARTESIAN_POINT('Ctrl Pts',(-0.494874876107118,0.000221385223355512,
-0.403567954534311));
#65213=CARTESIAN_POINT('',(-0.494154610429637,-0.000443820138194773,-0.503567954534311));
#65214=CARTESIAN_POINT('Ctrl Pts',(-0.494874876107118,0.000221385223355512,
-0.403567954534311));
#65215=CARTESIAN_POINT('Ctrl Pts',(-0.494946148405776,0.0129152101729008,
-0.40397832234148));
#65216=CARTESIAN_POINT('Ctrl Pts',(-0.488762631718723,0.1886798315986,-0.409662746777461));
#65217=CARTESIAN_POINT('Ctrl Pts',(-0.279363609231548,0.512214322021286,
-0.420621227842251));
#65218=CARTESIAN_POINT('Ctrl Pts',(0.27706667089454,0.513460431776094,-0.436443397728689));
#65219=CARTESIAN_POINT('Ctrl Pts',(0.58149216890127,0.0476908023280638,
-0.45226556761512));
#65220=CARTESIAN_POINT('Ctrl Pts',(0.357023961520341,-0.461455771170997,
-0.468087737501555));
#65221=CARTESIAN_POINT('Ctrl Pts',(-0.192173816477921,-0.550887266295114,
-0.48390990738799));
#65222=CARTESIAN_POINT('Ctrl Pts',(-0.472035147994241,-0.243205736814157,
-0.495736646398908));
#65223=CARTESIAN_POINT('Ctrl Pts',(-0.494512371951871,-0.0401451165327019,
-0.502289328781015));
#65224=CARTESIAN_POINT('Ctrl Pts',(-0.494154610429637,-0.000443820138194773,
-0.503567954534311));
#65225=CARTESIAN_POINT('',(-0.493923623855364,0.000162705886329681,-0.603567957626487));
#65226=CARTESIAN_POINT('Ctrl Pts',(-0.494154610429637,-0.000443820138194773,
-0.503567954534311));
#65227=CARTESIAN_POINT('Ctrl Pts',(-0.493036682507162,0.123614204662111,
-0.507563385409827));
#65228=CARTESIAN_POINT('Ctrl Pts',(-0.382981343090829,0.413199679253085,
-0.516832872914155));
#65229=CARTESIAN_POINT('Ctrl Pts',(0.10242155967994,0.574384395972835,-0.531376417047293));
#65230=CARTESIAN_POINT('Ctrl Pts',(0.537342980930237,0.227310898597556,
-0.547198586933727));
#65231=CARTESIAN_POINT('Ctrl Pts',(0.483525636177959,-0.326511749309766,
-0.563020756820162));
#65232=CARTESIAN_POINT('Ctrl Pts',(-0.0100788586177245,-0.583357998977174,
-0.578842926706596));
#65233=CARTESIAN_POINT('Ctrl Pts',(-0.423901001261801,-0.349516357851695,
-0.592358659277979));
#65234=CARTESIAN_POINT('Ctrl Pts',(-0.493178983690631,-0.0923124040730076,
-0.60060033522055));
#65235=CARTESIAN_POINT('Ctrl Pts',(-0.493454077256828,0.000162454800537643,
-0.60356795453431));
#65236=CARTESIAN_POINT('Ctrl Pts',(-0.494199973167426,0.00016285366162209,
-0.603567959446373));
#65237=CARTESIAN_POINT('Ctrl Pts',(-0.494191229533384,0.0266965137958892,
-0.604418169378795));
#65238=CARTESIAN_POINT('Ctrl Pts',(-0.492041366961323,0.0531673311879112,
-0.605268379311217));
#65239=CARTESIAN_POINT('Ctrl Pts',(-0.487805636429523,0.0792420410362358,
-0.606118589243638));
#65240=CARTESIAN_POINT('Ctrl Pts',(-0.483545285296569,0.105468312705251,
-0.606973741105082));
#65241=CARTESIAN_POINT('Ctrl Pts',(-0.477174931701992,0.131293374138508,
-0.607828892966525));
#65242=CARTESIAN_POINT('Ctrl Pts',(-0.468800804875319,0.156395157687997,
-0.608684044827968));
#65243=CARTESIAN_POINT('Ctrl Pts',(-0.462914752160757,0.174038838546902,
-0.6092851187118));
#65244=CARTESIAN_POINT('Ctrl Pts',(-0.456039796877744,0.191325538833742,
-0.609886192595632));
#65245=CARTESIAN_POINT('Ctrl Pts',(-0.448226612564715,0.20815029134921,
-0.610487266479464));
#65246=CARTESIAN_POINT('Ctrl Pts',(-0.437966149383268,0.230244964507506,
-0.611276611285282));
#65247=CARTESIAN_POINT('Ctrl Pts',(-0.426039665523985,0.251640350874873,
-0.6120659560911));
#65248=CARTESIAN_POINT('Ctrl Pts',(-0.412565452518453,0.272072393653315,
-0.612855300896918));
#65249=CARTESIAN_POINT('Ctrl Pts',(-0.399114683965311,0.292468885705791,
-0.613643272282506));
#65250=CARTESIAN_POINT('Ctrl Pts',(-0.384121865758108,0.311904759778303,
-0.614431243668095));
#65251=CARTESIAN_POINT('Ctrl Pts',(-0.367751076835709,0.330140554137441,
-0.615219215053683));
#65252=CARTESIAN_POINT('Ctrl Pts',(-0.351397634154326,0.348357026123933,
-0.616006351516677));
#65253=CARTESIAN_POINT('Ctrl Pts',(-0.333669560200077,0.36537541101292,
-0.61679348797967));
#65254=CARTESIAN_POINT('Ctrl Pts',(-0.314771364395952,0.380989013170079,
-0.617580624442664));
#65255=CARTESIAN_POINT('Ctrl Pts',(-0.295864722284549,0.396609593627331,
-0.618368112706248));
#65256=CARTESIAN_POINT('Ctrl Pts',(-0.275787434261984,0.41082367793531,
-0.619155600969831));
#65257=CARTESIAN_POINT('Ctrl Pts',(-0.254778215899747,0.423463930816949,
-0.619943089233415));
#65258=CARTESIAN_POINT('Ctrl Pts',(-0.233765382240666,0.436106358851683,
-0.620730713009124));
#65259=CARTESIAN_POINT('Ctrl Pts',(-0.211820907179082,0.447174080969499,
-0.621518336784833));
#65260=CARTESIAN_POINT('Ctrl Pts',(-0.18920904419388,0.456545263468189,
-0.622305960560542));
#65261=CARTESIAN_POINT('Ctrl Pts',(-0.166547864377789,0.465936884664161,
-0.623095302156166));
#65262=CARTESIAN_POINT('Ctrl Pts',(-0.143217046425942,0.473624346369207,
-0.623884643751791));
#65263=CARTESIAN_POINT('Ctrl Pts',(-0.119498511422257,0.479534926535977,
-0.624673985347415));
#65264=CARTESIAN_POINT('Ctrl Pts',(-0.103117558636715,0.483617005578042,
-0.62521913568691));
#65265=CARTESIAN_POINT('Ctrl Pts',(-0.0865520094296256,0.486852600934384,
-0.625764286026405));
#65266=CARTESIAN_POINT('Ctrl Pts',(-0.0698965878358467,0.48923216064452,
-0.6263094363659));
#65267=CARTESIAN_POINT('Ctrl Pts',(-0.0457862380653544,0.492676805776325,
-0.627098594736267));
#65268=CARTESIAN_POINT('Ctrl Pts',(-0.0213536736036407,0.494344433489065,
-0.627887753106634));
#65269=CARTESIAN_POINT('Ctrl Pts',(0.00311537835969982,0.494190180414055,
-0.628676911477001));
#65270=CARTESIAN_POINT('Ctrl Pts',(0.0275418356991093,0.494036195855852,
-0.629464696116009));
#65271=CARTESIAN_POINT('Ctrl Pts',(0.0520039677474236,0.492066577542858,
-0.630252480755017));
#65272=CARTESIAN_POINT('Ctrl Pts',(0.0762116868837025,0.488288253782886,
-0.631040265394026));
#65273=CARTESIAN_POINT('Ctrl Pts',(0.100393757474185,0.484513933229886,
-0.631827215359999));
#65274=CARTESIAN_POINT('Ctrl Pts',(0.124321263762377,0.478934791172687,
-0.632614165325973));
#65275=CARTESIAN_POINT('Ctrl Pts',(0.147709532962699,0.471609514187258,
-0.633401115291947));
#65276=CARTESIAN_POINT('Ctrl Pts',(0.171108332587079,0.464280939041014,
-0.634188419577292));
#65277=CARTESIAN_POINT('Ctrl Pts',(0.193966740932735,0.455204844567866,
-0.634975723862637));
#65278=CARTESIAN_POINT('Ctrl Pts',(0.216014424973876,0.444490054110557,
-0.635763028147983));
#65279=CARTESIAN_POINT('Ctrl Pts',(0.238065935515635,0.43377340404059,-0.636550469074453));
#65280=CARTESIAN_POINT('Ctrl Pts',(0.259305828612904,0.421417819004453,
-0.637337910000922));
#65281=CARTESIAN_POINT('Ctrl Pts',(0.279487991968314,0.407578338906179,
-0.638125350927392));
#65282=CARTESIAN_POINT('Ctrl Pts',(0.299714305925911,0.393708583491549,
-0.638914514463598));
#65283=CARTESIAN_POINT('Ctrl Pts',(0.318877717704755,0.37834887532309,-0.639703677999804));
#65284=CARTESIAN_POINT('Ctrl Pts',(0.336763654525841,0.361695840438344,
-0.640492841536009));
#65285=CARTESIAN_POINT('Ctrl Pts',(0.349144207197986,0.35016869609002,-0.641039096441451));
#65286=CARTESIAN_POINT('Ctrl Pts',(0.360913380964598,0.338022736759383,
-0.641585351346892));
#65287=CARTESIAN_POINT('Ctrl Pts',(0.372011165225625,0.325332649679482,
-0.642131606252334));
#65288=CARTESIAN_POINT('Ctrl Pts',(0.388048694568756,0.306994066127674,
-0.642921005187183));
#65289=CARTESIAN_POINT('Ctrl Pts',(0.402771380822854,0.287415961485453,
-0.643710404122033));
#65290=CARTESIAN_POINT('Ctrl Pts',(0.415985784972064,0.266813542949334,
-0.644499803056882));
#65291=CARTESIAN_POINT('Ctrl Pts',(0.429177169125266,0.246247014612053,
-0.64528782682868));
#65292=CARTESIAN_POINT('Ctrl Pts',(0.440865072248985,0.224660263493484,
-0.646075850600479));
#65293=CARTESIAN_POINT('Ctrl Pts',(0.450897100945209,0.202300381510282,
-0.646863874372277));
#65294=CARTESIAN_POINT('Ctrl Pts',(0.460918476799838,0.179964243107574,
-0.647651061354961));
#65295=CARTESIAN_POINT('Ctrl Pts',(0.469287161597707,0.15685722216568,-0.648438248337644));
#65296=CARTESIAN_POINT('Ctrl Pts',(0.475897104792094,0.133250086868651,
-0.649225435320328));
#65297=CARTESIAN_POINT('Ctrl Pts',(0.482509973753802,0.109632502316165,
-0.650012970736558));
#65298=CARTESIAN_POINT('Ctrl Pts',(0.487362337295631,0.0855150232019731,
-0.650800506152787));
#65299=CARTESIAN_POINT('Ctrl Pts',(0.490397992575441,0.0611837305006642,
-0.651588041569017));
#65300=CARTESIAN_POINT('Ctrl Pts',(0.493434163220453,0.0368483070597128,
-0.652375710685655));
#65301=CARTESIAN_POINT('Ctrl Pts',(0.494652951573273,0.0122996895892027,
-0.653163379802293));
#65302=CARTESIAN_POINT('Ctrl Pts',(0.494050102097953,-0.0121711386896278,
-0.653951048918932));
#65303=CARTESIAN_POINT('Ctrl Pts',(0.493445940628029,-0.0366952233715363,
-0.654740432257233));
#65304=CARTESIAN_POINT('Ctrl Pts',(0.491012279604423,-0.0611404871652856,
-0.655529815595535));
#65305=CARTESIAN_POINT('Ctrl Pts',(0.486796920891336,-0.0852197031836814,
-0.656319198933837));
#65306=CARTESIAN_POINT('Ctrl Pts',(0.48388733779075,-0.101839992172365,
-0.656864058002148));
#65307=CARTESIAN_POINT('Ctrl Pts',(0.480130017358319,-0.118286007874321,
-0.657408917070458));
#65308=CARTESIAN_POINT('Ctrl Pts',(0.475554570486741,-0.13446743281989,
-0.657953776138768));
#65309=CARTESIAN_POINT('Ctrl Pts',(0.468924039663125,-0.157916822547936,
-0.658743361276211));
#65310=CARTESIAN_POINT('Ctrl Pts',(0.460536659523053,-0.180939245255025,
-0.659532946413655));
#65311=CARTESIAN_POINT('Ctrl Pts',(0.450467533895641,-0.203255112865531,
-0.660322531551098));
#65312=CARTESIAN_POINT('Ctrl Pts',(0.440415891764968,-0.225532232384789,
-0.661110745694704));
#65313=CARTESIAN_POINT('Ctrl Pts',(0.428688535079481,-0.247104585693906,
-0.66189895983831));
#65314=CARTESIAN_POINT('Ctrl Pts',(0.415409667071266,-0.267709634686053,
-0.662687173981916));
#65315=CARTESIAN_POINT('Ctrl Pts',(0.402144836964618,-0.288292900823717,
-0.66347455485626));
#65316=CARTESIAN_POINT('Ctrl Pts',(0.387332102670531,-0.307910298342129,
-0.664261935730603));
#65317=CARTESIAN_POINT('Ctrl Pts',(0.371140771576259,-0.326325248293446,
-0.665049316604946));
#65318=CARTESIAN_POINT('Ctrl Pts',(0.354942213600477,-0.34474841762219,
-0.665837048920949));
#65319=CARTESIAN_POINT('Ctrl Pts',(0.337364270730379,-0.361967531821357,
-0.666624781236952));
#65320=CARTESIAN_POINT('Ctrl Pts',(0.318616254647902,-0.377779462483263,
-0.667412513552956));
#65321=CARTESIAN_POINT('Ctrl Pts',(0.299865009486434,-0.393594116525226,
-0.668200381544641));
#65322=CARTESIAN_POINT('Ctrl Pts',(0.279943836914778,-0.408000677387485,
-0.668988249536327));
#65323=CARTESIAN_POINT('Ctrl Pts',(0.259094471956554,-0.420836897861338,
-0.669776117528012));
#65324=CARTESIAN_POINT('Ctrl Pts',(0.238199748108907,-0.433701044207574,
-0.670565699567929));
#65325=CARTESIAN_POINT('Ctrl Pts',(0.216373410584568,-0.444987696202054,
-0.671355281607845));
#65326=CARTESIAN_POINT('Ctrl Pts',(0.193882421600628,-0.45458029719102,
-0.672144863647761));
#65327=CARTESIAN_POINT('Ctrl Pts',(0.178395470307243,-0.461185615632067,
-0.672688557773575));
#65328=CARTESIAN_POINT('Ctrl Pts',(0.162593874688042,-0.466988692461513,
-0.673232251899389));
#65329=CARTESIAN_POINT('Ctrl Pts',(0.146568870670712,-0.471965259473949,
-0.673775946025203));
#65330=CARTESIAN_POINT('Ctrl Pts',(0.123334115400948,-0.479180815644323,
-0.674564251596997));
#65331=CARTESIAN_POINT('Ctrl Pts',(0.099499908992319,-0.484696776467554,
-0.675352557168792));
#65332=CARTESIAN_POINT('Ctrl Pts',(0.0753406616753785,-0.488423407197399,
-0.676140862740586));
#65333=CARTESIAN_POINT('Ctrl Pts',(0.0512235350854168,-0.49214354068859,
-0.676927793931659));
#65334=CARTESIAN_POINT('Ctrl Pts',(0.0267831641950888,-0.494080378759341,
-0.677714725122732));
#65335=CARTESIAN_POINT('Ctrl Pts',(0.00230653230264751,-0.494194617442093,
-0.678501656313805));
#65336=CARTESIAN_POINT('Ctrl Pts',(-0.0221441954689344,-0.494308735223708,
-0.679287754679481));
#65337=CARTESIAN_POINT('Ctrl Pts',(-0.0466304160046617,-0.49260405195665,
-0.680073853045156));
#65338=CARTESIAN_POINT('Ctrl Pts',(-0.0708622501506096,-0.4890932237351,
-0.680859951410832));
#65339=CARTESIAN_POINT('Ctrl Pts',(-0.0951053905960956,-0.485580757400839,
-0.681646416561107));
#65340=CARTESIAN_POINT('Ctrl Pts',(-0.119093215612431,-0.480260540258949,
-0.682432881711382));
#65341=CARTESIAN_POINT('Ctrl Pts',(-0.142542033323854,-0.4731970083759,
-0.683219346861658));
#65342=CARTESIAN_POINT('Ctrl Pts',(-0.165995093287149,-0.466132198591264,
-0.684005954295578));
#65343=CARTESIAN_POINT('Ctrl Pts',(-0.188908293129803,-0.457323672770647,
-0.684792561729498));
#65344=CARTESIAN_POINT('Ctrl Pts',(-0.211014537655382,-0.446885337528639,
-0.685579169163419));
#65345=CARTESIAN_POINT('Ctrl Pts',(-0.233169828021835,-0.436423843358452,
-0.686367521797569));
#65346=CARTESIAN_POINT('Ctrl Pts',(-0.254513974367191,-0.424325651739701,
-0.68715587443172));
#65347=CARTESIAN_POINT('Ctrl Pts',(-0.27480444503967,-0.410750723659057,
-0.68794422706587));
#65348=CARTESIAN_POINT('Ctrl Pts',(-0.288993604250444,-0.401257754327777,
-0.688495523347792));
#65349=CARTESIAN_POINT('Ctrl Pts',(-0.302668046169075,-0.391043594242111,
-0.689046819629715));
#65350=CARTESIAN_POINT('Ctrl Pts',(-0.315754697256002,-0.380174448327042,
-0.689598115911637));
#65351=CARTESIAN_POINT('Ctrl Pts',(-0.334269196694398,-0.364797191410533,
-0.690378069058874));
#65352=CARTESIAN_POINT('Ctrl Pts',(-0.351715095282875,-0.348016403869801,
-0.691158022206111));
#65353=CARTESIAN_POINT('Ctrl Pts',(-0.367870045722719,-0.330007983933668,
-0.691937975353348));
#65354=CARTESIAN_POINT('Ctrl Pts',(-0.383996609505757,-0.312031207476621,
-0.692716558006606));
#65355=CARTESIAN_POINT('Ctrl Pts',(-0.398836213732678,-0.292831564643769,
-0.693495140659864));
#65356=CARTESIAN_POINT('Ctrl Pts',(-0.41220165015197,-0.272623255816508,
-0.694273723313121));
#65357=CARTESIAN_POINT('Ctrl Pts',(-0.425561954706966,-0.252422706279352,
-0.695052007017628));
#65358=CARTESIAN_POINT('Ctrl Pts',(-0.437448782125241,-0.2312148239441,
-0.695830290722135));
#65359=CARTESIAN_POINT('Ctrl Pts',(-0.44771653219203,-0.209245183461753,
-0.696608574426642));
#65360=CARTESIAN_POINT('Ctrl Pts',(-0.457980502294138,-0.187283630872522,
-0.697386571614152));
#65361=CARTESIAN_POINT('Ctrl Pts',(-0.466626279375811,-0.164561523677347,
-0.698164568801661));
#65362=CARTESIAN_POINT('Ctrl Pts',(-0.473555426179341,-0.141346730899949,
-0.698942565989171));
#65363=CARTESIAN_POINT('Ctrl Pts',(-0.480497095026677,-0.118089985388637,
-0.699721969138358));
#65364=CARTESIAN_POINT('Ctrl Pts',(-0.485715746205358,-0.0943394653797793,
-0.700501372287546));
#65365=CARTESIAN_POINT('Ctrl Pts',(-0.489163270445009,-0.0703770903600209,
-0.701280775436733));
#65366=CARTESIAN_POINT('Ctrl Pts',(-0.492535554042889,-0.0469376832295417,
-0.702043168468205));
#65367=CARTESIAN_POINT('Ctrl Pts',(-0.494213349678348,-0.0232962356163744,
-0.702805561499676));
#65368=CARTESIAN_POINT('Ctrl Pts',(-0.494199919830197,0.000281495695726313,
-0.703567954531148));
#65369=CARTESIAN_POINT('Origin',(0.,0.,-0.920658989190502));
#65370=CARTESIAN_POINT('',(-0.437199811556163,-0.000405925184154985,-0.170658989186969));
#65371=CARTESIAN_POINT('Ctrl Pts',(-0.00922985932074797,0.43710256198851,
-0.195314102181071));
#65372=CARTESIAN_POINT('Ctrl Pts',(-0.0315222221120698,0.436631836373096,
-0.194501442586441));
#65373=CARTESIAN_POINT('Ctrl Pts',(-0.0538211649838741,0.434450494946843,
-0.193688782991811));
#65374=CARTESIAN_POINT('Ctrl Pts',(-0.0758452307453741,0.430570947665052,
-0.192876123397182));
#65375=CARTESIAN_POINT('Ctrl Pts',(-0.0978465938203715,0.426695399469836,
-0.192064301502376));
#65376=CARTESIAN_POINT('Ctrl Pts',(-0.119572937063035,0.421125217966566,
-0.19125247960757));
#65377=CARTESIAN_POINT('Ctrl Pts',(-0.140749458739654,0.413924425305507,
-0.190440657712765));
#65378=CARTESIAN_POINT('Ctrl Pts',(-0.161936626482776,0.406720012592076,
-0.189628427690977));
#65379=CARTESIAN_POINT('Ctrl Pts',(-0.182572738074923,0.397883565095202,
-0.188816197669189));
#65380=CARTESIAN_POINT('Ctrl Pts',(-0.202398840300782,0.387528772409093,
-0.188003967647401));
#65381=CARTESIAN_POINT('Ctrl Pts',(-0.222230291718209,0.377171185942891,
-0.187191518481481));
#65382=CARTESIAN_POINT('Ctrl Pts',(-0.24125068040462,0.365294798452339,
-0.18637906931556));
#65383=CARTESIAN_POINT('Ctrl Pts',(-0.259226882313261,0.352058608027338,
-0.185566620149639));
#65384=CARTESIAN_POINT('Ctrl Pts',(-0.277241404192072,0.338794201941163,
-0.184752439081286));
#65385=CARTESIAN_POINT('Ctrl Pts',(-0.294206749929414,0.324164669578954,
-0.183938258012934));
#65386=CARTESIAN_POINT('Ctrl Pts',(-0.309923124603311,0.308369091894957,
-0.183124076944581));
#65387=CARTESIAN_POINT('Ctrl Pts',(-0.317001146030817,0.301255400625376,
-0.18275740262132));
#65388=CARTESIAN_POINT('Ctrl Pts',(-0.32382636374821,0.293905688877171,
-0.182390728298059));
#65389=CARTESIAN_POINT('Ctrl Pts',(-0.330383231586033,0.286340287571919,
-0.182024053974797));
#65390=CARTESIAN_POINT('Ctrl Pts',(-0.344802295372176,0.269703380029126,
-0.181217708538743));
#65391=CARTESIAN_POINT('Ctrl Pts',(-0.358007064617044,0.251921858419598,
-0.180411363102688));
#65392=CARTESIAN_POINT('Ctrl Pts',(-0.369812380149333,0.233200865110499,
-0.179605017666633));
#65393=CARTESIAN_POINT('Ctrl Pts',(-0.381596643628483,0.214513256368282,
-0.178800110161392));
#65394=CARTESIAN_POINT('Ctrl Pts',(-0.39198596824022,0.194890077933115,
-0.17799520265615));
#65395=CARTESIAN_POINT('Ctrl Pts',(-0.400836298367205,0.174568330207047,
-0.177190295150909));
#65396=CARTESIAN_POINT('Ctrl Pts',(-0.409677025326455,0.154268632862072,
-0.1763862610212));
#65397=CARTESIAN_POINT('Ctrl Pts',(-0.4169817556723,0.133272525650334,-0.175582226891491));
#65398=CARTESIAN_POINT('Ctrl Pts',(-0.422653074331143,0.111840148240392,
-0.174778192761782));
#65399=CARTESIAN_POINT('Ctrl Pts',(-0.428326882958909,0.0903983610340917,
-0.173973805624225));
#65400=CARTESIAN_POINT('Ctrl Pts',(-0.432365646160191,0.0685206233884101,
-0.173169418486668));
#65401=CARTESIAN_POINT('Ctrl Pts',(-0.434722135461347,0.0464812321257325,
-0.172365031349111));
#65402=CARTESIAN_POINT('Ctrl Pts',(-0.436388111915708,0.030899957517756,
-0.171796350629574));
#65403=CARTESIAN_POINT('Ctrl Pts',(-0.437214336588321,0.0152381961726338,
-0.171227669910038));
#65404=CARTESIAN_POINT('Ctrl Pts',(-0.437199811556254,-0.000405925086964313,
-0.170658989190502));
#65405=CARTESIAN_POINT('',(0.43681045027439,0.0184518435687243,-0.120000432818402));
#65406=CARTESIAN_POINT('Ctrl Pts',(-0.437199811556163,-0.000405925184156353,
-0.170658989186969));
#65407=CARTESIAN_POINT('Ctrl Pts',(-0.437174206827099,-0.0279833782682871,
-0.169656518955322));
#65408=CARTESIAN_POINT('Ctrl Pts',(-0.434535377857394,-0.0554441171566531,
-0.168654048723676));
#65409=CARTESIAN_POINT('Ctrl Pts',(-0.429372126588209,-0.0823615013772751,
-0.16765157849203));
#65410=CARTESIAN_POINT('Ctrl Pts',(-0.426883229251288,-0.0953367765306281,
-0.167168347024141));
#65411=CARTESIAN_POINT('Ctrl Pts',(-0.423808466932811,-0.108186137755551,
-0.166685115556252));
#65412=CARTESIAN_POINT('Ctrl Pts',(-0.420161672749106,-0.120863595646799,
-0.166201884088363));
#65413=CARTESIAN_POINT('Ctrl Pts',(-0.414011914527358,-0.142242181048175,
-0.165386988444969));
#65414=CARTESIAN_POINT('Ctrl Pts',(-0.406208909896096,-0.163210776284862,
-0.164572092801575));
#65415=CARTESIAN_POINT('Ctrl Pts',(-0.396827640688903,-0.183498402132766,
-0.16375719715818));
#65416=CARTESIAN_POINT('Ctrl Pts',(-0.387463194782531,-0.203749646460747,
-0.162943762855916));
#65417=CARTESIAN_POINT('Ctrl Pts',(-0.376526348646218,-0.223321681805135,
-0.162130328553652));
#65418=CARTESIAN_POINT('Ctrl Pts',(-0.364140998075861,-0.241961099188105,
-0.161316894251388));
#65419=CARTESIAN_POINT('Ctrl Pts',(-0.351768955503626,-0.260580488608998,
-0.160504333980271));
#65420=CARTESIAN_POINT('Ctrl Pts',(-0.337951868176142,-0.278268642824925,
-0.159691773709154));
#65421=CARTESIAN_POINT('Ctrl Pts',(-0.322858308296458,-0.294798834400595,
-0.158879213438037));
#65422=CARTESIAN_POINT('Ctrl Pts',(-0.307758065787926,-0.311336344669533,
-0.158066293408272));
#65423=CARTESIAN_POINT('Ctrl Pts',(-0.291380688599474,-0.32671432818191,
-0.157253373378506));
#65424=CARTESIAN_POINT('Ctrl Pts',(-0.273933983018575,-0.340740389369354,
-0.156440453348741));
#65425=CARTESIAN_POINT('Ctrl Pts',(-0.256483336968056,-0.354769618448165,
-0.155627349714875));
#65426=CARTESIAN_POINT('Ctrl Pts',(-0.237963456582662,-0.367445893883955,
-0.154814246081008));
#65427=CARTESIAN_POINT('Ctrl Pts',(-0.218613434383194,-0.378618549872012,
-0.154001142447142));
#65428=CARTESIAN_POINT('Ctrl Pts',(-0.199222816794282,-0.389814645539686,
-0.153186332962072));
#65429=CARTESIAN_POINT('Ctrl Pts',(-0.178999221425296,-0.399500507709868,
-0.152371523477002));
#65430=CARTESIAN_POINT('Ctrl Pts',(-0.158205278778461,-0.407571993354094,
-0.151556713991931));
#65431=CARTESIAN_POINT('Ctrl Pts',(-0.148192931689111,-0.411458438419815,
-0.151164380728597));
#65432=CARTESIAN_POINT('Ctrl Pts',(-0.13804861769082,-0.414971330636069,
-0.150772047465263));
#65433=CARTESIAN_POINT('Ctrl Pts',(-0.127802767782729,-0.418103208008589,
-0.150379714201928));
#65434=CARTESIAN_POINT('Ctrl Pts',(-0.106505478982892,-0.424613209373686,
-0.149564200126477));
#65435=CARTESIAN_POINT('Ctrl Pts',(-0.0846507791638919,-0.429509775307143,
-0.148748686051025));
#65436=CARTESIAN_POINT('Ctrl Pts',(-0.0625073938790264,-0.432708522807735,
-0.147933171975573));
#65437=CARTESIAN_POINT('Ctrl Pts',(-0.0404028108791555,-0.435901665080827,
-0.147119086941308));
#65438=CARTESIAN_POINT('Ctrl Pts',(-0.0180112363006184,-0.437402741450067,
-0.146305001907042));
#65439=CARTESIAN_POINT('Ctrl Pts',(0.00438680710504075,-0.437177991124237,
-0.145490916872777));
#65440=CARTESIAN_POINT('Ctrl Pts',(0.0267616142569755,-0.436953473959647,
-0.144677676389353));
#65441=CARTESIAN_POINT('Ctrl Pts',(0.0491421680956022,-0.435006665496692,
-0.143864435905929));
#65442=CARTESIAN_POINT('Ctrl Pts',(0.0712460812121622,-0.431355811264796,
-0.143051195422505));
#65443=CARTESIAN_POINT('Ctrl Pts',(0.093360723961109,-0.427703184843351,
-0.142237560177693));
#65444=CARTESIAN_POINT('Ctrl Pts',(0.115197752260316,-0.422344958720878,
-0.14142392493288));
#65445=CARTESIAN_POINT('Ctrl Pts',(0.136482264438377,-0.415350973868815,
-0.140610289688068));
#65446=CARTESIAN_POINT('Ctrl Pts',(0.157772123242929,-0.408355232141876,
-0.139796450059725));
#65447=CARTESIAN_POINT('Ctrl Pts',(0.178508523103308,-0.399723165427198,
-0.138982610431382));
#65448=CARTESIAN_POINT('Ctrl Pts',(0.198434570732757,-0.389573563191994,
-0.138168770803039));
#65449=CARTESIAN_POINT('Ctrl Pts',(0.218402865165291,-0.379402441975454,
-0.137353205688379));
#65450=CARTESIAN_POINT('Ctrl Pts',(0.23755676455108,-0.367707726858595,
-0.13653764057372));
#65451=CARTESIAN_POINT('Ctrl Pts',(0.255665599555166,-0.354653268988314,
-0.13572207545906));
#65452=CARTESIAN_POINT('Ctrl Pts',(0.264284695671018,-0.348439858401775,
-0.135333898411205));
#65453=CARTESIAN_POINT('Ctrl Pts',(0.272667507689819,-0.341919023909054,
-0.13494572136335));
#65454=CARTESIAN_POINT('Ctrl Pts',(0.280791942218824,-0.335111511567389,
-0.134557544315494));
#65455=CARTESIAN_POINT('Ctrl Pts',(0.297492947322032,-0.321117639384359,
-0.133759587628905));
#65456=CARTESIAN_POINT('Ctrl Pts',(0.313202957866233,-0.305823455159743,
-0.132961630942315));
#65457=CARTESIAN_POINT('Ctrl Pts',(0.327708795017198,-0.289397279994779,
-0.132163674255725));
#65458=CARTESIAN_POINT('Ctrl Pts',(0.342188440452228,-0.273000763904939,
-0.131367158358429));
#65459=CARTESIAN_POINT('Ctrl Pts',(0.35546768938981,-0.255476819080919,
-0.130570642461133));
#65460=CARTESIAN_POINT('Ctrl Pts',(0.367368586639539,-0.237031984235182,
-0.129774126563837));
#65461=CARTESIAN_POINT('Ctrl Pts',(0.379537806510062,-0.218171284406993,
-0.128959652085051));
#65462=CARTESIAN_POINT('Ctrl Pts',(0.390265160915261,-0.198348215478529,
-0.128145177606265));
#65463=CARTESIAN_POINT('Ctrl Pts',(0.399405653984382,-0.177817219541044,
-0.127330703127478));
#65464=CARTESIAN_POINT('Ctrl Pts',(0.408340170441622,-0.15774887971519,
-0.126534582439055));
#65465=CARTESIAN_POINT('Ctrl Pts',(0.415758405797366,-0.137004945668643,
-0.125738461750631));
#65466=CARTESIAN_POINT('Ctrl Pts',(0.421573066228182,-0.115844679769807,
-0.124942341062208));
#65467=CARTESIAN_POINT('Ctrl Pts',(0.427588803694421,-0.0939526697585951,
-0.12411868968824));
#65468=CARTESIAN_POINT('Ctrl Pts',(0.43188766654941,-0.0716157931141208,
-0.123295038314273));
#65469=CARTESIAN_POINT('Ctrl Pts',(0.43443041023611,-0.0491330709612701,
-0.122471386940305));
#65470=CARTESIAN_POINT('Ctrl Pts',(0.43697315392281,-0.0266503488084183,
-0.121647735566337));
#65471=CARTESIAN_POINT('Ctrl Pts',(0.437759823048745,-0.00402265593044939,
-0.12082408419237));
#65472=CARTESIAN_POINT('Ctrl Pts',(0.43681045027439,0.0184518435687243,
-0.120000432818402));
#65473=CARTESIAN_POINT('',(0.159436307123189,-0.407092009220176,-0.12));
#65474=CARTESIAN_POINT('Origin',(0.,0.,-0.12));
#65475=CARTESIAN_POINT('',(-0.437199999925775,8.05617700352763E-6,-0.150941010806857));
#65476=CARTESIAN_POINT('Ctrl Pts',(-0.437199999925775,8.05617700357433E-6,
-0.150941010806857));
#65477=CARTESIAN_POINT('Ctrl Pts',(-0.437200411510969,-0.0223282264816288,
-0.150121936742549));
#65478=CARTESIAN_POINT('Ctrl Pts',(-0.435484786799362,-0.0447284246752743,
-0.149302862678242));
#65479=CARTESIAN_POINT('Ctrl Pts',(-0.43204974625499,-0.0669093174453197,
-0.148483788613934));
#65480=CARTESIAN_POINT('Ctrl Pts',(-0.428621461812277,-0.08904658442274,
-0.147666325519736));
#65481=CARTESIAN_POINT('Ctrl Pts',(-0.423480525826266,-0.110964704565275,
-0.146848862425539));
#65482=CARTESIAN_POINT('Ctrl Pts',(-0.41667541902183,-0.132383666601974,
-0.146031399331341));
#65483=CARTESIAN_POINT('Ctrl Pts',(-0.409593050690594,-0.154675304746105,
-0.145180630210932));
#65484=CARTESIAN_POINT('Ctrl Pts',(-0.400707930092937,-0.176425394702839,
-0.144329861090523));
#65485=CARTESIAN_POINT('Ctrl Pts',(-0.390133072634072,-0.197332272163217,
-0.143479091970115));
#65486=CARTESIAN_POINT('Ctrl Pts',(-0.379985497716015,-0.217394396514025,
-0.142662698612483));
#65487=CARTESIAN_POINT('Ctrl Pts',(-0.368282628512785,-0.236679550736123,
-0.141846305254851));
#65488=CARTESIAN_POINT('Ctrl Pts',(-0.355172417599625,-0.254943903195267,
-0.14102991189722));
#65489=CARTESIAN_POINT('Ctrl Pts',(-0.34206142917299,-0.273209338839131,
-0.140213470122607));
#65490=CARTESIAN_POINT('Ctrl Pts',(-0.327543361401381,-0.290453292232999,
-0.139397028347994));
#65491=CARTESIAN_POINT('Ctrl Pts',(-0.3118077799158,-0.306463290434564,
-0.138580586573381));
#65492=CARTESIAN_POINT('Ctrl Pts',(-0.296049869827803,-0.322496006632592,
-0.137762986277629));
#65493=CARTESIAN_POINT('Ctrl Pts',(-0.279071522280868,-0.337290801418832,
-0.136945385981878));
#65494=CARTESIAN_POINT('Ctrl Pts',(-0.261097572399393,-0.350673491566077,
-0.136127785686126));
#65495=CARTESIAN_POINT('Ctrl Pts',(-0.258858041626556,-0.35234095734882,
-0.136025913752896));
#65496=CARTESIAN_POINT('Ctrl Pts',(-0.25660309183787,-0.353986555224397,
-0.135924041819665));
#65497=CARTESIAN_POINT('Ctrl Pts',(-0.254333188587303,-0.355609995898619,
-0.135822169886434));
#65498=CARTESIAN_POINT('Ctrl Pts',(-0.236102803290399,-0.368648414602289,
-0.135004000833075));
#65499=CARTESIAN_POINT('Ctrl Pts',(-0.216831887317712,-0.380306736362932,
-0.134185831779715));
#65500=CARTESIAN_POINT('Ctrl Pts',(-0.196755198149015,-0.390424425467134,
-0.133367662726355));
#65501=CARTESIAN_POINT('Ctrl Pts',(-0.176702518611316,-0.400530014868049,
-0.132550472118042));
#65502=CARTESIAN_POINT('Ctrl Pts',(-0.15584659277195,-0.409098288862712,
-0.131733281509728));
#65503=CARTESIAN_POINT('Ctrl Pts',(-0.134447898286254,-0.416013945254734,
-0.130916090901415));
#65504=CARTESIAN_POINT('Ctrl Pts',(-0.113054594805081,-0.422927859375287,
-0.130099106169131));
#65505=CARTESIAN_POINT('Ctrl Pts',(-0.0911194600821032,-0.428189754850942,
-0.129282121436848));
#65506=CARTESIAN_POINT('Ctrl Pts',(-0.0689198346927786,-0.431733594229034,
-0.128465136704564));
#65507=CARTESIAN_POINT('Ctrl Pts',(-0.0639014865065837,-0.432534698734327,
-0.128280452784115));
#65508=CARTESIAN_POINT('Ctrl Pts',(-0.058869668093171,-0.433248214564207,
-0.128095768863666));
#65509=CARTESIAN_POINT('Ctrl Pts',(-0.0538276487004057,-0.433873742274623,
-0.127911084943217));
#65510=CARTESIAN_POINT('Ctrl Pts',(-0.0281379123489383,-0.437060886295561,
-0.126970096649617));
#65511=CARTESIAN_POINT('Ctrl Pts',(-0.00221150245003065,-0.437956315129622,
-0.126029108356018));
#65512=CARTESIAN_POINT('Ctrl Pts',(0.0235731099185724,-0.436564025646602,
-0.125088120062418));
#65513=CARTESIAN_POINT('Ctrl Pts',(0.0494083253767184,-0.435169003752934,
-0.124145285050543));
#65514=CARTESIAN_POINT('Ctrl Pts',(0.0751009302224881,-0.43147733488461,
-0.123202450038669));
#65515=CARTESIAN_POINT('Ctrl Pts',(0.100276446654969,-0.425544914487593,
-0.122259615026794));
#65516=CARTESIAN_POINT('Ctrl Pts',(0.120388475631987,-0.420805666685124,
-0.121506410017863));
#65517=CARTESIAN_POINT('Ctrl Pts',(0.140170569315508,-0.414637374937239,
-0.120753205008931));
#65518=CARTESIAN_POINT('Ctrl Pts',(0.159436307123189,-0.407092009220176,
-0.12));
#65519=CARTESIAN_POINT('Ctrl Pts',(-0.00922985932074711,0.43710256198851,
-0.175603427251549));
#65520=CARTESIAN_POINT('Ctrl Pts',(-0.0316398144068825,0.436629353293763,
-0.174789798874397));
#65521=CARTESIAN_POINT('Ctrl Pts',(-0.05401454645459,0.434428359633278,
-0.173976170497244));
#65522=CARTESIAN_POINT('Ctrl Pts',(-0.0760722143289932,0.430530902731829,
-0.173162542120091));
#65523=CARTESIAN_POINT('Ctrl Pts',(-0.098137492626593,0.426632101114493,
-0.172348633021681));
#65524=CARTESIAN_POINT('Ctrl Pts',(-0.119884794677085,0.421035830047629,
-0.17153472392327));
#65525=CARTESIAN_POINT('Ctrl Pts',(-0.141043448082782,0.413824341663126,
-0.170720814824859));
#65526=CARTESIAN_POINT('Ctrl Pts',(-0.162246071690038,0.406597866946945,
-0.169905214326414));
#65527=CARTESIAN_POINT('Ctrl Pts',(-0.182856949803843,0.397749755060883,
-0.169089613827968));
#65528=CARTESIAN_POINT('Ctrl Pts',(-0.202625341126216,0.387410391101587,
-0.168274013329523));
#65529=CARTESIAN_POINT('Ctrl Pts',(-0.209149388368132,0.383998150933847,
-0.16800484543945));
#65530=CARTESIAN_POINT('Ctrl Pts',(-0.215581891325189,0.380423853186842,
-0.167735677549376));
#65531=CARTESIAN_POINT('Ctrl Pts',(-0.221914529893185,0.376693219241184,
-0.167466509659303));
#65532=CARTESIAN_POINT('Ctrl Pts',(-0.240883208540412,0.365518541307841,
-0.166660248705969));
#65533=CARTESIAN_POINT('Ctrl Pts',(-0.259065747553711,0.352871957896418,
-0.165853987752634));
#65534=CARTESIAN_POINT('Ctrl Pts',(-0.276221285039249,0.338888833824996,
-0.1650477267993));
#65535=CARTESIAN_POINT('Ctrl Pts',(-0.293345921637636,0.3249308964281,-0.164242918098846));
#65536=CARTESIAN_POINT('Ctrl Pts',(-0.309446629671869,0.309641603187625,
-0.163438109398393));
#65537=CARTESIAN_POINT('Ctrl Pts',(-0.32431133029229,0.293199592503205,
-0.162633300697939));
#65538=CARTESIAN_POINT('Ctrl Pts',(-0.339160503636931,0.276774756711222,
-0.161829332679512));
#65539=CARTESIAN_POINT('Ctrl Pts',(-0.35277572259787,0.259200111547914,
-0.161025364661085));
#65540=CARTESIAN_POINT('Ctrl Pts',(-0.364981679555856,0.240691116555195,
-0.160221396642658));
#65541=CARTESIAN_POINT('Ctrl Pts',(-0.377195275526492,0.22217053783763,
-0.159416925466479));
#65542=CARTESIAN_POINT('Ctrl Pts',(-0.387997430440119,0.202715040834984,
-0.1586124542903));
#65543=CARTESIAN_POINT('Ctrl Pts',(-0.397255788478525,0.182569653886688,
-0.157807983114121));
#65544=CARTESIAN_POINT('Ctrl Pts',(-0.406517033128674,0.162417985920715,
-0.157003261116368));
#65545=CARTESIAN_POINT('Ctrl Pts',(-0.414233252420819,0.141576678642802,
-0.156198539118614));
#65546=CARTESIAN_POINT('Ctrl Pts',(-0.420320381114166,0.120310503365427,
-0.15539381712086));
#65547=CARTESIAN_POINT('Ctrl Pts',(-0.426422168501408,0.0989931160356346,
-0.154587157235141));
#65548=CARTESIAN_POINT('Ctrl Pts',(-0.430886886337158,0.0772495345773366,
-0.153780497349423));
#65549=CARTESIAN_POINT('Ctrl Pts',(-0.433681462773864,0.0553554771122185,
-0.152973837463704));
#65550=CARTESIAN_POINT('Ctrl Pts',(-0.435216757877885,0.0433272359834948,
-0.152530671566759));
#65551=CARTESIAN_POINT('Ctrl Pts',(-0.43624888740812,0.0312536725423513,
-0.152087505669814));
#65552=CARTESIAN_POINT('Ctrl Pts',(-0.436779063571225,0.0191804490521891,
-0.151644339772869));
#65553=CARTESIAN_POINT('Ctrl Pts',(-0.437059536605343,0.0127934896611146,
-0.151409896785079));
#65554=CARTESIAN_POINT('Ctrl Pts',(-0.437199882116983,0.00640135457303683,
-0.151175453797288));
#65555=CARTESIAN_POINT('Ctrl Pts',(-0.437199999925774,8.05624901829692E-6,
-0.150941010809498));
#65556=CARTESIAN_POINT('Origin',(4.51336705371395E-17,0.,-0.12));
#65557=CARTESIAN_POINT('',(0.436962529762211,0.0516115063121503,-0.12));
#65558=CARTESIAN_POINT('Ctrl Pts',(0.43738504590192,0.0184879624732976,
-0.12));
#65559=CARTESIAN_POINT('Ctrl Pts',(0.437692020904658,0.0295490537246066,
-0.12));
#65560=CARTESIAN_POINT('Ctrl Pts',(0.437554515524168,0.0405981455361159,
-0.12));
#65561=CARTESIAN_POINT('Ctrl Pts',(0.436962529762211,0.0516115063121503,
-0.12));
#65562=CARTESIAN_POINT('',(0.118083290997715,-0.423832528941423,-0.12));
#65563=CARTESIAN_POINT('Origin',(0.,0.,-0.12));
#65564=CARTESIAN_POINT('Ctrl Pts',(0.11807574112921,-0.423808297522097,
-0.12));
#65565=CARTESIAN_POINT('Ctrl Pts',(0.125113297528677,-0.421379174521328,
-0.12));
#65566=CARTESIAN_POINT('Ctrl Pts',(0.132087840054081,-0.418769592094058,
-0.120000000000008));
#65567=CARTESIAN_POINT('Ctrl Pts',(0.145881768282444,-0.413195704088879,
-0.120000000000008));
#65568=CARTESIAN_POINT('Ctrl Pts',(0.15269989343557,-0.410232605099891,
-0.12));
#65569=CARTESIAN_POINT('Ctrl Pts',(0.159436307123189,-0.407092009220176,
-0.12));
#65570=CARTESIAN_POINT('Ctrl Pts',(-0.191616906624657,0.39225821899835,
-0.769079186525837));
#65571=CARTESIAN_POINT('Ctrl Pts',(-0.256609926003248,0.3605093333859,-0.766442158211432));
#65572=CARTESIAN_POINT('Ctrl Pts',(-0.36955373332459,0.26409422716641,-0.761168101582621));
#65573=CARTESIAN_POINT('Ctrl Pts',(-0.480807942249448,-0.0140930329678582,
-0.750619988324998));
#65574=CARTESIAN_POINT('Ctrl Pts',(-0.332057960250246,-0.3941381812961,
-0.737434846752968));
#65575=CARTESIAN_POINT('Ctrl Pts',(0.15018603425576,-0.493306196243262,
-0.721612676866535));
#65576=CARTESIAN_POINT('Ctrl Pts',(0.494996424724238,-0.143038083793679,
-0.705790506980099));
#65577=CARTESIAN_POINT('Ctrl Pts',(0.390010833532397,0.336947617464268,
-0.689968337093666));
#65578=CARTESIAN_POINT('Ctrl Pts',(-0.0699280367938378,0.510661735563277,
-0.674146167207231));
#65579=CARTESIAN_POINT('Ctrl Pts',(-0.466149582960942,0.219803044164238,
-0.658323997320798));
#65580=CARTESIAN_POINT('Ctrl Pts',(-0.438446333712939,-0.270923223572784,
-0.642501827434362));
#65581=CARTESIAN_POINT('Ctrl Pts',(-0.0119251715759321,-0.515260161789781,
-0.626679657547929));
#65582=CARTESIAN_POINT('Ctrl Pts',(0.425426395664575,-0.290930041698329,
-0.610857487661495));
#65583=CARTESIAN_POINT('Ctrl Pts',(0.475841582620101,0.198006753256743,
-0.59503531777506));
#65584=CARTESIAN_POINT('Ctrl Pts',(0.0934527706364431,0.506851252932052,
-0.579213147888625));
#65585=CARTESIAN_POINT('Ctrl Pts',(-0.373933347002199,0.354689364040992,
-0.563390978002191));
#65586=CARTESIAN_POINT('Ctrl Pts',(-0.501211178777902,-0.120077651523246,
-0.547568808115756));
#65587=CARTESIAN_POINT('Ctrl Pts',(-0.172613939570439,-0.485629104653691,
-0.531746638229323));
#65588=CARTESIAN_POINT('Ctrl Pts',(0.312983245232899,-0.409478420630284,
-0.515924468342887));
#65589=CARTESIAN_POINT('Ctrl Pts',(0.513908037004678,0.0391114426547363,
-0.500102298456454));
#65590=CARTESIAN_POINT('Ctrl Pts',(0.247409909573403,0.452127740210172,
-0.484280128570019));
#65591=CARTESIAN_POINT('Ctrl Pts',(-0.244118787161056,0.453913163939864,
-0.468457958683585));
#65592=CARTESIAN_POINT('Ctrl Pts',(-0.513610319356525,0.0428438566086168,
-0.45263578879715));
#65593=CARTESIAN_POINT('Ctrl Pts',(-0.31594979384439,-0.407193914453912,
-0.436813618910716));
#65594=CARTESIAN_POINT('Ctrl Pts',(0.169081494863269,-0.486870199065095,
-0.420991449024282));
#65595=CARTESIAN_POINT('Ctrl Pts',(0.500325443658047,-0.123715832661201,
-0.405169279137847));
#65596=CARTESIAN_POINT('Ctrl Pts',(0.376500546994966,0.35196379580438,-0.389347109251413));
#65597=CARTESIAN_POINT('Ctrl Pts',(-0.0897687952733545,0.50751615949993,
-0.373524939364978));
#65598=CARTESIAN_POINT('Ctrl Pts',(-0.474389315494283,0.201459615718978,
-0.357702769478544));
#65599=CARTESIAN_POINT('Ctrl Pts',(-0.427531089604827,-0.287834076420048,
-0.34188059959211));
#65600=CARTESIAN_POINT('Ctrl Pts',(0.0081862010117207,-0.515328709734928,
-0.326058429705676));
#65601=CARTESIAN_POINT('Ctrl Pts',(0.43645774796877,-0.274109918055601,
-0.310236259819241));
#65602=CARTESIAN_POINT('Ctrl Pts',(0.467751075340982,0.216427395685096,
-0.294414089932807));
#65603=CARTESIAN_POINT('Ctrl Pts',(0.0736033601307095,0.510108275435923,
-0.278591920046372));
#65604=CARTESIAN_POINT('Ctrl Pts',(-0.387489830816053,0.339833599072979,
-0.262769750159938));
#65605=CARTESIAN_POINT('Ctrl Pts',(-0.49614359495678,-0.139556847917794,
-0.246947580273503));
#65606=CARTESIAN_POINT('Ctrl Pts',(-0.153531570178307,-0.491972426948004,
-0.231125410387069));
#65607=CARTESIAN_POINT('Ctrl Pts',(0.328723417402025,-0.396996540727841,
-0.215303240500635));
#65608=CARTESIAN_POINT('Ctrl Pts',(0.511991387155289,0.0592196476372865,
-0.199481070614201));
#65609=CARTESIAN_POINT('Ctrl Pts',(0.229576097471973,0.461276673347663,
-0.183658900727766));
#65610=CARTESIAN_POINT('Ctrl Pts',(-0.261642352685609,0.444353606285138,
-0.167836730841332));
#65611=CARTESIAN_POINT('Ctrl Pts',(-0.514894954705951,0.0221490527857774,
-0.152014560954898));
#65612=CARTESIAN_POINT('Ctrl Pts',(-0.335682896194775,-0.344516885087901,
-0.138829419382869));
#65613=CARTESIAN_POINT('Ctrl Pts',(-0.0554577497370425,-0.450848389249885,
-0.128277377956503));
#65614=CARTESIAN_POINT('Ctrl Pts',(0.0920701638712636,-0.432846326389371,
-0.122999393158948));
#65615=CARTESIAN_POINT('Ctrl Pts',(0.159503405388502,-0.406376930613758,
-0.120358436675798));
#65616=CARTESIAN_POINT('Ctrl Pts',(-0.200102980078069,0.409630026725342,
-0.757916851848296));
#65617=CARTESIAN_POINT('Ctrl Pts',(-0.267974323431935,0.376475088901128,
-0.755279823533891));
#65618=CARTESIAN_POINT('Ctrl Pts',(-0.385920035135933,0.275790079321805,
-0.750005766905079));
#65619=CARTESIAN_POINT('Ctrl Pts',(-0.502101321767911,-0.0147171663757771,
-0.739457653647457));
#65620=CARTESIAN_POINT('Ctrl Pts',(-0.346763699378963,-0.411593246280656,
-0.726272512075427));
#65621=CARTESIAN_POINT('Ctrl Pts',(0.156837272608476,-0.515153081729957,
-0.710450342188994));
#65622=CARTESIAN_POINT('Ctrl Pts',(0.51691816479081,-0.149372763269987,
-0.694628172302559));
#65623=CARTESIAN_POINT('Ctrl Pts',(0.407283112055635,0.351869903196366,
-0.678806002416125));
#65624=CARTESIAN_POINT('Ctrl Pts',(-0.0730249162244601,0.533277239978685,
-0.66298383252969));
#65625=CARTESIAN_POINT('Ctrl Pts',(-0.486793792654988,0.229537387604584,
-0.647161662643257));
#65626=CARTESIAN_POINT('Ctrl Pts',(-0.457863658931299,-0.282921509193673,
-0.631339492756821));
#65627=CARTESIAN_POINT('Ctrl Pts',(-0.0124532976359992,-0.538079315159844,
-0.615517322870387));
#65628=CARTESIAN_POINT('Ctrl Pts',(0.444267111268556,-0.303814362540081,
-0.599695152983953));
#65629=CARTESIAN_POINT('Ctrl Pts',(0.496915018641129,0.206775811697394,
-0.583872983097518));
#65630=CARTESIAN_POINT('Ctrl Pts',(0.097591482037307,0.529298003785622,
-0.568050813211084));
#65631=CARTESIAN_POINT('Ctrl Pts',(-0.390493607290488,0.3703973725326,-0.55222864332465));
#65632=CARTESIAN_POINT('Ctrl Pts',(-0.52340814956562,-0.125395490063117,
-0.536406473438216));
#65633=CARTESIAN_POINT('Ctrl Pts',(-0.180258435017528,-0.507135997368949,
-0.520584303551781));
#65634=CARTESIAN_POINT('Ctrl Pts',(0.326844228877396,-0.427612853631347,
-0.504762133665347));
#65635=CARTESIAN_POINT('Ctrl Pts',(0.536667309279451,0.0408435579523025,
-0.488939963778913));
#65636=CARTESIAN_POINT('Ctrl Pts',(0.258366868970805,0.472150969273484,
-0.473117793892478));
#65637=CARTESIAN_POINT('Ctrl Pts',(-0.254929993727836,0.474015463462993,
-0.457295624006044));
#65638=CARTESIAN_POINT('Ctrl Pts',(-0.536356406710014,0.0447412680667841,
-0.441473454119609));
#65639=CARTESIAN_POINT('Ctrl Pts',(-0.329942156028828,-0.425227174298811,
-0.425651284233175));
#65640=CARTESIAN_POINT('Ctrl Pts',(0.176569550120485,-0.508432055710849,
-0.409829114346741));
#65641=CARTESIAN_POINT('Ctrl Pts',(0.522483188192614,-0.129194794104669,
-0.394006944460306));
#65642=CARTESIAN_POINT('Ctrl Pts',(0.39317450000532,0.367551097972806,-0.378184774573872));
#65643=CARTESIAN_POINT('Ctrl Pts',(-0.093744355697186,0.529992356846891,
-0.362362604687438));
#65644=CARTESIAN_POINT('Ctrl Pts',(-0.495398435449882,0.210381589917405,
-0.346540434801003));
#65645=CARTESIAN_POINT('Ctrl Pts',(-0.446465015080988,-0.300581287289494,
-0.330718264914569));
#65646=CARTESIAN_POINT('Ctrl Pts',(0.00854874054079198,-0.538150898864768,
-0.314896095028135));
#65647=CARTESIAN_POINT('Ctrl Pts',(0.455787005359554,-0.286249331742543,
-0.299073925141701));
#65648=CARTESIAN_POINT('Ctrl Pts',(0.488466209789068,0.22601224291735,-0.283251755255266));
#65649=CARTESIAN_POINT('Ctrl Pts',(0.0768630073689911,0.532699268948942,
-0.267429585368832));
#65650=CARTESIAN_POINT('Ctrl Pts',(-0.404650462540456,0.354883695301281,
-0.251607415482397));
#65651=CARTESIAN_POINT('Ctrl Pts',(-0.51811613936535,-0.145737355072503,
-0.235785245595963));
#65652=CARTESIAN_POINT('Ctrl Pts',(-0.160330971154458,-0.513760244242811,
-0.219963075709529));
#65653=CARTESIAN_POINT('Ctrl Pts',(0.343281480753889,-0.414578192914544,
-0.204140905823094));
#65654=CARTESIAN_POINT('Ctrl Pts',(0.534665777403248,0.0618422882413304,
-0.18831873593666));
#65655=CARTESIAN_POINT('Ctrl Pts',(0.239743256834957,0.481705078133685,
-0.172496566050225));
#65656=CARTESIAN_POINT('Ctrl Pts',(-0.273229619501072,0.464032544895762,
-0.156674396163791));
#65657=CARTESIAN_POINT('Ctrl Pts',(-0.537697934272806,0.0231299604320526,
-0.140852226277357));
#65658=CARTESIAN_POINT('Ctrl Pts',(-0.350549171641664,-0.359774388427747,
-0.127667084705328));
#65659=CARTESIAN_POINT('Ctrl Pts',(-0.0579137884348772,-0.470814960127794,
-0.117115043278961));
#65660=CARTESIAN_POINT('Ctrl Pts',(0.0961476442316455,-0.452015645968122,
-0.111837058481407));
#65661=CARTESIAN_POINT('Ctrl Pts',(0.166567279020736,-0.424374008970292,
-0.109196101998257));
#65662=CARTESIAN_POINT('Ctrl Pts',(-0.208589053531481,0.427001834452336,
-0.746754517170756));
#65663=CARTESIAN_POINT('Ctrl Pts',(-0.279338720860621,0.392440844416355,
-0.74411748885635));
#65664=CARTESIAN_POINT('Ctrl Pts',(-0.402286336947276,0.287485931477201,
-0.738843432227539));
#65665=CARTESIAN_POINT('Ctrl Pts',(-0.523394701286374,-0.0153412997836962,
-0.728295318969915));
#65666=CARTESIAN_POINT('Ctrl Pts',(-0.361469438507679,-0.429048311265211,
-0.715110177397887));
#65667=CARTESIAN_POINT('Ctrl Pts',(0.163488510961194,-0.536999967216652,
-0.699288007511452));
#65668=CARTESIAN_POINT('Ctrl Pts',(0.538839904857383,-0.155707442746293,
-0.683465837625019));
#65669=CARTESIAN_POINT('Ctrl Pts',(0.424555390578873,0.366792188928465,
-0.667643667738583));
#65670=CARTESIAN_POINT('Ctrl Pts',(-0.076121795655082,0.555892744394093,
-0.65182149785215));
#65671=CARTESIAN_POINT('Ctrl Pts',(-0.507438002349034,0.239271731044931,
-0.635999327965715));
#65672=CARTESIAN_POINT('Ctrl Pts',(-0.47728098414966,-0.294919794814562,
-0.620177158079281));
#65673=CARTESIAN_POINT('Ctrl Pts',(-0.0129814236960666,-0.560898468529907,
-0.604354988192846));
#65674=CARTESIAN_POINT('Ctrl Pts',(0.463107826872538,-0.316698683381835,
-0.588532818306413));
#65675=CARTESIAN_POINT('Ctrl Pts',(0.517988454662157,0.215544870138044,
-0.572710648419977));
#65676=CARTESIAN_POINT('Ctrl Pts',(0.101730193438172,0.551744754639191,
-0.556888478533544));
#65677=CARTESIAN_POINT('Ctrl Pts',(-0.407053867578776,0.386105381024208,
-0.541066308647109));
#65678=CARTESIAN_POINT('Ctrl Pts',(-0.545605120353339,-0.130713328602987,
-0.525244138760675));
#65679=CARTESIAN_POINT('Ctrl Pts',(-0.187902930464619,-0.528642890084206,
-0.50942196887424));
#65680=CARTESIAN_POINT('Ctrl Pts',(0.340705212521894,-0.445747286632409,
-0.493599798987806));
#65681=CARTESIAN_POINT('Ctrl Pts',(0.559426581554225,0.042575673249869,
-0.477777629101371));
#65682=CARTESIAN_POINT('Ctrl Pts',(0.269323828368205,0.492174198336795,
-0.461955459214937));
#65683=CARTESIAN_POINT('Ctrl Pts',(-0.265741200294616,0.494117762986121,
-0.446133289328503));
#65684=CARTESIAN_POINT('Ctrl Pts',(-0.559102494063503,0.0466386795249515,
-0.430311119442069));
#65685=CARTESIAN_POINT('Ctrl Pts',(-0.343934518213266,-0.44326043414371,
-0.414488949555634));
#65686=CARTESIAN_POINT('Ctrl Pts',(0.184057605377702,-0.529993912356603,
-0.3986667796692));
#65687=CARTESIAN_POINT('Ctrl Pts',(0.544640932727182,-0.134673755548136,
-0.382844609782765));
#65688=CARTESIAN_POINT('Ctrl Pts',(0.409848453015675,0.383138400141232,
-0.367022439896332));
#65689=CARTESIAN_POINT('Ctrl Pts',(-0.097719916121017,0.552468554193852,
-0.351200270009897));
#65690=CARTESIAN_POINT('Ctrl Pts',(-0.516407555405482,0.219303564115831,
-0.335378100123463));
#65691=CARTESIAN_POINT('Ctrl Pts',(-0.46539894055715,-0.31332849815894,
-0.319555930237028));
#65692=CARTESIAN_POINT('Ctrl Pts',(0.00891128006986319,-0.560973087994608,
-0.303733760350594));
#65693=CARTESIAN_POINT('Ctrl Pts',(0.475116262750338,-0.298388745429484,
-0.287911590464159));
#65694=CARTESIAN_POINT('Ctrl Pts',(0.509181344237154,0.235597090149604,
-0.272089420577725));
#65695=CARTESIAN_POINT('Ctrl Pts',(0.0801226546072732,0.555290262461962,
-0.25626725069129));
#65696=CARTESIAN_POINT('Ctrl Pts',(-0.421811094264861,0.369933791529583,
-0.240445080804857));
#65697=CARTESIAN_POINT('Ctrl Pts',(-0.54008868377392,-0.151917862227212,
-0.224622910918422));
#65698=CARTESIAN_POINT('Ctrl Pts',(-0.16713037213061,-0.535548061537618,
-0.208800741031988));
#65699=CARTESIAN_POINT('Ctrl Pts',(0.357839544105755,-0.43215984510125,
-0.192978571145553));
#65700=CARTESIAN_POINT('Ctrl Pts',(0.557340167651207,0.0644649288453748,
-0.177156401259119));
#65701=CARTESIAN_POINT('Ctrl Pts',(0.249910416197941,0.502133482919706,
-0.161334231372684));
#65702=CARTESIAN_POINT('Ctrl Pts',(-0.284816886316535,0.483711483506385,
-0.14551206148625));
#65703=CARTESIAN_POINT('Ctrl Pts',(-0.560500913839662,0.0241108680783272,
-0.129689891599816));
#65704=CARTESIAN_POINT('Ctrl Pts',(-0.365415447088553,-0.375031891767592,
-0.116504750027787));
#65705=CARTESIAN_POINT('Ctrl Pts',(-0.0603698271327118,-0.490781531005703,
-0.10595270860142));
#65706=CARTESIAN_POINT('Ctrl Pts',(0.100225124592028,-0.471184965546873,
-0.100674723803866));
#65707=CARTESIAN_POINT('Ctrl Pts',(0.17363115265297,-0.442371087326825,
-0.098033767320716));
#65708=CARTESIAN_POINT('Ctrl Pts',(-0.217075126984893,0.444373642179328,
-0.735592182493215));
#65709=CARTESIAN_POINT('Ctrl Pts',(-0.290703118289308,0.408406599931581,
-0.732955154178809));
#65710=CARTESIAN_POINT('Ctrl Pts',(-0.418652638758619,0.299181783632597,
-0.727681097549997));
#65711=CARTESIAN_POINT('Ctrl Pts',(-0.544688080804837,-0.0159654331916153,
-0.717132984292375));
#65712=CARTESIAN_POINT('Ctrl Pts',(-0.376175177636396,-0.446503376249768,
-0.703947842720345));
#65713=CARTESIAN_POINT('Ctrl Pts',(0.170139749313912,-0.558846852703347,
-0.688125672833912));
#65714=CARTESIAN_POINT('Ctrl Pts',(0.560761644923954,-0.162042122222599,
-0.672303502947477));
#65715=CARTESIAN_POINT('Ctrl Pts',(0.441827669102111,0.381714474660563,
-0.656481333061043));
#65716=CARTESIAN_POINT('Ctrl Pts',(-0.0792186750857043,0.578508248809501,
-0.640659163174609));
#65717=CARTESIAN_POINT('Ctrl Pts',(-0.528082212043081,0.249006074485278,
-0.624836993288174));
#65718=CARTESIAN_POINT('Ctrl Pts',(-0.496698309368021,-0.30691808043545,
-0.60901482340174));
#65719=CARTESIAN_POINT('Ctrl Pts',(-0.0135095497561338,-0.58371762189997,
-0.593192653515305));
#65720=CARTESIAN_POINT('Ctrl Pts',(0.48194854247652,-0.329583004223587,
-0.577370483628871));
#65721=CARTESIAN_POINT('Ctrl Pts',(0.539061890683185,0.224313928578695,
-0.561548313742437));
#65722=CARTESIAN_POINT('Ctrl Pts',(0.105868904839035,0.57419150549276,-0.545726143856003));
#65723=CARTESIAN_POINT('Ctrl Pts',(-0.423614127867063,0.401813389515817,
-0.529903973969568));
#65724=CARTESIAN_POINT('Ctrl Pts',(-0.567802091141058,-0.136031167142859,
-0.514081804083134));
#65725=CARTESIAN_POINT('Ctrl Pts',(-0.195547425911708,-0.550149782799461,
-0.498259634196699));
#65726=CARTESIAN_POINT('Ctrl Pts',(0.354566196166392,-0.463881719633473,
-0.482437464310265));
#65727=CARTESIAN_POINT('Ctrl Pts',(0.582185853828999,0.044307788547436,
-0.466615294423831));
#65728=CARTESIAN_POINT('Ctrl Pts',(0.280280787765607,0.512197427400107,
-0.450793124537396));
#65729=CARTESIAN_POINT('Ctrl Pts',(-0.276552406861396,0.514220062509251,
-0.434970954650963));
#65730=CARTESIAN_POINT('Ctrl Pts',(-0.581848581416993,0.0485360909831188,
-0.419148784764527));
#65731=CARTESIAN_POINT('Ctrl Pts',(-0.357926880397705,-0.461293693988608,
-0.403326614878094));
#65732=CARTESIAN_POINT('Ctrl Pts',(0.191545660634918,-0.551555769002358,
-0.387504444991659));
#65733=CARTESIAN_POINT('Ctrl Pts',(0.566798677261749,-0.140152716991604,
-0.371682275105225));
#65734=CARTESIAN_POINT('Ctrl Pts',(0.42652240602603,0.398725702309659,-0.35586010521879));
#65735=CARTESIAN_POINT('Ctrl Pts',(-0.101695476544849,0.574944751540813,
-0.340037935332356));
#65736=CARTESIAN_POINT('Ctrl Pts',(-0.537416675361082,0.228225538314257,
-0.324215765445922));
#65737=CARTESIAN_POINT('Ctrl Pts',(-0.484332866033311,-0.326075709028386,
-0.308393595559487));
#65738=CARTESIAN_POINT('Ctrl Pts',(0.00927381959893476,-0.583795277124447,
-0.292571425673053));
#65739=CARTESIAN_POINT('Ctrl Pts',(0.494445520141122,-0.310528159116424,
-0.276749255786619));
#65740=CARTESIAN_POINT('Ctrl Pts',(0.52989647868524,0.245181937381857,-0.260927085900184));
#65741=CARTESIAN_POINT('Ctrl Pts',(0.083382301845555,0.577881255974982,
-0.24510491601375));
#65742=CARTESIAN_POINT('Ctrl Pts',(-0.438971725989264,0.384983887757886,
-0.229282746127315));
#65743=CARTESIAN_POINT('Ctrl Pts',(-0.562061228182491,-0.158098369381922,
-0.213460576240881));
#65744=CARTESIAN_POINT('Ctrl Pts',(-0.173929773106761,-0.557335878832425,
-0.197638406354447));
#65745=CARTESIAN_POINT('Ctrl Pts',(0.37239760745762,-0.449741497287954,
-0.181816236468012));
#65746=CARTESIAN_POINT('Ctrl Pts',(0.580014557899165,0.0670875694494189,
-0.165994066581578));
#65747=CARTESIAN_POINT('Ctrl Pts',(0.260077575560924,0.522561887705728,
-0.150171896695144));
#65748=CARTESIAN_POINT('Ctrl Pts',(-0.296404153131998,0.503390422117009,
-0.134349726808709));
#65749=CARTESIAN_POINT('Ctrl Pts',(-0.583303893406517,0.0250917757246023,
-0.118527556922275));
#65750=CARTESIAN_POINT('Ctrl Pts',(-0.380281722535441,-0.390289395107438,
-0.105342415350246));
#65751=CARTESIAN_POINT('Ctrl Pts',(-0.0628258658305463,-0.510748101883613,
-0.0947903739238797));
#65752=CARTESIAN_POINT('Ctrl Pts',(0.104302604952409,-0.490354285125624,
-0.0895123891263246));
#65753=CARTESIAN_POINT('Ctrl Pts',(0.180695026285204,-0.460368165683359,
-0.0868714326431751));
#65754=CARTESIAN_POINT('',(0.117283993805721,-0.424080729103529,-0.119999999999908));
#65755=CARTESIAN_POINT('Ctrl Pts',(0.117283993805721,-0.424080729103529,
-0.12));
#65756=CARTESIAN_POINT('Ctrl Pts',(0.117550426203052,-0.423997995716161,
-0.12));
#65757=CARTESIAN_POINT('Ctrl Pts',(0.117816858600383,-0.423915262328792,
-0.12));
#65758=CARTESIAN_POINT('Ctrl Pts',(0.118083290997715,-0.423832528941423,
-0.12));
#65759=CARTESIAN_POINT('Ctrl Pts',(-0.491123371243679,0.0606208880126489,
-0.12));
#65760=CARTESIAN_POINT('Ctrl Pts',(-0.492080117217891,0.047615190510706,
-0.12));
#65761=CARTESIAN_POINT('Ctrl Pts',(-0.492488068218865,0.0346059367317309,
-0.12));
#65762=CARTESIAN_POINT('Ctrl Pts',(-0.492330824576398,0.0216199151589219,
-0.119999999999999));
#65763=CARTESIAN_POINT('Ctrl Pts',(-0.49201965108577,-0.00407845711732452,
-0.119999999999999));
#65764=CARTESIAN_POINT('Ctrl Pts',(-0.489498465803643,-0.0296866016555778,
-0.119999999999999));
#65765=CARTESIAN_POINT('Ctrl Pts',(-0.484915318387734,-0.054991083609342,
-0.119999999999999));
#65766=CARTESIAN_POINT('Ctrl Pts',(-0.481966249957855,-0.0712734856558606,
-0.119999999999999));
#65767=CARTESIAN_POINT('Ctrl Pts',(-0.478162287482436,-0.0874300941371983,
-0.119999999999999));
#65768=CARTESIAN_POINT('Ctrl Pts',(-0.47353228316563,-0.10340020940642,
-0.119999999999999));
#65769=CARTESIAN_POINT('Ctrl Pts',(-0.471503718009439,-0.110397269702435,
-0.119999999999999));
#65770=CARTESIAN_POINT('Ctrl Pts',(-0.469316487641571,-0.117358474639077,
-0.119999999999999));
#65771=CARTESIAN_POINT('Ctrl Pts',(-0.466972594711345,-0.124278411688063,
-0.119999999999999));
#65772=CARTESIAN_POINT('Ctrl Pts',(-0.464920047601107,-0.130338200772182,
-0.119999999999999));
#65773=CARTESIAN_POINT('Ctrl Pts',(-0.462750029372983,-0.136358237212316,
-0.119999999999999));
#65774=CARTESIAN_POINT('Ctrl Pts',(-0.460466874239735,-0.142329905900782,
-0.119999999999999));
#65775=CARTESIAN_POINT('Ctrl Pts',(-0.454534266424897,-0.157846840257503,
-0.119999999999998));
#65776=CARTESIAN_POINT('Ctrl Pts',(-0.447834494625283,-0.173049044034483,
-0.119999999999999));
#65777=CARTESIAN_POINT('Ctrl Pts',(-0.440405049160724,-0.187879519724027,
-0.119999999999999));
#65778=CARTESIAN_POINT('Ctrl Pts',(-0.430752165148136,-0.207148368572245,
-0.119999999999998));
#65779=CARTESIAN_POINT('Ctrl Pts',(-0.419868031369589,-0.225790477133216,
-0.119999999999999));
#65780=CARTESIAN_POINT('Ctrl Pts',(-0.407815725943723,-0.243668211022738,
-0.119999999999999));
#65781=CARTESIAN_POINT('Ctrl Pts',(-0.401748202520733,-0.252668445027085,
-0.119999999999999));
#65782=CARTESIAN_POINT('Ctrl Pts',(-0.395384296714486,-0.261474691340732,
-0.119999999999999));
#65783=CARTESIAN_POINT('Ctrl Pts',(-0.388730354116756,-0.27006745480899,
-0.119999999999999));
#65784=CARTESIAN_POINT('Ctrl Pts',(-0.383733104832073,-0.27652079889252,
-0.119999999999999));
#65785=CARTESIAN_POINT('Ctrl Pts',(-0.378570178487854,-0.282856065934985,
-0.119999999999999));
#65786=CARTESIAN_POINT('Ctrl Pts',(-0.373251230417089,-0.289056005825397,
-0.119999999999999));
#65787=CARTESIAN_POINT('Ctrl Pts',(-0.366987352291694,-0.296357387102605,
-0.119999999999999));
#65788=CARTESIAN_POINT('Ctrl Pts',(-0.360518140092558,-0.303458590347285,
-0.119999999999999));
#65789=CARTESIAN_POINT('Ctrl Pts',(-0.353851489645469,-0.31034682109201,
-0.119999999999999));
#65790=CARTESIAN_POINT('Ctrl Pts',(-0.336767631137862,-0.327998497949016,
-0.119999999999999));
#65791=CARTESIAN_POINT('Ctrl Pts',(-0.318385138846978,-0.344259173584621,
-0.119999999999999));
#65792=CARTESIAN_POINT('Ctrl Pts',(-0.298792194188593,-0.35891278731163,
-0.119999999999999));
#65793=CARTESIAN_POINT('Ctrl Pts',(-0.289653252506453,-0.365747825312231,
-0.119999999999999));
#65794=CARTESIAN_POINT('Ctrl Pts',(-0.280250534791944,-0.37223265094451,
-0.119999999999999));
#65795=CARTESIAN_POINT('Ctrl Pts',(-0.270591090586766,-0.378341879595979,
-0.119999999999999));
#65796=CARTESIAN_POINT('Ctrl Pts',(-0.260227879567575,-0.384896213813854,
-0.12));
#65797=CARTESIAN_POINT('Ctrl Pts',(-0.249569109631511,-0.391018236754718,
-0.119999999999999));
#65798=CARTESIAN_POINT('Ctrl Pts',(-0.23864629776066,-0.396699229261459,
-0.12));
#65799=CARTESIAN_POINT('Ctrl Pts',(-0.232340801497141,-0.399978739835099,
-0.12));
#65800=CARTESIAN_POINT('Ctrl Pts',(-0.225949975898595,-0.403109514421454,
-0.12));
#65801=CARTESIAN_POINT('Ctrl Pts',(-0.219496623082571,-0.406083117869338,
-0.12));
#65802=CARTESIAN_POINT('Ctrl Pts',(-0.197213019410682,-0.416351051856378,
-0.12));
#65803=CARTESIAN_POINT('Ctrl Pts',(-0.174132212877899,-0.424776976216567,
-0.12));
#65804=CARTESIAN_POINT('Ctrl Pts',(-0.150520658792025,-0.431330470391991,
-0.12));
#65805=CARTESIAN_POINT('Ctrl Pts',(-0.135040134457732,-0.435627160295939,
-0.12));
#65806=CARTESIAN_POINT('Ctrl Pts',(-0.119330949077229,-0.439117977054067,
-0.12));
#65807=CARTESIAN_POINT('Ctrl Pts',(-0.103466627673514,-0.441782460714082,
-0.12));
#65808=CARTESIAN_POINT('Ctrl Pts',(-0.0936646074926034,-0.443428753797949,
-0.12));
#65809=CARTESIAN_POINT('Ctrl Pts',(-0.0838033584053894,-0.444759400455696,
-0.12));
#65810=CARTESIAN_POINT('Ctrl Pts',(-0.0739005440596103,-0.44576771286662,
-0.12));
#65811=CARTESIAN_POINT('Ctrl Pts',(-0.067775904198683,-0.446391328554906,
-0.12));
#65812=CARTESIAN_POINT('Ctrl Pts',(-0.0616324034529957,-0.446891719509591,
-0.12));
#65813=CARTESIAN_POINT('Ctrl Pts',(-0.0554891763724216,-0.447266361985043,
-0.12));
#65814=CARTESIAN_POINT('Ctrl Pts',(-0.0312303804256718,-0.448745775857556,
-0.12));
#65815=CARTESIAN_POINT('Ctrl Pts',(-0.00694611010869578,-0.448273303612837,
-0.120000000000001));
#65816=CARTESIAN_POINT('Ctrl Pts',(0.0171508719125321,-0.445867538950042,
-0.12));
#65817=CARTESIAN_POINT('Ctrl Pts',(0.0278703336077171,-0.444797342602311,
-0.12));
#65818=CARTESIAN_POINT('Ctrl Pts',(0.0385536205803394,-0.443343713284888,
-0.120000000000001));
#65819=CARTESIAN_POINT('Ctrl Pts',(0.0491779042183454,-0.441505648869441,
-0.12));
#65820=CARTESIAN_POINT('Ctrl Pts',(0.0567863132575334,-0.440189348741395,
-0.12));
#65821=CARTESIAN_POINT('Ctrl Pts',(0.0643592452838578,-0.438676618147634,
-0.119999999999995));
#65822=CARTESIAN_POINT('Ctrl Pts',(0.0718799379532853,-0.436969919520122,
-0.119999999999986));
#65823=CARTESIAN_POINT('Ctrl Pts',(0.0872391156201996,-0.433484404475689,
-0.119999999999966));
#65824=CARTESIAN_POINT('Ctrl Pts',(0.102394078399616,-0.42918816774082,
-0.11999999999993));
#65825=CARTESIAN_POINT('Ctrl Pts',(0.117283993805721,-0.424080729103529,
-0.119999999999908));
#65826=CARTESIAN_POINT('Ctrl Pts',(-0.254468725618617,-0.356220527001759,
-0.735799999999999));
#65827=CARTESIAN_POINT('Ctrl Pts',(-0.264353107583362,-0.350156188421938,
-0.7358));
#65828=CARTESIAN_POINT('Ctrl Pts',(-0.273959725733427,-0.343690194162452,
-0.7358));
#65829=CARTESIAN_POINT('Ctrl Pts',(-0.283259413984319,-0.33682783052223,
-0.7358));
#65830=CARTESIAN_POINT('Ctrl Pts',(-0.298891697970022,-0.32529256026983,
-0.7358));
#65831=CARTESIAN_POINT('Ctrl Pts',(-0.313657637511065,-0.312638532827742,
-0.7358));
#65832=CARTESIAN_POINT('Ctrl Pts',(-0.327524596172051,-0.299000188399973,
-0.7358));
#65833=CARTESIAN_POINT('Ctrl Pts',(-0.335926090867447,-0.290737202898599,
-0.7358));
#65834=CARTESIAN_POINT('Ctrl Pts',(-0.34400320179419,-0.28210496066844,
-0.7358));
#65835=CARTESIAN_POINT('Ctrl Pts',(-0.35171720368204,-0.27316538278638,
-0.7358));
#65836=CARTESIAN_POINT('Ctrl Pts',(-0.362858848127632,-0.260253589439211,
-0.7358));
#65837=CARTESIAN_POINT('Ctrl Pts',(-0.373251963872608,-0.246695048235492,
-0.7358));
#65838=CARTESIAN_POINT('Ctrl Pts',(-0.382874250241917,-0.232577275099803,
-0.7358));
#65839=CARTESIAN_POINT('Ctrl Pts',(-0.38925049206296,-0.223222083201244,
-0.7358));
#65840=CARTESIAN_POINT('Ctrl Pts',(-0.395288097963382,-0.213621077157663,
-0.7358));
#65841=CARTESIAN_POINT('Ctrl Pts',(-0.400978371636687,-0.203797431456546,
-0.7358));
#65842=CARTESIAN_POINT('Ctrl Pts',(-0.406284528499182,-0.194636922130562,
-0.7358));
#65843=CARTESIAN_POINT('Ctrl Pts',(-0.41129110449982,-0.185276541719071,
-0.7358));
#65844=CARTESIAN_POINT('Ctrl Pts',(-0.415971025607449,-0.17577527097872,
-0.7358));
#65845=CARTESIAN_POINT('Ctrl Pts',(-0.426946975539136,-0.153491674837857,
-0.735799999999999));
#65846=CARTESIAN_POINT('Ctrl Pts',(-0.436153495753634,-0.130397933826654,
-0.735799999999999));
#65847=CARTESIAN_POINT('Ctrl Pts',(-0.443515830646781,-0.106740513259217,
-0.735799999999999));
#65848=CARTESIAN_POINT('Ctrl Pts',(-0.448460962867434,-0.0908502998413962,
-0.735799999999999));
#65849=CARTESIAN_POINT('Ctrl Pts',(-0.452573339202578,-0.0747048900916328,
-0.735799999999999));
#65850=CARTESIAN_POINT('Ctrl Pts',(-0.455818868496034,-0.0583724448329422,
-0.7358));
#65851=CARTESIAN_POINT('Ctrl Pts',(-0.457715300061376,-0.048829050850876,
-0.7358));
#65852=CARTESIAN_POINT('Ctrl Pts',(-0.459315495404145,-0.0392223922419898,
-0.735799999999999));
#65853=CARTESIAN_POINT('Ctrl Pts',(-0.460611248197923,-0.0295634006085556,
-0.735799999999999));
#65854=CARTESIAN_POINT('Ctrl Pts',(-0.461670102536421,-0.0216703323893049,
-0.7358));
#65855=CARTESIAN_POINT('Ctrl Pts',(-0.462524716732938,-0.0137458036513584,
-0.7358));
#65856=CARTESIAN_POINT('Ctrl Pts',(-0.46316948393252,-0.00582069942906378,
-0.7358));
#65857=CARTESIAN_POINT('Ctrl Pts',(-0.464873163375957,0.0151199395478807,
-0.7358));
#65858=CARTESIAN_POINT('Ctrl Pts',(-0.465119446792888,0.0361029865051353,
-0.7358));
#65859=CARTESIAN_POINT('Ctrl Pts',(-0.463852359252848,0.0569912948890308,
-0.7358));
#65860=CARTESIAN_POINT('Ctrl Pts',(-0.462665925504757,0.0765500019428417,
-0.7358));
#65861=CARTESIAN_POINT('Ctrl Pts',(-0.460152673100683,0.0960261356778588,
-0.735799999999999));
#65862=CARTESIAN_POINT('Ctrl Pts',(-0.45638650963416,0.11531015705626,-0.7358));
#65863=CARTESIAN_POINT('Ctrl Pts',(-0.454589389354817,0.124512016241201,
-0.7358));
#65864=CARTESIAN_POINT('Ctrl Pts',(-0.452506667493876,0.133670136132281,
-0.7358));
#65865=CARTESIAN_POINT('Ctrl Pts',(-0.450144715443353,0.142772427126565,
-0.7358));
#65866=CARTESIAN_POINT('Ctrl Pts',(-0.447579296485356,0.152658821675842,
-0.7358));
#65867=CARTESIAN_POINT('Ctrl Pts',(-0.444681359880229,0.162487158070278,
-0.7358));
#65868=CARTESIAN_POINT('Ctrl Pts',(-0.441474687718473,0.172195204108906,
-0.7358));
#65869=CARTESIAN_POINT('Ctrl Pts',(-0.433512738542325,0.19629962303926,
-0.7358));
#65870=CARTESIAN_POINT('Ctrl Pts',(-0.423642167106932,0.219710854775425,
-0.7358));
#65871=CARTESIAN_POINT('Ctrl Pts',(-0.412025148055811,0.242201623455124,
-0.7358));
#65872=CARTESIAN_POINT('Ctrl Pts',(-0.405546266354503,0.254744861010819,
-0.7358));
#65873=CARTESIAN_POINT('Ctrl Pts',(-0.398523189811845,0.267001785731961,
-0.7358));
#65874=CARTESIAN_POINT('Ctrl Pts',(-0.390977259868107,0.278931318470491,
-0.7358));
#65875=CARTESIAN_POINT('Ctrl Pts',(-0.383863888782996,0.290177009044596,
-0.7358));
#65876=CARTESIAN_POINT('Ctrl Pts',(-0.376285824866845,0.301131796958498,
-0.7358));
#65877=CARTESIAN_POINT('Ctrl Pts',(-0.368262330391237,0.311773139319828,
-0.7358));
#65878=CARTESIAN_POINT('Ctrl Pts',(-0.362781109777742,0.31904273304654,
-0.7358));
#65879=CARTESIAN_POINT('Ctrl Pts',(-0.35708820557215,0.326169789138345,
-0.7358));
#65880=CARTESIAN_POINT('Ctrl Pts',(-0.351214427199837,0.3331182156288,-0.735799999999999));
#65881=CARTESIAN_POINT('Ctrl Pts',(-0.334524773991188,0.352861355584183,
-0.735799999999999));
#65882=CARTESIAN_POINT('Ctrl Pts',(-0.316345467065958,0.371211611582931,
-0.735799999999999));
#65883=CARTESIAN_POINT('Ctrl Pts',(-0.296847946523699,0.388026973344292,
-0.735799999999999));
#65884=CARTESIAN_POINT('Ctrl Pts',(-0.277484732686358,0.404726504181137,
-0.735799999999999));
#65885=CARTESIAN_POINT('Ctrl Pts',(-0.256820572877241,0.419913180880695,
-0.7358));
#65886=CARTESIAN_POINT('Ctrl Pts',(-0.234984580042639,0.433415741977161,
-0.7358));
#65887=CARTESIAN_POINT('Ctrl Pts',(-0.229048153413863,0.437086606125949,
-0.7358));
#65888=CARTESIAN_POINT('Ctrl Pts',(-0.22302493302737,0.440632765949028,
-0.7358));
#65889=CARTESIAN_POINT('Ctrl Pts',(-0.21691713542861,0.4440502182833,-0.7358));
#65890=CARTESIAN_POINT('Origin',(-4.51336705371395E-17,0.,-0.7358));
#65891=CARTESIAN_POINT('',(-0.4942,-6.05220448138622E-17,-0.7358));
#65892=CARTESIAN_POINT('Origin',(0.,0.,-0.7358));
#65893=CARTESIAN_POINT('',(0.228820166259496,0.438035354181574,-0.7358));
#65894=CARTESIAN_POINT('Origin',(0.,0.,-0.7358));
#65895=CARTESIAN_POINT('Ctrl Pts',(0.228820166259493,0.438035354181575,
-0.735799999999999));
#65896=CARTESIAN_POINT('Ctrl Pts',(0.236316989062907,0.433616458939398,
-0.735799999999999));
#65897=CARTESIAN_POINT('Ctrl Pts',(0.243680112356663,0.428989449384103,
-0.735799999999998));
#65898=CARTESIAN_POINT('Ctrl Pts',(0.250899612637304,0.424153891241464,
-0.735799999999999));
#65899=CARTESIAN_POINT('Ctrl Pts',(0.267310017136389,0.413162345841524,
-0.735799999999999));
#65900=CARTESIAN_POINT('Ctrl Pts',(0.282979251405834,0.401094089156516,
-0.735799999999999));
#65901=CARTESIAN_POINT('Ctrl Pts',(0.297859083959773,0.388055028479292,
-0.735799999999999));
#65902=CARTESIAN_POINT('Ctrl Pts',(0.303851274087403,0.382804127275908,
-0.735799999999999));
#65903=CARTESIAN_POINT('Ctrl Pts',(0.309715294869631,0.377395648238053,
-0.735799999999999));
#65904=CARTESIAN_POINT('Ctrl Pts',(0.315447349016218,0.37183601851886,-0.735799999999999));
#65905=CARTESIAN_POINT('Ctrl Pts',(0.320512199566927,0.366923522418006,
-0.735799999999999));
#65906=CARTESIAN_POINT('Ctrl Pts',(0.325471210362565,0.361895553184773,
-0.735799999999999));
#65907=CARTESIAN_POINT('Ctrl Pts',(0.330316186686871,0.356763312701958,
-0.735799999999999));
#65908=CARTESIAN_POINT('Ctrl Pts',(0.347900557934295,0.338136344077132,
-0.735799999999999));
#65909=CARTESIAN_POINT('Ctrl Pts',(0.364009894806326,0.318115267361153,
-0.735799999999999));
#65910=CARTESIAN_POINT('Ctrl Pts',(0.378529988854265,0.296924385166985,
-0.735799999999999));
#65911=CARTESIAN_POINT('Ctrl Pts',(0.383986361678478,0.288961258113977,
-0.735799999999999));
#65912=CARTESIAN_POINT('Ctrl Pts',(0.389218397477593,0.280831801409261,
-0.735799999999999));
#65913=CARTESIAN_POINT('Ctrl Pts',(0.394216643597978,0.272550027802377,
-0.735799999999999));
#65914=CARTESIAN_POINT('Ctrl Pts',(0.398123146411223,0.266077202912462,
-0.7358));
#65915=CARTESIAN_POINT('Ctrl Pts',(0.40188294746496,0.259517556378562,-0.735799999999999));
#65916=CARTESIAN_POINT('Ctrl Pts',(0.405489037713727,0.252884933996346,
-0.735799999999999));
#65917=CARTESIAN_POINT('Ctrl Pts',(0.417666248863211,0.23048759015542,-0.735799999999999));
#65918=CARTESIAN_POINT('Ctrl Pts',(0.428112091848353,0.207230094193275,
-0.7358));
#65919=CARTESIAN_POINT('Ctrl Pts',(0.436709111403403,0.183328936062516,
-0.7358));
#65920=CARTESIAN_POINT('Ctrl Pts',(0.442380018901443,0.167562860856144,
-0.7358));
#65921=CARTESIAN_POINT('Ctrl Pts',(0.447245552684248,0.151516184828499,
-0.7358));
#65922=CARTESIAN_POINT('Ctrl Pts',(0.451259697186057,0.135248728490274,
-0.7358));
#65923=CARTESIAN_POINT('Ctrl Pts',(0.45361287992984,0.125712375844498,-0.7358));
#65924=CARTESIAN_POINT('Ctrl Pts',(0.455673284346557,0.116100135704311,
-0.7358));
#65925=CARTESIAN_POINT('Ctrl Pts',(0.457429894614468,0.106424173228407,
-0.7358));
#65926=CARTESIAN_POINT('Ctrl Pts',(0.45881226543766,0.0988096394542803,
-0.735799999999999));
#65927=CARTESIAN_POINT('Ctrl Pts',(0.460006040688075,0.0911556810687175,
-0.7358));
#65928=CARTESIAN_POINT('Ctrl Pts',(0.461003311645071,0.0834930990972771,
-0.7358));
#65929=CARTESIAN_POINT('Ctrl Pts',(0.46375279125733,0.0623673330655312,
-0.7358));
#65930=CARTESIAN_POINT('Ctrl Pts',(0.465020086686708,0.0411290663620106,
-0.7358));
#65931=CARTESIAN_POINT('Ctrl Pts',(0.464720781957338,0.0199037385120108,
-0.7358));
#65932=CARTESIAN_POINT('Ctrl Pts',(0.464453659527758,0.000960632748610985,
-0.7358));
#65933=CARTESIAN_POINT('Ctrl Pts',(0.462938198968576,-0.017972555627716,
-0.7358));
#65934=CARTESIAN_POINT('Ctrl Pts',(0.460221890912084,-0.0367828973530338,
-0.7358));
#65935=CARTESIAN_POINT('Ctrl Pts',(0.458149135112,-0.0511366613966768,-0.7358));
#65936=CARTESIAN_POINT('Ctrl Pts',(0.455376742418919,-0.0654188854679344,
-0.7358));
#65937=CARTESIAN_POINT('Ctrl Pts',(0.451919535610315,-0.0795763120724046,
-0.7358));
#65938=CARTESIAN_POINT('Ctrl Pts',(0.447468037670369,-0.0978054082340508,
-0.7358));
#65939=CARTESIAN_POINT('Ctrl Pts',(0.441907724804691,-0.115721130446471,
-0.7358));
#65940=CARTESIAN_POINT('Ctrl Pts',(0.435296532066892,-0.133213011861257,
-0.7358));
#65941=CARTESIAN_POINT('Ctrl Pts',(0.426856194344684,-0.155544441664159,
-0.7358));
#65942=CARTESIAN_POINT('Ctrl Pts',(0.416703258734146,-0.177189395420981,
-0.7358));
#65943=CARTESIAN_POINT('Ctrl Pts',(0.404917880756747,-0.19791002689791,
-0.7358));
#65944=CARTESIAN_POINT('Ctrl Pts',(0.398500717044332,-0.209192455401017,
-0.7358));
#65945=CARTESIAN_POINT('Ctrl Pts',(0.391598855565479,-0.220200352930322,
-0.7358));
#65946=CARTESIAN_POINT('Ctrl Pts',(0.384228438675215,-0.230904646838916,
-0.7358));
#65947=CARTESIAN_POINT('Ctrl Pts',(0.379522006890116,-0.237739949351449,
-0.7358));
#65948=CARTESIAN_POINT('Ctrl Pts',(0.374622283186425,-0.244453507108068,
-0.735799999999999));
#65949=CARTESIAN_POINT('Ctrl Pts',(0.369553954994059,-0.251011959085564,
-0.735799999999999));
#65950=CARTESIAN_POINT('Ctrl Pts',(0.354874618110099,-0.270007123242443,
-0.735799999999999));
#65951=CARTESIAN_POINT('Ctrl Pts',(0.338750738128904,-0.287754783607563,
-0.735799999999999));
#65952=CARTESIAN_POINT('Ctrl Pts',(0.321310977016985,-0.30409383577115,
-0.7358));
#65953=CARTESIAN_POINT('Ctrl Pts',(0.304262041952272,-0.32006672883822,
-0.7358));
#65954=CARTESIAN_POINT('Ctrl Pts',(0.285954603339099,-0.334694148798622,
-0.7358));
#65955=CARTESIAN_POINT('Ctrl Pts',(0.26648175861671,-0.347784488239777,
-0.7358));
#65956=CARTESIAN_POINT('Ctrl Pts',(0.262319512338524,-0.35058249836084,
-0.7358));
#65957=CARTESIAN_POINT('Ctrl Pts',(0.258103949731175,-0.353310108913971,
-0.7358));
#65958=CARTESIAN_POINT('Ctrl Pts',(0.253835875722689,-0.355965150255044,
-0.7358));
#65959=CARTESIAN_POINT('Ctrl Pts',(0.287047174344898,-0.402732536982762,
-0.768920421448668));
#65960=CARTESIAN_POINT('Ctrl Pts',(0.353806905076701,-0.355150314361416,
-0.766282186574675));
#65961=CARTESIAN_POINT('Ctrl Pts',(0.462114121615473,-0.226365817495061,
-0.761006923386275));
#65962=CARTESIAN_POINT('Ctrl Pts',(0.534659959470215,0.105244592708357,
-0.750457603569065));
#65963=CARTESIAN_POINT('Ctrl Pts',(0.297699882545806,0.502243459957053,
-0.737272461997036));
#65964=CARTESIAN_POINT('Ctrl Pts',(-0.259650455921768,0.523296542714125,
-0.721450292110602));
#65965=CARTESIAN_POINT('Ctrl Pts',(-0.579765127206865,0.0677026564476974,
-0.705628122224166));
#65966=CARTESIAN_POINT('Ctrl Pts',(-0.37310450485665,-0.449122313750527,
-0.689805952337734));
#65967=CARTESIAN_POINT('Ctrl Pts',(0.173195203905992,-0.55762972329304,
-0.673983782451298));
#65968=CARTESIAN_POINT('Ctrl Pts',(0.561818783331492,-0.158854163257542,
-0.658161612564864));
#65969=CARTESIAN_POINT('Ctrl Pts',(0.439518970328374,0.38435807019179,-0.642339442678429));
#65970=CARTESIAN_POINT('Ctrl Pts',(-0.0825831408533865,0.578004249452697,
-0.626517272791996));
#65971=CARTESIAN_POINT('Ctrl Pts',(-0.529551478372892,0.245916087209467,
-0.61069510290556));
#65972=CARTESIAN_POINT('Ctrl Pts',(-0.494879278247576,-0.309837196314249,
-0.594872933019126));
#65973=CARTESIAN_POINT('Ctrl Pts',(-0.010086200220884,-0.583782926351103,
-0.579050763132692));
#65974=CARTESIAN_POINT('Ctrl Pts',(0.483877844048874,-0.326749585733395,
-0.563228593246258));
#65975=CARTESIAN_POINT('Ctrl Pts',(0.537734390222952,0.227476475521788,
-0.547406423359823));
#65976=CARTESIAN_POINT('Ctrl Pts',(0.102496165195714,0.57480278682962,-0.531584253473389));
#65977=CARTESIAN_POINT('Ctrl Pts',(-0.425966598017122,0.399319450617198,
-0.515762083586955));
#65978=CARTESIAN_POINT('Ctrl Pts',(-0.566993494230472,-0.139363031519207,
-0.499939913700521));
#65979=CARTESIAN_POINT('Ctrl Pts',(-0.192313798984891,-0.551288541463694,
-0.484117743814086));
#65980=CARTESIAN_POINT('Ctrl Pts',(0.357284023531408,-0.461791902996352,
-0.468295573927652));
#65981=CARTESIAN_POINT('Ctrl Pts',(0.581915737174481,0.0477255410775767,
-0.452473404041217));
#65982=CARTESIAN_POINT('Ctrl Pts',(0.27726849072569,0.513834444634811,-0.436651234154783));
#65983=CARTESIAN_POINT('Ctrl Pts',(-0.27956710218963,0.512587427193721,
-0.420829064268349));
#65984=CARTESIAN_POINT('Ctrl Pts',(-0.58212365522641,0.0451187683232971,
-0.405006894381914));
#65985=CARTESIAN_POINT('Ctrl Pts',(-0.355212141653185,-0.463387539189459,
-0.38918472449548));
#65986=CARTESIAN_POINT('Ctrl Pts',(0.194781019166425,-0.550421584642162,
-0.373362554609046));
#65987=CARTESIAN_POINT('Ctrl Pts',(0.567611984296084,-0.136822304140763,
-0.357540384722611));
#65988=CARTESIAN_POINT('Ctrl Pts',(0.42417384978651,0.401223586671516,-0.341718214836177));
#65989=CARTESIAN_POINT('Ctrl Pts',(-0.10506963626688,0.574337384533757,
-0.325896044949742));
#65990=CARTESIAN_POINT('Ctrl Pts',(-0.538747758010019,0.225066856229725,
-0.310073875063308));
#65991=CARTESIAN_POINT('Ctrl Pts',(-0.482409667299879,-0.328915644435373,
-0.294251705176874));
#65992=CARTESIAN_POINT('Ctrl Pts',(0.012701054010981,-0.583727824779955,
-0.278429535290439));
#65993=CARTESIAN_POINT('Ctrl Pts',(0.496261505533139,-0.30762543078323,
-0.262607365404005));
#65994=CARTESIAN_POINT('Ctrl Pts',(0.528445756192563,0.248300491667137,
-0.246785195517571));
#65995=CARTESIAN_POINT('Ctrl Pts',(0.079991563384182,0.578339295116359,
-0.230963025631136));
#65996=CARTESIAN_POINT('Ctrl Pts',(-0.441232296079768,0.382441561355567,
-0.215140855744702));
#65997=CARTESIAN_POINT('Ctrl Pts',(-0.561108876051582,-0.161476479615712,
-0.199318685858268));
#65998=CARTESIAN_POINT('Ctrl Pts',(-0.170682109742751,-0.558192502483715,
-0.183496515971833));
#65999=CARTESIAN_POINT('Ctrl Pts',(0.375086411458179,-0.447847981815665,
-0.167674346085399));
#66000=CARTESIAN_POINT('Ctrl Pts',(0.57949957025952,0.071091217505752,-0.151852176198965));
#66001=CARTESIAN_POINT('Ctrl Pts',(0.310985042693996,0.44746619959015,-0.138667034626936));
#66002=CARTESIAN_POINT('Ctrl Pts',(-0.0218228806034698,0.514106220352834,
-0.128118921369313));
#66003=CARTESIAN_POINT('Ctrl Pts',(-0.183213450909262,0.466623101184697,
-0.122844864740502));
#66004=CARTESIAN_POINT('Ctrl Pts',(-0.253566780180828,0.424609779704417,
-0.120207836426096));
#66005=CARTESIAN_POINT('Ctrl Pts',(0.275865587548243,-0.387044562250431,
-0.757797765364769));
#66006=CARTESIAN_POINT('Ctrl Pts',(0.340024771086357,-0.341315849434336,
-0.755159530490776));
#66007=CARTESIAN_POINT('Ctrl Pts',(0.444113006737419,-0.217548001949956,
-0.749884267302376));
#66008=CARTESIAN_POINT('Ctrl Pts',(0.513832906365942,0.101144912748319,
-0.739334947485166));
#66009=CARTESIAN_POINT('Ctrl Pts',(0.286103331966143,0.482679153660087,
-0.726149805913137));
#66010=CARTESIAN_POINT('Ctrl Pts',(-0.249536076233809,0.502912138213013,
-0.710327636026703));
#66011=CARTESIAN_POINT('Ctrl Pts',(-0.557181055071921,0.0650653786860826,
-0.694505466140268));
#66012=CARTESIAN_POINT('Ctrl Pts',(-0.358570655447406,-0.431627279545863,
-0.678683296253835));
#66013=CARTESIAN_POINT('Ctrl Pts',(0.166448587397194,-0.535907909916455,
-0.662861126367399));
#66014=CARTESIAN_POINT('Ctrl Pts',(0.539933790022817,-0.152666185206451,
-0.647038956480965));
#66015=CARTESIAN_POINT('Ctrl Pts',(0.422398023129646,0.36938585131295,-0.631216786594532));
#66016=CARTESIAN_POINT('Ctrl Pts',(-0.0793662112337171,0.555488770250224,
-0.615394616708097));
#66017=CARTESIAN_POINT('Ctrl Pts',(-0.508923420172224,0.236336713783819,
-0.599572446821662));
#66018=CARTESIAN_POINT('Ctrl Pts',(-0.475601835032119,-0.297767850878864,
-0.583750276935229));
#66019=CARTESIAN_POINT('Ctrl Pts',(-0.00969330409335463,-0.561042345551805,
-0.567928107048793));
#66020=CARTESIAN_POINT('Ctrl Pts',(0.465028948829617,-0.31402143795773,
-0.55210593716236));
#66021=CARTESIAN_POINT('Ctrl Pts',(0.516787576266163,0.218615395592856,
-0.536283767275924));
#66022=CARTESIAN_POINT('Ctrl Pts',(0.0985035470134388,0.552412016857531,
-0.520461597389491));
#66023=CARTESIAN_POINT('Ctrl Pts',(-0.409373567623862,0.383764428670513,
-0.504639427503056));
#66024=CARTESIAN_POINT('Ctrl Pts',(-0.544906926113765,-0.133934307697998,
-0.488817257616623));
#66025=CARTESIAN_POINT('Ctrl Pts',(-0.184822439975864,-0.529813741405321,
-0.472995087730187));
#66026=CARTESIAN_POINT('Ctrl Pts',(0.343366442460311,-0.44380333976757,
-0.457172917843752));
#66027=CARTESIAN_POINT('Ctrl Pts',(0.559247890544722,0.0458664484695617,
-0.44135074795732));
#66028=CARTESIAN_POINT('Ctrl Pts',(0.266467821107177,0.493818625092579,
-0.425528578070885));
#66029=CARTESIAN_POINT('Ctrl Pts',(-0.268676892851193,0.492620183756744,
-0.409706408184451));
#66030=CARTESIAN_POINT('Ctrl Pts',(-0.559447709392226,0.0433612194976846,
-0.393884238298015));
#66031=CARTESIAN_POINT('Ctrl Pts',(-0.341375268316301,-0.445336819819863,
-0.378062068411582));
#66032=CARTESIAN_POINT('Ctrl Pts',(0.187193552482174,-0.528980555872327,
-0.362239898525148));
#66033=CARTESIAN_POINT('Ctrl Pts',(0.545501323622579,-0.131492551381623,
-0.346417728638712));
#66034=CARTESIAN_POINT('Ctrl Pts',(0.407650653802841,0.385594391332905,
-0.330595558752279));
#66035=CARTESIAN_POINT('Ctrl Pts',(-0.100976771530301,0.551964743763527,
-0.314773388865843));
#66036=CARTESIAN_POINT('Ctrl Pts',(-0.517761469496849,0.21629964020077,
-0.29895121897941));
#66037=CARTESIAN_POINT('Ctrl Pts',(-0.463617963187935,-0.316103120377524,
-0.283129049092976));
#66038=CARTESIAN_POINT('Ctrl Pts',(0.0122062993137546,-0.560989390397886,
-0.26730687920654));
#66039=CARTESIAN_POINT('Ctrl Pts',(0.476930219271146,-0.295642242086072,
-0.251484709320108));
#66040=CARTESIAN_POINT('Ctrl Pts',(0.507860770105602,0.238628236555884,
-0.235662539433672));
#66041=CARTESIAN_POINT('Ctrl Pts',(0.0768755856323659,0.555810764602103,
-0.219840369547239));
#66042=CARTESIAN_POINT('Ctrl Pts',(-0.424044608281193,0.367543997835894,
-0.204018199660804));
#66043=CARTESIAN_POINT('Ctrl Pts',(-0.539251536350318,-0.155186352299316,
-0.18819602977437));
#66044=CARTESIAN_POINT('Ctrl Pts',(-0.164033387876457,-0.536448766702277,
-0.172373859887935));
#66045=CARTESIAN_POINT('Ctrl Pts',(0.360475359196343,-0.4304025877204,-0.156551690001501));
#66046=CARTESIAN_POINT('Ctrl Pts',(0.556925842584725,0.068321942313148,
-0.140729520115067));
#66047=CARTESIAN_POINT('Ctrl Pts',(0.298870984246006,0.43003567737475,-0.127544378543038));
#66048=CARTESIAN_POINT('Ctrl Pts',(-0.0209727958249744,0.494079814105516,
-0.116996265285415));
#66049=CARTESIAN_POINT('Ctrl Pts',(-0.176076585311013,0.448446344283576,
-0.111722208656604));
#66050=CARTESIAN_POINT('Ctrl Pts',(-0.243689382962719,0.408069602580887,
-0.109085180342198));
#66051=CARTESIAN_POINT('Ctrl Pts',(0.264684000751588,-0.371356587518099,
-0.746675109280871));
#66052=CARTESIAN_POINT('Ctrl Pts',(0.326242637096013,-0.327481384507258,
-0.744036874406877));
#66053=CARTESIAN_POINT('Ctrl Pts',(0.426111891859364,-0.208730186404851,
-0.738761611218477));
#66054=CARTESIAN_POINT('Ctrl Pts',(0.493005853261671,0.0970452327882826,
-0.728212291401267));
#66055=CARTESIAN_POINT('Ctrl Pts',(0.274506781386479,0.463114847363122,
-0.715027149829239));
#66056=CARTESIAN_POINT('Ctrl Pts',(-0.239421696545848,0.482527733711901,
-0.699204979942805));
#66057=CARTESIAN_POINT('Ctrl Pts',(-0.534596982936976,0.0624281009244681,
-0.68338281005637));
#66058=CARTESIAN_POINT('Ctrl Pts',(-0.344036806038162,-0.414132245341199,
-0.667560640169936));
#66059=CARTESIAN_POINT('Ctrl Pts',(0.159701970888396,-0.51418609653987,
-0.651738470283501));
#66060=CARTESIAN_POINT('Ctrl Pts',(0.518048796714141,-0.146478207155357,
-0.635916300397068));
#66061=CARTESIAN_POINT('Ctrl Pts',(0.405277075930918,0.35441363243411,-0.620094130510632));
#66062=CARTESIAN_POINT('Ctrl Pts',(-0.0761492816140481,0.532973291047753,
-0.604271960624199));
#66063=CARTESIAN_POINT('Ctrl Pts',(-0.488295361971557,0.226757340358172,
-0.588449790737764));
#66064=CARTESIAN_POINT('Ctrl Pts',(-0.456324391816661,-0.285698505443478,
-0.57262762085133));
#66065=CARTESIAN_POINT('Ctrl Pts',(-0.00930040796582533,-0.538301764752508,
-0.556805450964895));
#66066=CARTESIAN_POINT('Ctrl Pts',(0.44618005361036,-0.301293290182064,
-0.540983281078462));
#66067=CARTESIAN_POINT('Ctrl Pts',(0.495840762309375,0.209754315663926,
-0.525161111192026));
#66068=CARTESIAN_POINT('Ctrl Pts',(0.0945109288311632,0.530021246885443,
-0.509338941305593));
#66069=CARTESIAN_POINT('Ctrl Pts',(-0.392780537230601,0.368209406723828,
-0.493516771419158));
#66070=CARTESIAN_POINT('Ctrl Pts',(-0.522820357997059,-0.128505583876788,
-0.477694601532724));
#66071=CARTESIAN_POINT('Ctrl Pts',(-0.177331080966838,-0.508338941346947,
-0.461872431646289));
#66072=CARTESIAN_POINT('Ctrl Pts',(0.329448861389214,-0.425814776538789,
-0.446050261759855));
#66073=CARTESIAN_POINT('Ctrl Pts',(0.536580043914961,0.0440073558615464,
-0.430228091873421));
#66074=CARTESIAN_POINT('Ctrl Pts',(0.255667151488665,0.473802805550347,
-0.414405921986986));
#66075=CARTESIAN_POINT('Ctrl Pts',(-0.257786683512757,0.472652940319767,
-0.398583752100552));
#66076=CARTESIAN_POINT('Ctrl Pts',(-0.536771763558043,0.0416036706720726,
-0.382761582214118));
#66077=CARTESIAN_POINT('Ctrl Pts',(-0.327538394979417,-0.427286100450265,
-0.366939412327683));
#66078=CARTESIAN_POINT('Ctrl Pts',(0.179606085797923,-0.507539527102493,
-0.351117242441249));
#66079=CARTESIAN_POINT('Ctrl Pts',(0.523390662949075,-0.126162798622482,
-0.335295072554814));
#66080=CARTESIAN_POINT('Ctrl Pts',(0.391127457819172,0.369965195994294,
-0.31947290266838));
#66081=CARTESIAN_POINT('Ctrl Pts',(-0.0968839067937205,0.529592102993296,
-0.303650732781946));
#66082=CARTESIAN_POINT('Ctrl Pts',(-0.496775180983678,0.207532424171815,
-0.287828562895511));
#66083=CARTESIAN_POINT('Ctrl Pts',(-0.444826259075989,-0.303290596319674,
-0.272006393009077));
#66084=CARTESIAN_POINT('Ctrl Pts',(0.0117115446165282,-0.538250956015816,
-0.256184223122643));
#66085=CARTESIAN_POINT('Ctrl Pts',(0.457598933009152,-0.283659053388913,
-0.240362053236208));
#66086=CARTESIAN_POINT('Ctrl Pts',(0.487275784018641,0.228955981444631,
-0.224539883349774));
#66087=CARTESIAN_POINT('Ctrl Pts',(0.0737596078805499,0.533282234087846,
-0.20871771346334));
#66088=CARTESIAN_POINT('Ctrl Pts',(-0.406856920482618,0.352646434316222,
-0.192895543576905));
#66089=CARTESIAN_POINT('Ctrl Pts',(-0.517394196649054,-0.148896224982918,
-0.177073373690471));
#66090=CARTESIAN_POINT('Ctrl Pts',(-0.157384666010164,-0.514705030920839,
-0.161251203804036));
#66091=CARTESIAN_POINT('Ctrl Pts',(0.345864306934509,-0.412957193625136,
-0.145429033917602));
#66092=CARTESIAN_POINT('Ctrl Pts',(0.534352114909929,0.0655526671205438,
-0.129606864031168));
#66093=CARTESIAN_POINT('Ctrl Pts',(0.286756925798016,0.412605155159349,
-0.116421722459139));
#66094=CARTESIAN_POINT('Ctrl Pts',(-0.0201227110464791,0.474053407858199,
-0.105873609201516));
#66095=CARTESIAN_POINT('Ctrl Pts',(-0.168939719712765,0.430269587382454,
-0.100599552572705));
#66096=CARTESIAN_POINT('Ctrl Pts',(-0.23381198574461,0.391529425457356,
-0.0979625242582989));
#66097=CARTESIAN_POINT('Ctrl Pts',(0.253502413954933,-0.355668612785768,
-0.735552453196972));
#66098=CARTESIAN_POINT('Ctrl Pts',(0.312460503105669,-0.313646919580179,
-0.732914218322978));
#66099=CARTESIAN_POINT('Ctrl Pts',(0.40811077698131,-0.199912370859746,
-0.727638955134579));
#66100=CARTESIAN_POINT('Ctrl Pts',(0.4721788001574,0.0929455528282454,-0.717089635317369));
#66101=CARTESIAN_POINT('Ctrl Pts',(0.262910230806816,0.443550541066156,
-0.70390449374534));
#66102=CARTESIAN_POINT('Ctrl Pts',(-0.229307316857889,0.462143329210789,
-0.688082323858905));
#66103=CARTESIAN_POINT('Ctrl Pts',(-0.512012910802029,0.0597908231628538,
-0.672260153972472));
#66104=CARTESIAN_POINT('Ctrl Pts',(-0.329502956628918,-0.396637211136535,
-0.656437984086036));
#66105=CARTESIAN_POINT('Ctrl Pts',(0.152955354379598,-0.492464283163283,
-0.640615814199603));
#66106=CARTESIAN_POINT('Ctrl Pts',(0.496163803405466,-0.140290229104266,
-0.624793644313168));
#66107=CARTESIAN_POINT('Ctrl Pts',(0.388156128732189,0.339441413555271,
-0.608971474426735));
#66108=CARTESIAN_POINT('Ctrl Pts',(-0.0729323519943785,0.510457811845281,
-0.593149304540299));
#66109=CARTESIAN_POINT('Ctrl Pts',(-0.467667303770891,0.217177966932526,
-0.577327134653866));
#66110=CARTESIAN_POINT('Ctrl Pts',(-0.437046948601204,-0.273629160008092,
-0.56150496476743));
#66111=CARTESIAN_POINT('Ctrl Pts',(-0.00890751183829607,-0.51556118395321,
-0.545682794880997));
#66112=CARTESIAN_POINT('Ctrl Pts',(0.427331158391103,-0.288565142406399,
-0.529860624994562));
#66113=CARTESIAN_POINT('Ctrl Pts',(0.474893948352587,0.200893235734995,
-0.514038455108128));
#66114=CARTESIAN_POINT('Ctrl Pts',(0.0905183106488877,0.507630476913353,
-0.498216285221693));
#66115=CARTESIAN_POINT('Ctrl Pts',(-0.376187506837341,0.352654384777143,
-0.482394115335259));
#66116=CARTESIAN_POINT('Ctrl Pts',(-0.500733789880351,-0.12307686005558,
-0.466571945448824));
#66117=CARTESIAN_POINT('Ctrl Pts',(-0.169839721957813,-0.486864141288574,
-0.450749775562391));
#66118=CARTESIAN_POINT('Ctrl Pts',(0.315531280318115,-0.407826213310007,
-0.434927605675956));
#66119=CARTESIAN_POINT('Ctrl Pts',(0.513912197285202,0.0421482632535317,
-0.419105435789522));
#66120=CARTESIAN_POINT('Ctrl Pts',(0.244866481870151,0.453786986008114,
-0.403283265903088));
#66121=CARTESIAN_POINT('Ctrl Pts',(-0.24689647417432,0.452685696882792,
-0.387461096016653));
#66122=CARTESIAN_POINT('Ctrl Pts',(-0.514095817723861,0.0398461218464604,
-0.371638926130219));
#66123=CARTESIAN_POINT('Ctrl Pts',(-0.313701521642532,-0.409235381080669,
-0.355816756243784));
#66124=CARTESIAN_POINT('Ctrl Pts',(0.172018619113672,-0.486098498332657,
-0.33999458635735));
#66125=CARTESIAN_POINT('Ctrl Pts',(0.501280002275571,-0.12083304586334,
-0.324172416470915));
#66126=CARTESIAN_POINT('Ctrl Pts',(0.374604261835502,0.354336000655682,
-0.308350246584481));
#66127=CARTESIAN_POINT('Ctrl Pts',(-0.0927910420571407,0.507219462223066,
-0.292528076698047));
#66128=CARTESIAN_POINT('Ctrl Pts',(-0.475788892470508,0.198765208142859,
-0.276705906811612));
#66129=CARTESIAN_POINT('Ctrl Pts',(-0.426034554964045,-0.290478072261824,
-0.260883736925178));
#66130=CARTESIAN_POINT('Ctrl Pts',(0.0112167899193015,-0.515512521633748,
-0.245061567038744));
#66131=CARTESIAN_POINT('Ctrl Pts',(0.438267646747159,-0.271675864691754,
-0.229239397152309));
#66132=CARTESIAN_POINT('Ctrl Pts',(0.46669079793168,0.219283726333378,-0.213417227265875));
#66133=CARTESIAN_POINT('Ctrl Pts',(0.0706436301287334,0.510753703573591,
-0.197595057379441));
#66134=CARTESIAN_POINT('Ctrl Pts',(-0.389669232684042,0.33774887079655,
-0.181772887493006));
#66135=CARTESIAN_POINT('Ctrl Pts',(-0.495536856947789,-0.142606097666521,
-0.165950717606572));
#66136=CARTESIAN_POINT('Ctrl Pts',(-0.150735944143869,-0.492961295139401,
-0.150128547720138));
#66137=CARTESIAN_POINT('Ctrl Pts',(0.331253254672673,-0.395511799529872,
-0.134306377833703));
#66138=CARTESIAN_POINT('Ctrl Pts',(0.511778387235135,0.0627833919279398,
-0.118484207947269));
#66139=CARTESIAN_POINT('Ctrl Pts',(0.274642867350025,0.395174632943949,
-0.10529906637524));
#66140=CARTESIAN_POINT('Ctrl Pts',(-0.0192726262679835,0.454027001610881,
-0.0947509531176172));
#66141=CARTESIAN_POINT('Ctrl Pts',(-0.161802854114516,0.412092830481332,
-0.0894768964888058));
#66142=CARTESIAN_POINT('Ctrl Pts',(-0.223934588526501,0.374989248333826,
-0.0868398681744001));
#66143=CARTESIAN_POINT('',(0.435851714755768,0.0627985268057629,-0.120000000000001));
#66144=CARTESIAN_POINT('Ctrl Pts',(0.436962529762211,0.0516115063121503,
-0.12));
#66145=CARTESIAN_POINT('Ctrl Pts',(0.436592258093396,0.0553405131433545,
-0.12));
#66146=CARTESIAN_POINT('Ctrl Pts',(0.436221986424582,0.0590695199745587,
-0.12));
#66147=CARTESIAN_POINT('Ctrl Pts',(0.435851714755768,0.0627985268057629,
-0.12));
#66148=CARTESIAN_POINT('Ctrl Pts',(0.228820166259496,0.438035354181574,
-0.7358));
#66149=CARTESIAN_POINT('Ctrl Pts',(0.22491465564395,0.440009924652994,-0.7358));
#66150=CARTESIAN_POINT('Ctrl Pts',(0.221009145028404,0.441984495124415,
-0.7358));
#66151=CARTESIAN_POINT('Ctrl Pts',(0.217103634412858,0.443959065595836,
-0.7358));
#66152=CARTESIAN_POINT('Ctrl Pts',(0.436199126192416,0.0628594907761131,
-0.120000000000003));
#66153=CARTESIAN_POINT('Ctrl Pts',(0.434282017858336,0.0862483264787582,
-0.120000000000003));
#66154=CARTESIAN_POINT('Ctrl Pts',(0.430334856380413,0.109415622186605,
-0.120000000000002));
#66155=CARTESIAN_POINT('Ctrl Pts',(0.424527759942032,0.132185099075521,
-0.120000000000001));
#66156=CARTESIAN_POINT('Ctrl Pts',(0.420100481655662,0.149544344214974,
-0.120000000000001));
#66157=CARTESIAN_POINT('Ctrl Pts',(0.414590868119256,0.166672689290124,
-0.120000000000001));
#66158=CARTESIAN_POINT('Ctrl Pts',(0.408054534382917,0.18348953378457,-0.120000000000001));
#66159=CARTESIAN_POINT('Ctrl Pts',(0.40502540392714,0.191282957113767,-0.120000000000001));
#66160=CARTESIAN_POINT('Ctrl Pts',(0.401780759259403,0.198995404037311,
-0.12));
#66161=CARTESIAN_POINT('Ctrl Pts',(0.398332969755228,0.206608400908161,
-0.12));
#66162=CARTESIAN_POINT('Ctrl Pts',(0.388174784716126,0.229038491498828,
-0.120000000000001));
#66163=CARTESIAN_POINT('Ctrl Pts',(0.376245486250458,0.250636268527475,
-0.120000000000001));
#66164=CARTESIAN_POINT('Ctrl Pts',(0.362715113103607,0.271207164179327,
-0.120000000000001));
#66165=CARTESIAN_POINT('Ctrl Pts',(0.352729984400094,0.286388049318335,
-0.12));
#66166=CARTESIAN_POINT('Ctrl Pts',(0.341871626615223,0.301009751788514,
-0.12));
#66167=CARTESIAN_POINT('Ctrl Pts',(0.33019145063168,0.31498725114189,-0.12));
#66168=CARTESIAN_POINT('Ctrl Pts',(0.325584301106223,0.320500561010141,
-0.120000000000001));
#66169=CARTESIAN_POINT('Ctrl Pts',(0.320849147972658,0.325913550689098,
-0.120000000000001));
#66170=CARTESIAN_POINT('Ctrl Pts',(0.315988625581974,0.331220579977179,
-0.120000000000001));
#66171=CARTESIAN_POINT('Ctrl Pts',(0.311350868263747,0.336284380108213,
-0.120000000000001));
#66172=CARTESIAN_POINT('Ctrl Pts',(0.306602392532854,0.34124766516251,-0.120000000000001));
#66173=CARTESIAN_POINT('Ctrl Pts',(0.30175612487152,0.346096268998127,-0.120000000000001));
#66174=CARTESIAN_POINT('Ctrl Pts',(0.291874915505376,0.355982241664367,
-0.12));
#66175=CARTESIAN_POINT('Ctrl Pts',(0.281576313869693,0.365403929425632,
-0.12));
#66176=CARTESIAN_POINT('Ctrl Pts',(0.270887565775841,0.374326851892634,
-0.12));
#66177=CARTESIAN_POINT('Ctrl Pts',(0.251903626591773,0.390174565391949,
-0.12));
#66178=CARTESIAN_POINT('Ctrl Pts',(0.231691070691565,0.40445115675579,-0.12));
#66179=CARTESIAN_POINT('Ctrl Pts',(0.210372408766704,0.416938641833649,
-0.120000000000001));
#66180=CARTESIAN_POINT('Ctrl Pts',(0.208825510914833,0.417844742972186,
-0.120000000000001));
#66181=CARTESIAN_POINT('Ctrl Pts',(0.207272774284322,0.418741407052641,
-0.12));
#66182=CARTESIAN_POINT('Ctrl Pts',(0.205714238886768,0.419628542173557,
-0.12));
#66183=CARTESIAN_POINT('Ctrl Pts',(0.194936314682677,0.425763452620268,
-0.12));
#66184=CARTESIAN_POINT('Ctrl Pts',(0.183881198468354,0.431442908347822,
-0.12));
#66185=CARTESIAN_POINT('Ctrl Pts',(0.172580759002838,0.436664729050456,
-0.12));
#66186=CARTESIAN_POINT('Ctrl Pts',(0.166054055780333,0.439680653706417,
-0.12));
#66187=CARTESIAN_POINT('Ctrl Pts',(0.159448793534031,0.442542034058426,
-0.12));
#66188=CARTESIAN_POINT('Ctrl Pts',(0.152787789335078,0.445242616657749,
-0.12));
#66189=CARTESIAN_POINT('Ctrl Pts',(0.129789624052855,0.454566803090074,
-0.12));
#66190=CARTESIAN_POINT('Ctrl Pts',(0.106076488766298,0.462002433444808,
-0.12));
#66191=CARTESIAN_POINT('Ctrl Pts',(0.0819188252479975,0.467568632172314,
-0.12));
#66192=CARTESIAN_POINT('Ctrl Pts',(0.0652486944624254,0.471409618726982,
-0.12));
#66193=CARTESIAN_POINT('Ctrl Pts',(0.0483660449802322,0.474359558588752,
-0.12));
#66194=CARTESIAN_POINT('Ctrl Pts',(0.0313536819883358,0.476412263640607,
-0.12));
#66195=CARTESIAN_POINT('Ctrl Pts',(0.0210620943032514,0.477654042577657,
-0.12));
#66196=CARTESIAN_POINT('Ctrl Pts',(0.0107229630418266,0.478567267564897,
-0.119999999999999));
#66197=CARTESIAN_POINT('Ctrl Pts',(0.000354321129172847,0.479148654832135,
-0.12));
#66198=CARTESIAN_POINT('Ctrl Pts',(-0.00641677334760411,0.479528321537498,
-0.12));
#66199=CARTESIAN_POINT('Ctrl Pts',(-0.0132040195152825,0.479766395875062,
-0.12));
#66200=CARTESIAN_POINT('Ctrl Pts',(-0.0199846559383493,0.479861665078788,
-0.12));
#66201=CARTESIAN_POINT('Ctrl Pts',(-0.0402355271055921,0.48014619358769,
-0.12));
#66202=CARTESIAN_POINT('Ctrl Pts',(-0.0604463821016128,0.479160928462546,
-0.12));
#66203=CARTESIAN_POINT('Ctrl Pts',(-0.0805127730529895,0.476939899349321,
-0.12));
#66204=CARTESIAN_POINT('Ctrl Pts',(-0.0927943658103894,0.475580523109864,
-0.119999999999999));
#66205=CARTESIAN_POINT('Ctrl Pts',(-0.105021940048514,0.473757828575607,
-0.12));
#66206=CARTESIAN_POINT('Ctrl Pts',(-0.117171754670614,0.471475909875768,
-0.12));
#66207=CARTESIAN_POINT('Ctrl Pts',(-0.129239401322921,0.469209423561742,
-0.12));
#66208=CARTESIAN_POINT('Ctrl Pts',(-0.141237375343505,0.466487419270226,
-0.12));
#66209=CARTESIAN_POINT('Ctrl Pts',(-0.153098179736105,0.463324713469219,
-0.12));
#66210=CARTESIAN_POINT('Ctrl Pts',(-0.178118993169746,0.456652866503944,
-0.12));
#66211=CARTESIAN_POINT('Ctrl Pts',(-0.202564229149912,0.448019164461463,
-0.12));
#66212=CARTESIAN_POINT('Ctrl Pts',(-0.226217519016056,0.437461691518522,
-0.12));
#66213=CARTESIAN_POINT('Ctrl Pts',(-0.235396166019609,0.433364869556706,
-0.12));
#66214=CARTESIAN_POINT('Ctrl Pts',(-0.244455472878046,0.428977817680041,
-0.12));
#66215=CARTESIAN_POINT('Ctrl Pts',(-0.253382212491109,0.424300712223195,
-0.12));
#66216=CARTESIAN_POINT('Origin',(0.,0.,0.3066185719505));
#66217=CARTESIAN_POINT('',(-0.25,0.144337567297406,0.288452994616207));
#66218=CARTESIAN_POINT('',(-0.25,-3.42699144208774E-17,0.266123895246948));
#66219=CARTESIAN_POINT('Ctrl Pts',(-0.25,0.144337567297406,0.288452994616208));
#66220=CARTESIAN_POINT('Ctrl Pts',(-0.25,0.0669872981077807,0.266123895246948));
#66221=CARTESIAN_POINT('Ctrl Pts',(-0.25,-3.79236588630711E-17,0.266123895246948));
#66222=CARTESIAN_POINT('',(1.76762539787485E-17,0.288675134594813,0.288452994616207));
#66223=CARTESIAN_POINT('Ctrl Pts',(1.76762539787485E-17,0.288675134594813,
0.288452994616207));
#66224=CARTESIAN_POINT('Ctrl Pts',(-0.125,0.21650635094611,0.246786327949541));
#66225=CARTESIAN_POINT('Ctrl Pts',(-0.25,0.144337567297406,0.288452994616207));
#66226=CARTESIAN_POINT('',(0.25,0.144337567297406,0.288452994616207));
#66227=CARTESIAN_POINT('Ctrl Pts',(0.25,0.144337567297406,0.288452994616207));
#66228=CARTESIAN_POINT('Ctrl Pts',(0.125,0.21650635094611,0.246786327949541));
#66229=CARTESIAN_POINT('Ctrl Pts',(1.76762539787484E-17,0.288675134594813,
0.288452994616207));
#66230=CARTESIAN_POINT('',(0.25,-0.144337567297407,0.288452994616207));
#66231=CARTESIAN_POINT('Ctrl Pts',(0.25,-0.144337567297407,0.288452994616207));
#66232=CARTESIAN_POINT('Ctrl Pts',(0.25,1.66533453693773E-16,0.246786327949541));
#66233=CARTESIAN_POINT('Ctrl Pts',(0.25,0.144337567297406,0.288452994616207));
#66234=CARTESIAN_POINT('',(-5.30287619362453E-17,-0.288675134594813,0.288452994616207));
#66235=CARTESIAN_POINT('Ctrl Pts',(-5.30287619362453E-17,-0.288675134594813,
0.288452994616207));
#66236=CARTESIAN_POINT('Ctrl Pts',(0.125,-0.21650635094611,0.246786327949541));
#66237=CARTESIAN_POINT('Ctrl Pts',(0.25,-0.144337567297407,0.288452994616207));
#66238=CARTESIAN_POINT('',(-0.25,-0.144337567297406,0.288452994616207));
#66239=CARTESIAN_POINT('Ctrl Pts',(-0.25,-0.144337567297406,0.288452994616207));
#66240=CARTESIAN_POINT('Ctrl Pts',(-0.125,-0.21650635094611,0.246786327949541));
#66241=CARTESIAN_POINT('Ctrl Pts',(-5.30287619362453E-17,-0.288675134594813,
0.288452994616207));
#66242=CARTESIAN_POINT('Ctrl Pts',(-0.25,-3.79236588630711E-17,0.266123895246948));
#66243=CARTESIAN_POINT('Ctrl Pts',(-0.25,-0.0669872981077806,0.266123895246948));
#66244=CARTESIAN_POINT('Ctrl Pts',(-0.25,-0.144337567297406,0.288452994616208));
#66245=CARTESIAN_POINT('',(-0.308675134594813,3.78018015557916E-17,0.3));
#66246=CARTESIAN_POINT('',(-0.320138837486628,-3.92057002610754E-17,0.3066185719505));
#66247=CARTESIAN_POINT('Origin',(0.,0.,0.3));
#66248=CARTESIAN_POINT('Origin',(-5.55111512312578E-17,-0.288675134594813,
0.3));
#66249=CARTESIAN_POINT('',(-5.55111512312578E-17,-0.288675134594813,-5.55111512312578E-17));
#66250=CARTESIAN_POINT('',(-5.30287619362453E-17,-0.288675134594813,0.3));
#66251=CARTESIAN_POINT('',(-0.25,-0.144337567297406,-5.55111512312578E-17));
#66252=CARTESIAN_POINT('',(-0.25,-0.144337567297406,-5.55111512312578E-17));
#66253=CARTESIAN_POINT('',(-0.25,-0.144337567297406,0.3));
#66254=CARTESIAN_POINT('Origin',(0.25,-0.144337567297407,0.3));
#66255=CARTESIAN_POINT('',(0.25,-0.144337567297407,-5.55111512312578E-17));
#66256=CARTESIAN_POINT('',(0.25,-0.144337567297407,0.3));
#66257=CARTESIAN_POINT('',(-5.30287619362453E-17,-0.288675134594813,-5.55111512312578E-17));
#66258=CARTESIAN_POINT('Origin',(0.25,0.144337567297406,0.3));
#66259=CARTESIAN_POINT('',(0.25,0.144337567297406,-5.55111512312578E-17));
#66260=CARTESIAN_POINT('',(0.25,0.144337567297406,0.3));
#66261=CARTESIAN_POINT('',(0.25,-0.144337567297407,-5.55111512312578E-17));
#66262=CARTESIAN_POINT('Origin',(0.,0.,-0.0731054258308761));
#66263=CARTESIAN_POINT('',(0.,0.,-0.147210851661752));
#66264=CARTESIAN_POINT('',(-0.243346949651439,2.98014062972907E-17,-5.55111512312578E-17));
#66265=CARTESIAN_POINT('',(-0.1225,-1.50019232895551E-17,-0.0731054258308761));
#66266=CARTESIAN_POINT('Origin',(0.,0.,-5.55111512312578E-17));
#66267=CARTESIAN_POINT('Origin',(0.,0.288675134594813,0.3));
#66268=CARTESIAN_POINT('',(2.77555756156289E-17,0.288675134594813,-5.55111512312578E-17));
#66269=CARTESIAN_POINT('',(1.76762539787485E-17,0.288675134594813,0.3));
#66270=CARTESIAN_POINT('',(0.25,0.144337567297406,-5.55111512312578E-17));
#66271=CARTESIAN_POINT('Origin',(-0.25,0.144337567297406,0.3));
#66272=CARTESIAN_POINT('',(-0.25,0.144337567297406,-5.55111512312578E-17));
#66273=CARTESIAN_POINT('',(-0.25,0.144337567297406,0.3));
#66274=CARTESIAN_POINT('',(1.76762539787485E-17,0.288675134594813,-5.55111512312578E-17));
#66275=CARTESIAN_POINT('Origin',(-0.25,-0.144337567297406,0.3));
#66276=CARTESIAN_POINT('',(-0.25,0.144337567297406,-5.55111512312578E-17));
#66277=CARTESIAN_POINT('Origin',(0.,0.,-5.55111512312578E-17));
#66278=CARTESIAN_POINT('Origin',(0.43,0.,-0.8));
#66279=CARTESIAN_POINT('',(-0.43,-5.26598123633362E-17,-0.8));
#66280=CARTESIAN_POINT('Origin',(0.,0.,-0.8));
#66281=CARTESIAN_POINT('Origin',(0.,0.,-0.765));
#66282=CARTESIAN_POINT('',(-0.465,-5.69460761603519E-17,-0.765));
#66283=CARTESIAN_POINT('Origin',(0.44,0.,-0.12));
#66284=CARTESIAN_POINT('',(-0.44,-5.38844591624835E-17,-0.12));
#66285=CARTESIAN_POINT('Origin',(0.,0.,-0.12));
#66286=CARTESIAN_POINT('Origin',(0.,0.,-0.12));
#66287=CARTESIAN_POINT('Origin',(0.,0.,-0.06));
#66288=CARTESIAN_POINT('',(-0.44,-5.38844591624836E-17,6.93889390390723E-18));
#66289=CARTESIAN_POINT('Origin',(0.,0.,0.));
#66290=CARTESIAN_POINT('',(-0.44,-5.38844591624835E-17,-0.06));
#66291=CARTESIAN_POINT('Origin',(0.68,0.,0.));
#66292=CARTESIAN_POINT('',(-0.68,-8.327598234202E-17,-1.73472347597681E-18));
#66293=CARTESIAN_POINT('Origin',(0.,0.,0.));
#66294=CARTESIAN_POINT('Origin',(0.,0.,0.01));
#66295=CARTESIAN_POINT('',(-0.7,-8.57252759403147E-17,0.02));
#66296=CARTESIAN_POINT('Origin',(0.,0.,0.02));
#66297=CARTESIAN_POINT('',(-0.69,-8.45006291411674E-17,0.01));
#66298=CARTESIAN_POINT('Origin',(0.,0.,0.14));
#66299=CARTESIAN_POINT('',(-0.7,-8.57252759403147E-17,0.26));
#66300=CARTESIAN_POINT('Origin',(0.,0.,0.26));
#66301=CARTESIAN_POINT('',(-0.7,-8.57252759403147E-17,0.14));
#66302=CARTESIAN_POINT('Origin',(0.,0.,0.28));
#66303=CARTESIAN_POINT('',(-0.66,-8.08266887437253E-17,0.3));
#66304=CARTESIAN_POINT('',(-0.68,8.327598234202E-17,0.28));
#66305=CARTESIAN_POINT('Origin',(0.,0.,0.3));
#66306=CARTESIAN_POINT('Origin',(0.,0.,0.3));
#66307=CARTESIAN_POINT('',(0.,0.,0.));
#66308=CARTESIAN_POINT('Origin',(0.,0.,0.005));
#66309=CARTESIAN_POINT('',(-0.51,-6.2456986756515E-17,0.01));
#66310=CARTESIAN_POINT('Origin',(0.,0.,0.01));
#66311=CARTESIAN_POINT('',(-0.52,-6.36816335556624E-17,0.));
#66312=CARTESIAN_POINT('',(-0.515,6.30693101560887E-17,0.005));
#66313=CARTESIAN_POINT('Origin',(0.,0.,0.));
#66314=CARTESIAN_POINT('Origin',(0.69,0.,0.));
#66315=CARTESIAN_POINT('',(-0.69,-8.45006291411674E-17,-2.60208521396521E-17));
#66316=CARTESIAN_POINT('Origin',(0.,0.,0.));
#66317=CARTESIAN_POINT('Origin',(0.,0.,0.005));
#66318=CARTESIAN_POINT('',(-0.7,-8.57252759403147E-17,0.00999999999999998));
#66319=CARTESIAN_POINT('Origin',(0.,0.,0.01));
#66320=CARTESIAN_POINT('',(-0.695,-8.5112952540741E-17,0.005));
#66321=CARTESIAN_POINT('Origin',(0.,0.,0.05));
#66322=CARTESIAN_POINT('',(-0.7,-8.57252759403147E-17,0.09));
#66323=CARTESIAN_POINT('Origin',(0.,0.,0.09));
#66324=CARTESIAN_POINT('',(-0.7,-8.57252759403147E-17,0.05));
#66325=CARTESIAN_POINT('Origin',(0.,0.,0.095));
#66326=CARTESIAN_POINT('',(-0.69,-8.45006291411674E-17,0.1));
#66327=CARTESIAN_POINT('',(-0.695,8.5112952540741E-17,0.095));
#66328=CARTESIAN_POINT('Origin',(0.,0.,0.1));
#66329=CARTESIAN_POINT('Origin',(0.52,0.,0.1));
#66330=CARTESIAN_POINT('',(-0.52,-6.36816335556624E-17,0.1));
#66331=CARTESIAN_POINT('Origin',(0.,0.,0.1));
#66332=CARTESIAN_POINT('Origin',(0.,0.,0.095));
#66333=CARTESIAN_POINT('',(-0.51,-6.2456986756515E-17,0.09));
#66334=CARTESIAN_POINT('Origin',(0.,0.,0.09));
#66335=CARTESIAN_POINT('',(-0.515,-6.30693101560887E-17,0.095));
#66336=CARTESIAN_POINT('Origin',(0.,0.,0.05));
#66337=CARTESIAN_POINT('',(-0.51,-6.2456986756515E-17,0.05));
#66338=CARTESIAN_POINT('',(0.,0.,0.));
#66339=CARTESIAN_POINT('Origin',(0.,0.,-0.36));
#66340=CARTESIAN_POINT('',(-0.55,-6.73555739531044E-17,-0.8));
#66341=CARTESIAN_POINT('Origin',(0.,0.,-0.8));
#66342=CARTESIAN_POINT('',(-0.55,-6.73555739531044E-17,0.08));
#66343=CARTESIAN_POINT('',(-0.55,-6.73555739531044E-17,-0.36));
#66344=CARTESIAN_POINT('Origin',(0.,0.,0.08));
#66345=CARTESIAN_POINT('Origin',(0.66,0.,-0.8));
#66346=CARTESIAN_POINT('',(-0.66,-8.08266887437253E-17,-0.8));
#66347=CARTESIAN_POINT('Origin',(0.,0.,-0.8));
#66348=CARTESIAN_POINT('Origin',(0.,0.,-0.78));
#66349=CARTESIAN_POINT('',(-0.7,-8.57252759403147E-17,-0.76));
#66350=CARTESIAN_POINT('Origin',(0.,0.,-0.76));
#66351=CARTESIAN_POINT('',(-0.68,-8.327598234202E-17,-0.78));
#66352=CARTESIAN_POINT('Origin',(0.,0.,-0.38));
#66353=CARTESIAN_POINT('',(-0.7,-8.57252759403147E-17,0.));
#66354=CARTESIAN_POINT('Origin',(0.,0.,0.));
#66355=CARTESIAN_POINT('',(-0.7,-8.57252759403147E-17,-0.38));
#66356=CARTESIAN_POINT('Origin',(1.85,0.,0.));
#66357=CARTESIAN_POINT('',(-1.85,-2.2655965784226E-16,-2.42861286636753E-17));
#66358=CARTESIAN_POINT('Origin',(0.,0.,0.));
#66359=CARTESIAN_POINT('Origin',(0.,0.,0.025));
#66360=CARTESIAN_POINT('',(-1.9,-2.32682891837997E-16,0.05));
#66361=CARTESIAN_POINT('Origin',(0.,0.,0.05));
#66362=CARTESIAN_POINT('',(-1.875,-2.29621274840129E-16,0.025));
#66363=CARTESIAN_POINT('Origin',(0.,0.,0.13));
#66364=CARTESIAN_POINT('',(-1.9,-2.32682891837997E-16,0.21));
#66365=CARTESIAN_POINT('Origin',(0.,0.,0.21));
#66366=CARTESIAN_POINT('',(-1.9,-2.32682891837997E-16,0.13));
#66367=CARTESIAN_POINT('Origin',(0.,0.,0.23));
#66368=CARTESIAN_POINT('',(-1.86,-2.27784304641408E-16,0.25));
#66369=CARTESIAN_POINT('',(-1.88,2.30233598239702E-16,0.23));
#66370=CARTESIAN_POINT('Origin',(0.,0.,0.25));
#66371=CARTESIAN_POINT('Origin',(0.,0.,0.25));
#66372=CARTESIAN_POINT('Origin',(0.55,0.,0.08));
#66373=CARTESIAN_POINT('',(0.,0.,0.));
#66374=CARTESIAN_POINT('Origin',(0.,0.,0.02));
#66375=CARTESIAN_POINT('',(-2.26,-2.76770176607302E-16,0.05));
#66376=CARTESIAN_POINT('Origin',(0.,0.,0.05));
#66377=CARTESIAN_POINT('',(-2.26,2.76770176607302E-16,0.));
#66378=CARTESIAN_POINT('',(-2.26,-2.76770176607302E-16,0.02));
#66379=CARTESIAN_POINT('Origin',(0.,0.,0.));
#66380=CARTESIAN_POINT('Origin',(0.,0.,0.02));
#66381=CARTESIAN_POINT('',(-2.3,-2.81668763803891E-16,0.));
#66382=CARTESIAN_POINT('Origin',(0.,0.,0.));
#66383=CARTESIAN_POINT('',(-2.3,-2.81668763803891E-16,0.05));
#66384=CARTESIAN_POINT('',(-2.3,-2.81668763803891E-16,0.02));
#66385=CARTESIAN_POINT('Origin',(0.,0.,0.05));
#66386=CARTESIAN_POINT('Origin',(2.26,0.,0.05));
#66387=CARTESIAN_POINT('Origin',(0.,0.,1.615));
#66388=CARTESIAN_POINT('',(-1.68,-2.05740662256755E-16,1.625));
#66389=CARTESIAN_POINT('Origin',(0.,0.,1.625));
#66390=CARTESIAN_POINT('',(-1.68,-2.05740662256755E-16,1.59));
#66391=CARTESIAN_POINT('',(-1.68,-2.05740662256755E-16,1.615));
#66392=CARTESIAN_POINT('Origin',(0.,0.,1.59));
#66393=CARTESIAN_POINT('Origin',(1.72,0.,1.59));
#66394=CARTESIAN_POINT('',(-1.72,-2.10639249453345E-16,1.59));
#66395=CARTESIAN_POINT('Origin',(0.,0.,1.59));
#66396=CARTESIAN_POINT('Origin',(0.,0.,1.615));
#66397=CARTESIAN_POINT('',(-1.72,2.10639249453345E-16,1.625));
#66398=CARTESIAN_POINT('',(-1.72,-2.10639249453345E-16,1.615));
#66399=CARTESIAN_POINT('Origin',(0.,0.,1.625));
#66400=CARTESIAN_POINT('Origin',(2.54,0.,0.));
#66401=CARTESIAN_POINT('',(-2.54,-3.11060286983428E-16,-9.71445146547012E-17));
#66402=CARTESIAN_POINT('Origin',(0.,0.,0.));
#66403=CARTESIAN_POINT('Origin',(1.31,0.,1.625));
#66404=CARTESIAN_POINT('',(-1.95,-2.38806125833734E-16,1.625));
#66405=CARTESIAN_POINT('Origin',(0.,0.,1.625));
#66406=CARTESIAN_POINT('Origin',(0.,0.,0.875));
#66407=CARTESIAN_POINT('',(-1.25,-1.53080849893419E-16,0.185));
#66408=CARTESIAN_POINT('Origin',(0.,0.,0.185));
#66409=CARTESIAN_POINT('',(-1.25,-1.53080849893419E-16,1.565));
#66410=CARTESIAN_POINT('',(-1.25,-1.53080849893419E-16,0.875));
#66411=CARTESIAN_POINT('Origin',(0.,0.,1.565));
#66412=CARTESIAN_POINT('Origin',(0.,0.,0.155));
#66413=CARTESIAN_POINT('',(-1.31,-1.60428730688303E-16,0.125));
#66414=CARTESIAN_POINT('',(-1.28,1.56754790290861E-16,0.155));
#66415=CARTESIAN_POINT('Origin',(0.,0.,0.125));
#66416=CARTESIAN_POINT('Origin',(1.8,0.,0.125));
#66417=CARTESIAN_POINT('',(-1.8,-2.20436423846524E-16,0.125));
#66418=CARTESIAN_POINT('Origin',(0.,0.,0.125));
#66419=CARTESIAN_POINT('Origin',(0.,0.,0.0925));
#66420=CARTESIAN_POINT('',(-2.18,-2.66973002214123E-16,0.06));
#66421=CARTESIAN_POINT('',(-1.99,2.43704713030323E-16,0.0925));
#66422=CARTESIAN_POINT('Origin',(0.,0.,0.0600000000000001));
#66423=CARTESIAN_POINT('Origin',(0.,0.,0.03));
#66424=CARTESIAN_POINT('',(-2.24,-2.74320883009007E-16,1.73472347597681E-17));
#66425=CARTESIAN_POINT('',(-2.21,2.70646942611565E-16,0.03));
#66426=CARTESIAN_POINT('Origin',(0.,0.,0.));
#66427=CARTESIAN_POINT('Origin',(2.54,0.,0.));
#66428=CARTESIAN_POINT('Origin',(0.,0.,0.03));
#66429=CARTESIAN_POINT('',(-2.6,-3.18408167778312E-16,0.0599999999999999));
#66430=CARTESIAN_POINT('Origin',(0.,0.,0.0600000000000001));
#66431=CARTESIAN_POINT('',(-2.57,-3.1473422738087E-16,0.03));
#66432=CARTESIAN_POINT('Origin',(0.,0.,0.65));
#66433=CARTESIAN_POINT('',(-2.6,-3.18408167778312E-16,1.24));
#66434=CARTESIAN_POINT('Origin',(0.,0.,1.24));
#66435=CARTESIAN_POINT('',(-2.6,-3.18408167778312E-16,0.65));
#66436=CARTESIAN_POINT('Origin',(0.,0.,1.27));
#66437=CARTESIAN_POINT('',(-2.54,-3.11060286983428E-16,1.3));
#66438=CARTESIAN_POINT('',(-2.57,3.1473422738087E-16,1.27));
#66439=CARTESIAN_POINT('Origin',(0.,0.,1.3));
#66440=CARTESIAN_POINT('Origin',(1.95,0.,1.3));
#66441=CARTESIAN_POINT('',(-1.95,-2.38806125833734E-16,1.3));
#66442=CARTESIAN_POINT('Origin',(0.,0.,1.3));
#66443=CARTESIAN_POINT('Origin',(0.,0.,1.4625));
#66444=CARTESIAN_POINT('',(-1.95,-2.38806125833734E-16,1.4625));
#66445=CARTESIAN_POINT('Origin',(1.31,0.,1.625));
#66446=CARTESIAN_POINT('',(-1.31,-1.60428730688303E-16,1.625));
#66447=CARTESIAN_POINT('Origin',(0.,0.,1.625));
#66448=CARTESIAN_POINT('Origin',(0.,0.,1.595));
#66449=CARTESIAN_POINT('',(-1.28,-1.56754790290861E-16,1.595));
#66450=CARTESIAN_POINT('',(0.,0.,0.));
#66451=CARTESIAN_POINT('Origin',(0.,0.,0.8));
#66452=CARTESIAN_POINT('',(-2.25,-2.75545529808154E-16,0.0600000000000001));
#66453=CARTESIAN_POINT('Origin',(0.,0.,0.0600000000000001));
#66454=CARTESIAN_POINT('',(-2.25,-2.75545529808154E-16,1.54));
#66455=CARTESIAN_POINT('',(-2.25,-2.75545529808154E-16,0.8));
#66456=CARTESIAN_POINT('Origin',(0.,0.,1.54));
#66457=CARTESIAN_POINT('Origin',(0.,0.,0.03));
#66458=CARTESIAN_POINT('',(-2.31,-2.82893410603039E-16,1.28369537222284E-16));
#66459=CARTESIAN_POINT('',(-2.28,2.79219470205597E-16,0.03));
#66460=CARTESIAN_POINT('Origin',(0.,0.,0.));
#66461=CARTESIAN_POINT('Origin',(2.67,0.,0.));
#66462=CARTESIAN_POINT('',(-2.67,-3.26980695372343E-16,0.));
#66463=CARTESIAN_POINT('Origin',(0.,0.,0.));
#66464=CARTESIAN_POINT('Origin',(0.,0.,0.0249999999999999));
#66465=CARTESIAN_POINT('',(-2.67,-3.26980695372343E-16,0.05));
#66466=CARTESIAN_POINT('Origin',(0.,0.,0.05));
#66467=CARTESIAN_POINT('',(-2.67,-3.26980695372343E-16,0.0249999999999999));
#66468=CARTESIAN_POINT('Origin',(3.18,0.,0.05));
#66469=CARTESIAN_POINT('',(-3.18,-3.89437682128858E-16,0.05));
#66470=CARTESIAN_POINT('Origin',(0.,0.,0.05));
#66471=CARTESIAN_POINT('Origin',(0.,0.,0.0249999999999999));
#66472=CARTESIAN_POINT('',(-3.18,-3.89437682128858E-16,-3.46944695195361E-18));
#66473=CARTESIAN_POINT('Origin',(0.,0.,0.));
#66474=CARTESIAN_POINT('',(-3.18,-3.89437682128858E-16,0.0249999999999999));
#66475=CARTESIAN_POINT('Origin',(3.69,0.,0.));
#66476=CARTESIAN_POINT('',(-3.69,-4.51894668885373E-16,1.28369537222284E-16));
#66477=CARTESIAN_POINT('Origin',(0.,0.,0.));
#66478=CARTESIAN_POINT('Origin',(0.,0.,0.03));
#66479=CARTESIAN_POINT('',(-3.75,-4.59242549680257E-16,0.0600000000000002));
#66480=CARTESIAN_POINT('Origin',(0.,0.,0.0600000000000001));
#66481=CARTESIAN_POINT('',(-3.72,-4.55568609282815E-16,0.03));
#66482=CARTESIAN_POINT('Origin',(0.,0.,0.8));
#66483=CARTESIAN_POINT('',(-3.75,-4.59242549680257E-16,1.54));
#66484=CARTESIAN_POINT('Origin',(0.,0.,1.54));
#66485=CARTESIAN_POINT('',(-3.75,-4.59242549680257E-16,0.8));
#66486=CARTESIAN_POINT('Origin',(0.,0.,1.57));
#66487=CARTESIAN_POINT('',(-3.69,-4.51894668885373E-16,1.6));
#66488=CARTESIAN_POINT('',(-3.72,4.55568609282815E-16,1.57));
#66489=CARTESIAN_POINT('Origin',(0.,0.,1.6));
#66490=CARTESIAN_POINT('Origin',(3.18,0.,1.6));
#66491=CARTESIAN_POINT('',(-3.18,-3.89437682128858E-16,1.6));
#66492=CARTESIAN_POINT('Origin',(0.,0.,1.6));
#66493=CARTESIAN_POINT('Origin',(0.,0.,1.575));
#66494=CARTESIAN_POINT('',(-3.18,-3.89437682128858E-16,1.55));
#66495=CARTESIAN_POINT('Origin',(0.,0.,1.55));
#66496=CARTESIAN_POINT('',(-3.18,-3.89437682128858E-16,1.575));
#66497=CARTESIAN_POINT('Origin',(2.67,0.,1.55));
#66498=CARTESIAN_POINT('',(-2.67,-3.26980695372343E-16,1.55));
#66499=CARTESIAN_POINT('Origin',(0.,0.,1.55));
#66500=CARTESIAN_POINT('Origin',(0.,0.,1.575));
#66501=CARTESIAN_POINT('',(-2.67,-3.26980695372343E-16,1.6));
#66502=CARTESIAN_POINT('Origin',(0.,0.,1.6));
#66503=CARTESIAN_POINT('',(-2.67,-3.26980695372343E-16,1.575));
#66504=CARTESIAN_POINT('Origin',(2.31,0.,1.6));
#66505=CARTESIAN_POINT('',(-2.31,-2.82893410603039E-16,1.6));
#66506=CARTESIAN_POINT('Origin',(0.,0.,1.6));
#66507=CARTESIAN_POINT('Origin',(0.,0.,1.57));
#66508=CARTESIAN_POINT('',(-2.28,-2.79219470205597E-16,1.57));
#66509=CARTESIAN_POINT('',(0.,0.,0.));
#66510=CARTESIAN_POINT('Origin',(3.05,0.,0.));
#66511=CARTESIAN_POINT('',(-3.05,-3.73517273739943E-16,-1.17961196366423E-16));
#66512=CARTESIAN_POINT('Origin',(0.,0.,0.));
#66513=CARTESIAN_POINT('',(-2.6,-3.18408167778312E-16,1.11022302462516E-16));
#66514=CARTESIAN_POINT('Origin',(0.,0.,0.));
#66515=CARTESIAN_POINT('Origin',(0.,0.,0.025));
#66516=CARTESIAN_POINT('',(-3.1,-3.7964050773568E-16,0.0499999999999999));
#66517=CARTESIAN_POINT('Origin',(0.,0.,0.05));
#66518=CARTESIAN_POINT('',(-3.075,-3.76578890737811E-16,0.025));
#66519=CARTESIAN_POINT('Origin',(0.,0.,0.405));
#66520=CARTESIAN_POINT('',(-3.1,-3.79640507735679E-16,0.76));
#66521=CARTESIAN_POINT('Origin',(0.,0.,0.76));
#66522=CARTESIAN_POINT('',(-3.1,-3.79640507735679E-16,0.405));
#66523=CARTESIAN_POINT('Origin',(0.,0.,0.78));
#66524=CARTESIAN_POINT('',(-3.06,-3.7474192053909E-16,0.8));
#66525=CARTESIAN_POINT('',(-3.08,3.77191214137385E-16,0.78));
#66526=CARTESIAN_POINT('Origin',(0.,0.,0.8));
#66527=CARTESIAN_POINT('Origin',(2.65,0.,0.8));
#66528=CARTESIAN_POINT('',(-2.65,-3.24531401774049E-16,0.8));
#66529=CARTESIAN_POINT('Origin',(0.,0.,0.8));
#66530=CARTESIAN_POINT('Origin',(0.,0.,0.725));
#66531=CARTESIAN_POINT('',(-2.65,-3.24531401774049E-16,0.65));
#66532=CARTESIAN_POINT('Origin',(0.,0.,0.65));
#66533=CARTESIAN_POINT('',(-2.65,-3.24531401774049E-16,0.725));
#66534=CARTESIAN_POINT('Origin',(2.4,0.,0.65));
#66535=CARTESIAN_POINT('',(-2.4,-2.93915231795365E-16,0.65));
#66536=CARTESIAN_POINT('Origin',(0.,0.,0.65));
#66537=CARTESIAN_POINT('Origin',(0.,0.,0.565));
#66538=CARTESIAN_POINT('',(-2.25,-2.75545529808154E-16,0.48));
#66539=CARTESIAN_POINT('Origin',(0.,0.,0.48));
#66540=CARTESIAN_POINT('',(-2.325,-2.8473038080176E-16,0.565));
#66541=CARTESIAN_POINT('Origin',(0.,0.,0.42));
#66542=CARTESIAN_POINT('',(-2.25,-2.75545529808154E-16,0.36));
#66543=CARTESIAN_POINT('Origin',(0.,0.,0.36));
#66544=CARTESIAN_POINT('',(-2.25,-2.75545529808154E-16,0.42));
#66545=CARTESIAN_POINT('Origin',(0.,0.,0.3));
#66546=CARTESIAN_POINT('',(-2.45,-3.00038465791102E-16,0.24));
#66547=CARTESIAN_POINT('',(-2.35,2.87791997799628E-16,0.3));
#66548=CARTESIAN_POINT('Origin',(0.,0.,0.24));
#66549=CARTESIAN_POINT('Origin',(0.,0.,0.12));
#66550=CARTESIAN_POINT('',(-2.525,3.09223316784707E-16,0.12));
#66551=CARTESIAN_POINT('',(0.,0.,0.));
#66552=CARTESIAN_POINT('Origin',(-0.56,2.257,0.01));
#66553=CARTESIAN_POINT('',(-0.685,2.257,0.02));
#66554=CARTESIAN_POINT('Origin',(-0.56,2.257,0.02));
#66555=CARTESIAN_POINT('',(-0.705,2.257,0.));
#66556=CARTESIAN_POINT('',(-0.695,2.257,0.01));
#66557=CARTESIAN_POINT('Origin',(-0.56,2.257,0.));
#66558=CARTESIAN_POINT('Origin',(-0.56,2.257,0.));
#66559=CARTESIAN_POINT('',(-0.685,2.257,0.18));
#66560=CARTESIAN_POINT('',(-0.685,2.257,0.));
#66561=CARTESIAN_POINT('Origin',(-0.56,2.257,0.18));
#66562=CARTESIAN_POINT('Origin',(0.,0.,0.));
#66563=CARTESIAN_POINT('',(0.23,2.39869342459544,0.));
#66564=CARTESIAN_POINT('',(0.23,2.74036493920062,0.));
#66565=CARTESIAN_POINT('',(0.23,0.9,0.));
#66566=CARTESIAN_POINT('',(-0.23,2.74036493920062,0.));
#66567=CARTESIAN_POINT('Origin',(0.,0.,0.));
#66568=CARTESIAN_POINT('',(-0.23,2.39869342459544,0.));
#66569=CARTESIAN_POINT('',(-0.23,1.45,0.));
#66570=CARTESIAN_POINT('',(-0.291967181462275,2.39175313794759,0.));
#66571=CARTESIAN_POINT('Origin',(0.,0.065,0.));
#66572=CARTESIAN_POINT('',(-0.859822464806605,2.24668062030488,0.));
#66573=CARTESIAN_POINT('Origin',(-0.56,2.257,0.));
#66574=CARTESIAN_POINT('',(0.859822464806605,2.24668062030488,0.));
#66575=CARTESIAN_POINT('Origin',(0.,0.065,0.));
#66576=CARTESIAN_POINT('',(0.291967181462275,2.39175313794759,0.));
#66577=CARTESIAN_POINT('Origin',(0.56,2.257,0.));
#66578=CARTESIAN_POINT('Origin',(0.,0.065,0.));
#66579=CARTESIAN_POINT('',(0.415,2.257,0.));
#66580=CARTESIAN_POINT('Origin',(0.56,2.257,0.));
#66581=CARTESIAN_POINT('Origin',(-0.56,2.257,0.19));
#66582=CARTESIAN_POINT('',(-0.705,2.257,0.2));
#66583=CARTESIAN_POINT('',(-0.695,2.257,0.19));
#66584=CARTESIAN_POINT('Origin',(-0.56,2.257,0.2));
#66585=CARTESIAN_POINT('Origin',(0.,0.,0.2));
#66586=CARTESIAN_POINT('',(0.23,2.74036493920062,0.2));
#66587=CARTESIAN_POINT('',(0.23,2.39869342459544,0.2));
#66588=CARTESIAN_POINT('',(0.23,0.9,0.2));
#66589=CARTESIAN_POINT('',(0.291967181462275,2.39175313794759,0.2));
#66590=CARTESIAN_POINT('Origin',(0.,0.065,0.2));
#66591=CARTESIAN_POINT('',(0.859822464806605,2.24668062030488,0.2));
#66592=CARTESIAN_POINT('Origin',(0.56,2.257,0.2));
#66593=CARTESIAN_POINT('',(-0.859822464806605,2.24668062030488,0.2));
#66594=CARTESIAN_POINT('Origin',(0.,0.065,0.2));
#66595=CARTESIAN_POINT('',(-0.291967181462275,2.39175313794759,0.2));
#66596=CARTESIAN_POINT('Origin',(-0.56,2.257,0.2));
#66597=CARTESIAN_POINT('',(-0.23,2.39869342459544,0.2));
#66598=CARTESIAN_POINT('Origin',(0.,0.065,0.2));
#66599=CARTESIAN_POINT('',(-0.23,2.74036493920062,0.2));
#66600=CARTESIAN_POINT('',(-0.23,1.45,0.2));
#66601=CARTESIAN_POINT('Origin',(0.,0.,0.2));
#66602=CARTESIAN_POINT('',(0.415,2.257,0.2));
#66603=CARTESIAN_POINT('Origin',(0.56,2.257,0.2));
#66604=CARTESIAN_POINT('Origin',(0.56,2.257,0.01));
#66605=CARTESIAN_POINT('',(0.435,2.257,0.02));
#66606=CARTESIAN_POINT('Origin',(0.56,2.257,0.02));
#66607=CARTESIAN_POINT('',(0.425,2.257,0.01));
#66608=CARTESIAN_POINT('Origin',(0.56,2.257,0.));
#66609=CARTESIAN_POINT('',(0.435,2.257,0.18));
#66610=CARTESIAN_POINT('',(0.435,2.257,0.));
#66611=CARTESIAN_POINT('Origin',(0.56,2.257,0.18));
#66612=CARTESIAN_POINT('Origin',(0.56,2.257,0.19));
#66613=CARTESIAN_POINT('',(0.425,2.257,0.19));
#66614=CARTESIAN_POINT('Origin',(-0.23,2.9,0.));
#66615=CARTESIAN_POINT('',(-0.23,2.39869342459544,0.));
#66616=CARTESIAN_POINT('',(-0.23,2.74036493920062,0.));
#66617=CARTESIAN_POINT('Origin',(0.23,1.8,0.));
#66618=CARTESIAN_POINT('',(0.23,2.39869342459544,0.));
#66619=CARTESIAN_POINT('',(0.23,2.74036493920062,0.));
#66620=CARTESIAN_POINT('Origin',(0.,0.065,0.));
#66621=CARTESIAN_POINT('',(-0.291967181462275,2.39175313794759,0.));
#66622=CARTESIAN_POINT('Origin',(-0.56,2.257,0.));
#66623=CARTESIAN_POINT('',(-0.859822464806605,2.24668062030488,0.));
#66624=CARTESIAN_POINT('Origin',(0.,0.065,0.));
#66625=CARTESIAN_POINT('',(0.859822464806605,2.24668062030488,0.));
#66626=CARTESIAN_POINT('Origin',(0.56,2.257,0.));
#66627=CARTESIAN_POINT('',(0.291967181462275,2.39175313794759,0.));
#66628=CARTESIAN_POINT('Origin',(0.,0.065,0.));
#66629=CARTESIAN_POINT('Origin',(0.,0.,0.));
#66630=CARTESIAN_POINT('',(0.,0.,0.));
#66631=CARTESIAN_POINT('Origin',(0.,0.,-2.1456589891905));
#66632=CARTESIAN_POINT('',(-0.0419392741328075,0.233437524640348,-1.89811014643447));
#66633=CARTESIAN_POINT('',(-0.0419392741328074,0.233437524640348,-1.91783866303197));
#66634=CARTESIAN_POINT('',(-0.0419392741328076,0.233437524640348,-2.1456589891905));
#66635=CARTESIAN_POINT('',(-0.137697683872004,-0.193109628142373,-1.9607937088529));
#66636=CARTESIAN_POINT('Ctrl Pts',(-0.137697683872004,-0.193109628142373,
-1.9607937088529));
#66637=CARTESIAN_POINT('Ctrl Pts',(-0.12637047603803,-0.201186544340074,
-1.95985501417045));
#66638=CARTESIAN_POINT('Ctrl Pts',(-0.114289949077831,-0.208291945347675,
-1.95891631948801));
#66639=CARTESIAN_POINT('Ctrl Pts',(-0.101649101270924,-0.214288219078449,
-1.95797762480556));
#66640=CARTESIAN_POINT('Ctrl Pts',(-0.0890324468673995,-0.220273016500722,
-1.95704072669716));
#66641=CARTESIAN_POINT('Ctrl Pts',(-0.075858331601906,-0.22515247421464,
-1.95610382858876));
#66642=CARTESIAN_POINT('Ctrl Pts',(-0.0623457780960344,-0.228833967274529,
-1.95516693048035));
#66643=CARTESIAN_POINT('Ctrl Pts',(-0.0488341882992543,-0.232515197772028,
-1.9542300991911));
#66644=CARTESIAN_POINT('Ctrl Pts',(-0.0349850177357809,-0.234998368896974,
-1.95329326790184));
#66645=CARTESIAN_POINT('Ctrl Pts',(-0.0210329134916387,-0.236240549387808,
-1.95235643661258));
#66646=CARTESIAN_POINT('Ctrl Pts',(-0.00708055823376012,-0.237482752226838,
-1.95141958846869));
#66647=CARTESIAN_POINT('Ctrl Pts',(0.00697388352572853,-0.237483875340244,
-1.9504827403248));
#66648=CARTESIAN_POINT('Ctrl Pts',(0.0208925910903226,-0.23625300053657,
-1.94954589218092));
#66649=CARTESIAN_POINT('Ctrl Pts',(0.0348412441386924,-0.235019477560191,
-1.94860702844968));
#66650=CARTESIAN_POINT('Ctrl Pts',(0.0486527402342993,-0.232548812747818,
-1.94766816471844));
#66651=CARTESIAN_POINT('Ctrl Pts',(0.0620972961073801,-0.228901521273128,
-1.9467293009872));
#66652=CARTESIAN_POINT('Ctrl Pts',(0.0652366861336961,-0.228049855320991,
-1.94651007028433));
#66653=CARTESIAN_POINT('Ctrl Pts',(0.068356140207546,-0.227134246202191,
-1.94629083958145));
#66654=CARTESIAN_POINT('Ctrl Pts',(0.0714528817785064,-0.226155845183243,
-1.94607160887858));
#66655=CARTESIAN_POINT('Ctrl Pts',(0.0848650768915338,-0.221918324852849,
-1.94512210602392));
#66656=CARTESIAN_POINT('Ctrl Pts',(0.0979424730591469,-0.216469828743788,
-1.94417260316927));
#66657=CARTESIAN_POINT('Ctrl Pts',(0.11045530094533,-0.209884747225892,
-1.94322310031462));
#66658=CARTESIAN_POINT('Ctrl Pts',(0.122943524780795,-0.203312613994437,
-1.9422754644733));
#66659=CARTESIAN_POINT('Ctrl Pts',(0.134868624317464,-0.195608655287244,
-1.94132782863197));
#66660=CARTESIAN_POINT('Ctrl Pts',(0.146021360452479,-0.186895005060615,
-1.94038019279065));
#66661=CARTESIAN_POINT('Ctrl Pts',(0.157172938080486,-0.178182259977326,
-1.9394326553864));
#66662=CARTESIAN_POINT('Ctrl Pts',(0.167551628355181,-0.168460504828884,
-1.93848511798215));
#66663=CARTESIAN_POINT('Ctrl Pts',(0.176978438280712,-0.157894309614755,
-1.9375375805779));
#66664=CARTESIAN_POINT('Ctrl Pts',(0.186403995536247,-0.14732951847643,
-1.93659016908599));
#66665=CARTESIAN_POINT('Ctrl Pts',(0.194877384600008,-0.135921143690584,
-1.93564275759408));
#66666=CARTESIAN_POINT('Ctrl Pts',(0.202259088856076,-0.123867839248571,
-1.93469534610217));
#66667=CARTESIAN_POINT('Ctrl Pts',(0.209658159563989,-0.111786177787108,
-1.93374570569734));
#66668=CARTESIAN_POINT('Ctrl Pts',(0.215960021336509,-0.0990572914205307,
-1.9327960652925));
#66669=CARTESIAN_POINT('Ctrl Pts',(0.221070752954074,-0.0859051966607303,
-1.93184642488766));
#66670=CARTESIAN_POINT('Ctrl Pts',(0.224046407741954,-0.0782475662721294,
-1.93129350952664));
#66671=CARTESIAN_POINT('Ctrl Pts',(0.226619178308375,-0.0704468605388091,
-1.93074059416561));
#66672=CARTESIAN_POINT('Ctrl Pts',(0.228778383837622,-0.0625494341592766,
-1.93018767880459));
#66673=CARTESIAN_POINT('Ctrl Pts',(0.232474781461577,-0.0490296336079843,
-1.92924112925243));
#66674=CARTESIAN_POINT('Ctrl Pts',(0.234981370144682,-0.0351342032452116,
-1.92829457970026));
#66675=CARTESIAN_POINT('Ctrl Pts',(0.236235029515445,-0.0210948205689673,
-1.9273480301481));
#66676=CARTESIAN_POINT('Ctrl Pts',(0.237486110216362,-0.00708431569924813,
-1.92640342756722));
#66677=CARTESIAN_POINT('Ctrl Pts',(0.237489230340424,0.00706873551438706,
-1.92545882498633));
#66678=CARTESIAN_POINT('Ctrl Pts',(0.236232450820277,0.0211236787621226,
-1.92451422240545));
#66679=CARTESIAN_POINT('Ctrl Pts',(0.234975900744799,0.0351760560611391,
-1.92356979227647));
#66680=CARTESIAN_POINT('Ctrl Pts',(0.232459931015672,0.0491295242772827,
-1.92262536214749));
#66681=CARTESIAN_POINT('Ctrl Pts',(0.228724667077634,0.0627455759016155,
-1.92168093201852));
#66682=CARTESIAN_POINT('Ctrl Pts',(0.224990083796739,0.0763591463457809,
-1.92073667398798));
#66683=CARTESIAN_POINT('Ctrl Pts',(0.220036886274952,0.0896346191670999,
-1.91979241595745));
#66684=CARTESIAN_POINT('Ctrl Pts',(0.213955295967831,0.102347994373695,
-1.91884815792692));
#66685=CARTESIAN_POINT('Ctrl Pts',(0.207859417454863,0.115091238629796,
-1.91790168143832));
#66686=CARTESIAN_POINT('Ctrl Pts',(0.200630255929949,0.127269011044877,
-1.91695520494971));
#66687=CARTESIAN_POINT('Ctrl Pts',(0.192404128186777,0.138681765498159,
-1.91600872846111));
#66688=CARTESIAN_POINT('Ctrl Pts',(0.187464621419128,0.145534731999475,
-1.91544040188427));
#66689=CARTESIAN_POINT('Ctrl Pts',(0.182166502845806,0.152112423109991,
-1.91487207530744));
#66690=CARTESIAN_POINT('Ctrl Pts',(0.176546005423108,0.158377677070173,
-1.9143037487306));
#66691=CARTESIAN_POINT('Ctrl Pts',(0.167169653179186,0.168829639523006,
-1.9133556422245));
#66692=CARTESIAN_POINT('Ctrl Pts',(0.156830382561657,0.17848120087317,-1.9124075357184));
#66693=CARTESIAN_POINT('Ctrl Pts',(0.145689671968511,0.187153680451942,
-1.9114594292123));
#66694=CARTESIAN_POINT('Ctrl Pts',(0.13457150480671,0.195808611109904,-1.91051324121702));
#66695=CARTESIAN_POINT('Ctrl Pts',(0.12265572453643,0.203487829808672,-1.90956705322175));
#66696=CARTESIAN_POINT('Ctrl Pts',(0.110138977720994,0.210050913379529,
-1.90862086522648));
#66697=CARTESIAN_POINT('Ctrl Pts',(0.097624262151212,0.216612931878512,
-1.90767483078071));
#66698=CARTESIAN_POINT('Ctrl Pts',(0.0845094877785817,0.222058744272142,
-1.90672879633494));
#66699=CARTESIAN_POINT('Ctrl Pts',(0.0710176130865216,0.226292905890779,
-1.90578276188917));
#66700=CARTESIAN_POINT('Ctrl Pts',(0.0575280064598183,0.230526355721359,
-1.90483688647749));
#66701=CARTESIAN_POINT('Ctrl Pts',(0.0436622270574184,0.233548326720256,
-1.90389101106581));
#66702=CARTESIAN_POINT('Ctrl Pts',(0.0296581196528709,0.235313358234623,
-1.90294513565413));
#66703=CARTESIAN_POINT('Ctrl Pts',(0.0156213338132154,0.237082508431184,
-1.90199705305227));
#66704=CARTESIAN_POINT('Ctrl Pts',(0.00144641050224148,0.237588802978478,
-1.90104897045041));
#66705=CARTESIAN_POINT('Ctrl Pts',(-0.0126244187202315,0.236838773592873,
-1.90010088784855));
#66706=CARTESIAN_POINT('Ctrl Pts',(-0.0209408662058052,0.236395474914494,
-1.89954053145124));
#66707=CARTESIAN_POINT('Ctrl Pts',(-0.0292209623871544,0.235514308440667,
-1.89898017505393));
#66708=CARTESIAN_POINT('Ctrl Pts',(-0.0374160476123589,0.234205081085082,
-1.89841981865661));
#66709=CARTESIAN_POINT('Ctrl Pts',(-0.0389256762846854,0.233963906393145,
-1.89831659458256));
#66710=CARTESIAN_POINT('Ctrl Pts',(-0.0404335213778545,0.233708047460805,
-1.89821337050852));
#66711=CARTESIAN_POINT('Ctrl Pts',(-0.0419392741328075,0.233437524640348,
-1.89811014643447));
#66712=CARTESIAN_POINT('',(0.137702479013104,-0.193106208855763,-1.9608));
#66713=CARTESIAN_POINT('Origin',(0.,0.,-1.9608));
#66714=CARTESIAN_POINT('Ctrl Pts',(0.137702479013104,-0.193106208855763,
-1.9608));
#66715=CARTESIAN_POINT('Ctrl Pts',(0.149477310386104,-0.184709671636007,
-1.95982953787546));
#66716=CARTESIAN_POINT('Ctrl Pts',(0.160496540954779,-0.175221999758771,
-1.95885907575091));
#66717=CARTESIAN_POINT('Ctrl Pts',(0.170563783261087,-0.164802841191118,
-1.95788861362637));
#66718=CARTESIAN_POINT('Ctrl Pts',(0.180623617019241,-0.154391350149052,
-1.95691886567112));
#66719=CARTESIAN_POINT('Ctrl Pts',(0.189732304539067,-0.143050282060555,
-1.95594911771588));
#66720=CARTESIAN_POINT('Ctrl Pts',(0.197730174513417,-0.130976176123346,
-1.95497936976064));
#66721=CARTESIAN_POINT('Ctrl Pts',(0.205737403722816,-0.118887940874727,
-1.95400848699086));
#66722=CARTESIAN_POINT('Ctrl Pts',(0.212630784608857,-0.106065601707679,
-1.95303760422109));
#66723=CARTESIAN_POINT('Ctrl Pts',(0.21829392961994,-0.0927347880575818,
-1.95206672145131));
#66724=CARTESIAN_POINT('Ctrl Pts',(0.223960335744276,-0.0793962978791635,
-1.95109527960021));
#66725=CARTESIAN_POINT('Ctrl Pts',(0.22839483161772,-0.0655494838953948,
-1.9501238377491));
#66726=CARTESIAN_POINT('Ctrl Pts',(0.231529867604011,-0.0514383226035734,
-1.94915239589799));
#66727=CARTESIAN_POINT('Ctrl Pts',(0.23467367162705,-0.0372876953594267,
-1.9481782371282));
#66728=CARTESIAN_POINT('Ctrl Pts',(0.23651064375352,-0.0228720170116576,
-1.94720407835841));
#66729=CARTESIAN_POINT('Ctrl Pts',(0.237024640569509,-0.00844395570185955,
-1.94622991958861));
#66730=CARTESIAN_POINT('Ctrl Pts',(0.23725571670898,-0.00195757173252825,
-1.94579196970108));
#66731=CARTESIAN_POINT('Ctrl Pts',(0.237220110839713,0.00453129736859094,
-1.94535401981354));
#66732=CARTESIAN_POINT('Ctrl Pts',(0.236919781413861,0.0109998999908311,
-1.94491606992601));
#66733=CARTESIAN_POINT('Ctrl Pts',(0.236276456812775,0.0248560554099354,
-1.94397795360293));
#66734=CARTESIAN_POINT('Ctrl Pts',(0.23441062882172,0.0387123928421089,
-1.94303983727984));
#66735=CARTESIAN_POINT('Ctrl Pts',(0.231329315697138,0.0523328608437726,
-1.94210172095676));
#66736=CARTESIAN_POINT('Ctrl Pts',(0.228255014392539,0.0659223341799007,
-1.94116573940626));
#66737=CARTESIAN_POINT('Ctrl Pts',(0.223970815010453,0.0792761621068477,
-1.94022975785576));
#66738=CARTESIAN_POINT('Ctrl Pts',(0.218535299951983,0.0921645447007527,
-1.93929377630527));
#66739=CARTESIAN_POINT('Ctrl Pts',(0.213101728896389,0.105048317786161,
-1.938358129507));
#66740=CARTESIAN_POINT('Ctrl Pts',(0.206517933627718,0.117466167693581,
-1.93742248270874));
#66741=CARTESIAN_POINT('Ctrl Pts',(0.198891613031466,0.129205676697045,
-1.93648683591048));
#66742=CARTESIAN_POINT('Ctrl Pts',(0.191267587961356,0.140941652102693,
-1.93555147074235));
#66743=CARTESIAN_POINT('Ctrl Pts',(0.18260213724279,0.151998982507965,-1.93461610557422));
#66744=CARTESIAN_POINT('Ctrl Pts',(0.173046444657011,0.162194046181011,
-1.9336807404061));
#66745=CARTESIAN_POINT('Ctrl Pts',(0.163468116365151,0.172413260114513,
-1.93274315952719));
#66746=CARTESIAN_POINT('Ctrl Pts',(0.152995954040751,0.181765534824852,
-1.93180557864829));
#66747=CARTESIAN_POINT('Ctrl Pts',(0.141817720437167,0.190104483889796,
-1.93086799776939));
#66748=CARTESIAN_POINT('Ctrl Pts',(0.134521763674017,0.195547259017382,
-1.93025604513027));
#66749=CARTESIAN_POINT('Ctrl Pts',(0.126925728673847,0.20055917307947,-1.92964409249114));
#66750=CARTESIAN_POINT('Ctrl Pts',(0.119087822964908,0.205109899923136,
-1.92903213985202));
#66751=CARTESIAN_POINT('Ctrl Pts',(0.106929239153337,0.212169233855818,
-1.92808284577682));
#66752=CARTESIAN_POINT('Ctrl Pts',(0.0941004426223774,0.218167136659545,
-1.92713355170162));
#66753=CARTESIAN_POINT('Ctrl Pts',(0.0808107590087802,0.222983411610426,
-1.92618425762642));
#66754=CARTESIAN_POINT('Ctrl Pts',(0.0675474741095219,0.227790119481285,
-1.92523684923517));
#66755=CARTESIAN_POINT('Ctrl Pts',(0.0538258694776703,0.231419511629482,
-1.92428944084392));
#66756=CARTESIAN_POINT('Ctrl Pts',(0.0398769046725999,0.233798659317654,
-1.92334203245268));
#66757=CARTESIAN_POINT('Ctrl Pts',(0.0259288860147947,0.236177645630117,
-1.92239468832339));
#66758=CARTESIAN_POINT('Ctrl Pts',(0.0117543479097061,0.237306364567924,
-1.9214473441941));
#66759=CARTESIAN_POINT('Ctrl Pts',(-0.0024045406954071,0.237162810763079,
-1.92050000006482));
#66760=CARTESIAN_POINT('Ctrl Pts',(-0.0156632124648629,0.237028384055392,
-1.91961288772054));
#66761=CARTESIAN_POINT('Ctrl Pts',(-0.0289075058911183,0.235778805895645,
-1.91872577537625));
#66762=CARTESIAN_POINT('Ctrl Pts',(-0.0419392741328073,0.233437524640348,
-1.91783866303197));
#66763=CARTESIAN_POINT('Origin',(0.,0.,-2.1456589891905));
#66764=CARTESIAN_POINT('',(-0.0419392500630468,0.233437528964709,-1.79799080372057));
#66765=CARTESIAN_POINT('',(-0.0419392741328097,0.233437524640348,-1.81760526556689));
#66766=CARTESIAN_POINT('',(-0.0419392741328076,0.233437524640348,-2.1456589891905));
#66767=CARTESIAN_POINT('',(-0.237174975484837,0.000107836760217876,-1.87594101081465));
#66768=CARTESIAN_POINT('Ctrl Pts',(-0.0419392500630493,0.233437528964708,
-1.79799080372057));
#66769=CARTESIAN_POINT('Ctrl Pts',(-0.0282675868112729,0.235893771996568,
-1.79898926705185));
#66770=CARTESIAN_POINT('Ctrl Pts',(-0.014401555316779,0.237145080218823,
-1.80001249030746));
#66771=CARTESIAN_POINT('Ctrl Pts',(0.00391717657812939,0.237183812422573,
-1.80134089095945));
#66772=CARTESIAN_POINT('Ctrl Pts',(0.00833543515462887,0.237069671857752,
-1.80165929127765));
#66773=CARTESIAN_POINT('Ctrl Pts',(0.017186016719489,0.236593265928485,
-1.80229025128174));
#66774=CARTESIAN_POINT('Ctrl Pts',(0.0216166837631987,0.236229671704668,
-1.80260265014077));
#66775=CARTESIAN_POINT('Ctrl Pts',(0.0272637718400154,0.235606018732023,
-1.80299429325227));
#66776=CARTESIAN_POINT('Ctrl Pts',(0.0284916570249254,0.235460686664155,
-1.80307905398002));
#66777=CARTESIAN_POINT('Ctrl Pts',(0.0304442378653119,0.235214081797173,
-1.80321314895662));
#66778=CARTESIAN_POINT('Ctrl Pts',(0.031169677629494,0.235119048841648,
-1.80326281685126));
#66779=CARTESIAN_POINT('Ctrl Pts',(0.0325548229261261,0.23493107062727,
-1.80335734618238));
#66780=CARTESIAN_POINT('Ctrl Pts',(0.0332145861601052,0.234838701492014,
-1.80340223711278));
#66781=CARTESIAN_POINT('Ctrl Pts',(0.0347872034170434,0.234611769703897,
-1.80350893326721));
#66782=CARTESIAN_POINT('Ctrl Pts',(0.0356996890314834,0.2344746559423,-1.80357059645435));
#66783=CARTESIAN_POINT('Ctrl Pts',(0.0388065076444369,0.233989255823198,
-1.80377978085021));
#66784=CARTESIAN_POINT('Ctrl Pts',(0.0409968157775473,0.233615450798555,
-1.80392595243139));
#66785=CARTESIAN_POINT('Ctrl Pts',(0.046352149475674,0.232623850032356,
-1.80428086177076));
#66786=CARTESIAN_POINT('Ctrl Pts',(0.0495105184518829,0.231972170865867,
-1.80448803692743));
#66787=CARTESIAN_POINT('Ctrl Pts',(0.0626142015597526,0.228988591234596,
-1.80534233722432));
#66788=CARTESIAN_POINT('Ctrl Pts',(0.0724175237677254,0.226079736434471,
-1.80596911731119));
#66789=CARTESIAN_POINT('Ctrl Pts',(0.0978266212221733,0.216717103424094,
-1.80762908603495));
#66790=CARTESIAN_POINT('Ctrl Pts',(0.112981015399952,0.209216532809259,
-1.80865976223155));
#66791=CARTESIAN_POINT('Ctrl Pts',(0.129881573591196,0.19847611239877,-1.80995397728956));
#66792=CARTESIAN_POINT('Ctrl Pts',(0.13251746723751,0.196725976137932,-1.8101602426783));
#66793=CARTESIAN_POINT('Ctrl Pts',(0.136355666874198,0.194065407908069,
-1.81046763045958));
#66794=CARTESIAN_POINT('Ctrl Pts',(0.137585635139072,0.193195350002201,
-1.81056722944285));
#66795=CARTESIAN_POINT('Ctrl Pts',(0.139758736546854,0.191626859475513,
-1.8107452077354));
#66796=CARTESIAN_POINT('Ctrl Pts',(0.140705140555662,0.190933027656012,
-1.81082340805523));
#66797=CARTESIAN_POINT('Ctrl Pts',(0.142690710160618,0.189454578399914,
-1.81098895762521));
#66798=CARTESIAN_POINT('Ctrl Pts',(0.143728638087296,0.188668371803563,
-1.81107636729729));
#66799=CARTESIAN_POINT('Ctrl Pts',(0.146474537996454,0.186552606848993,
-1.81130998054245));
#66800=CARTESIAN_POINT('Ctrl Pts',(0.148170838271243,0.185208173543935,
-1.8114567689564));
#66801=CARTESIAN_POINT('Ctrl Pts',(0.156680807594783,0.178271704161976,
-1.81220606159333));
#66802=CARTESIAN_POINT('Ctrl Pts',(0.163196550835474,0.172326804781988,
-1.81282275249359));
#66803=CARTESIAN_POINT('Ctrl Pts',(0.17716749081423,0.158075495315829,-1.81424668472668));
#66804=CARTESIAN_POINT('Ctrl Pts',(0.184398047034072,0.149577761665817,
-1.81505977316738));
#66805=CARTESIAN_POINT('Ctrl Pts',(0.19821885125347,0.130802849606491,-1.81676238936714));
#66806=CARTESIAN_POINT('Ctrl Pts',(0.204669421318344,0.120459891476853,
-1.81764961698169));
#66807=CARTESIAN_POINT('Ctrl Pts',(0.211255574220567,0.107830200586463,
-1.81864318672013));
#66808=CARTESIAN_POINT('Ctrl Pts',(0.212189139154548,0.105981317936876,
-1.81878648036838));
#66809=CARTESIAN_POINT('Ctrl Pts',(0.213464135592412,0.103371840901509,
-1.81898547749613));
#66810=CARTESIAN_POINT('Ctrl Pts',(0.213825927605133,0.102621378922579,
-1.81904233525338));
#66811=CARTESIAN_POINT('Ctrl Pts',(0.214472400358779,0.101262143515778,
-1.81914462488984));
#66812=CARTESIAN_POINT('Ctrl Pts',(0.214758461757127,0.100654038017529,
-1.81919013972173));
#66813=CARTESIAN_POINT('Ctrl Pts',(0.215339168592224,0.0994058328464185,
-1.81928304445913));
#66814=CARTESIAN_POINT('Ctrl Pts',(0.215633552271421,0.0987656230764895,
-1.81933041843311));
#66815=CARTESIAN_POINT('Ctrl Pts',(0.216386146042179,0.0971095174691044,
-1.81945227614837));
#66816=CARTESIAN_POINT('Ctrl Pts',(0.216840063503095,0.096091672710009,
-1.81952650281159));
#66817=CARTESIAN_POINT('Ctrl Pts',(0.218755428779171,0.0917140479537584,
-1.81984304986639));
#66818=CARTESIAN_POINT('Ctrl Pts',(0.22014618113985,0.0883236476538218,
-1.82008144570525));
#66819=CARTESIAN_POINT('Ctrl Pts',(0.223800386771826,0.0787920562297992,
-1.82073665232227));
#66820=CARTESIAN_POINT('Ctrl Pts',(0.225889170826399,0.0725871625319044,
-1.82114619480944));
#66821=CARTESIAN_POINT('Ctrl Pts',(0.228782327710164,0.0626506272602354,
-1.82178690085556));
#66822=CARTESIAN_POINT('Ctrl Pts',(0.229757858455704,0.0589727228294529,
-1.82202084874544));
#66823=CARTESIAN_POINT('Ctrl Pts',(0.234889673513442,0.0375585172278741,
-1.82337208320385));
#66824=CARTESIAN_POINT('Ctrl Pts',(0.237079574940827,0.0194162524769529,
-1.82447973176487));
#66825=CARTESIAN_POINT('Ctrl Pts',(0.237187590033331,-0.00188090725826167,
-1.82585714436869));
#66826=CARTESIAN_POINT('Ctrl Pts',(0.237143083508221,-0.0049645937470575,
-1.82605829387516));
#66827=CARTESIAN_POINT('Ctrl Pts',(0.236987875577185,-0.00953684228642896,
-1.8263594853224));
#66828=CARTESIAN_POINT('Ctrl Pts',(0.236923227625293,-0.0110267208193047,
-1.82645809244125));
#66829=CARTESIAN_POINT('Ctrl Pts',(0.236782711563533,-0.0136857833778987,
-1.82663495366969));
#66830=CARTESIAN_POINT('Ctrl Pts',(0.236712221404468,-0.0148552117198704,
-1.82671303692317));
#66831=CARTESIAN_POINT('Ctrl Pts',(0.236544547503257,-0.0173313138987364,
-1.8268790285168));
#66832=CARTESIAN_POINT('Ctrl Pts',(0.236445194116183,-0.0186377964005856,
-1.82696700240654));
#66833=CARTESIAN_POINT('Ctrl Pts',(0.23614979072489,-0.0221384174290009,
-1.82720380306762));
#66834=CARTESIAN_POINT('Ctrl Pts',(0.235933992795775,-0.0243307142868619,
-1.82735324346547));
#66835=CARTESIAN_POINT('Ctrl Pts',(0.234635697439217,-0.0358690467146313,
-1.82814602460467));
#66836=CARTESIAN_POINT('Ctrl Pts',(0.233028462332726,-0.0451463579057098,
-1.82880564188899));
#66837=CARTESIAN_POINT('Ctrl Pts',(0.228443559405747,-0.0646396449436121,
-1.83023822411047));
#66838=CARTESIAN_POINT('Ctrl Pts',(0.225320948591251,-0.0748009698632225,
-1.83101339990323));
#66839=CARTESIAN_POINT('Ctrl Pts',(0.217236987229194,-0.0959396106555246,
-1.83266618307894));
#66840=CARTESIAN_POINT('Ctrl Pts',(0.212098743571396,-0.106819933349215,
-1.83354162760002));
#66841=CARTESIAN_POINT('Ctrl Pts',(0.205128663422169,-0.119073685059738,
-1.83452510304342));
#66842=CARTESIAN_POINT('Ctrl Pts',(0.204075981014947,-0.120868961040342,
-1.83466909723506));
#66843=CARTESIAN_POINT('Ctrl Pts',(0.202568099176248,-0.123364673191028,
-1.83486889655289));
#66844=CARTESIAN_POINT('Ctrl Pts',(0.20213265977402,-0.124076852397924,
-1.83492586804764));
#66845=CARTESIAN_POINT('Ctrl Pts',(0.201339694745126,-0.125358526016224,
-1.83502829738034));
#66846=CARTESIAN_POINT('Ctrl Pts',(0.200983490731757,-0.125928826003704,
-1.83507383892603));
#66847=CARTESIAN_POINT('Ctrl Pts',(0.200249392987781,-0.127093102923555,
-1.83516672708757));
#66848=CARTESIAN_POINT('Ctrl Pts',(0.199871272496017,-0.127686924414544,
-1.83521405827665));
#66849=CARTESIAN_POINT('Ctrl Pts',(0.198889442970073,-0.129213796104573,
-1.83533566706376));
#66850=CARTESIAN_POINT('Ctrl Pts',(0.198281801578081,-0.13014431571462,
-1.83540968962578));
#66851=CARTESIAN_POINT('Ctrl Pts',(0.195659140593141,-0.134099553284646,
-1.83572410174785));
#66852=CARTESIAN_POINT('Ctrl Pts',(0.193581160970091,-0.137082191109466,
-1.83596063247336));
#66853=CARTESIAN_POINT('Ctrl Pts',(0.187619430405574,-0.145233295922761,
-1.83660899642791));
#66854=CARTESIAN_POINT('Ctrl Pts',(0.183591580251059,-0.150292729834986,
-1.83701374402225));
#66855=CARTESIAN_POINT('Ctrl Pts',(0.176474595520834,-0.158518672669928,
-1.83768743028312));
#66856=CARTESIAN_POINT('Ctrl Pts',(0.173494785823795,-0.161774575345168,
-1.83795855102901));
#66857=CARTESIAN_POINT('Ctrl Pts',(0.15814076627188,-0.177638732782072,
-1.83931257757304));
#66858=CARTESIAN_POINT('Ctrl Pts',(0.144477710736296,-0.188918308839718,
-1.84038893672197));
#66859=CARTESIAN_POINT('Ctrl Pts',(0.12707407283701,-0.200284601411832,
-1.84173284868373));
#66860=CARTESIAN_POINT('Ctrl Pts',(0.124424882131842,-0.201941052712327,
-1.84193658444565));
#66861=CARTESIAN_POINT('Ctrl Pts',(0.120457309818049,-0.204314131750754,
-1.84224091372841));
#66862=CARTESIAN_POINT('Ctrl Pts',(0.119163535633641,-0.205071401037203,
-1.84234002803086));
#66863=CARTESIAN_POINT('Ctrl Pts',(0.116845143993157,-0.206399050165758,
-1.84251746349776));
#66864=CARTESIAN_POINT('Ctrl Pts',(0.115823302486003,-0.206974196702347,
-1.84259560968766));
#66865=CARTESIAN_POINT('Ctrl Pts',(0.113654308927228,-0.208173928917217,
-1.84276138275939));
#66866=CARTESIAN_POINT('Ctrl Pts',(0.112506181740366,-0.208796660821598,
-1.84284907257368));
#66867=CARTESIAN_POINT('Ctrl Pts',(0.109425319930819,-0.210434898677635,
-1.84308425139582));
#66868=CARTESIAN_POINT('Ctrl Pts',(0.107483647613497,-0.211433233345502,
-1.84323233919946));
#66869=CARTESIAN_POINT('Ctrl Pts',(0.0973816543078754,-0.216452185349494,
-1.84400235335656));
#66870=CARTESIAN_POINT('Ctrl Pts',(0.0890097058776161,-0.220027202977841,
-1.84463943972918));
#66871=CARTESIAN_POINT('Ctrl Pts',(0.0702608810731703,-0.226788008117977,
-1.84606328788048));
#66872=CARTESIAN_POINT('Ctrl Pts',(0.0598284575954476,-0.229760562478916,
-1.84685395122733));
#66873=CARTESIAN_POINT('Ctrl Pts',(0.0373393350305363,-0.234532544069527,
-1.84853290704963));
#66874=CARTESIAN_POINT('Ctrl Pts',(0.0252708436418725,-0.236138060286027,
-1.84941900940058));
#66875=CARTESIAN_POINT('Ctrl Pts',(0.0110630306850422,-0.236925898578749,
-1.85041158955824));
#66876=CARTESIAN_POINT('Ctrl Pts',(0.00899312594283196,-0.237013494300426,
-1.85055492101486));
#66877=CARTESIAN_POINT('Ctrl Pts',(0.00608929338007281,-0.237098282458763,
-1.85075397032715));
#66878=CARTESIAN_POINT('Ctrl Pts',(0.00525619520105101,-0.237118214195767,
-1.85081084286576));
#66879=CARTESIAN_POINT('Ctrl Pts',(0.00375093002656609,-0.237146290242015,
-1.85091315855521));
#66880=CARTESIAN_POINT('Ctrl Pts',(0.00307880167948047,-0.237155968664331,
-1.85095868468695));
#66881=CARTESIAN_POINT('Ctrl Pts',(0.00170144037645741,-0.237169945529206,
-1.85105164023833));
#66882=CARTESIAN_POINT('Ctrl Pts',(0.000996215548390938,-0.237173956304892,
-1.85109905356954));
#66883=CARTESIAN_POINT('Ctrl Pts',(-0.000824408665852629,-0.237176189889346,
-1.85122101396435));
#66884=CARTESIAN_POINT('Ctrl Pts',(-0.00193981217147089,-0.237169690203402,
-1.85129530372941));
#66885=CARTESIAN_POINT('Ctrl Pts',(-0.00672236624312382,-0.237108078906661,
-1.85161215793729));
#66886=CARTESIAN_POINT('Ctrl Pts',(-0.0103882357251234,-0.236975778189748,
-1.85185079362262));
#66887=CARTESIAN_POINT('Ctrl Pts',(-0.0205911832038786,-0.236370311544264,
-1.85250682793523));
#66888=CARTESIAN_POINT('Ctrl Pts',(-0.0271141607436452,-0.235711170147424,
-1.8529169462639));
#66889=CARTESIAN_POINT('Ctrl Pts',(-0.0358713947009013,-0.234457842276661,
-1.85346464732926));
#66890=CARTESIAN_POINT('Ctrl Pts',(-0.0381360953048283,-0.234100139367924,
-1.85360601918351));
#66891=CARTESIAN_POINT('Ctrl Pts',(-0.0601113142505172,-0.23030185762165,
-1.85497798506941));
#66892=CARTESIAN_POINT('Ctrl Pts',(-0.0793146302337192,-0.224413514151641,
-1.85618678514247));
#66893=CARTESIAN_POINT('Ctrl Pts',(-0.100149646615677,-0.215012000629097,
-1.85766774619856));
#66894=CARTESIAN_POINT('Ctrl Pts',(-0.102727400341699,-0.213792404480238,
-1.85785396715669));
#66895=CARTESIAN_POINT('Ctrl Pts',(-0.106595565747967,-0.211876174690437,
-1.85813830122538));
#66896=CARTESIAN_POINT('Ctrl Pts',(-0.107902597174045,-0.21121353507617,
-1.85823523629233));
#66897=CARTESIAN_POINT('Ctrl Pts',(-0.110189865027876,-0.210027163087761,
-1.85840643094883));
#66898=CARTESIAN_POINT('Ctrl Pts',(-0.111172727103218,-0.209508568478321,
-1.85848050799205));
#66899=CARTESIAN_POINT('Ctrl Pts',(-0.113277237293965,-0.208379171833997,
-1.85864024789927));
#66900=CARTESIAN_POINT('Ctrl Pts',(-0.11439766445566,-0.207766181077483,
-1.85872598681694));
#66901=CARTESIAN_POINT('Ctrl Pts',(-0.11668704510527,-0.206489517742784,
-1.85890263332605));
#66902=CARTESIAN_POINT('Ctrl Pts',(-0.117855414556305,-0.205824897820943,
-1.85899357264267));
#66903=CARTESIAN_POINT('Ctrl Pts',(-0.120749661278421,-0.204145799884859,
-1.85922084518851));
#66904=CARTESIAN_POINT('Ctrl Pts',(-0.122468435365179,-0.203119349697744,
-1.85935760513207));
#66905=CARTESIAN_POINT('Ctrl Pts',(-0.127288183597471,-0.200157586826751,
-1.85974627769366));
#66906=CARTESIAN_POINT('Ctrl Pts',(-0.130357590998437,-0.19817224126737,
-1.85999995924093));
#66907=CARTESIAN_POINT('Ctrl Pts',(-0.140760178193324,-0.191097405309512,
-1.86088137071236));
#66908=CARTESIAN_POINT('Ctrl Pts',(-0.147850636320891,-0.185665846099503,
-1.86152059901013));
#66909=CARTESIAN_POINT('Ctrl Pts',(-0.164280923778104,-0.171540538330984,
-1.86309183401066));
#66910=CARTESIAN_POINT('Ctrl Pts',(-0.173258822725673,-0.162467707772275,
-1.86403027489312));
#66911=CARTESIAN_POINT('Ctrl Pts',(-0.185812852589775,-0.147550574914649,
-1.86543548560185));
#66912=CARTESIAN_POINT('Ctrl Pts',(-0.189939139180032,-0.142199614228725,
-1.86591569649194));
#66913=CARTESIAN_POINT('Ctrl Pts',(-0.194628602336177,-0.135549252179181,
-1.86647809355813));
#66914=CARTESIAN_POINT('Ctrl Pts',(-0.195415578686871,-0.134412218379724,
-1.86657308458988));
#66915=CARTESIAN_POINT('Ctrl Pts',(-0.196626335087387,-0.132629788697261,
-1.86672011072611));
#66916=CARTESIAN_POINT('Ctrl Pts',(-0.197056969034579,-0.131989118860632,
-1.86677258290071));
#66917=CARTESIAN_POINT('Ctrl Pts',(-0.197848065857735,-0.13079967320799,
-1.86686929356309));
#66918=CARTESIAN_POINT('Ctrl Pts',(-0.198209378410447,-0.130251502882987,
-1.86691358632051));
#66919=CARTESIAN_POINT('Ctrl Pts',(-0.199032960629449,-0.128990630623477,
-1.86701483834222));
#66920=CARTESIAN_POINT('Ctrl Pts',(-0.199493681761564,-0.128276939466522,
-1.86707169515392));
#66921=CARTESIAN_POINT('Ctrl Pts',(-0.200924291641534,-0.126034469097009,
-1.86724897566372));
#66922=CARTESIAN_POINT('Ctrl Pts',(-0.201880544132622,-0.12449700705014,
-1.86736854389031));
#66923=CARTESIAN_POINT('Ctrl Pts',(-0.204095344717588,-0.12084341839375,
-1.86764842615613));
#66924=CARTESIAN_POINT('Ctrl Pts',(-0.205338755149752,-0.118718314401139,
-1.86780790769662));
#66925=CARTESIAN_POINT('Ctrl Pts',(-0.209759972332458,-0.110884694427224,
-1.86838525710799));
#66926=CARTESIAN_POINT('Ctrl Pts',(-0.212734835616159,-0.105064568502138,
-1.86879412521511));
#66927=CARTESIAN_POINT('Ctrl Pts',(-0.222835441311536,-0.0831099172756618,
-1.87029018363164));
#66928=CARTESIAN_POINT('Ctrl Pts',(-0.22839559577176,-0.0663199965379573,
-1.87134930950847));
#66929=CARTESIAN_POINT('Ctrl Pts',(-0.233342763019596,-0.0429251512636557,
-1.87286049976554));
#66930=CARTESIAN_POINT('Ctrl Pts',(-0.234397330451919,-0.0367327425098595,
-1.87326317853471));
#66931=CARTESIAN_POINT('Ctrl Pts',(-0.235463468218853,-0.0285127411615625,
-1.87380497609718));
#66932=CARTESIAN_POINT('Ctrl Pts',(-0.235696658365334,-0.0265161478848097,
-1.87393712798372));
#66933=CARTESIAN_POINT('Ctrl Pts',(-0.236035478295466,-0.023255981006669,
-1.87415392337934));
#66934=CARTESIAN_POINT('Ctrl Pts',(-0.236156406592251,-0.0219940716077888,
-1.87423808373788));
#66935=CARTESIAN_POINT('Ctrl Pts',(-0.236365238049562,-0.0196140911963583,
-1.87439730092783));
#66936=CARTESIAN_POINT('Ctrl Pts',(-0.2364553387219,-0.0184962441299297,
-1.87447228634766));
#66937=CARTESIAN_POINT('Ctrl Pts',(-0.236621627272399,-0.0162328136701359,
-1.87462454586558));
#66938=CARTESIAN_POINT('Ctrl Pts',(-0.236697431439527,-0.0150872330738839,
-1.87470182994859));
#66939=CARTESIAN_POINT('Ctrl Pts',(-0.236885405409102,-0.0118948426179452,
-1.87491783635867));
#66940=CARTESIAN_POINT('Ctrl Pts',(-0.236979359191677,-0.00984710277714088,
-1.87505712398689));
#66941=CARTESIAN_POINT('Ctrl Pts',(-0.237133582672749,-0.00515922991764161,
-1.87537774355154));
#66942=CARTESIAN_POINT('Ctrl Pts',(-0.237176322468442,-0.00251884913445103,
-1.87555959789399));
#66943=CARTESIAN_POINT('Ctrl Pts',(-0.237174968833357,0.000121589045928318,
-1.87574276215633));
#66944=CARTESIAN_POINT('Ctrl Pts',(-0.0419392741328075,0.233437524640348,
-1.89811014643447));
#66945=CARTESIAN_POINT('Ctrl Pts',(-0.0557647178783972,0.230953652023264,
-1.89716236890311));
#66946=CARTESIAN_POINT('Ctrl Pts',(-0.0694132968284817,0.227229285998194,
-1.89621459137175));
#66947=CARTESIAN_POINT('Ctrl Pts',(-0.0826482297992921,0.222308908359614,
-1.89526681384039));
#66948=CARTESIAN_POINT('Ctrl Pts',(-0.0958578704916535,0.217397933682242,
-1.89432084753492));
#66949=CARTESIAN_POINT('Ctrl Pts',(-0.108654636960885,0.211295710624007,
-1.89337488122945));
#66950=CARTESIAN_POINT('Ctrl Pts',(-0.120816083667543,0.204096679424819,
-1.89242891492398));
#66951=CARTESIAN_POINT('Ctrl Pts',(-0.132976886900327,0.196898029133314,
-1.8914829986705));
#66952=CARTESIAN_POINT('Ctrl Pts',(-0.14450169745988,0.188603071532895,
-1.89053708241702));
#66953=CARTESIAN_POINT('Ctrl Pts',(-0.155192756435186,0.179352136800901,
-1.88959116616354));
#66954=CARTESIAN_POINT('Ctrl Pts',(-0.165883101262724,0.170101820018392,
-1.88864531309594));
#66955=CARTESIAN_POINT('Ctrl Pts',(-0.175739189356455,0.159896216519811,
-1.88769946002834));
#66956=CARTESIAN_POINT('Ctrl Pts',(-0.184598172414416,0.148914389386176,
-1.88675360696074));
#66957=CARTESIAN_POINT('Ctrl Pts',(-0.193477638346253,0.137907171146288,
-1.88580556698422));
#66958=CARTESIAN_POINT('Ctrl Pts',(-0.201354913365268,0.126120829148612,
-1.8848575270077));
#66959=CARTESIAN_POINT('Ctrl Pts',(-0.208109274133015,0.113765155670924,
-1.88390948703118));
#66960=CARTESIAN_POINT('Ctrl Pts',(-0.211371365641569,0.107797849671148,
-1.88345162088166));
#66961=CARTESIAN_POINT('Ctrl Pts',(-0.214372225391734,0.101698120202883,
-1.88299375473214));
#66962=CARTESIAN_POINT('Ctrl Pts',(-0.217102271967589,0.0954912777771402,
-1.88253588858262));
#66963=CARTESIAN_POINT('Ctrl Pts',(-0.223316722733585,0.0813625383599422,
-1.88149364019435));
#66964=CARTESIAN_POINT('Ctrl Pts',(-0.228161089732516,0.0665956597385658,
-1.88045139180608));
#66965=CARTESIAN_POINT('Ctrl Pts',(-0.231525608196456,0.0514574909440909,
-1.87940914341781));
#66966=CARTESIAN_POINT('Ctrl Pts',(-0.234866127370754,0.0364273035149854,
-1.87837432944287));
#66967=CARTESIAN_POINT('Ctrl Pts',(-0.236747587829712,0.0210316072282276,
-1.87733951546794));
#66968=CARTESIAN_POINT('Ctrl Pts',(-0.237110022140893,0.00555139850354441,
-1.87630470149301));
#66969=CARTESIAN_POINT('Ctrl Pts',(-0.237152481940009,0.00373786558891791,
-1.87618347126689));
#66970=CARTESIAN_POINT('Ctrl Pts',(-0.23717415009495,0.00192319013249233,
-1.87606224104077));
#66971=CARTESIAN_POINT('Ctrl Pts',(-0.237174975484837,0.000107836760217876,
-1.87594101081465));
#66972=CARTESIAN_POINT('',(-0.237174951380842,0.000151863410009322,-1.8956589891905));
#66973=CARTESIAN_POINT('Ctrl Pts',(-0.0419392741328073,0.233437524640348,
-1.91783866303197));
#66974=CARTESIAN_POINT('Ctrl Pts',(-0.0558822279275878,0.230932540223977,
-1.91688952349866));
#66975=CARTESIAN_POINT('Ctrl Pts',(-0.0695810299052555,0.22717752105336,
-1.91594038396535));
#66976=CARTESIAN_POINT('Ctrl Pts',(-0.0828055599448024,0.222250354031726,
-1.91499124443204));
#66977=CARTESIAN_POINT('Ctrl Pts',(-0.0913653365601734,0.219061170830079,
-1.91437689954737));
#66978=CARTESIAN_POINT('Ctrl Pts',(-0.0997267139021598,0.215381955367923,
-1.91376255466271));
#66979=CARTESIAN_POINT('Ctrl Pts',(-0.107832458568548,0.211244269754383,
-1.91314820977804));
#66980=CARTESIAN_POINT('Ctrl Pts',(-0.120360313440485,0.204849258931122,
-1.91219870743455));
#66981=CARTESIAN_POINT('Ctrl Pts',(-0.132357915464483,0.197315221878836,
-1.91124920509106));
#66982=CARTESIAN_POINT('Ctrl Pts',(-0.143610941870615,0.188753484736136,
-1.91029970274757));
#66983=CARTESIAN_POINT('Ctrl Pts',(-0.154841841101612,0.18020858280295,
-1.90935206744002));
#66984=CARTESIAN_POINT('Ctrl Pts',(-0.16533037523629,0.170640436808729,
-1.90840443213246));
#66985=CARTESIAN_POINT('Ctrl Pts',(-0.174890356906369,0.160204068881421,
-1.9074567968249));
#66986=CARTESIAN_POINT('Ctrl Pts',(-0.184449345255448,0.14976878533521,
-1.90650925998051));
#66987=CARTESIAN_POINT('Ctrl Pts',(-0.193079377014223,0.138466038552127,
-1.90556172313612));
#66988=CARTESIAN_POINT('Ctrl Pts',(-0.200631105799812,0.126487706954251,
-1.90461418629173));
#66989=CARTESIAN_POINT('Ctrl Pts',(-0.208181830959439,0.114510967278559,
-1.90366677537514));
#66990=CARTESIAN_POINT('Ctrl Pts',(-0.214654110773553,0.101859535013325,
-1.90271936445854));
#66991=CARTESIAN_POINT('Ctrl Pts',(-0.219943163533292,0.0887523827283964,
-1.90177195354195));
#66992=CARTESIAN_POINT('Ctrl Pts',(-0.225244659434385,0.0756143942699501,
-1.90082231372569));
#66993=CARTESIAN_POINT('Ctrl Pts',(-0.229357100911607,0.0620193346874439,
-1.89987267390942));
#66994=CARTESIAN_POINT('Ctrl Pts',(-0.232224865083146,0.0482036581818705,
-1.89892303409316));
#66995=CARTESIAN_POINT('Ctrl Pts',(-0.233894591620518,0.0401596209761488,
-1.89837011596345));
#66996=CARTESIAN_POINT('Ctrl Pts',(-0.235143329028863,0.0320410305536099,
-1.89781719783375));
#66997=CARTESIAN_POINT('Ctrl Pts',(-0.235968201078832,0.0238953699410578,
-1.89726427970405));
#66998=CARTESIAN_POINT('Ctrl Pts',(-0.236766486397861,0.0160122548797073,
-1.8967291828662));
#66999=CARTESIAN_POINT('Ctrl Pts',(-0.237169869832119,0.00808804811135685,
-1.89619408602835));
#67000=CARTESIAN_POINT('Ctrl Pts',(-0.237174951380842,0.000151863410009322,
-1.8956589891905));
#67001=CARTESIAN_POINT('Ctrl Pts',(-0.237174944447511,0.000162330896843699,
-1.89549312073154));
#67002=CARTESIAN_POINT('Ctrl Pts',(-0.237184634811181,-0.0139958577776726,
-1.89459963185786));
#67003=CARTESIAN_POINT('Ctrl Pts',(-0.235926558959752,-0.0281278877879236,
-1.89374477756997));
#67004=CARTESIAN_POINT('Ctrl Pts',(-0.231083450137942,-0.0550021575796279,
-1.89206500264375));
#67005=CARTESIAN_POINT('Ctrl Pts',(-0.227680677881489,-0.0677217709568628,
-1.89124514588661));
#67006=CARTESIAN_POINT('Ctrl Pts',(-0.222445439750269,-0.0823138738571256,
-1.89023594839191));
#67007=CARTESIAN_POINT('Ctrl Pts',(-0.221615602453172,-0.0845226099006235,
-1.89008131918506));
#67008=CARTESIAN_POINT('Ctrl Pts',(-0.220263814763681,-0.0879637560919081,
-1.88983728224874));
#67009=CARTESIAN_POINT('Ctrl Pts',(-0.219764135091431,-0.0892047940555895,
-1.88974862573526));
#67010=CARTESIAN_POINT('Ctrl Pts',(-0.218812432448759,-0.0915119712257564,
-1.889582566415));
#67011=CARTESIAN_POINT('Ctrl Pts',(-0.218363047202494,-0.0925791607530103,
-1.8895052554225));
#67012=CARTESIAN_POINT('Ctrl Pts',(-0.217343636753233,-0.0949513137335354,
-1.88933226837249));
#67013=CARTESIAN_POINT('Ctrl Pts',(-0.216769641181143,-0.0962545111880764,
-1.88923645823292));
#67014=CARTESIAN_POINT('Ctrl Pts',(-0.215286426228996,-0.0995414334624076,
-1.88899279559419));
#67015=CARTESIAN_POINT('Ctrl Pts',(-0.214361517129657,-0.101517888615515,
-1.88884440631225));
#67016=CARTESIAN_POINT('Ctrl Pts',(-0.207030084992107,-0.116637510019767,
-1.88769442986415));
#67017=CARTESIAN_POINT('Ctrl Pts',(-0.199448979523235,-0.129173240309845,
-1.88665102448432));
#67018=CARTESIAN_POINT('Ctrl Pts',(-0.183174348102441,-0.151202777242698,
-1.88465772615423));
#67019=CARTESIAN_POINT('Ctrl Pts',(-0.174767310243425,-0.160846262397933,
-1.88371656013858));
#67020=CARTESIAN_POINT('Ctrl Pts',(-0.162872252175924,-0.172451138215211,
-1.88252447175839));
#67021=CARTESIAN_POINT('Ctrl Pts',(-0.160054919331403,-0.175069105875549,
-1.88225118622152));
#67022=CARTESIAN_POINT('Ctrl Pts',(-0.155882235161675,-0.178761543374882,
-1.88186074051206));
#67023=CARTESIAN_POINT('Ctrl Pts',(-0.154576957411494,-0.179891426335815,
-1.88174055174873));
#67024=CARTESIAN_POINT('Ctrl Pts',(-0.152240612567697,-0.181869619765219,
-1.88152902085354));
#67025=CARTESIAN_POINT('Ctrl Pts',(-0.151214514026267,-0.182723653819556,
-1.88143732053154));
#67026=CARTESIAN_POINT('Ctrl Pts',(-0.149595250030316,-0.184048403933412,
-1.88129455392657));
#67027=CARTESIAN_POINT('Ctrl Pts',(-0.149006967933456,-0.184525004728834,
-1.88124308264791));
#67028=CARTESIAN_POINT('Ctrl Pts',(-0.147939873196809,-0.185381087970523,
-1.88115044673451));
#67029=CARTESIAN_POINT('Ctrl Pts',(-0.147461877763405,-0.185761536589055,
-1.8811092144553));
#67030=CARTESIAN_POINT('Ctrl Pts',(-0.146341403284033,-0.186646300199484,
-1.88101316627766));
#67031=CARTESIAN_POINT('Ctrl Pts',(-0.145697783590055,-0.187149148008554,
-1.88095845441033));
#67032=CARTESIAN_POINT('Ctrl Pts',(-0.144035796094616,-0.188433856768741,
-1.88081831502408));
#67033=CARTESIAN_POINT('Ctrl Pts',(-0.143013638585458,-0.189210803845375,
-1.88073321748207));
#67034=CARTESIAN_POINT('Ctrl Pts',(-0.13624011529885,-0.194273141411539,
-1.88017607107161));
#67035=CARTESIAN_POINT('Ctrl Pts',(-0.130302591288763,-0.198304511268763,
-1.87971952406197));
#67036=CARTESIAN_POINT('Ctrl Pts',(-0.111330316063401,-0.209965267756706,
-1.8783263351731));
#67037=CARTESIAN_POINT('Ctrl Pts',(-0.0977441774117247,-0.2166240225215,
-1.87741762174244));
#67038=CARTESIAN_POINT('Ctrl Pts',(-0.0735408108175652,-0.225742475739598,
-1.87581509773933));
#67039=CARTESIAN_POINT('Ctrl Pts',(-0.0632192353012449,-0.22884754835643,
-1.87513677632853));
#67040=CARTESIAN_POINT('Ctrl Pts',(-0.0504987335144055,-0.231747846824982,
-1.87428643717059));
#67041=CARTESIAN_POINT('Ctrl Pts',(-0.0482670265010115,-0.232222910483537,
-1.87413676407644));
#67042=CARTESIAN_POINT('Ctrl Pts',(-0.0447247916369375,-0.232923680269989,
-1.87389826712956));
#67043=CARTESIAN_POINT('Ctrl Pts',(-0.043418585282702,-0.233170697446638,
-1.87381012212225));
#67044=CARTESIAN_POINT('Ctrl Pts',(-0.0409570690840748,-0.233614795274303,
-1.87364360984173));
#67045=CARTESIAN_POINT('Ctrl Pts',(-0.0398022364022077,-0.233814319432332,
-1.87356532275594));
#67046=CARTESIAN_POINT('Ctrl Pts',(-0.0371961175448163,-0.234244720174029,
-1.87338825345078));
#67047=CARTESIAN_POINT('Ctrl Pts',(-0.035744080114253,-0.234470681872684,
-1.87328931905078));
#67048=CARTESIAN_POINT('Ctrl Pts',(-0.0314564437638208,-0.235097157778114,
-1.87299631617937));
#67049=CARTESIAN_POINT('Ctrl Pts',(-0.0286156702447432,-0.235459813170809,
-1.87280107089615));
#67050=CARTESIAN_POINT('Ctrl Pts',(-0.00607571946853295,-0.23792336944405,
-1.87124246550739));
#67051=CARTESIAN_POINT('Ctrl Pts',(0.0138062545315421,-0.237599495419691,
-1.86980086325133));
#67052=CARTESIAN_POINT('Ctrl Pts',(0.0356711915459823,-0.234488285018245,
-1.86819004997522));
#67053=CARTESIAN_POINT('Ctrl Pts',(0.0379260362484901,-0.234134161698333,
-1.86802375445623));
#67054=CARTESIAN_POINT('Ctrl Pts',(0.0466792913279063,-0.232629693084337,
-1.86737813726479));
#67055=CARTESIAN_POINT('Ctrl Pts',(0.0531341105863897,-0.231240801438476,
-1.86690183691386));
#67056=CARTESIAN_POINT('Ctrl Pts',(0.0630905107760069,-0.228659464811337,
-1.86617415332546));
#67057=CARTESIAN_POINT('Ctrl Pts',(0.0666362464695275,-0.227651439141091,
-1.86591644081523));
#67058=CARTESIAN_POINT('Ctrl Pts',(0.0712267750376253,-0.226229928730689,
-1.8655858998817));
#67059=CARTESIAN_POINT('Ctrl Pts',(0.0722939425948105,-0.225891168761478,
-1.8655092805891));
#67060=CARTESIAN_POINT('Ctrl Pts',(0.0740317263022084,-0.225325952815515,
-1.86538492139253));
#67061=CARTESIAN_POINT('Ctrl Pts',(0.0747037832309765,-0.225104034428257,
-1.86533692786114));
#67062=CARTESIAN_POINT('Ctrl Pts',(0.0760130376177374,-0.2246651993077,
-1.86524363968965));
#67063=CARTESIAN_POINT('Ctrl Pts',(0.0766503173732511,-0.224448574351676,
-1.86519833018889));
#67064=CARTESIAN_POINT('Ctrl Pts',(0.0780755269895758,-0.223957337300892,
-1.86509720405988));
#67065=CARTESIAN_POINT('Ctrl Pts',(0.0788629556942779,-0.223681271270112,
-1.86504147165853));
#67066=CARTESIAN_POINT('Ctrl Pts',(0.0816026596227852,-0.222704487702123,
-1.86484799564965));
#67067=CARTESIAN_POINT('Ctrl Pts',(0.083547253596568,-0.221982296669889,
-1.86471144037634));
#67068=CARTESIAN_POINT('Ctrl Pts',(0.0967670071953243,-0.216874355296772,
-1.86378676723038));
#67069=CARTESIAN_POINT('Ctrl Pts',(0.107703178028697,-0.211656420477618,
-1.86303960269599));
#67070=CARTESIAN_POINT('Ctrl Pts',(0.127520715768036,-0.200265232626141,
-1.86163625154334));
#67071=CARTESIAN_POINT('Ctrl Pts',(0.136471278748143,-0.194276290790153,
-1.86098072229129));
#67072=CARTESIAN_POINT('Ctrl Pts',(0.152261756939972,-0.182079382547959,
-1.85973699341377));
#67073=CARTESIAN_POINT('Ctrl Pts',(0.159205505579167,-0.176040112756565,
-1.85915400034019));
#67074=CARTESIAN_POINT('Ctrl Pts',(0.167346648273412,-0.168082940673496,
-1.85841132850765));
#67075=CARTESIAN_POINT('Ctrl Pts',(0.16889131157139,-0.166530777883194,
-1.85826757948975));
#67076=CARTESIAN_POINT('Ctrl Pts',(0.171323703491092,-0.164017923394397,
-1.85803647922126));
#67077=CARTESIAN_POINT('Ctrl Pts',(0.172225384605834,-0.163070866048064,
-1.85794973829414));
#67078=CARTESIAN_POINT('Ctrl Pts',(0.173920588187102,-0.161260609887282,
-1.85778457888987));
#67079=CARTESIAN_POINT('Ctrl Pts',(0.174715633705693,-0.160398885751305,
-1.85770622916352));
#67080=CARTESIAN_POINT('Ctrl Pts',(0.176511105732669,-0.158423643698509,
-1.857527223829));
#67081=CARTESIAN_POINT('Ctrl Pts',(0.177507436745531,-0.157306487631131,
-1.8574263999426));
#67082=CARTESIAN_POINT('Ctrl Pts',(0.180542366063355,-0.153837964311554,
-1.85711458647974));
#67083=CARTESIAN_POINT('Ctrl Pts',(0.182545242289507,-0.151455927980086,
-1.85690214316056));
#67084=CARTESIAN_POINT('Ctrl Pts',(0.195749072900072,-0.135110035056083,
-1.85545492185889));
#67085=CARTESIAN_POINT('Ctrl Pts',(0.2053828610913,-0.119958606548223,-1.85415803876152));
#67086=CARTESIAN_POINT('Ctrl Pts',(0.215038755403543,-0.100137732087421,
-1.85254753678398));
#67087=CARTESIAN_POINT('Ctrl Pts',(0.216759393908215,-0.0963566170039159,
-1.85224419311605));
#67088=CARTESIAN_POINT('Ctrl Pts',(0.220922478150781,-0.086531567122758,
-1.85146825662011));
#67089=CARTESIAN_POINT('Ctrl Pts',(0.22321685612571,-0.0804282293298775,
-1.85099784207076));
#67090=CARTESIAN_POINT('Ctrl Pts',(0.226400825825719,-0.0707672208891036,
-1.85027812974325));
#67091=CARTESIAN_POINT('Ctrl Pts',(0.227464328460476,-0.067270471932179,
-1.85002259891089));
#67092=CARTESIAN_POINT('Ctrl Pts',(0.22874586359911,-0.0626781427933214,
-1.84969463707151));
#67093=CARTESIAN_POINT('Ctrl Pts',(0.229037519483508,-0.061603851257538,
-1.84961845584768));
#67094=CARTESIAN_POINT('Ctrl Pts',(0.229501311461506,-0.0598466749729449,
-1.8494947725221));
#67095=CARTESIAN_POINT('Ctrl Pts',(0.229677984765912,-0.0591650218863398,
-1.84944701851049));
#67096=CARTESIAN_POINT('Ctrl Pts',(0.230017147733215,-0.0578320239696665,
-1.8493540880373));
#67097=CARTESIAN_POINT('Ctrl Pts',(0.230179911544511,-0.0571807623722538,
-1.84930889720696));
#67098=CARTESIAN_POINT('Ctrl Pts',(0.23053828631472,-0.0557204802656415,
-1.84920802582521));
#67099=CARTESIAN_POINT('Ctrl Pts',(0.230732410112268,-0.0549110949968989,
-1.84915242945969));
#67100=CARTESIAN_POINT('Ctrl Pts',(0.231394376746947,-0.052085570196356,
-1.84895938205504));
#67101=CARTESIAN_POINT('Ctrl Pts',(0.231840103265428,-0.050064273154927,
-1.84882311791282));
#67102=CARTESIAN_POINT('Ctrl Pts',(0.234724276832261,-0.0361193597687741,
-1.84789399314954));
#67103=CARTESIAN_POINT('Ctrl Pts',(0.236268574193361,-0.0240277295893806,
-1.84714273569856));
#67104=CARTESIAN_POINT('Ctrl Pts',(0.237422862085469,-0.000992052638308131,
-1.84572718424032));
#67105=CARTESIAN_POINT('Ctrl Pts',(0.237218004461241,0.009909990692749,
-1.84506365284641));
#67106=CARTESIAN_POINT('Ctrl Pts',(0.235473282860477,0.0297672532661437,
-1.84382050702397));
#67107=CARTESIAN_POINT('Ctrl Pts',(0.234167329857106,0.0387219479702918,
-1.84324691795644));
#67108=CARTESIAN_POINT('Ctrl Pts',(0.231916639982723,0.0497131348529717,
-1.84251496396376));
#67109=CARTESIAN_POINT('Ctrl Pts',(0.231450387475106,0.0518405371871796,
-1.84237199337972));
#67110=CARTESIAN_POINT('Ctrl Pts',(0.230658276485097,0.0552307891212038,
-1.84214193388744));
#67111=CARTESIAN_POINT('Ctrl Pts',(0.230351176628517,0.0564979281788567,
-1.8420554479519));
#67112=CARTESIAN_POINT('Ctrl Pts',(0.229748447653327,0.058898240960359,
-1.84189064052908));
#67113=CARTESIAN_POINT('Ctrl Pts',(0.229454841969792,0.0600318865189183,
-1.84181238655193));
#67114=CARTESIAN_POINT('Ctrl Pts',(0.228766587479204,0.0626104834683579,
-1.84163341499536));
#67115=CARTESIAN_POINT('Ctrl Pts',(0.228366624731581,0.0640539516055271,
-1.8415325276798));
#67116=CARTESIAN_POINT('Ctrl Pts',(0.22709032540394,0.0684961674646237,
-1.84121982902522));
#67117=CARTESIAN_POINT('Ctrl Pts',(0.226168421029031,0.0714813580847788,
-1.8410065478741));
#67118=CARTESIAN_POINT('Ctrl Pts',(0.219645360881962,0.0912122683677192,
-1.83957513821474));
#67119=CARTESIAN_POINT('Ctrl Pts',(0.212249019757952,0.107302797973203,
-1.83829672182847));
#67120=CARTESIAN_POINT('Ctrl Pts',(0.200866988495921,0.126189525921918,
-1.83668599610456));
#67121=CARTESIAN_POINT('Ctrl Pts',(0.198491235353379,0.129894472106342,
-1.83636456098707));
#67122=CARTESIAN_POINT('Ctrl Pts',(0.192361876016848,0.138891909783512,
-1.83557298816622));
#67123=CARTESIAN_POINT('Ctrl Pts',(0.188491356638195,0.14410091527999,-1.835104860218));
#67124=CARTESIAN_POINT('Ctrl Pts',(0.182121738318622,0.151976697045788,
-1.83438826168345));
#67125=CARTESIAN_POINT('Ctrl Pts',(0.179766493735932,0.154755469500671,
-1.83413361014865));
#67126=CARTESIAN_POINT('Ctrl Pts',(0.176610224117248,0.158309962085933,
-1.83380664145114));
#67127=CARTESIAN_POINT('Ctrl Pts',(0.175866572383603,0.159135678586182,
-1.83373059695881));
#67128=CARTESIAN_POINT('Ctrl Pts',(0.174642791121286,0.160475452311941,
-1.83360710818035));
#67129=CARTESIAN_POINT('Ctrl Pts',(0.1741661401743,0.160992642487537,-1.83355941285533));
#67130=CARTESIAN_POINT('Ctrl Pts',(0.173229561643626,0.161999849436406,
-1.83346649219864));
#67131=CARTESIAN_POINT('Ctrl Pts',(0.172769841476089,0.162490043202691,
-1.83342125293572));
#67132=CARTESIAN_POINT('Ctrl Pts',(0.171735111891281,0.163584006296584,
-1.83332023867585));
#67133=CARTESIAN_POINT('Ctrl Pts',(0.171158984147169,0.164186716789967,
-1.83326454831863));
#67134=CARTESIAN_POINT('Ctrl Pts',(0.169137266316699,0.166279510882546,
-1.83307098918828));
#67135=CARTESIAN_POINT('Ctrl Pts',(0.167675250491103,0.167753693522431,
-1.83293431354991));
#67136=CARTESIAN_POINT('Ctrl Pts',(0.157576201511409,0.177672822352053,
-1.83201076196862));
#67137=CARTESIAN_POINT('Ctrl Pts',(0.148323189318488,0.185467511110483,
-1.83126476813234));
#67138=CARTESIAN_POINT('Ctrl Pts',(0.129812952595336,0.198785092292248,
-1.82986496964348));
#67139=CARTESIAN_POINT('Ctrl Pts',(0.120696104130112,0.204448910574454,
-1.82921178507571));
#67140=CARTESIAN_POINT('Ctrl Pts',(0.103041103751826,0.213823357649805,
-1.82796624768861));
#67141=CARTESIAN_POINT('Ctrl Pts',(0.0946075770403748,0.217686180527965,
-1.827378813469));
#67142=CARTESIAN_POINT('Ctrl Pts',(0.0839251200256205,0.221840867631301,
-1.82663111859779));
#67143=CARTESIAN_POINT('Ctrl Pts',(0.0818690070886439,0.222607864799082,
-1.82648706987633));
#67144=CARTESIAN_POINT('Ctrl Pts',(0.0785702775611092,0.223786515705193,
-1.82625560572852));
#67145=CARTESIAN_POINT('Ctrl Pts',(0.0773343509236932,0.224216616641623,
-1.82616880435029));
#67146=CARTESIAN_POINT('Ctrl Pts',(0.0749847268885639,0.225012544963826,
-1.82600360571782));
#67147=CARTESIAN_POINT('Ctrl Pts',(0.0738717495269176,0.225380387776795,
-1.82592527785344));
#67148=CARTESIAN_POINT('Ctrl Pts',(0.0713332086653112,0.226198560836576,
-1.82574642806855));
#67149=CARTESIAN_POINT('Ctrl Pts',(0.0699060341096111,0.226643689080322,
-1.82564573887647));
#67150=CARTESIAN_POINT('Ctrl Pts',(0.0655046212560836,0.227970939430144,
-1.82533473324368));
#67151=CARTESIAN_POINT('Ctrl Pts',(0.0625173104459858,0.228808192458946,
-1.82512297401412));
#67152=CARTESIAN_POINT('Ctrl Pts',(0.0421326182723946,0.234092412119568,
-1.82367276592415));
#67153=CARTESIAN_POINT('Ctrl Pts',(0.024298328226178,0.236608897301523,
-1.82237178865636));
#67154=CARTESIAN_POINT('Ctrl Pts',(-0.00715941131273107,0.237452081302828,
-1.82007360149346));
#67155=CARTESIAN_POINT('Ctrl Pts',(-0.0206814933532748,0.236658204907083,
-1.81908679755903));
#67156=CARTESIAN_POINT('Ctrl Pts',(-0.0355525043970215,0.234500029678021,
-1.81804667772843));
#67157=CARTESIAN_POINT('Ctrl Pts',(-0.037039478066328,0.234269762977691,
-1.81794320048208));
#67158=CARTESIAN_POINT('Ctrl Pts',(-0.0393031790927103,0.233897122639109,
-1.81778657560314));
#67159=CARTESIAN_POINT('Ctrl Pts',(-0.0400815204268637,0.233765000869813,
-1.81773288588515));
#67160=CARTESIAN_POINT('Ctrl Pts',(-0.0412193742211361,0.233566002461466,
-1.81765465084603));
#67161=CARTESIAN_POINT('Ctrl Pts',(-0.0415793972373618,0.233502179951423,
-1.8176299341645));
#67162=CARTESIAN_POINT('Ctrl Pts',(-0.0419392741328096,0.233437524640348,
-1.81760526556689));
#67163=CARTESIAN_POINT('Origin',(0.,0.,-2.1456589891905));
#67164=CARTESIAN_POINT('',(-0.0419392692346775,0.233437525520344,-1.69793969278784));
#67165=CARTESIAN_POINT('',(-0.0419393124730349,0.233437517752158,-1.71790170279738));
#67166=CARTESIAN_POINT('',(-0.0419392741328076,0.233437524640348,-2.1456589891905));
#67167=CARTESIAN_POINT('Ctrl Pts',(-0.0419392692346775,0.233437525520344,
-1.69793969278784));
#67168=CARTESIAN_POINT('Ctrl Pts',(-0.0371287966350787,0.234301772624793,
-1.6982501843674));
#67169=CARTESIAN_POINT('Ctrl Pts',(-0.032292004561194,0.235017255155577,
-1.69856447585913));
#67170=CARTESIAN_POINT('Ctrl Pts',(-0.0252667305782954,0.235835411594207,
-1.69902590010247));
#67171=CARTESIAN_POINT('Ctrl Pts',(-0.0230943975890999,0.236058038017637,
-1.69916925119909));
#67172=CARTESIAN_POINT('Ctrl Pts',(-0.0196182458083198,0.236365841914204,
-1.69939985294673));
#67173=CARTESIAN_POINT('Ctrl Pts',(-0.0183162262750079,0.236470299470237,
-1.69948649738776));
#67174=CARTESIAN_POINT('Ctrl Pts',(-0.0158439214709464,0.236648105014684,
-1.69965156354595));
#67175=CARTESIAN_POINT('Ctrl Pts',(-0.014673821697801,0.23672353986501,
-1.69972991725923));
#67176=CARTESIAN_POINT('Ctrl Pts',(-0.0120067902043739,0.236875630287251,
-1.6999090584211));
#67177=CARTESIAN_POINT('Ctrl Pts',(-0.0105096072730364,0.236946777168043,
-1.70001001535038));
#67178=CARTESIAN_POINT('Ctrl Pts',(-0.00589094467926848,0.237122398173867,
-1.70032272188493));
#67179=CARTESIAN_POINT('Ctrl Pts',(-0.00276810692013724,0.237179406583153,
-1.70053593808214));
#67180=CARTESIAN_POINT('Ctrl Pts',(0.0180267418323495,0.237148296859321,
-1.70196826815008));
#67181=CARTESIAN_POINT('Ctrl Pts',(0.035637175020166,0.235146856451655,
-1.70324771751406));
#67182=CARTESIAN_POINT('Ctrl Pts',(0.0571333906288445,0.23023246264618,
-1.70485824146629));
#67183=CARTESIAN_POINT('Ctrl Pts',(0.061380482877471,0.229136746020173,
-1.70517853501963));
#67184=CARTESIAN_POINT('Ctrl Pts',(0.0718174415717139,0.226133067267341,
-1.70596810384619));
#67185=CARTESIAN_POINT('Ctrl Pts',(0.0779645775605586,0.224088029518718,
-1.70643536910158));
#67186=CARTESIAN_POINT('Ctrl Pts',(0.0874233130926202,0.220504839799236,
-1.70715089509841));
#67187=CARTESIAN_POINT('Ctrl Pts',(0.0907960691438752,0.219137622188636,
-1.70740530474828));
#67188=CARTESIAN_POINT('Ctrl Pts',(0.0951567347037798,0.217251956489909,
-1.70773208625057));
#67189=CARTESIAN_POINT('Ctrl Pts',(0.09617413444592,0.216803488773754,-1.70780817314177));
#67190=CARTESIAN_POINT('Ctrl Pts',(0.0978306600255841,0.216059339937072,
-1.70793175863884));
#67191=CARTESIAN_POINT('Ctrl Pts',(0.0984716748848465,0.215767944082327,
-1.70797950809556));
#67192=CARTESIAN_POINT('Ctrl Pts',(0.0997222949091607,0.21519269663022,
-1.7080725095042));
#67193=CARTESIAN_POINT('Ctrl Pts',(0.100332004183731,0.214909101107828,
-1.7081177753938));
#67194=CARTESIAN_POINT('Ctrl Pts',(0.101695781294438,0.21426769544878,-1.70821887467106));
#67195=CARTESIAN_POINT('Ctrl Pts',(0.102449190781078,0.213908486523314,
-1.70827462313361));
#67196=CARTESIAN_POINT('Ctrl Pts',(0.105073535010709,0.212640211518016,
-1.70846850461914));
#67197=CARTESIAN_POINT('Ctrl Pts',(0.106934458587307,0.211710485347377,
-1.70860543946312));
#67198=CARTESIAN_POINT('Ctrl Pts',(0.119464876992314,0.205242844945281,
-1.70952538823911));
#67199=CARTESIAN_POINT('Ctrl Pts',(0.1297135827923,0.198924465120284,-1.71026794446004));
#67200=CARTESIAN_POINT('Ctrl Pts',(0.1480384393526,0.18560600323059,-1.71165864432544));
#67201=CARTESIAN_POINT('Ctrl Pts',(0.156206923877903,0.17878578375222,-1.71230624536357));
#67202=CARTESIAN_POINT('Ctrl Pts',(0.170679347399284,0.164950769374471,
-1.71355311850542));
#67203=CARTESIAN_POINT('Ctrl Pts',(0.177076286558787,0.158063762872574,
-1.71414805101863));
#67204=CARTESIAN_POINT('Ctrl Pts',(0.184447904541046,0.149116733369563,
-1.7149042019278));
#67205=CARTESIAN_POINT('Ctrl Pts',(0.185824381896733,0.147397856893892,
-1.71504873788519));
#67206=CARTESIAN_POINT('Ctrl Pts',(0.187981341245023,0.144626113075517,
-1.71528079573552));
#67207=CARTESIAN_POINT('Ctrl Pts',(0.188777397481656,0.143585484373308,
-1.71536769763333));
#67208=CARTESIAN_POINT('Ctrl Pts',(0.190268987078782,0.141601787438656,
-1.71553296631488));
#67209=CARTESIAN_POINT('Ctrl Pts',(0.190966235412761,0.140660052954229,
-1.71561126267076));
#67210=CARTESIAN_POINT('Ctrl Pts',(0.192535305053894,0.138507626897638,
-1.71578987119754));
#67211=CARTESIAN_POINT('Ctrl Pts',(0.193402731252858,0.137293808191824,
-1.71589034910425));
#67212=CARTESIAN_POINT('Ctrl Pts',(0.196029412680728,0.133543911999489,
-1.71620006514583));
#67213=CARTESIAN_POINT('Ctrl Pts',(0.197750601279868,0.13098169794209,-1.71641072955723));
#67214=CARTESIAN_POINT('Ctrl Pts',(0.209265050054842,0.113096472569572,
-1.71787540546711));
#67215=CARTESIAN_POINT('Ctrl Pts',(0.217315911428638,0.0967275721864568,
-1.71919380376489));
#67216=CARTESIAN_POINT('Ctrl Pts',(0.224703613739888,0.0759931480312389,
-1.72080140268741));
#67217=CARTESIAN_POINT('Ctrl Pts',(0.225902395432838,0.0723517861603751,
-1.72108123755319));
#67218=CARTESIAN_POINT('Ctrl Pts',(0.22890707679145,0.062420644573984,-1.72183571978181));
#67219=CARTESIAN_POINT('Ctrl Pts',(0.230541939000404,0.0560821948155643,
-1.722308000844));
#67220=CARTESIAN_POINT('Ctrl Pts',(0.232680118736906,0.0461016705786794,
-1.72303019545722));
#67221=CARTESIAN_POINT('Ctrl Pts',(0.233364503638271,0.0425019267676532,
-1.72328638315693));
#67222=CARTESIAN_POINT('Ctrl Pts',(0.234147987313098,0.0377881297580144,
-1.7236150763283));
#67223=CARTESIAN_POINT('Ctrl Pts',(0.234322973746065,0.0366874203474679,
-1.72369134931222));
#67224=CARTESIAN_POINT('Ctrl Pts',(0.234595933156294,0.0348887573497782,
-1.7238151602851));
#67225=CARTESIAN_POINT('Ctrl Pts',(0.234698563262774,0.0341915439605781,
-1.72386295081084));
#67226=CARTESIAN_POINT('Ctrl Pts',(0.234892989785021,0.0328285789570707,
-1.72395596701296));
#67227=CARTESIAN_POINT('Ctrl Pts',(0.234985066351809,0.0321628800839689,
-1.72400120706889));
#67228=CARTESIAN_POINT('Ctrl Pts',(0.2351849536989,0.0306710335112133,-1.72410218147261));
#67229=CARTESIAN_POINT('Ctrl Pts',(0.235291244461667,0.029844682521119,
-1.72415783157489));
#67230=CARTESIAN_POINT('Ctrl Pts',(0.235646596284867,0.0269620562251806,
-1.72435103620877));
#67231=CARTESIAN_POINT('Ctrl Pts',(0.235873082488558,0.0249030217145075,
-1.72448740348092));
#67232=CARTESIAN_POINT('Ctrl Pts',(0.237243400767329,0.0107402556632508,
-1.72541579262485));
#67233=CARTESIAN_POINT('Ctrl Pts',(0.237482216190972,-0.00143444589990504,
-1.72616635489699));
#67234=CARTESIAN_POINT('Ctrl Pts',(0.236165921497674,-0.0243941535462405,
-1.72757792863405));
#67235=CARTESIAN_POINT('Ctrl Pts',(0.234804889310994,-0.0351578066973479,
-1.72823822039477));
#67236=CARTESIAN_POINT('Ctrl Pts',(0.230956442517926,-0.0547161584103204,
-1.72948114300453));
#67237=CARTESIAN_POINT('Ctrl Pts',(0.228688240202105,-0.0635326375192434,
-1.73005806201125));
#67238=CARTESIAN_POINT('Ctrl Pts',(0.225255000034431,-0.0742760535111648,
-1.7307938814289));
#67239=CARTESIAN_POINT('Ctrl Pts',(0.224561753873381,-0.0763463511906751,
-1.7309372049059));
#67240=CARTESIAN_POINT('Ctrl Pts',(0.223408263412331,-0.0796394022090826,
-1.73116777260335));
#67241=CARTESIAN_POINT('Ctrl Pts',(0.222966314661338,-0.0808684670041031,
-1.73125441093155));
#67242=CARTESIAN_POINT('Ctrl Pts',(0.22210838839416,-0.0831938657442761,
-1.73141947213356));
#67243=CARTESIAN_POINT('Ctrl Pts',(0.221694386716202,-0.0842908910017697,
-1.73149782705979));
#67244=CARTESIAN_POINT('Ctrl Pts',(0.220732611810652,-0.0867833036889839,
-1.73167698037627));
#67245=CARTESIAN_POINT('Ctrl Pts',(0.220179714255993,-0.0881766463774786,
-1.73177794833478));
#67246=CARTESIAN_POINT('Ctrl Pts',(0.218433919496877,-0.0924573583499218,
-1.7320907245545));
#67247=CARTESIAN_POINT('Ctrl Pts',(0.217197195243552,-0.0953263712460283,
-1.73230400035997));
#67248=CARTESIAN_POINT('Ctrl Pts',(0.20859527678713,-0.114244476112031,
-1.73373544800115));
#67249=CARTESIAN_POINT('Ctrl Pts',(0.199515363056517,-0.129449543973588,
-1.73501384883128));
#67250=CARTESIAN_POINT('Ctrl Pts',(0.18617075548076,-0.147009596010536,
-1.73662469551224));
#67251=CARTESIAN_POINT('Ctrl Pts',(0.183409241612209,-0.150440760732392,
-1.73694632552688));
#67252=CARTESIAN_POINT('Ctrl Pts',(0.176357577589377,-0.158719446032334,
-1.73773692262608));
#67253=CARTESIAN_POINT('Ctrl Pts',(0.171961217468533,-0.163472348417104,
-1.73820389321613));
#67254=CARTESIAN_POINT('Ctrl Pts',(0.164798755024177,-0.170606505449436,
-1.73891902690364));
#67255=CARTESIAN_POINT('Ctrl Pts',(0.16216294631855,-0.173113811638388,
-1.73917333160133));
#67256=CARTESIAN_POINT('Ctrl Pts',(0.158647475233605,-0.176307104233043,
-1.73950000006214));
#67257=CARTESIAN_POINT('Ctrl Pts',(0.15781935031295,-0.177048776303312,
-1.7395760757885));
#67258=CARTESIAN_POINT('Ctrl Pts',(0.156458242560708,-0.178250651326304,
-1.73969964766496));
#67259=CARTESIAN_POINT('Ctrl Pts',(0.155928382766988,-0.1787143414619,-1.73974739456614));
#67260=CARTESIAN_POINT('Ctrl Pts',(0.154888451314804,-0.179616258897454,
-1.73984039468729));
#67261=CARTESIAN_POINT('Ctrl Pts',(0.154378569645772,-0.180054686311474,
-1.73988566181945));
#67262=CARTESIAN_POINT('Ctrl Pts',(0.153231599626905,-0.181032467417762,
-1.73998676777583));
#67263=CARTESIAN_POINT('Ctrl Pts',(0.152593508203342,-0.181570643800616,
-1.74004252163597));
#67264=CARTESIAN_POINT('Ctrl Pts',(0.150355094085289,-0.183438423116216,
-1.74023644139134));
#67265=CARTESIAN_POINT('Ctrl Pts',(0.148740073448511,-0.184750373934941,
-1.74037340847613));
#67266=CARTESIAN_POINT('Ctrl Pts',(0.137683673381442,-0.193492987199117,
-1.74129297067195));
#67267=CARTESIAN_POINT('Ctrl Pts',(0.12770551808618,-0.200219141713083,
-1.74203515444148));
#67268=CARTESIAN_POINT('Ctrl Pts',(0.108028799506185,-0.211410800821003,
-1.74342484008459));
#67269=CARTESIAN_POINT('Ctrl Pts',(0.0984561547738076,-0.216035009790264,
-1.74407180825317));
#67270=CARTESIAN_POINT('Ctrl Pts',(0.0798805286347172,-0.223516373858651,
-1.7453188648375));
#67271=CARTESIAN_POINT('Ctrl Pts',(0.0709544612949117,-0.226508059428522,
-1.7459146797503));
#67272=CARTESIAN_POINT('Ctrl Pts',(0.0597483949223565,-0.229536408680303,
-1.74667182614111));
#67273=CARTESIAN_POINT('Ctrl Pts',(0.0576138916008783,-0.230081447673283,
-1.74681641980918));
#67274=CARTESIAN_POINT('Ctrl Pts',(0.0541981200994316,-0.230903143159002,
-1.74704854842856));
#67275=CARTESIAN_POINT('Ctrl Pts',(0.0529215809786821,-0.231199056859538,
-1.74713546270623));
#67276=CARTESIAN_POINT('Ctrl Pts',(0.0504990685385622,-0.23173950382593,
-1.747300740945));
#67277=CARTESIAN_POINT('Ctrl Pts',(0.0493536035275094,-0.231986153230337,
-1.74737903436004));
#67278=CARTESIAN_POINT('Ctrl Pts',(0.0467459466916553,-0.232527464728643,
-1.7475576167204));
#67279=CARTESIAN_POINT('Ctrl Pts',(0.0452827204979859,-0.232816838807933,
-1.74765807122044));
#67280=CARTESIAN_POINT('Ctrl Pts',(0.0407852696601377,-0.23366227316649,
-1.74796764248087));
#67281=CARTESIAN_POINT('Ctrl Pts',(0.0377429505312559,-0.234172936618899,
-1.7481781835874));
#67282=CARTESIAN_POINT('Ctrl Pts',(0.0166808833046302,-0.237287186318497,
-1.74964420480863));
#67283=CARTESIAN_POINT('Ctrl Pts',(-0.00157338997851186,-0.237867062825944,
-1.75096424667569));
#67284=CARTESIAN_POINT('Ctrl Pts',(-0.0235085183083695,-0.236037829829799,
-1.75257184277125));
#67285=CARTESIAN_POINT('Ctrl Pts',(-0.0272986087407516,-0.235629569757196,
-1.75285009644845));
#67286=CARTESIAN_POINT('Ctrl Pts',(-0.0375653165665592,-0.234272614653689,
-1.75360314816787));
#67287=CARTESIAN_POINT('Ctrl Pts',(-0.0440155664850886,-0.233146847368946,
-1.75407556739695));
#67288=CARTESIAN_POINT('Ctrl Pts',(-0.0539918152787328,-0.230976818269961,
-1.75479794558265));
#67289=CARTESIAN_POINT('Ctrl Pts',(-0.0575539720588981,-0.23011508131599,
-1.75505418213814));
#67290=CARTESIAN_POINT('Ctrl Pts',(-0.0621719113940535,-0.228883980025758,
-1.75538292788393));
#67291=CARTESIAN_POINT('Ctrl Pts',(-0.06324685253013,-0.22858927937995,
-1.75545920602704));
#67292=CARTESIAN_POINT('Ctrl Pts',(-0.0649980215446012,-0.228095888744375,
-1.7555830232952));
#67293=CARTESIAN_POINT('Ctrl Pts',(-0.0656754966235909,-0.227901747345606,
-1.7556308150032));
#67294=CARTESIAN_POINT('Ctrl Pts',(-0.0669973014848966,-0.227516579265103,
-1.75572383242033));
#67295=CARTESIAN_POINT('Ctrl Pts',(-0.0676416988422023,-0.227325829684345,
-1.75576907251866));
#67296=CARTESIAN_POINT('Ctrl Pts',(-0.0690831201836953,-0.226892479399009,
-1.75587004536072));
#67297=CARTESIAN_POINT('Ctrl Pts',(-0.0698797023615972,-0.22664841043365,
-1.75592569387407));
#67298=CARTESIAN_POINT('Ctrl Pts',(-0.0726520013762823,-0.225782985968168,
-1.75611888487856));
#67299=CARTESIAN_POINT('Ctrl Pts',(-0.07462092007861,-0.225139932174956,
-1.75625524036277));
#67300=CARTESIAN_POINT('Ctrl Pts',(-0.0880914363734373,-0.220544290708814,
-1.75718389130812));
#67301=CARTESIAN_POINT('Ctrl Pts',(-0.0992841077765119,-0.215737404444969,
-1.75793469780409));
#67302=CARTESIAN_POINT('Ctrl Pts',(-0.119664298256086,-0.205060963001253,
-1.75934687839085));
#67303=CARTESIAN_POINT('Ctrl Pts',(-0.128912331858323,-0.199376888551832,
-1.7600075276878));
#67304=CARTESIAN_POINT('Ctrl Pts',(-0.145137197186066,-0.187802469106299,
-1.76125030218137));
#67305=CARTESIAN_POINT('Ctrl Pts',(-0.152225389661359,-0.182104297397841,
-1.76182667453311));
#67306=CARTESIAN_POINT('Ctrl Pts',(-0.160588518911486,-0.174551059218529,
-1.76256187751194));
#67307=CARTESIAN_POINT('Ctrl Pts',(-0.162188020554886,-0.173065854941128,
-1.76270516437074));
#67308=CARTESIAN_POINT('Ctrl Pts',(-0.164711436459337,-0.170657050688398,
-1.76293568778416));
#67309=CARTESIAN_POINT('Ctrl Pts',(-0.165648638202693,-0.169747503062354,
-1.76302231888555));
#67310=CARTESIAN_POINT('Ctrl Pts',(-0.167412958574379,-0.16800671680448,
-1.7631873757744));
#67311=CARTESIAN_POINT('Ctrl Pts',(-0.168241520312579,-0.167176991083608,
-1.76326573369276));
#67312=CARTESIAN_POINT('Ctrl Pts',(-0.170115393927684,-0.165272445428651,
-1.76344490714452));
#67313=CARTESIAN_POINT('Ctrl Pts',(-0.171156726207246,-0.164193798187904,
-1.76354589237277));
#67314=CARTESIAN_POINT('Ctrl Pts',(-0.174337022194409,-0.160836410402298,
-1.7638587726081));
#67315=CARTESIAN_POINT('Ctrl Pts',(-0.176441150621054,-0.158525288080713,
-1.76407213653543));
#67316=CARTESIAN_POINT('Ctrl Pts',(-0.190112922887156,-0.142899085607667,
-1.76550228622493));
#67317=CARTESIAN_POINT('Ctrl Pts',(-0.200207881602859,-0.128373095693726,
-1.7667791435396));
#67318=CARTESIAN_POINT('Ctrl Pts',(-0.215170485425602,-0.100719313762183,
-1.76907557861254));
#67319=CARTESIAN_POINT('Ctrl Pts',(-0.220669930043714,-0.0880203631203799,
-1.77008477857942));
#67320=CARTESIAN_POINT('Ctrl Pts',(-0.225510372989238,-0.0734801681962261,
-1.77114563972998));
#67321=CARTESIAN_POINT('Ctrl Pts',(-0.225973909804841,-0.0720420420888783,
-1.7712495583202));
#67322=CARTESIAN_POINT('Ctrl Pts',(-0.226659024856208,-0.0698447716957313,
-1.77140669931785));
#67323=CARTESIAN_POINT('Ctrl Pts',(-0.226890592173997,-0.069088819000598,
-1.77146046971265));
#67324=CARTESIAN_POINT('Ctrl Pts',(-0.227307210202494,-0.0677040795699109,
-1.77155841286855));
#67325=CARTESIAN_POINT('Ctrl Pts',(-0.227493436001042,-0.0670756796399827,
-1.77160265079527));
#67326=CARTESIAN_POINT('Ctrl Pts',(-0.227908576823507,-0.0656532110891207,
-1.77170232194437));
#67327=CARTESIAN_POINT('Ctrl Pts',(-0.228135948525569,-0.0648587122766279,
-1.77175766585196));
#67328=CARTESIAN_POINT('Ctrl Pts',(-0.228714589309954,-0.0627960883985072,
-1.77190054151389));
#67329=CARTESIAN_POINT('Ctrl Pts',(-0.229059471619472,-0.0615261792727594,
-1.77198772113345));
#67330=CARTESIAN_POINT('Ctrl Pts',(-0.23143881793859,-0.0524676537366121,
-1.77260444783947));
#67331=CARTESIAN_POINT('Ctrl Pts',(-0.23308639318249,-0.0445818818422,-1.77311441502904));
#67332=CARTESIAN_POINT('Ctrl Pts',(-0.23621322905722,-0.0245770790752242,
-1.77437552441747));
#67333=CARTESIAN_POINT('Ctrl Pts',(-0.23716447290241,-0.0123997790984111,
-1.77511444457095));
#67334=CARTESIAN_POINT('Ctrl Pts',(-0.237185568223226,0.0122448055089872,
-1.77663336339897));
#67335=CARTESIAN_POINT('Ctrl Pts',(-0.23621628787675,0.0246725294036408,
-1.77741178370879));
#67336=CARTESIAN_POINT('Ctrl Pts',(-0.233905237174039,0.0393191648082009,
-1.7783768335306));
#67337=CARTESIAN_POINT('Ctrl Pts',(-0.233498484371059,0.04166669918446,
-1.77853294004969));
#67338=CARTESIAN_POINT('Ctrl Pts',(-0.23280351116214,0.0453471507595598,
-1.77878012319147));
#67339=CARTESIAN_POINT('Ctrl Pts',(-0.232539034570062,0.0466844316802177,
-1.77887044559743));
#67340=CARTESIAN_POINT('Ctrl Pts',(-0.232029243591978,0.0491502219033092,
-1.77903796573602));
#67341=CARTESIAN_POINT('Ctrl Pts',(-0.231787185207946,0.0502793684045034,
-1.77911505726072));
#67342=CARTESIAN_POINT('Ctrl Pts',(-0.231230920573847,0.0527847971283286,
-1.77928698041455));
#67343=CARTESIAN_POINT('Ctrl Pts',(-0.230912655210498,0.0541601232552643,
-1.77938193974669));
#67344=CARTESIAN_POINT('Ctrl Pts',(-0.22995441073413,0.0581389474750131,
-1.77965839727738));
#67345=CARTESIAN_POINT('Ctrl Pts',(-0.229282559096718,0.0607344654645677,
-1.77984091131453));
#67346=CARTESIAN_POINT('Ctrl Pts',(-0.224633657572367,0.0775161988928925,
-1.78103560412374));
#67347=CARTESIAN_POINT('Ctrl Pts',(-0.219386770959641,0.0913145314764611,
-1.78208922235472));
#67348=CARTESIAN_POINT('Ctrl Pts',(-0.205729670451209,0.119128510280837,
-1.78434498511081));
#67349=CARTESIAN_POINT('Ctrl Pts',(-0.197082115277084,0.132947378184802,
-1.78554542520255));
#67350=CARTESIAN_POINT('Ctrl Pts',(-0.185714337261873,0.147536989754321,
-1.78683792526994));
#67351=CARTESIAN_POINT('Ctrl Pts',(-0.184315372054303,0.149281020029628,
-1.78699281630458));
#67352=CARTESIAN_POINT('Ctrl Pts',(-0.182344510676915,0.15166805599514,
-1.78720505791824));
#67353=CARTESIAN_POINT('Ctrl Pts',(-0.18179351604347,0.152328058365742,
-1.78726376782028));
#67354=CARTESIAN_POINT('Ctrl Pts',(-0.180840297133733,0.153457321419483,
-1.78736424418783));
#67355=CARTESIAN_POINT('Ctrl Pts',(-0.180439810021333,0.153928027163815,
-1.78740613249747));
#67356=CARTESIAN_POINT('Ctrl Pts',(-0.179593808938075,0.154914521317799,
-1.78749392633291));
#67357=CARTESIAN_POINT('Ctrl Pts',(-0.17914790395882,0.155429963811847,
-1.7875398007564));
#67358=CARTESIAN_POINT('Ctrl Pts',(-0.178038145931827,0.156701665006331,
-1.78765300833025));
#67359=CARTESIAN_POINT('Ctrl Pts',(-0.17737168015547,0.157455645794402,
-1.78772015129858));
#67360=CARTESIAN_POINT('Ctrl Pts',(-0.174849169802852,0.16027305089246,
-1.78797123527754));
#67361=CARTESIAN_POINT('Ctrl Pts',(-0.172961669040362,0.162308181298798,
-1.78815299169916));
#67362=CARTESIAN_POINT('Ctrl Pts',(-0.168011491502528,0.167461082939212,
-1.78861568277769));
#67363=CARTESIAN_POINT('Ctrl Pts',(-0.164897501630042,0.17052827977056,
-1.78889353457784));
#67364=CARTESIAN_POINT('Ctrl Pts',(-0.154703488025146,0.180028573636075,
-1.78976911452611));
#67365=CARTESIAN_POINT('Ctrl Pts',(-0.147318219221917,0.18612044022142,
-1.79035396772996));
#67366=CARTESIAN_POINT('Ctrl Pts',(-0.127006269313363,0.200906581356134,
-1.79189371948727));
#67367=CARTESIAN_POINT('Ctrl Pts',(-0.113558782386345,0.208802232665008,
-1.79284936163473));
#67368=CARTESIAN_POINT('Ctrl Pts',(-0.0965644993398727,0.21665013677787,
-1.79405877030531));
#67369=CARTESIAN_POINT('Ctrl Pts',(-0.0936669139367885,0.217918544403896,
-1.79426489998666));
#67370=CARTESIAN_POINT('Ctrl Pts',(-0.0893479764318352,0.219707091159926,
-1.79457246989879));
#67371=CARTESIAN_POINT('Ctrl Pts',(-0.0879455419069915,0.22027221404261,
-1.794672392306));
#67372=CARTESIAN_POINT('Ctrl Pts',(-0.0854416054859059,0.221253472128248,
-1.79485092986333));
#67373=CARTESIAN_POINT('Ctrl Pts',(-0.0843422179254959,0.2216748904736,
-1.7949293646418));
#67374=CARTESIAN_POINT('Ctrl Pts',(-0.0820354495447255,0.22253947905544,
-1.7950940561207));
#67375=CARTESIAN_POINT('Ctrl Pts',(-0.0808275136238489,0.222981047734035,
-1.79518036328306));
#67376=CARTESIAN_POINT('Ctrl Pts',(-0.0776461585768175,0.224114765305109,
-1.79540787742805));
#67377=CARTESIAN_POINT('Ctrl Pts',(-0.0756671093598199,0.224790662710331,
-1.79554961641383));
#67378=CARTESIAN_POINT('Ctrl Pts',(-0.0662339549736757,0.227873649818092,
-1.79622638152544));
#67379=CARTESIAN_POINT('Ctrl Pts',(-0.0586733271183367,0.229936411793327,
-1.7967724699271));
#67380=CARTESIAN_POINT('Ctrl Pts',(-0.0480073595660445,0.232286081287475,
-1.79754805523746));
#67381=CARTESIAN_POINT('Ctrl Pts',(-0.0449781099096792,0.23289156918018,
-1.7977688709484));
#67382=CARTESIAN_POINT('Ctrl Pts',(-0.0419392500630493,0.233437528964708,
-1.79799080372057));
#67383=CARTESIAN_POINT('Ctrl Pts',(-0.0419392741328096,0.233437524640348,
-1.81760526556689));
#67384=CARTESIAN_POINT('Ctrl Pts',(-0.0422246088831205,0.233386261535449,
-1.81758570663374));
#67385=CARTESIAN_POINT('Ctrl Pts',(-0.0425098517635914,0.2333344748991,
-1.81756617774455));
#67386=CARTESIAN_POINT('Ctrl Pts',(-0.0436093707511774,0.233132771009703,
-1.81749098927691));
#67387=CARTESIAN_POINT('Ctrl Pts',(-0.0444229647295536,0.232979111494353,
-1.81743554172198));
#67388=CARTESIAN_POINT('Ctrl Pts',(-0.0465328294537987,0.232569177508753,
-1.81729220175974));
#67389=CARTESIAN_POINT('Ctrl Pts',(-0.0478278138186597,0.232306321405142,
-1.81720466527269));
#67390=CARTESIAN_POINT('Ctrl Pts',(-0.0571309294967675,0.230336881567906,
-1.81657854849105));
#67391=CARTESIAN_POINT('Ctrl Pts',(-0.065049066315338,0.228227237965445,
-1.81606022297569));
#67392=CARTESIAN_POINT('Ctrl Pts',(-0.0771927254296154,0.224308167962868,
-1.81526595629149));
#67393=CARTESIAN_POINT('Ctrl Pts',(-0.0815010573453379,0.222778928322139,
-1.81498431454518));
#67394=CARTESIAN_POINT('Ctrl Pts',(-0.0950381294844814,0.217528645486334,
-1.81409257352345));
#67395=CARTESIAN_POINT('Ctrl Pts',(-0.104077907003057,0.213351217043882,
-1.81348642716782));
#67396=CARTESIAN_POINT('Ctrl Pts',(-0.121850003482557,0.203739416455373,
-1.81223233037505));
#67397=CARTESIAN_POINT('Ctrl Pts',(-0.130544431266464,0.198280824566761,
-1.81158491863131));
#67398=CARTESIAN_POINT('Ctrl Pts',(-0.14068290626407,0.190959078011664,
-1.81076963332027));
#67399=CARTESIAN_POINT('Ctrl Pts',(-0.142489225026791,0.18961505681025,
-1.81062191479122));
#67400=CARTESIAN_POINT('Ctrl Pts',(-0.145324276518914,0.187442202734499,
-1.81038596330318));
#67401=CARTESIAN_POINT('Ctrl Pts',(-0.146365719574649,0.186630117412527,
-1.81029838810508));
#67402=CARTESIAN_POINT('Ctrl Pts',(-0.148316578219735,0.185082525197438,
-1.81013260170882));
#67403=CARTESIAN_POINT('Ctrl Pts',(-0.149227444295666,0.184348903692869,
-1.81005446738617));
#67404=CARTESIAN_POINT('Ctrl Pts',(-0.151273570910773,0.182675829509065,
-1.80987727330228));
#67405=CARTESIAN_POINT('Ctrl Pts',(-0.152405568141666,0.181732480783426,
-1.80977805751174));
#67406=CARTESIAN_POINT('Ctrl Pts',(-0.155734271168668,0.178905535548853,
-1.80948271973171));
#67407=CARTESIAN_POINT('Ctrl Pts',(-0.157905308812134,0.176992276735527,
-1.80928538607277));
#67408=CARTESIAN_POINT('Ctrl Pts',(-0.174578663431968,0.161747658586013,
-1.80773189184986));
#67409=CARTESIAN_POINT('Ctrl Pts',(-0.187401353991968,0.146698463779471,
-1.80629828075995));
#67410=CARTESIAN_POINT('Ctrl Pts',(-0.204857522272324,0.12013211026744,
-1.80397793463329));
#67411=CARTESIAN_POINT('Ctrl Pts',(-0.210718257825865,0.109527225876218,
-1.80309928727604));
#67412=CARTESIAN_POINT('Ctrl Pts',(-0.216364772566557,0.0971622087771301,
-1.80215852130915));
#67413=CARTESIAN_POINT('Ctrl Pts',(-0.216972126623969,0.0957982576953321,
-1.80205585457936));
#67414=CARTESIAN_POINT('Ctrl Pts',(-0.217879783902641,0.0937069860932872,
-1.80190022303876));
#67415=CARTESIAN_POINT('Ctrl Pts',(-0.218189401797958,0.0929837860302456,
-1.80184672541694));
#67416=CARTESIAN_POINT('Ctrl Pts',(-0.218750332982474,0.0916553428999317,
-1.80174906368497));
#67417=CARTESIAN_POINT('Ctrl Pts',(-0.219002737651016,0.0910505957403779,
-1.80170483656576));
#67418=CARTESIAN_POINT('Ctrl Pts',(-0.219569234752227,0.0896773160588872,
-1.80160492273518));
#67419=CARTESIAN_POINT('Ctrl Pts',(-0.219881800926178,0.0889081747601063,
-1.80154932763591));
#67420=CARTESIAN_POINT('Ctrl Pts',(-0.220684310991653,0.0869032941126098,
-1.80140531633062));
#67421=CARTESIAN_POINT('Ctrl Pts',(-0.221167924145811,0.0856650288820689,
-1.80131726185175));
#67422=CARTESIAN_POINT('Ctrl Pts',(-0.2247401280476,0.0762866627949354,
-1.8006565807432));
#67423=CARTESIAN_POINT('Ctrl Pts',(-0.227389185159766,0.0679851086415468,
-1.80010691500392));
#67424=CARTESIAN_POINT('Ctrl Pts',(-0.230600643256581,0.0556055575569116,
-1.79931263554828));
#67425=CARTESIAN_POINT('Ctrl Pts',(-0.23152328552715,0.0516294916798794,
-1.79906128675766));
#67426=CARTESIAN_POINT('Ctrl Pts',(-0.233924859197877,0.039914800132482,
-1.79832692217921));
#67427=CARTESIAN_POINT('Ctrl Pts',(-0.23512139376539,0.0321241326543517,
-1.79784622100817));
#67428=CARTESIAN_POINT('Ctrl Pts',(-0.236754954501028,0.0162563737886748,
-1.79686202282117));
#67429=CARTESIAN_POINT('Ctrl Pts',(-0.237171079224004,0.00818791057595655,
-1.79635888636619));
#67430=CARTESIAN_POINT('Ctrl Pts',(-0.237177386889776,-0.00489263773771135,
-1.79552559647331));
#67431=CARTESIAN_POINT('Ctrl Pts',(-0.237021247212718,-0.00989815163286558,
-1.79520260220827));
#67432=CARTESIAN_POINT('Ctrl Pts',(-0.236590546774835,-0.0167428478078149,
-1.79475343268494));
#67433=CARTESIAN_POINT('Ctrl Pts',(-0.236452615215791,-0.0185895188412432,
-1.79463150321382));
#67434=CARTESIAN_POINT('Ctrl Pts',(-0.236197354986612,-0.0215412274122031,
-1.7944353358585));
#67435=CARTESIAN_POINT('Ctrl Pts',(-0.236093857948845,-0.0226474093072384,
-1.79436153300627));
#67436=CARTESIAN_POINT('Ctrl Pts',(-0.235863988168266,-0.0249311506058672,
-1.79420855168445));
#67437=CARTESIAN_POINT('Ctrl Pts',(-0.235736559883318,-0.0261085700804269,
-1.7941293420643));
#67438=CARTESIAN_POINT('Ctrl Pts',(-0.235417678729328,-0.028862046031564,
-1.79394329057562));
#67439=CARTESIAN_POINT('Ctrl Pts',(-0.235219210106757,-0.030437216405649,
-1.79383623077473));
#67440=CARTESIAN_POINT('Ctrl Pts',(-0.234516717286978,-0.0355946058332425,
-1.79348357812263));
#67441=CARTESIAN_POINT('Ctrl Pts',(-0.233946572451736,-0.0391671466644057,
-1.79323592371365));
#67442=CARTESIAN_POINT('Ctrl Pts',(-0.230898611526427,-0.0558101549525806,
-1.79206575504119));
#67443=CARTESIAN_POINT('Ctrl Pts',(-0.227406010435155,-0.0686683945522261,
-1.79111202140262));
#67444=CARTESIAN_POINT('Ctrl Pts',(-0.217275742243629,-0.0964833165233793,
-1.78895691567429));
#67445=CARTESIAN_POINT('Ctrl Pts',(-0.210131617289113,-0.111187002642677,
-1.78775308456659));
#67446=CARTESIAN_POINT('Ctrl Pts',(-0.200379833773667,-0.126904314738665,
-1.78646109942568));
#67447=CARTESIAN_POINT('Ctrl Pts',(-0.199198687516331,-0.12875040438966,
-1.78630932166144));
#67448=CARTESIAN_POINT('Ctrl Pts',(-0.197522433954854,-0.131292026948759,
-1.78610060423131));
#67449=CARTESIAN_POINT('Ctrl Pts',(-0.197048948808188,-0.132001591223906,
-1.78604236193242));
#67450=CARTESIAN_POINT('Ctrl Pts',(-0.196226903881339,-0.133219226838685,
-1.7859424838881));
#67451=CARTESIAN_POINT('Ctrl Pts',(-0.19588017767724,-0.13372851686052,
-1.78590072932225));
#67452=CARTESIAN_POINT('Ctrl Pts',(-0.195144865043252,-0.134799587714983,
-1.7858129699912));
#67453=CARTESIAN_POINT('Ctrl Pts',(-0.194755829118427,-0.135361051439229,
-1.78576699771368));
#67454=CARTESIAN_POINT('Ctrl Pts',(-0.193782994837488,-0.136752187116081,
-1.78565315086778));
#67455=CARTESIAN_POINT('Ctrl Pts',(-0.193196280224435,-0.137579821085454,
-1.78558547142583));
#67456=CARTESIAN_POINT('Ctrl Pts',(-0.190949105303398,-0.140707017207383,
-1.78532983774709));
#67457=CARTESIAN_POINT('Ctrl Pts',(-0.189252674920491,-0.142980601124255,
-1.78514417188698));
#67458=CARTESIAN_POINT('Ctrl Pts',(-0.184757083241285,-0.148785414851225,
-1.78466905294354));
#67459=CARTESIAN_POINT('Ctrl Pts',(-0.181897276319982,-0.152268399185218,
-1.78438289534952));
#67460=CARTESIAN_POINT('Ctrl Pts',(-0.164516480140254,-0.172247562214298,
-1.78272089550249));
#67461=CARTESIAN_POINT('Ctrl Pts',(-0.14785921584081,-0.186742164664861,
-1.78141946274587));
#67462=CARTESIAN_POINT('Ctrl Pts',(-0.125040611242471,-0.201604657202883,
-1.77968747851324));
#67463=CARTESIAN_POINT('Ctrl Pts',(-0.120543741007083,-0.204325211901945,
-1.77934891109686));
#67464=CARTESIAN_POINT('Ctrl Pts',(-0.114314767229415,-0.207816442661382,
-1.778881445741));
#67465=CARTESIAN_POINT('Ctrl Pts',(-0.112658138334739,-0.208719149512561,
-1.77875726695489));
#67466=CARTESIAN_POINT('Ctrl Pts',(-0.110003152677722,-0.210125049401805,
-1.77855839635612));
#67467=CARTESIAN_POINT('Ctrl Pts',(-0.109011679168349,-0.210641125417597,
-1.77848416211732));
#67468=CARTESIAN_POINT('Ctrl Pts',(-0.106965108404931,-0.211688075262727,
-1.77833097477434));
#67469=CARTESIAN_POINT('Ctrl Pts',(-0.105909621131383,-0.212218113480382,
-1.77825199499501));
#67470=CARTESIAN_POINT('Ctrl Pts',(-0.103445951142906,-0.213432347235163,
-1.77806767684125));
#67471=CARTESIAN_POINT('Ctrl Pts',(-0.102034878831108,-0.21411052041243,
-1.7779621327569));
#67472=CARTESIAN_POINT('Ctrl Pts',(-0.0974570899010838,-0.216255114275751,
-1.77761974459099));
#67473=CARTESIAN_POINT('Ctrl Pts',(-0.0942648210789319,-0.217665569332193,
-1.77738100229604));
#67474=CARTESIAN_POINT('Ctrl Pts',(-0.0866275748507787,-0.220840454617206,
-1.77680957544679));
#67475=CARTESIAN_POINT('Ctrl Pts',(-0.082158197746704,-0.222541834829099,
-1.77647495527151));
#67476=CARTESIAN_POINT('Ctrl Pts',(-0.0641865043012014,-0.228768038151814,
-1.77512873507427));
#67477=CARTESIAN_POINT('Ctrl Pts',(-0.0503411202545978,-0.232207692042918,
-1.77408777640383));
#67478=CARTESIAN_POINT('Ctrl Pts',(-0.0245155959738507,-0.236204374912188,
-1.7721806180759));
#67479=CARTESIAN_POINT('Ctrl Pts',(-0.0126367752292691,-0.237136880421377,
-1.77131716988441));
#67480=CARTESIAN_POINT('Ctrl Pts',(0.000607927362936147,-0.23717803381994,
-1.77040055003912));
#67481=CARTESIAN_POINT('Ctrl Pts',(0.0019528419942021,-0.237170773745787,
-1.77030801200717));
#67482=CARTESIAN_POINT('Ctrl Pts',(0.00413253994607958,-0.237140464487511,
-1.77015898623531));
#67483=CARTESIAN_POINT('Ctrl Pts',(0.00496736861772641,-0.237124446412701,
-1.77010213506341));
#67484=CARTESIAN_POINT('Ctrl Pts',(0.00645759485272556,-0.237087979471249,
-1.77000107592872));
#67485=CARTESIAN_POINT('Ctrl Pts',(0.00711300879699002,-0.23706922128587,
-1.76995677711602));
#67486=CARTESIAN_POINT('Ctrl Pts',(0.00855102537612164,-0.237022095612318,
-1.76985990877358));
#67487=CARTESIAN_POINT('Ctrl Pts',(0.00933357021466848,-0.236992570252592,
-1.7698074037868));
#67488=CARTESIAN_POINT('Ctrl Pts',(0.0115902197694559,-0.236896232152906,
-1.76965655972279));
#67489=CARTESIAN_POINT('Ctrl Pts',(0.0130638978233652,-0.236819536461065,
-1.76955874996291));
#67490=CARTESIAN_POINT('Ctrl Pts',(0.0253880638188002,-0.236062747086201,
-1.7687458952489));
#67491=CARTESIAN_POINT('Ctrl Pts',(0.0361822176882157,-0.234650987420839,
-1.76806687022452));
#67492=CARTESIAN_POINT('Ctrl Pts',(0.0641677279359495,-0.229012717023274,
-1.76630665030344));
#67493=CARTESIAN_POINT('Ctrl Pts',(0.0810472239583556,-0.223597048615859,
-1.7652412307388));
#67494=CARTESIAN_POINT('Ctrl Pts',(0.101881666506948,-0.21424005826287,
-1.76378779691733));
#67495=CARTESIAN_POINT('Ctrl Pts',(0.106524222243309,-0.211969951554247,
-1.7634547492042));
#67496=CARTESIAN_POINT('Ctrl Pts',(0.112744455486857,-0.208672423662257,
-1.76299378543093));
#67497=CARTESIAN_POINT('Ctrl Pts',(0.114389712856402,-0.207775084883823,
-1.76287041795289));
#67498=CARTESIAN_POINT('Ctrl Pts',(0.116996874383364,-0.206312762406059,
-1.76267252287729));
#67499=CARTESIAN_POINT('Ctrl Pts',(0.117965748248855,-0.205760313750698,
-1.76259844466805));
#67500=CARTESIAN_POINT('Ctrl Pts',(0.11995350227874,-0.204608248893662,
-1.76244533559134));
#67501=CARTESIAN_POINT('Ctrl Pts',(0.12097186595071,-0.204007808147772,
-1.76236627645481));
#67502=CARTESIAN_POINT('Ctrl Pts',(0.123334948920558,-0.202590587948241,
-1.76218135087122));
#67503=CARTESIAN_POINT('Ctrl Pts',(0.124676101048679,-0.201767999370211,
-1.76207527443289));
#67504=CARTESIAN_POINT('Ctrl Pts',(0.129003084550629,-0.199054453395888,
-1.76172930739334));
#67505=CARTESIAN_POINT('Ctrl Pts',(0.131954733542683,-0.197110165117121,
-1.76148746241492));
#67506=CARTESIAN_POINT('Ctrl Pts',(0.138861366757028,-0.192336014437533,
-1.76090717699937));
#67507=CARTESIAN_POINT('Ctrl Pts',(0.142774803680835,-0.189449126110858,
-1.76056671881602));
#67508=CARTESIAN_POINT('Ctrl Pts',(0.158172640118204,-0.177342180987372,
-1.75917937912675));
#67509=CARTESIAN_POINT('Ctrl Pts',(0.168874854955217,-0.167182622849758,
-1.75810107048424));
#67510=CARTESIAN_POINT('Ctrl Pts',(0.185967867689111,-0.14762944651732,
-1.75620694932065));
#67511=CARTESIAN_POINT('Ctrl Pts',(0.192759995940159,-0.138643951505345,
-1.75539243536873));
#67512=CARTESIAN_POINT('Ctrl Pts',(0.199627828742628,-0.128072434747595,
-1.75451983334028));
#67513=CARTESIAN_POINT('Ctrl Pts',(0.200356654481993,-0.126929231341742,
-1.7544265371124));
#67514=CARTESIAN_POINT('Ctrl Pts',(0.201520141280725,-0.125069243823416,
-1.75427654022832));
#67515=CARTESIAN_POINT('Ctrl Pts',(0.201960863228489,-0.124356314157022,
-1.75421946852363));
#67516=CARTESIAN_POINT('Ctrl Pts',(0.202739690084116,-0.123081390927575,
-1.75411817812442));
#67517=CARTESIAN_POINT('Ctrl Pts',(0.203079252506474,-0.122520316537109,
-1.75407386674992));
#67518=CARTESIAN_POINT('Ctrl Pts',(0.20381781772885,-0.121288445122501,
-1.75397715921445));
#67519=CARTESIAN_POINT('Ctrl Pts',(0.204215839445421,-0.120617082984172,
-1.75392482608115));
#67520=CARTESIAN_POINT('Ctrl Pts',(0.205350517866711,-0.11868144931886,
-1.75377497137765));
#67521=CARTESIAN_POINT('Ctrl Pts',(0.206078814572423,-0.117412282372357,
-1.75367796849171));
#67522=CARTESIAN_POINT('Ctrl Pts',(0.211806672943705,-0.107213117844503,
-1.75290774765169));
#67523=CARTESIAN_POINT('Ctrl Pts',(0.216235876158186,-0.0979735709636499,
-1.75226642380738));
#67524=CARTESIAN_POINT('Ctrl Pts',(0.226035850376233,-0.0735992866731304,
-1.75064355638263));
#67525=CARTESIAN_POINT('Ctrl Pts',(0.230492965113802,-0.0581553645011969,
-1.74967685505498));
#67526=CARTESIAN_POINT('Ctrl Pts',(0.234611094090271,-0.0354795756479239,
-1.74822626099026));
#67527=CARTESIAN_POINT('Ctrl Pts',(0.235557477819984,-0.0285276333323937,
-1.74777797783194));
#67528=CARTESIAN_POINT('Ctrl Pts',(0.236384563734877,-0.0194601885439522,
-1.74718336595542));
#67529=CARTESIAN_POINT('Ctrl Pts',(0.236547077462784,-0.0173735601452316,
-1.74704586721124));
#67530=CARTESIAN_POINT('Ctrl Pts',(0.23676484115846,-0.0140016025243686,
-1.74682247478272));
#67531=CARTESIAN_POINT('Ctrl Pts',(0.236837287666206,-0.0127174660279749,
-1.74673712124373));
#67532=CARTESIAN_POINT('Ctrl Pts',(0.236956012128841,-0.0102573793628458,
-1.74657304139895));
#67533=CARTESIAN_POINT('Ctrl Pts',(0.237003989296173,-0.00908154650503912,
-1.74649437083388));
#67534=CARTESIAN_POINT('Ctrl Pts',(0.237094413137359,-0.00637019798465789,
-1.74631237410626));
#67535=CARTESIAN_POINT('Ctrl Pts',(0.237130696359459,-0.00483454382221716,
-1.74620885822027));
#67536=CARTESIAN_POINT('Ctrl Pts',(0.237198310614449,2.64541996312906E-5,
-1.74587974756742));
#67537=CARTESIAN_POINT('Ctrl Pts',(0.237174621684088,0.00335203400002923,
-1.74565245432632));
#67538=CARTESIAN_POINT('Ctrl Pts',(0.2369547064943,0.0111619046549588,-1.74511338737453));
#67539=CARTESIAN_POINT('Ctrl Pts',(0.236701093387147,0.0156431745928053,
-1.74479996061432));
#67540=CARTESIAN_POINT('Ctrl Pts',(0.235250107450525,0.0326906265683364,
-1.74359196553677));
#67541=CARTESIAN_POINT('Ctrl Pts',(0.233177587168043,0.0451601412476616,
-1.74267434928164));
#67542=CARTESIAN_POINT('Ctrl Pts',(0.2269511790872,0.0701207250392759,-1.7407954941748));
#67543=CARTESIAN_POINT('Ctrl Pts',(0.222730122529124,0.0825536918064508,
-1.73983724189428));
#67544=CARTESIAN_POINT('Ctrl Pts',(0.216681234592023,0.0964648610074144,
-1.73877923678251));
#67545=CARTESIAN_POINT('Ctrl Pts',(0.215834915283595,0.0983438706615251,
-1.7386366754137));
#67546=CARTESIAN_POINT('Ctrl Pts',(0.214613000457316,0.100965001189892,
-1.73843853357414));
#67547=CARTESIAN_POINT('Ctrl Pts',(0.214257858322897,0.101716476687329,
-1.73838181106852));
#67548=CARTESIAN_POINT('Ctrl Pts',(0.21360873295855,0.103071531058045,-1.73827970324171));
#67549=CARTESIAN_POINT('Ctrl Pts',(0.213316123924634,0.103675757173621,
-1.73823423574815));
#67550=CARTESIAN_POINT('Ctrl Pts',(0.212710923698674,0.104912062061687,
-1.73814134598709));
#67551=CARTESIAN_POINT('Ctrl Pts',(0.212398073293054,0.105544001824988,
-1.73809394019016));
#67552=CARTESIAN_POINT('Ctrl Pts',(0.211582326536876,0.107173446332444,
-1.73797187517052));
#67553=CARTESIAN_POINT('Ctrl Pts',(0.211075185793868,0.108168824374664,
-1.73789747474233));
#67554=CARTESIAN_POINT('Ctrl Pts',(0.208862697158191,0.112436516503552,
-1.73757903537841));
#67555=CARTESIAN_POINT('Ctrl Pts',(0.207088041319392,0.115672569411573,
-1.73733897914664));
#67556=CARTESIAN_POINT('Ctrl Pts',(0.201922935750103,0.124590825931142,
-1.736677637795));
#67557=CARTESIAN_POINT('Ctrl Pts',(0.198369079184624,0.130174755778603,
-1.73626378564027));
#67558=CARTESIAN_POINT('Ctrl Pts',(0.193033220000682,0.137831541864277,
-1.73568620926313));
#67559=CARTESIAN_POINT('Ctrl Pts',(0.191442108753656,0.140033129471458,
-1.73551890247147));
#67560=CARTESIAN_POINT('Ctrl Pts',(0.178188503943821,0.157723640797833,
-1.73416049422983));
#67561=CARTESIAN_POINT('Ctrl Pts',(0.1647062533374,0.171754641608623,-1.73298659682459));
#67562=CARTESIAN_POINT('Ctrl Pts',(0.147366681848749,0.185859726015681,
-1.73153946368953));
#67563=CARTESIAN_POINT('Ctrl Pts',(0.145031142214995,0.187687887685678,
-1.73134586580446));
#67564=CARTESIAN_POINT('Ctrl Pts',(0.141488995430069,0.190354933909949,
-1.73105383595194));
#67565=CARTESIAN_POINT('Ctrl Pts',(0.14030781839386,0.191227227731517,-1.73095671196292));
#67566=CARTESIAN_POINT('Ctrl Pts',(0.138171812430985,0.192774214007054,
-1.73078149195571));
#67567=CARTESIAN_POINT('Ctrl Pts',(0.137219942716272,0.193452925988174,
-1.73070355451308));
#67568=CARTESIAN_POINT('Ctrl Pts',(0.135179492918029,0.194885192098844,
-1.73053677350147));
#67569=CARTESIAN_POINT('Ctrl Pts',(0.134089546961815,0.195636721187718,
-1.73044785613788));
#67570=CARTESIAN_POINT('Ctrl Pts',(0.131116572785768,0.19765010221744,-1.73020575110217));
#67571=CARTESIAN_POINT('Ctrl Pts',(0.129221695166951,0.198894121183745,
-1.73005190111323));
#67572=CARTESIAN_POINT('Ctrl Pts',(0.118408184374765,0.20577361584526,-1.72917623250012));
#67573=CARTESIAN_POINT('Ctrl Pts',(0.109140421937473,0.210835458194456,
-1.72843370813801));
#67574=CARTESIAN_POINT('Ctrl Pts',(0.0855207006109245,0.221760510941409,
-1.72656335808938));
#67575=CARTESIAN_POINT('Ctrl Pts',(0.0708724869390377,0.226866839570555,
-1.72542037123355));
#67576=CARTESIAN_POINT('Ctrl Pts',(0.0490219580523127,0.232159263702428,
-1.72379822044009));
#67577=CARTESIAN_POINT('Ctrl Pts',(0.0421415614799232,0.233506285169764,
-1.72329939002018));
#67578=CARTESIAN_POINT('Ctrl Pts',(0.0338275761943979,0.234754409094052,
-1.72271820866506));
#67579=CARTESIAN_POINT('Ctrl Pts',(0.0324423417790905,0.234949850388549,
-1.72262209023703));
#67580=CARTESIAN_POINT('Ctrl Pts',(0.0302867495638811,0.235234552274076,
-1.72247371153436));
#67581=CARTESIAN_POINT('Ctrl Pts',(0.0295175741385323,0.235332306841149,
-1.72242100142236));
#67582=CARTESIAN_POINT('Ctrl Pts',(0.0280964304667106,0.235505842786432,
-1.72232406493486));
#67583=CARTESIAN_POINT('Ctrl Pts',(0.0274446264459685,0.235582690129883,
-1.72227978236074));
#67584=CARTESIAN_POINT('Ctrl Pts',(0.0259529424472506,0.235752283864299,
-1.72217883750642));
#67585=CARTESIAN_POINT('Ctrl Pts',(0.0251128787018391,0.235843248678904,
-1.72212227503345));
#67586=CARTESIAN_POINT('Ctrl Pts',(0.0224970179996491,0.236112367103913,
-1.72194698558677));
#67587=CARTESIAN_POINT('Ctrl Pts',(0.0207196346509031,0.236274973133956,
-1.72182908534887));
#67588=CARTESIAN_POINT('Ctrl Pts',(0.0062656107358857,0.237432953073083,
-1.72087881991969));
#67589=CARTESIAN_POINT('Ctrl Pts',(-0.00647229680483934,0.237427598613414,
-1.72009394717104));
#67590=CARTESIAN_POINT('Ctrl Pts',(-0.0267963352841244,0.235781232699088,
-1.71884247966409));
#67591=CARTESIAN_POINT('Ctrl Pts',(-0.0344016266277004,0.234791736067342,
-1.7183744766436));
#67592=CARTESIAN_POINT('Ctrl Pts',(-0.0419393124730365,0.233437517752158,
-1.71790170279738));
#67593=CARTESIAN_POINT('Origin',(0.,0.,-2.1456589891905));
#67594=CARTESIAN_POINT('',(-0.0419392741218017,0.233437524642326,-1.59829545246927));
#67595=CARTESIAN_POINT('',(-0.0419392757399419,0.233437524351611,-1.61803181050061));
#67596=CARTESIAN_POINT('',(-0.0419392741328076,0.233437524640348,-2.1456589891905));
#67597=CARTESIAN_POINT('',(-0.237174999934351,-5.58036924603097E-6,-1.6761644476277));
#67598=CARTESIAN_POINT('Ctrl Pts',(-0.0419392741218017,0.233437524642326,
-1.59829545246927));
#67599=CARTESIAN_POINT('Ctrl Pts',(-0.0413949734322705,0.233535313444096,
-1.59833049339946));
#67600=CARTESIAN_POINT('Ctrl Pts',(-0.0408503180760221,0.233631200819013,
-1.59836547307769));
#67601=CARTESIAN_POINT('Ctrl Pts',(-0.0261237725611548,0.236170756412341,
-1.59930911111679));
#67602=CARTESIAN_POINT('Ctrl Pts',(-0.0117482039028465,0.237320697836993,
-1.6001779974016));
#67603=CARTESIAN_POINT('Ctrl Pts',(0.0155055078283608,0.237016889532454,
-1.60185623824416));
#67604=CARTESIAN_POINT('Ctrl Pts',(0.0283326117277322,0.235827531878034,
-1.60265931191078));
#67605=CARTESIAN_POINT('Ctrl Pts',(0.0433522038510075,0.233191498241831,
-1.60365171553424));
#67606=CARTESIAN_POINT('Ctrl Pts',(0.0456988912846523,0.232742989339567,
-1.60380824990311));
#67607=CARTESIAN_POINT('Ctrl Pts',(0.0493747370613882,0.23198271128988,
-1.60405596363868));
#67608=CARTESIAN_POINT('Ctrl Pts',(0.0507087042723419,0.231694778051929,
-1.60414638338378));
#67609=CARTESIAN_POINT('Ctrl Pts',(0.0531667062711942,0.231141981113734,
-1.6043139969158));
#67610=CARTESIAN_POINT('Ctrl Pts',(0.0542914404429776,0.23088038786852,
-1.60439108366358));
#67611=CARTESIAN_POINT('Ctrl Pts',(0.0567851649177315,0.230281162352141,
-1.60456288717164));
#67612=CARTESIAN_POINT('Ctrl Pts',(0.0581531358986633,0.229939516666364,
-1.60465773071789));
#67613=CARTESIAN_POINT('Ctrl Pts',(0.0621051226769359,0.22891500090963,
-1.60493350641761));
#67614=CARTESIAN_POINT('Ctrl Pts',(0.0646806727077449,0.228200642995041,
-1.60511544666754));
#67615=CARTESIAN_POINT('Ctrl Pts',(0.0797593891788329,0.223742620004651,
-1.60619412201389));
#67616=CARTESIAN_POINT('Ctrl Pts',(0.0919463914150931,0.219016163076366,
-1.60712275880188));
#67617=CARTESIAN_POINT('Ctrl Pts',(0.115478999887907,0.207578063856908,
-1.60902104079597));
#67618=CARTESIAN_POINT('Ctrl Pts',(0.126780616184222,0.200874907416396,
-1.60998749903883));
#67619=CARTESIAN_POINT('Ctrl Pts',(0.142547492591773,0.189660264730919,
-1.61137876604397));
#67620=CARTESIAN_POINT('Ctrl Pts',(0.147481153179584,0.185849746311779,
-1.61182075172669));
#67621=CARTESIAN_POINT('Ctrl Pts',(0.153298359573892,0.180979086231881,
-1.61234488653896));
#67622=CARTESIAN_POINT('Ctrl Pts',(0.154329849179837,0.180100290311074,
-1.6124379422448));
#67623=CARTESIAN_POINT('Ctrl Pts',(0.155932290767049,0.178711184568227,
-1.61258261577368));
#67624=CARTESIAN_POINT('Ctrl Pts',(0.156508379807423,0.178206885067961,
-1.61263464939922));
#67625=CARTESIAN_POINT('Ctrl Pts',(0.157570181228333,0.177268280053452,
-1.61273057893336));
#67626=CARTESIAN_POINT('Ctrl Pts',(0.1580565452793,0.176834763649822,-1.61277452801657));
#67627=CARTESIAN_POINT('Ctrl Pts',(0.159177733372892,0.17582708106696,-1.61287586843687));
#67628=CARTESIAN_POINT('Ctrl Pts',(0.159811241793498,0.175251477288967,
-1.61293315121102));
#67629=CARTESIAN_POINT('Ctrl Pts',(0.16179816855889,0.173426428275415,-1.61311293510964));
#67630=CARTESIAN_POINT('Ctrl Pts',(0.163140195008985,0.172164603393105,
-1.61323454790499));
#67631=CARTESIAN_POINT('Ctrl Pts',(0.166281119511135,0.169141675263853,
-1.61352000616053));
#67632=CARTESIAN_POINT('Ctrl Pts',(0.16806697907303,0.167367286711644,-1.61368297513337));
#67633=CARTESIAN_POINT('Ctrl Pts',(0.174545201819023,0.160722394205297,
-1.61427819753519));
#67634=CARTESIAN_POINT('Ctrl Pts',(0.1790571657802,0.155679993082782,-1.61470086562913));
#67635=CARTESIAN_POINT('Ctrl Pts',(0.193177831506098,0.138471819306723,
-1.61607751793761));
#67636=CARTESIAN_POINT('Ctrl Pts',(0.201810001450371,0.125558124101835,
-1.61701188170121));
#67637=CARTESIAN_POINT('Ctrl Pts',(0.212784142470918,0.105048462862456,
-1.61847031792467));
#67638=CARTESIAN_POINT('Ctrl Pts',(0.216108627861405,0.0980271018759928,
-1.61896505258933));
#67639=CARTESIAN_POINT('Ctrl Pts',(0.219911011325856,0.0888583373384086,
-1.61961276853596));
#67640=CARTESIAN_POINT('Ctrl Pts',(0.220712028667404,0.0868496223938283,
-1.61975475479359));
#67641=CARTESIAN_POINT('Ctrl Pts',(0.221950990051769,0.0836147882397324,
-1.61998367948646));
#67642=CARTESIAN_POINT('Ctrl Pts',(0.222406512295942,0.082395497273673,
-1.62007002743457));
#67643=CARTESIAN_POINT('Ctrl Pts',(0.223253593823615,0.0800699104714561,
-1.62023486571211));
#67644=CARTESIAN_POINT('Ctrl Pts',(0.223647024587239,0.0789643338852406,
-1.62031329085876));
#67645=CARTESIAN_POINT('Ctrl Pts',(0.224526985280065,0.0764322257864434,
-1.62049307136517));
#67646=CARTESIAN_POINT('Ctrl Pts',(0.225008149815646,0.0750038971754316,
-1.6205946006837));
#67647=CARTESIAN_POINT('Ctrl Pts',(0.226458168703679,0.0705599792611813,
-1.62091090327736));
#67648=CARTESIAN_POINT('Ctrl Pts',(0.227380217964405,0.0675296056053373,
-1.62112719237233));
#67649=CARTESIAN_POINT('Ctrl Pts',(0.229386152900982,0.0604293519272302,
-1.62163558522881));
#67650=CARTESIAN_POINT('Ctrl Pts',(0.230422839012534,0.0563473620230462,
-1.62192909662139));
#67651=CARTESIAN_POINT('Ctrl Pts',(0.233833177876745,0.0412443651867521,
-1.62301962732722));
#67652=CARTESIAN_POINT('Ctrl Pts',(0.235528749373441,0.0300867145550502,
-1.6238350251399));
#67653=CARTESIAN_POINT('Ctrl Pts',(0.237624724114097,0.00380089811443625,
-1.62575870348746));
#67654=CARTESIAN_POINT('Ctrl Pts',(0.237384977223515,-0.0113316018646385,
-1.62686903423174));
#67655=CARTESIAN_POINT('Ctrl Pts',(0.235486256780553,-0.0283228907579257,
-1.62806030653738));
#67656=CARTESIAN_POINT('Ctrl Pts',(0.235239595441707,-0.030303410158227,
-1.62819825814928));
#67657=CARTESIAN_POINT('Ctrl Pts',(0.234857787833126,-0.0330825526157371,
-1.62839034852503));
#67658=CARTESIAN_POINT('Ctrl Pts',(0.234743514883374,-0.0338838908928301,
-1.62844556132753));
#67659=CARTESIAN_POINT('Ctrl Pts',(0.234527749747542,-0.035343439573764,
-1.62854578780731));
#67660=CARTESIAN_POINT('Ctrl Pts',(0.234427583449303,-0.0360018372403216,
-1.62859087400398));
#67661=CARTESIAN_POINT('Ctrl Pts',(0.234214139111045,-0.0373661446680005,
-1.62868402845268));
#67662=CARTESIAN_POINT('Ctrl Pts',(0.234100440947087,-0.0380719753836788,
-1.62873207294345));
#67663=CARTESIAN_POINT('Ctrl Pts',(0.233793764919076,-0.0399224693310695,
-1.62885766585968));
#67664=CARTESIAN_POINT('Ctrl Pts',(0.233595569306069,-0.0410662660881281,
-1.62893492673946));
#67665=CARTESIAN_POINT('Ctrl Pts',(0.232655255169041,-0.0462656568579803,
-1.62928464530654));
#67666=CARTESIAN_POINT('Ctrl Pts',(0.231815813809006,-0.0503032028047273,
-1.6295520886842));
#67667=CARTESIAN_POINT('Ctrl Pts',(0.229069316080241,-0.061977022304927,
-1.63031871594378));
#67668=CARTESIAN_POINT('Ctrl Pts',(0.226886923580297,-0.0695431197798385,
-1.63080731984747));
#67669=CARTESIAN_POINT('Ctrl Pts',(0.218115398944938,-0.095102373304124,
-1.63247117722391));
#67670=CARTESIAN_POINT('Ctrl Pts',(0.209728011531457,-0.112396144146593,
-1.63362659751256));
#67671=CARTESIAN_POINT('Ctrl Pts',(0.197362698131944,-0.13158054532031,
-1.63509467646254));
#67672=CARTESIAN_POINT('Ctrl Pts',(0.195301209558607,-0.134621356780313,
-1.63533329059811));
#67673=CARTESIAN_POINT('Ctrl Pts',(0.192312151569573,-0.138817156949249,
-1.63567164988855));
#67674=CARTESIAN_POINT('Ctrl Pts',(0.191443052722284,-0.140013299739052,
-1.63576917818688));
#67675=CARTESIAN_POINT('Ctrl Pts',(0.189911135091101,-0.142080750622941,
-1.63593966554805));
#67676=CARTESIAN_POINT('Ctrl Pts',(0.189253355222977,-0.142955749787963,
-1.63601242797433));
#67677=CARTESIAN_POINT('Ctrl Pts',(0.18786376721004,-0.144777823008143,
-1.63616524394636));
#67678=CARTESIAN_POINT('Ctrl Pts',(0.187130802085842,-0.145723971553174,
-1.63624534168774));
#67679=CARTESIAN_POINT('Ctrl Pts',(0.185364857989815,-0.147968247098068,
-1.63643714665675));
#67680=CARTESIAN_POINT('Ctrl Pts',(0.184325370326003,-0.149261148116954,
-1.63654911142046));
#67681=CARTESIAN_POINT('Ctrl Pts',(0.180703527281388,-0.153670412735909,
-1.63693611973467));
#67682=CARTESIAN_POINT('Ctrl Pts',(0.178055145383202,-0.156731369612234,
-1.63721381912614));
#67683=CARTESIAN_POINT('Ctrl Pts',(0.160653110548373,-0.175833805542629,
-1.639006847277));
#67684=CARTESIAN_POINT('Ctrl Pts',(0.143827426909285,-0.189842733681717,
-1.64061450061909));
#67685=CARTESIAN_POINT('Ctrl Pts',(0.12458568285217,-0.201819625353787,
-1.64225777891425));
#67686=CARTESIAN_POINT('Ctrl Pts',(0.123836716298305,-0.202280056526028,
-1.64232144152219));
#67687=CARTESIAN_POINT('Ctrl Pts',(0.120111675296871,-0.204541602126206,
-1.64263653581542));
#67688=CARTESIAN_POINT('Ctrl Pts',(0.117098670355735,-0.206281324546274,
-1.64288657011153));
#67689=CARTESIAN_POINT('Ctrl Pts',(0.110150669761161,-0.210091818195628,
-1.64345068357491));
#67690=CARTESIAN_POINT('Ctrl Pts',(0.10619332500407,-0.212119603072217,
-1.64376315946186));
#67691=CARTESIAN_POINT('Ctrl Pts',(0.101065179174825,-0.214567795967495,
-1.64415488220214));
#67692=CARTESIAN_POINT('Ctrl Pts',(0.0999451565232579,-0.215091783576791,
-1.64423964836462));
#67693=CARTESIAN_POINT('Ctrl Pts',(0.0981559607496579,-0.215911841441022,
-1.64437374925309));
#67694=CARTESIAN_POINT('Ctrl Pts',(0.0974894460041401,-0.216213607018129,
-1.64442341769012));
#67695=CARTESIAN_POINT('Ctrl Pts',(0.0962134395366314,-0.21678422083649,
-1.64451794301122));
#67696=CARTESIAN_POINT('Ctrl Pts',(0.095604202864094,-0.217053589595494,
-1.64456282941928));
#67697=CARTESIAN_POINT('Ctrl Pts',(0.0941485192184657,-0.217689889603353,
-1.64466951028082));
#67698=CARTESIAN_POINT('Ctrl Pts',(0.0933010406874348,-0.218054460133688,
-1.6447311627555));
#67699=CARTESIAN_POINT('Ctrl Pts',(0.0904060112228617,-0.219279883122465,
-1.64494029382484));
#67700=CARTESIAN_POINT('Ctrl Pts',(0.0883484308578926,-0.220116945397696,
-1.64508642347101));
#67701=CARTESIAN_POINT('Ctrl Pts',(0.083276931842472,-0.222097551381693,
-1.64544121499253));
#67702=CARTESIAN_POINT('Ctrl Pts',(0.0802508133774784,-0.223208823270988,
-1.64564831534385));
#67703=CARTESIAN_POINT('Ctrl Pts',(0.0675510058753456,-0.227580843852173,
-1.64650212849881));
#67704=CARTESIAN_POINT('Ctrl Pts',(0.0576939746507311,-0.230277258892178,
-1.64712851635495));
#67705=CARTESIAN_POINT('Ctrl Pts',(0.0311626151990876,-0.235723668564269,
-1.64878880045725));
#67706=CARTESIAN_POINT('Ctrl Pts',(0.0143191388386974,-0.237342864681485,
-1.64982015376749));
#67707=CARTESIAN_POINT('Ctrl Pts',(-0.00571599421691471,-0.237127213773188,
-1.65111512222287));
#67708=CARTESIAN_POINT('Ctrl Pts',(-0.00887814354972187,-0.237029882352843,
-1.65132136430564));
#67709=CARTESIAN_POINT('Ctrl Pts',(-0.0135418026440606,-0.236792883404537,
-1.65162872000869));
#67710=CARTESIAN_POINT('Ctrl Pts',(-0.0150455296281969,-0.236702095284314,
-1.65172831045588));
#67711=CARTESIAN_POINT('Ctrl Pts',(-0.0177188107137425,-0.236515118462665,
-1.65190627447209));
#67712=CARTESIAN_POINT('Ctrl Pts',(-0.0188887182533277,-0.236424562497925,
-1.65198446907519));
#67713=CARTESIAN_POINT('Ctrl Pts',(-0.0213552248115881,-0.236215220097435,
-1.65215000743558));
#67714=CARTESIAN_POINT('Ctrl Pts',(-0.0226516100724843,-0.236094430845322,
-1.65223741161772));
#67715=CARTESIAN_POINT('Ctrl Pts',(-0.0261001806599078,-0.235744449584559,
-1.65247101203827));
#67716=CARTESIAN_POINT('Ctrl Pts',(-0.0282502914752019,-0.235496465854739,
-1.6526177931089));
#67717=CARTESIAN_POINT('Ctrl Pts',(-0.0391383057254565,-0.234089440979614,
-1.65336706789977));
#67718=CARTESIAN_POINT('Ctrl Pts',(-0.0478091099154606,-0.232473500080804,
-1.65398374875289));
#67719=CARTESIAN_POINT('Ctrl Pts',(-0.0671943387794745,-0.227730333746132,
-1.6554076783253));
#67720=CARTESIAN_POINT('Ctrl Pts',(-0.0778187542503669,-0.224322067731814,
-1.65622077518125));
#67721=CARTESIAN_POINT('Ctrl Pts',(-0.0994633979154409,-0.215655227443034,
-1.65792353899741));
#67722=CARTESIAN_POINT('Ctrl Pts',(-0.110399512114428,-0.210266857668785,
-1.65881090526219));
#67723=CARTESIAN_POINT('Ctrl Pts',(-0.12265490928234,-0.203007478089665,
-1.65980447447126));
#67724=CARTESIAN_POINT('Ctrl Pts',(-0.124421567514111,-0.201929535224735,
-1.65994765152851));
#67725=CARTESIAN_POINT('Ctrl Pts',(-0.126941264798086,-0.200346492504208,
-1.66015154053104));
#67726=CARTESIAN_POINT('Ctrl Pts',(-0.12770581270293,-0.199860019105865,
-1.66021336352036));
#67727=CARTESIAN_POINT('Ctrl Pts',(-0.129018981398303,-0.199013852198732,
-1.66031944990293));
#67728=CARTESIAN_POINT('Ctrl Pts',(-0.129568928424485,-0.198656245203887,
-1.6603638476303));
#67729=CARTESIAN_POINT('Ctrl Pts',(-0.130629593675061,-0.197960261613705,
-1.66044940783192));
#67730=CARTESIAN_POINT('Ctrl Pts',(-0.131140489568088,-0.197622184836077,
-1.66049059050903));
#67731=CARTESIAN_POINT('Ctrl Pts',(-0.132550158912963,-0.19668148594751,
-1.66060415736031));
#67732=CARTESIAN_POINT('Ctrl Pts',(-0.133446141143098,-0.196074677275335,
-1.66067626686307));
#67733=CARTESIAN_POINT('Ctrl Pts',(-0.137117779568356,-0.193551214581425,
-1.66097160074371));
#67734=CARTESIAN_POINT('Ctrl Pts',(-0.139856701605216,-0.191581481382912,
-1.66119152444396));
#67735=CARTESIAN_POINT('Ctrl Pts',(-0.147172934558227,-0.186079352714719,
-1.66178070692516));
#67736=CARTESIAN_POINT('Ctrl Pts',(-0.151664788468511,-0.182436836735152,
-1.66214435185298));
#67737=CARTESIAN_POINT('Ctrl Pts',(-0.169258844545271,-0.167070112726255,
-1.66359678140266));
#67738=CARTESIAN_POINT('Ctrl Pts',(-0.1811716340073,-0.154070887154443,
-1.66465066145245));
#67739=CARTESIAN_POINT('Ctrl Pts',(-0.195797262466384,-0.134043094438326,
-1.6662098858082));
#67740=CARTESIAN_POINT('Ctrl Pts',(-0.199786798348596,-0.128020852332756,
-1.66667102606022));
#67741=CARTESIAN_POINT('Ctrl Pts',(-0.204580115768191,-0.120014240902144,
-1.66728030973783));
#67742=CARTESIAN_POINT('Ctrl Pts',(-0.205640747018169,-0.118187666354509,
-1.6674190492857));
#67743=CARTESIAN_POINT('Ctrl Pts',(-0.207309952707263,-0.115222523554017,
-1.66764398540523));
#67744=CARTESIAN_POINT('Ctrl Pts',(-0.207933889060767,-0.114092699563961,
-1.66772962820959));
#67745=CARTESIAN_POINT('Ctrl Pts',(-0.209108715401395,-0.111923675214683,
-1.6678939484224));
#67746=CARTESIAN_POINT('Ctrl Pts',(-0.20966115893827,-0.110885356458971,
-1.66797256749072));
#67747=CARTESIAN_POINT('Ctrl Pts',(-0.210913680279988,-0.108488414087502,
-1.66815398618416));
#67748=CARTESIAN_POINT('Ctrl Pts',(-0.211608387434762,-0.107127058660382,
-1.66825697118826));
#67749=CARTESIAN_POINT('Ctrl Pts',(-0.213753108207485,-0.102821968548953,
-1.66858253831989));
#67750=CARTESIAN_POINT('Ctrl Pts',(-0.215155161109763,-0.099854911012428,
-1.66880676691892));
#67751=CARTESIAN_POINT('Ctrl Pts',(-0.218296098698196,-0.0928344812107769,
-1.669337227123));
#67752=CARTESIAN_POINT('Ctrl Pts',(-0.219984321796218,-0.0887599091338202,
-1.66964504032935));
#67753=CARTESIAN_POINT('Ctrl Pts',(-0.225920895096946,-0.0732201963942533,
-1.67081877307354));
#67754=CARTESIAN_POINT('Ctrl Pts',(-0.229393855406376,-0.0614804579089014,
-1.67170631270962));
#67755=CARTESIAN_POINT('Ctrl Pts',(-0.234975782045599,-0.0353388640426506,
-1.6736582750488));
#67756=CARTESIAN_POINT('Ctrl Pts',(-0.236697422564825,-0.020901481585207,
-1.67472107080143));
#67757=CARTESIAN_POINT('Ctrl Pts',(-0.237127843845484,-0.00494658693984074,
-1.67582647678214));
#67758=CARTESIAN_POINT('Ctrl Pts',(-0.237153654686387,-0.00349676692401314,
-1.67592628109097));
#67759=CARTESIAN_POINT('Ctrl Pts',(-0.237170415107311,-0.00155466799264505,
-1.67605903166901));
#67760=CARTESIAN_POINT('Ctrl Pts',(-0.237173130369242,-0.0010625612894877,
-1.6760925882354));
#67761=CARTESIAN_POINT('Ctrl Pts',(-0.237174766855387,-0.000382157342303444,
-1.67613886949327));
#67762=CARTESIAN_POINT('Ctrl Pts',(-0.237174995504198,-0.000193869267784506,
-1.67615166469862));
#67763=CARTESIAN_POINT('Ctrl Pts',(-0.237174999934351,-5.58036924603097E-6,
-1.6761644476277));
#67764=CARTESIAN_POINT('Ctrl Pts',(-0.237174999935275,-5.54095249315624E-6,
-1.6761644503037));
#67765=CARTESIAN_POINT('Ctrl Pts',(-0.237175003412458,0.000143296411532458,
-1.67617455486763));
#67766=CARTESIAN_POINT('Ctrl Pts',(-0.237174866787022,0.00029213433142796,
-1.67618465176352));
#67767=CARTESIAN_POINT('Ctrl Pts',(-0.237173764301833,0.000885099671302591,
-1.67622484650095));
#67768=CARTESIAN_POINT('Ctrl Pts',(-0.237171691051888,0.00132922972991396,
-1.67625488299834));
#67769=CARTESIAN_POINT('Ctrl Pts',(-0.237163054307791,0.0024843037420253,
-1.67633281664781));
#67770=CARTESIAN_POINT('Ctrl Pts',(-0.237154541646107,0.00319523146845797,
-1.67638060341992));
#67771=CARTESIAN_POINT('Ctrl Pts',(-0.237124732704956,0.00500494879468164,
-1.676501814298));
#67772=CARTESIAN_POINT('Ctrl Pts',(-0.237098995752081,0.00610366309204758,
-1.67657499664219));
#67773=CARTESIAN_POINT('Ctrl Pts',(-0.236962674218472,0.0105907941415603,
-1.67687235438578));
#67774=CARTESIAN_POINT('Ctrl Pts',(-0.236787076666774,0.0139770201528288,
-1.67709322101093));
#67775=CARTESIAN_POINT('Ctrl Pts',(-0.236333966548885,0.0201514036218907,
-1.67749138378574));
#67776=CARTESIAN_POINT('Ctrl Pts',(-0.236079553186763,0.0229405448033126,
-1.67766953876236));
#67777=CARTESIAN_POINT('Ctrl Pts',(-0.233709624884289,0.0446618178700894,
-1.6790481268826));
#67778=CARTESIAN_POINT('Ctrl Pts',(-0.2293695077312,0.0632818324143625,
-1.68018283632627));
#67779=CARTESIAN_POINT('Ctrl Pts',(-0.220905147427721,0.0865165795628418,
-1.68172833276153));
#67780=CARTESIAN_POINT('Ctrl Pts',(-0.218771413377802,0.0917783445964427,
-1.68208705324888));
#67781=CARTESIAN_POINT('Ctrl Pts',(-0.214828922389161,0.10057962302854,
-1.68270634029631));
#67782=CARTESIAN_POINT('Ctrl Pts',(-0.213116199490399,0.104159536366658,
-1.68296384762949));
#67783=CARTESIAN_POINT('Ctrl Pts',(-0.210567004580605,0.109161475097841,
-1.68333255980468));
#67784=CARTESIAN_POINT('Ctrl Pts',(-0.209804210028063,0.110620451497574,
-1.68344120307412));
#67785=CARTESIAN_POINT('Ctrl Pts',(-0.208461824726874,0.113124158890964,
-1.68362960511825));
#67786=CARTESIAN_POINT('Ctrl Pts',(-0.20788940827443,0.114172682946437,
-1.68370910777592));
#67787=CARTESIAN_POINT('Ctrl Pts',(-0.206776031325403,0.116175977033382,
-1.68386218600479));
#67788=CARTESIAN_POINT('Ctrl Pts',(-0.206236316398129,0.117131406969948,
-1.68393571540357));
#67789=CARTESIAN_POINT('Ctrl Pts',(-0.204948486762792,0.119374689900586,
-1.68410961031858));
#67790=CARTESIAN_POINT('Ctrl Pts',(-0.204194840163119,0.120659296738656,
-1.68421017382159));
#67791=CARTESIAN_POINT('Ctrl Pts',(-0.20150703271411,0.125143413758136,
-1.68456473169383));
#67792=CARTESIAN_POINT('Ctrl Pts',(-0.199509453618836,0.128304066147017,
-1.68482101947851));
#67793=CARTESIAN_POINT('Ctrl Pts',(-0.18339732705697,0.152510759688757,
-1.68683525745198));
#67794=CARTESIAN_POINT('Ctrl Pts',(-0.166067080113734,0.171217097387719,
-1.68872542029754));
#67795=CARTESIAN_POINT('Ctrl Pts',(-0.143196532691493,0.189104367221874,
-1.69080483405225));
#67796=CARTESIAN_POINT('Ctrl Pts',(-0.140224753548115,0.191318400208875,
-1.69106779016169));
#67797=CARTESIAN_POINT('Ctrl Pts',(-0.135193480051496,0.194886550803115,
-1.69149961849899));
#67798=CARTESIAN_POINT('Ctrl Pts',(-0.133162637147586,0.196279795188257,
-1.69167043611682));
#67799=CARTESIAN_POINT('Ctrl Pts',(-0.130492895897082,0.19805083639496,
-1.69189013149301));
#67800=CARTESIAN_POINT('Ctrl Pts',(-0.129873500436236,0.198457561200043,
-1.69194076727626));
#67801=CARTESIAN_POINT('Ctrl Pts',(-0.128664819944472,0.199243156716865,
-1.69203891232782));
#67802=CARTESIAN_POINT('Ctrl Pts',(-0.128075742800216,0.199622332238864,
-1.6920864409107));
#67803=CARTESIAN_POINT('Ctrl Pts',(-0.126943583072925,0.200344003040888,
-1.69217719191584));
#67804=CARTESIAN_POINT('Ctrl Pts',(-0.126400781153951,0.200686908820421,
-1.69222044007238));
#67805=CARTESIAN_POINT('Ctrl Pts',(-0.125088546889456,0.201508454316071,
-1.69232437979053));
#67806=CARTESIAN_POINT('Ctrl Pts',(-0.124317740655207,0.201984903270952,
-1.69238492892121));
#67807=CARTESIAN_POINT('Ctrl Pts',(-0.121777859780622,0.20353480114067,
-1.69258285720489));
#67808=CARTESIAN_POINT('Ctrl Pts',(-0.119997408367916,0.204589552782499,
-1.69271909338105));
#67809=CARTESIAN_POINT('Ctrl Pts',(-0.107663265693049,0.211679962274617,
-1.6936473766617));
#67810=CARTESIAN_POINT('Ctrl Pts',(-0.0966715123753824,0.216920446875706,
-1.69439795221352));
#67811=CARTESIAN_POINT('Ctrl Pts',(-0.0752178915824162,0.22519234343167,
-1.69580926644089));
#67812=CARTESIAN_POINT('Ctrl Pts',(-0.0648557486026952,0.228392304754425,
-1.69646929077252));
#67813=CARTESIAN_POINT('Ctrl Pts',(-0.0502099450086752,0.231837650920918,
-1.69740741540228));
#67814=CARTESIAN_POINT('Ctrl Pts',(-0.0460843784969549,0.232692817260734,
-1.6976721470331));
#67815=CARTESIAN_POINT('Ctrl Pts',(-0.0419392692346775,0.233437525520344,
-1.69793969278784));
#67816=CARTESIAN_POINT('',(-0.237174910032345,-0.000206582064046445,-1.69575651031441));
#67817=CARTESIAN_POINT('Ctrl Pts',(-0.0419393124730366,0.233437517752158,
-1.71790170279738));
#67818=CARTESIAN_POINT('Ctrl Pts',(-0.052470414665017,0.231545503178974,
-1.71724117783118));
#67819=CARTESIAN_POINT('Ctrl Pts',(-0.0628695321719981,0.228941590339487,
-1.71657092986479));
#67820=CARTESIAN_POINT('Ctrl Pts',(-0.0759806226596189,0.22469605505406,
-1.71567946392309));
#67821=CARTESIAN_POINT('Ctrl Pts',(-0.0788774560950214,0.223695591578132,
-1.71547954587856));
#67822=CARTESIAN_POINT('Ctrl Pts',(-0.0831502404666846,0.222126609230186,
-1.71517985700841));
#67823=CARTESIAN_POINT('Ctrl Pts',(-0.0845416118194761,0.221600786819642,
-1.71508149983606));
#67824=CARTESIAN_POINT('Ctrl Pts',(-0.0870192971135828,0.220637697656498,
-1.71490492890357));
#67825=CARTESIAN_POINT('Ctrl Pts',(-0.0881075014422767,0.220205403663207,
-1.71482688398868));
#67826=CARTESIAN_POINT('Ctrl Pts',(-0.0892370120543696,0.219746987733947,
-1.71474534935636));
#67827=CARTESIAN_POINT('Ctrl Pts',(-0.0892815750003084,0.219728885911692,
-1.71474213168723));
#67828=CARTESIAN_POINT('Ctrl Pts',(-0.0893608251426186,0.219696665785716,
-1.71473640790215));
#67829=CARTESIAN_POINT('Ctrl Pts',(-0.0893955145187637,0.219682552815313,
-1.71473390196658));
#67830=CARTESIAN_POINT('Ctrl Pts',(-0.0894572124536817,0.21965743469228,
-1.7147294440264));
#67831=CARTESIAN_POINT('Ctrl Pts',(-0.0894842223347905,0.219646432770289,
-1.71472749213109));
#67832=CARTESIAN_POINT('Ctrl Pts',(-0.0895322678313714,0.219626852087955,
-1.71472401951473));
#67833=CARTESIAN_POINT('Ctrl Pts',(-0.089553304248772,0.219618275285139,
-1.71472249885993));
#67834=CARTESIAN_POINT('Ctrl Pts',(-0.0895907287796458,0.219603010578249,
-1.71471979322012));
#67835=CARTESIAN_POINT('Ctrl Pts',(-0.0896071173802752,0.219596323860614,
-1.71471860827523));
#67836=CARTESIAN_POINT('Ctrl Pts',(-0.0896482411909376,0.219579539552672,
-1.71471563460843));
#67837=CARTESIAN_POINT('Ctrl Pts',(-0.0896729754382398,0.219569439619552,
-1.71471384580728));
#67838=CARTESIAN_POINT('Ctrl Pts',(-0.0897211736445032,0.219549748957708,
-1.71471035955603));
#67839=CARTESIAN_POINT('Ctrl Pts',(-0.0897446377741547,0.219540158646032,
-1.71470866212008));
#67840=CARTESIAN_POINT('Ctrl Pts',(-0.0897903691672221,0.21952145865184,
-1.71470535336562));
#67841=CARTESIAN_POINT('Ctrl Pts',(-0.0898126365837152,0.219512349342124,
-1.71470374205975));
#67842=CARTESIAN_POINT('Ctrl Pts',(-0.0898560433057266,0.219494584507746,
-1.71470060065989));
#67843=CARTESIAN_POINT('Ctrl Pts',(-0.0898771827485931,0.219485929316583,
-1.71469907057719));
#67844=CARTESIAN_POINT('Ctrl Pts',(-0.089918397903792,0.219469047508133,
-1.71469608702622));
#67845=CARTESIAN_POINT('Ctrl Pts',(-0.08993847373847,0.21946082118981,-1.71469463356812));
#67846=CARTESIAN_POINT('Ctrl Pts',(-0.0899776219576175,0.219444773455151,
-1.71469179895807));
#67847=CARTESIAN_POINT('Ctrl Pts',(-0.0899966944527697,0.219436952306363,
-1.71469041781517));
#67848=CARTESIAN_POINT('Ctrl Pts',(-0.0900338924456024,0.219421692683195,
-1.71468772379767));
#67849=CARTESIAN_POINT('Ctrl Pts',(-0.0900520180421404,0.219414254448981,
-1.71468641093122));
#67850=CARTESIAN_POINT('Ctrl Pts',(-0.0900873751137297,0.219399739783615,
-1.71468384968175));
#67851=CARTESIAN_POINT('Ctrl Pts',(-0.0901046066777239,0.219392663567978,
-1.71468260130603));
#67852=CARTESIAN_POINT('Ctrl Pts',(-0.0901382252242824,0.219378853338914,
-1.71468016548946));
#67853=CARTESIAN_POINT('Ctrl Pts',(-0.0901546122869155,0.21937211951904,
-1.71467897805517));
#67854=CARTESIAN_POINT('Ctrl Pts',(-0.0901865882624179,0.219358975669308,
-1.71467666079328));
#67855=CARTESIAN_POINT('Ctrl Pts',(-0.0902021772467975,0.219352565813669,
-1.71467553097162));
#67856=CARTESIAN_POINT('Ctrl Pts',(-0.0902326005956391,0.219340052594271,
-1.71467332581287));
#67857=CARTESIAN_POINT('Ctrl Pts',(-0.0902474350257179,0.219333949386747,
-1.71467225048103));
#67858=CARTESIAN_POINT('Ctrl Pts',(-0.0902763901032299,0.219322033202578,
-1.71467015137112));
#67859=CARTESIAN_POINT('Ctrl Pts',(-0.0902905108069977,0.219316220367748,
-1.71466912759798));
#67860=CARTESIAN_POINT('Ctrl Pts',(-0.0903180767457681,0.219304869643581,
-1.71466712885419));
#67861=CARTESIAN_POINT('Ctrl Pts',(-0.0903315220339558,0.219299331881042,
-1.7146661538878));
#67862=CARTESIAN_POINT('Ctrl Pts',(-0.0903577731167727,0.219288516922832,
-1.71466425017275));
#67863=CARTESIAN_POINT('Ctrl Pts',(-0.0903705789589261,0.219283239841684,
-1.71466332142796));
#67864=CARTESIAN_POINT('Ctrl Pts',(-0.0903955849418993,0.219272932716641,
-1.71466150772691));
#67865=CARTESIAN_POINT('Ctrl Pts',(-0.0904077851254341,0.219267902776166,
-1.71466062277416));
#67866=CARTESIAN_POINT('Ctrl Pts',(-0.0904316115481425,0.219258077196653,
-1.71465889437314));
#67867=CARTESIAN_POINT('Ctrl Pts',(-0.090443237826432,0.219253281650786,
-1.714658050928));
#67868=CARTESIAN_POINT('Ctrl Pts',(-0.0904659463003456,0.219243912865814,
-1.71465640339346));
#67869=CARTESIAN_POINT('Ctrl Pts',(-0.0904770285312157,0.219239339710945,
-1.7146555993069));
#67870=CARTESIAN_POINT('Ctrl Pts',(-0.0918039699081931,0.218691650947072,
-1.71455931480511));
#67871=CARTESIAN_POINT('Ctrl Pts',(-0.0931148873865717,0.218136710981778,
-1.71446343469572));
#67872=CARTESIAN_POINT('Ctrl Pts',(-0.0971582988594385,0.216381957391532,
-1.71416529844162));
#67873=CARTESIAN_POINT('Ctrl Pts',(-0.0998731106176644,0.215142387458849,
-1.71396169759898));
#67874=CARTESIAN_POINT('Ctrl Pts',(-0.106112569344353,0.212149934264756,
-1.71348554241654));
#67875=CARTESIAN_POINT('Ctrl Pts',(-0.109618323557994,0.210359910666094,
-1.71321177768223));
#67876=CARTESIAN_POINT('Ctrl Pts',(-0.121922004639338,0.203686614970498,
-1.71222844444857));
#67877=CARTESIAN_POINT('Ctrl Pts',(-0.130451136622435,0.198332232430276,
-1.71150423927462));
#67878=CARTESIAN_POINT('Ctrl Pts',(-0.151424374476446,0.183226320157479,
-1.70962325668375));
#67879=CARTESIAN_POINT('Ctrl Pts',(-0.163282242033374,0.172743126392853,
-1.70845775976851));
#67880=CARTESIAN_POINT('Ctrl Pts',(-0.175868137659138,0.159153541293116,
-1.70715693223449));
#67881=CARTESIAN_POINT('Ctrl Pts',(-0.177690693889794,0.157116105018937,
-1.70696684935604));
#67882=CARTESIAN_POINT('Ctrl Pts',(-0.180151641990481,0.154267395359076,
-1.70670832070887));
#67883=CARTESIAN_POINT('Ctrl Pts',(-0.180820491580162,0.153482876263535,
-1.70663786019124));
#67884=CARTESIAN_POINT('Ctrl Pts',(-0.181882272751237,0.152220897902633,
-1.70652572413574));
#67885=CARTESIAN_POINT('Ctrl Pts',(-0.182278479926713,0.151746231180519,
-1.70648381634638));
#67886=CARTESIAN_POINT('Ctrl Pts',(-0.183107059982614,0.150745642485521,
-1.70639605052671));
#67887=CARTESIAN_POINT('Ctrl Pts',(-0.18353903194204,0.150219399268201,
-1.70635022317439));
#67888=CARTESIAN_POINT('Ctrl Pts',(-0.184602083130875,0.148912922621912,
-1.70623724713287));
#67889=CARTESIAN_POINT('Ctrl Pts',(-0.185230497398954,0.148130518610366,
-1.70617028704228));
#67890=CARTESIAN_POINT('Ctrl Pts',(-0.187566502593951,0.145183975948144,
-1.70592061279501));
#67891=CARTESIAN_POINT('Ctrl Pts',(-0.189241365110963,0.142994010776344,
-1.70574005207734));
#67892=CARTESIAN_POINT('Ctrl Pts',(-0.20025831147995,0.128056084576701,
-1.70453790643847));
#67893=CARTESIAN_POINT('Ctrl Pts',(-0.208345295510102,0.114429532041464,
-1.7035813684058));
#67894=CARTESIAN_POINT('Ctrl Pts',(-0.218749183721279,0.0920813448084949,
-1.70206876652322));
#67895=CARTESIAN_POINT('Ctrl Pts',(-0.222029858525925,0.0838624278279787,
-1.70152358359472));
#67896=CARTESIAN_POINT('Ctrl Pts',(-0.227007627957384,0.0690343756026345,
-1.7005379259616));
#67897=CARTESIAN_POINT('Ctrl Pts',(-0.228893069435958,0.0624992604882175,
-1.70010291213344));
#67898=CARTESIAN_POINT('Ctrl Pts',(-0.230982545438021,0.0538824885112005,
-1.69952371996331));
#67899=CARTESIAN_POINT('Ctrl Pts',(-0.231443652613897,0.0518661169124639,
-1.69938780314305));
#67900=CARTESIAN_POINT('Ctrl Pts',(-0.232147500154828,0.0485917628194526,
-1.69916635198425));
#67901=CARTESIAN_POINT('Ctrl Pts',(-0.232406529978652,0.0473373632120651,
-1.69908134040437));
#67902=CARTESIAN_POINT('Ctrl Pts',(-0.232884339077109,0.0449249809981179,
-1.69891748942797));
#67903=CARTESIAN_POINT('Ctrl Pts',(-0.233104673812937,0.0437673424494301,
-1.69883870232299));
#67904=CARTESIAN_POINT('Ctrl Pts',(-0.233523128832349,0.0414759391227606,
-1.69868241868451));
#67905=CARTESIAN_POINT('Ctrl Pts',(-0.233721641556557,0.0403422782272066,
-1.69860493702333));
#67906=CARTESIAN_POINT('Ctrl Pts',(-0.234160557063099,0.0377236911775027,
-1.6984255766842));
#67907=CARTESIAN_POINT('Ctrl Pts',(-0.234395097368543,0.0362378463453015,
-1.69832351555668));
#67908=CARTESIAN_POINT('Ctrl Pts',(-0.235197598807343,0.0308197225275599,
-1.69795025213469));
#67909=CARTESIAN_POINT('Ctrl Pts',(-0.23568083538695,0.0268757572059763,
-1.69767643048821));
#67910=CARTESIAN_POINT('Ctrl Pts',(-0.236811228339999,0.0152341338636049,
-1.69686161869962));
#67911=CARTESIAN_POINT('Ctrl Pts',(-0.237181636093005,0.00751554444000314,
-1.69631281396535));
#67912=CARTESIAN_POINT('Ctrl Pts',(-0.237174910032345,-0.000206582064046445,
-1.69575651031441));
#67913=CARTESIAN_POINT('Ctrl Pts',(-0.23717491023877,-0.000206344932647713,
-1.69575652739741));
#67914=CARTESIAN_POINT('Ctrl Pts',(-0.237157180591062,-0.0205849776901013,
-1.69428844669781));
#67915=CARTESIAN_POINT('Ctrl Pts',(-0.234513236349716,-0.0408764697135139,
-1.6927680918941));
#67916=CARTESIAN_POINT('Ctrl Pts',(-0.228894938723376,-0.0621425514459061,
-1.69122992573039));
#67917=CARTESIAN_POINT('Ctrl Pts',(-0.228466403219468,-0.0637000204472546,
-1.69111766083907));
#67918=CARTESIAN_POINT('Ctrl Pts',(-0.227663245470384,-0.0665065965353731,
-1.69091620357677));
#67919=CARTESIAN_POINT('Ctrl Pts',(-0.227294173327026,-0.0677572113261506,
-1.69082673957857));
#67920=CARTESIAN_POINT('Ctrl Pts',(-0.226697674189515,-0.0697187353092507,
-1.69068697001384));
#67921=CARTESIAN_POINT('Ctrl Pts',(-0.226477180202674,-0.0704317004088306,
-1.69063628214129));
#67922=CARTESIAN_POINT('Ctrl Pts',(-0.226054949474159,-0.071774492600173,
-1.69054104962184));
#67923=CARTESIAN_POINT('Ctrl Pts',(-0.225853945042602,-0.0724045129121424,
-1.69049646671612));
#67924=CARTESIAN_POINT('Ctrl Pts',(-0.225380589747264,-0.0738670261675179,
-1.69039319128249));
#67925=CARTESIAN_POINT('Ctrl Pts',(-0.225106259276207,-0.0746988613394432,
-1.690334614762));
#67926=CARTESIAN_POINT('Ctrl Pts',(-0.224188942165128,-0.0774294346738284,
-1.69014281163176));
#67927=CARTESIAN_POINT('Ctrl Pts',(-0.223526470624683,-0.0793216031707172,
-1.69001066550158));
#67928=CARTESIAN_POINT('Ctrl Pts',(-0.217567643406588,-0.0956735741837433,
-1.68887346507427));
#67929=CARTESIAN_POINT('Ctrl Pts',(-0.210897879602875,-0.109596231993451,
-1.68793639908497));
#67930=CARTESIAN_POINT('Ctrl Pts',(-0.197190004059619,-0.13225272925852,
-1.68631330835599));
#67931=CARTESIAN_POINT('Ctrl Pts',(-0.19079927011016,-0.141316295681844,
-1.68563296896661));
#67932=CARTESIAN_POINT('Ctrl Pts',(-0.181164663114807,-0.153129746536141,
-1.68466877165995));
#67933=CARTESIAN_POINT('Ctrl Pts',(-0.178445711399983,-0.156289729225064,
-1.68440254491068));
#67934=CARTESIAN_POINT('Ctrl Pts',(-0.173553953805227,-0.161680824977024,
-1.68393196751487));
#67935=CARTESIAN_POINT('Ctrl Pts',(-0.171417812881863,-0.163943880662194,
-1.68372908224305));
#67936=CARTESIAN_POINT('Ctrl Pts',(-0.168238769456387,-0.167181729418243,
-1.68343045201469));
#67937=CARTESIAN_POINT('Ctrl Pts',(-0.167230555393448,-0.168190235724517,
-1.68333621105053));
#67938=CARTESIAN_POINT('Ctrl Pts',(-0.166198053055606,-0.169204575127073,
-1.6832401477154));
#67939=CARTESIAN_POINT('Ctrl Pts',(-0.16618277781715,-0.169219577591904,
-1.68323872661598));
#67940=CARTESIAN_POINT('Ctrl Pts',(-0.166151114141369,-0.169250667419559,
-1.68323578105735));
#67941=CARTESIAN_POINT('Ctrl Pts',(-0.166134725399423,-0.169266754470103,
-1.68323425658465));
#67942=CARTESIAN_POINT('Ctrl Pts',(-0.166100704825517,-0.169300139077184,
-1.68323109224278));
#67943=CARTESIAN_POINT('Ctrl Pts',(-0.166083072628262,-0.169317436259359,
-1.6832294523574));
#67944=CARTESIAN_POINT('Ctrl Pts',(-0.166046413945018,-0.169353387184813,
-1.68322604318276));
#67945=CARTESIAN_POINT('Ctrl Pts',(-0.166027387017896,-0.169372040475925,
-1.68322427387389));
#67946=CARTESIAN_POINT('Ctrl Pts',(-0.165987761787904,-0.169410874483293,
-1.68322058945122));
#67947=CARTESIAN_POINT('Ctrl Pts',(-0.165967162948092,-0.169431054649117,
-1.68321867431354));
#67948=CARTESIAN_POINT('Ctrl Pts',(-0.165924185100876,-0.169473143608142,
-1.68321467890185));
#67949=CARTESIAN_POINT('Ctrl Pts',(-0.165901805434801,-0.16949505172508,
-1.68321259859854));
#67950=CARTESIAN_POINT('Ctrl Pts',(-0.165855017984594,-0.16954083519938,
-1.68320824990633));
#67951=CARTESIAN_POINT('Ctrl Pts',(-0.165830609384606,-0.169564709718448,
-1.68320598148113));
#67952=CARTESIAN_POINT('Ctrl Pts',(-0.165779467301703,-0.169614711164627,
-1.68320122908784));
#67953=CARTESIAN_POINT('Ctrl Pts',(-0.165752732797996,-0.169640837041939,
-1.68319874507429));
#67954=CARTESIAN_POINT('Ctrl Pts',(-0.165696580682709,-0.169695684875623,
-1.68319352837377));
#67955=CARTESIAN_POINT('Ctrl Pts',(-0.165667161779537,-0.169724405502736,
-1.68319079562923));
#67956=CARTESIAN_POINT('Ctrl Pts',(-0.165605204415702,-0.169784860812962,
-1.68318504111908));
#67957=CARTESIAN_POINT('Ctrl Pts',(-0.165572664301311,-0.169816593791666,
-1.68318201927972));
#67958=CARTESIAN_POINT('Ctrl Pts',(-0.165503927330314,-0.1698835872495,
-1.68317563694354));
#67959=CARTESIAN_POINT('Ctrl Pts',(-0.165467728327327,-0.169918845513685,
-1.68317227635091));
#67960=CARTESIAN_POINT('Ctrl Pts',(-0.165411628792834,-0.169973452207973,
-1.68316706909839));
#67961=CARTESIAN_POINT('Ctrl Pts',(-0.165391736111512,-0.169992808734408,
-1.6831652227896));
#67962=CARTESIAN_POINT('Ctrl Pts',(-0.165334626359688,-0.170048359729382,
-1.68315992270308));
#67963=CARTESIAN_POINT('Ctrl Pts',(-0.165297400820845,-0.170084545453185,
-1.68315646854648));
#67964=CARTESIAN_POINT('Ctrl Pts',(-0.165187064580053,-0.170191729253609,
-1.68314623213565));
#67965=CARTESIAN_POINT('Ctrl Pts',(-0.165113920067816,-0.170262692362983,
-1.68313944836739));
#67966=CARTESIAN_POINT('Ctrl Pts',(-0.164199874793727,-0.171148334960564,
-1.68305470274398));
#67967=CARTESIAN_POINT('Ctrl Pts',(-0.163353011594101,-0.171956811323076,
-1.68297647371683));
#67968=CARTESIAN_POINT('Ctrl Pts',(-0.161417549239935,-0.173777342178364,
-1.68279831126105));
#67969=CARTESIAN_POINT('Ctrl Pts',(-0.160325361474269,-0.174785491818389,
-1.68269821491546));
#67970=CARTESIAN_POINT('Ctrl Pts',(-0.156956597635245,-0.177836904452586,
-1.68239076207132));
#67971=CARTESIAN_POINT('Ctrl Pts',(-0.154649983447817,-0.179846376726283,
-1.68218200896848));
#67972=CARTESIAN_POINT('Ctrl Pts',(-0.138195617390948,-0.193630425809376,
-1.68070434169805));
#67973=CARTESIAN_POINT('Ctrl Pts',(-0.122760571644535,-0.203765451123917,
-1.67936921032285));
#67974=CARTESIAN_POINT('Ctrl Pts',(-0.0945483389667432,-0.217912386417895,
-1.67706425910662));
#67975=CARTESIAN_POINT('Ctrl Pts',(-0.0823114352816662,-0.222823031305432,
-1.67610472197689));
#67976=CARTESIAN_POINT('Ctrl Pts',(-0.0682932819849794,-0.227134904289521,
-1.6750895653239));
#67977=CARTESIAN_POINT('Ctrl Pts',(-0.066853297979091,-0.22756290108941,
-1.67498625766919));
#67978=CARTESIAN_POINT('Ctrl Pts',(-0.0646512577182661,-0.228194691938939,
-1.67482985751953));
#67979=CARTESIAN_POINT('Ctrl Pts',(-0.0638921225311366,-0.22840840456902,
-1.67477622446273));
#67980=CARTESIAN_POINT('Ctrl Pts',(-0.0625002784601605,-0.228792756036485,
-1.67467842857025));
#67981=CARTESIAN_POINT('Ctrl Pts',(-0.0618679247264918,-0.228964560432744,
-1.67463420162206));
#67982=CARTESIAN_POINT('Ctrl Pts',(-0.0604348370734335,-0.229347545897333,
-1.67453442861028));
#67983=CARTESIAN_POINT('Ctrl Pts',(-0.059633703299846,-0.229557155898233,
-1.67447897291913));
#67984=CARTESIAN_POINT('Ctrl Pts',(-0.0575507864926815,-0.230090493699902,
-1.67433558058076));
#67985=CARTESIAN_POINT('Ctrl Pts',(-0.0562673447682712,-0.230407713467742,
-1.67424800044231));
#67986=CARTESIAN_POINT('Ctrl Pts',(-0.0469974130212168,-0.232616822161363,
-1.67362055981486));
#67987=CARTESIAN_POINT('Ctrl Pts',(-0.0389192012064967,-0.234103972247925,
-1.67310105597248));
#67988=CARTESIAN_POINT('Ctrl Pts',(-0.0166862644013108,-0.23701384841901,
-1.67170551773418));
#67989=CARTESIAN_POINT('Ctrl Pts',(-0.00245580051308762,-0.237587850527465,
-1.67084807818523));
#67990=CARTESIAN_POINT('Ctrl Pts',(0.0222530302080953,-0.236363201104281,
-1.66931404003925));
#67991=CARTESIAN_POINT('Ctrl Pts',(0.0327177312100396,-0.235143080853157,
-1.66865037987484));
#67992=CARTESIAN_POINT('Ctrl Pts',(0.0452937888356439,-0.232820930285271,
-1.66781678782396));
#67993=CARTESIAN_POINT('Ctrl Pts',(0.047515504108547,-0.232377686477648,
-1.66766816729781));
#67994=CARTESIAN_POINT('Ctrl Pts',(0.0510246900051521,-0.231625157689122,
-1.66743110925161));
#67995=CARTESIAN_POINT('Ctrl Pts',(0.0523165433744463,-0.231336793082054,
-1.66734334039548));
#67996=CARTESIAN_POINT('Ctrl Pts',(0.0547447295738881,-0.230773399630376,
-1.667177394927));
#67997=CARTESIAN_POINT('Ctrl Pts',(0.0558815784585395,-0.230500751620637,
-1.66709929698662));
#67998=CARTESIAN_POINT('Ctrl Pts',(0.0584420225985232,-0.229866630540486,
-1.66692246664108));
#67999=CARTESIAN_POINT('Ctrl Pts',(0.0598643581327024,-0.229500318731439,
-1.66682358075949));
#68000=CARTESIAN_POINT('Ctrl Pts',(0.0641502633238746,-0.228353963467647,
-1.66652357369212));
#68001=CARTESIAN_POINT('Ctrl Pts',(0.0670025881770273,-0.22753338370541,
-1.66632115274849));
#68002=CARTESIAN_POINT('Ctrl Pts',(0.0883524898015625,-0.220955021774782,
-1.66478444993675));
#68003=CARTESIAN_POINT('Ctrl Pts',(0.106094297452694,-0.213004673118266,
-1.66337569702148));
#68004=CARTESIAN_POINT('Ctrl Pts',(0.12500412500385,-0.201577276900321,
-1.66176266752614));
#68005=CARTESIAN_POINT('Ctrl Pts',(0.127315529573917,-0.200125425793602,
-1.66156359871335));
#68006=CARTESIAN_POINT('Ctrl Pts',(0.135142654857335,-0.195018514124812,
-1.66088385192511));
#68007=CARTESIAN_POINT('Ctrl Pts',(0.140530600564594,-0.191172487870343,
-1.66040607842604));
#68008=CARTESIAN_POINT('Ctrl Pts',(0.14866222216491,-0.184838152202823,
-1.65967661453991));
#68009=CARTESIAN_POINT('Ctrl Pts',(0.151520343984657,-0.182502569553957,
-1.65941851092251));
#68010=CARTESIAN_POINT('Ctrl Pts',(0.155171268528208,-0.179374206590474,
-1.65908777643997));
#68011=CARTESIAN_POINT('Ctrl Pts',(0.156014434164411,-0.178641330669532,
-1.65901132085006));
#68012=CARTESIAN_POINT('Ctrl Pts',(0.157381320787173,-0.177436179228383,
-1.65888729935182));
#68013=CARTESIAN_POINT('Ctrl Pts',(0.157908157341729,-0.176967487720228,
-1.65883947917616));
#68014=CARTESIAN_POINT('Ctrl Pts',(0.158932493392311,-0.176047987415613,
-1.6587464784643));
#68015=CARTESIAN_POINT('Ctrl Pts',(0.159430179906112,-0.175597406247439,
-1.65870128305898));
#68016=CARTESIAN_POINT('Ctrl Pts',(0.160539718285173,-0.174584278428505,
-1.65860048510387));
#68017=CARTESIAN_POINT('Ctrl Pts',(0.161150546110789,-0.174020610737428,
-1.65854496596836));
#68018=CARTESIAN_POINT('Ctrl Pts',(0.163265368615457,-0.172048382646694,
-1.65835259681015));
#68019=CARTESIAN_POINT('Ctrl Pts',(0.164754012049177,-0.170623394586858,
-1.65821692089826));
#68020=CARTESIAN_POINT('Ctrl Pts',(0.175574246991383,-0.159992164364411,
-1.65722705216902));
#68021=CARTESIAN_POINT('Ctrl Pts',(0.184148127779807,-0.150044552570448,
-1.65642130465746));
#68022=CARTESIAN_POINT('Ctrl Pts',(0.199275683101352,-0.129230126706398,
-1.6548434990787));
#68023=CARTESIAN_POINT('Ctrl Pts',(0.205867676875826,-0.118447024207546,
-1.65407350062453));
#68024=CARTESIAN_POINT('Ctrl Pts',(0.213598510709018,-0.103188146454109,
-1.65299460121818));
#68025=CARTESIAN_POINT('Ctrl Pts',(0.215512471342336,-0.09912864528375,
-1.65270867614093));
#68026=CARTESIAN_POINT('Ctrl Pts',(0.218642217894794,-0.0919707475758003,
-1.65220445184955));
#68027=CARTESIAN_POINT('Ctrl Pts',(0.219910104286968,-0.0888964684794111,
-1.65198787499301));
#68028=CARTESIAN_POINT('Ctrl Pts',(0.221668554010249,-0.0843646386891815,
-1.65166808129659));
#68029=CARTESIAN_POINT('Ctrl Pts',(0.222210277724175,-0.0829272716628046,
-1.65156657568996));
#68030=CARTESIAN_POINT('Ctrl Pts',(0.223142306479953,-0.0803795783009577,
-1.65138647677795));
#68031=CARTESIAN_POINT('Ctrl Pts',(0.223538384402725,-0.0792714082253722,
-1.65130807863437));
#68032=CARTESIAN_POINT('Ctrl Pts',(0.224350064659753,-0.0769459777216967,
-1.65114341589405));
#68033=CARTESIAN_POINT('Ctrl Pts',(0.224764043608607,-0.0757281954622659,
-1.65105710051559));
#68034=CARTESIAN_POINT('Ctrl Pts',(0.225825612059335,-0.0725200279909076,
-1.65082945498842));
#68035=CARTESIAN_POINT('Ctrl Pts',(0.226456782289814,-0.0705243701603183,
-1.65068759140964));
#68036=CARTESIAN_POINT('Ctrl Pts',(0.229088059447948,-0.0618049349896727,
-1.65006648413415));
#68037=CARTESIAN_POINT('Ctrl Pts',(0.230815538385571,-0.0550032600622956,
-1.64957855368143));
#68038=CARTESIAN_POINT('Ctrl Pts',(0.235493073283074,-0.0324356463933141,
-1.64794783550951));
#68039=CARTESIAN_POINT('Ctrl Pts',(0.237146429378257,-0.0164474939926009,
-1.64677064021288));
#68040=CARTESIAN_POINT('Ctrl Pts',(0.237192638167339,0.0098164657577528,
-1.6448582902849));
#68041=CARTESIAN_POINT('Ctrl Pts',(0.236548263926154,0.0200419383520721,
-1.64412022645384));
#68042=CARTESIAN_POINT('Ctrl Pts',(0.235058806373024,0.0316461556477715,
-1.64331088365781));
#68043=CARTESIAN_POINT('Ctrl Pts',(0.234859091574168,0.0330957549622613,
-1.64321029781273));
#68044=CARTESIAN_POINT('Ctrl Pts',(0.234532295490491,0.0353156074959141,
-1.64305715307967));
#68045=CARTESIAN_POINT('Ctrl Pts',(0.234414810614051,0.0360872050722019,
-1.64300408655352));
#68046=CARTESIAN_POINT('Ctrl Pts',(0.234191595284752,0.0375060989005817,
-1.64290682352088));
#68047=CARTESIAN_POINT('Ctrl Pts',(0.234086988717764,0.038153538358511,
-1.64286256774081));
#68048=CARTESIAN_POINT('Ctrl Pts',(0.23384257519367,0.0396274294370454,
-1.6427620990309));
#68049=CARTESIAN_POINT('Ctrl Pts',(0.233701071910317,0.0404535805450527,
-1.6427059821209));
#68050=CARTESIAN_POINT('Ctrl Pts',(0.233319226423434,0.0426140504752146,
-1.64255970853903));
#68051=CARTESIAN_POINT('Ctrl Pts',(0.2330718136613,0.0439471114377123,-1.64246993238373));
#68052=CARTESIAN_POINT('Ctrl Pts',(0.230664970819543,0.0563227476213644,
-1.64164031538453));
#68053=CARTESIAN_POINT('Ctrl Pts',(0.227733419951994,0.0672022320847831,
-1.64093908349473));
#68054=CARTESIAN_POINT('Ctrl Pts',(0.22351973073066,0.0793310999483972,
-1.64014824972499));
#68055=CARTESIAN_POINT('Ctrl Pts',(0.222984517748316,0.0808232537580587,
-1.64005080401535));
#68056=CARTESIAN_POINT('Ctrl Pts',(0.218499832212858,0.0929426682953969,
-1.63925733015927));
#68057=CARTESIAN_POINT('Ctrl Pts',(0.213808104613146,0.103279233520729,
-1.63856710653441));
#68058=CARTESIAN_POINT('Ctrl Pts',(0.204152407266693,0.121048513537255,
-1.63730495828086));
#68059=CARTESIAN_POINT('Ctrl Pts',(0.199474550600821,0.128611135922112,
-1.63674091273525));
#68060=CARTESIAN_POINT('Ctrl Pts',(0.193141231733835,0.137670435450131,
-1.63601966279915));
#68061=CARTESIAN_POINT('Ctrl Pts',(0.191874315379319,0.139430738281067,
-1.63587727215916));
#68062=CARTESIAN_POINT('Ctrl Pts',(0.18980807663954,0.142220152053972,-1.63564786941395));
#68063=CARTESIAN_POINT('Ctrl Pts',(0.189024084804779,0.143260506967485,
-1.63556145258007));
#68064=CARTESIAN_POINT('Ctrl Pts',(0.187518083015122,0.145225082312253,
-1.63539659610589));
#68065=CARTESIAN_POINT('Ctrl Pts',(0.186797708245683,0.146150511799278,
-1.63531822254369));
#68066=CARTESIAN_POINT('Ctrl Pts',(0.185137978125632,0.148250366858739,
-1.6351387208456));
#68067=CARTESIAN_POINT('Ctrl Pts',(0.184194264453201,0.149421266824015,
-1.63503742038396));
#68068=CARTESIAN_POINT('Ctrl Pts',(0.181238757845033,0.153017723422935,
-1.63472245000505));
#68069=CARTESIAN_POINT('Ctrl Pts',(0.179189783115478,0.155412132692644,
-1.63450728212836));
#68070=CARTESIAN_POINT('Ctrl Pts',(0.165689458861937,0.170566476123119,
-1.6331090044744));
#68071=CARTESIAN_POINT('Ctrl Pts',(0.152932715529392,0.182091451040202,
-1.63186953869485));
#68072=CARTESIAN_POINT('Ctrl Pts',(0.130932188417867,0.1980129192153,-1.62988622741946));
#68073=CARTESIAN_POINT('Ctrl Pts',(0.122451475954019,0.203366691535162,
-1.62915364894644));
#68074=CARTESIAN_POINT('Ctrl Pts',(0.11085799405431,0.209696583273971,-1.62821189354252));
#68075=CARTESIAN_POINT('Ctrl Pts',(0.10802811031955,0.211168372070908,-1.62798649001198));
#68076=CARTESIAN_POINT('Ctrl Pts',(0.103194277712658,0.213559773586262,
-1.62760995108571));
#68077=CARTESIAN_POINT('Ctrl Pts',(0.101205683322833,0.214509315378902,
-1.62745741719782));
#68078=CARTESIAN_POINT('Ctrl Pts',(0.09836891670005,0.215815620864276,-1.62724345475326));
#68079=CARTESIAN_POINT('Ctrl Pts',(0.0975315296552249,0.216195344019782,
-1.62718073810462));
#68080=CARTESIAN_POINT('Ctrl Pts',(0.0960843096693439,0.216841483276736,
-1.62707313583831));
#68081=CARTESIAN_POINT('Ctrl Pts',(0.0954755308803292,0.217110217363173,
-1.62702811191803));
#68082=CARTESIAN_POINT('Ctrl Pts',(0.0941941761281132,0.21766941560904,
-1.6269338566329));
#68083=CARTESIAN_POINT('Ctrl Pts',(0.0935213780306655,0.217959329224692,
-1.62688465812623));
#68084=CARTESIAN_POINT('Ctrl Pts',(0.0917047824816403,0.218732153369597,
-1.62675257581389));
#68085=CARTESIAN_POINT('Ctrl Pts',(0.0905584994538912,0.219209216026502,
-1.62667003584843));
#68086=CARTESIAN_POINT('Ctrl Pts',(0.0852362816501132,0.221375354896636,
-1.62629027578228));
#68087=CARTESIAN_POINT('Ctrl Pts',(0.0810162119952549,0.22295437014655,
-1.62599900467261));
#68088=CARTESIAN_POINT('Ctrl Pts',(0.0735680116787141,0.225501800381747,
-1.62549769546265));
#68089=CARTESIAN_POINT('Ctrl Pts',(0.0703596525575211,0.226523366075457,
-1.62528579308882));
#68090=CARTESIAN_POINT('Ctrl Pts',(0.0621964622093398,0.228932404337942,
-1.62475429749068));
#68091=CARTESIAN_POINT('Ctrl Pts',(0.0572161794161748,0.23022762190028,
-1.62443704790002));
#68092=CARTESIAN_POINT('Ctrl Pts',(0.0388132782934101,0.234379537614686,
-1.62327816374289));
#68093=CARTESIAN_POINT('Ctrl Pts',(0.0251929274813872,0.236231946603039,
-1.62244461852425));
#68094=CARTESIAN_POINT('Ctrl Pts',(0.00680270278645107,0.237123845681054,
-1.62128531824732));
#68095=CARTESIAN_POINT('Ctrl Pts',(0.0021108001608454,0.237212004935238,
-1.62098680656104));
#68096=CARTESIAN_POINT('Ctrl Pts',(-0.00602025926877484,0.237123535332844,
-1.62046246901015));
#68097=CARTESIAN_POINT('Ctrl Pts',(-0.00945872637578249,0.237011276234417,
-1.62023856695493));
#68098=CARTESIAN_POINT('Ctrl Pts',(-0.0144478135261466,0.236739655900411,
-1.61990997126444));
#68099=CARTESIAN_POINT('Ctrl Pts',(-0.0160013252897077,0.23663972909591,
-1.61980712854234));
#68100=CARTESIAN_POINT('Ctrl Pts',(-0.0187302043561134,0.236437204838378,
-1.61962550385825));
#68101=CARTESIAN_POINT('Ctrl Pts',(-0.0199060119794063,0.236341115737117,
-1.6195469283242));
#68102=CARTESIAN_POINT('Ctrl Pts',(-0.0223528122925231,0.23612277040315,
-1.61938273148388));
#68103=CARTESIAN_POINT('Ctrl Pts',(-0.0236236294669529,0.235999014702225,
-1.6192970655003));
#68104=CARTESIAN_POINT('Ctrl Pts',(-0.0269318279979655,0.235649865024365,
-1.61907302355486));
#68105=CARTESIAN_POINT('Ctrl Pts',(-0.0289673591628409,0.235408313124346,
-1.61893414455652));
#68106=CARTESIAN_POINT('Ctrl Pts',(-0.034659392386036,0.23465791087814,
-1.61854280990291));
#68107=CARTESIAN_POINT('Ctrl Pts',(-0.038306984633953,0.2340901000619,-1.61828856529244));
#68108=CARTESIAN_POINT('Ctrl Pts',(-0.0419392757399419,0.233437524351611,
-1.61803181050061));
#68109=CARTESIAN_POINT('Origin',(0.,0.,-2.1456589891905));
#68110=CARTESIAN_POINT('',(-0.0419392735583895,0.233437524743548,-1.49813919362704));
#68111=CARTESIAN_POINT('',(-0.0419392871413391,0.233437522303241,-1.51768363453027));
#68112=CARTESIAN_POINT('',(-0.0419392741328076,0.233437524640348,-2.1456589891905));
#68113=CARTESIAN_POINT('Ctrl Pts',(-0.0419392735583878,0.233437524743548,
-1.49813919362704));
#68114=CARTESIAN_POINT('Ctrl Pts',(-0.0403526003689305,0.233722585686572,
-1.49825693285339));
#68115=CARTESIAN_POINT('Ctrl Pts',(-0.0387626152701877,0.233991542611384,
-1.49837468919692));
#68116=CARTESIAN_POINT('Ctrl Pts',(-0.0349451157565634,0.234597298026795,
-1.49865674407909));
#68117=CARTESIAN_POINT('Ctrl Pts',(-0.0327157377689241,0.234918568965427,
-1.49882091429307));
#68118=CARTESIAN_POINT('Ctrl Pts',(-0.0239929327900559,0.236049012636772,
-1.49946050857385));
#68119=CARTESIAN_POINT('Ctrl Pts',(-0.01747128207471,0.236621138183647,
-1.49993284946457));
#68120=CARTESIAN_POINT('Ctrl Pts',(-0.00727404522223611,0.237091737755044,
-1.50065512348649));
#68121=CARTESIAN_POINT('Ctrl Pts',(-0.00361049104734264,0.237175824764138,
-1.50091133227188));
#68122=CARTESIAN_POINT('Ctrl Pts',(0.00116829973749349,0.237174741188912,
-1.50124004805536));
#68123=CARTESIAN_POINT('Ctrl Pts',(0.00228283310931947,0.237166632515784,
-1.50131632319342));
#68124=CARTESIAN_POINT('Ctrl Pts',(0.00410194056428352,0.237140572942378,
-1.50144013674687));
#68125=CARTESIAN_POINT('Ctrl Pts',(0.00480654913001082,0.237127337880786,
-1.50148792771894));
#68126=CARTESIAN_POINT('Ctrl Pts',(0.00618294274336731,0.237095346771428,
-1.50158094413403));
#68127=CARTESIAN_POINT('Ctrl Pts',(0.00685472176362094,0.237076875819526,
-1.50162618396144));
#68128=CARTESIAN_POINT('Ctrl Pts',(0.00835912202114733,0.237029111703741,
-1.50172715707174));
#68129=CARTESIAN_POINT('Ctrl Pts',(0.00919169422975093,0.236998285912196,
-1.50178280611683));
#68130=CARTESIAN_POINT('Ctrl Pts',(0.0120934306043169,0.236875535553353,
-1.50197600320352));
#68131=CARTESIAN_POINT('Ctrl Pts',(0.0141616101806051,0.236760891874265,
-1.50211236411089));
#68132=CARTESIAN_POINT('Ctrl Pts',(0.0283593181106992,0.235787167133492,
-1.50304089513483));
#68133=CARTESIAN_POINT('Ctrl Pts',(0.0404102307192574,0.234023350843837,
-1.50379158936632));
#68134=CARTESIAN_POINT('Ctrl Pts',(0.0628473306437485,0.228953483000353,
-1.50520348802103));
#68135=CARTESIAN_POINT('Ctrl Pts',(0.0732442863940249,0.225842310135339,
-1.50586397007022));
#68136=CARTESIAN_POINT('Ctrl Pts',(0.091903459910376,0.218834197757721,
-1.50710682163704));
#68137=CARTESIAN_POINT('Ctrl Pts',(0.100223506659529,0.215150811543088,
-1.50768345774627));
#68138=CARTESIAN_POINT('Ctrl Pts',(0.110253014288989,0.210002425457461,
-1.50841895791524));
#68139=CARTESIAN_POINT('Ctrl Pts',(0.112181125593001,0.208978803699889,
-1.50856226209941));
#68140=CARTESIAN_POINT('Ctrl Pts',(0.115239777492522,0.207300458425837,
-1.50879280621596));
#68141=CARTESIAN_POINT('Ctrl Pts',(0.116379544375256,0.20666273954255,-1.50887944048197));
#68142=CARTESIAN_POINT('Ctrl Pts',(0.118532482574293,0.205434676003937,
-1.5090444987553));
#68143=CARTESIAN_POINT('Ctrl Pts',(0.119546659596171,0.2048461657544,-1.50912285485526));
#68144=CARTESIAN_POINT('Ctrl Pts',(0.121847453205156,0.203488147631162,
-1.50930201760913));
#68145=CARTESIAN_POINT('Ctrl Pts',(0.123131210386247,0.202713918930156,
-1.5094029938949));
#68146=CARTESIAN_POINT('Ctrl Pts',(0.127067824261604,0.20028857249091,-1.5097158215292));
#68147=CARTESIAN_POINT('Ctrl Pts',(0.129695365667227,0.198597217335201,
-1.50992914111335));
#68148=CARTESIAN_POINT('Ctrl Pts',(0.146936313427526,0.187011091402289,
-1.5113599349279));
#68149=CARTESIAN_POINT('Ctrl Pts',(0.16043696772387,0.175565323953528,-1.51263755909178));
#68150=CARTESIAN_POINT('Ctrl Pts',(0.175572283406681,0.159517615244273,
-1.51424869033332));
#68151=CARTESIAN_POINT('Ctrl Pts',(0.178512991741656,0.156219745690236,
-1.51457135617857));
#68152=CARTESIAN_POINT('Ctrl Pts',(0.185527952185885,0.147895884524635,
-1.51536272525409));
#68153=CARTESIAN_POINT('Ctrl Pts',(0.189492239776667,0.142781357474674,
-1.51582944268662));
#68154=CARTESIAN_POINT('Ctrl Pts',(0.195350747418637,0.134548451101161,
-1.51654423959651));
#68155=CARTESIAN_POINT('Ctrl Pts',(0.197390525903791,0.13153776670685,-1.51679845436004));
#68156=CARTESIAN_POINT('Ctrl Pts',(0.199962526085301,0.127546870855848,
-1.51712502622282));
#68157=CARTESIAN_POINT('Ctrl Pts',(0.200558092893519,0.126608323585253,
-1.51720109263065));
#68158=CARTESIAN_POINT('Ctrl Pts',(0.201520094992038,0.125068491788823,
-1.5173246533053));
#68159=CARTESIAN_POINT('Ctrl Pts',(0.201890481526255,0.124469714493431,
-1.51737239823772));
#68160=CARTESIAN_POINT('Ctrl Pts',(0.202609413532483,0.123295816597441,
-1.51746539792279));
#68161=CARTESIAN_POINT('Ctrl Pts',(0.202958187220563,0.122720850307326,
-1.51751066656476));
#68162=CARTESIAN_POINT('Ctrl Pts',(0.203734434947989,0.121428816742796,
-1.51761177938801));
#68163=CARTESIAN_POINT('Ctrl Pts',(0.204160582396517,0.120710952970522,
-1.51766753856944));
#68164=CARTESIAN_POINT('Ctrl Pts',(0.205635769817062,0.118195776179702,
-1.51786149435082));
#68165=CARTESIAN_POINT('Ctrl Pts',(0.206664974130446,0.116386857200065,
-1.51799849156476));
#68166=CARTESIAN_POINT('Ctrl Pts',(0.213470861231888,0.104049878128328,
-1.51891768698643));
#68167=CARTESIAN_POINT('Ctrl Pts',(0.218465283812093,0.0931084284711445,
-1.51965951824881));
#68168=CARTESIAN_POINT('Ctrl Pts',(0.226270439510772,0.0718764945556738,
-1.52104825062062));
#68169=CARTESIAN_POINT('Ctrl Pts',(0.229258777445018,0.0616842518846413,
-1.521694626286));
#68170=CARTESIAN_POINT('Ctrl Pts',(0.233593252141522,0.0421296923970143,
-1.52294183886079));
#68171=CARTESIAN_POINT('Ctrl Pts',(0.23508189421692,0.0328205675152876,
-1.52353846344611));
#68172=CARTESIAN_POINT('Ctrl Pts',(0.236230919693698,0.0212553478775441,
-1.52429652331921));
#68173=CARTESIAN_POINT('Ctrl Pts',(0.236418214008599,0.0190595062975572,
-1.52444117003284));
#68174=CARTESIAN_POINT('Ctrl Pts',(0.236668049534541,0.0155541808922851,
-1.52467336389789));
#68175=CARTESIAN_POINT('Ctrl Pts',(0.236750382950365,0.0142462019333863,
-1.5247602897569));
#68176=CARTESIAN_POINT('Ctrl Pts',(0.236885784910824,0.0117676841364564,
-1.52492557731148));
#68177=CARTESIAN_POINT('Ctrl Pts',(0.236941027771759,0.0105972994782463,
-1.5250038683533));
#68178=CARTESIAN_POINT('Ctrl Pts',(0.237046865842675,0.00793649006466121,
-1.52518242763867));
#68179=CARTESIAN_POINT('Ctrl Pts',(0.237092080224086,0.00644591331735392,
-1.52528286127322));
#68180=CARTESIAN_POINT('Ctrl Pts',(0.23718764657318,0.00187258819260197,
-1.52559230238027));
#68181=CARTESIAN_POINT('Ctrl Pts',(0.2371919453507,-0.0012106913590628,
-1.52580273245632));
#68182=CARTESIAN_POINT('Ctrl Pts',(0.236806234750191,-0.0225162407726303,
-1.527269971454));
#68183=CARTESIAN_POINT('Ctrl Pts',(0.234376900259723,-0.0406373752304413,
-1.52859150064718));
#68184=CARTESIAN_POINT('Ctrl Pts',(0.22896645522489,-0.061973566132968,
-1.53019910913681));
#68185=CARTESIAN_POINT('Ctrl Pts',(0.227946326950483,-0.0656264670646265,
-1.53047594671459));
#68186=CARTESIAN_POINT('Ctrl Pts',(0.224927617249713,-0.075514234110407,
-1.53122771618989));
#68187=CARTESIAN_POINT('Ctrl Pts',(0.222757672168899,-0.0816937182181737,
-1.53170025811718));
#68188=CARTESIAN_POINT('Ctrl Pts',(0.218978401871383,-0.0911804290418259,
-1.53242279915932));
#68189=CARTESIAN_POINT('Ctrl Pts',(0.217543290257257,-0.0945533269945362,
-1.53267907896747));
#68190=CARTESIAN_POINT('Ctrl Pts',(0.215570433643927,-0.0989070834577553,
-1.53300787107483));
#68191=CARTESIAN_POINT('Ctrl Pts',(0.215103218492084,-0.0999191099715619,
-1.5330841536173));
#68192=CARTESIAN_POINT('Ctrl Pts',(0.214328977921189,-0.101565577377538,
-1.53320797614158));
#68193=CARTESIAN_POINT('Ctrl Pts',(0.214026235303011,-0.102201995674903,
-1.53325576874724));
#68194=CARTESIAN_POINT('Ctrl Pts',(0.213429278224202,-0.103442618959504,
-1.53334878576498));
#68195=CARTESIAN_POINT('Ctrl Pts',(0.213135326267643,-0.104046936208847,
-1.53339402457898));
#68196=CARTESIAN_POINT('Ctrl Pts',(0.212471230250406,-0.105397585044266,
-1.53349499276515));
#68197=CARTESIAN_POINT('Ctrl Pts',(0.212099710721139,-0.106143239923163,
-1.53355063792639));
#68198=CARTESIAN_POINT('Ctrl Pts',(0.210791007509068,-0.108735551334171,
-1.53374380830403));
#68199=CARTESIAN_POINT('Ctrl Pts',(0.209833541761557,-0.11057194236618,
-1.53388014681627));
#68200=CARTESIAN_POINT('Ctrl Pts',(0.203085872677736,-0.123110373508932,
-1.53480918671718));
#68201=CARTESIAN_POINT('Ctrl Pts',(0.19650285113427,-0.133366943993421,
-1.53556035353904));
#68202=CARTESIAN_POINT('Ctrl Pts',(0.182590932122008,-0.1517601579827,-1.53697586876211));
#68203=CARTESIAN_POINT('Ctrl Pts',(0.175430635886981,-0.159983361572266,
-1.53763945189577));
#68204=CARTESIAN_POINT('Ctrl Pts',(0.161339378743874,-0.174078463899533,
-1.53888251345984));
#68205=CARTESIAN_POINT('Ctrl Pts',(0.154588207765221,-0.18010042785522,
-1.53945596483905));
#68206=CARTESIAN_POINT('Ctrl Pts',(0.145803708159033,-0.187077549739037,
-1.54018786886537));
#68207=CARTESIAN_POINT('Ctrl Pts',(0.144078460705597,-0.188409467834584,
-1.54033095246942));
#68208=CARTESIAN_POINT('Ctrl Pts',(0.141291031214913,-0.190500732117462,
-1.54056122553606));
#68209=CARTESIAN_POINT('Ctrl Pts',(0.140240483022783,-0.191275432936191,
-1.54064781188387));
#68210=CARTESIAN_POINT('Ctrl Pts',(0.138234060436025,-0.192729604417816,
-1.54081283297547));
#68211=CARTESIAN_POINT('Ctrl Pts',(0.13727943361882,-0.193410736268062,
-1.54089120026589));
#68212=CARTESIAN_POINT('Ctrl Pts',(0.135091941419078,-0.194947170837933,
-1.54107046462445));
#68213=CARTESIAN_POINT('Ctrl Pts',(0.133855942349463,-0.19579790236774,
-1.54117153203704));
#68214=CARTESIAN_POINT('Ctrl Pts',(0.130015561772675,-0.198387856963129,
-1.54148493060846));
#68215=CARTESIAN_POINT('Ctrl Pts',(0.127384832963406,-0.20008720796019,
-1.54169873776807));
#68216=CARTESIAN_POINT('Ctrl Pts',(0.109811136979919,-0.21095208871016,
-1.54312195639264));
#68217=CARTESIAN_POINT('Ctrl Pts',(0.0939276013892588,-0.218487195255883,
-1.54439061142367));
#68218=CARTESIAN_POINT('Ctrl Pts',(0.068147143198341,-0.227382903442695,
-1.54638245531063));
#68219=CARTESIAN_POINT('Ctrl Pts',(0.0587438344862851,-0.229991740195819,
-1.54709473150502));
#68220=CARTESIAN_POINT('Ctrl Pts',(0.0461340717715222,-0.232666049386161,
-1.54801334056481));
#68221=CARTESIAN_POINT('Ctrl Pts',(0.0430491433158123,-0.233256546300021,
-1.54823520428722));
#68222=CARTESIAN_POINT('Ctrl Pts',(0.0378060564099866,-0.234152573755792,
-1.54860647990618));
#68223=CARTESIAN_POINT('Ctrl Pts',(0.0356538164773341,-0.234489939900515,
-1.54875724269302));
#68224=CARTESIAN_POINT('Ctrl Pts',(0.0325908839470168,-0.234926909750811,
-1.5489691880057));
#68225=CARTESIAN_POINT('Ctrl Pts',(0.0316838675929623,-0.235050954573529,
-1.54903162666025));
#68226=CARTESIAN_POINT('Ctrl Pts',(0.0301167676648912,-0.235256037423696,
-1.54913892006547));
#68227=CARTESIAN_POINT('Ctrl Pts',(0.0294570265270114,-0.235339555691331,
-1.54918391079166));
#68228=CARTESIAN_POINT('Ctrl Pts',(0.0280675509064115,-0.235509518174503,
-1.54927827972268));
#68229=CARTESIAN_POINT('Ctrl Pts',(0.0273377581672127,-0.235595347110625,
-1.54932762371291));
#68230=CARTESIAN_POINT('Ctrl Pts',(0.0253645571366234,-0.235818117688735,
-1.54946047020111));
#68231=CARTESIAN_POINT('Ctrl Pts',(0.0241204238724349,-0.235948618795346,
-1.54954362216039));
#68232=CARTESIAN_POINT('Ctrl Pts',(0.01829072215585,-0.23651352109108,-1.54993064505786));
#68233=CARTESIAN_POINT('Ctrl Pts',(0.0136938250253303,-0.236824158474367,
-1.5502282873018));
#68234=CARTESIAN_POINT('Ctrl Pts',(0.00594124313793845,-0.237121518081253,
-1.55072196631789));
#68235=CARTESIAN_POINT('Ctrl Pts',(0.0027898263478255,-0.237179533316197,
-1.55092034567002));
#68236=CARTESIAN_POINT('Ctrl Pts',(-0.0146548208244471,-0.237152913396436,
-1.55201020544053));
#68237=CARTESIAN_POINT('Ctrl Pts',(-0.0289168759591554,-0.235839170098116,
-1.55287223014267));
#68238=CARTESIAN_POINT('Ctrl Pts',(-0.0530798299700456,-0.231387338564605,
-1.55439224574075));
#68239=CARTESIAN_POINT('Ctrl Pts',(-0.0630525803721703,-0.228870933593862,
-1.55503743737435));
#68240=CARTESIAN_POINT('Ctrl Pts',(-0.0755404455863732,-0.22484157278426,
-1.55588788112081));
#68241=CARTESIAN_POINT('Ctrl Pts',(-0.0782347820119654,-0.223918309924308,
-1.55607393214493));
#68242=CARTESIAN_POINT('Ctrl Pts',(-0.0822704737345905,-0.222453678469284,
-1.55635681147324));
#68243=CARTESIAN_POINT('Ctrl Pts',(-0.0836246361951811,-0.221948169576309,
-1.55645245293647));
#68244=CARTESIAN_POINT('Ctrl Pts',(-0.0860641264696326,-0.221012013180196,
-1.55662609951111));
#68245=CARTESIAN_POINT('Ctrl Pts',(-0.087151063484527,-0.220585665637363,
-1.55670395854886));
#68246=CARTESIAN_POINT('Ctrl Pts',(-0.0894790927337202,-0.219652611139689,
-1.55687179493788));
#68247=CARTESIAN_POINT('Ctrl Pts',(-0.090719120556606,-0.219143374652647,
-1.55696185549327));
#68248=CARTESIAN_POINT('Ctrl Pts',(-0.0940580904649978,-0.217738979005214,
-1.557206188833));
#68249=CARTESIAN_POINT('Ctrl Pts',(-0.096148494384201,-0.216824015627731,
-1.55736112852527));
#68250=CARTESIAN_POINT('Ctrl Pts',(-0.10731839960784,-0.211741691327165,
-1.5581999606161));
#68251=CARTESIAN_POINT('Ctrl Pts',(-0.116139746961318,-0.207034521989676,
-1.55890224612895));
#68252=CARTESIAN_POINT('Ctrl Pts',(-0.139098352316603,-0.192853676827186,
-1.56083835176652));
#68253=CARTESIAN_POINT('Ctrl Pts',(-0.152556285958983,-0.182393573845782,
-1.56209687960328));
#68254=CARTESIAN_POINT('Ctrl Pts',(-0.169206965890734,-0.166309540009794,
-1.56376022108362));
#68255=CARTESIAN_POINT('Ctrl Pts',(-0.173465964134562,-0.161862393558947,
-1.56419637674309));
#68256=CARTESIAN_POINT('Ctrl Pts',(-0.178417386678673,-0.156272000504373,
-1.56471180321978));
#68257=CARTESIAN_POINT('Ctrl Pts',(-0.179279153207211,-0.155282605059267,
-1.56480183471092));
#68258=CARTESIAN_POINT('Ctrl Pts',(-0.180619405019962,-0.153717829017834,
-1.56494230011409));
#68259=CARTESIAN_POINT('Ctrl Pts',(-0.181103437612204,-0.153147266877444,
-1.5649931222925));
#68260=CARTESIAN_POINT('Ctrl Pts',(-0.182010081172323,-0.152068234956686,
-1.56508847810162));
#68261=CARTESIAN_POINT('Ctrl Pts',(-0.182433263737258,-0.151560291716579,
-1.56513305107814));
#68262=CARTESIAN_POINT('Ctrl Pts',(-0.183410460061543,-0.150377346263434,
-1.56523614049781));
#68263=CARTESIAN_POINT('Ctrl Pts',(-0.183962876694107,-0.149701046049113,
-1.56529454246618));
#68264=CARTESIAN_POINT('Ctrl Pts',(-0.185760914361094,-0.147474801579748,
-1.56548510269854));
#68265=CARTESIAN_POINT('Ctrl Pts',(-0.186990820523314,-0.145912193070795,
-1.56561619996631));
#68266=CARTESIAN_POINT('Ctrl Pts',(-0.197781627399318,-0.131841793500857,
-1.56677507184123));
#68267=CARTESIAN_POINT('Ctrl Pts',(-0.206096087345197,-0.11842456948595,
-1.56773162403626));
#68268=CARTESIAN_POINT('Ctrl Pts',(-0.219863767401986,-0.0903005080396204,
-1.56965120240518));
#68269=CARTESIAN_POINT('Ctrl Pts',(-0.225313796306159,-0.075682661650732,
-1.57061036730523));
#68270=CARTESIAN_POINT('Ctrl Pts',(-0.229994294282153,-0.0579839484923982,
-1.57179800862275));
#68271=CARTESIAN_POINT('Ctrl Pts',(-0.230649866709464,-0.0553186374757089,
-1.57197743184894));
#68272=CARTESIAN_POINT('Ctrl Pts',(-0.231575232285671,-0.051253508068792,
-1.57225223798412));
#68273=CARTESIAN_POINT('Ctrl Pts',(-0.23187891798976,-0.0498615838088404,
-1.57234653568833));
#68274=CARTESIAN_POINT('Ctrl Pts',(-0.232408381862603,-0.0473253103862923,
-1.57251876537644));
#68275=CARTESIAN_POINT('Ctrl Pts',(-0.232638295266252,-0.0461818628381915,
-1.5725965625038));
#68276=CARTESIAN_POINT('Ctrl Pts',(-0.233117358477165,-0.0437048976327094,
-1.57276543351551));
#68277=CARTESIAN_POINT('Ctrl Pts',(-0.23336351846313,-0.0423708510422573,
-1.57285659970519));
#68278=CARTESIAN_POINT('Ctrl Pts',(-0.234005308331653,-0.0387173421779607,
-1.57310689861532));
#68279=CARTESIAN_POINT('Ctrl Pts',(-0.234377878661777,-0.0363940408689096,
-1.57326675419077));
#68280=CARTESIAN_POINT('Ctrl Pts',(-0.236363365187718,-0.0227138366397453,
-1.57421235800029));
#68281=CARTESIAN_POINT('Ctrl Pts',(-0.237184984577307,-0.0112592180260812,
-1.57502272257575));
#68282=CARTESIAN_POINT('Ctrl Pts',(-0.23716687031361,0.00935657934971425,
-1.57650990145017));
#68283=CARTESIAN_POINT('Ctrl Pts',(-0.236629549187816,0.0184963197536797,
-1.57717907270038));
#68284=CARTESIAN_POINT('Ctrl Pts',(-0.235383558988599,0.0291378701453599,
-1.57796111466374));
#68285=CARTESIAN_POINT('Ctrl Pts',(-0.235185941931456,0.0306921502255948,
-1.57807539920959));
#68286=CARTESIAN_POINT('Ctrl Pts',(-0.233547229905083,0.0426338639009862,
-1.57895353549401));
#68287=CARTESIAN_POINT('Ctrl Pts',(-0.231433839853078,0.0529186618183489,
-1.57971079543511));
#68288=CARTESIAN_POINT('Ctrl Pts',(-0.228286216710733,0.0643367624147382,
-1.58053060395141));
#68289=CARTESIAN_POINT('Ctrl Pts',(-0.227915013344541,0.0656396423157721,
-1.58062382745949));
#68290=CARTESIAN_POINT('Ctrl Pts',(-0.227296148252182,0.0677432197782579,
-1.58077374153251));
#68291=CARTESIAN_POINT('Ctrl Pts',(-0.227055376583825,0.0685458886798055,
-1.58083080232548));
#68292=CARTESIAN_POINT('Ctrl Pts',(-0.226618533964416,0.0699746459128448,
-1.58093209593542));
#68293=CARTESIAN_POINT('Ctrl Pts',(-0.226424114666178,0.070601213440327,
-1.58097642123452));
#68294=CARTESIAN_POINT('Ctrl Pts',(-0.225992505048857,0.0719720671855698,
-1.58107318730141));
#68295=CARTESIAN_POINT('Ctrl Pts',(-0.225754236262176,0.0727159930622962,
-1.58112556477085));
#68296=CARTESIAN_POINT('Ctrl Pts',(-0.225058363969718,0.0748522637399902,
-1.58127562100822));
#68297=CARTESIAN_POINT('Ctrl Pts',(-0.224591514746974,0.0762415920055359,
-1.58137277914787));
#68298=CARTESIAN_POINT('Ctrl Pts',(-0.220730747035128,0.0873878254732538,
-1.5821494529609));
#68299=CARTESIAN_POINT('Ctrl Pts',(-0.216715092128115,0.0969191430188302,
-1.58279647101808));
#68300=CARTESIAN_POINT('Ctrl Pts',(-0.204803838991282,0.120716014100129,
-1.58443989603002));
#68301=CARTESIAN_POINT('Ctrl Pts',(-0.196038712819069,0.134483387828047,
-1.58542126925986));
#68302=CARTESIAN_POINT('Ctrl Pts',(-0.181754083713967,0.152521272843102,
-1.58687176305908));
#68303=CARTESIAN_POINT('Ctrl Pts',(-0.177352977769336,0.157617238544378,
-1.58730254230416));
#68304=CARTESIAN_POINT('Ctrl Pts',(-0.171328868542365,0.164020270325979,
-1.58787687538116));
#68305=CARTESIAN_POINT('Ctrl Pts',(-0.169896817305636,0.165503176106197,
-1.58801234567089));
#68306=CARTESIAN_POINT('Ctrl Pts',(-0.167544802464842,0.167876017632505,
-1.58823326780594));
#68307=CARTESIAN_POINT('Ctrl Pts',(-0.166636625412965,0.168777525432041,
-1.58831820189973));
#68308=CARTESIAN_POINT('Ctrl Pts',(-0.164877514863053,0.170495679148747,
-1.58848203992736));
#68309=CARTESIAN_POINT('Ctrl Pts',(-0.164027695964611,0.17131341566146,
-1.58856089262049));
#68310=CARTESIAN_POINT('Ctrl Pts',(-0.162045594720039,0.173192419394738,
-1.58874414802871));
#68311=CARTESIAN_POINT('Ctrl Pts',(-0.160908935215939,0.174248969214105,
-1.5888487488674));
#68312=CARTESIAN_POINT('Ctrl Pts',(-0.157240902808065,0.177591989205021,
-1.58918480878934));
#68313=CARTESIAN_POINT('Ctrl Pts',(-0.154670638839328,0.179834945207608,
-1.58941806902809));
#68314=CARTESIAN_POINT('Ctrl Pts',(-0.148492258278884,0.184996098578095,
-1.5899739141462));
#68315=CARTESIAN_POINT('Ctrl Pts',(-0.144845210246446,0.187865290446729,
-1.59029829506591));
#68316=CARTESIAN_POINT('Ctrl Pts',(-0.12164429786254,0.205040499020205,
-1.59233907212551));
#68317=CARTESIAN_POINT('Ctrl Pts',(-0.100082369864355,0.216384358933479,
-1.59415771635204));
#68318=CARTESIAN_POINT('Ctrl Pts',(-0.0743544254437696,0.225238369261192,
-1.59607307737764));
#68319=CARTESIAN_POINT('Ctrl Pts',(-0.0715115974071082,0.226157018599424,
-1.59628118595296));
#68320=CARTESIAN_POINT('Ctrl Pts',(-0.0676290671327156,0.227331106576671,
-1.59655995328095));
#68321=CARTESIAN_POINT('Ctrl Pts',(-0.0666040160675047,0.227633538591691,
-1.59663304122716));
#68322=CARTESIAN_POINT('Ctrl Pts',(-0.0649756006170944,0.228102046198254,
-1.59674830317951));
#68323=CARTESIAN_POINT('Ctrl Pts',(-0.0643735785280153,0.228272675907759,
-1.59679073255126));
#68324=CARTESIAN_POINT('Ctrl Pts',(-0.0631210725835327,0.228622321690159,
-1.59687861727664));
#68325=CARTESIAN_POINT('Ctrl Pts',(-0.062470491743581,0.228800947231329,
-1.59692404765882));
#68326=CARTESIAN_POINT('Ctrl Pts',(-0.0608816579816892,0.229229900539494,
-1.59703448174924));
#68327=CARTESIAN_POINT('Ctrl Pts',(-0.0599425989567112,0.229477250490129,
-1.59709931591161));
#68328=CARTESIAN_POINT('Ctrl Pts',(-0.0565513129593959,0.230348283771568,
-1.59733197331986));
#68329=CARTESIAN_POINT('Ctrl Pts',(-0.0540905608930938,0.230938509841191,
-1.59749800523825));
#68330=CARTESIAN_POINT('Ctrl Pts',(-0.0484075384125142,0.232205789651432,
-1.59787606103081));
#68331=CARTESIAN_POINT('Ctrl Pts',(-0.0451796913467915,0.232855352832219,
-1.59808684124396));
#68332=CARTESIAN_POINT('Ctrl Pts',(-0.0419392741218017,0.233437524642326,
-1.59829545246927));
#68333=CARTESIAN_POINT('Ctrl Pts',(-0.0419392757399419,0.233437524351611,
-1.61803181050061));
#68334=CARTESIAN_POINT('Ctrl Pts',(-0.0448253805600994,0.232919008118186,
-1.61782780117959));
#68335=CARTESIAN_POINT('Ctrl Pts',(-0.0477018253624859,0.232346976417747,
-1.61762220998104));
#68336=CARTESIAN_POINT('Ctrl Pts',(-0.0665627472268817,0.228231078868697,
-1.6162592909867));
#68337=CARTESIAN_POINT('Ctrl Pts',(-0.082152447815779,0.223093875629562,
-1.61505775634771));
#68338=CARTESIAN_POINT('Ctrl Pts',(-0.106545044553912,0.21214995997301,
-1.6131106274145));
#68339=CARTESIAN_POINT('Ctrl Pts',(-0.11571631766398,0.207290224297602,
-1.61236257754996));
#68340=CARTESIAN_POINT('Ctrl Pts',(-0.125788627065247,0.201075485959217,
-1.61154380133823));
#68341=CARTESIAN_POINT('Ctrl Pts',(-0.127029118554178,0.200294116399598,
-1.61144302152065));
#68342=CARTESIAN_POINT('Ctrl Pts',(-0.12891931375671,0.199078881886963,
-1.61128964454322));
#68343=CARTESIAN_POINT('Ctrl Pts',(-0.129574225193482,0.198653242819663,
-1.61123653742812));
#68344=CARTESIAN_POINT('Ctrl Pts',(-0.130775130330684,0.197864286774164,
-1.6111392367465));
#68345=CARTESIAN_POINT('Ctrl Pts',(-0.131321721560386,0.19750193963529,
-1.61109498355794));
#68346=CARTESIAN_POINT('Ctrl Pts',(-0.132562871229332,0.196671724079642,
-1.61099456702984));
#68347=CARTESIAN_POINT('Ctrl Pts',(-0.1332564603171,0.196202440654019,-1.61093849929123));
#68348=CARTESIAN_POINT('Ctrl Pts',(-0.135064330725534,0.194965223710152,
-1.61079244056339));
#68349=CARTESIAN_POINT('Ctrl Pts',(-0.136174569437207,0.194191397179468,
-1.61070282827568));
#68350=CARTESIAN_POINT('Ctrl Pts',(-0.145680592230037,0.187444165012068,
-1.60993571367215));
#68351=CARTESIAN_POINT('Ctrl Pts',(-0.153686614280069,0.180938195371603,
-1.60929050051278));
#68352=CARTESIAN_POINT('Ctrl Pts',(-0.16874719762037,0.166976111990685,
-1.60802234707679));
#68353=CARTESIAN_POINT('Ctrl Pts',(-0.175791676964131,0.159542875115537,
-1.60740046339865));
#68354=CARTESIAN_POINT('Ctrl Pts',(-0.18753428391113,0.145426919488356,
-1.60626780584322));
#68355=CARTESIAN_POINT('Ctrl Pts',(-0.192409057189505,0.138913050417115,
-1.60576128509703));
#68356=CARTESIAN_POINT('Ctrl Pts',(-0.198858253472461,0.129302871034174,
-1.60502410889906));
#68357=CARTESIAN_POINT('Ctrl Pts',(-0.200714446697319,0.126402320015458,
-1.60480288118514));
#68358=CARTESIAN_POINT('Ctrl Pts',(-0.203917010455068,0.12114938193312,
-1.60440363483024));
#68359=CARTESIAN_POINT('Ctrl Pts',(-0.205287464014855,0.118812356395178,
-1.60422649127343));
#68360=CARTESIAN_POINT('Ctrl Pts',(-0.207313357874855,0.115217883051229,
-1.60395448549345));
#68361=CARTESIAN_POINT('Ctrl Pts',(-0.207998081739118,0.11397713267939,
-1.60386067466868));
#68362=CARTESIAN_POINT('Ctrl Pts',(-0.209171918164477,0.111804280567195,
-1.60369649279287));
#68363=CARTESIAN_POINT('Ctrl Pts',(-0.209666026095908,0.110874911235665,
-1.60362630179277));
#68364=CARTESIAN_POINT('Ctrl Pts',(-0.2107661005386,0.108772126692896,-1.60346754451242));
#68365=CARTESIAN_POINT('Ctrl Pts',(-0.211368481142887,0.107596885356162,
-1.60337885460028));
#68366=CARTESIAN_POINT('Ctrl Pts',(-0.212971215415024,0.104404555737766,
-1.60313801571861));
#68367=CARTESIAN_POINT('Ctrl Pts',(-0.213952691199311,0.102378196763698,
-1.60298521615846));
#68368=CARTESIAN_POINT('Ctrl Pts',(-0.218720926029562,0.092165557337005,
-1.6022152621633));
#68369=CARTESIAN_POINT('Ctrl Pts',(-0.222066930649408,0.083782906557399,
-1.60158330450425));
#68370=CARTESIAN_POINT('Ctrl Pts',(-0.225095352756358,0.074728465753995,
-1.60090108818646));
#68371=CARTESIAN_POINT('Ctrl Pts',(-0.225261751686517,0.0742253639108846,
-1.60086318421204));
#68372=CARTESIAN_POINT('Ctrl Pts',(-0.230857472539021,0.0571147524739912,
-1.5995741765043));
#68373=CARTESIAN_POINT('Ctrl Pts',(-0.234436308771632,0.0399601541125883,
-1.59827993360627));
#68374=CARTESIAN_POINT('Ctrl Pts',(-0.236690627417089,0.0163772768627074,
-1.59657726251572));
#68375=CARTESIAN_POINT('Ctrl Pts',(-0.237038764327972,0.0101640384228324,
-1.59613634377581));
#68376=CARTESIAN_POINT('Ctrl Pts',(-0.23716408303571,0.00262845668443124,
-1.59561614313132));
#68377=CARTESIAN_POINT('Ctrl Pts',(-0.23717501418411,0.00131297859049132,
-1.59552587121188));
#68378=CARTESIAN_POINT('Ctrl Pts',(-0.237174991904851,-0.000751352849641178,
-1.5953851263894));
#68379=CARTESIAN_POINT('Ctrl Pts',(-0.237171437763164,-0.00150015495153717,
-1.59533426257375));
#68380=CARTESIAN_POINT('Ctrl Pts',(-0.237158072402004,-0.00290961275161045,
-1.59523889401));
#68381=CARTESIAN_POINT('Ctrl Pts',(-0.237149047112992,-0.00357024049217805,
-1.59519434940052));
#68382=CARTESIAN_POINT('Ctrl Pts',(-0.237121444682551,-0.0051173458443599,
-1.5950903844646));
#68383=CARTESIAN_POINT('Ctrl Pts',(-0.237100657091772,-0.00600376772102378,
-1.59503108710061));
#68384=CARTESIAN_POINT('Ctrl Pts',(-0.237016452093551,-0.00890111005079207,
-1.59483809002992));
#68385=CARTESIAN_POINT('Ctrl Pts',(-0.236932416881283,-0.0109114076643369,
-1.59470547402414));
#68386=CARTESIAN_POINT('Ctrl Pts',(-0.236668833765064,-0.0157426928009187,
-1.59438934917823));
#68387=CARTESIAN_POINT('Ctrl Pts',(-0.236464416753113,-0.018562067842114,
-1.59420699295673));
#68388=CARTESIAN_POINT('Ctrl Pts',(-0.235474923760893,-0.0294955531655902,
-1.59350574820215));
#68389=CARTESIAN_POINT('Ctrl Pts',(-0.234322107712655,-0.0375712313196251,
-1.59300039577045));
#68390=CARTESIAN_POINT('Ctrl Pts',(-0.22889712927067,-0.0652788779971918,
-1.59126346106171));
#68391=CARTESIAN_POINT('Ctrl Pts',(-0.222552201560954,-0.0844136581320735,
-1.59005069501236));
#68392=CARTESIAN_POINT('Ctrl Pts',(-0.212643298963519,-0.105085206262819,
-1.5885654089827));
#68393=CARTESIAN_POINT('Ctrl Pts',(-0.211367639957468,-0.107628029890246,
-1.58837962913555));
#68394=CARTESIAN_POINT('Ctrl Pts',(-0.209367015345032,-0.111443146026963,
-1.58809587933566));
#68395=CARTESIAN_POINT('Ctrl Pts',(-0.208675467580815,-0.112732741380211,
-1.58799908163612));
#68396=CARTESIAN_POINT('Ctrl Pts',(-0.207410266440159,-0.115040547801208,
-1.58782421671853));
#68397=CARTESIAN_POINT('Ctrl Pts',(-0.206840932332536,-0.116061082585927,
-1.58774630536856));
#68398=CARTESIAN_POINT('Ctrl Pts',(-0.20560892914254,-0.118231596427108,
-1.58757932528566));
#68399=CARTESIAN_POINT('Ctrl Pts',(-0.204944104820854,-0.119380299512177,
-1.58749018082305));
#68400=CARTESIAN_POINT('Ctrl Pts',(-0.203110067364868,-0.122488728537328,
-1.58724680480496));
#68401=CARTESIAN_POINT('Ctrl Pts',(-0.201922181019589,-0.124437214131901,
-1.58709189903665));
#68402=CARTESIAN_POINT('Ctrl Pts',(-0.194920244012957,-0.135558157436927,
-1.58619386269258));
#68403=CARTESIAN_POINT('Ctrl Pts',(-0.188510613607033,-0.144338498989121,
-1.58542872498265));
#68404=CARTESIAN_POINT('Ctrl Pts',(-0.171594242740078,-0.164454793572754,
-1.58353752637507));
#68405=CARTESIAN_POINT('Ctrl Pts',(-0.160537939460671,-0.175264077918458,
-1.58239798684725));
#68406=CARTESIAN_POINT('Ctrl Pts',(-0.143248817321769,-0.189148893207022,
-1.58079981652409));
#68407=CARTESIAN_POINT('Ctrl Pts',(-0.137808277619231,-0.193148711075333,
-1.58031993437694));
#68408=CARTESIAN_POINT('Ctrl Pts',(-0.131056535695983,-0.197681752515671,
-1.57975789585834));
#68409=CARTESIAN_POINT('Ctrl Pts',(-0.129902318587938,-0.198442129299966,
-1.57966294943602));
#68410=CARTESIAN_POINT('Ctrl Pts',(-0.128093480546965,-0.199611212575235,
-1.57951599193981));
#68411=CARTESIAN_POINT('Ctrl Pts',(-0.12744342321421,-0.200026872861384,
-1.5794635441475));
#68412=CARTESIAN_POINT('Ctrl Pts',(-0.126236318509734,-0.200790447536555,
-1.57936684427133));
#68413=CARTESIAN_POINT('Ctrl Pts',(-0.125679854786443,-0.201139220568089,
-1.57932253826151));
#68414=CARTESIAN_POINT('Ctrl Pts',(-0.124399705473633,-0.201934188927431,
-1.57922122609034));
#68415=CARTESIAN_POINT('Ctrl Pts',(-0.123675063128399,-0.202378808663552,
-1.57916432263383));
#68416=CARTESIAN_POINT('Ctrl Pts',(-0.121398418630204,-0.203758897447544,
-1.57898688478273));
#68417=CARTESIAN_POINT('Ctrl Pts',(-0.11983803264698,-0.204680508985244,
-1.57886720641069));
#68418=CARTESIAN_POINT('Ctrl Pts',(-0.116131029040646,-0.206813050795847,
-1.57858704707638));
#68419=CARTESIAN_POINT('Ctrl Pts',(-0.113975763673021,-0.208008606116302,
-1.57842739937182));
#68420=CARTESIAN_POINT('Ctrl Pts',(-0.106032497992382,-0.212254303865473,
-1.57784928952455));
#68421=CARTESIAN_POINT('Ctrl Pts',(-0.100137269307851,-0.215098395725834,
-1.57743983747774));
#68422=CARTESIAN_POINT('Ctrl Pts',(-0.0906152336394982,-0.21921573080034,
-1.57679757205473));
#68423=CARTESIAN_POINT('Ctrl Pts',(-0.0870624959189503,-0.220650810132163,
-1.57656199791734));
#68424=CARTESIAN_POINT('Ctrl Pts',(-0.0664526318686506,-0.228400563924269,
-1.57521088632839));
#68425=CARTESIAN_POINT('Ctrl Pts',(-0.0487510743039558,-0.232821857679894,
-1.57410482193531));
#68426=CARTESIAN_POINT('Ctrl Pts',(-0.0276591421225758,-0.235576897961391,
-1.57272912428341));
#68427=CARTESIAN_POINT('Ctrl Pts',(-0.0245919141816058,-0.235916805928248,
-1.57252784560778));
#68428=CARTESIAN_POINT('Ctrl Pts',(-0.0200337176549391,-0.23633208684842,
-1.57222650997896));
#68429=CARTESIAN_POINT('Ctrl Pts',(-0.0185471820476079,-0.236453392837338,
-1.57212788994346));
#68430=CARTESIAN_POINT('Ctrl Pts',(-0.0158912994391405,-0.236644922448308,
-1.57195102838453));
#68431=CARTESIAN_POINT('Ctrl Pts',(-0.0147223798344311,-0.236720519106242,
-1.57187295789503));
#68432=CARTESIAN_POINT('Ctrl Pts',(-0.0122454224141728,-0.236862292326132,
-1.57170701771441));
#68433=CARTESIAN_POINT('Ctrl Pts',(-0.0109373047304288,-0.236926298966222,
-1.57161908269013));
#68434=CARTESIAN_POINT('Ctrl Pts',(-0.00742955300061291,-0.237068822926058,
-1.57138244668804));
#68435=CARTESIAN_POINT('Ctrl Pts',(-0.00522928954504909,-0.237127558546657,
-1.57123313346676));
#68436=CARTESIAN_POINT('Ctrl Pts',(0.00635404935427809,-0.237275483284894,
-1.57044220184766));
#68437=CARTESIAN_POINT('Ctrl Pts',(0.0157342978430609,-0.236838383638481,
-1.56978439981627));
#68438=CARTESIAN_POINT('Ctrl Pts',(0.0356405595703932,-0.234722984347898,
-1.56835247685168));
#68439=CARTESIAN_POINT('Ctrl Pts',(0.0461298632089687,-0.232888676800962,
-1.56757600914355));
#68440=CARTESIAN_POINT('Ctrl Pts',(0.0681396971986026,-0.227494122084667,
-1.56592107634686));
#68441=CARTESIAN_POINT('Ctrl Pts',(0.0795860880552203,-0.223746969316612,
-1.56504477648228));
#68442=CARTESIAN_POINT('Ctrl Pts',(0.0926216159837324,-0.218351878931473,
-1.56406058919018));
#68443=CARTESIAN_POINT('Ctrl Pts',(0.0945329973376726,-0.21753119301078,
-1.56391666796137));
#68444=CARTESIAN_POINT('Ctrl Pts',(0.0971957780596239,-0.21634615241026,
-1.56371695962002));
#68445=CARTESIAN_POINT('Ctrl Pts',(0.0979563604836231,-0.216002843566867,
-1.56366000744057));
#68446=CARTESIAN_POINT('Ctrl Pts',(0.0993263524834753,-0.215375737259282,
-1.56355760905645));
#68447=CARTESIAN_POINT('Ctrl Pts',(0.0999363962822983,-0.215093350050745,
-1.56351207923177));
#68448=CARTESIAN_POINT('Ctrl Pts',(0.101182695938329,-0.214509995189509,
-1.56341921294));
#68449=CARTESIAN_POINT('Ctrl Pts',(0.101818825764001,-0.214208783075014,
-1.5633718919076));
#68450=CARTESIAN_POINT('Ctrl Pts',(0.103455764355276,-0.21342474117569,
-1.56325030255618));
#68451=CARTESIAN_POINT('Ctrl Pts',(0.104454551882658,-0.21293769519829,
-1.56317628922051));
#68452=CARTESIAN_POINT('Ctrl Pts',(0.108705700198137,-0.210827567588547,
-1.56286185872002));
#68453=CARTESIAN_POINT('Ctrl Pts',(0.111924134523603,-0.209136759408554,
-1.56262530115006));
#68454=CARTESIAN_POINT('Ctrl Pts',(0.12075580255814,-0.204234720056343,
-1.56197679227005));
#68455=CARTESIAN_POINT('Ctrl Pts',(0.126278718686508,-0.200866826557076,
-1.56157193052418));
#68456=CARTESIAN_POINT('Ctrl Pts',(0.135330607630634,-0.194825841464226,
-1.56089792181914));
#68457=CARTESIAN_POINT('Ctrl Pts',(0.138934652818485,-0.19227232145599,
-1.5606265955807));
#68458=CARTESIAN_POINT('Ctrl Pts',(0.156578725015797,-0.179015944720803,
-1.55927307059438));
#68459=CARTESIAN_POINT('Ctrl Pts',(0.16946248981502,-0.166871163373313,
-1.55819737168683));
#68460=CARTESIAN_POINT('Ctrl Pts',(0.182899899045689,-0.151027702305313,
-1.55685423620292));
#68461=CARTESIAN_POINT('Ctrl Pts',(0.184873215905236,-0.148605627382765,
-1.5566505173462));
#68462=CARTESIAN_POINT('Ctrl Pts',(0.187721544500754,-0.144964990623914,
-1.55634623056634));
#68463=CARTESIAN_POINT('Ctrl Pts',(0.188633814498065,-0.143775904207863,
-1.55624714174698));
#68464=CARTESIAN_POINT('Ctrl Pts',(0.190239387617031,-0.141641554640548,
-1.55606976006927));
#68465=CARTESIAN_POINT('Ctrl Pts',(0.190937073792697,-0.140699638836436,
-1.55599164215179));
#68466=CARTESIAN_POINT('Ctrl Pts',(0.192397013132775,-0.138697780799072,
-1.55582593792496));
#68467=CARTESIAN_POINT('Ctrl Pts',(0.193157551384084,-0.13763664223583,
-1.55573828879223));
#68468=CARTESIAN_POINT('Ctrl Pts',(0.195165666785093,-0.134785399572777,
-1.55550324171146));
#68469=CARTESIAN_POINT('Ctrl Pts',(0.196397341691543,-0.132984303776592,
-1.55535524576509));
#68470=CARTESIAN_POINT('Ctrl Pts',(0.202627891522382,-0.123597904885718,
-1.55458620003902));
#68471=CARTESIAN_POINT('Ctrl Pts',(0.207212204733981,-0.115747870474028,
-1.55395003284956));
#68472=CARTESIAN_POINT('Ctrl Pts',(0.216257954015978,-0.0979904267812124,
-1.55252639588848));
#68473=CARTESIAN_POINT('Ctrl Pts',(0.220512125623393,-0.0879999833909121,
-1.55173494670563));
#68474=CARTESIAN_POINT('Ctrl Pts',(0.228055491319261,-0.0662619916257181,
-1.55005451203028));
#68475=CARTESIAN_POINT('Ctrl Pts',(0.231153824412979,-0.0544786847534756,
-1.54916771819621));
#68476=CARTESIAN_POINT('Ctrl Pts',(0.233705691664736,-0.0404712150169731,
-1.54817455328728));
#68477=CARTESIAN_POINT('Ctrl Pts',(0.234050184699699,-0.0384289127149271,
-1.54803126360847));
#68478=CARTESIAN_POINT('Ctrl Pts',(0.234495665138618,-0.0355592100236386,
-1.54783228232833));
#68479=CARTESIAN_POINT('Ctrl Pts',(0.234619100103016,-0.0347354617892509,
-1.54777543639346));
#68480=CARTESIAN_POINT('Ctrl Pts',(0.234834249724351,-0.0332461592872965,
-1.54767317228876));
#68481=CARTESIAN_POINT('Ctrl Pts',(0.234927480781002,-0.0325808343269141,
-1.54762767117023));
#68482=CARTESIAN_POINT('Ctrl Pts',(0.235112675384859,-0.0312170900386859,
-1.54753479408695));
#68483=CARTESIAN_POINT('Ctrl Pts',(0.23520435644733,-0.0305186431263219,
-1.54748743403413));
#68484=CARTESIAN_POINT('Ctrl Pts',(0.235432975287881,-0.028714726930122,
-1.5473656252953));
#68485=CARTESIAN_POINT('Ctrl Pts',(0.235565241515327,-0.0276086672510516,
-1.54729143334992));
#68486=CARTESIAN_POINT('Ctrl Pts',(0.236098697966602,-0.0228644339758852,
-1.54697515882675));
#68487=CARTESIAN_POINT('Ctrl Pts',(0.23642345782649,-0.0192179523995993,
-1.54673699223175));
#68488=CARTESIAN_POINT('Ctrl Pts',(0.237092526549318,-0.0090449698864053,
-1.54608259769615));
#68489=CARTESIAN_POINT('Ctrl Pts',(0.237251750755394,-0.00250933525563609,
-1.54567361576959));
#68490=CARTESIAN_POINT('Ctrl Pts',(0.237074360950808,0.00794202820876042,
-1.54502644709862));
#68491=CARTESIAN_POINT('Ctrl Pts',(0.236910833666278,0.0118569134303206,
-1.5447855775441));
#68492=CARTESIAN_POINT('Ctrl Pts',(0.235447125741487,0.0338274066397509,
-1.54343455705116));
#68493=CARTESIAN_POINT('Ctrl Pts',(0.232180434876699,0.0516894852950028,
-1.54233338054061));
#68494=CARTESIAN_POINT('Ctrl Pts',(0.226014732182807,0.0719644789403343,
-1.54096289516608));
#68495=CARTESIAN_POINT('Ctrl Pts',(0.225057166030109,0.0749053801037273,
-1.54076117758595));
#68496=CARTESIAN_POINT('Ctrl Pts',(0.223552564501143,0.079236733408524,
-1.54045931095087));
#68497=CARTESIAN_POINT('Ctrl Pts',(0.223049431365746,0.0806421726657788,
-1.54036060635765));
#68498=CARTESIAN_POINT('Ctrl Pts',(0.222127830795571,0.0831419258734293,
-1.54018365116373));
#68499=CARTESIAN_POINT('Ctrl Pts',(0.221714455426029,0.0842380746603786,
-1.54010557230142));
#68500=CARTESIAN_POINT('Ctrl Pts',(0.220822055629857,0.0865523752381976,
-1.53993967557087));
#68501=CARTESIAN_POINT('Ctrl Pts',(0.220341035212367,0.087769710004237,
-1.53985179282678));
#68502=CARTESIAN_POINT('Ctrl Pts',(0.21902550993899,0.091019974198752,-1.53961544748848));
#68503=CARTESIAN_POINT('Ctrl Pts',(0.218172803279667,0.0930453494221007,
-1.53946637526698));
#68504=CARTESIAN_POINT('Ctrl Pts',(0.213553675006278,0.103604108676579,
-1.53867952657932));
#68505=CARTESIAN_POINT('Ctrl Pts',(0.209314887335971,0.111920602462604,
-1.53802576850633));
#68506=CARTESIAN_POINT('Ctrl Pts',(0.199197372849681,0.129175816892105,
-1.53659531412792));
#68507=CARTESIAN_POINT('Ctrl Pts',(0.193181233905292,0.138010747883932,
-1.53581596621799));
#68508=CARTESIAN_POINT('Ctrl Pts',(0.179151971643283,0.155890249861244,
-1.5341562542592));
#68509=CARTESIAN_POINT('Ctrl Pts',(0.171000524460262,0.164791011818302,
-1.53327806041202));
#68510=CARTESIAN_POINT('Ctrl Pts',(0.160691007038307,0.174455435602565,
-1.53229227614546));
#68511=CARTESIAN_POINT('Ctrl Pts',(0.159156288233608,0.175856689966613,
-1.53214849088208));
#68512=CARTESIAN_POINT('Ctrl Pts',(0.156979957509692,0.177791927058622,
-1.53194893903163));
#68513=CARTESIAN_POINT('Ctrl Pts',(0.156353696833787,0.178342922276559,
-1.53189200969239));
#68514=CARTESIAN_POINT('Ctrl Pts',(0.155217574750184,0.17933191815341,-1.53178964018432));
#68515=CARTESIAN_POINT('Ctrl Pts',(0.154708734540378,0.179771076308688,
-1.5317441165398));
#68516=CARTESIAN_POINT('Ctrl Pts',(0.153663151867028,0.180665746427945,
-1.53165124797291));
#68517=CARTESIAN_POINT('Ctrl Pts',(0.153126237508268,0.181121041277761,
-1.5316039185876));
#68518=CARTESIAN_POINT('Ctrl Pts',(0.15173616977246,0.1822891971724,-1.53148228226324));
#68519=CARTESIAN_POINT('Ctrl Pts',(0.150880005006412,0.182998472216423,
-1.53140823068345));
#68520=CARTESIAN_POINT('Ctrl Pts',(0.147199355803761,0.186004251457002,
-1.53109340631247));
#68521=CARTESIAN_POINT('Ctrl Pts',(0.144327022069157,0.188241722628779,
-1.53085650512341));
#68522=CARTESIAN_POINT('Ctrl Pts',(0.136201568036226,0.194275852817154,
-1.5302067416342));
#68523=CARTESIAN_POINT('Ctrl Pts',(0.130842459506234,0.197924826773105,
-1.52980100209372));
#68524=CARTESIAN_POINT('Ctrl Pts',(0.121647353085139,0.203648776817385,
-1.52913022882568));
#68525=CARTESIAN_POINT('Ctrl Pts',(0.117891831130865,0.205845622711681,
-1.52886294117754));
#68526=CARTESIAN_POINT('Ctrl Pts',(0.098557526277699,0.216452717935185,
-1.52751035921817));
#68527=CARTESIAN_POINT('Ctrl Pts',(0.082134568345313,0.223202134276999,
-1.52643183025522));
#68528=CARTESIAN_POINT('Ctrl Pts',(0.0621134700864995,0.228918407631067,
-1.5250856418275));
#68529=CARTESIAN_POINT('Ctrl Pts',(0.0590960108539749,0.229715869147917,
-1.52488212178102));
#68530=CARTESIAN_POINT('Ctrl Pts',(0.0546081342243292,0.230807661679454,
-1.52457807534288));
#68531=CARTESIAN_POINT('Ctrl Pts',(0.0531491686735988,0.231147984437338,
-1.52447902459574));
#68532=CARTESIAN_POINT('Ctrl Pts',(0.0505431752407854,0.231729889920066,
-1.52430168525066));
#68533=CARTESIAN_POINT('Ctrl Pts',(0.0493973861112057,0.231976836357658,
-1.52422357127617));
#68534=CARTESIAN_POINT('Ctrl Pts',(0.0469712672034625,0.232480936817258,
-1.52405784833121));
#68535=CARTESIAN_POINT('Ctrl Pts',(0.0456905538446019,0.232736028790258,
-1.52397017633583));
#68536=CARTESIAN_POINT('Ctrl Pts',(0.0422629836936132,0.233389349151447,
-1.52373500223649));
#68537=CARTESIAN_POINT('Ctrl Pts',(0.0401126681567993,0.233768520945373,
-1.52358690100049));
#68538=CARTESIAN_POINT('Ctrl Pts',(0.0289672507140675,0.235575524796537,
-1.52281614370083));
#68539=CARTESIAN_POINT('Ctrl Pts',(0.0199016736731542,0.236513879936278,
-1.5221782883199));
#68540=CARTESIAN_POINT('Ctrl Pts',(-1.4024014571486E-5,0.237422171039584,
-1.52075395183144));
#68541=CARTESIAN_POINT('Ctrl Pts',(-0.0108539915600171,0.23717387463299,
-1.51996361814138));
#68542=CARTESIAN_POINT('Ctrl Pts',(-0.028443735834832,0.235562387824582,
-1.5186736308643));
#68543=CARTESIAN_POINT('Ctrl Pts',(-0.0352170706831922,0.234645232886711,
-1.51817526932316));
#68544=CARTESIAN_POINT('Ctrl Pts',(-0.0419392871413391,0.233437522303241,
-1.51768363453027));
#68545=CARTESIAN_POINT('Origin',(0.,0.,-2.1456589891905));
#68546=CARTESIAN_POINT('',(-0.0419392741322232,0.233437524640453,-1.39788629978594));
#68547=CARTESIAN_POINT('',(-0.0419392748056672,0.233437524519463,-1.41774927189049));
#68548=CARTESIAN_POINT('',(-0.0419392741328076,0.233437524640348,-2.1456589891905));
#68549=CARTESIAN_POINT('',(-0.237174975146335,-0.000108578706768982,-1.47575156156963));
#68550=CARTESIAN_POINT('Ctrl Pts',(-0.0419392741322232,0.233437524640453,
-1.39788629978594));
#68551=CARTESIAN_POINT('Ctrl Pts',(-0.0417180158744456,0.233477275793321,
-1.39790131808953));
#68552=CARTESIAN_POINT('Ctrl Pts',(-0.0414967013879086,0.233516712322986,
-1.39791634640987));
#68553=CARTESIAN_POINT('Ctrl Pts',(-0.03997497007651,0.233785641439333,
-1.39801972238812));
#68554=CARTESIAN_POINT('Ctrl Pts',(-0.0386727356578481,0.234004580660391,
-1.39810840368024));
#68555=CARTESIAN_POINT('Ctrl Pts',(-0.0351472170219117,0.234567079239536,
-1.39834910766252));
#68556=CARTESIAN_POINT('Ctrl Pts',(-0.0329208096375801,0.23488989167629,
-1.39850177937129));
#68557=CARTESIAN_POINT('Ctrl Pts',(-0.0205616969838143,0.236502708322871,
-1.39935321128919));
#68558=CARTESIAN_POINT('Ctrl Pts',(-0.0103598125379389,0.237168582931925,
-1.40007131630334));
#68559=CARTESIAN_POINT('Ctrl Pts',(0.00983488366610878,0.237181181891399,
-1.40152083381518));
#68560=CARTESIAN_POINT('Ctrl Pts',(0.0198076613864323,0.236557124939314,
-1.4022501113566));
#68561=CARTESIAN_POINT('Ctrl Pts',(0.0341751828074724,0.234743020647505,
-1.4033075762913));
#68562=CARTESIAN_POINT('Ctrl Pts',(0.0386226802781399,0.234052385055344,
-1.40363577598582));
#68563=CARTESIAN_POINT('Ctrl Pts',(0.0511782513117806,0.231735024255397,
-1.40456114737663));
#68564=CARTESIAN_POINT('Ctrl Pts',(0.0592255204948725,0.229810145643756,
-1.40515298587548));
#68565=CARTESIAN_POINT('Ctrl Pts',(0.0684271973005747,0.227093492737877,
-1.40581676211146));
#68566=CARTESIAN_POINT('Ctrl Pts',(0.0696946706410852,0.226707716803832,
-1.4059078976691));
#68567=CARTESIAN_POINT('Ctrl Pts',(0.0717499760047658,0.226063285224635,
-1.40605512569324));
#68568=CARTESIAN_POINT('Ctrl Pts',(0.0725397807810432,0.225811089719167,
-1.40611156779772));
#68569=CARTESIAN_POINT('Ctrl Pts',(0.0739516835641688,0.225352077547534,
-1.40621220635755));
#68570=CARTESIAN_POINT('Ctrl Pts',(0.0745742607516494,0.22514681881604,
-1.40625649022976));
#68571=CARTESIAN_POINT('Ctrl Pts',(0.0759436644003392,0.224689033840108,
-1.40635369094314));
#68572=CARTESIAN_POINT('Ctrl Pts',(0.0766900875522137,0.224435363985013,
-1.40640654024647));
#68573=CARTESIAN_POINT('Ctrl Pts',(0.0788530244302914,0.223688245316555,
-1.40655933775896));
#68574=CARTESIAN_POINT('Ctrl Pts',(0.080266170777264,0.223185063725022,
-1.4066587354356));
#68575=CARTESIAN_POINT('Ctrl Pts',(0.0936881257930744,0.218261909338375,
-1.40759953923139));
#68576=CARTESIAN_POINT('Ctrl Pts',(0.105327294131923,0.212889603563721,
-1.40839094762103));
#68577=CARTESIAN_POINT('Ctrl Pts',(0.13287309346103,0.197360026008351,-1.41033273705339));
#68578=CARTESIAN_POINT('Ctrl Pts',(0.148108278852666,0.18619906552795,-1.41147468771679));
#68579=CARTESIAN_POINT('Ctrl Pts',(0.164076912938587,0.171288981820243,
-1.41288836970618));
#68580=CARTESIAN_POINT('Ctrl Pts',(0.166250179703749,0.169180451128731,
-1.41308594002728));
#68581=CARTESIAN_POINT('Ctrl Pts',(0.169425175322059,0.165979766785024,
-1.4133828055702));
#68582=CARTESIAN_POINT('Ctrl Pts',(0.170458054400523,0.164918842275546,
-1.41348072702198));
#68583=CARTESIAN_POINT('Ctrl Pts',(0.172289593164401,0.163001984611306,
-1.41365684200265));
#68584=CARTESIAN_POINT('Ctrl Pts',(0.173091984094836,0.162149671161329,
-1.4137348704784));
#68585=CARTESIAN_POINT('Ctrl Pts',(0.17478358582726,0.160325958570626,-1.41390126213349));
#68586=CARTESIAN_POINT('Ctrl Pts',(0.175671078058892,0.15935302657418,-1.41398969474534));
#68587=CARTESIAN_POINT('Ctrl Pts',(0.178041482653542,0.156710552792748,
-1.41422901305029));
#68588=CARTESIAN_POINT('Ctrl Pts',(0.179508963501372,0.155027411542843,
-1.41438053502395));
#68589=CARTESIAN_POINT('Ctrl Pts',(0.187361030769182,0.145760421728771,
-1.41521012223092));
#68590=CARTESIAN_POINT('Ctrl Pts',(0.193288262647181,0.137803687082492,
-1.41590635290925));
#68591=CARTESIAN_POINT('Ctrl Pts',(0.204268242513911,0.120956492033935,
-1.41734800311278));
#68592=CARTESIAN_POINT('Ctrl Pts',(0.20927950829322,0.112062712993019,-1.41809280223622));
#68593=CARTESIAN_POINT('Ctrl Pts',(0.214642323710848,0.100922483452259,
-1.41899567148415));
#68594=CARTESIAN_POINT('Ctrl Pts',(0.215555299066054,0.0989575057310869,
-1.41915381260305));
#68595=CARTESIAN_POINT('Ctrl Pts',(0.220801063905372,0.0872499738251653,
-1.42008870073981));
#68596=CARTESIAN_POINT('Ctrl Pts',(0.224500325589006,0.0772355193366812,
-1.42085914020115));
#68597=CARTESIAN_POINT('Ctrl Pts',(0.227896164392543,0.0657050634842037,
-1.42169114483246));
#68598=CARTESIAN_POINT('Ctrl Pts',(0.228267880313989,0.0644018023238318,
-1.42178440382792));
#68599=CARTESIAN_POINT('Ctrl Pts',(0.228851382788145,0.0622874600940939,
-1.42193436350777));
#68600=CARTESIAN_POINT('Ctrl Pts',(0.229070070039358,0.061478338913267,
-1.42199143477438));
#68601=CARTESIAN_POINT('Ctrl Pts',(0.22945228028266,0.06003384122748,-1.42209273955511));
#68602=CARTESIAN_POINT('Ctrl Pts',(0.229617460816204,0.0593989288000395,
-1.42213706563693));
#68603=CARTESIAN_POINT('Ctrl Pts',(0.229973518346591,0.0580066502121284,
-1.42223382471026));
#68604=CARTESIAN_POINT('Ctrl Pts',(0.230163290180798,0.05724902188514,-1.42228619447312));
#68605=CARTESIAN_POINT('Ctrl Pts',(0.230698261311157,0.0550675872870964,
-1.42243620611052));
#68606=CARTESIAN_POINT('Ctrl Pts',(0.231034022972514,0.0536414712569274,
-1.42253332783677));
#68607=CARTESIAN_POINT('Ctrl Pts',(0.233624760573055,0.0421617196478598,
-1.42330819945264));
#68608=CARTESIAN_POINT('Ctrl Pts',(0.2352359390451,0.0319726239218326,-1.42395362207822));
#68609=CARTESIAN_POINT('Ctrl Pts',(0.237663091612336,0.00556783595630032,
-1.42559129702647));
#68610=CARTESIAN_POINT('Ctrl Pts',(0.237488122953125,-0.010683077692122,
-1.42656856752845));
#68611=CARTESIAN_POINT('Ctrl Pts',(0.234888007935024,-0.0335556617833019,
-1.4280191073462));
#68612=CARTESIAN_POINT('Ctrl Pts',(0.233827783020413,-0.040285396487299,
-1.42845480617632));
#68613=CARTESIAN_POINT('Ctrl Pts',(0.23206974185919,-0.0489887789261965,
-1.42903481620551));
#68614=CARTESIAN_POINT('Ctrl Pts',(0.231633354083273,-0.051012296321916,
-1.42917083735685));
#68615=CARTESIAN_POINT('Ctrl Pts',(0.230884016810966,-0.0542788509147047,
-1.42939243560929));
#68616=CARTESIAN_POINT('Ctrl Pts',(0.230587372652463,-0.0555255467241055,
-1.42947748895719));
#68617=CARTESIAN_POINT('Ctrl Pts',(0.229998495429776,-0.0579142662485055,
-1.42964140513735));
#68618=CARTESIAN_POINT('Ctrl Pts',(0.229707822124248,-0.0590566380975076,
-1.42972021551665));
#68619=CARTESIAN_POINT('Ctrl Pts',(0.229015822727977,-0.0616938331768712,
-1.42990314707741));
#68620=CARTESIAN_POINT('Ctrl Pts',(0.228608359557043,-0.0631869753556153,
-1.43000746413829));
#68621=CARTESIAN_POINT('Ctrl Pts',(0.227262413432004,-0.0679356693006557,
-1.43034166487229));
#68622=CARTESIAN_POINT('Ctrl Pts',(0.226268809838192,-0.0711750191416556,
-1.43057332177028));
#68623=CARTESIAN_POINT('Ctrl Pts',(0.223763820229987,-0.0787583675917747,
-1.43112463823769));
#68624=CARTESIAN_POINT('Ctrl Pts',(0.222194834380575,-0.0830817575420814,
-1.4314460544567));
#68625=CARTESIAN_POINT('Ctrl Pts',(0.211856710958257,-0.109176751618474,
-1.43342971160973));
#68626=CARTESIAN_POINT('Ctrl Pts',(0.200023261566123,-0.129588831847011,
-1.43518731180815));
#68627=CARTESIAN_POINT('Ctrl Pts',(0.183115788880297,-0.150777517222346,
-1.43710599965592));
#68628=CARTESIAN_POINT('Ctrl Pts',(0.180778147620777,-0.153572513004489,
-1.43736088086582));
#68629=CARTESIAN_POINT('Ctrl Pts',(0.177616866838394,-0.157180021258988,
-1.43769105721541));
#68630=CARTESIAN_POINT('Ctrl Pts',(0.176850510712848,-0.158041790249973,
-1.43777002309563));
#68631=CARTESIAN_POINT('Ctrl Pts',(0.175600041117248,-0.159427459641087,
-1.43789709743272));
#68632=CARTESIAN_POINT('Ctrl Pts',(0.175119808028802,-0.159954812988614,
-1.43794548326542));
#68633=CARTESIAN_POINT('Ctrl Pts',(0.174180724207529,-0.160976740729747,
-1.43803928086469));
#68634=CARTESIAN_POINT('Ctrl Pts',(0.173722133680186,-0.161471533170899,
-1.43808470945402));
#68635=CARTESIAN_POINT('Ctrl Pts',(0.172598408722607,-0.16267363830348,
-1.4381951319603));
#68636=CARTESIAN_POINT('Ctrl Pts',(0.171931020374284,-0.163378846879691,
-1.43825995641693));
#68637=CARTESIAN_POINT('Ctrl Pts',(0.169509534141475,-0.165906285757507,
-1.43849253890809));
#68638=CARTESIAN_POINT('Ctrl Pts',(0.167730572779489,-0.167704603526047,
-1.4386585071294));
#68639=CARTESIAN_POINT('Ctrl Pts',(0.163177058129923,-0.17216270525143,
-1.43907227369118));
#68640=CARTESIAN_POINT('Ctrl Pts',(0.16036592203834,-0.174784220662538,
-1.43931774981842));
#68641=CARTESIAN_POINT('Ctrl Pts',(0.146744586031513,-0.186881306487395,
-1.44046812851552));
#68642=CARTESIAN_POINT('Ctrl Pts',(0.135150896485953,-0.195430006833203,
-1.44133605221261));
#68643=CARTESIAN_POINT('Ctrl Pts',(0.111834438521158,-0.209549496725397,
-1.44301440210219));
#68644=CARTESIAN_POINT('Ctrl Pts',(0.100291255550789,-0.21531263792928,
-1.44381864326232));
#68645=CARTESIAN_POINT('Ctrl Pts',(0.086120809048198,-0.220999764494372,
-1.4448123411068));
#68646=CARTESIAN_POINT('Ctrl Pts',(0.0838901169891483,-0.221856118350098,
-1.44496889198576));
#68647=CARTESIAN_POINT('Ctrl Pts',(0.0803656021851481,-0.22314841056952,
-1.44521662615804));
#68648=CARTESIAN_POINT('Ctrl Pts',(0.0790802638549645,-0.223607144096794,
-1.44530704962001));
#68649=CARTESIAN_POINT('Ctrl Pts',(0.0767001855823566,-0.224433499315008,
-1.44547466666692));
#68650=CARTESIAN_POINT('Ctrl Pts',(0.0756065761486757,-0.224804269632509,
-1.44555175318055));
#68651=CARTESIAN_POINT('Ctrl Pts',(0.0731717810759798,-0.22560997087226,
-1.44572355194719));
#68652=CARTESIAN_POINT('Ctrl Pts',(0.0718293457237878,-0.226040955241188,
-1.44581839095064));
#68653=CARTESIAN_POINT('Ctrl Pts',(0.0679315346937054,-0.227254106186454,
-1.44609414010938));
#68654=CARTESIAN_POINT('Ctrl Pts',(0.0653667523079446,-0.228005063230244,
-1.44627605806188));
#68655=CARTESIAN_POINT('Ctrl Pts',(0.0502687969417475,-0.232150002322363,
-1.44735011117685));
#68656=CARTESIAN_POINT('Ctrl Pts',(0.037488629829059,-0.234552932241655,
-1.4482737957892));
#68657=CARTESIAN_POINT('Ctrl Pts',(0.0116579680877888,-0.237244200540142,
-1.45015765546247));
#68658=CARTESIAN_POINT('Ctrl Pts',(-0.00135059597956813,-0.237526618653894,
-1.45111455511102));
#68659=CARTESIAN_POINT('Ctrl Pts',(-0.0207136129501226,-0.236355654367896,
-1.45251056038645));
#68660=CARTESIAN_POINT('Ctrl Pts',(-0.0270927506522178,-0.235709669280235,
-1.4529655266607));
#68661=CARTESIAN_POINT('Ctrl Pts',(-0.0347895741262106,-0.234613573098142,
-1.45350269108032));
#68662=CARTESIAN_POINT('Ctrl Pts',(-0.0361390404583626,-0.234409498795688,
-1.4535964256256));
#68663=CARTESIAN_POINT('Ctrl Pts',(-0.0382448730749671,-0.234072424364735,
-1.45374192339876));
#68664=CARTESIAN_POINT('Ctrl Pts',(-0.0390024565063026,-0.233947384241106,
-1.45379410986171));
#68665=CARTESIAN_POINT('Ctrl Pts',(-0.0404014421049144,-0.233709495303012,
-1.45389017247768));
#68666=CARTESIAN_POINT('Ctrl Pts',(-0.0410429860422308,-0.233597684131298,
-1.45393410314572));
#68667=CARTESIAN_POINT('Ctrl Pts',(-0.0425235031536307,-0.233333365346629,
-1.45403521088997));
#68668=CARTESIAN_POINT('Ctrl Pts',(-0.0433621221315177,-0.233178974449585,
-1.45409228119432));
#68669=CARTESIAN_POINT('Ctrl Pts',(-0.0459926076329107,-0.23268001649431,
-1.45427071397988));
#68670=CARTESIAN_POINT('Ctrl Pts',(-0.0477813926821057,-0.232319282557509,
-1.45439120696135));
#68671=CARTESIAN_POINT('Ctrl Pts',(-0.0519974765152204,-0.231418291479187,
-1.45467358720743));
#68672=CARTESIAN_POINT('Ctrl Pts',(-0.054420833424717,-0.23086042785102,
-1.45483462335879));
#68673=CARTESIAN_POINT('Ctrl Pts',(-0.0632751560660881,-0.228674958606493,
-1.4554198241311));
#68674=CARTESIAN_POINT('Ctrl Pts',(-0.0696462064266515,-0.226815786063484,
-1.4558347429976));
#68675=CARTESIAN_POINT('Ctrl Pts',(-0.0883866319381735,-0.220482730437716,
-1.45705887381467));
#68676=CARTESIAN_POINT('Ctrl Pts',(-0.100470320113976,-0.215245331034556,
-1.45785421754155));
#68677=CARTESIAN_POINT('Ctrl Pts',(-0.120884682909554,-0.204301682727748,
-1.45929249561858));
#68678=CARTESIAN_POINT('Ctrl Pts',(-0.129401950223741,-0.199016036320406,
-1.45992483000394));
#68679=CARTESIAN_POINT('Ctrl Pts',(-0.139421971966469,-0.191882057641465,
-1.46072617197113));
#68680=CARTESIAN_POINT('Ctrl Pts',(-0.141265559083674,-0.190528873219768,
-1.46087612721574));
#68681=CARTESIAN_POINT('Ctrl Pts',(-0.144159223654674,-0.188339849483859,
-1.46111569257743));
#68682=CARTESIAN_POINT('Ctrl Pts',(-0.145222301037575,-0.187521368980477,
-1.46120462463978));
#68683=CARTESIAN_POINT('Ctrl Pts',(-0.147156294487133,-0.186006047127048,
-1.4613681416619));
#68684=CARTESIAN_POINT('Ctrl Pts',(-0.148029353980594,-0.185311993302888,
-1.46144261437169));
#68685=CARTESIAN_POINT('Ctrl Pts',(-0.148929261989617,-0.184586178291161,
-1.46152007057849));
#68686=CARTESIAN_POINT('Ctrl Pts',(-0.148961044335912,-0.184560530892332,
-1.46152280702652));
#68687=CARTESIAN_POINT('Ctrl Pts',(-0.149021894573208,-0.184511400621211,
-1.46152804793698));
#68688=CARTESIAN_POINT('Ctrl Pts',(-0.149050963544898,-0.184487919083402,
-1.46153055234557));
#68689=CARTESIAN_POINT('Ctrl Pts',(-0.149106764748591,-0.184442821798687,
-1.46153536129486));
#68690=CARTESIAN_POINT('Ctrl Pts',(-0.149133497834717,-0.184421207106,-1.46153766579299));
#68691=CARTESIAN_POINT('Ctrl Pts',(-0.149184937196628,-0.184379597973357,
-1.46154210130256));
#68692=CARTESIAN_POINT('Ctrl Pts',(-0.149209644156208,-0.184359604376758,
-1.46154423227993));
#68693=CARTESIAN_POINT('Ctrl Pts',(-0.14925728815938,-0.184321033600422,
-1.46154834263563));
#68694=CARTESIAN_POINT('Ctrl Pts',(-0.149280225756973,-0.184302457102899,
-1.4615503219864));
#68695=CARTESIAN_POINT('Ctrl Pts',(-0.149324545929468,-0.184266549773775,
-1.46155414741404));
#68696=CARTESIAN_POINT('Ctrl Pts',(-0.149345928957762,-0.18424921949988,
-1.46155599346837));
#68697=CARTESIAN_POINT('Ctrl Pts',(-0.149387321254059,-0.18421566040183,
-1.46155956777281));
#68698=CARTESIAN_POINT('Ctrl Pts',(-0.149407330896319,-0.184199432038166,
-1.46156129600429));
#68699=CARTESIAN_POINT('Ctrl Pts',(-0.149446130482059,-0.184167954038028,
-1.46156464782109));
#68700=CARTESIAN_POINT('Ctrl Pts',(-0.149464920737452,-0.184152704784807,
-1.46156627139091));
#68701=CARTESIAN_POINT('Ctrl Pts',(-0.149501413410188,-0.184123079849844,
-1.46156942515416));
#68702=CARTESIAN_POINT('Ctrl Pts',(-0.149519116089556,-0.184108704489585,
-1.4615709553346));
#68703=CARTESIAN_POINT('Ctrl Pts',(-0.150638741112207,-0.183199251358231,
-1.46166775112811));
#68704=CARTESIAN_POINT('Ctrl Pts',(-0.151732585497013,-0.182294317979909,
-1.46176341422604));
#68705=CARTESIAN_POINT('Ctrl Pts',(-0.154073979078429,-0.180321618032845,
-1.46197059519738));
#68706=CARTESIAN_POINT('Ctrl Pts',(-0.155318688741653,-0.179250611296165,
-1.46208224283019));
#68707=CARTESIAN_POINT('Ctrl Pts',(-0.158604971914649,-0.176363009745009,
-1.46238111300163));
#68708=CARTESIAN_POINT('Ctrl Pts',(-0.160626388404096,-0.174523954223284,
-1.46256925180537));
#68709=CARTESIAN_POINT('Ctrl Pts',(-0.166798035983302,-0.168711020511071,
-1.46315734558808));
#68710=CARTESIAN_POINT('Ctrl Pts',(-0.170835719935327,-0.164621204565371,
-1.46356196397502));
#68711=CARTESIAN_POINT('Ctrl Pts',(-0.190433080646042,-0.143272721018108,
-1.46562831269273));
#68712=CARTESIAN_POINT('Ctrl Pts',(-0.203543292903344,-0.123942804942166,
-1.46737177133099));
#68713=CARTESIAN_POINT('Ctrl Pts',(-0.214616452691466,-0.10097957856647,
-1.46915379271452));
#68714=CARTESIAN_POINT('Ctrl Pts',(-0.215569780863005,-0.0989280929213326,
-1.46931054233741));
#68715=CARTESIAN_POINT('Ctrl Pts',(-0.216846180175783,-0.0960752821580489,
-1.46952484624184));
#68716=CARTESIAN_POINT('Ctrl Pts',(-0.217194407805216,-0.0952854394698288,
-1.46958379475124));
#68717=CARTESIAN_POINT('Ctrl Pts',(-0.217784905235448,-0.093926027963194,
-1.4696845713024));
#68718=CARTESIAN_POINT('Ctrl Pts',(-0.218029268836749,-0.0933573865871296,
-1.46972652277562));
#68719=CARTESIAN_POINT('Ctrl Pts',(-0.218537693353963,-0.0921613829037323,
-1.46981432171694));
#68720=CARTESIAN_POINT('Ctrl Pts',(-0.218801284065018,-0.0915338299492834,
-1.46986013882558));
#68721=CARTESIAN_POINT('Ctrl Pts',(-0.219446157546607,-0.0899798212374725,
-1.46997299494483));
#68722=CARTESIAN_POINT('Ctrl Pts',(-0.219824284505007,-0.0890520540117648,
-1.47003984641765));
#68723=CARTESIAN_POINT('Ctrl Pts',(-0.221215782656704,-0.085575017414246,
-1.47028853076473));
#68724=CARTESIAN_POINT('Ctrl Pts',(-0.222190825871268,-0.0830105089607385,
-1.47046823267838));
#68725=CARTESIAN_POINT('Ctrl Pts',(-0.224579214202513,-0.0763848317532693,
-1.47092445191497));
#68726=CARTESIAN_POINT('Ctrl Pts',(-0.225927062428807,-0.0723009883580598,
-1.47119799395673));
#68727=CARTESIAN_POINT('Ctrl Pts',(-0.233791840176752,-0.0460979656414309,
-1.47291810075487));
#68728=CARTESIAN_POINT('Ctrl Pts',(-0.23716441931536,-0.0231663128024612,
-1.47427942647711));
#68729=CARTESIAN_POINT('Ctrl Pts',(-0.237174975146335,-0.000108578706768982,
-1.47575156156963));
#68730=CARTESIAN_POINT('Ctrl Pts',(-0.237174975268681,-0.000108311127839238,
-1.47575157865337));
#68731=CARTESIAN_POINT('Ctrl Pts',(-0.237176942139156,0.00419865589782415,
-1.47602655971673));
#68732=CARTESIAN_POINT('Ctrl Pts',(-0.237061591014441,0.00850470375074625,
-1.47630458183463));
#68733=CARTESIAN_POINT('Ctrl Pts',(-0.23674953108947,0.0142762308575994,
-1.47668253285185));
#68734=CARTESIAN_POINT('Ctrl Pts',(-0.236656282952957,0.0157465811043548,
-1.47677928072747));
#68735=CARTESIAN_POINT('Ctrl Pts',(-0.236466528519261,0.0183538326312364,
-1.47695170294741));
#68736=CARTESIAN_POINT('Ctrl Pts',(-0.236375505087181,0.0194910954087698,
-1.47702720537737));
#68737=CARTESIAN_POINT('Ctrl Pts',(-0.236177920258972,0.0217543018139207,
-1.47717806497058));
#68738=CARTESIAN_POINT('Ctrl Pts',(-0.236071503487122,0.0228802279399359,
-1.47725341569058));
#68739=CARTESIAN_POINT('Ctrl Pts',(-0.235826903284639,0.0252844911395987,
-1.47741497731558));
#68740=CARTESIAN_POINT('Ctrl Pts',(-0.235686369531058,0.0265625471159161,
-1.47750125985415));
#68741=CARTESIAN_POINT('Ctrl Pts',(-0.23529017709805,0.0299145391006344,
-1.47772863696547));
#68742=CARTESIAN_POINT('Ctrl Pts',(-0.235017494159398,0.0319863101926931,
-1.47787026237332));
#68743=CARTESIAN_POINT('Ctrl Pts',(-0.233711756277124,0.040986079465285,
-1.47849040316061));
#68744=CARTESIAN_POINT('Ctrl Pts',(-0.232399548797854,0.0478693631792046,
-1.4789775804693));
#68745=CARTESIAN_POINT('Ctrl Pts',(-0.227985198379171,0.0664994283455132,
-1.48033214961534));
#68746=CARTESIAN_POINT('Ctrl Pts',(-0.224282571822886,0.0780813465774943,
-1.48121515174549));
#68747=CARTESIAN_POINT('Ctrl Pts',(-0.215995457900528,0.0984643019394832,
-1.48282214009222));
#68748=CARTESIAN_POINT('Ctrl Pts',(-0.211714293275484,0.107360772627073,
-1.48354300050456));
#68749=CARTESIAN_POINT('Ctrl Pts',(-0.205345684533884,0.118722889252388,
-1.48447141503645));
#68750=CARTESIAN_POINT('Ctrl Pts',(-0.203744912691526,0.121449525291398,
-1.48469479268469));
#68751=CARTESIAN_POINT('Ctrl Pts',(-0.200944168466027,0.126008786036631,
-1.48506832513154));
#68752=CARTESIAN_POINT('Ctrl Pts',(-0.199772488970182,0.127858228158493,
-1.48521985099335));
#68753=CARTESIAN_POINT('Ctrl Pts',(-0.198073755895315,0.130459224207009,
-1.48543267126681));
#68754=CARTESIAN_POINT('Ctrl Pts',(-0.197567732101147,0.131224286083186,
-1.4854952354785));
#68755=CARTESIAN_POINT('Ctrl Pts',(-0.196687051479929,0.132539152683675,
-1.48560267373702));
#68756=CARTESIAN_POINT('Ctrl Pts',(-0.196314500126047,0.133090346382632,
-1.4856476847727));
#68757=CARTESIAN_POINT('Ctrl Pts',(-0.19552604670506,0.134246357187083,
-1.48574201974106));
#68758=CARTESIAN_POINT('Ctrl Pts',(-0.195109651966513,0.134850817960496,
-1.48579131001653));
#68759=CARTESIAN_POINT('Ctrl Pts',(-0.193978175510031,0.136477117105381,
-1.4859238562774));
#68760=CARTESIAN_POINT('Ctrl Pts',(-0.193257816880505,0.137495281558845,
-1.48600676442978));
#68761=CARTESIAN_POINT('Ctrl Pts',(-0.189863940379462,0.142212859993805,
-1.48639080806166));
#68762=CARTESIAN_POINT('Ctrl Pts',(-0.187091828439924,0.14584055565954,
-1.48668583075819));
#68763=CARTESIAN_POINT('Ctrl Pts',(-0.181448784345523,0.152799308373986,
-1.48725611972243));
#68764=CARTESIAN_POINT('Ctrl Pts',(-0.178586588391015,0.15613495478841,
-1.48753159899791));
#68765=CARTESIAN_POINT('Ctrl Pts',(-0.16427753170964,0.17190229910262,-1.48885475749445));
#68766=CARTESIAN_POINT('Ctrl Pts',(-0.151617324412263,0.183165807133074,
-1.48986924296888));
#68767=CARTESIAN_POINT('Ctrl Pts',(-0.133652607439386,0.195999468553181,
-1.49125403085675));
#68768=CARTESIAN_POINT('Ctrl Pts',(-0.129340536682154,0.198871393849842,
-1.49158245329919));
#68769=CARTESIAN_POINT('Ctrl Pts',(-0.122774301136254,0.202940710414367,
-1.4920795099872));
#68770=CARTESIAN_POINT('Ctrl Pts',(-0.120589106158515,0.204246732317007,
-1.49224443472819));
#68771=CARTESIAN_POINT('Ctrl Pts',(-0.116551409552228,0.206572551991343,
-1.4925485933385));
#68772=CARTESIAN_POINT('Ctrl Pts',(-0.114705465280959,0.207603241940051,
-1.4926874302666));
#68773=CARTESIAN_POINT('Ctrl Pts',(-0.111723549725092,0.209216294145764,
-1.49291148799726));
#68774=CARTESIAN_POINT('Ctrl Pts',(-0.110596198904925,0.209814417948167,
-1.49299614643234));
#68775=CARTESIAN_POINT('Ctrl Pts',(-0.108479606801616,0.210915592323176,
-1.49315502775177));
#68776=CARTESIAN_POINT('Ctrl Pts',(-0.107491551325656,0.211420856346486,
-1.49322916992968));
#68777=CARTESIAN_POINT('Ctrl Pts',(-0.105192700118224,0.212576144309204,
-1.49340163206101));
#68778=CARTESIAN_POINT('Ctrl Pts',(-0.103879374560099,0.213221004269078,
-1.49350012919098));
#68779=CARTESIAN_POINT('Ctrl Pts',(-0.0999973484469963,0.215082750961096,
-1.49379123460219));
#68780=CARTESIAN_POINT('Ctrl Pts',(-0.097412719933139,0.21626562424125,
-1.49398500316672));
#68781=CARTESIAN_POINT('Ctrl Pts',(-0.0778616014625455,0.22479174676208,
-1.4954509833057));
#68782=CARTESIAN_POINT('Ctrl Pts',(-0.0601175388771464,0.230171626328724,
-1.49679027381849));
#68783=CARTESIAN_POINT('Ctrl Pts',(-0.0419392735583878,0.233437524743548,
-1.49813919362704));
#68784=CARTESIAN_POINT('',(-0.237174890926,0.00020565781626766,-1.49572693511662));
#68785=CARTESIAN_POINT('Ctrl Pts',(-0.0419392871413391,0.233437522303241,
-1.51768363453027));
#68786=CARTESIAN_POINT('Ctrl Pts',(-0.0471714318927572,0.232497517376314,
-1.51730097734907));
#68787=CARTESIAN_POINT('Ctrl Pts',(-0.0523726113577256,0.231381492634979,
-1.51692242868031));
#68788=CARTESIAN_POINT('Ctrl Pts',(-0.0595435759879914,0.229588401993189,
-1.51640681856276));
#68789=CARTESIAN_POINT('Ctrl Pts',(-0.0615466280965262,0.229059566642998,
-1.51626349131255));
#68790=CARTESIAN_POINT('Ctrl Pts',(-0.0643451390067523,0.228281356278343,
-1.51606446676699));
#68791=CARTESIAN_POINT('Ctrl Pts',(-0.0651465346722758,0.228053948904293,
-1.51600761450086));
#68792=CARTESIAN_POINT('Ctrl Pts',(-0.0665920699758293,0.227635516121258,
-1.51590534239749));
#68793=CARTESIAN_POINT('Ctrl Pts',(-0.0672366264977959,0.22744596738836,
-1.51585983957156));
#68794=CARTESIAN_POINT('Ctrl Pts',(-0.0685553060007903,0.227052079500925,
-1.51576696314701));
#68795=CARTESIAN_POINT('Ctrl Pts',(-0.069229337734572,0.226847472140091,
-1.5157196054318));
#68796=CARTESIAN_POINT('Ctrl Pts',(-0.07096672319545,0.226311610905123,
-1.51559780983191));
#68797=CARTESIAN_POINT('Ctrl Pts',(-0.0720286881448549,0.225975859855935,
-1.51552362858249));
#68798=CARTESIAN_POINT('Ctrl Pts',(-0.0765688759044532,0.224505175025978,
-1.51520746481205));
#68799=CARTESIAN_POINT('Ctrl Pts',(-0.0800231582017908,0.223297255022286,
-1.51496939487481));
#68800=CARTESIAN_POINT('Ctrl Pts',(-0.0895609428699645,0.219712223293451,
-1.5143153546838));
#68801=CARTESIAN_POINT('Ctrl Pts',(-0.0955765161121631,0.217162992879243,
-1.51390662097318));
#68802=CARTESIAN_POINT('Ctrl Pts',(-0.115163937034608,0.207890533857276,
-1.51256485681436));
#68803=CARTESIAN_POINT('Ctrl Pts',(-0.12819633713789,0.200117243049169,
-1.51165196407475));
#68804=CARTESIAN_POINT('Ctrl Pts',(-0.14714250026197,0.186201699203614,
-1.51018228661346));
#68805=CARTESIAN_POINT('Ctrl Pts',(-0.153618568216865,0.180895827529956,
-1.5096504936495));
#68806=CARTESIAN_POINT('Ctrl Pts',(-0.161433200390491,0.173770496131775,
-1.50896075478208));
#68807=CARTESIAN_POINT('Ctrl Pts',(-0.163045133068398,0.172258954934857,
-1.50881572440554));
#68808=CARTESIAN_POINT('Ctrl Pts',(-0.165579775709671,0.169814718831981,
-1.50858307790472));
#68809=CARTESIAN_POINT('Ctrl Pts',(-0.166516299625678,0.168896485155012,
-1.50849608771351));
#68810=CARTESIAN_POINT('Ctrl Pts',(-0.168274474096228,0.167143810159057,
-1.50833078211358));
#68811=CARTESIAN_POINT('Ctrl Pts',(-0.169097657189908,0.166310956208243,
-1.50825253819057));
#68812=CARTESIAN_POINT('Ctrl Pts',(-0.169935727207506,0.165450385790348,
-1.50817199347841));
#68813=CARTESIAN_POINT('Ctrl Pts',(-0.169956823886617,0.165428714418298,
-1.50816996535157));
#68814=CARTESIAN_POINT('Ctrl Pts',(-0.169997390835274,0.165387026437855,
-1.50816606433595));
#68815=CARTESIAN_POINT('Ctrl Pts',(-0.170016861717709,0.165367010423533,
-1.50816419147391));
#68816=CARTESIAN_POINT('Ctrl Pts',(-0.170054362569926,0.165328446025054,
-1.50816058339409));
#68817=CARTESIAN_POINT('Ctrl Pts',(-0.170072393042106,0.16530989812789,
-1.50815884819826));
#68818=CARTESIAN_POINT('Ctrl Pts',(-0.170107171171144,0.165274110249768,
-1.50815550044037));
#68819=CARTESIAN_POINT('Ctrl Pts',(-0.170123919243162,0.165256870671227,
-1.50815388789646));
#68820=CARTESIAN_POINT('Ctrl Pts',(-0.170156268160965,0.165223562278893,
-1.50815077255669));
#68821=CARTESIAN_POINT('Ctrl Pts',(-0.170171869352431,0.165207493800046,
-1.50814926977595));
#68822=CARTESIAN_POINT('Ctrl Pts',(-0.171178221271394,0.164170705799564,
-1.50805231260119));
#68823=CARTESIAN_POINT('Ctrl Pts',(-0.172159752148018,0.163141115807951,
-1.50795645913309));
#68824=CARTESIAN_POINT('Ctrl Pts',(-0.175241965133097,0.159849194895349,
-1.50765129272431));
#68825=CARTESIAN_POINT('Ctrl Pts',(-0.177307693064479,0.157554726575058,
-1.50744051267301));
#68826=CARTESIAN_POINT('Ctrl Pts',(-0.182033563850823,0.152094882062049,
-1.50694313634357));
#68827=CARTESIAN_POINT('Ctrl Pts',(-0.184656819752731,0.148899049221967,
-1.50665515382933));
#68828=CARTESIAN_POINT('Ctrl Pts',(-0.193902552873168,0.137014965635709,
-1.50559538619098));
#68829=CARTESIAN_POINT('Ctrl Pts',(-0.200005691996505,0.127941302566981,
-1.50480634350546));
#68830=CARTESIAN_POINT('Ctrl Pts',(-0.213271536587294,0.104936496587429,
-1.50287015943048));
#68831=CARTESIAN_POINT('Ctrl Pts',(-0.219723944567586,0.0906525363456694,
-1.50171871634479));
#68832=CARTESIAN_POINT('Ctrl Pts',(-0.225361513210689,0.0739469146941872,
-1.50049060972911));
#68833=CARTESIAN_POINT('Ctrl Pts',(-0.225975355009574,0.0720492707501277,
-1.50035279911072));
#68834=CARTESIAN_POINT('Ctrl Pts',(-0.226823716508061,0.0693090632846857,
-1.50015644688656));
#68835=CARTESIAN_POINT('Ctrl Pts',(-0.227077608573104,0.0684726541757891,
-1.50009686531871));
#68836=CARTESIAN_POINT('Ctrl Pts',(-0.227515387546249,0.0670012391406965,
-1.49999268975817));
#68837=CARTESIAN_POINT('Ctrl Pts',(-0.227701251991867,0.0663668403783956,
-1.49994798364524));
#68838=CARTESIAN_POINT('Ctrl Pts',(-0.228091569782818,0.0650136511197901,
-1.49985307585601));
#68839=CARTESIAN_POINT('Ctrl Pts',(-0.228295280472651,0.0642946653366138,
-1.49980291676825));
#68840=CARTESIAN_POINT('Ctrl Pts',(-0.228846330875349,0.0623141203021017,
-1.49966545208398));
#68841=CARTESIAN_POINT('Ctrl Pts',(-0.229186640602815,0.0610506077530508,
-1.49957853992801));
#68842=CARTESIAN_POINT('Ctrl Pts',(-0.229925465995759,0.0582142011210711,
-1.49938505447321));
#68843=CARTESIAN_POINT('Ctrl Pts',(-0.230318336993567,0.0566398896464389,
-1.49927877226639));
#68844=CARTESIAN_POINT('Ctrl Pts',(-0.234983752348552,0.0370929145236071,
-1.4979714404334));
#68845=CARTESIAN_POINT('Ctrl Pts',(-0.237158875310678,0.0186829392630581,
-1.49686470085717));
#68846=CARTESIAN_POINT('Ctrl Pts',(-0.237174910684078,0.000205832454907566,
-1.4957269803945));
#68847=CARTESIAN_POINT('Ctrl Pts',(-0.237174910837396,0.000205655715385434,
-1.49572696951183));
#68848=CARTESIAN_POINT('Ctrl Pts',(-0.23718515411427,-0.0116075257210512,
-1.49499957749808));
#68849=CARTESIAN_POINT('Ctrl Pts',(-0.236312832446797,-0.0234039734777036,
-1.49426295624968));
#68850=CARTESIAN_POINT('Ctrl Pts',(-0.234249678855294,-0.0371971188456194,
-1.49336070055333));
#68851=CARTESIAN_POINT('Ctrl Pts',(-0.233905402214962,-0.0393039443191361,
-1.49322177898696));
#68852=CARTESIAN_POINT('Ctrl Pts',(-0.233288649907576,-0.0427824888308832,
-1.49299041613219));
#68853=CARTESIAN_POINT('Ctrl Pts',(-0.233032392784451,-0.0441569847375077,
-1.4928984792637));
#68854=CARTESIAN_POINT('Ctrl Pts',(-0.232549374032932,-0.0466263801682069,
-1.4927323339357));
#68855=CARTESIAN_POINT('Ctrl Pts',(-0.232326992812036,-0.0477221021034335,
-1.49265826547222));
#68856=CARTESIAN_POINT('Ctrl Pts',(-0.231879993566383,-0.0498473625473571,
-1.49251390886118));
#68857=CARTESIAN_POINT('Ctrl Pts',(-0.231656244919416,-0.0508770586564626,
-1.49244364996621));
#68858=CARTESIAN_POINT('Ctrl Pts',(-0.231138381236587,-0.0531860161629698,
-1.49228537244786));
#68859=CARTESIAN_POINT('Ctrl Pts',(-0.230840494736191,-0.0544643871314177,
-1.49219723484231));
#68860=CARTESIAN_POINT('Ctrl Pts',(-0.230011562238014,-0.0578927115593672,
-1.4919594721015));
#68861=CARTESIAN_POINT('Ctrl Pts',(-0.229461001239384,-0.0600377643207175,
-1.49180922453777));
#68862=CARTESIAN_POINT('Ctrl Pts',(-0.226667329155433,-0.0703219593690826,
-1.49108150580196));
#68863=CARTESIAN_POINT('Ctrl Pts',(-0.224020994548223,-0.078344240590904,
-1.49049116571055));
#68864=CARTESIAN_POINT('Ctrl Pts',(-0.217536292916935,-0.0949647457629705,
-1.48921967676172));
#68865=CARTESIAN_POINT('Ctrl Pts',(-0.213602244430633,-0.103510379630981,
-1.48853685472646));
#68866=CARTESIAN_POINT('Ctrl Pts',(-0.202654065488087,-0.123993942641413,
-1.48684137696234));
#68867=CARTESIAN_POINT('Ctrl Pts',(-0.195081844294637,-0.135596112891994,
-1.48582715899228));
#68868=CARTESIAN_POINT('Ctrl Pts',(-0.185086862425553,-0.148325249313563,
-1.48469506267158));
#68869=CARTESIAN_POINT('Ctrl Pts',(-0.183604956647462,-0.150155743061591,
-1.48453180002851));
#68870=CARTESIAN_POINT('Ctrl Pts',(-0.18148198663144,-0.152699664057588,
-1.48430459970435));
#68871=CARTESIAN_POINT('Ctrl Pts',(-0.180863543041265,-0.153431671285566,
-1.48423918693189));
#68872=CARTESIAN_POINT('Ctrl Pts',(-0.179803818540037,-0.154670679733016,
-1.48412843534704));
#68873=CARTESIAN_POINT('Ctrl Pts',(-0.17936479200404,-0.155179585531877,
-1.48408293638605));
#68874=CARTESIAN_POINT('Ctrl Pts',(-0.178510952469771,-0.156160864634009,
-1.48399519681754));
#68875=CARTESIAN_POINT('Ctrl Pts',(-0.178096419711479,-0.156633460998203,
-1.48395293546085));
#68876=CARTESIAN_POINT('Ctrl Pts',(-0.176961809306586,-0.157916668666113,
-1.48383815466504));
#68877=CARTESIAN_POINT('Ctrl Pts',(-0.176238033274916,-0.158724011844247,
-1.48376590464018));
#68878=CARTESIAN_POINT('Ctrl Pts',(-0.173423334868071,-0.161820704265128,
-1.48348851206267));
#68879=CARTESIAN_POINT('Ctrl Pts',(-0.171293030393398,-0.164074048478592,
-1.48328609608841));
#68880=CARTESIAN_POINT('Ctrl Pts',(-0.158280087499714,-0.177308765826556,
-1.48208899933428));
#68881=CARTESIAN_POINT('Ctrl Pts',(-0.146387995992337,-0.187247569120274,
-1.48115337117834));
#68882=CARTESIAN_POINT('Ctrl Pts',(-0.125386894107019,-0.201566879575749,
-1.47959338592066));
#68883=CARTESIAN_POINT('Ctrl Pts',(-0.116817546009545,-0.206651200659605,
-1.47897885270855));
#68884=CARTESIAN_POINT('Ctrl Pts',(-0.104472683996936,-0.212961807546468,
-1.47809983542279));
#68885=CARTESIAN_POINT('Ctrl Pts',(-0.10094736143533,-0.214655306997721,
-1.47784955854477));
#68886=CARTESIAN_POINT('Ctrl Pts',(-0.0946756484998511,-0.217479450113013,
-1.47740434320699));
#68887=CARTESIAN_POINT('Ctrl Pts',(-0.0919468366995563,-0.218647130285726,
-1.47721064681708));
#68888=CARTESIAN_POINT('Ctrl Pts',(-0.0878803065073688,-0.220297642778365,
-1.47692166089365));
#68889=CARTESIAN_POINT('Ctrl Pts',(-0.0865589343164124,-0.220820176677017,
-1.47682770749383));
#68890=CARTESIAN_POINT('Ctrl Pts',(-0.085221778457886,-0.221335106219755,
-1.47673255891512));
#68891=CARTESIAN_POINT('Ctrl Pts',(-0.0852105861826441,-0.221339415313327,
-1.47673176249643));
#68892=CARTESIAN_POINT('Ctrl Pts',(-0.0851876530705312,-0.221348242702754,
-1.47673013061405));
#68893=CARTESIAN_POINT('Ctrl Pts',(-0.0851759122015334,-0.221352760913206,
-1.47672929514757));
#68894=CARTESIAN_POINT('Ctrl Pts',(-0.0851518516321547,-0.221362017886643,
-1.47672758301405));
#68895=CARTESIAN_POINT('Ctrl Pts',(-0.0851395318944815,-0.221366756555765,
-1.47672670634379));
#68896=CARTESIAN_POINT('Ctrl Pts',(-0.0851142813630605,-0.221376466511165,
-1.47672490950785));
#68897=CARTESIAN_POINT('Ctrl Pts',(-0.0851013505310047,-0.221381437692319,
-1.4767239893388));
#68898=CARTESIAN_POINT('Ctrl Pts',(-0.0850748435006703,-0.22139162549623,
-1.47672210306178));
#68899=CARTESIAN_POINT('Ctrl Pts',(-0.0850612672580441,-0.221396842003182,
-1.47672113694993));
#68900=CARTESIAN_POINT('Ctrl Pts',(-0.0850334328468549,-0.22140753410071,
-1.47671915618346));
#68901=CARTESIAN_POINT('Ctrl Pts',(-0.08501917462876,-0.221413009562947,
-1.47671814152451));
#68902=CARTESIAN_POINT('Ctrl Pts',(-0.0849899372882785,-0.221424234089587,
-1.47671606088757));
#68903=CARTESIAN_POINT('Ctrl Pts',(-0.0849749581118485,-0.221429983011144,
-1.47671499490486));
#68904=CARTESIAN_POINT('Ctrl Pts',(-0.084944237279569,-0.221441769913107,
-1.47671280865898));
#68905=CARTESIAN_POINT('Ctrl Pts',(-0.0849284955635096,-0.221447807734861,
-1.47671168839056));
#68906=CARTESIAN_POINT('Ctrl Pts',(-0.0848962052829576,-0.221460188900053,
-1.47670939041271));
#68907=CARTESIAN_POINT('Ctrl Pts',(-0.0848796566516423,-0.22146653206702,
-1.47670821269743));
#68908=CARTESIAN_POINT('Ctrl Pts',(-0.0837731946952754,-0.221890501821456,
-1.47662946843166));
#68909=CARTESIAN_POINT('Ctrl Pts',(-0.0826802311840069,-0.222300072504914,
-1.47655163503368));
#68910=CARTESIAN_POINT('Ctrl Pts',(-0.0803262679976836,-0.223162421462658,
-1.4763838731902));
#68911=CARTESIAN_POINT('Ctrl Pts',(-0.079064370756416,-0.223612613312384,
-1.47629386174449));
#68912=CARTESIAN_POINT('Ctrl Pts',(-0.0756450131076889,-0.224799934340451,
-1.4760497105278));
#68913=CARTESIAN_POINT('Ctrl Pts',(-0.0734806741502606,-0.225516669851043,
-1.47589490520239));
#68914=CARTESIAN_POINT('Ctrl Pts',(-0.061806631537716,-0.229196715682635,
-1.47505823942772));
#68915=CARTESIAN_POINT('Ctrl Pts',(-0.0521289607106422,-0.231589545149481,
-1.47435809973337));
#68916=CARTESIAN_POINT('Ctrl Pts',(-0.0291804723717781,-0.235752196584288,
-1.47268494077267));
#68917=CARTESIAN_POINT('Ctrl Pts',(-0.0158526900075045,-0.237021624268995,
-1.47170261479783));
#68918=CARTESIAN_POINT('Ctrl Pts',(0.00404036154203669,-0.237230495947095,
-1.47025604575925));
#68919=CARTESIAN_POINT('Ctrl Pts',(0.0105713654065964,-0.23702930295838,
-1.46978464202488));
#68920=CARTESIAN_POINT('Ctrl Pts',(0.0207355203658927,-0.23629516781333,
-1.46906363177332));
#68921=CARTESIAN_POINT('Ctrl Pts',(0.0243785750500932,-0.235947148434781,
-1.46880777220532));
#68922=CARTESIAN_POINT('Ctrl Pts',(0.0291183200395713,-0.235383399006347,
-1.46847944830705));
#68923=CARTESIAN_POINT('Ctrl Pts',(0.0302233733893709,-0.23524406244156,
-1.46840322589248));
#68924=CARTESIAN_POINT('Ctrl Pts',(0.0320256527664648,-0.235003902860228,
-1.46827948688433));
#68925=CARTESIAN_POINT('Ctrl Pts',(0.0327234679344847,-0.234907750987677,
-1.46823171814076));
#68926=CARTESIAN_POINT('Ctrl Pts',(0.0340859893669858,-0.234713820042142,
-1.46813873659073));
#68927=CARTESIAN_POINT('Ctrl Pts',(0.0347507231055326,-0.234616323495928,
-1.46809350946589));
#68928=CARTESIAN_POINT('Ctrl Pts',(0.0362387016816675,-0.234391618907756,
-1.46799255717252));
#68929=CARTESIAN_POINT('Ctrl Pts',(0.0370617171350629,-0.234262894391862,
-1.46793691625957));
#68930=CARTESIAN_POINT('Ctrl Pts',(0.0399288806333547,-0.233798964737036,
-1.46774371094434));
#68931=CARTESIAN_POINT('Ctrl Pts',(0.0419693719147703,-0.233441307310008,
-1.46760733407865));
#68932=CARTESIAN_POINT('Ctrl Pts',(0.055943315143799,-0.230802796110215,
-1.46667947043548));
#68933=CARTESIAN_POINT('Ctrl Pts',(0.0676924019440297,-0.22763435623067,
-1.46592938535968));
#68934=CARTESIAN_POINT('Ctrl Pts',(0.0893523920683164,-0.219966602000067,
-1.46451903935053));
#68935=CARTESIAN_POINT('Ctrl Pts',(0.0992971883847658,-0.215659951408117,
-1.46385948749981));
#68936=CARTESIAN_POINT('Ctrl Pts',(0.117010425830783,-0.20650335589636,
-1.46261624934149));
#68937=CARTESIAN_POINT('Ctrl Pts',(0.12485920386034,-0.201854466664892,
-1.46203818975448));
#68938=CARTESIAN_POINT('Ctrl Pts',(0.134232314174322,-0.195546506609168,
-1.46130111270457));
#68939=CARTESIAN_POINT('Ctrl Pts',(0.13602721805316,-0.194302202357451,
-1.46115774134598));
#68940=CARTESIAN_POINT('Ctrl Pts',(0.138867559287086,-0.192274510029199,
-1.46092713351769));
#68941=CARTESIAN_POINT('Ctrl Pts',(0.13992417989916,-0.191506945025557,
-1.46084050363642));
#68942=CARTESIAN_POINT('Ctrl Pts',(0.14191694789207,-0.190034034563014,
-1.46067548263932));
#68943=CARTESIAN_POINT('Ctrl Pts',(0.142854313901792,-0.189330397205168,
-1.46059715962374));
#68944=CARTESIAN_POINT('Ctrl Pts',(0.144977675316932,-0.187711741926462,
-1.46041811350873));
#68945=CARTESIAN_POINT('Ctrl Pts',(0.146160284771637,-0.186792385748309,
-1.46031722127542));
#68946=CARTESIAN_POINT('Ctrl Pts',(0.149778910432317,-0.183923874915833,
-1.46000481192785));
#68947=CARTESIAN_POINT('Ctrl Pts',(0.152185153197636,-0.1819378775954,-1.45979183178573));
#68948=CARTESIAN_POINT('Ctrl Pts',(0.167993145987693,-0.168357672447239,
-1.45835642167721));
#68949=CARTESIAN_POINT('Ctrl Pts',(0.180095960521503,-0.155342268676589,
-1.45707327796906));
#68950=CARTESIAN_POINT('Ctrl Pts',(0.193206272125239,-0.137629934209965,
-1.45546379644826));
#68951=CARTESIAN_POINT('Ctrl Pts',(0.195682311009935,-0.13408615282924,
-1.45514811947415));
#68952=CARTESIAN_POINT('Ctrl Pts',(0.201630114589586,-0.125057542498326,
-1.45436207173725));
#68953=CARTESIAN_POINT('Ctrl Pts',(0.204976417486793,-0.119493814367877,
-1.4538937575076));
#68954=CARTESIAN_POINT('Ctrl Pts',(0.209838731413352,-0.110602726333762,
-1.45317685456136));
#68955=CARTESIAN_POINT('Ctrl Pts',(0.211513188662552,-0.107365873966534,
-1.45292208995909));
#68956=CARTESIAN_POINT('Ctrl Pts',(0.213600586123493,-0.103092225859727,
-1.45259494324688));
#68957=CARTESIAN_POINT('Ctrl Pts',(0.214081649571237,-0.102089494389382,
-1.45251883537212));
#68958=CARTESIAN_POINT('Ctrl Pts',(0.214855710306689,-0.100446503344674,
-1.45239523513154));
#68959=CARTESIAN_POINT('Ctrl Pts',(0.215152934552959,-0.0998082715603084,
-1.4523474916534));
#68960=CARTESIAN_POINT('Ctrl Pts',(0.215728331291025,-0.0985582030945205,
-1.45225451931483));
#68961=CARTESIAN_POINT('Ctrl Pts',(0.21600675135178,-0.0979464941012095,
-1.45220927640747));
#68962=CARTESIAN_POINT('Ctrl Pts',(0.21662480099455,-0.0965731414169772,
-1.45210824755391));
#68963=CARTESIAN_POINT('Ctrl Pts',(0.216963024831639,-0.0958108655488671,
-1.45205254628071));
#68964=CARTESIAN_POINT('Ctrl Pts',(0.218129504727468,-0.0931440442815503,
-1.45185892534696));
#68965=CARTESIAN_POINT('Ctrl Pts',(0.21893678877651,-0.0912303516386376,
-1.45172219992765));
#68966=CARTESIAN_POINT('Ctrl Pts',(0.22426024029244,-0.0781331374932253,
-1.45079982215831));
#68967=CARTESIAN_POINT('Ctrl Pts',(0.227943353732895,-0.0666284086146129,
-1.45005492311008));
#68968=CARTESIAN_POINT('Ctrl Pts',(0.233210055274903,-0.0444901641214075,
-1.44865799371922));
#68969=CARTESIAN_POINT('Ctrl Pts',(0.234978406182421,-0.0339329397472972,
-1.44800655919398));
#68970=CARTESIAN_POINT('Ctrl Pts',(0.236942349735022,-0.0140320890595671,
-1.44676072748228));
#68971=CARTESIAN_POINT('Ctrl Pts',(0.237310355582883,-0.00472661951041226,
-1.44617107144383));
#68972=CARTESIAN_POINT('Ctrl Pts',(0.237088488501456,0.0067714356822805,
-1.44542090502571));
#68973=CARTESIAN_POINT('Ctrl Pts',(0.237015624852722,0.00896642430360502,
-1.44527674927325));
#68974=CARTESIAN_POINT('Ctrl Pts',(0.236850716485898,0.0124672065347807,
-1.44504517755603));
#68975=CARTESIAN_POINT('Ctrl Pts',(0.236778323660225,0.0137738326831459,
-1.44495837729446));
#68976=CARTESIAN_POINT('Ctrl Pts',(0.236620633908695,0.0162489627919629,
-1.44479322268115));
#68977=CARTESIAN_POINT('Ctrl Pts',(0.23653748416878,0.0174175681802019,
-1.44471493803572));
#68978=CARTESIAN_POINT('Ctrl Pts',(0.236328663921222,0.0200741912275866,
-1.44453624626719));
#68979=CARTESIAN_POINT('Ctrl Pts',(0.23619759210099,0.0215617219232392,
-1.44443567249847));
#68980=CARTESIAN_POINT('Ctrl Pts',(0.235751684794361,0.0261286277531596,
-1.44412525207691));
#68981=CARTESIAN_POINT('Ctrl Pts',(0.235390616438148,0.0292030509584075,
-1.44391396923633));
#68982=CARTESIAN_POINT('Ctrl Pts',(0.232511191979616,0.0501695646280451,
-1.44245661140471));
#68983=CARTESIAN_POINT('Ctrl Pts',(0.228015916144205,0.0677269613842048,
-1.44114708661915));
#68984=CARTESIAN_POINT('Ctrl Pts',(0.220164708528558,0.0882897355770886,
-1.43953950784137));
#68985=CARTESIAN_POINT('Ctrl Pts',(0.218664109567756,0.0919433747896704,
-1.43925116649498));
#68986=CARTESIAN_POINT('Ctrl Pts',(0.214440487029725,0.101537919074301,
-1.43848890248179));
#68987=CARTESIAN_POINT('Ctrl Pts',(0.211561832824276,0.107407047668004,
-1.43801727800746));
#68988=CARTESIAN_POINT('Ctrl Pts',(0.20669820461392,0.116366783659128,-1.43729597447291));
#68989=CARTESIAN_POINT('Ctrl Pts',(0.204877773285303,0.119542786422501,
-1.43704003683545));
#68990=CARTESIAN_POINT('Ctrl Pts',(0.202408298040216,0.123628889160507,
-1.43671162902922));
#68991=CARTESIAN_POINT('Ctrl Pts',(0.201825436287929,0.124578147125233,
-1.43663539846692));
#68992=CARTESIAN_POINT('Ctrl Pts',(0.200863085177926,0.12612096512354,-1.43651164958742));
#68993=CARTESIAN_POINT('Ctrl Pts',(0.200487609128549,0.126716989586637,
-1.43646387904636));
#68994=CARTESIAN_POINT('Ctrl Pts',(0.19974885607119,0.127878170400072,-1.43637089683534));
#68995=CARTESIAN_POINT('Ctrl Pts',(0.199385825417262,0.12844346852402,-1.43632567082774));
#68996=CARTESIAN_POINT('Ctrl Pts',(0.198567333545759,0.129706161972041,
-1.43622472396048));
#68997=CARTESIAN_POINT('Ctrl Pts',(0.198110585990482,0.130402723037392,
-1.43616908732682));
#68998=CARTESIAN_POINT('Ctrl Pts',(0.196505415726022,0.132822782033982,
-1.43597591144874));
#68999=CARTESIAN_POINT('Ctrl Pts',(0.195338056591969,0.134533691691649,
-1.43583955926682));
#69000=CARTESIAN_POINT('Ctrl Pts',(0.187165339638882,0.146181123179203,
-1.43491117934512));
#69001=CARTESIAN_POINT('Ctrl Pts',(0.179426473628093,0.155582781967428,
-1.43416061314105));
#69002=CARTESIAN_POINT('Ctrl Pts',(0.163462806086276,0.172192313192935,
-1.432746592364));
#69003=CARTESIAN_POINT('Ctrl Pts',(0.155395452420754,0.179506337252501,
-1.43208389056705));
#69004=CARTESIAN_POINT('Ctrl Pts',(0.139738541951283,0.191852164169122,
-1.43084043988288));
#69005=CARTESIAN_POINT('Ctrl Pts',(0.132307081654853,0.197050552727842,
-1.43026561501085));
#69006=CARTESIAN_POINT('Ctrl Pts',(0.122741654976787,0.202956205718214,
-1.42953219025916));
#69007=CARTESIAN_POINT('Ctrl Pts',(0.120870605688514,0.20407604334043,-1.42938904205155));
#69008=CARTESIAN_POINT('Ctrl Pts',(0.117855328784402,0.205824696630286,
-1.42915870843379));
#69009=CARTESIAN_POINT('Ctrl Pts',(0.116720858855932,0.206470155853359,
-1.42907212702932));
#69010=CARTESIAN_POINT('Ctrl Pts',(0.114557522802467,0.207677463186617,
-1.42890714372396));
#69011=CARTESIAN_POINT('Ctrl Pts',(0.113529702725674,0.20824111328019,-1.42882880946459));
#69012=CARTESIAN_POINT('Ctrl Pts',(0.111177888956655,0.209508246638588,
-1.42864966093714));
#69013=CARTESIAN_POINT('Ctrl Pts',(0.109851329531481,0.210206835338007,
-1.42854867681695));
#69014=CARTESIAN_POINT('Ctrl Pts',(0.105737897788014,0.212323467545589,
-1.42823569213766));
#69015=CARTESIAN_POINT('Ctrl Pts',(0.102929635006296,0.21369896234916,-1.42802222073969));
#69016=CARTESIAN_POINT('Ctrl Pts',(0.0841334307977906,0.222448945924058,
-1.42659410511235));
#69017=CARTESIAN_POINT('Ctrl Pts',(0.0673968609072315,0.228077634589926,
-1.42531962852989));
#69018=CARTESIAN_POINT('Ctrl Pts',(0.0457994821767047,0.232754416960778,
-1.42370567017068));
#69019=CARTESIAN_POINT('Ctrl Pts',(0.0413772883799832,0.233581103960074,
-1.42337713507821));
#69020=CARTESIAN_POINT('Ctrl Pts',(0.0305734752473814,0.235284312741661,
-1.42258208702174));
#69021=CARTESIAN_POINT('Ctrl Pts',(0.024174084774717,0.236027689082033,
-1.4221174941943));
#69022=CARTESIAN_POINT('Ctrl Pts',(0.01413710797081,0.236781045973489,-1.42140554479404));
#69023=CARTESIAN_POINT('Ctrl Pts',(0.0105162383851371,0.236969478690863,
-1.42115210482567));
#69024=CARTESIAN_POINT('Ctrl Pts',(0.00578259343837471,0.237107095192875,
-1.42082638304683));
#69025=CARTESIAN_POINT('Ctrl Pts',(0.00467270794150724,0.237131564538216,
-1.4207504143985));
#69026=CARTESIAN_POINT('Ctrl Pts',(0.00285915130602412,0.237158809495083,
-1.42062698282719));
#69027=CARTESIAN_POINT('Ctrl Pts',(0.00215558294161852,0.237166247941148,
-1.42057927005124));
#69028=CARTESIAN_POINT('Ctrl Pts',(0.000779610703593176,0.237174671771469,
-1.42048630870671));
#69029=CARTESIAN_POINT('Ctrl Pts',(0.000107220803301362,0.237175928888627,
-1.420441046422));
#69030=CARTESIAN_POINT('Ctrl Pts',(-0.00140021851308484,0.237172336748445,
-1.42033992379895));
#69031=CARTESIAN_POINT('Ctrl Pts',(-0.00223526377391046,0.237165936801454,
-1.42028414864492));
#69032=CARTESIAN_POINT('Ctrl Pts',(-0.00515354594639942,0.237128155942764,
-1.42009001796556));
#69033=CARTESIAN_POINT('Ctrl Pts',(-0.00723646033378336,0.237073734831898,
-1.41995286493257));
#69034=CARTESIAN_POINT('Ctrl Pts',(-0.0202610147860963,0.236561611929272,
-1.41910253015864));
#69035=CARTESIAN_POINT('Ctrl Pts',(-0.0311607401173676,0.235373990943297,
-1.41842278355567));
#69036=CARTESIAN_POINT('Ctrl Pts',(-0.0419392748056671,0.233437524519463,
-1.41774927189049));
#69037=CARTESIAN_POINT('Origin',(0.,0.,-2.1456589891905));
#69038=CARTESIAN_POINT('',(-0.0419392737720405,0.233437524705164,-1.29816138490414));
#69039=CARTESIAN_POINT('',(-0.0419392741368905,0.233437524639615,-1.31805175208418));
#69040=CARTESIAN_POINT('',(-0.0419392741328076,0.233437524640348,-2.1456589891905));
#69041=CARTESIAN_POINT('Ctrl Pts',(-0.0419392737720407,0.233437524705164,
-1.29816138490414));
#69042=CARTESIAN_POINT('Ctrl Pts',(-0.0318728565423017,0.235246052398536,
-1.29878870397928));
#69043=CARTESIAN_POINT('Ctrl Pts',(-0.0216995162353172,0.236401635171646,
-1.29941285583831));
#69044=CARTESIAN_POINT('Ctrl Pts',(-0.0024103744417276,0.237336633302986,
-1.30061709041487));
#69045=CARTESIAN_POINT('Ctrl Pts',(0.00667910759640316,0.237254816497144,
-1.30119317327307));
#69046=CARTESIAN_POINT('Ctrl Pts',(0.0179183508302511,0.236507242965848,
-1.30192804875745));
#69047=CARTESIAN_POINT('Ctrl Pts',(0.0200937231710433,0.236332361386772,
-1.30207131475618));
#69048=CARTESIAN_POINT('Ctrl Pts',(0.0235664635680065,0.236004889438547,
-1.3023018119501));
#69049=CARTESIAN_POINT('Ctrl Pts',(0.024865555383796,0.235871554206155,
-1.30238843792096));
#69050=CARTESIAN_POINT('Ctrl Pts',(0.0273288910901284,0.23559814791868,
-1.30255348974753));
#69051=CARTESIAN_POINT('Ctrl Pts',(0.0284933303413513,0.235460157206682,
-1.30263184777442));
#69052=CARTESIAN_POINT('Ctrl Pts',(0.0311442927438584,0.235126055116324,
-1.30281102806703));
#69053=CARTESIAN_POINT('Ctrl Pts',(0.0326300629188021,0.234924472073839,
-1.30291202008764));
#69054=CARTESIAN_POINT('Ctrl Pts',(0.0372071763632039,0.234259210752228,
-1.30322494625904));
#69055=CARTESIAN_POINT('Ctrl Pts',(0.0402912332081526,0.23374851164379,
-1.30343834998415));
#69056=CARTESIAN_POINT('Ctrl Pts',(0.0606950674918734,0.229953989604255,
-1.30486787521392));
#69057=CARTESIAN_POINT('Ctrl Pts',(0.0776095034816172,0.224809406618693,
-1.30614399388456));
#69058=CARTESIAN_POINT('Ctrl Pts',(0.102686612660891,0.214012066510612,
-1.30813810224086));
#69059=CARTESIAN_POINT('Ctrl Pts',(0.111336286194037,0.209642450517734,
-1.30884529806275));
#69060=CARTESIAN_POINT('Ctrl Pts',(0.122395508431192,0.203177519984765,
-1.30975809664146));
#69061=CARTESIAN_POINT('Ctrl Pts',(0.125064611282575,0.201545553441463,
-1.30997905753906));
#69062=CARTESIAN_POINT('Ctrl Pts',(0.12953093611788,0.198691806902404,-1.31034898631507));
#69063=CARTESIAN_POINT('Ctrl Pts',(0.131345028471709,0.19749729587155,-1.31049929311839));
#69064=CARTESIAN_POINT('Ctrl Pts',(0.133899218734225,0.19576469518554,-1.31071071533704));
#69065=CARTESIAN_POINT('Ctrl Pts',(0.134652944125372,0.195247026525157,
-1.31077307874387));
#69066=CARTESIAN_POINT('Ctrl Pts',(0.13594950503168,0.194345451959674,-1.31088028541602));
#69067=CARTESIAN_POINT('Ctrl Pts',(0.136493749002289,0.193963602629301,
-1.31092526404964));
#69068=CARTESIAN_POINT('Ctrl Pts',(0.137636544001775,0.193154609187066,
-1.31101965370857));
#69069=CARTESIAN_POINT('Ctrl Pts',(0.13823472076293,0.192726965699511,-1.31106903018319));
#69070=CARTESIAN_POINT('Ctrl Pts',(0.139846947296754,0.191562998444501,
-1.31120205827568));
#69071=CARTESIAN_POINT('Ctrl Pts',(0.140857183313191,0.190821395869145,
-1.31128535771404));
#69072=CARTESIAN_POINT('Ctrl Pts',(0.145573130683965,0.187301613002203,
-1.31167419120482));
#69073=CARTESIAN_POINT('Ctrl Pts',(0.149203101246535,0.18442307880345,-1.31197342557776));
#69074=CARTESIAN_POINT('Ctrl Pts',(0.155163216788652,0.179405504003362,
-1.31246908424052));
#69075=CARTESIAN_POINT('Ctrl Pts',(0.157538926960821,0.177323000920065,
-1.31266788326903));
#69076=CARTESIAN_POINT('Ctrl Pts',(0.170976909111297,0.165060208632435,
-1.31380424178202));
#69077=CARTESIAN_POINT('Ctrl Pts',(0.181093084635821,0.153893808827574,
-1.31470935671998));
#69078=CARTESIAN_POINT('Ctrl Pts',(0.196364816361512,0.133428316553375,
-1.31629290456829));
#69079=CARTESIAN_POINT('Ctrl Pts',(0.202078559425883,0.124605260854633,
-1.31695511577607));
#69080=CARTESIAN_POINT('Ctrl Pts',(0.20829081268262,0.113455043740425,-1.31778710713011));
#69081=CARTESIAN_POINT('Ctrl Pts',(0.209364631289577,0.111461025390306,
-1.31793568098041));
#69082=CARTESIAN_POINT('Ctrl Pts',(0.211020599189383,0.10827760489307,-1.31817270052789));
#69083=CARTESIAN_POINT('Ctrl Pts',(0.211621643640911,0.107098145762735,
-1.31826047827057));
#69084=CARTESIAN_POINT('Ctrl Pts',(0.212735047343839,0.104867287953199,
-1.31842646319314));
#69085=CARTESIAN_POINT('Ctrl Pts',(0.213249566190888,0.103817006727997,
-1.31850459184072));
#69086=CARTESIAN_POINT('Ctrl Pts',(0.214393111044191,0.10143833003414,-1.31868152279029));
#69087=CARTESIAN_POINT('Ctrl Pts',(0.215017593996348,0.100107816707867,
-1.31878047895287));
#69088=CARTESIAN_POINT('Ctrl Pts',(0.216826650429969,0.0961584407935901,
-1.31907422995178));
#69089=CARTESIAN_POINT('Ctrl Pts',(0.217975992875584,0.0935238329877993,
-1.31927021683345));
#69090=CARTESIAN_POINT('Ctrl Pts',(0.226682940753395,0.0725321709673598,
-1.32083262915924));
#69091=CARTESIAN_POINT('Ctrl Pts',(0.231955037949759,0.0533161961942209,
-1.32227791060544));
#69092=CARTESIAN_POINT('Ctrl Pts',(0.235948576275878,0.0254730994360653,
-1.32433082673592));
#69093=CARTESIAN_POINT('Ctrl Pts',(0.236694376928316,0.017216236257691,
-1.32493317461051));
#69094=CARTESIAN_POINT('Ctrl Pts',(0.237166923880965,0.00468417668534722,
-1.32582434843599));
#69095=CARTESIAN_POINT('Ctrl Pts',(0.237212803024866,0.000427656028375762,
-1.32612298124362));
#69096=CARTESIAN_POINT('Ctrl Pts',(0.237125169022792,-0.00500111645075131,
-1.3264968511908));
#69097=CARTESIAN_POINT('Ctrl Pts',(0.23709753001091,-0.00617400646635365,
-1.32657720792946));
#69098=CARTESIAN_POINT('Ctrl Pts',(0.237038958680632,-0.00806397607175334,
-1.3267059679238));
#69099=CARTESIAN_POINT('Ctrl Pts',(0.237013473121604,-0.00878118649158647,
-1.32675466170852));
#69100=CARTESIAN_POINT('Ctrl Pts',(0.236958117025209,-0.010162336191754,
-1.32684809399495));
#69101=CARTESIAN_POINT('Ctrl Pts',(0.236928710869638,-0.0108262772136131,
-1.32689285617956));
#69102=CARTESIAN_POINT('Ctrl Pts',(0.236857577223833,-0.0122928722308543,
-1.32699141164523));
#69103=CARTESIAN_POINT('Ctrl Pts',(0.236814559276926,-0.0130954632416445,
-1.32704513390151));
#69104=CARTESIAN_POINT('Ctrl Pts',(0.236647806088015,-0.0159363179718838,
-1.32723458790831));
#69105=CARTESIAN_POINT('Ctrl Pts',(0.236501824776447,-0.0179732558570746,
-1.32736915024778));
#69106=CARTESIAN_POINT('Ctrl Pts',(0.235081904851881,-0.0347448833719733,
-1.32846843083687));
#69107=CARTESIAN_POINT('Ctrl Pts',(0.232458404305983,-0.0493348075127487,
-1.3293707771645));
#69108=CARTESIAN_POINT('Ctrl Pts',(0.225417108335508,-0.074636901487737,
-1.33098035651496));
#69109=CARTESIAN_POINT('Ctrl Pts',(0.221544629299971,-0.0854487639734451,
-1.33168362053006));
#69110=CARTESIAN_POINT('Ctrl Pts',(0.215184927706626,-0.0998274523309159,
-1.33267730220626));
#69111=CARTESIAN_POINT('Ctrl Pts',(0.213360110607767,-0.10367031071428,
-1.33294880295714));
#69112=CARTESIAN_POINT('Ctrl Pts',(0.209986809922639,-0.110307336863774,
-1.3334298702877));
#69113=CARTESIAN_POINT('Ctrl Pts',(0.20848335008671,-0.113123207446429,
-1.33363793069504));
#69114=CARTESIAN_POINT('Ctrl Pts',(0.206184767297774,-0.117226736981188,
-1.3339474817845));
#69115=CARTESIAN_POINT('Ctrl Pts',(0.205433374906296,-0.118538577794571,
-1.33404741701478));
#69116=CARTESIAN_POINT('Ctrl Pts',(0.204076267862656,-0.120856261348862,
-1.33422576680816));
#69117=CARTESIAN_POINT('Ctrl Pts',(0.203475523510242,-0.121864967316903,
-1.33430399952499));
#69118=CARTESIAN_POINT('Ctrl Pts',(0.202194301645057,-0.123980372511511,
-1.33446938013217));
#69119=CARTESIAN_POINT('Ctrl Pts',(0.201512172553515,-0.125086020729689,
-1.33455658668214));
#69120=CARTESIAN_POINT('Ctrl Pts',(0.19967651071696,-0.128007418389305,
-1.33478909001379));
#69121=CARTESIAN_POINT('Ctrl Pts',(0.198507322310904,-0.129813137053506,
-1.33493496195895));
#69122=CARTESIAN_POINT('Ctrl Pts',(0.193092686939065,-0.137931378491709,
-1.33560085850526));
#69123=CARTESIAN_POINT('Ctrl Pts',(0.188570024744863,-0.144052679399986,
-1.33613119987034));
#69124=CARTESIAN_POINT('Ctrl Pts',(0.173903888267402,-0.162026343238043,
-1.33777777351593));
#69125=CARTESIAN_POINT('Ctrl Pts',(0.162879660220001,-0.173104655240237,
-1.33892334399001));
#69126=CARTESIAN_POINT('Ctrl Pts',(0.145585768374689,-0.187358753403299,
-1.34055434621625));
#69127=CARTESIAN_POINT('Ctrl Pts',(0.140136450290107,-0.191468812744281,
-1.34104741838494));
#69128=CARTESIAN_POINT('Ctrl Pts',(0.131416419089888,-0.197473744069596,
-1.34179712653934));
#69129=CARTESIAN_POINT('Ctrl Pts',(0.128265037058233,-0.199535057094684,
-1.34206056531066));
#69130=CARTESIAN_POINT('Ctrl Pts',(0.124109648538934,-0.202113932843209,
-1.34239703749904));
#69131=CARTESIAN_POINT('Ctrl Pts',(0.123149361223076,-0.2027004727848,-1.34247405592901));
#69132=CARTESIAN_POINT('Ctrl Pts',(0.121578893509951,-0.203644428404196,
-1.34259877010456));
#69133=CARTESIAN_POINT('Ctrl Pts',(0.120971238818345,-0.204005980253957,
-1.34264672518083));
#69134=CARTESIAN_POINT('Ctrl Pts',(0.119784229925712,-0.204705076740272,
-1.34273980511593));
#69135=CARTESIAN_POINT('Ctrl Pts',(0.119205049184147,-0.205042889286391,
-1.34278494610547));
#69136=CARTESIAN_POINT('Ctrl Pts',(0.117908058854139,-0.205792018040861,
-1.34288543551574));
#69137=CARTESIAN_POINT('Ctrl Pts',(0.117189506591715,-0.206202048069211,
-1.34294070233705));
#69138=CARTESIAN_POINT('Ctrl Pts',(0.114694105301188,-0.207608750484607,
-1.34313128551846));
#69139=CARTESIAN_POINT('Ctrl Pts',(0.112906510590903,-0.208586316949343,
-1.34326545643358));
#69140=CARTESIAN_POINT('Ctrl Pts',(0.0988281324601051,-0.216051207410918,
-1.34430562031925));
#69141=CARTESIAN_POINT('Ctrl Pts',(0.0859995524639044,-0.221470781655309,
-1.34515687352145));
#69142=CARTESIAN_POINT('Ctrl Pts',(0.0562006729503547,-0.231076797054721,
-1.34707588083529));
#69143=CARTESIAN_POINT('Ctrl Pts',(0.0390974139453236,-0.234576845660657,
-1.3481411629216));
#69144=CARTESIAN_POINT('Ctrl Pts',(0.0191139479844233,-0.236418551702822,
-1.34944404144082));
#69145=CARTESIAN_POINT('Ctrl Pts',(0.0164578992359098,-0.236618281658662,
-1.34961825459668));
#69146=CARTESIAN_POINT('Ctrl Pts',(0.0123934301455407,-0.236855158761854,
-1.34988670167322));
#69147=CARTESIAN_POINT('Ctrl Pts',(0.0109870498319288,-0.236924561695109,
-1.34997992727444));
#69148=CARTESIAN_POINT('Ctrl Pts',(0.00842641519950863,-0.237028077354934,
-1.35015031813964));
#69149=CARTESIAN_POINT('Ctrl Pts',(0.00727236299628516,-0.237066291536844,
-1.35022735253578));
#69150=CARTESIAN_POINT('Ctrl Pts',(0.00475220155882484,-0.237131322504469,
-1.35039612377189));
#69151=CARTESIAN_POINT('Ctrl Pts',(0.00338605444781345,-0.237154763881754,
-1.35048796355386));
#69152=CARTESIAN_POINT('Ctrl Pts',(-0.000376626373560403,-0.23718680840193,
-1.35074191567724));
#69153=CARTESIAN_POINT('Ctrl Pts',(-0.00277314986803306,-0.237170893728291,
-1.35090478611391));
#69154=CARTESIAN_POINT('Ctrl Pts',(-0.0202806608630571,-0.23678924777322,
-1.35210321463882));
#69155=CARTESIAN_POINT('Ctrl Pts',(-0.0353234499490055,-0.235016066115311,
-1.35318313313352));
#69156=CARTESIAN_POINT('Ctrl Pts',(-0.0616875174485937,-0.229319311422092,
-1.35514652493496));
#69157=CARTESIAN_POINT('Ctrl Pts',(-0.0730781341977933,-0.225947546942119,
-1.35601868456264));
#69158=CARTESIAN_POINT('Ctrl Pts',(-0.0897529703027928,-0.219617987423714,
-1.35729902081691));
#69159=CARTESIAN_POINT('Ctrl Pts',(-0.0952555907767075,-0.217287924551768,
-1.35772192455968));
#69160=CARTESIAN_POINT('Ctrl Pts',(-0.101843096852828,-0.214200041048182,
-1.35822397525818));
#69161=CARTESIAN_POINT('Ctrl Pts',(-0.103016824081451,-0.213638030582018,
-1.3583132582707));
#69162=CARTESIAN_POINT('Ctrl Pts',(-0.104855940123149,-0.2127387335393,
-1.35845282009326));
#69163=CARTESIAN_POINT('Ctrl Pts',(-0.105524443558607,-0.212407930119331,
-1.35850347921444));
#69164=CARTESIAN_POINT('Ctrl Pts',(-0.106783079708057,-0.211777695694204,
-1.3585987097302));
#69165=CARTESIAN_POINT('Ctrl Pts',(-0.107373516308844,-0.211478950518598,
-1.35864331898204));
#69166=CARTESIAN_POINT('Ctrl Pts',(-0.108743973514942,-0.210778316581784,
-1.35874672376161));
#69167=CARTESIAN_POINT('Ctrl Pts',(-0.109523023891553,-0.21037456551568,
-1.35880540252259));
#69168=CARTESIAN_POINT('Ctrl Pts',(-0.112081475832221,-0.209030556698077,
-1.35899782775761));
#69169=CARTESIAN_POINT('Ctrl Pts',(-0.113851208940743,-0.208071943675324,
-1.35913048436589));
#69170=CARTESIAN_POINT('Ctrl Pts',(-0.128906197390237,-0.199667488174845,
-1.36025699421414));
#69171=CARTESIAN_POINT('Ctrl Pts',(-0.141459878144863,-0.190979449466593,
-1.36118442651156));
#69172=CARTESIAN_POINT('Ctrl Pts',(-0.161639891119704,-0.173924401410632,
-1.36280382106334));
#69173=CARTESIAN_POINT('Ctrl Pts',(-0.16966275991616,-0.166107418033556,
-1.36349063718634));
#69174=CARTESIAN_POINT('Ctrl Pts',(-0.179892323263126,-0.154623128759083,
-1.36446318701204));
#69175=CARTESIAN_POINT('Ctrl Pts',(-0.182597445506285,-0.15141905330792,
-1.36473093215617));
#69176=CARTESIAN_POINT('Ctrl Pts',(-0.187187918017403,-0.145679886293315,
-1.3652059453144));
#69177=CARTESIAN_POINT('Ctrl Pts',(-0.189110226393582,-0.143175649690379,
-1.36541176078678));
#69178=CARTESIAN_POINT('Ctrl Pts',(-0.191874430459063,-0.139421839070389,
-1.36571860120614));
#69179=CARTESIAN_POINT('Ctrl Pts',(-0.192755373022699,-0.138201346842064,
-1.3658181105055));
#69180=CARTESIAN_POINT('Ctrl Pts',(-0.194302200536161,-0.136014749329729,
-1.36599598390912));
#69181=CARTESIAN_POINT('Ctrl Pts',(-0.194972651829061,-0.135051923800692,
-1.36607416972506));
#69182=CARTESIAN_POINT('Ctrl Pts',(-0.196372379931966,-0.133009646320417,
-1.36623974610283));
#69183=CARTESIAN_POINT('Ctrl Pts',(-0.197099959917208,-0.131929084350244,
-1.36632719750948));
#69184=CARTESIAN_POINT('Ctrl Pts',(-0.199014322998506,-0.129034793056295,
-1.36656106012519));
#69185=CARTESIAN_POINT('Ctrl Pts',(-0.20018518325261,-0.127210732406274,
-1.36670805848678));
#69186=CARTESIAN_POINT('Ctrl Pts',(-0.20546983525563,-0.118724208131854,
-1.36739039644434));
#69187=CARTESIAN_POINT('Ctrl Pts',(-0.209276680072112,-0.111877333672706,
-1.3679367073092));
#69188=CARTESIAN_POINT('Ctrl Pts',(-0.220242475636262,-0.0896291922228234,
-1.369699207038));
#69189=CARTESIAN_POINT('Ctrl Pts',(-0.226090417077609,-0.0736420839027499,
-1.3709513432726));
#69190=CARTESIAN_POINT('Ctrl Pts',(-0.231556805039093,-0.0516331267031599,
-1.37259524400254));
#69191=CARTESIAN_POINT('Ctrl Pts',(-0.232731946391666,-0.0460476223073438,
-1.37300537014251));
#69192=CARTESIAN_POINT('Ctrl Pts',(-0.234088995878537,-0.0382022299993802,
-1.37356727587456));
#69193=CARTESIAN_POINT('Ctrl Pts',(-0.234441737759472,-0.0359741684758743,
-1.37372527399775));
#69194=CARTESIAN_POINT('Ctrl Pts',(-0.235003462666067,-0.032065844513887,
-1.37399928675627));
#69195=CARTESIAN_POINT('Ctrl Pts',(-0.235226336770555,-0.0303877730415673,
-1.37411592904399));
#69196=CARTESIAN_POINT('Ctrl Pts',(-0.23553137299862,-0.0278861513270842,
-1.37428817807476));
#69197=CARTESIAN_POINT('Ctrl Pts',(-0.235627216419629,-0.0270643684048602,
-1.37434449940631));
#69198=CARTESIAN_POINT('Ctrl Pts',(-0.235784285608267,-0.0256534990311193,
-1.37444072472845));
#69199=CARTESIAN_POINT('Ctrl Pts',(-0.235847607184581,-0.0250646676608368,
-1.37448074375953));
#69200=CARTESIAN_POINT('Ctrl Pts',(-0.235987429711496,-0.0237169836300684,
-1.37457201246847));
#69201=CARTESIAN_POINT('Ctrl Pts',(-0.236062476539668,-0.0229579943710578,
-1.37462318037575));
#69202=CARTESIAN_POINT('Ctrl Pts',(-0.236259470637116,-0.0208625069446904,
-1.37476384003465));
#69203=CARTESIAN_POINT('Ctrl Pts',(-0.236373739881703,-0.019525290370001,
-1.37485291734278));
#69204=CARTESIAN_POINT('Ctrl Pts',(-0.236938100357669,-0.0121872429385602,
-1.37533834460322));
#69205=CARTESIAN_POINT('Ctrl Pts',(-0.23717107801787,-0.00617137255013728,
-1.37572390747684));
#69206=CARTESIAN_POINT('Ctrl Pts',(-0.237185663879248,0.0164961723705386,
-1.37715177446449));
#69207=CARTESIAN_POINT('Ctrl Pts',(-0.235443376631179,0.0331005582226649,
-1.37815009812945));
#69208=CARTESIAN_POINT('Ctrl Pts',(-0.229819634506442,0.0595162181980795,
-1.37982509561166));
#69209=CARTESIAN_POINT('Ctrl Pts',(-0.227002126689017,0.0694927282228469,
-1.38047813891077));
#69210=CARTESIAN_POINT('Ctrl Pts',(-0.222773324296751,0.0814206274086489,
-1.38130250023246));
#69211=CARTESIAN_POINT('Ctrl Pts',(-0.221973151845707,0.0835774601011955,
-1.38145332930051));
#69212=CARTESIAN_POINT('Ctrl Pts',(-0.220655730281342,0.0869760749368039,
-1.38169397737837));
#69213=CARTESIAN_POINT('Ctrl Pts',(-0.22015905901245,0.0882257191863792,
-1.3817831077328));
#69214=CARTESIAN_POINT('Ctrl Pts',(-0.219211491722091,0.0905520007675374,
-1.38195027226123));
#69215=CARTESIAN_POINT('Ctrl Pts',(-0.218763220562161,0.0916296687289643,
-1.38202821575225));
#69216=CARTESIAN_POINT('Ctrl Pts',(-0.217744262228406,0.0940291966348703,
-1.38220291374211));
#69217=CARTESIAN_POINT('Ctrl Pts',(-0.217169459997576,0.0953492477078107,
-1.38229980599598));
#69218=CARTESIAN_POINT('Ctrl Pts',(-0.215433515662661,0.0992387582484171,
-1.38258767710358));
#69219=CARTESIAN_POINT('Ctrl Pts',(-0.214238567629329,0.101792758849093,
-1.38277980488933));
#69220=CARTESIAN_POINT('Ctrl Pts',(-0.208569341916651,0.113367538751907,
-1.3836651786895));
#69221=CARTESIAN_POINT('Ctrl Pts',(-0.203569508197109,0.12211787820237,
-1.38437636179456));
#69222=CARTESIAN_POINT('Ctrl Pts',(-0.189541261975669,0.143401510018687,
-1.38621133985064));
#69223=CARTESIAN_POINT('Ctrl Pts',(-0.17981757480942,0.15542036194543,-1.38735081068616));
#69224=CARTESIAN_POINT('Ctrl Pts',(-0.164345785805216,0.171132625022037,
-1.38893927386564));
#69225=CARTESIAN_POINT('Ctrl Pts',(-0.159498851202622,0.175658893310532,
-1.38941031312268));
#69226=CARTESIAN_POINT('Ctrl Pts',(-0.153423819071305,0.18087290157415,
-1.38996355463857));
#69227=CARTESIAN_POINT('Ctrl Pts',(-0.152371633739448,0.181760172316185,
-1.39005809489226));
#69228=CARTESIAN_POINT('Ctrl Pts',(-0.150718488115591,0.18312976685428,
-1.39020457041831));
#69229=CARTESIAN_POINT('Ctrl Pts',(-0.150122820799587,0.183618389290984,
-1.39025693781813));
#69230=CARTESIAN_POINT('Ctrl Pts',(-0.14901467226277,0.184518399934664,
-1.39035358370004));
#69231=CARTESIAN_POINT('Ctrl Pts',(-0.148502862725296,0.184930560598091,
-1.39039791528265));
#69232=CARTESIAN_POINT('Ctrl Pts',(-0.14732314457597,0.185872532782397,
-1.39049940824487));
#69233=CARTESIAN_POINT('Ctrl Pts',(-0.14665408651702,0.186400875360567,
-1.39055646570941));
#69234=CARTESIAN_POINT('Ctrl Pts',(-0.144544920422733,0.18804805826034,
-1.39073481705062));
#69235=CARTESIAN_POINT('Ctrl Pts',(-0.143094707450883,0.189153935820108,
-1.39085524255602));
#69236=CARTESIAN_POINT('Ctrl Pts',(-0.139638856142722,0.19172674268913,
-1.39113743757307));
#69237=CARTESIAN_POINT('Ctrl Pts',(-0.137622604812363,0.193179123387222,
-1.39129835748516));
#69238=CARTESIAN_POINT('Ctrl Pts',(-0.130147561610856,0.198387226734763,
-1.3918829584528));
#69239=CARTESIAN_POINT('Ctrl Pts',(-0.124554568153433,0.201945665591074,
-1.39229741389112));
#69240=CARTESIAN_POINT('Ctrl Pts',(-0.116663997406113,0.206513184762994,
-1.39286162901114));
#69241=CARTESIAN_POINT('Ctrl Pts',(-0.114488924788223,0.207726912520161,
-1.39301509919563));
#69242=CARTESIAN_POINT('Ctrl Pts',(-0.0949889995657393,0.218208873400792,
-1.39437612568214));
#69243=CARTESIAN_POINT('Ctrl Pts',(-0.0765961291658136,0.225324152174435,
-1.39556460958456));
#69244=CARTESIAN_POINT('Ctrl Pts',(-0.0547249015365923,0.230793346803669,
-1.39702461114125));
#69245=CARTESIAN_POINT('Ctrl Pts',(-0.0519001250913411,0.231444938589804,
-1.39721385423976));
#69246=CARTESIAN_POINT('Ctrl Pts',(-0.0476212369053222,0.232349679773836,
-1.39750187036786));
#69247=CARTESIAN_POINT('Ctrl Pts',(-0.0461754744523153,0.232641314664901,
-1.39759941697803));
#69248=CARTESIAN_POINT('Ctrl Pts',(-0.0437988604473316,0.233097691697676,
-1.39776018666513));
#69249=CARTESIAN_POINT('Ctrl Pts',(-0.0428695642994561,0.233270389153531,
-1.39782315466176));
#69250=CARTESIAN_POINT('Ctrl Pts',(-0.0419392741322232,0.233437524640453,
-1.39788629978594));
#69251=CARTESIAN_POINT('Ctrl Pts',(-0.0419392748056671,0.233437524519463,
-1.41774927189049));
#69252=CARTESIAN_POINT('Ctrl Pts',(-0.0429471299453534,0.233256453743654,
-1.41768629466649));
#69253=CARTESIAN_POINT('Ctrl Pts',(-0.0439539256977684,0.233068835573067,
-1.41762337549457));
#69254=CARTESIAN_POINT('Ctrl Pts',(-0.0553224712183252,0.230873984485438,
-1.41691253152495));
#69255=CARTESIAN_POINT('Ctrl Pts',(-0.06554011284678,0.228183825399038,
-1.41626953355095));
#69256=CARTESIAN_POINT('Ctrl Pts',(-0.0845470134801674,0.221797166627857,
-1.41502133823456));
#69257=CARTESIAN_POINT('Ctrl Pts',(-0.0933589172298425,0.21823441694041,
-1.41442000382171));
#69258=CARTESIAN_POINT('Ctrl Pts',(-0.103926582184271,0.21320441263141,
-1.41365666145969));
#69259=CARTESIAN_POINT('Ctrl Pts',(-0.105906886730761,0.212227676923995,
-1.41351173996655));
#69260=CARTESIAN_POINT('Ctrl Pts',(-0.109040949761314,0.210627090303489,
-1.41327922726768));
#69261=CARTESIAN_POINT('Ctrl Pts',(-0.110203701302611,0.210021056079053,
-1.41319226071762));
#69262=CARTESIAN_POINT('Ctrl Pts',(-0.112395315967638,0.208855560161318,
-1.41302697402601));
#69263=CARTESIAN_POINT('Ctrl Pts',(-0.113425180465265,0.208298056672012,
-1.4129487251493));
#69264=CARTESIAN_POINT('Ctrl Pts',(-0.115754902574239,0.207014491955191,
-1.41277037102908));
#69265=CARTESIAN_POINT('Ctrl Pts',(-0.117052126120474,0.206283777704563,
-1.41267010151584));
#69266=CARTESIAN_POINT('Ctrl Pts',(-0.12100477299107,0.204007999381784,
-1.41236157398488));
#69267=CARTESIAN_POINT('Ctrl Pts',(-0.123637036916123,0.202423566950073,
-1.41215190508976));
#69268=CARTESIAN_POINT('Ctrl Pts',(-0.14168873956102,0.191074287202917,
-1.41068384569535));
#69269=CARTESIAN_POINT('Ctrl Pts',(-0.155964082793625,0.179610800336821,
-1.40936050605517));
#69270=CARTESIAN_POINT('Ctrl Pts',(-0.171438256427541,0.16393658487103,
-1.40775186298924));
#69271=CARTESIAN_POINT('Ctrl Pts',(-0.174030178785387,0.161182434296163,
-1.40747580711049));
#69272=CARTESIAN_POINT('Ctrl Pts',(-0.180927865979405,0.153492582535266,
-1.40672462599093));
#69273=CARTESIAN_POINT('Ctrl Pts',(-0.185097094813663,0.148438346239104,
-1.40625189756647));
#69274=CARTESIAN_POINT('Ctrl Pts',(-0.191265397099604,0.140295987032012,
-1.40552912763804));
#69275=CARTESIAN_POINT('Ctrl Pts',(-0.193410895170719,0.1373231422284,-1.40527279989218));
#69276=CARTESIAN_POINT('Ctrl Pts',(-0.196117824728577,0.133382987960167,
-1.40494397285027));
#69277=CARTESIAN_POINT('Ctrl Pts',(-0.196742428822608,0.132459954242744,
-1.40486770161186));
#69278=CARTESIAN_POINT('Ctrl Pts',(-0.197751246559312,0.130946254226803,
-1.40474390345106));
#69279=CARTESIAN_POINT('Ctrl Pts',(-0.198139366648698,0.130358231151531,
-1.40469612393591));
#69280=CARTESIAN_POINT('Ctrl Pts',(-0.198892400805194,0.129206210193456,
-1.40460313841397));
#69281=CARTESIAN_POINT('Ctrl Pts',(-0.199257547194572,0.128642379306804,
-1.4045579179733));
#69282=CARTESIAN_POINT('Ctrl Pts',(-0.200069914758296,0.127376226476415,
-1.40445699815584));
#69283=CARTESIAN_POINT('Ctrl Pts',(-0.200515847591602,0.126673078352879,
-1.40440138285757));
#69284=CARTESIAN_POINT('Ctrl Pts',(-0.202057029098631,0.124214407135713,
-1.40420835368872));
#69285=CARTESIAN_POINT('Ctrl Pts',(-0.203133038189173,0.122446851567583,
-1.40407212451938));
#69286=CARTESIAN_POINT('Ctrl Pts',(-0.210398053986977,0.110153239504552,
-1.40314038635887));
#69287=CARTESIAN_POINT('Ctrl Pts',(-0.215790055530291,0.0991756341979563,
-1.40238672240567));
#69288=CARTESIAN_POINT('Ctrl Pts',(-0.224366071248034,0.0776636051631953,
-1.40096535398361));
#69289=CARTESIAN_POINT('Ctrl Pts',(-0.227710469400293,0.0672287226322368,
-1.40029846074522));
#69290=CARTESIAN_POINT('Ctrl Pts',(-0.23173807816398,0.0508393571751145,
-1.39924548116094));
#69291=CARTESIAN_POINT('Ctrl Pts',(-0.232937127973371,0.0450273680455295,
-1.39887118490579));
#69292=CARTESIAN_POINT('Ctrl Pts',(-0.234594034787844,0.0351343118694262,
-1.39822768237138));
#69293=CARTESIAN_POINT('Ctrl Pts',(-0.235166141860016,0.0310751267202716,
-1.39796187696801));
#69294=CARTESIAN_POINT('Ctrl Pts',(-0.235822529548355,0.0253474491833521,
-1.39758335393401));
#69295=CARTESIAN_POINT('Ctrl Pts',(-0.235994829399859,0.02368963660025,
-1.39747339153144));
#69296=CARTESIAN_POINT('Ctrl Pts',(-0.236260910537195,0.0208374146375821,
-1.39728344957301));
#69297=CARTESIAN_POINT('Ctrl Pts',(-0.23636314237732,0.0196438420905053,
-1.39720373787824));
#69298=CARTESIAN_POINT('Ctrl Pts',(-0.236541317896038,0.0173602798973365,
-1.39705077733226));
#69299=CARTESIAN_POINT('Ctrl Pts',(-0.236618780331892,0.0162704368460603,
-1.39697757828265));
#69300=CARTESIAN_POINT('Ctrl Pts',(-0.236782862912788,0.0137120570755085,
-1.39680526371827));
#69301=CARTESIAN_POINT('Ctrl Pts',(-0.23686335489601,0.0122431865033005,
-1.39670595880646));
#69302=CARTESIAN_POINT('Ctrl Pts',(-0.23709509445159,0.00714687402652576,
-1.39636007339823));
#69303=CARTESIAN_POINT('Ctrl Pts',(-0.237176706813453,0.00351693476401216,
-1.39611134354054));
#69304=CARTESIAN_POINT('Ctrl Pts',(-0.237170428945466,-0.0096271083778691,
-1.39520165287263));
#69305=CARTESIAN_POINT('Ctrl Pts',(-0.236593455660036,-0.0191308966005396,
-1.39452629322106));
#69306=CARTESIAN_POINT('Ctrl Pts',(-0.233338429146559,-0.0459526329521729,
-1.39257640518096));
#69307=CARTESIAN_POINT('Ctrl Pts',(-0.229311743919245,-0.0630442636455679,
-1.39127764092337));
#69308=CARTESIAN_POINT('Ctrl Pts',(-0.222065781622701,-0.0834001484286103,
-1.38974309070626));
#69309=CARTESIAN_POINT('Ctrl Pts',(-0.220590552924236,-0.0872273410722001,
-1.38945540392021));
#69310=CARTESIAN_POINT('Ctrl Pts',(-0.218554935371255,-0.0921258317882973,
-1.38908993986535));
#69311=CARTESIAN_POINT('Ctrl Pts',(-0.21808469671968,-0.0932335447607527,
-1.38900748196616));
#69312=CARTESIAN_POINT('Ctrl Pts',(-0.217317997457725,-0.0950020684538213,
-1.38887618675399));
#69313=CARTESIAN_POINT('Ctrl Pts',(-0.217026913361217,-0.0956651657722182,
-1.38882703854436));
#69314=CARTESIAN_POINT('Ctrl Pts',(-0.21646116949202,-0.096938073019583,
-1.38873286072264));
#69315=CARTESIAN_POINT('Ctrl Pts',(-0.216186963279736,-0.0975480641393312,
-1.38868780644797));
#69316=CARTESIAN_POINT('Ctrl Pts',(-0.215521331154094,-0.0990122175391209,
-1.38857983181633));
#69317=CARTESIAN_POINT('Ctrl Pts',(-0.215127397500648,-0.0998652408191562,
-1.38851706308935));
#69318=CARTESIAN_POINT('Ctrl Pts',(-0.213740106358193,-0.10282297388671,
-1.38829982491187));
#69319=CARTESIAN_POINT('Ctrl Pts',(-0.212720809829733,-0.104915466418026,
-1.388146849749));
#69320=CARTESIAN_POINT('Ctrl Pts',(-0.210122481711546,-0.110055912561179,
-1.38777199047017));
#69321=CARTESIAN_POINT('Ctrl Pts',(-0.20850773805157,-0.113085308027284,
-1.38755190827367));
#69322=CARTESIAN_POINT('Ctrl Pts',(-0.201221121613751,-0.126068514666707,
-1.38660770909614));
#69323=CARTESIAN_POINT('Ctrl Pts',(-0.194897703930561,-0.135639722797267,
-1.38590853109235));
#69324=CARTESIAN_POINT('Ctrl Pts',(-0.178631829447137,-0.156760043844247,
-1.38427459882961));
#69325=CARTESIAN_POINT('Ctrl Pts',(-0.168221760574742,-0.167882118757019,
-1.38333965131958));
#69326=CARTESIAN_POINT('Ctrl Pts',(-0.154413733032921,-0.180051844099157,
-1.38215052405384));
#69327=CARTESIAN_POINT('Ctrl Pts',(-0.151964900048369,-0.182123406136785,
-1.38194147873121));
#69328=CARTESIAN_POINT('Ctrl Pts',(-0.148311745381434,-0.185088765740522,
-1.3816318269125));
#69329=CARTESIAN_POINT('Ctrl Pts',(-0.147139687643511,-0.186021872822759,
-1.38153280303838));
#69330=CARTESIAN_POINT('Ctrl Pts',(-0.145032621628037,-0.187666993041948,
-1.38135530928337));
#69331=CARTESIAN_POINT('Ctrl Pts',(-0.144101004916162,-0.188383284583807,
-1.381277012559));
#69332=CARTESIAN_POINT('Ctrl Pts',(-0.142133704031066,-0.189872749941943,
-1.38111202676177));
#69333=CARTESIAN_POINT('Ctrl Pts',(-0.141096948940548,-0.190644438358404,
-1.38102528297351));
#69334=CARTESIAN_POINT('Ctrl Pts',(-0.138341766994595,-0.192660419583374,
-1.38079526112967));
#69335=CARTESIAN_POINT('Ctrl Pts',(-0.136612895246199,-0.193890170228473,
-1.38065142923181));
#69336=CARTESIAN_POINT('Ctrl Pts',(-0.128100401593597,-0.199774751356675,
-1.37994548947575));
#69337=CARTESIAN_POINT('Ctrl Pts',(-0.121094958642767,-0.204097151313251,
-1.37937111212416));
#69338=CARTESIAN_POINT('Ctrl Pts',(-0.105352792476685,-0.212714047412349,
-1.37809420760581));
#69339=CARTESIAN_POINT('Ctrl Pts',(-0.0965475001049797,-0.216852552458957,
-1.37738840730181));
#69340=CARTESIAN_POINT('Ctrl Pts',(-0.0741821801217256,-0.225731544944955,
-1.3756318807314));
#69341=CARTESIAN_POINT('Ctrl Pts',(-0.0603967063129183,-0.229804345371231,
-1.37457931256262));
#69342=CARTESIAN_POINT('Ctrl Pts',(-0.0445002670189007,-0.2329703305017,
-1.37344939102814));
#69343=CARTESIAN_POINT('Ctrl Pts',(-0.0426695804121364,-0.233312571661833,
-1.37332052292008));
#69344=CARTESIAN_POINT('Ctrl Pts',(-0.0398705077542063,-0.233801800395719,
-1.37312559123558));
#69345=CARTESIAN_POINT('Ctrl Pts',(-0.0389049751829175,-0.233964403805189,
-1.37305873052469));
#69346=CARTESIAN_POINT('Ctrl Pts',(-0.0372777583448618,-0.234228088245201,
-1.37294672087146));
#69347=CARTESIAN_POINT('Ctrl Pts',(-0.0366166099122925,-0.234332354810391,
-1.37290139682346));
#69348=CARTESIAN_POINT('Ctrl Pts',(-0.0352548714283871,-0.234541204041472,
-1.37280843933128));
#69349=CARTESIAN_POINT('Ctrl Pts',(-0.0345542414362199,-0.234645449103323,
-1.37276082485481));
#69350=CARTESIAN_POINT('Ctrl Pts',(-0.0327330803718395,-0.23490808139759,
-1.37263758835211));
#69351=CARTESIAN_POINT('Ctrl Pts',(-0.0316118478432321,-0.235061592907282,
-1.37256223460363));
#69352=CARTESIAN_POINT('Ctrl Pts',(-0.0266917272786496,-0.235699380569875,
-1.37223367535917));
#69353=CARTESIAN_POINT('Ctrl Pts',(-0.0228822902957143,-0.23609966361483,
-1.3719847727049));
#69354=CARTESIAN_POINT('Ctrl Pts',(-0.0120826331528088,-0.236970578587025,
-1.37129038046716));
#69355=CARTESIAN_POINT('Ctrl Pts',(-0.0050786400173435,-0.2372240861543,
-1.37085324878858));
#69356=CARTESIAN_POINT('Ctrl Pts',(0.0179500283192576,-0.237036998915701,
-1.36943058559849));
#69357=CARTESIAN_POINT('Ctrl Pts',(0.0339182507468475,-0.235283419466258,
-1.36846447640405));
#69358=CARTESIAN_POINT('Ctrl Pts',(0.0564575881648879,-0.230464475200226,
-1.36701384257709));
#69359=CARTESIAN_POINT('Ctrl Pts',(0.0632582589663762,-0.228691302104172,
-1.36656481679112));
#69360=CARTESIAN_POINT('Ctrl Pts',(0.0719704511805524,-0.226001369708364,
-1.36596936728562));
#69361=CARTESIAN_POINT('Ctrl Pts',(0.0739628151600318,-0.225357197498067,
-1.36583180614467));
#69362=CARTESIAN_POINT('Ctrl Pts',(0.0771650071169762,-0.224274825017162,
-1.36560833610127));
#69363=CARTESIAN_POINT('Ctrl Pts',(0.0783802840535355,-0.223853001812999,
-1.3655229680166));
#69364=CARTESIAN_POINT('Ctrl Pts',(0.0807005860550093,-0.223026412877333,
-1.36535887620145));
#69365=CARTESIAN_POINT('Ctrl Pts',(0.0818061507671564,-0.222623267070293,
-1.36528020834205));
#69366=CARTESIAN_POINT('Ctrl Pts',(0.0843474518637464,-0.221675091774994,
-1.3650982412579));
#69367=CARTESIAN_POINT('Ctrl Pts',(0.0857809730416737,-0.221124316663985,
-1.36499475253513));
#69368=CARTESIAN_POINT('Ctrl Pts',(0.0902994010818894,-0.219337735912614,
-1.36466582372755));
#69369=CARTESIAN_POINT('Ctrl Pts',(0.0933636187113242,-0.218051042145838,
-1.36443868788434));
#69370=CARTESIAN_POINT('Ctrl Pts',(0.100496385621436,-0.214878015437962,
-1.36390006384044));
#69371=CARTESIAN_POINT('Ctrl Pts',(0.104540358629836,-0.212939883411607,
-1.36358692633651));
#69372=CARTESIAN_POINT('Ctrl Pts',(0.119731242323108,-0.205122396791407,
-1.36238071825746));
#69373=CARTESIAN_POINT('Ctrl Pts',(0.130457240857722,-0.198473202165949,
-1.36146467590324));
#69374=CARTESIAN_POINT('Ctrl Pts',(0.151176346371205,-0.183221343677735,
-1.35958568862047));
#69375=CARTESIAN_POINT('Ctrl Pts',(0.161085967741501,-0.174572979836453,
-1.35862569667976));
#69376=CARTESIAN_POINT('Ctrl Pts',(0.171666909520577,-0.16366647180175,
-1.35756581343514));
#69377=CARTESIAN_POINT('Ctrl Pts',(0.173084942369714,-0.16216610392902,
-1.35742299629438));
#69378=CARTESIAN_POINT('Ctrl Pts',(0.175046656083968,-0.160035435669459,
-1.35722455929758));
#69379=CARTESIAN_POINT('Ctrl Pts',(0.175606836291864,-0.159420549415688,
-1.35716779310845));
#69380=CARTESIAN_POINT('Ctrl Pts',(0.17661339218452,-0.158303952077766,
-1.35706562971752));
#69381=CARTESIAN_POINT('Ctrl Pts',(0.177060893198148,-0.157803268923824,
-1.35702015007105));
#69382=CARTESIAN_POINT('Ctrl Pts',(0.177973765308479,-0.156773136534114,
-1.35692726452776));
#69383=CARTESIAN_POINT('Ctrl Pts',(0.178438912007092,-0.156243502877947,
-1.35687987490297));
#69384=CARTESIAN_POINT('Ctrl Pts',(0.179634359814534,-0.15487001897758,
-1.35675789997811));
#69385=CARTESIAN_POINT('Ctrl Pts',(0.180361089120951,-0.154023062097295,
-1.35668357275254));
#69386=CARTESIAN_POINT('Ctrl Pts',(0.183458107362167,-0.150361704638763,
-1.35636589381563));
#69387=CARTESIAN_POINT('Ctrl Pts',(0.18576884883244,-0.14749731461147,-1.35612650132637));
#69388=CARTESIAN_POINT('Ctrl Pts',(0.192027494092287,-0.139358565646511,
-1.35546760397506));
#69389=CARTESIAN_POINT('Ctrl Pts',(0.195823875336761,-0.133971604301315,
-1.35505546605861));
#69390=CARTESIAN_POINT('Ctrl Pts',(0.201133990348386,-0.125727703035984,
-1.35444850223891));
#69391=CARTESIAN_POINT('Ctrl Pts',(0.202821461987519,-0.122986960986254,
-1.35425042430521));
#69392=CARTESIAN_POINT('Ctrl Pts',(0.213996540516776,-0.103980859844897,
-1.35289651813524));
#69393=CARTESIAN_POINT('Ctrl Pts',(0.221572491773095,-0.0866722844692302,
-1.3517541149914));
#69394=CARTESIAN_POINT('Ctrl Pts',(0.22789824770484,-0.0657535607218792,
-1.35033997355525));
#69395=CARTESIAN_POINT('Ctrl Pts',(0.228718781702932,-0.0628399522235472,
-1.35014247279239));
#69396=CARTESIAN_POINT('Ctrl Pts',(0.229857201130097,-0.0584793859985416,
-1.34984571138063));
#69397=CARTESIAN_POINT('Ctrl Pts',(0.2302176743965,-0.0570437877981794,
-1.34974782350547));
#69398=CARTESIAN_POINT('Ctrl Pts',(0.230839025646515,-0.0544673681293576,
-1.34957176917375));
#69399=CARTESIAN_POINT('Ctrl Pts',(0.231104944369353,-0.0533278028436546,
-1.34949376765513));
#69400=CARTESIAN_POINT('Ctrl Pts',(0.231652076489912,-0.0509021522962062,
-1.34932743410502));
#69401=CARTESIAN_POINT('Ctrl Pts',(0.231931035687726,-0.0496156045405141,
-1.34923903269144));
#69402=CARTESIAN_POINT('Ctrl Pts',(0.232654094637426,-0.0461414726759075,
-1.34899980147271));
#69403=CARTESIAN_POINT('Ctrl Pts',(0.233078036066404,-0.0439498778300113,
-1.34884833586036));
#69404=CARTESIAN_POINT('Ctrl Pts',(0.23521512146049,-0.0319998117682699,
-1.34801920778947));
#69405=CARTESIAN_POINT('Ctrl Pts',(0.236346216869232,-0.0221485761220135,
-1.34732340164914));
#69406=CARTESIAN_POINT('Ctrl Pts',(0.237385352686255,-0.00206735097595695,
-1.34588188362514));
#69407=CARTESIAN_POINT('Ctrl Pts',(0.237254544561929,0.00814475353624223,
-1.34513676143195));
#69408=CARTESIAN_POINT('Ctrl Pts',(0.236307634784926,0.0203697165068839,
-1.34424135858273));
#69409=CARTESIAN_POINT('Ctrl Pts',(0.23612181286623,0.0224212662869678,
-1.34409100529598));
#69410=CARTESIAN_POINT('Ctrl Pts',(0.234797871217047,0.0351849887777631,
-1.34315573282199));
#69411=CARTESIAN_POINT('Ctrl Pts',(0.232957608875962,0.0458130032771233,
-1.34237703706866));
#69412=CARTESIAN_POINT('Ctrl Pts',(0.230079265180973,0.0575964266217463,
-1.34153743714864));
#69413=CARTESIAN_POINT('Ctrl Pts',(0.229746450762631,0.0589099753947206,
-1.34144419070656));
#69414=CARTESIAN_POINT('Ctrl Pts',(0.229189630387646,0.0610311074394687,
-1.34129425723242));
#69415=CARTESIAN_POINT('Ctrl Pts',(0.228972575422344,0.0618404601477494,
-1.34123719966252));
#69416=CARTESIAN_POINT('Ctrl Pts',(0.228577999236883,0.0632811898750169,
-1.34113592353936));
#69417=CARTESIAN_POINT('Ctrl Pts',(0.22840214422485,0.063912997703503,-1.34109161242942));
#69418=CARTESIAN_POINT('Ctrl Pts',(0.228011219893008,0.0652952803985223,
-1.34099489265104));
#69419=CARTESIAN_POINT('Ctrl Pts',(0.227795064856602,0.0660454276271205,
-1.34094254711387));
#69420=CARTESIAN_POINT('Ctrl Pts',(0.227162888951108,0.0681993107448984,
-1.34079262361014));
#69421=CARTESIAN_POINT('Ctrl Pts',(0.226737560230538,0.0696003099903044,
-1.34069556504387));
#69422=CARTESIAN_POINT('Ctrl Pts',(0.223223889427796,0.0807999031382693,
-1.33992269814227));
#69423=CARTESIAN_POINT('Ctrl Pts',(0.219514397376743,0.0903936637310679,
-1.33927903149315));
#69424=CARTESIAN_POINT('Ctrl Pts',(0.208410349768753,0.114356542456391,
-1.33764771829156));
#69425=CARTESIAN_POINT('Ctrl Pts',(0.200151198567343,0.128264500313431,
-1.33667499509042));
#69426=CARTESIAN_POINT('Ctrl Pts',(0.186436603748621,0.146768389193457,
-1.33522438379733));
#69427=CARTESIAN_POINT('Ctrl Pts',(0.182089506981463,0.152128119778144,
-1.33478321621127));
#69428=CARTESIAN_POINT('Ctrl Pts',(0.176136271622478,0.158846840050143,
-1.33419689484953));
#69429=CARTESIAN_POINT('Ctrl Pts',(0.174736838051403,0.160384979812369,
-1.33406026392175));
#69430=CARTESIAN_POINT('Ctrl Pts',(0.172441387726069,0.162842240247576,
-1.33383793601572));
#69431=CARTESIAN_POINT('Ctrl Pts',(0.171557797697396,0.163772859011835,
-1.33375276960803));
#69432=CARTESIAN_POINT('Ctrl Pts',(0.169848915416609,0.165543690646399,
-1.33358881521645));
#69433=CARTESIAN_POINT('Ctrl Pts',(0.169024829627993,0.166385018748336,
-1.33351008108543));
#69434=CARTESIAN_POINT('Ctrl Pts',(0.167107085451819,0.168313937291127,
-1.33332759238982));
#69435=CARTESIAN_POINT('Ctrl Pts',(0.166009025680677,0.169397056324437,
-1.33322364470926));
#69436=CARTESIAN_POINT('Ctrl Pts',(0.162485511194223,0.172805465234497,
-1.33289173735513));
#69437=CARTESIAN_POINT('Ctrl Pts',(0.160021265152094,0.175089870768702,
-1.33266203808378));
#69438=CARTESIAN_POINT('Ctrl Pts',(0.154108437845492,0.180342072950492,
-1.33211621187048));
#69439=CARTESIAN_POINT('Ctrl Pts',(0.150621441701078,0.183264427782036,
-1.33179837493704));
#69440=CARTESIAN_POINT('Ctrl Pts',(0.12926598355019,0.200140515028974,-1.32987557459896));
#69441=CARTESIAN_POINT('Ctrl Pts',(0.109559503383775,0.211571239441693,
-1.32818217708357));
#69442=CARTESIAN_POINT('Ctrl Pts',(0.0844684286795744,0.221667002692134,
-1.32625765233554));
#69443=CARTESIAN_POINT('Ctrl Pts',(0.0803590516932933,0.223189615035733,
-1.32594979805719));
#69444=CARTESIAN_POINT('Ctrl Pts',(0.0750443276835538,0.22499298560114,
-1.32556295431464));
#69445=CARTESIAN_POINT('Ctrl Pts',(0.0738760162098553,0.225379300470429,
-1.32547860663166));
#69446=CARTESIAN_POINT('Ctrl Pts',(0.0720097249742363,0.225980338190002,
-1.32534502295089));
#69447=CARTESIAN_POINT('Ctrl Pts',(0.0713136883165767,0.226200954097564,
-1.32529545736386));
#69448=CARTESIAN_POINT('Ctrl Pts',(0.0699805046981877,0.226616754913183,
-1.32520102101074));
#69449=CARTESIAN_POINT('Ctrl Pts',(0.0693435447264682,0.226812472012421,
-1.32515612155123));
#69450=CARTESIAN_POINT('Ctrl Pts',(0.0678204103913752,0.227273465690268,
-1.32504926427574));
#69451=CARTESIAN_POINT('Ctrl Pts',(0.0669334819703331,0.227536250596239,
-1.32498744990321));
#69452=CARTESIAN_POINT('Ctrl Pts',(0.0638962244466875,0.228416852680628,
-1.32477709224167));
#69453=CARTESIAN_POINT('Ctrl Pts',(0.0617386241588662,0.229009452362055,
-1.32462991967725));
#69454=CARTESIAN_POINT('Ctrl Pts',(0.0564222575080445,0.230389028030097,
-1.32427207538616));
#69455=CARTESIAN_POINT('Ctrl Pts',(0.0532549881082419,0.231141696375161,
-1.32406300078719));
#69456=CARTESIAN_POINT('Ctrl Pts',(0.0399171142029785,0.234022562892254,
-1.32319588936015));
#69457=CARTESIAN_POINT('Ctrl Pts',(0.0296271888497427,0.235546595181886,
-1.32255883153795));
#69458=CARTESIAN_POINT('Ctrl Pts',(0.00270132566876937,0.237741502872241,
-1.32090298004351));
#69459=CARTESIAN_POINT('Ctrl Pts',(-0.0139611691113274,0.23734641893675,
-1.31988604334673));
#69460=CARTESIAN_POINT('Ctrl Pts',(-0.033591505261568,0.234805579509177,
-1.31860683335724));
#69461=CARTESIAN_POINT('Ctrl Pts',(-0.0367297670179699,0.234335170332696,
-1.31839997276463));
#69462=CARTESIAN_POINT('Ctrl Pts',(-0.0405519932500514,0.233683574011484,
-1.31814477381336));
#69463=CARTESIAN_POINT('Ctrl Pts',(-0.0412459145842788,0.23356209328554,
-1.31809831128101));
#69464=CARTESIAN_POINT('Ctrl Pts',(-0.0419392741369039,0.233437524639612,
-1.31805175208418));
#69465=CARTESIAN_POINT('Origin',(0.,0.,-2.1456589891905));
#69466=CARTESIAN_POINT('',(-0.0419392699415209,0.233437525393353,-1.19828290886153));
#69467=CARTESIAN_POINT('',(-0.041939274136423,0.233437524639699,-1.21783461098805));
#69468=CARTESIAN_POINT('',(-0.0419392741328076,0.233437524640348,-2.1456589891905));
#69469=CARTESIAN_POINT('',(-0.23717491446692,0.000201426436582323,-1.27600110192935));
#69470=CARTESIAN_POINT('Ctrl Pts',(-0.0419392699415209,0.233437525393353,
-1.19828290886153));
#69471=CARTESIAN_POINT('Ctrl Pts',(-0.0375335716888505,0.234229050954585,
-1.198602388006));
#69472=CARTESIAN_POINT('Ctrl Pts',(-0.033105142309298,0.234895910556959,
-1.19891811259145));
#69473=CARTESIAN_POINT('Ctrl Pts',(-0.0273288220524848,0.235599050176692,
-1.1993207924431));
#69474=CARTESIAN_POINT('Ctrl Pts',(-0.0259969815930074,0.235749727706377,
-1.199413009077));
#69475=CARTESIAN_POINT('Ctrl Pts',(-0.0238347252023007,0.235975807113033,
-1.19956162851533));
#69476=CARTESIAN_POINT('Ctrl Pts',(-0.0230050853663194,0.23605813218132,
-1.19961839155736));
#69477=CARTESIAN_POINT('Ctrl Pts',(-0.0215221072182611,0.236197395351657,
-1.19971936871144));
#69478=CARTESIAN_POINT('Ctrl Pts',(-0.0208689508174868,0.23625600012612,
-1.19976367287095));
#69479=CARTESIAN_POINT('Ctrl Pts',(-0.0194338546162219,0.236378766840449,
-1.19986064273661));
#69480=CARTESIAN_POINT('Ctrl Pts',(-0.0186518346691687,0.236441758634999,
-1.19991324313493));
#69481=CARTESIAN_POINT('Ctrl Pts',(-0.0163919179361852,0.236612513133608,
-1.20006459190996));
#69482=CARTESIAN_POINT('Ctrl Pts',(-0.0149132730379966,0.236710310103008,
-1.20016280565689));
#69483=CARTESIAN_POINT('Ctrl Pts',(-0.00222524823829375,0.237430124516555,
-1.20099934766508));
#69484=CARTESIAN_POINT('Ctrl Pts',(0.00901590548175787,0.237269464910186,
-1.20169925092852));
#69485=CARTESIAN_POINT('Ctrl Pts',(0.0387686965193935,0.234725603632027,
-1.20353873484218));
#69486=CARTESIAN_POINT('Ctrl Pts',(0.0570793929326259,0.230956743988287,
-1.20466237556514));
#69487=CARTESIAN_POINT('Ctrl Pts',(0.0787267563728954,0.223766728035313,
-1.20612397067814));
#69488=CARTESIAN_POINT('Ctrl Pts',(0.0826576774958468,0.222344677630813,
-1.206394736598));
#69489=CARTESIAN_POINT('Ctrl Pts',(0.0881554191161044,0.220189873714043,
-1.2067821181835));
#69490=CARTESIAN_POINT('Ctrl Pts',(0.0897550892326629,0.219542665785454,
-1.2068958907564));
#69491=CARTESIAN_POINT('Ctrl Pts',(0.092351989574049,0.218458864188389,
-1.20708238603676));
#69492=CARTESIAN_POINT('Ctrl Pts',(0.0933535468765892,0.218032751069364,
-1.20715475277753));
#69493=CARTESIAN_POINT('Ctrl Pts',(0.0954556219844288,0.217121282961472,
-1.20730758471329));
#69494=CARTESIAN_POINT('Ctrl Pts',(0.0965554486869348,0.216634421364518,
-1.20738809961092));
#69495=CARTESIAN_POINT('Ctrl Pts',(0.099192734216556,0.215442898124175,
-1.20758252374353));
#69496=CARTESIAN_POINT('Ctrl Pts',(0.100726433123141,0.214730124308128,
-1.2076967089646));
#69497=CARTESIAN_POINT('Ctrl Pts',(0.106091992143453,0.212166393656812,
-1.20810021416272));
#69498=CARTESIAN_POINT('Ctrl Pts',(0.109881337151372,0.210228868317865,
-1.20839250436415));
#69499=CARTESIAN_POINT('Ctrl Pts',(0.119098303118215,0.205198872537217,
-1.20912220733912));
#69500=CARTESIAN_POINT('Ctrl Pts',(0.124459553273245,0.201992057558137,
-1.20956331990691));
#69501=CARTESIAN_POINT('Ctrl Pts',(0.138566333363702,0.192779162508644,
-1.21076875221957));
#69502=CARTESIAN_POINT('Ctrl Pts',(0.14704558181697,0.186392067274509,-1.21154287397845));
#69503=CARTESIAN_POINT('Ctrl Pts',(0.164151871164029,0.171610771149758,
-1.21319388934757));
#69504=CARTESIAN_POINT('Ctrl Pts',(0.172627208081991,0.163082795514992,
-1.21406862173344));
#69505=CARTESIAN_POINT('Ctrl Pts',(0.181772243374075,0.152365239229572,
-1.21505150918695));
#69506=CARTESIAN_POINT('Ctrl Pts',(0.18310268747856,0.150763792618592,-1.21519556270663));
#69507=CARTESIAN_POINT('Ctrl Pts',(0.184936967490161,0.148495777033672,
-1.21539543456646));
#69508=CARTESIAN_POINT('Ctrl Pts',(0.185458585696061,0.147843805368463,
-1.21545242012444));
#69509=CARTESIAN_POINT('Ctrl Pts',(0.186394107378123,0.146661752388024,
-1.21555487112382));
#69510=CARTESIAN_POINT('Ctrl Pts',(0.186809219041781,0.146132640433667,
-1.21560042032738));
#69511=CARTESIAN_POINT('Ctrl Pts',(0.18765427416922,0.145046025926246,-1.21569331831912));
#69512=CARTESIAN_POINT('Ctrl Pts',(0.188083994851933,0.144488363422198,
-1.21574065171482));
#69513=CARTESIAN_POINT('Ctrl Pts',(0.18918561232246,0.143045516074784,-1.21586226105625));
#69514=CARTESIAN_POINT('Ctrl Pts',(0.189853791831849,0.142157495149407,
-1.21593628201826));
#69515=CARTESIAN_POINT('Ctrl Pts',(0.192679999325499,0.138345951144541,
-1.21625064542326));
#69516=CARTESIAN_POINT('Ctrl Pts',(0.194777058866314,0.135377565306569,
-1.21648713100904));
#69517=CARTESIAN_POINT('Ctrl Pts',(0.200411454103742,0.126999944798079,
-1.21713533541856));
#69518=CARTESIAN_POINT('Ctrl Pts',(0.203797327226507,0.121492379964609,
-1.21753997385796));
#69519=CARTESIAN_POINT('Ctrl Pts',(0.209111452476666,0.111999484198508,
-1.21821377993903));
#69520=CARTESIAN_POINT('Ctrl Pts',(0.211160658382324,0.108086362965915,
-1.21848512385362));
#69521=CARTESIAN_POINT('Ctrl Pts',(0.220850817074418,0.0882534555678281,
-1.21983893035908));
#69522=CARTESIAN_POINT('Ctrl Pts',(0.226805497127547,0.071574697556417,
-1.22091486815826));
#69523=CARTESIAN_POINT('Ctrl Pts',(0.231570621596853,0.0513496594690051,
-1.22225828064958));
#69524=CARTESIAN_POINT('Ctrl Pts',(0.232226870004729,0.0482951309811835,
-1.22246200318195));
#69525=CARTESIAN_POINT('Ctrl Pts',(0.23310843446395,0.0437571195147533,
-1.22276631444747));
#69526=CARTESIAN_POINT('Ctrl Pts',(0.233380333225057,0.0422829471140898,
-1.2228654241886));
#69527=CARTESIAN_POINT('Ctrl Pts',(0.233839973352956,0.0396512592634784,
-1.22304285243333));
#69528=CARTESIAN_POINT('Ctrl Pts',(0.234033140820919,0.0384947322581955,
-1.2231209959828));
#69529=CARTESIAN_POINT('Ctrl Pts',(0.234423333912465,0.0360470119439916,
-1.22328676447424));
#69530=CARTESIAN_POINT('Ctrl Pts',(0.234618284463202,0.0347555323619409,
-1.22337445235446));
#69531=CARTESIAN_POINT('Ctrl Pts',(0.235110584483999,0.0313011222896039,
-1.22360962838645));
#69532=CARTESIAN_POINT('Ctrl Pts',(0.235388745978136,0.0291356294528762,
-1.22375771536972));
#69533=CARTESIAN_POINT('Ctrl Pts',(0.236671314626061,0.0179284385121385,
-1.22452774614878));
#69534=CARTESIAN_POINT('Ctrl Pts',(0.237184672265297,0.00883934162330922,
-1.22516485220924));
#69535=CARTESIAN_POINT('Ctrl Pts',(0.23716317265967,-0.0110931547559999,
-1.22658884910768));
#69536=CARTESIAN_POINT('Ctrl Pts',(0.236408704781146,-0.0219162313744683,
-1.22737964729629));
#69537=CARTESIAN_POINT('Ctrl Pts',(0.233243498756143,-0.0446906506752908,
-1.22905888857587));
#69538=CARTESIAN_POINT('Ctrl Pts',(0.230646363080531,-0.0565870840435355,
-1.2299451411992));
#69539=CARTESIAN_POINT('Ctrl Pts',(0.226552130538029,-0.0702168360177963,
-1.23093785208365));
#69540=CARTESIAN_POINT('Ctrl Pts',(0.225930175862904,-0.0721929932594657,
-1.23108118188371));
#69541=CARTESIAN_POINT('Ctrl Pts',(0.225021859586135,-0.0749522349768024,
-1.23128022060694));
#69542=CARTESIAN_POINT('Ctrl Pts',(0.22475716305234,-0.0757422770246938,
-1.23133708444167));
#69543=CARTESIAN_POINT('Ctrl Pts',(0.224271454412186,-0.077167007120609,
-1.23143938159245));
#69544=CARTESIAN_POINT('Ctrl Pts',(0.224051897942451,-0.0778021806965472,
-1.23148489790129));
#69545=CARTESIAN_POINT('Ctrl Pts',(0.223596589534452,-0.0791014687970383,
-1.23157780822877));
#69546=CARTESIAN_POINT('Ctrl Pts',(0.223360572993072,-0.0797654792657574,
-1.23162518630813));
#69547=CARTESIAN_POINT('Ctrl Pts',(0.222743688972042,-0.0814768160695972,
-1.23174704688657));
#69548=CARTESIAN_POINT('Ctrl Pts',(0.222358387838322,-0.0825225424583822,
-1.23182127238899));
#69549=CARTESIAN_POINT('Ctrl Pts',(0.220675204369397,-0.0869933929168607,
-1.23213774736747));
#69550=CARTESIAN_POINT('Ctrl Pts',(0.219305368477771,-0.0903911233521313,
-1.2323760754072));
#69551=CARTESIAN_POINT('Ctrl Pts',(0.215271781032465,-0.0997638206390286,
-1.2330310195956));
#69552=CARTESIAN_POINT('Ctrl Pts',(0.212438670425472,-0.105662591894336,
-1.23344037618754));
#69553=CARTESIAN_POINT('Ctrl Pts',(0.207565674377541,-0.114817851775556,
-1.23408247598968));
#69554=CARTESIAN_POINT('Ctrl Pts',(0.205684564094864,-0.118154599439263,
-1.23431797982359));
#69555=CARTESIAN_POINT('Ctrl Pts',(0.194409279385959,-0.137068935582851,
-1.2356691781174));
#69556=CARTESIAN_POINT('Ctrl Pts',(0.183329837601139,-0.151568289716536,
-1.23677538157028));
#69557=CARTESIAN_POINT('Ctrl Pts',(0.168560572967574,-0.166879707730256,
-1.23815124522914));
#69558=CARTESIAN_POINT('Ctrl Pts',(0.166375106479975,-0.169058646987889,
-1.23835253008245));
#69559=CARTESIAN_POINT('Ctrl Pts',(0.163071042917213,-0.17222671408156,
-1.23865389315342));
#69560=CARTESIAN_POINT('Ctrl Pts',(0.161984560066371,-0.173248977516235,
-1.23875253452157));
#69561=CARTESIAN_POINT('Ctrl Pts',(0.160027601322428,-0.175055763783461,
-1.23892944317364));
#69562=CARTESIAN_POINT('Ctrl Pts',(0.159160811215797,-0.175844219999847,
-1.23900753940827));
#69563=CARTESIAN_POINT('Ctrl Pts',(0.157312469455246,-0.177500660132121,
-1.23917354399123));
#69564=CARTESIAN_POINT('Ctrl Pts',(0.156329499418021,-0.178366994944431,
-1.23926151778802));
#69565=CARTESIAN_POINT('Ctrl Pts',(0.153675191617895,-0.180667557593463,
-1.23949828294124));
#69566=CARTESIAN_POINT('Ctrl Pts',(0.151991005567457,-0.182086695124216,
-1.23964768738499));
#69567=CARTESIAN_POINT('Ctrl Pts',(0.143017698628761,-0.189436590708973,
-1.24043964756818));
#69568=CARTESIAN_POINT('Ctrl Pts',(0.135401559154596,-0.194952970771413,
-1.24109843569143));
#69569=CARTESIAN_POINT('Ctrl Pts',(0.118517889648167,-0.205714414925099,
-1.24253068438605));
#69570=CARTESIAN_POINT('Ctrl Pts',(0.109183376990809,-0.210817153469351,
-1.2433064161843));
#69571=CARTESIAN_POINT('Ctrl Pts',(0.0886256387895476,-0.220322580180069,
-1.24496044281448));
#69572=CARTESIAN_POINT('Ctrl Pts',(0.0773433116924118,-0.224531986851791,
-1.24583657246531));
#69573=CARTESIAN_POINT('Ctrl Pts',(0.0637935348351434,-0.228444043699048,
-1.24682040732057));
#69574=CARTESIAN_POINT('Ctrl Pts',(0.0617900912740089,-0.228994064429848,
-1.24696414925404));
#69575=CARTESIAN_POINT('Ctrl Pts',(0.0589723462046585,-0.229727967098623,
-1.2471636624892));
#69576=CARTESIAN_POINT('Ctrl Pts',(0.0581639773478486,-0.229933965033463,
-1.24722059570296));
#69577=CARTESIAN_POINT('Ctrl Pts',(0.0567021794328324,-0.230298274974983,
-1.24732298052519));
#69578=CARTESIAN_POINT('Ctrl Pts',(0.0560491333760602,-0.230458081431589,
-1.247368515565));
#69579=CARTESIAN_POINT('Ctrl Pts',(0.0547105801916713,-0.230779611491156,
-1.24746141877361));
#69580=CARTESIAN_POINT('Ctrl Pts',(0.0540250183372702,-0.23094106194336,
-1.24750877131527));
#69581=CARTESIAN_POINT('Ctrl Pts',(0.0522546133921074,-0.231349678920033,
-1.24763048832594));
#69582=CARTESIAN_POINT('Ctrl Pts',(0.0511687167463624,-0.231592273414444,
-1.24770459694924));
#69583=CARTESIAN_POINT('Ctrl Pts',(0.0465172289896875,-0.232597124113077,
-1.24801986346981));
#69584=CARTESIAN_POINT('Ctrl Pts',(0.04293581155542,-0.233284792408089,
-1.2482571369598));
#69585=CARTESIAN_POINT('Ctrl Pts',(0.0329342313703243,-0.234967036408672,
-1.24890821912993));
#69586=CARTESIAN_POINT('Ctrl Pts',(0.0264866970737981,-0.235780912877295,
-1.24931487121684));
#69587=CARTESIAN_POINT('Ctrl Pts',(0.00687954081525848,-0.237441338683237,
-1.25053339237953));
#69588=CARTESIAN_POINT('Ctrl Pts',(-0.00632420959262735,-0.237456796389125,
-1.25133061006629));
#69589=CARTESIAN_POINT('Ctrl Pts',(-0.0295998977389296,-0.23554048620596,
-1.25277999032555));
#69590=CARTESIAN_POINT('Ctrl Pts',(-0.0396734207663531,-0.234054387118378,
-1.25342192307541));
#69591=CARTESIAN_POINT('Ctrl Pts',(-0.0518601175622236,-0.23144709601843,
-1.25423380177062));
#69592=CARTESIAN_POINT('Ctrl Pts',(-0.0540934470559132,-0.230935333877508,
-1.25438403453708));
#69593=CARTESIAN_POINT('Ctrl Pts',(-0.0576231802799222,-0.230072493752527,
-1.25462394377638));
#69594=CARTESIAN_POINT('Ctrl Pts',(-0.0589246567527828,-0.229742612477567,
-1.25471293883549));
#69595=CARTESIAN_POINT('Ctrl Pts',(-0.0613523491467177,-0.229105287215435,
-1.25487998184532));
#69596=CARTESIAN_POINT('Ctrl Pts',(-0.0624792368081042,-0.228800542525143,
-1.25495794031191));
#69597=CARTESIAN_POINT('Ctrl Pts',(-0.0649935405305061,-0.228100638576624,
-1.25513284451306));
#69598=CARTESIAN_POINT('Ctrl Pts',(-0.0663796835255853,-0.227701117882089,
-1.25522992950839));
#69599=CARTESIAN_POINT('Ctrl Pts',(-0.0704775831593784,-0.226479403771714,
-1.25551895219583));
#69600=CARTESIAN_POINT('Ctrl Pts',(-0.0731782623176248,-0.225621255141515,
-1.25571205269697));
#69601=CARTESIAN_POINT('Ctrl Pts',(-0.0854993628401374,-0.221461703704126,
-1.256605488278));
#69602=CARTESIAN_POINT('Ctrl Pts',(-0.0949153568900448,-0.217592399978162,
-1.25732414063531));
#69603=CARTESIAN_POINT('Ctrl Pts',(-0.112525807015649,-0.208994793021325,
-1.25873543197637));
#69604=CARTESIAN_POINT('Ctrl Pts',(-0.120744111772503,-0.204356856942591,
-1.25942482440171));
#69605=CARTESIAN_POINT('Ctrl Pts',(-0.138211384784208,-0.193077068790269,
-1.26094278702197));
#69606=CARTESIAN_POINT('Ctrl Pts',(-0.147304152967612,-0.186232866438805,
-1.2617691230051));
#69607=CARTESIAN_POINT('Ctrl Pts',(-0.157431156384765,-0.177402626885747,
-1.26270633061598));
#69608=CARTESIAN_POINT('Ctrl Pts',(-0.158972736150481,-0.176022529564649,
-1.26284947525539));
#69609=CARTESIAN_POINT('Ctrl Pts',(-0.161109231262601,-0.174058868412775,
-1.26304830073329));
#69610=CARTESIAN_POINT('Ctrl Pts',(-0.16171937944521,-0.173492122113766,
-1.26310513334465));
#69611=CARTESIAN_POINT('Ctrl Pts',(-0.162816427076907,-0.172462294910592,
-1.26320739105558));
#69612=CARTESIAN_POINT('Ctrl Pts',(-0.16330436681252,-0.172000336954926,
-1.26325289895056));
#69613=CARTESIAN_POINT('Ctrl Pts',(-0.164300144224293,-0.171049525211686,
-1.2633458125583));
#69614=CARTESIAN_POINT('Ctrl Pts',(-0.164807776125104,-0.170560471472699,
-1.26339320219093));
#69615=CARTESIAN_POINT('Ctrl Pts',(-0.166061136652461,-0.169342160739758,
-1.26351029119111));
#69616=CARTESIAN_POINT('Ctrl Pts',(-0.166804258197174,-0.168610225247599,
-1.26357978669083));
#69617=CARTESIAN_POINT('Ctrl Pts',(-0.169842567043281,-0.165577904399008,
-1.2638643523494));
#69618=CARTESIAN_POINT('Ctrl Pts',(-0.17209531239819,-0.163235247481622,
-1.26407635958309));
#69619=CARTESIAN_POINT('Ctrl Pts',(-0.178046145200246,-0.156786716397018,
-1.26464167672656));
#69620=CARTESIAN_POINT('Ctrl Pts',(-0.181650208091099,-0.152596574309805,
-1.26498984948423));
#69621=CARTESIAN_POINT('Ctrl Pts',(-0.192170894356137,-0.1394634735735,
-1.26603783972241));
#69622=CARTESIAN_POINT('Ctrl Pts',(-0.198597626473805,-0.130148810332736,
-1.26672393660317));
#69623=CARTESIAN_POINT('Ctrl Pts',(-0.211088406002638,-0.108952149726945,
-1.26823749611137));
#69624=CARTESIAN_POINT('Ctrl Pts',(-0.216864221891957,-0.0969470252752098,
-1.26906651398851));
#69625=CARTESIAN_POINT('Ctrl Pts',(-0.222456474065697,-0.0822850555721773,
-1.27008769915586));
#69626=CARTESIAN_POINT('Ctrl Pts',(-0.22327577558371,-0.0800352458470144,
-1.27024456687028));
#69627=CARTESIAN_POINT('Ctrl Pts',(-0.224508736693512,-0.0764831570705249,
-1.27049269320788));
#69628=CARTESIAN_POINT('Ctrl Pts',(-0.224945457692375,-0.0751890091612959,
-1.27058318796867));
#69629=CARTESIAN_POINT('Ctrl Pts',(-0.22573071461815,-0.0727939451664079,
-1.27075087250793));
#69630=CARTESIAN_POINT('Ctrl Pts',(-0.226082437064376,-0.0716941109488004,
-1.27082795459784));
#69631=CARTESIAN_POINT('Ctrl Pts',(-0.226845376240919,-0.0692469510009841,
-1.27099966276104));
#69632=CARTESIAN_POINT('Ctrl Pts',(-0.227252646192095,-0.0678984506049609,
-1.27109441490519));
#69633=CARTESIAN_POINT('Ctrl Pts',(-0.228395959125987,-0.0639873051448738,
-1.27136965688094));
#69634=CARTESIAN_POINT('Ctrl Pts',(-0.229100812321567,-0.0614158460565036,
-1.27155114879985));
#69635=CARTESIAN_POINT('Ctrl Pts',(-0.230599005450093,-0.0555649249063948,
-1.27196545181937));
#69636=CARTESIAN_POINT('Ctrl Pts',(-0.231366002077995,-0.0522793772816916,
-1.27219905356402));
#69637=CARTESIAN_POINT('Ctrl Pts',(-0.235476150772003,-0.0328053735575508,
-1.27358951773686));
#69638=CARTESIAN_POINT('Ctrl Pts',(-0.23718894756512,-0.0163222182344524,
-1.27479481870023));
#69639=CARTESIAN_POINT('Ctrl Pts',(-0.23717491446692,0.000201426436582323,
-1.27600110192935));
#69640=CARTESIAN_POINT('Ctrl Pts',(-0.237174914325959,0.000201592345835819,
-1.2760011140413));
#69641=CARTESIAN_POINT('Ctrl Pts',(-0.237164711325221,0.0122054996164438,
-1.27687744077041));
#69642=CARTESIAN_POINT('Ctrl Pts',(-0.236243205108348,0.0241930379328251,
-1.2777500309929));
#69643=CARTESIAN_POINT('Ctrl Pts',(-0.234237295365433,0.037232730661517,
-1.27866541082618));
#69644=CARTESIAN_POINT('Ctrl Pts',(-0.234048209895879,0.0384034159463861,
-1.27874728070692));
#69645=CARTESIAN_POINT('Ctrl Pts',(-0.233720671664886,0.0403389675235547,
-1.27888207023377));
#69646=CARTESIAN_POINT('Ctrl Pts',(-0.233587227708098,0.0411046439954152,
-1.27893524295015));
#69647=CARTESIAN_POINT('Ctrl Pts',(-0.23333984698255,0.0424839489625012,
-1.27903074546642));
#69648=CARTESIAN_POINT('Ctrl Pts',(-0.233227248121317,0.0430978058118354,
-1.27907314705763));
#69649=CARTESIAN_POINT('Ctrl Pts',(-0.23299135169158,0.044355843035674,
-1.27915982637008));
#69650=CARTESIAN_POINT('Ctrl Pts',(-0.232867806255701,0.0449999511598508,
-1.27920408612858));
#69651=CARTESIAN_POINT('Ctrl Pts',(-0.232580899645795,0.046462919709769,
-1.27930434746129));
#69652=CARTESIAN_POINT('Ctrl Pts',(-0.2324158850276,0.0472814364017038,
-1.27936025490184));
#69653=CARTESIAN_POINT('Ctrl Pts',(-0.231973877075751,0.0494156730779478,
-1.27950558048546));
#69654=CARTESIAN_POINT('Ctrl Pts',(-0.231690007676864,0.0507299609639537,
-1.27959462625443));
#69655=CARTESIAN_POINT('Ctrl Pts',(-0.229285134333641,0.0614228190819688,
-1.28031596780371));
#69656=CARTESIAN_POINT('Ctrl Pts',(-0.226606491376217,0.0706681017237945,
-1.28092019026395));
#69657=CARTESIAN_POINT('Ctrl Pts',(-0.2197396681336,0.0899072699785791,
-1.28218447014225));
#69658=CARTESIAN_POINT('Ctrl Pts',(-0.215414026783435,0.0998280690438886,
-1.28284094821804));
#69659=CARTESIAN_POINT('Ctrl Pts',(-0.205278457628415,0.119320003481633,
-1.28419575650169));
#69660=CARTESIAN_POINT('Ctrl Pts',(-0.199438498708143,0.128843898637117,
-1.28489320437353));
#69661=CARTESIAN_POINT('Ctrl Pts',(-0.191229478648633,0.140328275660303,
-1.28580649322059));
#69662=CARTESIAN_POINT('Ctrl Pts',(-0.189463721957386,0.142703311984585,
-1.2859995224078));
#69663=CARTESIAN_POINT('Ctrl Pts',(-0.186727391371704,0.146243488590924,
-1.28629398268726));
#69664=CARTESIAN_POINT('Ctrl Pts',(-0.185789282195805,0.14743343950999,
-1.28639414273404));
#69665=CARTESIAN_POINT('Ctrl Pts',(-0.184103926614648,0.149529609829552,
-1.28657274471922));
#69666=CARTESIAN_POINT('Ctrl Pts',(-0.183361222864139,0.150439429257537,
-1.28665100293165));
#69667=CARTESIAN_POINT('Ctrl Pts',(-0.181783978282007,0.152342537969004,
-1.28681628383399));
#69668=CARTESIAN_POINT('Ctrl Pts',(-0.180947986126268,0.153334568299571,
-1.28690336404868));
#69669=CARTESIAN_POINT('Ctrl Pts',(-0.178709723529789,0.155946807167504,
-1.28713516627107));
#69670=CARTESIAN_POINT('Ctrl Pts',(-0.177293590594479,0.157554924258461,
-1.28728045729717));
#69671=CARTESIAN_POINT('Ctrl Pts',(-0.170869325001078,0.164653828080447,
-1.2879337325548));
#69672=CARTESIAN_POINT('Ctrl Pts',(-0.165627045253658,0.169926073398702,
-1.2884515267302));
#69673=CARTESIAN_POINT('Ctrl Pts',(-0.1467069323037,0.18724592294889,-1.29027063376794));
#69674=CARTESIAN_POINT('Ctrl Pts',(-0.131895116773179,0.197958337777178,
-1.29161756148034));
#69675=CARTESIAN_POINT('Ctrl Pts',(-0.111488680257177,0.209401721877813,
-1.2933093239065));
#69676=CARTESIAN_POINT('Ctrl Pts',(-0.106889022700937,0.211786568850279,
-1.29368053776999));
#69677=CARTESIAN_POINT('Ctrl Pts',(-0.0994022702734951,0.215362213773916,
-1.29426501866394));
#69678=CARTESIAN_POINT('Ctrl Pts',(-0.0965634841762156,0.216649925701232,
-1.29448224201419));
#69679=CARTESIAN_POINT('Ctrl Pts',(-0.0927842382502456,0.218275191950834,
-1.29476491903108));
#69680=CARTESIAN_POINT('Ctrl Pts',(-0.0918660066237008,0.218663236975568,
-1.29483309981837));
#69681=CARTESIAN_POINT('Ctrl Pts',(-0.0902943486979534,0.219315772471328,
-1.29494891378608));
#69682=CARTESIAN_POINT('Ctrl Pts',(-0.0896421493947211,0.219583156336118,
-1.29499671515367));
#69683=CARTESIAN_POINT('Ctrl Pts',(-0.0883659215240853,0.220099741073461,
-1.2950897354139));
#69684=CARTESIAN_POINT('Ctrl Pts',(-0.0877420124376722,0.220349203261255,
-1.29513496880239));
#69685=CARTESIAN_POINT('Ctrl Pts',(-0.0863425109168294,0.220901889754347,
-1.29523591061485));
#69686=CARTESIAN_POINT('Ctrl Pts',(-0.0855663567175502,0.221203690607967,
-1.29529153497173));
#69687=CARTESIAN_POINT('Ctrl Pts',(-0.0828563669927195,0.222241048706764,
-1.29548456233221));
#69688=CARTESIAN_POINT('Ctrl Pts',(-0.0809144429371287,0.222955410160999,
-1.29562078093307));
#69689=CARTESIAN_POINT('Ctrl Pts',(-0.0674903770669402,0.227695119963206,
-1.29654967589162));
#69690=CARTESIAN_POINT('Ctrl Pts',(-0.0557211499386474,0.230857637130987,
-1.29730081186011));
#69691=CARTESIAN_POINT('Ctrl Pts',(-0.0431533968831323,0.233216949903831,
-1.29808568538759));
#69692=CARTESIAN_POINT('Ctrl Pts',(-0.0425465299387445,0.233328425353389,
-1.29812354190914));
#69693=CARTESIAN_POINT('Ctrl Pts',(-0.0419392737720405,0.233437524705164,
-1.29816138490414));
#69694=CARTESIAN_POINT('',(-0.237174952428875,-0.000150217712243535,-1.29551725116514));
#69695=CARTESIAN_POINT('Ctrl Pts',(-0.0419392741369039,0.233437524639612,
-1.31805175208418));
#69696=CARTESIAN_POINT('Ctrl Pts',(-0.042730075991894,0.233295449556202,
-1.31799864962229));
#69697=CARTESIAN_POINT('Ctrl Pts',(-0.0435201470678421,0.233149357634431,
-1.31794542141065));
#69698=CARTESIAN_POINT('Ctrl Pts',(-0.0454620452621817,0.232780066948212,
-1.31781415312616));
#69699=CARTESIAN_POINT('Ctrl Pts',(-0.0466129730601121,0.232552333433665,
-1.31773597114705));
#69700=CARTESIAN_POINT('Ctrl Pts',(-0.0490359513137738,0.232054190364414,
-1.31757055131564));
#69701=CARTESIAN_POINT('Ctrl Pts',(-0.050307558321464,0.23178183976685,
-1.31748325375812));
#69702=CARTESIAN_POINT('Ctrl Pts',(-0.0536836674373283,0.231029659408946,
-1.31725015907493));
#69703=CARTESIAN_POINT('Ctrl Pts',(-0.0557839261533372,0.230531543875296,
-1.31710378126733));
#69704=CARTESIAN_POINT('Ctrl Pts',(-0.0663492673567317,0.227872945028406,
-1.31636027600193));
#69705=CARTESIAN_POINT('Ctrl Pts',(-0.0746961947294473,0.225274831226444,
-1.31574922389491));
#69706=CARTESIAN_POINT('Ctrl Pts',(-0.0981163616342415,0.21654006267436,
-1.31396641411693));
#69707=CARTESIAN_POINT('Ctrl Pts',(-0.112727240200996,0.209305772108647,
-1.31276685571552));
#69708=CARTESIAN_POINT('Ctrl Pts',(-0.133385234861601,0.196282870298228,
-1.31099755499191));
#69709=CARTESIAN_POINT('Ctrl Pts',(-0.140060670955096,0.191576679291413,
-1.31041362154172));
#69710=CARTESIAN_POINT('Ctrl Pts',(-0.147517045988519,0.18572139828791,
-1.30975778931733));
#69711=CARTESIAN_POINT('Ctrl Pts',(-0.14854653590204,0.184899008941244,
-1.30966716026067));
#69712=CARTESIAN_POINT('Ctrl Pts',(-0.150210778352039,0.183546686736372,
-1.30952059461133));
#69713=CARTESIAN_POINT('Ctrl Pts',(-0.150849690876075,0.183021952125626,
-1.30946431322245));
#69714=CARTESIAN_POINT('Ctrl Pts',(-0.151990015547791,0.182075383043787,
-1.30936385766208));
#69715=CARTESIAN_POINT('Ctrl Pts',(-0.152492434628887,0.181654802716175,
-1.30931959728962));
#69716=CARTESIAN_POINT('Ctrl Pts',(-0.152998514021164,0.181227578977539,
-1.30927501426978));
#69717=CARTESIAN_POINT('Ctrl Pts',(-0.153003903197675,0.181223029113358,
-1.30927453951051));
#69718=CARTESIAN_POINT('Ctrl Pts',(-0.153014573372623,0.181214019900141,
-1.30927359952144));
#69719=CARTESIAN_POINT('Ctrl Pts',(-0.15301985437923,0.181209560560513,
-1.30927313429093));
#69720=CARTESIAN_POINT('Ctrl Pts',(-0.153030312063891,0.181200729194285,
-1.30927221302026));
#69721=CARTESIAN_POINT('Ctrl Pts',(-0.153035488748899,0.18119635717723,
-1.3092717569795));
#69722=CARTESIAN_POINT('Ctrl Pts',(-0.153045741461448,0.181187697401525,
-1.30927085376493));
#69723=CARTESIAN_POINT('Ctrl Pts',(-0.15305081749675,0.181183409650905,
-1.30927040659045));
#69724=CARTESIAN_POINT('Ctrl Pts',(-0.153060872419423,0.181174915486908,
-1.30926952079929));
#69725=CARTESIAN_POINT('Ctrl Pts',(-0.153065851313057,0.181170709082049,
-1.30926908218206));
#69726=CARTESIAN_POINT('Ctrl Pts',(-0.153075715302852,0.181162374820004,
-1.30926821321026));
#69727=CARTESIAN_POINT('Ctrl Pts',(-0.153080600405643,0.181158246970298,
-1.30926778285511));
#69728=CARTESIAN_POINT('Ctrl Pts',(-0.153090280018972,0.181150067149086,
-1.3092669301251));
#69729=CARTESIAN_POINT('Ctrl Pts',(-0.153095074535158,0.181146015185209,
-1.30926650774975));
#69730=CARTESIAN_POINT('Ctrl Pts',(-0.153104576037755,0.181137984584362,
-1.30926567070958));
#69731=CARTESIAN_POINT('Ctrl Pts',(-0.153109283030601,0.181134005953715,
-1.3092652560442));
#69732=CARTESIAN_POINT('Ctrl Pts',(-0.153118612420609,0.181126119574247,
-1.30926443416548));
#69733=CARTESIAN_POINT('Ctrl Pts',(-0.153123234822777,0.181122211832359,
-1.30926402695171));
#69734=CARTESIAN_POINT('Ctrl Pts',(-0.153132397836263,0.181114464892435,
-1.30926321972914));
#69735=CARTESIAN_POINT('Ctrl Pts',(-0.153136938453594,0.181110625699921,
-1.30926281971982));
#69736=CARTESIAN_POINT('Ctrl Pts',(-0.153145940587735,0.18110301361556,
-1.30926202666915));
#69737=CARTESIAN_POINT('Ctrl Pts',(-0.153150402108979,0.181099240730042,
-1.30926163362742));
#69738=CARTESIAN_POINT('Ctrl Pts',(-0.153159248626411,0.181091759111717,
-1.30926085428506));
#69739=CARTESIAN_POINT('Ctrl Pts',(-0.15316363362728,0.181088050384534,
-1.30926046798403));
#69740=CARTESIAN_POINT('Ctrl Pts',(-0.153172329572949,0.181080695023181,
-1.30925970190556));
#69741=CARTESIAN_POINT('Ctrl Pts',(-0.153176640522496,0.181077048394114,
-1.30925932212772));
#69742=CARTESIAN_POINT('Ctrl Pts',(-0.153185190733487,0.181069815253067,
-1.30925856888705));
#69743=CARTESIAN_POINT('Ctrl Pts',(-0.153189429999315,0.181066228746057,
-1.30925819542383));
#69744=CARTESIAN_POINT('Ctrl Pts',(-0.153197839118215,0.181059113949964,
-1.30925745461198));
#69745=CARTESIAN_POINT('Ctrl Pts',(-0.15320200897386,0.18105558566697,-1.30925708726312));
#69746=CARTESIAN_POINT('Ctrl Pts',(-0.153210281449584,0.181048585501309,
-1.30925635848818));
#69747=CARTESIAN_POINT('Ctrl Pts',(-0.153214384074708,0.18104511362225,
-1.30925599706166));
#69748=CARTESIAN_POINT('Ctrl Pts',(-0.153222524185682,0.181038224513905,
-1.30925527994674));
#69749=CARTESIAN_POINT('Ctrl Pts',(-0.153226561675178,0.181034807289045,
-1.30925492425802));
#69750=CARTESIAN_POINT('Ctrl Pts',(-0.153234573525726,0.181028025809549,
-1.30925421844157));
#69751=CARTESIAN_POINT('Ctrl Pts',(-0.153238547890653,0.1810246615588,-1.3092538683135));
#69752=CARTESIAN_POINT('Ctrl Pts',(-0.153246435430799,0.181017984407744,
-1.30925317344755));
#69753=CARTESIAN_POINT('Ctrl Pts',(-0.153250348607233,0.18101467151325,
-1.30925282870958));
#69754=CARTESIAN_POINT('Ctrl Pts',(-0.153258115622694,0.181008095526915,
-1.30925214446066));
#69755=CARTESIAN_POINT('Ctrl Pts',(-0.153261969467306,0.181004832436878,
-1.30925180494923));
#69756=CARTESIAN_POINT('Ctrl Pts',(-0.153269619612282,0.180998354560623,
-1.30925113099543));
#69757=CARTESIAN_POINT('Ctrl Pts',(-0.153273415914893,0.180995139778744,
-1.30925079655287));
#69758=CARTESIAN_POINT('Ctrl Pts',(-0.153280952694623,0.180988757081913,
-1.30925013258541));
#69759=CARTESIAN_POINT('Ctrl Pts',(-0.153284693175082,0.180985589170099,
-1.30924980306023));
#69760=CARTESIAN_POINT('Ctrl Pts',(-0.153292119970424,0.180979298825339,
-1.30924914878129));
#69761=CARTESIAN_POINT('Ctrl Pts',(-0.153295806286824,0.180976176396815,
-1.30924882402742));
#69762=CARTESIAN_POINT('Ctrl Pts',(-0.153303126344122,0.180969975688781,
-1.30924817915103));
#69763=CARTESIAN_POINT('Ctrl Pts',(-0.153306760089473,0.180966897410959,
-1.30924785902814));
#69764=CARTESIAN_POINT('Ctrl Pts',(-0.15331397654739,0.180960783713698,
-1.30924722327781));
#69765=CARTESIAN_POINT('Ctrl Pts',(-0.153317559260781,0.180957748298785,
-1.30924690765032));
#69766=CARTESIAN_POINT('Ctrl Pts',(-0.153324675130603,0.180951719092528,
-1.3092462807608));
#69767=CARTESIAN_POINT('Ctrl Pts',(-0.153328208291232,0.18094872530263,
-1.3092459694984));
#69768=CARTESIAN_POINT('Ctrl Pts',(-0.153335226485888,0.180942778149307,
-1.30924535121307));
#69769=CARTESIAN_POINT('Ctrl Pts',(-0.153338711522067,0.180939824788851,
-1.30924504418995));
#69770=CARTESIAN_POINT('Ctrl Pts',(-0.15334563484607,0.180933957340709,
-1.30924443426177));
#69771=CARTESIAN_POINT('Ctrl Pts',(-0.153349073135526,0.180931043256233,
-1.30924413135656));
#69772=CARTESIAN_POINT('Ctrl Pts',(-0.153974111205272,0.180401268487822,
-1.30918906694146));
#69773=CARTESIAN_POINT('Ctrl Pts',(-0.154593003363402,0.179871198233511,
-1.30913453806626));
#69774=CARTESIAN_POINT('Ctrl Pts',(-0.156513418482666,0.17820916272353,
-1.30896527184002));
#69775=CARTESIAN_POINT('Ctrl Pts',(-0.157805368327269,0.177066151470791,
-1.30885130671589));
#69776=CARTESIAN_POINT('Ctrl Pts',(-0.160840949646248,0.174320899717232,
-1.30858298542288));
#69777=CARTESIAN_POINT('Ctrl Pts',(-0.162573311824768,0.17270641671578,
-1.30842941912404));
#69778=CARTESIAN_POINT('Ctrl Pts',(-0.168715494165297,0.166807848914186,
-1.30788206772881));
#69779=CARTESIAN_POINT('Ctrl Pts',(-0.172982790538499,0.16237838941339,
-1.30749630022158));
#69780=CARTESIAN_POINT('Ctrl Pts',(-0.190532264389932,0.142683933354184,
-1.3058597150181));
#69781=CARTESIAN_POINT('Ctrl Pts',(-0.202002789868823,0.125921094758135,
-1.30465033655044));
#69782=CARTESIAN_POINT('Ctrl Pts',(-0.213333168216489,0.103743831041836,
-1.30306022406101));
#69783=CARTESIAN_POINT('Ctrl Pts',(-0.215335873966919,0.0995202482763043,
-1.30275823840336));
#69784=CARTESIAN_POINT('Ctrl Pts',(-0.217936690649239,0.093588635341723,
-1.3023337883921));
#69785=CARTESIAN_POINT('Ctrl Pts',(-0.218642086521764,0.0919286217612416,
-1.30221497010903));
#69786=CARTESIAN_POINT('Ctrl Pts',(-0.219747912898177,0.0892415272025777,
-1.30202250882702));
#69787=CARTESIAN_POINT('Ctrl Pts',(-0.220160244942868,0.0882193962646792,
-1.30194927005371));
#69788=CARTESIAN_POINT('Ctrl Pts',(-0.221002999172407,0.0860875809313934,
-1.30179643888395));
#69789=CARTESIAN_POINT('Ctrl Pts',(-0.221432221402953,0.0849774585940837,
-1.30171680868392));
#69790=CARTESIAN_POINT('Ctrl Pts',(-0.222426897684242,0.0823461563325304,
-1.30152793309061));
#69791=CARTESIAN_POINT('Ctrl Pts',(-0.222985123949682,0.0808223270210209,
-1.30141845032215));
#69792=CARTESIAN_POINT('Ctrl Pts',(-0.224806734250036,0.0756871866577657,
-1.30104909428505));
#69793=CARTESIAN_POINT('Ctrl Pts',(-0.225998309472044,0.072051225791986,
-1.30078688038987));
#69794=CARTESIAN_POINT('Ctrl Pts',(-0.23112078003655,0.0550406911746145,
-1.29955625758056));
#69795=CARTESIAN_POINT('Ctrl Pts',(-0.233955043153285,0.0413668760454999,
-1.29855372346693));
#69796=CARTESIAN_POINT('Ctrl Pts',(-0.236645699533647,0.0183393274071569,
-1.29686353817375));
#69797=CARTESIAN_POINT('Ctrl Pts',(-0.237180810115524,0.00909833581418968,
-1.29618544677203));
#69798=CARTESIAN_POINT('Ctrl Pts',(-0.237174952428875,-0.000150217712243535,
-1.29551725116514));
#69799=CARTESIAN_POINT('Ctrl Pts',(-0.237174952219374,-0.000150548123425626,
-1.29551722729338));
#69800=CARTESIAN_POINT('Ctrl Pts',(-0.237171634097938,-0.00537794834055943,
-1.29513955477401));
#69801=CARTESIAN_POINT('Ctrl Pts',(-0.236995496033019,-0.0106042469816567,
-1.29476539307927));
#69802=CARTESIAN_POINT('Ctrl Pts',(-0.236475414555163,-0.018383575706604,
-1.29421726023887));
#69803=CARTESIAN_POINT('Ctrl Pts',(-0.236262459004787,-0.0209434790540369,
-1.29403832264722));
#69804=CARTESIAN_POINT('Ctrl Pts',(-0.235921164725,-0.0243711274954405,
-1.29380108654061));
#69805=CARTESIAN_POINT('Ctrl Pts',(-0.235829550734013,-0.025242243960233,
-1.29374099920503));
#69806=CARTESIAN_POINT('Ctrl Pts',(-0.235660972814824,-0.0267640770103183,
-1.29363640837812));
#69807=CARTESIAN_POINT('Ctrl Pts',(-0.2355861350564,-0.0274150127010362,
-1.29359179371062));
#69808=CARTESIAN_POINT('Ctrl Pts',(-0.235433595423304,-0.0286950261190728,
-1.29350431381029));
#69809=CARTESIAN_POINT('Ctrl Pts',(-0.235356067352883,-0.0293241193842705,
-1.29346143984812));
#69810=CARTESIAN_POINT('Ctrl Pts',(-0.235183068228193,-0.0306830036354225,
-1.2933690960295));
#69811=CARTESIAN_POINT('Ctrl Pts',(-0.235086721484119,-0.0314126680249628,
-1.29331967554479));
#69812=CARTESIAN_POINT('Ctrl Pts',(-0.234816635056893,-0.0333872502279775,
-1.29318635247581));
#69813=CARTESIAN_POINT('Ctrl Pts',(-0.23463638991153,-0.0346312760248702,
-1.29310280491599));
#69814=CARTESIAN_POINT('Ctrl Pts',(-0.233738782597306,-0.0404974072691783,
-1.29271070994837));
#69815=CARTESIAN_POINT('Ctrl Pts',(-0.232894630751464,-0.0450994062680839,
-1.29240859214907));
#69816=CARTESIAN_POINT('Ctrl Pts',(-0.230619787514339,-0.0557200987495107,
-1.29171782944799));
#69817=CARTESIAN_POINT('Ctrl Pts',(-0.229088689447391,-0.0617138335465195,
-1.2913328760493));
#69818=CARTESIAN_POINT('Ctrl Pts',(-0.222727433056254,-0.0830924110380073,
-1.28995607619125));
#69819=CARTESIAN_POINT('Ctrl Pts',(-0.216566812966617,-0.0980339839073789,
-1.28898367988846));
#69820=CARTESIAN_POINT('Ctrl Pts',(-0.20570165626276,-0.118260699163556,
-1.28753621870337));
#69821=CARTESIAN_POINT('Ctrl Pts',(-0.202206053653733,-0.124142911784749,
-1.28709834196644));
#69822=CARTESIAN_POINT('Ctrl Pts',(-0.197364389524526,-0.131541980008034,
-1.28652028957603));
#69823=CARTESIAN_POINT('Ctrl Pts',(-0.196246183779255,-0.133204465774659,
-1.28638855865525));
#69824=CARTESIAN_POINT('Ctrl Pts',(-0.194386793057418,-0.135894665593498,
-1.2861722417754));
#69825=CARTESIAN_POINT('Ctrl Pts',(-0.193658182465301,-0.136930981557038,
-1.28608813367788));
#69826=CARTESIAN_POINT('Ctrl Pts',(-0.192232963770691,-0.138923967124943,
-1.28592483948853));
#69827=CARTESIAN_POINT('Ctrl Pts',(-0.191537427492375,-0.139881359672107,
-1.28584569629284));
#69828=CARTESIAN_POINT('Ctrl Pts',(-0.189912248950479,-0.142083538730366,
-1.28566200207196));
#69829=CARTESIAN_POINT('Ctrl Pts',(-0.188977490960681,-0.1433244640304,
-1.28555725374669));
#69830=CARTESIAN_POINT('Ctrl Pts',(-0.185886145086666,-0.147345517049598,
-1.28521370262834));
#69831=CARTESIAN_POINT('Ctrl Pts',(-0.183679962746033,-0.150086739263715,
-1.28497295477629));
#69832=CARTESIAN_POINT('Ctrl Pts',(-0.168912809352094,-0.167621781113879,
-1.28338873371208));
#69833=CARTESIAN_POINT('Ctrl Pts',(-0.154639268560768,-0.18087292746228,
-1.28197236788306));
#69834=CARTESIAN_POINT('Ctrl Pts',(-0.13745828529144,-0.193288471559709,
-1.28042601100721));
#69835=CARTESIAN_POINT('Ctrl Pts',(-0.135989027908764,-0.194324979914469,
-1.28029497955843));
#69836=CARTESIAN_POINT('Ctrl Pts',(-0.129023477869157,-0.199121235296442,
-1.27967979088504));
#69837=CARTESIAN_POINT('Ctrl Pts',(-0.123381836011182,-0.202665385995047,
-1.27919884255916));
#69838=CARTESIAN_POINT('Ctrl Pts',(-0.115433704140734,-0.20720340892685,
-1.27855105574359));
#69839=CARTESIAN_POINT('Ctrl Pts',(-0.113249803560968,-0.208405076251547,
-1.2783760361788));
#69840=CARTESIAN_POINT('Ctrl Pts',(-0.109915405330685,-0.21017189422047,
-1.27811371159392));
#69841=CARTESIAN_POINT('Ctrl Pts',(-0.108778667310689,-0.210762480438063,
-1.27802512910914));
#69842=CARTESIAN_POINT('Ctrl Pts',(-0.106683914014119,-0.211829335827046,
-1.27786351424136));
#69843=CARTESIAN_POINT('Ctrl Pts',(-0.105727360575849,-0.212308385047584,
-1.27779032816967));
#69844=CARTESIAN_POINT('Ctrl Pts',(-0.104148176050817,-0.213085932704761,
-1.27767055123375));
#69845=CARTESIAN_POINT('Ctrl Pts',(-0.1035274373105,-0.213388207374404,
-1.27762373393007));
#69846=CARTESIAN_POINT('Ctrl Pts',(-0.102300169901742,-0.213979221144839,
-1.27753170390752));
#69847=CARTESIAN_POINT('Ctrl Pts',(-0.101693721967763,-0.214268100222872,
-1.27748648379952));
#69848=CARTESIAN_POINT('Ctrl Pts',(-0.100332867286164,-0.214909258926846,
-1.27738556559921));
#69849=CARTESIAN_POINT('Ctrl Pts',(-0.0995778086216152,-0.215260154028732,
-1.2773299515766));
#69850=CARTESIAN_POINT('Ctrl Pts',(-0.09694003186964,-0.216469147219884,
-1.27713693117663));
#69851=CARTESIAN_POINT('Ctrl Pts',(-0.0950478812284026,-0.217306609345889,
-1.27700070935946));
#69852=CARTESIAN_POINT('Ctrl Pts',(-0.0820238171277684,-0.222868363670622,
-1.27607666430147));
#69853=CARTESIAN_POINT('Ctrl Pts',(-0.0705542621662209,-0.22676063497048,
-1.27532986130998));
#69854=CARTESIAN_POINT('Ctrl Pts',(-0.0484440247797162,-0.232422554556084,
-1.273928823142));
#69855=CARTESIAN_POINT('Ctrl Pts',(-0.0378830685748147,-0.234375620482233,
-1.27327520930931));
#69856=CARTESIAN_POINT('Ctrl Pts',(-0.0180321672712933,-0.236669574006756,
-1.27203002205858));
#69857=CARTESIAN_POINT('Ctrl Pts',(-0.00878445716549035,-0.237192852391894,
-1.27144342271638));
#69858=CARTESIAN_POINT('Ctrl Pts',(0.00266243741233339,-0.237170194644882,
-1.27069670591225));
#69859=CARTESIAN_POINT('Ctrl Pts',(0.00485518784719147,-0.237135438983914,
-1.27055275456942));
#69860=CARTESIAN_POINT('Ctrl Pts',(0.0083544466254571,-0.237031421036525,
-1.27032143403947));
#69861=CARTESIAN_POINT('Ctrl Pts',(0.0096614444347577,-0.236981745525032,
-1.27023467817484));
#69862=CARTESIAN_POINT('Ctrl Pts',(0.0121383832377233,-0.236867079064401,
-1.27006955854794));
#69863=CARTESIAN_POINT('Ctrl Pts',(0.0133083877502891,-0.236804223405379,
-1.2699912640744));
#69864=CARTESIAN_POINT('Ctrl Pts',(0.0159695621484252,-0.236641473976454,
-1.26981248080178));
#69865=CARTESIAN_POINT('Ctrl Pts',(0.0174603375210886,-0.236536150633577,
-1.26971182471406));
#69866=CARTESIAN_POINT('Ctrl Pts',(0.022041762181863,-0.236168926455461,
-1.26940089093279));
#69867=CARTESIAN_POINT('Ctrl Pts',(0.0251282419003797,-0.235860490488281,
-1.26918917014795));
#69868=CARTESIAN_POINT('Ctrl Pts',(0.0460643524293472,-0.233352720933325,
-1.26773707333084));
#69869=CARTESIAN_POINT('Ctrl Pts',(0.063616607020624,-0.229190111206138,
-1.26643391523741));
#69870=CARTESIAN_POINT('Ctrl Pts',(0.0843219399406033,-0.221716201527491,
-1.2648261583496));
#69871=CARTESIAN_POINT('Ctrl Pts',(0.0880819126316785,-0.220249497086493,
-1.26453151117589));
#69872=CARTESIAN_POINT('Ctrl Pts',(0.0978193820114174,-0.216161812915336,
-1.26376362443696));
#69873=CARTESIAN_POINT('Ctrl Pts',(0.103729718730266,-0.213388654317691,
-1.26329263026846));
#69874=CARTESIAN_POINT('Ctrl Pts',(0.112762165808324,-0.208686480800197,
-1.26257216424315));
#69875=CARTESIAN_POINT('Ctrl Pts',(0.115966559720571,-0.206922966262217,
-1.2623164495848));
#69876=CARTESIAN_POINT('Ctrl Pts',(0.120091978619876,-0.204526617525639,
-1.26198828144166));
#69877=CARTESIAN_POINT('Ctrl Pts',(0.121050936636414,-0.203960514482649,
-1.26191207415715));
#69878=CARTESIAN_POINT('Ctrl Pts',(0.122609901682587,-0.203025340134603,
-1.26178835347969));
#69879=CARTESIAN_POINT('Ctrl Pts',(0.123212300933918,-0.20266032087964,
-1.26174058807389));
#69880=CARTESIAN_POINT('Ctrl Pts',(0.124386129497664,-0.201941879811416,
-1.26164760774918));
#69881=CARTESIAN_POINT('Ctrl Pts',(0.124957695741152,-0.201588705848002,
-1.26160237854773));
#69882=CARTESIAN_POINT('Ctrl Pts',(0.126234628231357,-0.2007921645663,-1.26150141617112));
#69883=CARTESIAN_POINT('Ctrl Pts',(0.126939181884179,-0.200347495294068,
-1.26144576730652));
#69884=CARTESIAN_POINT('Ctrl Pts',(0.129387855789633,-0.198783945879309,
-1.2612525072822));
#69885=CARTESIAN_POINT('Ctrl Pts',(0.131119704425123,-0.197645890911342,
-1.26111608454046));
#69886=CARTESIAN_POINT('Ctrl Pts',(0.142889682698122,-0.189688638844779,
-1.26018910740534));
#69887=CARTESIAN_POINT('Ctrl Pts',(0.152407791396253,-0.18212957541118,
-1.25943985144953));
#69888=CARTESIAN_POINT('Ctrl Pts',(0.169227325834228,-0.166525773452984,
-1.25803158513234));
#69889=CARTESIAN_POINT('Ctrl Pts',(0.176636746286817,-0.15864479611635,
-1.25737326660319));
#69890=CARTESIAN_POINT('Ctrl Pts',(0.189277757269659,-0.143211545128199,
-1.25612959322725));
#69891=CARTESIAN_POINT('Ctrl Pts',(0.194657998254533,-0.135808137752186,
-1.25554972705993));
#69892=CARTESIAN_POINT('Ctrl Pts',(0.200777796390083,-0.126273652379607,
-1.25481061043636));
#69893=CARTESIAN_POINT('Ctrl Pts',(0.201933020777368,-0.124417898244251,
-1.25466711528058));
#69894=CARTESIAN_POINT('Ctrl Pts',(0.203737408712755,-0.121427985283587,
-1.25443635532781));
#69895=CARTESIAN_POINT('Ctrl Pts',(0.2044031534096,-0.120303940414581,-1.25434969855404));
#69896=CARTESIAN_POINT('Ctrl Pts',(0.205648464610499,-0.118161174672097,
-1.25418465658479));
#69897=CARTESIAN_POINT('Ctrl Pts',(0.206229834282845,-0.117143542558504,
-1.25410633974369));
#69898=CARTESIAN_POINT('Ctrl Pts',(0.207536655641705,-0.114816195516537,
-1.25392735013452));
#69899=CARTESIAN_POINT('Ctrl Pts',(0.208257289599811,-0.113503847235874,
-1.25382650862904));
#69900=CARTESIAN_POINT('Ctrl Pts',(0.210439272130048,-0.109439491171847,
-1.25351441662176));
#69901=CARTESIAN_POINT('Ctrl Pts',(0.211858800665463,-0.106665535448604,
-1.25330170739145));
#69902=CARTESIAN_POINT('Ctrl Pts',(0.221009786292477,-0.0878795019611069,
-1.25186248216073));
#69903=CARTESIAN_POINT('Ctrl Pts',(0.226972714652791,-0.071072425063611,
-1.25057478603627));
#69904=CARTESIAN_POINT('Ctrl Pts',(0.23196578719813,-0.0496180113711474,
-1.2489659391383));
#69905=CARTESIAN_POINT('Ctrl Pts',(0.23281833876877,-0.0454499222168456,
-1.24865529365496));
#69906=CARTESIAN_POINT('Ctrl Pts',(0.234689074717624,-0.0348606316198101,
-1.24787346617379));
#69907=CARTESIAN_POINT('Ctrl Pts',(0.235556304334753,-0.0284159164161385,
-1.24740438800428));
#69908=CARTESIAN_POINT('Ctrl Pts',(0.236495178386044,-0.0183115955785285,
-1.24668646901585));
#69909=CARTESIAN_POINT('Ctrl Pts',(0.23674883461385,-0.0146723157346005,
-1.24643143326267));
#69910=CARTESIAN_POINT('Ctrl Pts',(0.236970187826219,-0.00991707694313436,
-1.24610399498103));
#69911=CARTESIAN_POINT('Ctrl Pts',(0.23701410034066,-0.0088053788183978,
-1.2460278586963));
#69912=CARTESIAN_POINT('Ctrl Pts',(0.237073029712417,-0.00698963480971464,
-1.24590422403685));
#69913=CARTESIAN_POINT('Ctrl Pts',(0.237092736053673,-0.00628577405220784,
-1.24585647429257));
#69914=CARTESIAN_POINT('Ctrl Pts',(0.237125123592204,-0.00490998964807286,
-1.2457634996832));
#69915=CARTESIAN_POINT('Ctrl Pts',(0.237138084012521,-0.00423808508776454,
-1.2457182607038));
#69916=CARTESIAN_POINT('Ctrl Pts',(0.237160723874961,-0.00273252965416426,
-1.24561725088874));
#69917=CARTESIAN_POINT('Ctrl Pts',(0.23716886402977,-0.00189885603442453,
-1.2455615646223));
#69918=CARTESIAN_POINT('Ctrl Pts',(0.237181929114934,0.0010103171958684,
-1.24536804708988));
#69919=CARTESIAN_POINT('Ctrl Pts',(0.237164006983026,0.0030858956645106,
-1.24523140839519));
#69920=CARTESIAN_POINT('Ctrl Pts',(0.236855975696026,0.0172380391428393,
-1.24430785743533));
#69921=CARTESIAN_POINT('Ctrl Pts',(0.235670793260351,0.029278926256905,
-1.24356183886617));
#69922=CARTESIAN_POINT('Ctrl Pts',(0.231711387432897,0.0517375644353026,
-1.24216194126137));
#69923=CARTESIAN_POINT('Ctrl Pts',(0.229135961708477,0.0621582230070684,
-1.24150868345963));
#69924=CARTESIAN_POINT('Ctrl Pts',(0.223037868932548,0.0811905635582971,
-1.24026338897375));
#69925=CARTESIAN_POINT('Ctrl Pts',(0.219697109667137,0.0898384556896925,
-1.23967628809932));
#69926=CARTESIAN_POINT('Ctrl Pts',(0.214950711467635,0.100264568671081,
-1.23892900526597));
#69927=CARTESIAN_POINT('Ctrl Pts',(0.214014255955503,0.102248177533602,
-1.23878502026979));
#69928=CARTESIAN_POINT('Ctrl Pts',(0.212475667693255,0.105393464085221,
-1.23855365838525));
#69929=CARTESIAN_POINT('Ctrl Pts',(0.211891186815793,0.106563673299053,
-1.23846689521107));
#69930=CARTESIAN_POINT('Ctrl Pts',(0.210764872071161,0.108772800560645,
-1.23830176983211));
#69931=CARTESIAN_POINT('Ctrl Pts',(0.210224959086611,0.10981265834605,-1.23822347698485));
#69932=CARTESIAN_POINT('Ctrl Pts',(0.2089789850388,0.112169502729805,-1.23804470881742));
#69933=CARTESIAN_POINT('Ctrl Pts',(0.208268143699632,0.113483891686965,
-1.23794406631471));
#69934=CARTESIAN_POINT('Ctrl Pts',(0.206044245486363,0.117504738436927,
-1.23763321728866));
#69935=CARTESIAN_POINT('Ctrl Pts',(0.204490550029108,0.12018821911787,-1.23742156881495));
#69936=CARTESIAN_POINT('Ctrl Pts',(0.193562812987793,0.138236613078181,
-1.23596858660539));
#69937=CARTESIAN_POINT('Ctrl Pts',(0.182520295047895,0.152518942990879,
-1.23466435896758));
#69938=CARTESIAN_POINT('Ctrl Pts',(0.16716816342122,0.168294240120174,-1.2330566403756));
#69939=CARTESIAN_POINT('Ctrl Pts',(0.164291207948998,0.171103903604674,
-1.23276306133683));
#69940=CARTESIAN_POINT('Ctrl Pts',(0.156560298139525,0.178279144287022,
-1.23199612319711));
#69941=CARTESIAN_POINT('Ctrl Pts',(0.151594827651014,0.182520135753204,
-1.2315250185454));
#69942=CARTESIAN_POINT('Ctrl Pts',(0.143583662718532,0.188809663702404,
-1.23080440570332));
#69943=CARTESIAN_POINT('Ctrl Pts',(0.140654847328787,0.191001504876608,
-1.23054865194719));
#69944=CARTESIAN_POINT('Ctrl Pts',(0.136769538780253,0.19377129301799,-1.23022044177899));
#69945=CARTESIAN_POINT('Ctrl Pts',(0.135858199523805,0.194411343499961,
-1.23014423041142));
#69946=CARTESIAN_POINT('Ctrl Pts',(0.134363122329689,0.195445716513194,
-1.23002050478715));
#69947=CARTESIAN_POINT('Ctrl Pts',(0.133782089102471,0.195843890417862,
-1.22997273848062));
#69948=CARTESIAN_POINT('Ctrl Pts',(0.132643381187188,0.19661679849068,-1.22987975782549));
#69949=CARTESIAN_POINT('Ctrl Pts',(0.13208587589669,0.196991759795486,-1.22983452918468));
#69950=CARTESIAN_POINT('Ctrl Pts',(0.130833527225999,0.197826345098317,
-1.22973356953006));
#69951=CARTESIAN_POINT('Ctrl Pts',(0.130137833216007,0.198284691994349,
-1.22967792281197));
#69952=CARTESIAN_POINT('Ctrl Pts',(0.127703553831087,0.199870147618594,
-1.22948467755738));
#69953=CARTESIAN_POINT('Ctrl Pts',(0.125952566342138,0.200978171250738,
-1.22934826720088));
#69954=CARTESIAN_POINT('Ctrl Pts',(0.113845466299531,0.208419146874247,
-1.22842105879279));
#69955=CARTESIAN_POINT('Ctrl Pts',(0.103029617362843,0.213972673431457,
-1.22767158618039));
#69956=CARTESIAN_POINT('Ctrl Pts',(0.0815401133080914,0.222997451456266,
-1.22624093729439));
#69957=CARTESIAN_POINT('Ctrl Pts',(0.0709533259188437,0.226588322450777,
-1.22556077352529));
#69958=CARTESIAN_POINT('Ctrl Pts',(0.051619799452518,0.231657509786112,
-1.2243130137973));
#69959=CARTESIAN_POINT('Ctrl Pts',(0.04296910465984,0.233416868901416,-1.22375291593235));
#69960=CARTESIAN_POINT('Ctrl Pts',(0.0320994835168327,0.235002741120943,
-1.22303612638464));
#69961=CARTESIAN_POINT('Ctrl Pts',(0.029953659643311,0.235285874927931,
-1.22289401866229));
#69962=CARTESIAN_POINT('Ctrl Pts',(0.0265115650955223,0.235692197664414,
-1.22266496356337));
#69963=CARTESIAN_POINT('Ctrl Pts',(0.0252175998501376,0.235834152884497,
-1.22257860821001));
#69964=CARTESIAN_POINT('Ctrl Pts',(0.0227555712173413,0.236083757272413,
-1.22241379870537));
#69965=CARTESIAN_POINT('Ctrl Pts',(0.0215877461187253,0.236193407193166,
-1.22233541004592));
#69966=CARTESIAN_POINT('Ctrl Pts',(0.018919161480489,0.236424010608196,
-1.22215577434696));
#69967=CARTESIAN_POINT('Ctrl Pts',(0.0174179800874936,0.236539343980611,
-1.22205435404391));
#69968=CARTESIAN_POINT('Ctrl Pts',(0.0127624308503408,0.236852464425862,
-1.22173862924454));
#69969=CARTESIAN_POINT('Ctrl Pts',(0.00960524562776476,0.237001491813655,
-1.22152281641792));
#69970=CARTESIAN_POINT('Ctrl Pts',(-0.00976928912817915,0.237528264782934,
-1.22018739965351));
#69971=CARTESIAN_POINT('Ctrl Pts',(-0.0259825454949993,0.236304302883026,
-1.21901805622511));
#69972=CARTESIAN_POINT('Ctrl Pts',(-0.0419392741364228,0.233437524639699,
-1.21783461098805));
#69973=CARTESIAN_POINT('Origin',(0.,0.,-2.1456589891905));
#69974=CARTESIAN_POINT('',(-0.0419392646935193,0.233437526336206,-1.0979250019446));
#69975=CARTESIAN_POINT('',(-0.0419392769977373,0.233437524125636,-1.11762795217595));
#69976=CARTESIAN_POINT('',(-0.0419392741328076,0.233437524640348,-2.1456589891905));
#69977=CARTESIAN_POINT('Ctrl Pts',(-0.0419392646935193,0.233437526336206,
-1.0979250019446));
#69978=CARTESIAN_POINT('Ctrl Pts',(-0.0367798115508998,0.234364471007092,
-1.09829310188845));
#69979=CARTESIAN_POINT('Ctrl Pts',(-0.031590035201231,0.23512029192747,
-1.09866598315669));
#69980=CARTESIAN_POINT('Ctrl Pts',(-0.0133490694662614,0.237161701207052,
-1.09998416170587));
#69981=CARTESIAN_POINT('Ctrl Pts',(-0.000221727773968937,0.237536913602359,
-1.1009477883589));
#69982=CARTESIAN_POINT('Ctrl Pts',(0.0193563500274205,0.236473110189919,
-1.10237332585635));
#69983=CARTESIAN_POINT('Ctrl Pts',(0.0258276626338947,0.235854072157193,
-1.10284226038659));
#69984=CARTESIAN_POINT('Ctrl Pts',(0.0358787685837513,0.234473867315965,
-1.10356000704841));
#69985=CARTESIAN_POINT('Ctrl Pts',(0.0394800893702072,0.23389443481767,
-1.10381500967153));
#69986=CARTESIAN_POINT('Ctrl Pts',(0.0441610573851744,0.233030083373694,
-1.10414242886719));
#69987=CARTESIAN_POINT('Ctrl Pts',(0.0452538604207088,0.232820331987028,
-1.1042185779424));
#69988=CARTESIAN_POINT('Ctrl Pts',(0.0470359159133121,0.232465264728848,
-1.10434223876748));
#69989=CARTESIAN_POINT('Ctrl Pts',(0.0477260532844254,0.2323245586722,-1.10439000193132));
#69990=CARTESIAN_POINT('Ctrl Pts',(0.0490737017725887,0.232043539874739,
-1.10448300818268));
#69991=CARTESIAN_POINT('Ctrl Pts',(0.0497312576145336,0.231903502855761,
-1.10452826535584));
#69992=CARTESIAN_POINT('Ctrl Pts',(0.0512033081783561,0.231583457172682,
-1.10462932263763));
#69993=CARTESIAN_POINT('Ctrl Pts',(0.052017474941726,0.231401941991485,
-1.10468503804935));
#69994=CARTESIAN_POINT('Ctrl Pts',(0.0548556102051486,0.230753455134415,
-1.10487869201424));
#69995=CARTESIAN_POINT('Ctrl Pts',(0.0568744577165943,0.230264178302399,
-1.10501543606347));
#69996=CARTESIAN_POINT('Ctrl Pts',(0.0705690603839299,0.226754121710169,
-1.10593777814762));
#69997=CARTESIAN_POINT('Ctrl Pts',(0.0820076009509888,0.222872726372553,
-1.10668263029302));
#69998=CARTESIAN_POINT('Ctrl Pts',(0.102936149509307,0.213940290431936,
-1.10807949606692));
#69999=CARTESIAN_POINT('Ctrl Pts',(0.11247468719825,0.209083080794677,-1.10873091381997));
#70000=CARTESIAN_POINT('Ctrl Pts',(0.129640777566244,0.198826156133788,
-1.10997670938076));
#70001=CARTESIAN_POINT('Ctrl Pts',(0.137340197346523,0.193587734490092,
-1.11056634640951));
#70002=CARTESIAN_POINT('Ctrl Pts',(0.146451822214929,0.186570816349023,
-1.1113165218975));
#70003=CARTESIAN_POINT('Ctrl Pts',(0.148173422293269,0.185206485136998,
-1.11146070741456));
#70004=CARTESIAN_POINT('Ctrl Pts',(0.150890307651567,0.182991281763887,
-1.11169233453881));
#70005=CARTESIAN_POINT('Ctrl Pts',(0.151897954224711,0.182155717808926,
-1.11177916024021));
#70006=CARTESIAN_POINT('Ctrl Pts',(0.153794553928681,0.180556332893498,
-1.11194436846431));
#70007=CARTESIAN_POINT('Ctrl Pts',(0.15468486571532,0.179794177880297,-1.11202268127352));
#70008=CARTESIAN_POINT('Ctrl Pts',(0.156697138930992,0.178045553509669,
-1.11220144501785));
#70009=CARTESIAN_POINT('Ctrl Pts',(0.157815492417706,0.177055027177479,
-1.11230206278249));
#70010=CARTESIAN_POINT('Ctrl Pts',(0.161223420302418,0.173978682412576,
-1.11261265044438));
#70011=CARTESIAN_POINT('Ctrl Pts',(0.163481476618586,0.171858600042796,
-1.1128240583128));
#70012=CARTESIAN_POINT('Ctrl Pts',(0.178610843598396,0.157085654089708,
-1.11428022246442));
#70013=CARTESIAN_POINT('Ctrl Pts',(0.190040553507443,0.143045743158656,
-1.11558827187724));
#70014=CARTESIAN_POINT('Ctrl Pts',(0.201906429152834,0.124505177128304,
-1.1171959901742));
#70015=CARTESIAN_POINT('Ctrl Pts',(0.203962424799734,0.121107700972162,
-1.11748589388616));
#70016=CARTESIAN_POINT('Ctrl Pts',(0.20917166458411,0.111990341899366,-1.11824942549489));
#70017=CARTESIAN_POINT('Ctrl Pts',(0.212175837015832,0.106188735867266,
-1.11872076896283));
#70018=CARTESIAN_POINT('Ctrl Pts',(0.216483745098903,0.0969544007845552,
-1.11944171790206));
#70019=CARTESIAN_POINT('Ctrl Pts',(0.217953760856338,0.0936030421037136,
-1.11969757404781));
#70020=CARTESIAN_POINT('Ctrl Pts',(0.219769482891282,0.0891885418279303,
-1.12002591083231));
#70021=CARTESIAN_POINT('Ctrl Pts',(0.220185980272891,0.0881552937625912,
-1.12010214917583));
#70022=CARTESIAN_POINT('Ctrl Pts',(0.220854006462542,0.0864637780669202,
-1.12022591815117));
#70023=CARTESIAN_POINT('Ctrl Pts',(0.221109903353052,0.085807271023417,
-1.12027370100594));
#70024=CARTESIAN_POINT('Ctrl Pts',(0.221604170550213,0.0845223280651768,
-1.12036671443582));
#70025=CARTESIAN_POINT('Ctrl Pts',(0.221842800630041,0.0838940055824742,
-1.12041195930821));
#70026=CARTESIAN_POINT('Ctrl Pts',(0.222371345300429,0.0824843015167374,
-1.12051295692071));
#70027=CARTESIAN_POINT('Ctrl Pts',(0.222659821661279,0.0817023810996366,
-1.1205686252894));
#70028=CARTESIAN_POINT('Ctrl Pts',(0.22365140598166,0.0789704132263401,
-1.12076195530891));
#70029=CARTESIAN_POINT('Ctrl Pts',(0.224333090305032,0.0770126150389728,
-1.12089842768379));
#70030=CARTESIAN_POINT('Ctrl Pts',(0.228825646436232,0.0635438726050909,
-1.12182479702267));
#70031=CARTESIAN_POINT('Ctrl Pts',(0.231775069070963,0.0517628573007589,
-1.12257346983025));
#70032=CARTESIAN_POINT('Ctrl Pts',(0.235621768978044,0.0291686353468052,
-1.12398030776406));
#70033=CARTESIAN_POINT('Ctrl Pts',(0.236704743517519,0.0184196155076348,
-1.12463779243811));
#70034=CARTESIAN_POINT('Ctrl Pts',(0.237347089273772,-0.0015250323724891,
-1.12588170695414));
#70035=CARTESIAN_POINT('Ctrl Pts',(0.237110933519941,-0.0106930850971394,
-1.1264627391622));
#70036=CARTESIAN_POINT('Ctrl Pts',(0.236162235121939,-0.0220037496602497,
-1.12720320249862));
#70037=CARTESIAN_POINT('Ctrl Pts',(0.235949240789082,-0.0241810161489934,
-1.12734680811525));
#70038=CARTESIAN_POINT('Ctrl Pts',(0.235560924218474,-0.0276539330917851,
-1.12757772263743));
#70039=CARTESIAN_POINT('Ctrl Pts',(0.235404950321511,-0.0289516542205399,
-1.12766442238254));
#70040=CARTESIAN_POINT('Ctrl Pts',(0.235088744104658,-0.0314107855699627,
-1.12782953169399));
#70041=CARTESIAN_POINT('Ctrl Pts',(0.234930610544518,-0.0325724300424209,
-1.12790787273382));
#70042=CARTESIAN_POINT('Ctrl Pts',(0.234550908608133,-0.0352149678859291,
-1.12808689777618));
#70043=CARTESIAN_POINT('Ctrl Pts',(0.234323917078178,-0.0366950187103823,
-1.1281877504441));
#70044=CARTESIAN_POINT('Ctrl Pts',(0.233581549313853,-0.0412473611854537,
-1.12849980461081));
#70045=CARTESIAN_POINT('Ctrl Pts',(0.233019663927399,-0.0443116192241604,
-1.12871246385869));
#70046=CARTESIAN_POINT('Ctrl Pts',(0.228843687765467,-0.0648016750872356,
-1.13015271215553));
#70047=CARTESIAN_POINT('Ctrl Pts',(0.223339037346654,-0.0817810165075423,
-1.13144160255495));
#70048=CARTESIAN_POINT('Ctrl Pts',(0.214238724560909,-0.101841608410182,
-1.13305048358938));
#70049=CARTESIAN_POINT('Ctrl Pts',(0.212384604892954,-0.105653796513923,
-1.13336001369849));
#70050=CARTESIAN_POINT('Ctrl Pts',(0.207430924343587,-0.115180884623488,
-1.13414073118266));
#70051=CARTESIAN_POINT('Ctrl Pts',(0.204196553583779,-0.120822197665742,
-1.13460980553231));
#70052=CARTESIAN_POINT('Ctrl Pts',(0.198791537851994,-0.129411012014511,
-1.13532773813752));
#70053=CARTESIAN_POINT('Ctrl Pts',(0.196777667369966,-0.132453156944946,
-1.13558279037206));
#70054=CARTESIAN_POINT('Ctrl Pts',(0.19405879078727,-0.136361301808681,
-1.13591026291336));
#70055=CARTESIAN_POINT('Ctrl Pts',(0.19341685635394,-0.13727031257325,-1.13598641718555));
#70056=CARTESIAN_POINT('Ctrl Pts',(0.192358195844793,-0.138747256569972,
-1.13611008430678));
#70057=CARTESIAN_POINT('Ctrl Pts',(0.191945304720318,-0.139317898144015,
-1.13615784861687));
#70058=CARTESIAN_POINT('Ctrl Pts',(0.191133356275669,-0.140429600537358,
-1.13625085528365));
#70059=CARTESIAN_POINT('Ctrl Pts',(0.190734531869393,-0.14097081598071,
-1.13629611173832));
#70060=CARTESIAN_POINT('Ctrl Pts',(0.189835746786442,-0.142179694670568,
-1.13639716553758));
#70061=CARTESIAN_POINT('Ctrl Pts',(0.189334549333362,-0.142846437882056,
-1.13645287820429));
#70062=CARTESIAN_POINT('Ctrl Pts',(0.187573158094216,-0.145164060184163,
-1.13664651325399));
#70063=CARTESIAN_POINT('Ctrl Pts',(0.186294762984918,-0.146801076335037,
-1.13678324143866));
#70064=CARTESIAN_POINT('Ctrl Pts',(0.17744585521328,-0.157830524743763,
-1.13770579236312));
#70065=CARTESIAN_POINT('Ctrl Pts',(0.169188828676269,-0.16665149611595,
-1.13845084416637));
#70066=CARTESIAN_POINT('Ctrl Pts',(0.152411067473868,-0.182036478942389,
-1.13984824140794));
#70067=CARTESIAN_POINT('Ctrl Pts',(0.144046763855794,-0.188724492665677,
-1.14049998640912));
#70068=CARTESIAN_POINT('Ctrl Pts',(0.127622223267001,-0.200127459957259,
-1.14174568685739));
#70069=CARTESIAN_POINT('Ctrl Pts',(0.119680166058774,-0.204975752704548,
-1.14233486674289));
#70070=CARTESIAN_POINT('Ctrl Pts',(0.109536259108629,-0.210377307727473,
-1.14308452634287));
#70071=CARTESIAN_POINT('Ctrl Pts',(0.10758362260767,-0.211382514132093,
-1.14322868138569));
#70072=CARTESIAN_POINT('Ctrl Pts',(0.104445394837434,-0.212943310233738,
-1.14346027106186));
#70073=CARTESIAN_POINT('Ctrl Pts',(0.103268643717226,-0.213516465370341,
-1.14354709014467));
#70074=CARTESIAN_POINT('Ctrl Pts',(0.101029351992212,-0.214584305688889,
-1.14371229314744));
#70075=CARTESIAN_POINT('Ctrl Pts',(0.0999677676067785,-0.215080913998919,
-1.14379060741616));
#70076=CARTESIAN_POINT('Ctrl Pts',(0.0975445528363097,-0.216192676143264,
-1.14396938477424));
#70077=CARTESIAN_POINT('Ctrl Pts',(0.0961807139521616,-0.216802866890058,
-1.14407001478885));
#70078=CARTESIAN_POINT('Ctrl Pts',(0.0919714157627855,-0.218638600606687,
-1.14438067882214));
#70079=CARTESIAN_POINT('Ctrl Pts',(0.0891077336828184,-0.219821266503457,
-1.14459215183858));
#70080=CARTESIAN_POINT('Ctrl Pts',(0.0694195379427486,-0.227504324527932,
-1.14604754065849));
#70081=CARTESIAN_POINT('Ctrl Pts',(0.0519271782830554,-0.232121991604896,
-1.14735465096144));
#70082=CARTESIAN_POINT('Ctrl Pts',(0.0301428343547714,-0.235285476744169,
-1.14896239364466));
#70083=CARTESIAN_POINT('Ctrl Pts',(0.0261872018706163,-0.235758514571029,
-1.14925322542085));
#70084=CARTESIAN_POINT('Ctrl Pts',(0.0157214208982848,-0.23674341107059,
-1.15001758514916));
#70085=CARTESIAN_POINT('Ctrl Pts',(0.00919840287627271,-0.237086496105111,
-1.15048883640984));
#70086=CARTESIAN_POINT('Ctrl Pts',(-0.000989006725740775,-0.237201151451644,
-1.15120966282682));
#70087=CARTESIAN_POINT('Ctrl Pts',(-0.00464787538912799,-0.237157680196853,
-1.15146548635012));
#70088=CARTESIAN_POINT('Ctrl Pts',(-0.00941777121983237,-0.236990563271742,
-1.15179378807042));
#70089=CARTESIAN_POINT('Ctrl Pts',(-0.0105307707046329,-0.236943715861734,
-1.15187002300753));
#70090=CARTESIAN_POINT('Ctrl Pts',(-0.0123471672718733,-0.236854437436524,
-1.15199378785587));
#70091=CARTESIAN_POINT('Ctrl Pts',(-0.0130507625365456,-0.236816711199495,
-1.15204156995918));
#70092=CARTESIAN_POINT('Ctrl Pts',(-0.0144251695490441,-0.236736872582281,
-1.15213458311347));
#70093=CARTESIAN_POINT('Ctrl Pts',(-0.0150959851280274,-0.236695043477522,
-1.15217982845365));
#70094=CARTESIAN_POINT('Ctrl Pts',(-0.0165982208412435,-0.236594958352632,
-1.15228082833727));
#70095=CARTESIAN_POINT('Ctrl Pts',(-0.0174295384816232,-0.236535169675584,
-1.15233649849688));
#70096=CARTESIAN_POINT('Ctrl Pts',(-0.0203274515066548,-0.236311389784029,
-1.15252984084061));
#70097=CARTESIAN_POINT('Ctrl Pts',(-0.0223922689776497,-0.236124681545236,
-1.15266632355011));
#70098=CARTESIAN_POINT('Ctrl Pts',(-0.0363692855367893,-0.234675828003325,
-1.15358314349622));
#70099=CARTESIAN_POINT('Ctrl Pts',(-0.048175032116428,-0.232539693511401,
-1.15432327526225));
#70100=CARTESIAN_POINT('Ctrl Pts',(-0.0699638891871704,-0.226865589767654,
-1.15570560675641));
#70101=CARTESIAN_POINT('Ctrl Pts',(-0.07996941314275,-0.223534844545659,
-1.15634735597856));
#70102=CARTESIAN_POINT('Ctrl Pts',(-0.0985374537651305,-0.215946938355736,
-1.15759586768057));
#70103=CARTESIAN_POINT('Ctrl Pts',(-0.107128782510009,-0.211816196857135,
-1.15819889367307));
#70104=CARTESIAN_POINT('Ctrl Pts',(-0.117378565001545,-0.206104677614221,
-1.15896417483642));
#70105=CARTESIAN_POINT('Ctrl Pts',(-0.119294071413432,-0.20500192594188,
-1.15910923653641));
#70106=CARTESIAN_POINT('Ctrl Pts',(-0.122321583501461,-0.203202195086298,
-1.15934194035894));
#70107=CARTESIAN_POINT('Ctrl Pts',(-0.123443730439871,-0.202522460916993,
-1.15942895632546));
#70108=CARTESIAN_POINT('Ctrl Pts',(-0.125557040455298,-0.201218245886004,
-1.15959431575223));
#70109=CARTESIAN_POINT('Ctrl Pts',(-0.126549332232269,-0.200595661249132,
-1.15967258771551));
#70110=CARTESIAN_POINT('Ctrl Pts',(-0.128792252297072,-0.199165140360875,
-1.15985096551648));
#70111=CARTESIAN_POINT('Ctrl Pts',(-0.130039956217819,-0.198352733778828,
-1.15995123546677));
#70112=CARTESIAN_POINT('Ctrl Pts',(-0.13383726454472,-0.195828997225761,
-1.16025965950965));
#70113=CARTESIAN_POINT('Ctrl Pts',(-0.136361265945692,-0.19407991432151,
-1.16046922264373));
#70114=CARTESIAN_POINT('Ctrl Pts',(-0.153745705485166,-0.181526304591085,
-1.16194554150995));
#70115=CARTESIAN_POINT('Ctrl Pts',(-0.167337942207479,-0.169077799770556,
-1.16327821337226));
#70116=CARTESIAN_POINT('Ctrl Pts',(-0.18174260520957,-0.15243004469822,
-1.16488600569931));
#70117=CARTESIAN_POINT('Ctrl Pts',(-0.184066024994794,-0.149616149185998,
-1.16515233782426));
#70118=CARTESIAN_POINT('Ctrl Pts',(-0.190381119026234,-0.141598069082342,
-1.16589454039798));
#70119=CARTESIAN_POINT('Ctrl Pts',(-0.194223494607145,-0.136279966921783,
-1.16636794035536));
#70120=CARTESIAN_POINT('Ctrl Pts',(-0.199864297572836,-0.127748599825389,
-1.16709162082814));
#70121=CARTESIAN_POINT('Ctrl Pts',(-0.201816713660103,-0.124641325233927,
-1.16734820356022));
#70122=CARTESIAN_POINT('Ctrl Pts',(-0.204267553770227,-0.120532114009814,
-1.16767732117223));
#70123=CARTESIAN_POINT('Ctrl Pts',(-0.204831992901538,-0.119570392818159,
-1.16775363527238));
#70124=CARTESIAN_POINT('Ctrl Pts',(-0.205742113495588,-0.117994322573419,
-1.16787749603055));
#70125=CARTESIAN_POINT('Ctrl Pts',(-0.206091868135685,-0.117382363865643,
-1.1679252955988));
#70126=CARTESIAN_POINT('Ctrl Pts',(-0.206769713668097,-0.116183981857287,
-1.16801831519171));
#70127=CARTESIAN_POINT('Ctrl Pts',(-0.207098047836004,-0.115597710748142,
-1.16806354969296));
#70128=CARTESIAN_POINT('Ctrl Pts',(-0.207827732597219,-0.114281703524437,
-1.16816449691621));
#70129=CARTESIAN_POINT('Ctrl Pts',(-0.208227744213148,-0.113551225395855,
-1.16822012554162));
#70130=CARTESIAN_POINT('Ctrl Pts',(-0.209608251784303,-0.110998394772349,
-1.16841318223844));
#70131=CARTESIAN_POINT('Ctrl Pts',(-0.210568772790058,-0.109165266905475,
-1.16854942543521));
#70132=CARTESIAN_POINT('Ctrl Pts',(-0.217030705839643,-0.0964301193337436,
-1.16948122206851));
#70133=CARTESIAN_POINT('Ctrl Pts',(-0.221707692869848,-0.0851285575530953,
-1.17023492700159));
#70134=CARTESIAN_POINT('Ctrl Pts',(-0.228886668415068,-0.0631085912129428,
-1.17165642729218));
#70135=CARTESIAN_POINT('Ctrl Pts',(-0.231555010257356,-0.0524792149611912,
-1.17232340992169));
#70136=CARTESIAN_POINT('Ctrl Pts',(-0.234522507227085,-0.035865684823955,
-1.173376367813));
#70137=CARTESIAN_POINT('Ctrl Pts',(-0.23534592502807,-0.0299906931523876,
-1.17375054319587));
#70138=CARTESIAN_POINT('Ctrl Pts',(-0.236364544315377,-0.0200144234771666,
-1.17439387417916));
#70139=CARTESIAN_POINT('Ctrl Pts',(-0.236675055693389,-0.0159276401333891,
-1.17465963204208));
#70140=CARTESIAN_POINT('Ctrl Pts',(-0.236962712114926,-0.0101701736989374,
-1.17503812091913));
#70141=CARTESIAN_POINT('Ctrl Pts',(-0.23702833711639,-0.00850450073222969,
-1.17514809805222));
#70142=CARTESIAN_POINT('Ctrl Pts',(-0.237110946904129,-0.00564051342665427,
-1.17533807811522));
#70143=CARTESIAN_POINT('Ctrl Pts',(-0.237136417925124,-0.00444249220207289,
-1.17541781319959));
#70144=CARTESIAN_POINT('Ctrl Pts',(-0.237167760966887,-0.00215140304656673,
-1.17557082767517));
#70145=CARTESIAN_POINT('Ctrl Pts',(-0.237175157069876,-0.0010583840107431,
-1.17564405729223));
#70146=CARTESIAN_POINT('Ctrl Pts',(-0.237174741680534,0.00178642760199683,
-1.17583527211774));
#70147=CARTESIAN_POINT('Ctrl Pts',(-0.23715507753422,0.00353812482777787,
-1.17595362460651));
#70148=CARTESIAN_POINT('Ctrl Pts',(-0.237011863470604,0.00995819632098395,
-1.17638972792835));
#70149=CARTESIAN_POINT('Ctrl Pts',(-0.236769853990665,0.0146225848959933,
-1.17671112571038));
#70150=CARTESIAN_POINT('Ctrl Pts',(-0.235812395804736,0.026364013917505,
-1.17753220430705));
#70151=CARTESIAN_POINT('Ctrl Pts',(-0.234916042727825,0.0334213101702695,
-1.17803691094854));
#70152=CARTESIAN_POINT('Ctrl Pts',(-0.230856515571357,0.0568889139292118,
-1.17974967845699));
#70153=CARTESIAN_POINT('Ctrl Pts',(-0.22627782844322,0.0730026233955595,
-1.18098663962895));
#70154=CARTESIAN_POINT('Ctrl Pts',(-0.217906823836924,0.0938158441443284,
-1.18259573249308));
#70155=CARTESIAN_POINT('Ctrl Pts',(-0.21557719070102,0.0990519230564529,
-1.18300110412899));
#70156=CARTESIAN_POINT('Ctrl Pts',(-0.212478364253266,0.105388225432735,
-1.1834881401991));
#70157=CARTESIAN_POINT('Ctrl Pts',(-0.211886766069377,0.106572660203199,
-1.18357902413048));
#70158=CARTESIAN_POINT('Ctrl Pts',(-0.210940642750093,0.108427862019017,
-1.18372105802144));
#70159=CARTESIAN_POINT('Ctrl Pts',(-0.21059277542902,0.109101966085748,
-1.18377260037059));
#70160=CARTESIAN_POINT('Ctrl Pts',(-0.209967279688984,0.110299925442415,
-1.18386406200718));
#70161=CARTESIAN_POINT('Ctrl Pts',(-0.209690921285973,0.110824409020092,
-1.18390405738454));
#70162=CARTESIAN_POINT('Ctrl Pts',(-0.209021449961354,0.112083487656867,
-1.18399996166854));
#70163=CARTESIAN_POINT('Ctrl Pts',(-0.208626429673238,0.112817053870883,
-1.18405574961404));
#70164=CARTESIAN_POINT('Ctrl Pts',(-0.207402921759457,0.115060746786211,
-1.18422616027394));
#70165=CARTESIAN_POINT('Ctrl Pts',(-0.206561820627709,0.116563982816697,
-1.18434002107219));
#70166=CARTESIAN_POINT('Ctrl Pts',(-0.198780679454096,0.130121854451292,
-1.1853653465641));
#70167=CARTESIAN_POINT('Ctrl Pts',(-0.190808059056369,0.141555124994127,
-1.18621936627424));
#70168=CARTESIAN_POINT('Ctrl Pts',(-0.170866808961038,0.16538090361281,
-1.18812422283224));
#70169=CARTESIAN_POINT('Ctrl Pts',(-0.158462159204998,0.17730191673118,
-1.18917161289272));
#70170=CARTESIAN_POINT('Ctrl Pts',(-0.142386233418689,0.189705219304556,
-1.19048406282894));
#70171=CARTESIAN_POINT('Ctrl Pts',(-0.139853423784967,0.19158008255297,
-1.19068951119054));
#70172=CARTESIAN_POINT('Ctrl Pts',(-0.136057571957042,0.194274496875286,
-1.19099590812578));
#70173=CARTESIAN_POINT('Ctrl Pts',(-0.134822804770519,0.195133426561145,
-1.191095347513));
#70174=CARTESIAN_POINT('Ctrl Pts',(-0.132610598882909,0.19664126203817,
-1.19127314290236));
#70175=CARTESIAN_POINT('Ctrl Pts',(-0.131636349362063,0.197294775181207,
-1.1913513211998));
#70176=CARTESIAN_POINT('Ctrl Pts',(-0.129569619459936,0.198658986384733,
-1.19151693059126));
#70177=CARTESIAN_POINT('Ctrl Pts',(-0.128476052404071,0.199367958808177,
-1.19160442289329));
#70178=CARTESIAN_POINT('Ctrl Pts',(-0.125546051942616,0.201233394959267,
-1.19183851259752));
#70179=CARTESIAN_POINT('Ctrl Pts',(-0.123699531701615,0.202373703122936,
-1.19198569916478));
#70180=CARTESIAN_POINT('Ctrl Pts',(-0.114201121407433,0.208060827212608,
-1.19274132021021));
#70181=CARTESIAN_POINT('Ctrl Pts',(-0.106314195626829,0.212199106191769,
-1.19336423610559));
#70182=CARTESIAN_POINT('Ctrl Pts',(-0.0878605932591958,0.220594383047642,
-1.19481131580663));
#70183=CARTESIAN_POINT('Ctrl Pts',(-0.0771822007688765,0.224553416472287,
-1.19564179880238));
#70184=CARTESIAN_POINT('Ctrl Pts',(-0.06297003361872,0.228688673782941,
-1.19672266195846));
#70185=CARTESIAN_POINT('Ctrl Pts',(-0.059657716118993,0.229575024998775,
-1.19697281403438));
#70186=CARTESIAN_POINT('Ctrl Pts',(-0.0515632186175443,0.231554029079316,
-1.19757855479759));
#70187=CARTESIAN_POINT('Ctrl Pts',(-0.0467648793695778,0.232570558798781,
-1.19793297986431));
#70188=CARTESIAN_POINT('Ctrl Pts',(-0.0419392699415209,0.233437525393353,
-1.19828290886153));
#70189=CARTESIAN_POINT('Ctrl Pts',(-0.041939274136423,0.233437524639699,
-1.21783461098805));
#70190=CARTESIAN_POINT('Ctrl Pts',(-0.0426432674237616,0.233311045542075,
-1.21778239868806));
#70191=CARTESIAN_POINT('Ctrl Pts',(-0.043346762008648,0.233181368630309,
-1.21773016760089));
#70192=CARTESIAN_POINT('Ctrl Pts',(-0.0540389257832951,0.231160385863027,
-1.21693553759598));
#70193=CARTESIAN_POINT('Ctrl Pts',(-0.0638968914046291,0.228631882994274,
-1.21619186825365));
#70194=CARTESIAN_POINT('Ctrl Pts',(-0.0766195564889107,0.224481099184353,
-1.21523749386044));
#70195=CARTESIAN_POINT('Ctrl Pts',(-0.0796560834308802,0.223421643636488,
-1.21501018080959));
#70196=CARTESIAN_POINT('Ctrl Pts',(-0.0847482635210627,0.221527938787716,
-1.21463080184728));
#70197=CARTESIAN_POINT('Ctrl Pts',(-0.0868154088882168,0.22072603268003,
-1.21447731157509));
#70198=CARTESIAN_POINT('Ctrl Pts',(-0.0897256243853002,0.219549863229728,
-1.21426225417374));
#70199=CARTESIAN_POINT('Ctrl Pts',(-0.0905781497778032,0.219199518634965,
-1.21419938160906));
#70200=CARTESIAN_POINT('Ctrl Pts',(-0.0920429676698517,0.218587547708031,
-1.2140915989717));
#70201=CARTESIAN_POINT('Ctrl Pts',(-0.0926562345163415,0.218328299040453,
-1.21404654933767));
#70202=CARTESIAN_POINT('Ctrl Pts',(-0.0939410738838145,0.217778765019048,
-1.21395233386869));
#70203=CARTESIAN_POINT('Ctrl Pts',(-0.0946124026783115,0.217487951739309,
-1.21390320021296));
#70204=CARTESIAN_POINT('Ctrl Pts',(-0.0964152105135642,0.21669706521441,
-1.21377148013796));
#70205=CARTESIAN_POINT('Ctrl Pts',(-0.0975441596143591,0.216191230120239,
-1.21368923432154));
#70206=CARTESIAN_POINT('Ctrl Pts',(-0.102719891697156,0.213823402332313,
-1.21331304579725));
#70207=CARTESIAN_POINT('Ctrl Pts',(-0.106717958595642,0.21185633567699,
-1.21302491633419));
#70208=CARTESIAN_POINT('Ctrl Pts',(-0.130637611581025,0.199238625398129,
-1.21130197056097));
#70209=CARTESIAN_POINT('Ctrl Pts',(-0.149009874234426,0.185899088748642,
-1.20997161250906));
#70210=CARTESIAN_POINT('Ctrl Pts',(-0.168478997329588,0.166995373724913,
-1.20826084139175));
#70211=CARTESIAN_POINT('Ctrl Pts',(-0.171647185520011,0.163737189538371,
-1.20797143840478));
#70212=CARTESIAN_POINT('Ctrl Pts',(-0.176989964973071,0.157917076966593,
-1.20746164681532));
#70213=CARTESIAN_POINT('Ctrl Pts',(-0.179207365019452,0.155396169167168,
-1.2072430350147));
#70214=CARTESIAN_POINT('Ctrl Pts',(-0.1823639492274,0.15165008381701,-1.20692079377868));
#70215=CARTESIAN_POINT('Ctrl Pts',(-0.183345928721492,0.150461384189584,
-1.20681891383569));
#70216=CARTESIAN_POINT('Ctrl Pts',(-0.185057349953819,0.148348052365386,
-1.20663838922153));
#70217=CARTESIAN_POINT('Ctrl Pts',(-0.185791632555776,0.147427394330266,
-1.20655994285945));
#70218=CARTESIAN_POINT('Ctrl Pts',(-0.18731183263042,0.145491942666614,
-1.2063954177499));
#70219=CARTESIAN_POINT('Ctrl Pts',(-0.188096427489744,0.144476163700002,
-1.20630928996589));
#70220=CARTESIAN_POINT('Ctrl Pts',(-0.190131143382502,0.141797241445922,
-1.20608268517788));
#70221=CARTESIAN_POINT('Ctrl Pts',(-0.191367668819423,0.140123960173734,
-1.20594168359108));
#70222=CARTESIAN_POINT('Ctrl Pts',(-0.196614008545141,0.132825568046982,
-1.20532880857199));
#70223=CARTESIAN_POINT('Ctrl Pts',(-0.200398658133802,0.127043539287908,
-1.20484852618026));
#70224=CARTESIAN_POINT('Ctrl Pts',(-0.212160122662664,0.107238754336975,
-1.20321973371885));
#70225=CARTESIAN_POINT('Ctrl Pts',(-0.218958395352845,0.09256984386528,
-1.20203580068697));
#70226=CARTESIAN_POINT('Ctrl Pts',(-0.227563828599233,0.0676178135817661,
-1.20011383446844));
#70227=CARTESIAN_POINT('Ctrl Pts',(-0.230278583307003,0.0576999922608403,
-1.19937301128378));
#70228=CARTESIAN_POINT('Ctrl Pts',(-0.232635944227891,0.0462021790844658,
-1.19856106024312));
#70229=CARTESIAN_POINT('Ctrl Pts',(-0.232916709799689,0.0447652819295154,
-1.19846042002002));
#70230=CARTESIAN_POINT('Ctrl Pts',(-0.233326763068729,0.0425583323512279,
-1.19830721017047));
#70231=CARTESIAN_POINT('Ctrl Pts',(-0.233465577801123,0.0417901189632514,
-1.19825413225684));
#70232=CARTESIAN_POINT('Ctrl Pts',(-0.233714030452848,0.0403752734776626,
-1.19815685866873));
#70233=CARTESIAN_POINT('Ctrl Pts',(-0.233824779758888,0.0397288702221894,
-1.19811260362287));
#70234=CARTESIAN_POINT('Ctrl Pts',(-0.234070929117119,0.0382554953722119,
-1.19801214958318));
#70235=CARTESIAN_POINT('Ctrl Pts',(-0.234204629049285,0.0374282589726527,
-1.19795604649148));
#70236=CARTESIAN_POINT('Ctrl Pts',(-0.234543053413201,0.0352614930589668,
-1.19780983328912));
#70237=CARTESIAN_POINT('Ctrl Pts',(-0.234740690846305,0.0339208647910625,
-1.19772010318464));
#70238=CARTESIAN_POINT('Ctrl Pts',(-0.236414371006712,0.0218518181606137,
-1.19691830900986));
#70239=CARTESIAN_POINT('Ctrl Pts',(-0.237165692648452,0.0110342417309567,
-1.19624196860633));
#70240=CARTESIAN_POINT('Ctrl Pts',(-0.237189966526827,-0.0174801366085886,
-1.19448383101853));
#70241=CARTESIAN_POINT('Ctrl Pts',(-0.235227740014875,-0.0351072123251257,
-1.19341787834779));
#70242=CARTESIAN_POINT('Ctrl Pts',(-0.230186434309013,-0.0573828222203118,
-1.19196437274814));
#70243=CARTESIAN_POINT('Ctrl Pts',(-0.228884237018761,-0.0623745352904542,
-1.19163189578001));
#70244=CARTESIAN_POINT('Ctrl Pts',(-0.226888867572798,-0.0691153367603384,
-1.19117160025476));
#70245=CARTESIAN_POINT('Ctrl Pts',(-0.226336055440587,-0.0709047084328291,
-1.19104831278622));
#70246=CARTESIAN_POINT('Ctrl Pts',(-0.225420383715599,-0.0737487263186357,
-1.19085051343898));
#70247=CARTESIAN_POINT('Ctrl Pts',(-0.225071167766121,-0.0748077094700161,
-1.19077645013998));
#70248=CARTESIAN_POINT('Ctrl Pts',(-0.224336316702724,-0.0769843849543035,
-1.19062334725718));
#70249=CARTESIAN_POINT('Ctrl Pts',(-0.223949766107451,-0.0781017329610288,
-1.19054427924332));
#70250=CARTESIAN_POINT('Ctrl Pts',(-0.223029129709321,-0.0806998499204871,
-1.19035929009358));
#70251=CARTESIAN_POINT('Ctrl Pts',(-0.222488629368415,-0.0821782700574747,
-1.19025315852848));
#70252=CARTESIAN_POINT('Ctrl Pts',(-0.220685338120716,-0.0869625506972465,
-1.18990682228929));
#70253=CARTESIAN_POINT('Ctrl Pts',(-0.219363319668876,-0.0902454171498826,
-1.18966465743708));
#70254=CARTESIAN_POINT('Ctrl Pts',(-0.216048375434738,-0.097973478762779,
-1.18908345578343));
#70255=CARTESIAN_POINT('Ctrl Pts',(-0.213991036099672,-0.102389129468412,
-1.18874239266833));
#70256=CARTESIAN_POINT('Ctrl Pts',(-0.20514865303143,-0.119934987770485,
-1.18735067571285));
#70257=CARTESIAN_POINT('Ctrl Pts',(-0.197279653408148,-0.132480269158027,
-1.18626837018449));
#70258=CARTESIAN_POINT('Ctrl Pts',(-0.181497998076469,-0.153086424613433,
-1.18437557275629));
#70259=CARTESIAN_POINT('Ctrl Pts',(-0.174080126472723,-0.161471810516364,
-1.18356618472631));
#70260=CARTESIAN_POINT('Ctrl Pts',(-0.165129842716036,-0.170252615626823,
-1.18269830427765));
#70261=CARTESIAN_POINT('Ctrl Pts',(-0.164154072812613,-0.171193629191316,
-1.18260502020909));
#70262=CARTESIAN_POINT('Ctrl Pts',(-0.1625620289862,-0.172702836549947,
-1.18245503838124));
#70263=CARTESIAN_POINT('Ctrl Pts',(-0.161950733553993,-0.173276204298726,
-1.18239796970843));
#70264=CARTESIAN_POINT('Ctrl Pts',(-0.160855683220197,-0.17429245513326,
-1.18229668173844));
#70265=CARTESIAN_POINT('Ctrl Pts',(-0.160373118015634,-0.174736584015536,
-1.18225236979393));
#70266=CARTESIAN_POINT('Ctrl Pts',(-0.159312196976313,-0.17570490528099,
-1.1821556574077));
#70267=CARTESIAN_POINT('Ctrl Pts',(-0.158733092249554,-0.176228247775858,
-1.18210332002352));
#70268=CARTESIAN_POINT('Ctrl Pts',(-0.157060789017248,-0.177724592910838,
-1.18195344369183));
#70269=CARTESIAN_POINT('Ctrl Pts',(-0.155961131073359,-0.178690369727646,
-1.18185642363749));
#70270=CARTESIAN_POINT('Ctrl Pts',(-0.147092081431071,-0.186335380591913,
-1.18108543255655));
#70271=CARTESIAN_POINT('Ctrl Pts',(-0.138905201989436,-0.192515856226519,
-1.18044342693715));
#70272=CARTESIAN_POINT('Ctrl Pts',(-0.116923368509795,-0.206975663473038,
-1.1788180998305));
#70273=CARTESIAN_POINT('Ctrl Pts',(-0.102642028157704,-0.214416897293547,
-1.17784964424824));
#70274=CARTESIAN_POINT('Ctrl Pts',(-0.0812338229270205,-0.222938909942981,
-1.1763990717586));
#70275=CARTESIAN_POINT('Ctrl Pts',(-0.0746391563416337,-0.22523248776701,
-1.17595288723864));
#70276=CARTESIAN_POINT('Ctrl Pts',(-0.0659518223529203,-0.227830424702331,
-1.17536070631811));
#70277=CARTESIAN_POINT('Ctrl Pts',(-0.0639424623218083,-0.228402509496634,
-1.17522344837878));
#70278=CARTESIAN_POINT('Ctrl Pts',(-0.0606850630214332,-0.229283571062877,
-1.17500035064011));
#70279=CARTESIAN_POINT('Ctrl Pts',(-0.0594415808420452,-0.229609083421537,
-1.17491504830998));
#70280=CARTESIAN_POINT('Ctrl Pts',(-0.0570544481608036,-0.230213283856152,
-1.17475100167034));
#70281=CARTESIAN_POINT('Ctrl Pts',(-0.0559112455733474,-0.230493597852465,
-1.17467231257606));
#70282=CARTESIAN_POINT('Ctrl Pts',(-0.0532697426525975,-0.23112048825232,
-1.1744901772587));
#70283=CARTESIAN_POINT('Ctrl Pts',(-0.0517700772258659,-0.231461021518108,
-1.17438654037031));
#70284=CARTESIAN_POINT('Ctrl Pts',(-0.047007957685412,-0.232493774222229,
-1.17405665198162));
#70285=CARTESIAN_POINT('Ctrl Pts',(-0.0437342859624637,-0.2331317511562,
-1.17382869066242));
#70286=CARTESIAN_POINT('Ctrl Pts',(-0.0360096315498282,-0.234468718296675,
-1.17328775003801));
#70287=CARTESIAN_POINT('Ctrl Pts',(-0.0315501541622061,-0.235110307354584,
-1.17297310204474));
#70288=CARTESIAN_POINT('Ctrl Pts',(-0.00519185329237518,-0.238139110969328,
-1.17109954244191));
#70289=CARTESIAN_POINT('Ctrl Pts',(0.0169309740180664,-0.237592714306224,
-1.16945751408562));
#70290=CARTESIAN_POINT('Ctrl Pts',(0.0435897094744356,-0.233188544262195,
-1.16752728814484));
#70291=CARTESIAN_POINT('Ctrl Pts',(0.0484942525374433,-0.2322181643712,
-1.16717491708163));
#70292=CARTESIAN_POINT('Ctrl Pts',(0.0546185946834486,-0.230803911213174,
-1.16674127149684));
#70293=CARTESIAN_POINT('Ctrl Pts',(0.0558699961668047,-0.230504186581823,
-1.16665300260769));
#70294=CARTESIAN_POINT('Ctrl Pts',(0.0578395936612615,-0.230015463309025,
-1.16651467641907));
#70295=CARTESIAN_POINT('Ctrl Pts',(0.0585594250101764,-0.229833256377454,
-1.16646424940534));
#70296=CARTESIAN_POINT('Ctrl Pts',(0.0599196974655453,-0.229482132515216,
-1.1663692133818));
#70297=CARTESIAN_POINT('Ctrl Pts',(0.0605602827239637,-0.229313914657534,
-1.16632456850734));
#70298=CARTESIAN_POINT('Ctrl Pts',(0.062068282962792,-0.228911153592259,
-1.1662197164826));
#70299=CARTESIAN_POINT('Ctrl Pts',(0.0629350812841534,-0.22867436148042,
-1.16615963890224));
#70300=CARTESIAN_POINT('Ctrl Pts',(0.0658038398927074,-0.227873126079228,
-1.16596137666121));
#70301=CARTESIAN_POINT('Ctrl Pts',(0.06779978693299,-0.227287255592521,
-1.16582435903735));
#70302=CARTESIAN_POINT('Ctrl Pts',(0.0792768821923279,-0.223753733212192,
-1.16504044166496));
#70303=CARTESIAN_POINT('Ctrl Pts',(0.0885742753545106,-0.220238964085418,
-1.16442088886412));
#70304=CARTESIAN_POINT('Ctrl Pts',(0.113709994481223,-0.208886396498186,
-1.16272027400538));
#70305=CARTESIAN_POINT('Ctrl Pts',(0.128932892464018,-0.199849368037075,
-1.16165628474119));
#70306=CARTESIAN_POINT('Ctrl Pts',(0.147143878956586,-0.186084608770122,
-1.1602038195267));
#70307=CARTESIAN_POINT('Ctrl Pts',(0.151171793568941,-0.182827474081539,
-1.15987003806815));
#70308=CARTESIAN_POINT('Ctrl Pts',(0.156514942831373,-0.178209433620596,
-1.15940768941758));
#70309=CARTESIAN_POINT('Ctrl Pts',(0.157925467869987,-0.176960661785372,
-1.15928368714886));
#70310=CARTESIAN_POINT('Ctrl Pts',(0.160148520271148,-0.174944791761097,
-1.15908503158904));
#70311=CARTESIAN_POINT('Ctrl Pts',(0.160970781155501,-0.174188507803499,
-1.15901083412621));
#70312=CARTESIAN_POINT('Ctrl Pts',(0.162651414624463,-0.172620663080795,
-1.15885767206547));
#70313=CARTESIAN_POINT('Ctrl Pts',(0.163509127065789,-0.171808443566612,
-1.15877868046286));
#70314=CARTESIAN_POINT('Ctrl Pts',(0.165490503833879,-0.169903883189675,
-1.15859424751607));
#70315=CARTESIAN_POINT('Ctrl Pts',(0.166609469420922,-0.168806756014027,
-1.15848859959192));
#70316=CARTESIAN_POINT('Ctrl Pts',(0.170191242252126,-0.165224581338649,
-1.15814549610098));
#70317=CARTESIAN_POINT('Ctrl Pts',(0.172609858264452,-0.162696207004697,
-1.157906130965));
#70318=CARTESIAN_POINT('Ctrl Pts',(0.178210440126726,-0.15657597942922,
-1.15733292593698));
#70319=CARTESIAN_POINT('Ctrl Pts',(0.181340973279195,-0.15293934826554,
-1.15699713391003));
#70320=CARTESIAN_POINT('Ctrl Pts',(0.193377046030653,-0.138068027708613,
-1.1556427945762));
#70321=CARTESIAN_POINT('Ctrl Pts',(0.201365622090606,-0.126131936532784,
-1.15459448459287));
#70322=CARTESIAN_POINT('Ctrl Pts',(0.213851484562006,-0.103235351280445,
-1.15269140409647));
#70323=CARTESIAN_POINT('Ctrl Pts',(0.218702504131413,-0.0925163502315752,
-1.15183913573745));
#70324=CARTESIAN_POINT('Ctrl Pts',(0.223206428849908,-0.0802042299955998,
-1.15093162811337));
#70325=CARTESIAN_POINT('Ctrl Pts',(0.223662451455706,-0.078923611252432,
-1.15083807838557));
#70326=CARTESIAN_POINT('Ctrl Pts',(0.224382169397844,-0.0768461252722291,
-1.15068775520898));
#70327=CARTESIAN_POINT('Ctrl Pts',(0.224652681774047,-0.0760516767686259,
-1.15063060818971));
#70328=CARTESIAN_POINT('Ctrl Pts',(0.225127096139052,-0.074633782038733,
-1.15052923654061));
#70329=CARTESIAN_POINT('Ctrl Pts',(0.225332634575074,-0.0740109091146725,
-1.15048491862404));
#70330=CARTESIAN_POINT('Ctrl Pts',(0.225776836108271,-0.0726457759233576,
-1.1503882580277));
#70331=CARTESIAN_POINT('Ctrl Pts',(0.226014424854859,-0.0719031868833949,
-1.1503359778874));
#70332=CARTESIAN_POINT('Ctrl Pts',(0.226686191203706,-0.0697673345178731,
-1.15018643258901));
#70333=CARTESIAN_POINT('Ctrl Pts',(0.227111186799947,-0.0683711879622448,
-1.15008968277201));
#70334=CARTESIAN_POINT('Ctrl Pts',(0.230362579922951,-0.0573251259809278,
-1.14933145496211));
#70335=CARTESIAN_POINT('Ctrl Pts',(0.232585962626882,-0.047506960406693,
-1.14870075649617));
#70336=CARTESIAN_POINT('Ctrl Pts',(0.236647272772651,-0.0221963316549909,
-1.14711626951225));
#70337=CARTESIAN_POINT('Ctrl Pts',(0.237593974859879,-0.00661129926719322,
-1.14617690937497));
#70338=CARTESIAN_POINT('Ctrl Pts',(0.236720771513213,0.0165016644178685,
-1.14472521323594));
#70339=CARTESIAN_POINT('Ctrl Pts',(0.236075278998369,0.0240306782890839,
-1.14424354496226));
#70340=CARTESIAN_POINT('Ctrl Pts',(0.234786703244166,0.0336420559040256,
-1.14361062633756));
#70341=CARTESIAN_POINT('Ctrl Pts',(0.234472772863252,0.0357645387869451,
-1.14346973376627));
#70342=CARTESIAN_POINT('Ctrl Pts',(0.233922836654266,0.0391633880952803,
-1.14324217168667));
#70343=CARTESIAN_POINT('Ctrl Pts',(0.233705068642686,0.0404426167860829,
-1.14315608033256));
#70344=CARTESIAN_POINT('Ctrl Pts',(0.233270327312588,0.0428755527529102,
-1.14299146956674));
#70345=CARTESIAN_POINT('Ctrl Pts',(0.233055263638428,0.04402956544546,-1.14291301311287));
#70346=CARTESIAN_POINT('Ctrl Pts',(0.23254337001669,0.0466674578513854,
-1.14273278763022));
#70347=CARTESIAN_POINT('Ctrl Pts',(0.232240889969586,0.0481501755166029,
-1.14263084121828));
#70348=CARTESIAN_POINT('Ctrl Pts',(0.231254337733099,0.0527604111687545,
-1.14231179123146));
#70349=CARTESIAN_POINT('Ctrl Pts',(0.230521141724206,0.0558769288640855,
-1.14209313318396));
#70350=CARTESIAN_POINT('Ctrl Pts',(0.228663209140359,0.0631138178054533,
-1.14157815574417));
#70351=CARTESIAN_POINT('Ctrl Pts',(0.227489837085896,0.0672204381811554,
-1.14128037762379));
#70352=CARTESIAN_POINT('Ctrl Pts',(0.22273413316225,0.0823098752403299,
-1.14016545633391));
#70353=CARTESIAN_POINT('Ctrl Pts',(0.218462121316603,0.0930572823219848,
-1.13932901333487));
#70354=CARTESIAN_POINT('Ctrl Pts',(0.207026492703291,0.11664989073627,-1.13741566163372));
#70355=CARTESIAN_POINT('Ctrl Pts',(0.199416796277902,0.129229182400962,
-1.13633821743566));
#70356=CARTESIAN_POINT('Ctrl Pts',(0.189474888511497,0.142672504028754,
-1.13517284077083));
#70357=CARTESIAN_POINT('Ctrl Pts',(0.188235529351324,0.144303717839589,
-1.1350312210815));
#70358=CARTESIAN_POINT('Ctrl Pts',(0.186480133724057,0.146553020090981,
-1.13483587175918));
#70359=CARTESIAN_POINT('Ctrl Pts',(0.18598189411616,0.147184792285298,-1.1347809955183));
#70360=CARTESIAN_POINT('Ctrl Pts',(0.185066232169903,0.14833378594118,-1.13468119793736));
#70361=CARTESIAN_POINT('Ctrl Pts',(0.184649832438878,0.148851811429472,
-1.13463620615016));
#70362=CARTESIAN_POINT('Ctrl Pts',(0.183779803802982,0.14992490848241,-1.13454301994349));
#70363=CARTESIAN_POINT('Ctrl Pts',(0.183325829322084,0.150479682373755,
-1.13449485085888));
#70364=CARTESIAN_POINT('Ctrl Pts',(0.182124172832322,0.151934642565317,
-1.13436851335886));
#70365=CARTESIAN_POINT('Ctrl Pts',(0.181372320531353,0.152831382336588,
-1.1342906388956));
#70366=CARTESIAN_POINT('Ctrl Pts',(0.177874875446163,0.156940649475194,
-1.13393354494358));
#70367=CARTESIAN_POINT('Ctrl Pts',(0.175050181434453,0.160085221321697,
-1.13365960265962));
#70368=CARTESIAN_POINT('Ctrl Pts',(0.166508432087525,0.169097630576571,
-1.13286652560206));
#70369=CARTESIAN_POINT('Ctrl Pts',(0.16056949764631,0.174747027053532,-1.13235885618539));
#70370=CARTESIAN_POINT('Ctrl Pts',(0.139154754956289,0.193102167292089,
-1.13062390588213));
#70371=CARTESIAN_POINT('Ctrl Pts',(0.122374374625392,0.204149272007522,
-1.12941495888262));
#70372=CARTESIAN_POINT('Ctrl Pts',(0.101844657950847,0.214214351954104,
-1.12793364640446));
#70373=CARTESIAN_POINT('Ctrl Pts',(0.0992601730673875,0.215424092985487,
-1.12774730711218));
#70374=CARTESIAN_POINT('Ctrl Pts',(0.0953166213266252,0.217183951896363,
-1.12746287091724));
#70375=CARTESIAN_POINT('Ctrl Pts',(0.093973185100963,0.217768610185506,
-1.12736595496512));
#70376=CARTESIAN_POINT('Ctrl Pts',(0.0915484904539209,0.218797213264977,
-1.12719096180378));
#70377=CARTESIAN_POINT('Ctrl Pts',(0.0904691954517588,0.219245686906772,
-1.12711304144637));
#70378=CARTESIAN_POINT('Ctrl Pts',(0.0881584162751297,0.220185904544184,
-1.12694613523589));
#70379=CARTESIAN_POINT('Ctrl Pts',(0.0869260391746348,0.220675332806878,
-1.1268570743614));
#70380=CARTESIAN_POINT('Ctrl Pts',(0.0835670349066219,0.221976830267272,
-1.12661416530842));
#70381=CARTESIAN_POINT('Ctrl Pts',(0.0814327624010879,0.222768640243523,
-1.12645964729178));
#70382=CARTESIAN_POINT('Ctrl Pts',(0.069161609172963,0.227121303014167,
-1.12556995828185));
#70383=CARTESIAN_POINT('Ctrl Pts',(0.0588048803807109,0.230020304572861,
-1.12481327104394));
#70384=CARTESIAN_POINT('Ctrl Pts',(0.0318700692891486,0.235621532120924,
-1.122834600259));
#70385=CARTESIAN_POINT('Ctrl Pts',(0.0151368066056107,0.237284733431819,
-1.12159275197029));
#70386=CARTESIAN_POINT('Ctrl Pts',(-0.00727937266991831,0.237130538190622,
-1.11998554124484));
#70387=CARTESIAN_POINT('Ctrl Pts',(-0.0129246656213208,0.236889945144055,
-1.11958601924403));
#70388=CARTESIAN_POINT('Ctrl Pts',(-0.01987106672925,0.236344790856433,
-1.11910494127196));
#70389=CARTESIAN_POINT('Ctrl Pts',(-0.021184827551682,0.236230655800076,
-1.11901442370359));
#70390=CARTESIAN_POINT('Ctrl Pts',(-0.0232513904948218,0.236033740842036,
-1.11887284609843));
#70391=CARTESIAN_POINT('Ctrl Pts',(-0.0240048407047941,0.235958304874383,
-1.1188213974902));
#70392=CARTESIAN_POINT('Ctrl Pts',(-0.0253475052931209,0.235817378555635,
-1.11873003233602));
#70393=CARTESIAN_POINT('Ctrl Pts',(-0.0259368354468668,0.235753287637763,
-1.11869004040564));
#70394=CARTESIAN_POINT('Ctrl Pts',(-0.0273551085037183,0.235593664798319,
-1.11859405626479));
#70395=CARTESIAN_POINT('Ctrl Pts',(-0.0281837947362655,0.235495967315535,
-1.11853818576082));
#70396=CARTESIAN_POINT('Ctrl Pts',(-0.0307287808913199,0.235182301381307,
-1.11836720624933));
#70397=CARTESIAN_POINT('Ctrl Pts',(-0.032443293570044,0.234951922723352,
-1.11825286679294));
#70398=CARTESIAN_POINT('Ctrl Pts',(-0.0367572909630109,0.234324126990049,
-1.11796695612443));
#70399=CARTESIAN_POINT('Ctrl Pts',(-0.0393523414674697,0.233902291759656,
-1.11779660855508));
#70400=CARTESIAN_POINT('Ctrl Pts',(-0.0419392769977373,0.233437524125636,
-1.11762795217595));
#70401=CARTESIAN_POINT('Origin',(0.,0.,-2.1456589891905));
#70402=CARTESIAN_POINT('',(-0.0419392532630312,0.233437528389801,-0.998011590250681));
#70403=CARTESIAN_POINT('',(-0.0419392742985056,0.233437524610579,-1.01798096863704));
#70404=CARTESIAN_POINT('',(-0.0419392741328076,0.233437524640348,-2.1456589891905));
#70405=CARTESIAN_POINT('',(-0.237174906576387,-0.000216561049440317,-1.0759596619759));
#70406=CARTESIAN_POINT('Ctrl Pts',(-0.0419392532630312,0.233437528389801,
-0.998011590250681));
#70407=CARTESIAN_POINT('Ctrl Pts',(-0.0328874669837367,0.235063767152132,
-0.998582398995608));
#70408=CARTESIAN_POINT('Ctrl Pts',(-0.0237399095455045,0.236163749446927,
-0.999162446510492));
#70409=CARTESIAN_POINT('Ctrl Pts',(-0.0117150820866228,0.236902426277311,
-0.999943121146646));
#70410=CARTESIAN_POINT('Ctrl Pts',(-0.00888529964478573,0.237025427029939,
-1.00012810595657));
#70411=CARTESIAN_POINT('Ctrl Pts',(-0.00459355961697687,0.237135012956913,
-1.00041089930749));
#70412=CARTESIAN_POINT('Ctrl Pts',(-0.00313274574200432,0.237158809457264,
-1.00050754806663));
#70413=CARTESIAN_POINT('Ctrl Pts',(-0.000503092558483613,0.237177346185061,
-1.00068227607908));
#70414=CARTESIAN_POINT('Ctrl Pts',(0.000665673775309822,0.237176945422453,
-1.00076020087131));
#70415=CARTESIAN_POINT('Ctrl Pts',(0.0031639062113637,0.237157622880442,
-1.00092735495426));
#70416=CARTESIAN_POINT('Ctrl Pts',(0.00449330666895667,0.237136160175794,
-1.0010166611308));
#70417=CARTESIAN_POINT('Ctrl Pts',(0.00811331635866864,0.237047265398379,
-1.00126085386602));
#70418=CARTESIAN_POINT('Ctrl Pts',(0.0104031907509557,0.236957812520127,
-1.00141642198706));
#70419=CARTESIAN_POINT('Ctrl Pts',(0.0237280251643335,0.236243771607516,
-1.00232837531452));
#70420=CARTESIAN_POINT('Ctrl Pts',(0.0347081994711379,0.23488170362907,
-1.00310759731519));
#70421=CARTESIAN_POINT('Ctrl Pts',(0.0588262379710849,0.230161696597181,
-1.00487713424754));
#70422=CARTESIAN_POINT('Ctrl Pts',(0.0718536144925931,0.226433128616646,
-1.0058730389529));
#70423=CARTESIAN_POINT('Ctrl Pts',(0.0879627006156639,0.220291504277364,
-1.00712273880018));
#70424=CARTESIAN_POINT('Ctrl Pts',(0.0914027502905743,0.218886552590294,
-1.00739058174466));
#70425=CARTESIAN_POINT('Ctrl Pts',(0.0993298084682449,0.215429570417215,
-1.00800811535297));
#70426=CARTESIAN_POINT('Ctrl Pts',(0.103788904671347,0.213317092807266,
-1.00835574730141));
#70427=CARTESIAN_POINT('Ctrl Pts',(0.109317569090208,0.210483457707194,
-1.00878430518142));
#70428=CARTESIAN_POINT('Ctrl Pts',(0.11045121507942,0.209890795776027,-1.00887204592977));
#70429=CARTESIAN_POINT('Ctrl Pts',(0.112233930905165,0.208940361061796,
-1.00900974461437));
#70430=CARTESIAN_POINT('Ctrl Pts',(0.112886193875657,0.208588678977381,
-1.00906006667923));
#70431=CARTESIAN_POINT('Ctrl Pts',(0.114118953759951,0.207916532909453,
-1.00915504600153));
#70432=CARTESIAN_POINT('Ctrl Pts',(0.114699751484382,0.207596693819212,
-1.00919973801262));
#70433=CARTESIAN_POINT('Ctrl Pts',(0.116067848969686,0.20683580292801,-1.00930489253789));
#70434=CARTESIAN_POINT('Ctrl Pts',(0.116853983652413,0.206392687633389,
-1.00936522341963));
#70435=CARTESIAN_POINT('Ctrl Pts',(0.119462227481973,0.204902836565376,
-1.00956514516226));
#70436=CARTESIAN_POINT('Ctrl Pts',(0.121273014794954,0.203836338420617,
-1.00970354236594));
#70437=CARTESIAN_POINT('Ctrl Pts',(0.131743308685783,0.19748072948478,-1.01050288285373));
#70438=CARTESIAN_POINT('Ctrl Pts',(0.140071413345457,0.191663731318453,
-1.01113529800079));
#70439=CARTESIAN_POINT('Ctrl Pts',(0.162298854787571,0.173913233054972,
-1.01288810378387));
#70440=CARTESIAN_POINT('Ctrl Pts',(0.175225468907639,0.160881092991682,
-1.01399132006797));
#70441=CARTESIAN_POINT('Ctrl Pts',(0.189314454932511,0.142941964745945,
-1.01544937550471));
#70442=CARTESIAN_POINT('Ctrl Pts',(0.192001204241583,0.139312244378768,
-1.01574136463577));
#70443=CARTESIAN_POINT('Ctrl Pts',(0.195600069986374,0.134148276139748,
-1.0161539904859));
#70444=CARTESIAN_POINT('Ctrl Pts',(0.196601057594817,0.132676943118815,
-1.01627124952305));
#70445=CARTESIAN_POINT('Ctrl Pts',(0.198192752576374,0.130279772499474,
-1.01646187371813));
#70446=CARTESIAN_POINT('Ctrl Pts',(0.198793765030266,0.129360833377872,
-1.01653484985654));
#70447=CARTESIAN_POINT('Ctrl Pts',(0.200034976506164,0.127433961445204,
-1.01668768413772));
#70448=CARTESIAN_POINT('Ctrl Pts',(0.200673986662028,0.126425303410582,
-1.01676758368978));
#70449=CARTESIAN_POINT('Ctrl Pts',(0.202174203059067,0.124017225489281,
-1.01695811367661));
#70450=CARTESIAN_POINT('Ctrl Pts',(0.203028526391919,0.122613611947533,
-1.01706899272458));
#70451=CARTESIAN_POINT('Ctrl Pts',(0.205885862603953,0.117807392083154,
-1.01744813865333));
#70452=CARTESIAN_POINT('Ctrl Pts',(0.20781837154148,0.114363854616889,-1.0177189180925));
#70453=CARTESIAN_POINT('Ctrl Pts',(0.219716648575738,0.0918640554198085,
-1.01948368449075));
#70454=CARTESIAN_POINT('Ctrl Pts',(0.227135822621361,0.0715777870506341,
-1.0210676646075));
#70455=CARTESIAN_POINT('Ctrl Pts',(0.233598132377264,0.0419700644412308,
-1.02326742557111));
#70456=CARTESIAN_POINT('Ctrl Pts',(0.23499585202499,0.0332649769896782,
-1.02389934409235));
#70457=CARTESIAN_POINT('Ctrl Pts',(0.236043393156607,0.023178974833921,
-1.02460094339431));
#70458=CARTESIAN_POINT('Ctrl Pts',(0.236169624155886,0.0218553690253736,
-1.02469240976647));
#70459=CARTESIAN_POINT('Ctrl Pts',(0.236356611385386,0.0197033648891967,
-1.02484006372003));
#70460=CARTESIAN_POINT('Ctrl Pts',(0.236424156608383,0.0188756074999746,
-1.02489660416898));
#70461=CARTESIAN_POINT('Ctrl Pts',(0.236537241350122,0.0173937891702756,
-1.02499734619934));
#70462=CARTESIAN_POINT('Ctrl Pts',(0.236584418191094,0.0167398790147472,
-1.02504163600444));
#70463=CARTESIAN_POINT('Ctrl Pts',(0.236682271258211,0.0153004152245222,
-1.02513876471091));
#70464=CARTESIAN_POINT('Ctrl Pts',(0.236731748733401,0.0145148000579126,
-1.02519153676507));
#70465=CARTESIAN_POINT('Ctrl Pts',(0.236863814288344,0.0122371202018512,
-1.02534388401045));
#70466=CARTESIAN_POINT('Ctrl Pts',(0.236936215633787,0.0107444699588521,
-1.02544291363546));
#70467=CARTESIAN_POINT('Ctrl Pts',(0.237469744551497,-0.0029233337106176,
-1.02634311689417));
#70468=CARTESIAN_POINT('Ctrl Pts',(0.237006223732121,-0.0151182247785406,
-1.02709898877298));
#70469=CARTESIAN_POINT('Ctrl Pts',(0.233359895024032,-0.0466738801794996,
-1.02905165307747));
#70470=CARTESIAN_POINT('Ctrl Pts',(0.228713478205454,-0.0657674262803102,
-1.03023622671175));
#70471=CARTESIAN_POINT('Ctrl Pts',(0.220743706638506,-0.0867908284242931,
-1.03169214632821));
#70472=CARTESIAN_POINT('Ctrl Pts',(0.219663356922596,-0.0894898896017913,
-1.03188192031583));
#70473=CARTESIAN_POINT('Ctrl Pts',(0.217959888565634,-0.0935288615691752,
-1.03217058702827));
#70474=CARTESIAN_POINT('Ctrl Pts',(0.217373387079859,-0.0948839891306491,
-1.03226824490129));
#70475=CARTESIAN_POINT('Ctrl Pts',(0.216299479621054,-0.0973030578894326,
-1.03244407088623));
#70476=CARTESIAN_POINT('Ctrl Pts',(0.215816776624352,-0.098369043922167,
-1.03252207613908));
#70477=CARTESIAN_POINT('Ctrl Pts',(0.214773064428318,-0.100629281616406,
-1.03268861721428));
#70478=CARTESIAN_POINT('Ctrl Pts',(0.214209940200906,-0.10182250693968,
-1.03277722396807));
#70479=CARTESIAN_POINT('Ctrl Pts',(0.212661990869801,-0.105032836442447,
-1.03301751246413));
#70480=CARTESIAN_POINT('Ctrl Pts',(0.211658459310503,-0.107040716971319,
-1.03316983939445));
#70481=CARTESIAN_POINT('Ctrl Pts',(0.205973115019017,-0.118023390920689,
-1.03401460575423));
#70482=CARTESIAN_POINT('Ctrl Pts',(0.20074956863665,-0.126704399862393,
-1.03472602563159));
#70483=CARTESIAN_POINT('Ctrl Pts',(0.189266154706185,-0.143287568152088,
-1.03617331534723));
#70484=CARTESIAN_POINT('Ctrl Pts',(0.18302486906244,-0.151178304973489,
-1.03690751354357));
#70485=CARTESIAN_POINT('Ctrl Pts',(0.173555566406408,-0.161701292355227,
-1.03794124076664));
#70486=CARTESIAN_POINT('Ctrl Pts',(0.170729944624433,-0.164681904472389,
-1.03824078853653));
#70487=CARTESIAN_POINT('Ctrl Pts',(0.164127239337451,-0.171294090140551,
-1.03891885496641));
#70488=CARTESIAN_POINT('Ctrl Pts',(0.160304174530373,-0.174877082034531,
-1.03929623101419));
#70489=CARTESIAN_POINT('Ctrl Pts',(0.15338834197926,-0.180941078839783,
-1.03994880934473));
#70490=CARTESIAN_POINT('Ctrl Pts',(0.150346170124209,-0.183476677229564,
-1.04022635704779));
#70491=CARTESIAN_POINT('Ctrl Pts',(0.146309856512411,-0.186673028196065,
-1.04058098470663));
#70492=CARTESIAN_POINT('Ctrl Pts',(0.145372428358341,-0.187403977520671,
-1.04066242095296));
#70493=CARTESIAN_POINT('Ctrl Pts',(0.14385756255374,-0.188566970246504,
-1.04079248906902));
#70494=CARTESIAN_POINT('Ctrl Pts',(0.143283595865195,-0.189003470241006,
-1.04084142183044));
#70495=CARTESIAN_POINT('Ctrl Pts',(0.142172060499349,-0.189840816116179,
-1.040935499293));
#70496=CARTESIAN_POINT('Ctrl Pts',(0.141634773774766,-0.190242006716238,
-1.04098066637468));
#70497=CARTESIAN_POINT('Ctrl Pts',(0.14033329058457,-0.191205251109326,
-1.04108935274394));
#70498=CARTESIAN_POINT('Ctrl Pts',(0.139567398979925,-0.191765016926872,
-1.04115271534903));
#70499=CARTESIAN_POINT('Ctrl Pts',(0.136865470104579,-0.193715008495149,
-1.04137424095241));
#70500=CARTESIAN_POINT('Ctrl Pts',(0.134911779621053,-0.195080686425464,
-1.04153083019186));
#70501=CARTESIAN_POINT('Ctrl Pts',(0.130002484486339,-0.198403369614229,
-1.04191638085985));
#70502=CARTESIAN_POINT('Ctrl Pts',(0.127022900960986,-0.200324058481473,
-1.0421434049713));
#70503=CARTESIAN_POINT('Ctrl Pts',(0.113618141034676,-0.208545586738434,
-1.04313946943985));
#70504=CARTESIAN_POINT('Ctrl Pts',(0.102759146159512,-0.214104986261021,
-1.043880738825));
#70505=CARTESIAN_POINT('Ctrl Pts',(0.078353275357788,-0.224313287520356,
-1.0455031004654));
#70506=CARTESIAN_POINT('Ctrl Pts',(0.0647175072562258,-0.228620345060222,
-1.0463840388326));
#70507=CARTESIAN_POINT('Ctrl Pts',(0.047637347623109,-0.232363944843467,
-1.04751365270468));
#70508=CARTESIAN_POINT('Ctrl Pts',(0.0444829098911758,-0.232988387831591,
-1.0477232174863));
#70509=CARTESIAN_POINT('Ctrl Pts',(0.0398398767476725,-0.233809783016239,
-1.04803351471761));
#70510=CARTESIAN_POINT('Ctrl Pts',(0.0383604657410812,-0.234057054813062,
-1.04813265536811));
#70511=CARTESIAN_POINT('Ctrl Pts',(0.0357174050464013,-0.234473090029224,
-1.04831030406536));
#70512=CARTESIAN_POINT('Ctrl Pts',(0.0345546481487389,-0.234647265436907,
-1.04838863815601));
#70513=CARTESIAN_POINT('Ctrl Pts',(0.0321113181250426,-0.234994709920152,
-1.04855364629658));
#70514=CARTESIAN_POINT('Ctrl Pts',(0.0308305313350409,-0.235166172450584,
-1.04864037468291));
#70515=CARTESIAN_POINT('Ctrl Pts',(0.0274456383381947,-0.235591190419684,
-1.04887022494702));
#70516=CARTESIAN_POINT('Ctrl Pts',(0.025339465049543,-0.23582701937936,
-1.04901389887267));
#70517=CARTESIAN_POINT('Ctrl Pts',(0.0150790451899801,-0.236836847666536,
-1.04971719532552));
#70518=CARTESIAN_POINT('Ctrl Pts',(0.00689247701912053,-0.237216222349132,
-1.05028897335556));
#70519=CARTESIAN_POINT('Ctrl Pts',(-0.010935306595929,-0.237118764713752,
-1.05155725051427));
#70520=CARTESIAN_POINT('Ctrl Pts',(-0.0205611797539401,-0.23647854088466,
-1.05225689039217));
#70521=CARTESIAN_POINT('Ctrl Pts',(-0.0444813435801031,-0.233415938758958,
-1.05401705718686));
#70522=CARTESIAN_POINT('Ctrl Pts',(-0.058644734225539,-0.230266061917528,
-1.05507986613364));
#70523=CARTESIAN_POINT('Ctrl Pts',(-0.0743911535359679,-0.225215816699783,
-1.0562325388305));
#70524=CARTESIAN_POINT('Ctrl Pts',(-0.0763407755922364,-0.224562451259908,
-1.05637469061892));
#70525=CARTESIAN_POINT('Ctrl Pts',(-0.0790425019147395,-0.223617783371932,
-1.05657065681236));
#70526=CARTESIAN_POINT('Ctrl Pts',(-0.0798019216930037,-0.22334789788808,
-1.05662562681713));
#70527=CARTESIAN_POINT('Ctrl Pts',(-0.0811855277493801,-0.22284822878947,
-1.05672555160807));
#70528=CARTESIAN_POINT('Ctrl Pts',(-0.0818101510958803,-0.222619680649577,
-1.05677057736536));
#70529=CARTESIAN_POINT('Ctrl Pts',(-0.0831057230684105,-0.222139444714125,
-1.05686378099344));
#70530=CARTESIAN_POINT('Ctrl Pts',(-0.0837765028109168,-0.221887340143546,
-1.05691193388252));
#70531=CARTESIAN_POINT('Ctrl Pts',(-0.0854211649531455,-0.221260692146922,
-1.05702976892045));
#70532=CARTESIAN_POINT('Ctrl Pts',(-0.0863937492568763,-0.22088275057311,
-1.05709925327053));
#70533=CARTESIAN_POINT('Ctrl Pts',(-0.0906408796508328,-0.219199991934776,
-1.05740194390823));
#70534=CARTESIAN_POINT('Ctrl Pts',(-0.0938887913882238,-0.217828610614234,
-1.05763149561957));
#70535=CARTESIAN_POINT('Ctrl Pts',(-0.102762227709214,-0.213846563826903,
-1.05825650708259));
#70536=CARTESIAN_POINT('Ctrl Pts',(-0.108318012812955,-0.211086824224093,
-1.05864544888771));
#70537=CARTESIAN_POINT('Ctrl Pts',(-0.130906403136762,-0.198739422430882,
-1.06024208565324));
#70538=CARTESIAN_POINT('Ctrl Pts',(-0.146828358876324,-0.187283951886437,
-1.06141161880125));
#70539=CARTESIAN_POINT('Ctrl Pts',(-0.164933380982727,-0.170514934803155,
-1.06298236528416));
#70540=CARTESIAN_POINT('Ctrl Pts',(-0.16858711682625,-0.166903388366593,
-1.06331349972926));
#70541=CARTESIAN_POINT('Ctrl Pts',(-0.173407270164107,-0.161819025781277,
-1.06377224666388));
#70542=CARTESIAN_POINT('Ctrl Pts',(-0.174677868838246,-0.16044662743858,
-1.06389536941813));
#70543=CARTESIAN_POINT('Ctrl Pts',(-0.176679745124417,-0.158232396170375,
-1.06409298896214));
#70544=CARTESIAN_POINT('Ctrl Pts',(-0.177421564252611,-0.157400165186986,
-1.06416703895057));
#70545=CARTESIAN_POINT('Ctrl Pts',(-0.178938429395325,-0.155674078535312,
-1.06432017840648));
#70546=CARTESIAN_POINT('Ctrl Pts',(-0.179712708512583,-0.15477959346681,
-1.0643992967408));
#70547=CARTESIAN_POINT('Ctrl Pts',(-0.18150325000867,-0.152679523876297,
-1.06458451566304));
#70548=CARTESIAN_POINT('Ctrl Pts',(-0.182514236298725,-0.15146953526645,
-1.06469082797053));
#70549=CARTESIAN_POINT('Ctrl Pts',(-0.185601172969272,-0.147699187317175,
-1.065020919775));
#70550=CARTESIAN_POINT('Ctrl Pts',(-0.187635793692647,-0.145105659311154,
-1.0652463335768));
#70551=CARTESIAN_POINT('Ctrl Pts',(-0.195901245011749,-0.134105089604968,
-1.06619612266519));
#70552=CARTESIAN_POINT('Ctrl Pts',(-0.201625529367028,-0.125333820426734,
-1.06693914961871));
#70553=CARTESIAN_POINT('Ctrl Pts',(-0.211529526301638,-0.107714086486119,
-1.06839988381389));
#70554=CARTESIAN_POINT('Ctrl Pts',(-0.215778630985866,-0.0989274259154191,
-1.06911441030379));
#70555=CARTESIAN_POINT('Ctrl Pts',(-0.223585882280169,-0.0798683966845085,
-1.07061571497298));
#70556=CARTESIAN_POINT('Ctrl Pts',(-0.227004321879618,-0.0695607733970581,
-1.07139992012034));
#70557=CARTESIAN_POINT('Ctrl Pts',(-0.230042881720824,-0.0577415812437741,
-1.07224462298994));
#70558=CARTESIAN_POINT('Ctrl Pts',(-0.230369105492029,-0.0564259965188515,
-1.07233789547921));
#70559=CARTESIAN_POINT('Ctrl Pts',(-0.230878795950737,-0.0542924006237782,
-1.07248787250035));
#70560=CARTESIAN_POINT('Ctrl Pts',(-0.231069229930386,-0.0534761088608329,
-1.07254494774915));
#70561=CARTESIAN_POINT('Ctrl Pts',(-0.231400995248288,-0.0520191351557926,
-1.07264625677788));
#70562=CARTESIAN_POINT('Ctrl Pts',(-0.231543999827295,-0.0513788594957119,
-1.072690583158));
#70563=CARTESIAN_POINT('Ctrl Pts',(-0.231851421600686,-0.0499750822061432,
-1.07278733957547));
#70564=CARTESIAN_POINT('Ctrl Pts',(-0.232014725645907,-0.0492113570970241,
-1.07283970641063));
#70565=CARTESIAN_POINT('Ctrl Pts',(-0.232345548010314,-0.0476259397672956,
-1.07294787467687));
#70566=CARTESIAN_POINT('Ctrl Pts',(-0.232512487172898,-0.046804136345465,
-1.0730036439289));
#70567=CARTESIAN_POINT('Ctrl Pts',(-0.232934153392311,-0.044670423374128,
-1.07314770599847));
#70568=CARTESIAN_POINT('Ctrl Pts',(-0.233182161286192,-0.0433571953696926,
-1.07323565141276));
#70569=CARTESIAN_POINT('Ctrl Pts',(-0.235904953605221,-0.02824009707736,
-1.07424050055651));
#70570=CARTESIAN_POINT('Ctrl Pts',(-0.237162096468213,-0.0142434182445045,
-1.07509988565631));
#70571=CARTESIAN_POINT('Ctrl Pts',(-0.237174901177882,-0.000216509264792025,
-1.07595967459035));
#70572=CARTESIAN_POINT('Ctrl Pts',(-0.237174901130082,-0.000216561620945157,
-1.07595967138114));
#70573=CARTESIAN_POINT('Ctrl Pts',(-0.237189705431092,0.0159968773670292,
-1.07695348516814));
#70574=CARTESIAN_POINT('Ctrl Pts',(-0.235542040756606,0.0321678926258792,
-1.07794491344652));
#70575=CARTESIAN_POINT('Ctrl Pts',(-0.23176777968398,0.0504135968378846,
-1.07914569342658));
#70576=CARTESIAN_POINT('Ctrl Pts',(-0.231241459655458,0.0527751940790963,
-1.07930264939856));
#70577=CARTESIAN_POINT('Ctrl Pts',(-0.230326963019487,0.056601820864279,
-1.07955971121239));
#70578=CARTESIAN_POINT('Ctrl Pts',(-0.229960703405532,0.0580719444617723,
-1.07965913188476));
#70579=CARTESIAN_POINT('Ctrl Pts',(-0.229223751514469,0.0609136334579724,
-1.07985265145588));
#70580=CARTESIAN_POINT('Ctrl Pts',(-0.228854769686687,0.0622855781284844,
-1.07994669231565));
#70581=CARTESIAN_POINT('Ctrl Pts',(-0.228160513377715,0.0647774704341915,
-1.08011865490051));
#70582=CARTESIAN_POINT('Ctrl Pts',(-0.227839259636772,0.0658984994159516,
-1.0801964439192));
#70583=CARTESIAN_POINT('Ctrl Pts',(-0.227125513974596,0.0683215244334877,
-1.08036553061352));
#70584=CARTESIAN_POINT('Ctrl Pts',(-0.226730067126667,0.0696225992475412,
-1.0804569224322));
#70585=CARTESIAN_POINT('Ctrl Pts',(-0.225615527623977,0.0731793646603695,
-1.08070844333898));
#70586=CARTESIAN_POINT('Ctrl Pts',(-0.224873830338733,0.0754277497807674,
-1.08086930698658));
#70587=CARTESIAN_POINT('Ctrl Pts',(-0.22021373697241,0.0888742967680971,
-1.08184294133655));
#70588=CARTESIAN_POINT('Ctrl Pts',(-0.215493881720441,0.0997749392634271,
-1.08268214585097));
#70589=CARTESIAN_POINT('Ctrl Pts',(-0.20511130094733,0.119544773962779,
-1.08429505731352));
#70590=CARTESIAN_POINT('Ctrl Pts',(-0.199634968243343,0.12848137665573,
-1.08506290981648));
#70591=CARTESIAN_POINT('Ctrl Pts',(-0.187760438733647,0.145257311659727,
-1.08655983209413));
#70592=CARTESIAN_POINT('Ctrl Pts',(-0.181414726954496,0.153109151133245,
-1.08728768669437));
#70593=CARTESIAN_POINT('Ctrl Pts',(-0.173496847363707,0.161720196384054,
-1.08809896660234));
#70594=CARTESIAN_POINT('Ctrl Pts',(-0.172393903535983,0.162895427631929,
-1.08820998287201));
#70595=CARTESIAN_POINT('Ctrl Pts',(-0.170818043531506,0.164540635583799,
-1.08836569809185));
#70596=CARTESIAN_POINT('Ctrl Pts',(-0.170355025013027,0.165019969198535,
-1.08841110296346));
#70597=CARTESIAN_POINT('Ctrl Pts',(-0.169424678355614,0.165975009130238,
-1.08850163178614));
#70598=CARTESIAN_POINT('Ctrl Pts',(-0.168957350123588,0.166450710954488,
-1.08854675488551));
#70599=CARTESIAN_POINT('Ctrl Pts',(-0.16797443054146,0.167442837392409,
-1.08864091991015));
#70600=CARTESIAN_POINT('Ctrl Pts',(-0.167458456231117,0.16795885979261,
-1.08868993110858));
#70601=CARTESIAN_POINT('Ctrl Pts',(-0.166067952773326,0.169336715430872,
-1.08882091867736));
#70602=CARTESIAN_POINT('Ctrl Pts',(-0.165189084824151,0.170194167196048,
-1.08890256112305));
#70603=CARTESIAN_POINT('Ctrl Pts',(-0.161167755970908,0.174057007744811,
-1.0892711727207));
#70604=CARTESIAN_POINT('Ctrl Pts',(-0.157949453299136,0.17698266422769,
-1.08955261297817));
#70605=CARTESIAN_POINT('Ctrl Pts',(-0.142864086655325,0.189956790708876,
-1.09082134948087));
#70606=CARTESIAN_POINT('Ctrl Pts',(-0.130106477553162,0.198912351494917,
-1.09175869978726));
#70607=CARTESIAN_POINT('Ctrl Pts',(-0.108842398924777,0.210912074384467,
-1.0932610700988));
#70608=CARTESIAN_POINT('Ctrl Pts',(-0.100884075607825,0.214832389749444,
-1.09381122744024));
#70609=CARTESIAN_POINT('Ctrl Pts',(-0.0893760010614183,0.219720628298945,
-1.09460603843072));
#70610=CARTESIAN_POINT('Ctrl Pts',(-0.0859943345376999,0.221066045291664,
-1.09483945884671));
#70611=CARTESIAN_POINT('Ctrl Pts',(-0.07993135007801,0.223318074355819,
-1.09525871385966));
#70612=CARTESIAN_POINT('Ctrl Pts',(-0.0772622037864236,0.224255510103424,
-1.095443537421));
#70613=CARTESIAN_POINT('Ctrl Pts',(-0.0732085240462829,0.225598251084243,
-1.09572492300848));
#70614=CARTESIAN_POINT('Ctrl Pts',(-0.0718359505443863,0.226039056226831,
-1.09582031734134));
#70615=CARTESIAN_POINT('Ctrl Pts',(-0.0693448632070169,0.226814093862479,
-1.09599370101598));
#70616=CARTESIAN_POINT('Ctrl Pts',(-0.0682277300479967,0.227152635900668,
-1.09607154634389));
#70617=CARTESIAN_POINT('Ctrl Pts',(-0.0658197149485878,0.227863007776267,
-1.09623956181735));
#70618=CARTESIAN_POINT('Ctrl Pts',(-0.0645280872643494,0.228232142814565,
-1.09632981677997));
#70619=CARTESIAN_POINT('Ctrl Pts',(-0.0610221660207296,0.22920196260782,
-1.09657519654198));
#70620=CARTESIAN_POINT('Ctrl Pts',(-0.0588022272735147,0.229781508898124,
-1.09673099792073));
#70621=CARTESIAN_POINT('Ctrl Pts',(-0.0517282751309758,0.231519042232843,
-1.0972289725201));
#70622=CARTESIAN_POINT('Ctrl Pts',(-0.0468474911537617,0.232555716920545,
-1.097574825708));
#70623=CARTESIAN_POINT('Ctrl Pts',(-0.0419392646935193,0.233437526336206,
-1.0979250019446));
#70624=CARTESIAN_POINT('',(-0.237174998221465,2.9045624302765E-5,-1.09587916587548));
#70625=CARTESIAN_POINT('Ctrl Pts',(-0.0419392769977373,0.233437524125636,
-1.11762795217595));
#70626=CARTESIAN_POINT('Ctrl Pts',(-0.0513124259767892,0.231753548540109,
-1.11701686568024));
#70627=CARTESIAN_POINT('Ctrl Pts',(-0.0605790275699475,0.229505954888564,
-1.11642777064907));
#70628=CARTESIAN_POINT('Ctrl Pts',(-0.0879950868366662,0.221078376363219,
-1.11466574714866));
#70629=CARTESIAN_POINT('Ctrl Pts',(-0.105550654404818,0.213255150629247,
-1.11350513299769));
#70630=CARTESIAN_POINT('Ctrl Pts',(-0.124485368601723,0.201900837211246,
-1.11207603739078));
#70631=CARTESIAN_POINT('Ctrl Pts',(-0.126968473698413,0.200348597502796,
-1.1118849554608));
#70632=CARTESIAN_POINT('Ctrl Pts',(-0.130674118200915,0.197935564341248,
-1.11159383872476));
#70633=CARTESIAN_POINT('Ctrl Pts',(-0.131918361143883,0.19710849454021,
-1.11149505217501));
#70634=CARTESIAN_POINT('Ctrl Pts',(-0.134100395479711,0.195628143615694,
-1.11131992125608));
#70635=CARTESIAN_POINT('Ctrl Pts',(-0.135041443410467,0.194979730037483,
-1.11124376235253));
#70636=CARTESIAN_POINT('Ctrl Pts',(-0.136110315901974,0.194231791184795,
-1.11115652475097));
#70637=CARTESIAN_POINT('Ctrl Pts',(-0.136242782026103,0.194138896533777,
-1.11114570038463));
#70638=CARTESIAN_POINT('Ctrl Pts',(-0.136434573915127,0.194004105473234,
-1.11113000944803));
#70639=CARTESIAN_POINT('Ctrl Pts',(-0.136493975877539,0.19396231708503,
-1.11112514701839));
#70640=CARTESIAN_POINT('Ctrl Pts',(-0.136596076258444,0.193890420870757,
-1.11111678494384));
#70641=CARTESIAN_POINT('Ctrl Pts',(-0.136638783968,0.193860326189709,-1.11111328580322));
#70642=CARTESIAN_POINT('Ctrl Pts',(-0.136713822532998,0.193807411931112,
-1.11110713533475));
#70643=CARTESIAN_POINT('Ctrl Pts',(-0.136746157640387,0.193784598360156,
-1.11110448423746));
#70644=CARTESIAN_POINT('Ctrl Pts',(-0.136803821010411,0.193743893177523,
-1.1110997551306));
#70645=CARTESIAN_POINT('Ctrl Pts',(-0.136829151483132,0.193726004684545,
-1.11109767724079));
#70646=CARTESIAN_POINT('Ctrl Pts',(-0.136874810623106,0.193693746573373,
-1.11109393090156));
#70647=CARTESIAN_POINT('Ctrl Pts',(-0.136895140541188,0.193679378718925,
-1.11109226251991));
#70648=CARTESIAN_POINT('Ctrl Pts',(-0.13693208422009,0.193653260623795,
-1.11108923016277));
#70649=CARTESIAN_POINT('Ctrl Pts',(-0.136948698734297,0.193641511443357,
-1.11108786622799));
#70650=CARTESIAN_POINT('Ctrl Pts',(-0.137008028291522,0.193599544282447,
-1.11108299495096));
#70651=CARTESIAN_POINT('Ctrl Pts',(-0.137050734821078,0.193569314323569,
-1.11107948714864));
#70652=CARTESIAN_POINT('Ctrl Pts',(-0.137134931478892,0.193509673607565,
-1.11107256876076));
#70653=CARTESIAN_POINT('Ctrl Pts',(-0.137176422159569,0.193480263631512,
-1.11106915820536));
#70654=CARTESIAN_POINT('Ctrl Pts',(-0.13725849991559,0.193422044512001,
-1.11106240881374));
#70655=CARTESIAN_POINT('Ctrl Pts',(-0.137299087389185,0.193393235932311,
-1.11105906999934));
#70656=CARTESIAN_POINT('Ctrl Pts',(-0.137379628812475,0.193336030307493,
-1.1110524420258));
#70657=CARTESIAN_POINT('Ctrl Pts',(-0.137419583034138,0.193307633647589,
-1.11104915288157));
#70658=CARTESIAN_POINT('Ctrl Pts',(-0.13749909645943,0.193251083969447,
-1.1110426047171));
#70659=CARTESIAN_POINT('Ctrl Pts',(-0.137538655827348,0.193222931185007,
-1.11103934570595));
#70660=CARTESIAN_POINT('Ctrl Pts',(-0.13761759481541,0.193166717009997,
-1.11103284013317));
#70661=CARTESIAN_POINT('Ctrl Pts',(-0.137656974504486,0.193138655720351,
-1.11102959357555));
#70662=CARTESIAN_POINT('Ctrl Pts',(-0.13773575257702,0.193082483486986,
-1.11102309657168));
#70663=CARTESIAN_POINT('Ctrl Pts',(-0.137775150942949,0.193054372522619,
-1.11101984612473));
#70664=CARTESIAN_POINT('Ctrl Pts',(-0.13907151442299,0.192128810646984,
-1.11091285472892));
#70665=CARTESIAN_POINT('Ctrl Pts',(-0.140319665436949,0.191219134239798,
-1.11080864375046));
#70666=CARTESIAN_POINT('Ctrl Pts',(-0.144603356338511,0.188032572701308,
-1.11044675414118));
#70667=CARTESIAN_POINT('Ctrl Pts',(-0.147592942604134,0.185695178882195,
-1.11018673188702));
#70668=CARTESIAN_POINT('Ctrl Pts',(-0.160659273511638,0.174964424376129,
-1.10901576787797));
#70669=CARTESIAN_POINT('Ctrl Pts',(-0.170084274352997,0.16581675588369,
-1.10807502211549));
#70670=CARTESIAN_POINT('Ctrl Pts',(-0.189708403693762,0.143327719309288,
-1.10590185709727));
#70671=CARTESIAN_POINT('Ctrl Pts',(-0.1993476841613,0.129586623932666,-1.10466559195508));
#70672=CARTESIAN_POINT('Ctrl Pts',(-0.20837924384152,0.113285773984156,
-1.1033690331386));
#70673=CARTESIAN_POINT('Ctrl Pts',(-0.209278287117749,0.111616194890113,
-1.10323812199244));
#70674=CARTESIAN_POINT('Ctrl Pts',(-0.210554283924761,0.109176956607938,
-1.10304977434837));
#70675=CARTESIAN_POINT('Ctrl Pts',(-0.21094721557263,0.108415804351397,
-1.10299140818392));
#70676=CARTESIAN_POINT('Ctrl Pts',(-0.211635058066689,0.107065479343845,
-1.10288860314279));
#70677=CARTESIAN_POINT('Ctrl Pts',(-0.21193164910076,0.106477184508045,
-1.10284406175229));
#70678=CARTESIAN_POINT('Ctrl Pts',(-0.212564060930533,0.105209670138415,
-1.10274863118305));
#70679=CARTESIAN_POINT('Ctrl Pts',(-0.212899081064536,0.10453007228669,
-1.10269779118598));
#70680=CARTESIAN_POINT('Ctrl Pts',(-0.213824737935954,0.102629439193682,
-1.10255648343408));
#70681=CARTESIAN_POINT('Ctrl Pts',(-0.2144081771224,0.101404901954349,-1.10246644628672));
#70682=CARTESIAN_POINT('Ctrl Pts',(-0.217940070430203,0.0938252929915238,
-1.1019148907721));
#70683=CARTESIAN_POINT('Ctrl Pts',(-0.22061656241397,0.0873465121088174,
-1.1014682033649));
#70684=CARTESIAN_POINT('Ctrl Pts',(-0.229720042864398,0.0622084831613126,
-1.09979318034984));
#70685=CARTESIAN_POINT('Ctrl Pts',(-0.234097051542799,0.0428932200546185,
-1.09861844446422));
#70686=CARTESIAN_POINT('Ctrl Pts',(-0.236542681461396,0.0180741705037209,
-1.0970467851354));
#70687=CARTESIAN_POINT('Ctrl Pts',(-0.236882552585845,0.0128750230385105,
-1.09671465885293));
#70688=CARTESIAN_POINT('Ctrl Pts',(-0.237133342782771,0.00512319446735597,
-1.09621256739257));
#70689=CARTESIAN_POINT('Ctrl Pts',(-0.237174686289266,0.00257615970376124,
-1.09604649594697));
#70690=CARTESIAN_POINT('Ctrl Pts',(-0.237174998221465,2.9045624302765E-5,
-1.09587916587548));
#70691=CARTESIAN_POINT('Ctrl Pts',(-0.237174998234998,2.89349044827048E-5,
-1.09587915860185));
#70692=CARTESIAN_POINT('Ctrl Pts',(-0.237175091574553,-0.000736155186613617,
-1.09582889677479));
#70693=CARTESIAN_POINT('Ctrl Pts',(-0.237171482819,-0.00150123555575333,
-1.09577852271994));
#70694=CARTESIAN_POINT('Ctrl Pts',(-0.23715504772398,-0.00322115387109381,
-1.09566501874773));
#70695=CARTESIAN_POINT('Ctrl Pts',(-0.237140156594989,-0.00417595238553839,
-1.09560182641588));
#70696=CARTESIAN_POINT('Ctrl Pts',(-0.237095373510457,-0.00624567023885131,
-1.09546443665023));
#70697=CARTESIAN_POINT('Ctrl Pts',(-0.237063382370882,-0.00736051648109467,
-1.0953901755463));
#70698=CARTESIAN_POINT('Ctrl Pts',(-0.236978720384648,-0.00972826804894033,
-1.0952318923194));
#70699=CARTESIAN_POINT('Ctrl Pts',(-0.236923973729274,-0.0109810601484171,
-1.09514780747047));
#70700=CARTESIAN_POINT('Ctrl Pts',(-0.236762754412604,-0.0141025542018507,
-1.09493743284993));
#70701=CARTESIAN_POINT('Ctrl Pts',(-0.236644091988894,-0.0159705130882173,
-1.09481076574039));
#70702=CARTESIAN_POINT('Ctrl Pts',(-0.236094200314016,-0.0232616765908722,
-1.0943132047075));
#70703=CARTESIAN_POINT('Ctrl Pts',(-0.235498567749214,-0.0286704243256552,
-1.09393724537711));
#70704=CARTESIAN_POINT('Ctrl Pts',(-0.2340185606868,-0.0388715235886166,
-1.09321467972771));
#70705=CARTESIAN_POINT('Ctrl Pts',(-0.233171416259019,-0.0436665498414046,
-1.0928693168324));
#70706=CARTESIAN_POINT('Ctrl Pts',(-0.227849219730846,-0.0691806141151254,
-1.09100251286758));
#70707=CARTESIAN_POINT('Ctrl Pts',(-0.2207598883747,-0.089253678435357,
-1.08941896474834));
#70708=CARTESIAN_POINT('Ctrl Pts',(-0.209741828236302,-0.110766449464546,
-1.08771852858905));
#70709=CARTESIAN_POINT('Ctrl Pts',(-0.208335094052613,-0.113390173611633,
-1.08751128898664));
#70710=CARTESIAN_POINT('Ctrl Pts',(-0.20637403424456,-0.116888005894681,
-1.08723588371031));
#70711=CARTESIAN_POINT('Ctrl Pts',(-0.205862915114923,-0.117785857436639,
-1.08716526998915));
#70712=CARTESIAN_POINT('Ctrl Pts',(-0.205002201128749,-0.119275102290707,
-1.08704831370501));
#70713=CARTESIAN_POINT('Ctrl Pts',(-0.204655879845547,-0.119868358521215,
-1.0870017680091));
#70714=CARTESIAN_POINT('Ctrl Pts',(-0.203995683534527,-0.12098808778858,
-1.08691401392839));
#70715=CARTESIAN_POINT('Ctrl Pts',(-0.203682337780679,-0.121514861582823,
-1.08687277112295));
#70716=CARTESIAN_POINT('Ctrl Pts',(-0.202851360180702,-0.12289959441002,
-1.08676444763731));
#70717=CARTESIAN_POINT('Ctrl Pts',(-0.202330320372337,-0.123755509700915,
-1.0866975851608));
#70718=CARTESIAN_POINT('Ctrl Pts',(-0.200466677005719,-0.126773695326562,
-1.08646204580914));
#70719=CARTESIAN_POINT('Ctrl Pts',(-0.199094655138995,-0.128917717934579,
-1.08629515694414));
#70720=CARTESIAN_POINT('Ctrl Pts',(-0.188870209299772,-0.144342501461747,
-1.08509445881174));
#70721=CARTESIAN_POINT('Ctrl Pts',(-0.178730613517719,-0.156723374597824,
-1.08412848094404));
#70722=CARTESIAN_POINT('Ctrl Pts',(-0.157112003028982,-0.178268626637153,
-1.08225579875219));
#70723=CARTESIAN_POINT('Ctrl Pts',(-0.145878519487975,-0.187572023640914,
-1.08135497780248));
#70724=CARTESIAN_POINT('Ctrl Pts',(-0.132277133420145,-0.196871623893918,
-1.08028575335904));
#70725=CARTESIAN_POINT('Ctrl Pts',(-0.130677092782299,-0.197937296623947,
-1.08016032714827));
#70726=CARTESIAN_POINT('Ctrl Pts',(-0.127964092362337,-0.199696999049357,
-1.07994813762921));
#70727=CARTESIAN_POINT('Ctrl Pts',(-0.126857992604295,-0.200401471953222,
-1.07986175943789));
#70728=CARTESIAN_POINT('Ctrl Pts',(-0.124681395355753,-0.201762501937129,
-1.07969200504493));
#70729=CARTESIAN_POINT('Ctrl Pts',(-0.123611412024013,-0.202419802020645,
-1.07960865960593));
#70730=CARTESIAN_POINT('Ctrl Pts',(-0.121575919518454,-0.203648065363674,
-1.07945027477432));
#70731=CARTESIAN_POINT('Ctrl Pts',(-0.120611478102009,-0.204220738439006,
-1.07937530062942));
#70732=CARTESIAN_POINT('Ctrl Pts',(-0.118339985056488,-0.205547819302834,
-1.07919886278744));
#70733=CARTESIAN_POINT('Ctrl Pts',(-0.117029735858778,-0.206296628243834,
-1.07909720025318));
#70734=CARTESIAN_POINT('Ctrl Pts',(-0.113094023585103,-0.208496331788863,
-1.07879210453458));
#70735=CARTESIAN_POINT('Ctrl Pts',(-0.110448173802008,-0.209909928318222,
-1.07858735915639));
#70736=CARTESIAN_POINT('Ctrl Pts',(-0.0913656990865444,-0.219644442121292,
-1.07711260343937));
#70737=CARTESIAN_POINT('Ctrl Pts',(-0.0740385308444054,-0.226073912500243,
-1.075776182441));
#70738=CARTESIAN_POINT('Ctrl Pts',(-0.0525204209895835,-0.231316911483036,
-1.07415868752096));
#70739=CARTESIAN_POINT('Ctrl Pts',(-0.0488741492114006,-0.232114683593674,
-1.07388628746343));
#70740=CARTESIAN_POINT('Ctrl Pts',(-0.0388544078163394,-0.234060332633326,
-1.07314424345131));
#70741=CARTESIAN_POINT('Ctrl Pts',(-0.032449957179367,-0.235033861177777,
-1.07267700638897));
#70742=CARTESIAN_POINT('Ctrl Pts',(-0.0223970304159877,-0.236143156378797,
-1.07196153656108));
#70743=CARTESIAN_POINT('Ctrl Pts',(-0.0187718046415923,-0.236458960940458,
-1.07170715473292));
#70744=CARTESIAN_POINT('Ctrl Pts',(-0.0140312424593468,-0.236762202170247,
-1.07138041968398));
#70745=CARTESIAN_POINT('Ctrl Pts',(-0.0129214589011289,-0.23682536216366,
-1.07130435196625));
#70746=CARTESIAN_POINT('Ctrl Pts',(-0.0111082135382834,-0.236915773428376,
-1.07118080037567));
#70747=CARTESIAN_POINT('Ctrl Pts',(-0.0104050176440958,-0.236947698338747,
-1.07113306575395));
#70748=CARTESIAN_POINT('Ctrl Pts',(-0.00903007294455535,-0.237003987767055,
-1.07104009660934));
#70749=CARTESIAN_POINT('Ctrl Pts',(-0.00835834786370987,-0.237028627961647,
-1.07099484813483));
#70750=CARTESIAN_POINT('Ctrl Pts',(-0.00685271293237036,-0.237077449192227,
-1.07089379231548));
#70751=CARTESIAN_POINT('Ctrl Pts',(-0.0060187534657266,-0.237100086986591,
-1.07083806979067));
#70752=CARTESIAN_POINT('Ctrl Pts',(-0.00310644659155155,-0.237163765609716,
-1.07064430234653));
#70753=CARTESIAN_POINT('Ctrl Pts',(-0.0010276219452319,-0.237181884733494,
-1.07050745403679));
#70754=CARTESIAN_POINT('Ctrl Pts',(0.0130863627277286,-0.237119325070918,
-1.06958664053427));
#70755=CARTESIAN_POINT('Ctrl Pts',(0.0251015762151883,-0.236149978756105,
-1.06884324054553));
#70756=CARTESIAN_POINT('Ctrl Pts',(0.0475138118662097,-0.23261099535582,
-1.06745032962378));
#70757=CARTESIAN_POINT('Ctrl Pts',(0.0579110556338668,-0.230242781766925,
-1.06680137983303));
#70758=CARTESIAN_POINT('Ctrl Pts',(0.0770815438338459,-0.224495144659416,
-1.06555484079948));
#70759=CARTESIAN_POINT('Ctrl Pts',(0.0858814662879557,-0.221278053191992,
-1.06496173061427));
#70760=CARTESIAN_POINT('Ctrl Pts',(0.0964852814027841,-0.216673509714544,
-1.06420766652896));
#70761=CARTESIAN_POINT('Ctrl Pts',(0.0984906270219844,-0.215769356475152,
-1.06406328178946));
#70762=CARTESIAN_POINT('Ctrl Pts',(0.101669132734447,-0.214282716537924,
-1.06383142868202));
#70763=CARTESIAN_POINT('Ctrl Pts',(0.102850577795691,-0.213718164151304,
-1.06374457868879));
#70764=CARTESIAN_POINT('Ctrl Pts',(0.105079993683318,-0.212630072589506,
-1.06357938474551));
#70765=CARTESIAN_POINT('Ctrl Pts',(0.10612888203209,-0.212108493831807,
-1.06350111096879));
#70766=CARTESIAN_POINT('Ctrl Pts',(0.10850479443007,-0.210904993185594,
-1.06332252101537));
#70767=CARTESIAN_POINT('Ctrl Pts',(0.109829323046227,-0.210218282237729,
-1.06322203890897));
#70768=CARTESIAN_POINT('Ctrl Pts',(0.113875523225334,-0.208071824061476,
-1.06291218950026));
#70769=CARTESIAN_POINT('Ctrl Pts',(0.116575139732711,-0.206571425869621,
-1.06270139366936));
#70770=CARTESIAN_POINT('Ctrl Pts',(0.134940388899677,-0.195889691099852,
-1.06123844749755));
#70771=CARTESIAN_POINT('Ctrl Pts',(0.149533093597661,-0.184989972385553,
-1.05992212966255));
#70772=CARTESIAN_POINT('Ctrl Pts',(0.165544430822195,-0.169887944322956,
-1.05831462477069));
#70773=CARTESIAN_POINT('Ctrl Pts',(0.168286668523524,-0.167171977485508,
-1.05803288850312));
#70774=CARTESIAN_POINT('Ctrl Pts',(0.175495847398169,-0.159674626734347,
-1.05727656477406));
#70775=CARTESIAN_POINT('Ctrl Pts',(0.179833520130493,-0.154773044979963,
-1.0568043292003));
#70776=CARTESIAN_POINT('Ctrl Pts',(0.186275209715283,-0.146856884427125,
-1.05608221386023));
#70777=CARTESIAN_POINT('Ctrl Pts',(0.18852122677911,-0.143962317855598,
-1.05582606020811));
#70778=CARTESIAN_POINT('Ctrl Pts',(0.19136190051001,-0.140120823239754,
-1.05549742024885));
#70779=CARTESIAN_POINT('Ctrl Pts',(0.192018065215006,-0.139220274481664,
-1.05542116715528));
#70780=CARTESIAN_POINT('Ctrl Pts',(0.193078717955802,-0.137742824145694,
-1.055297390978));
#70781=CARTESIAN_POINT('Ctrl Pts',(0.193487015613042,-0.137168698154314,
-1.05524961546611));
#70782=CARTESIAN_POINT('Ctrl Pts',(0.194279639560536,-0.1360435722647,-1.05515663142343));
#70783=CARTESIAN_POINT('Ctrl Pts',(0.194664191553741,-0.135492746839748,
-1.05511140850166));
#70784=CARTESIAN_POINT('Ctrl Pts',(0.195520196121846,-0.134255454313557,
-1.05501047662591));
#70785=CARTESIAN_POINT('Ctrl Pts',(0.195990388869477,-0.133568116058034,
-1.05495485181618));
#70786=CARTESIAN_POINT('Ctrl Pts',(0.197616678398928,-0.131163691172546,
-1.05476175725491));
#70787=CARTESIAN_POINT('Ctrl Pts',(0.198753948395189,-0.129433898867819,
-1.05462547325677));
#70788=CARTESIAN_POINT('Ctrl Pts',(0.206427772586406,-0.117422283885265,
-1.05369545313188));
#70789=CARTESIAN_POINT('Ctrl Pts',(0.212187092026569,-0.106663643226348,
-1.05294336708235));
#70790=CARTESIAN_POINT('Ctrl Pts',(0.22148826207626,-0.0855217818231289,
-1.05152570006612));
#70791=CARTESIAN_POINT('Ctrl Pts',(0.225187494961732,-0.0752436529550886,
-1.05086090103726));
#70792=CARTESIAN_POINT('Ctrl Pts',(0.230625826470045,-0.0560794113212364,
-1.04961829083679));
#70793=CARTESIAN_POINT('Ctrl Pts',(0.232589460107917,-0.0472788204214101,
-1.04904664657693));
#70794=CARTESIAN_POINT('Ctrl Pts',(0.234400022564185,-0.0362401678811255,
-1.04831681355707));
#70795=CARTESIAN_POINT('Ctrl Pts',(0.234722793368587,-0.034087095810669,
-1.04817388664357));
#70796=CARTESIAN_POINT('Ctrl Pts',(0.235191488870558,-0.0306373282530253,
-1.04794382495191));
#70797=CARTESIAN_POINT('Ctrl Pts',(0.235356436951206,-0.0293433091148237,
-1.04785729162268));
#70798=CARTESIAN_POINT('Ctrl Pts',(0.235649343438506,-0.0268838620793663,
-1.04769234555208));
#70799=CARTESIAN_POINT('Ctrl Pts',(0.235779351885715,-0.0257187138578892,
-1.04761399999654));
#70800=CARTESIAN_POINT('Ctrl Pts',(0.236056057896234,-0.0230601373195481,
-1.04743474919486));
#70801=CARTESIAN_POINT('Ctrl Pts',(0.236197229786942,-0.0215661972405644,
-1.04733367337973));
#70802=CARTESIAN_POINT('Ctrl Pts',(0.236589422685795,-0.016948367597855,
-1.04702011391224));
#70803=CARTESIAN_POINT('Ctrl Pts',(0.2367927022762,-0.0138208755589679,
-1.0468061515963));
#70804=CARTESIAN_POINT('Ctrl Pts',(0.237722037298659,0.00677620364881257,
-1.04538587271513));
#70805=CARTESIAN_POINT('Ctrl Pts',(0.236576147313844,0.0242732632793495,
-1.04412065615394));
#70806=CARTESIAN_POINT('Ctrl Pts',(0.231077711792158,0.0552262430860495,
-1.04182459464647));
#70807=CARTESIAN_POINT('Ctrl Pts',(0.227427272091829,0.0687296762748372,
-1.04080404284123));
#70808=CARTESIAN_POINT('Ctrl Pts',(0.222090132341755,0.0832479479033649,
-1.03973332840307));
#70809=CARTESIAN_POINT('Ctrl Pts',(0.221557148684481,0.0846562335241625,
-1.03962977432557));
#70810=CARTESIAN_POINT('Ctrl Pts',(0.220724352835959,0.0867949524713409,
-1.03947307988995));
#70811=CARTESIAN_POINT('Ctrl Pts',(0.220434257605839,0.0875290913289815,
-1.03941939594348));
#70812=CARTESIAN_POINT('Ctrl Pts',(0.219896656181607,0.0888699643860071,
-1.03932155150976));
#70813=CARTESIAN_POINT('Ctrl Pts',(0.219650299542593,0.0894771250243933,
-1.0392773264773));
#70814=CARTESIAN_POINT('Ctrl Pts',(0.219087230717095,0.0908485015742039,
-1.03917761291892));
#70815=CARTESIAN_POINT('Ctrl Pts',(0.21876903443996,0.0916120872141515,
-1.03912221427717));
#70816=CARTESIAN_POINT('Ctrl Pts',(0.217933084267518,0.093588949350268,
-1.03897906968969));
#70817=CARTESIAN_POINT('Ctrl Pts',(0.217409183732837,0.094799618574917,
-1.03889167822227));
#70818=CARTESIAN_POINT('Ctrl Pts',(0.213580967907953,0.103447474205728,
-1.03826896095055));
#70819=CARTESIAN_POINT('Ctrl Pts',(0.209905514373401,0.110715470439914,
-1.03775364882532));
#70820=CARTESIAN_POINT('Ctrl Pts',(0.203568743915175,0.121791192591615,
-1.03695921095531));
#70821=CARTESIAN_POINT('Ctrl Pts',(0.201157532622864,0.125733756117386,
-1.03667449757163));
#70822=CARTESIAN_POINT('Ctrl Pts',(0.193202655206651,0.137925546639449,
-1.03578044117108));
#70823=CARTESIAN_POINT('Ctrl Pts',(0.187255165100317,0.145897979656046,
-1.03517502885233));
#70824=CARTESIAN_POINT('Ctrl Pts',(0.174176957476517,0.161306931076453,
-1.03392066065903));
#70825=CARTESIAN_POINT('Ctrl Pts',(0.167027487007076,0.168698896557807,
-1.03327217708998));
#70826=CARTESIAN_POINT('Ctrl Pts',(0.157754326489912,0.177117549237143,
-1.03245568373969));
#70827=CARTESIAN_POINT('Ctrl Pts',(0.156065250086892,0.178607645179499,
-1.03230790604976));
#70828=CARTESIAN_POINT('Ctrl Pts',(0.153352434336726,0.180933015403953,
-1.03207188359628));
#70829=CARTESIAN_POINT('Ctrl Pts',(0.152342468736309,0.181784205253794,
-1.03198429735767));
#70830=CARTESIAN_POINT('Ctrl Pts',(0.150424938152886,0.183373079636745,
-1.03181850480131));
#70831=CARTESIAN_POINT('Ctrl Pts',(0.149518920503259,0.184112576107187,
-1.03174037548469));
#70832=CARTESIAN_POINT('Ctrl Pts',(0.147459360863589,0.18576837112643,-1.03156321280375));
#70833=CARTESIAN_POINT('Ctrl Pts',(0.146302685382501,0.186680676280721,
-1.03146402359801));
#70834=CARTESIAN_POINT('Ctrl Pts',(0.142850364442756,0.189351834811302,
-1.03116883024725));
#70835=CARTESIAN_POINT('Ctrl Pts',(0.140531036795825,0.191079487061952,
-1.03097161614323));
#70836=CARTESIAN_POINT('Ctrl Pts',(0.122165203349238,0.204244819851684,
-1.02941780110421));
#70837=CARTESIAN_POINT('Ctrl Pts',(0.104784162220107,0.213682601983038,
-1.02798368722188));
#70838=CARTESIAN_POINT('Ctrl Pts',(0.0841692305464473,0.221750930055794,
-1.02636782537346));
#70839=CARTESIAN_POINT('Ctrl Pts',(0.0818834250948052,0.222605119581157,
-1.02618990283439));
#70840=CARTESIAN_POINT('Ctrl Pts',(0.0733384096662811,0.225648901353173,
-1.02553012043249));
#70841=CARTESIAN_POINT('Ctrl Pts',(0.067000990327593,0.227611133647803,
-1.02505127370563));
#70842=CARTESIAN_POINT('Ctrl Pts',(0.0570163551471063,0.230249371175679,
-1.02432038737577));
#70843=CARTESIAN_POINT('Ctrl Pts',(0.0534216029919816,0.231109873773933,
-1.02406190742171));
#70844=CARTESIAN_POINT('Ctrl Pts',(0.0487152233525572,0.232120780696613,
-1.02373076888635));
#70845=CARTESIAN_POINT('Ctrl Pts',(0.0476208014169346,0.232347776435435,
-1.02365427435596));
#70846=CARTESIAN_POINT('Ctrl Pts',(0.0458332384667774,0.232705376511691,
-1.02353020565478));
#70847=CARTESIAN_POINT('Ctrl Pts',(0.0451410629968801,0.232840637498089,
-1.02348237686285));
#70848=CARTESIAN_POINT('Ctrl Pts',(0.0437889121513203,0.23309861087764,
-1.02338937283421));
#70849=CARTESIAN_POINT('Ctrl Pts',(0.0431290049686393,0.233221611707747,
-1.02334418263677));
#70850=CARTESIAN_POINT('Ctrl Pts',(0.0416511707215966,0.233490579871536,
-1.02324341014954));
#70851=CARTESIAN_POINT('Ctrl Pts',(0.0408329725228978,0.233635055841077,
-1.02318791113496));
#70852=CARTESIAN_POINT('Ctrl Pts',(0.0379847521636842,0.23412257000662,
-1.02299567993711));
#70853=CARTESIAN_POINT('Ctrl Pts',(0.0359509664546327,0.234443485511614,
-1.02286011965641));
#70854=CARTESIAN_POINT('Ctrl Pts',(0.0209030832056344,0.23661749123796,
-1.0218679409433));
#70855=CARTESIAN_POINT('Ctrl Pts',(0.00775741603820414,0.237412491359641,
-1.02106005793333));
#70856=CARTESIAN_POINT('Ctrl Pts',(-0.0176494674194245,0.236835177217374,
-1.01950176485479));
#70857=CARTESIAN_POINT('Ctrl Pts',(-0.0298697332375505,0.235605932599213,
-1.01875328707626));
#70858=CARTESIAN_POINT('Ctrl Pts',(-0.0419392742985053,0.233437524610579,
-1.01798096863704));
#70859=CARTESIAN_POINT('Origin',(0.,0.,-2.1456589891905));
#70860=CARTESIAN_POINT('',(-0.0419392741323876,0.233437524640424,-0.898335233456629));
#70861=CARTESIAN_POINT('',(-0.0419392742314872,0.23343752462262,-0.917975447697368));
#70862=CARTESIAN_POINT('',(-0.0419392741328076,0.233437524640348,-2.1456589891905));
#70863=CARTESIAN_POINT('Ctrl Pts',(-0.0419392741323876,0.233437524640424,
-0.898335233456629));
#70864=CARTESIAN_POINT('Ctrl Pts',(-0.0403252167073179,0.233727505426162,
-0.898443857794283));
#70865=CARTESIAN_POINT('Ctrl Pts',(-0.038708130257032,0.234000749953858,
-0.898551621961256));
#70866=CARTESIAN_POINT('Ctrl Pts',(-0.0251098457204889,0.236153669473257,
-0.899449899231117));
#70867=CARTESIAN_POINT('Ctrl Pts',(-0.0130019729095658,0.237128835285574,
-0.900198716281383));
#70868=CARTESIAN_POINT('Ctrl Pts',(0.00992325448858503,0.237213055365717,
-0.901605921069753));
#70869=CARTESIAN_POINT('Ctrl Pts',(0.0207077636629997,0.236515715439281,
-0.902263625290515));
#70870=CARTESIAN_POINT('Ctrl Pts',(0.0404854078477219,0.233873476118602,
-0.903507465746095));
#70871=CARTESIAN_POINT('Ctrl Pts',(0.0494850752401278,0.232135884354093,
-0.904088180041554));
#70872=CARTESIAN_POINT('Ctrl Pts',(0.0604810905426268,0.229344288161047,
-0.904828284488241));
#70873=CARTESIAN_POINT('Ctrl Pts',(0.0625935115543583,0.228776783373871,
-0.904971868424185));
#70874=CARTESIAN_POINT('Ctrl Pts',(0.0659551457550852,0.227823632645041,
-0.905202756304612));
#70875=CARTESIAN_POINT('Ctrl Pts',(0.0672095761349562,0.227456724681438,
-0.90528945134025));
#70876=CARTESIAN_POINT('Ctrl Pts',(0.0695833611387194,0.226741065846799,
-0.905454556972059));
#70877=CARTESIAN_POINT('Ctrl Pts',(0.0707032910172304,0.226394345430478,
-0.905532899086215));
#70878=CARTESIAN_POINT('Ctrl Pts',(0.0732477607157296,0.225585878609355,
-0.905711933990074));
#70879=CARTESIAN_POINT('Ctrl Pts',(0.0746705783162725,0.22511891886867,
-0.905812795514403));
#70880=CARTESIAN_POINT('Ctrl Pts',(0.0790400158785356,0.223638916805066,
-0.906124905055433));
#70881=CARTESIAN_POINT('Ctrl Pts',(0.0819710668511112,0.222581292584412,
-0.906337611570714));
#70882=CARTESIAN_POINT('Ctrl Pts',(0.101488411795579,0.215100973646811,
-0.907777210647533));
#70883=CARTESIAN_POINT('Ctrl Pts',(0.117324808009818,0.20688882552848,-0.909065324755007));
#70884=CARTESIAN_POINT('Ctrl Pts',(0.135621469890837,0.194619779130859,
-0.91067429562498));
#70885=CARTESIAN_POINT('Ctrl Pts',(0.139086954137596,0.192158428194524,
-0.910984664934843));
#70886=CARTESIAN_POINT('Ctrl Pts',(0.147679127347507,0.18570158644759,-0.911766095433172));
#70887=CARTESIAN_POINT('Ctrl Pts',(0.152711535056764,0.181585798745035,
-0.912235051338868));
#70888=CARTESIAN_POINT('Ctrl Pts',(0.160294678541035,0.17484535251084,-0.912952826428152));
#70889=CARTESIAN_POINT('Ctrl Pts',(0.162964447699258,0.172359721674602,
-0.913207836636389));
#70890=CARTESIAN_POINT('Ctrl Pts',(0.166372684963927,0.169036529986393,
-0.913535263988172));
#70891=CARTESIAN_POINT('Ctrl Pts',(0.167163917661775,0.168254104041823,
-0.913611413858016));
#70892=CARTESIAN_POINT('Ctrl Pts',(0.16844694644382,0.166967370849943,-0.913735075645796));
#70893=CARTESIAN_POINT('Ctrl Pts',(0.16894204322303,0.166466401293174,-0.913782838984906));
#70894=CARTESIAN_POINT('Ctrl Pts',(0.16990534527678,0.16548294850936,-0.91387584529976));
#70895=CARTESIAN_POINT('Ctrl Pts',(0.170373741176174,0.165000669501783,
-0.913921102363046));
#70896=CARTESIAN_POINT('Ctrl Pts',(0.171418677556239,0.163915567834917,
-0.91402215911227));
#70897=CARTESIAN_POINT('Ctrl Pts',(0.171994107212792,0.16331167603736,-0.914077874104222));
#70898=CARTESIAN_POINT('Ctrl Pts',(0.173991247752349,0.161193488010231,
-0.914271525176473));
#70899=CARTESIAN_POINT('Ctrl Pts',(0.17539629169421,0.15966351008791,-0.91440826679957));
#70900=CARTESIAN_POINT('Ctrl Pts',(0.184821377450756,0.149125768850062,
-0.915330640689937));
#70901=CARTESIAN_POINT('Ctrl Pts',(0.192165335529015,0.139534924322692,
-0.916075523251781));
#70902=CARTESIAN_POINT('Ctrl Pts',(0.204583443620507,0.120465475508186,
-0.917472470051787));
#70903=CARTESIAN_POINT('Ctrl Pts',(0.209805753388142,0.111120894624367,
-0.918123937718689));
#70904=CARTESIAN_POINT('Ctrl Pts',(0.21835970768849,0.0930461625228591,
-0.919369718806663));
#70905=CARTESIAN_POINT('Ctrl Pts',(0.221841045827886,0.0844101290063846,
-0.919959286147717));
#70906=CARTESIAN_POINT('Ctrl Pts',(0.225506072521575,0.0735106569322762,
-0.920709382993452));
#70907=CARTESIAN_POINT('Ctrl Pts',(0.226177180205952,0.0714191014263156,
-0.920853563867372));
#70908=CARTESIAN_POINT('Ctrl Pts',(0.227201701447309,0.0680667390380779,
-0.921085185285922));
#70909=CARTESIAN_POINT('Ctrl Pts',(0.227573902725698,0.0668117713085899,
-0.9211720099789));
#70910=CARTESIAN_POINT('Ctrl Pts',(0.228259620095684,0.0644274786626634,
-0.921337217407301));
#70911=CARTESIAN_POINT('Ctrl Pts',(0.228575191833377,0.0632987817128979,
-0.92141553043871));
#70912=CARTESIAN_POINT('Ctrl Pts',(0.229273975268266,0.0607260802248824,
-0.921594296256433));
#70913=CARTESIAN_POINT('Ctrl Pts',(0.229651931151901,0.0592807126738795,
-0.921694915886843));
#70914=CARTESIAN_POINT('Ctrl Pts',(0.230771441123677,0.054828058816994,
-0.922005515179969));
#70915=CARTESIAN_POINT('Ctrl Pts',(0.231467735635185,0.051809843173654,
-0.92221693297017));
#70916=CARTESIAN_POINT('Ctrl Pts',(0.235816328725352,0.0311179605776463,
-0.923672979373517));
#70917=CARTESIAN_POINT('Ctrl Pts',(0.237499412197457,0.0130942003070141,
-0.924980886126771));
#70918=CARTESIAN_POINT('Ctrl Pts',(0.237040731320142,-0.00891359794742625,
-0.926588607967737));
#70919=CARTESIAN_POINT('Ctrl Pts',(0.236858192349084,-0.012882466804857,
-0.926878652492061));
#70920=CARTESIAN_POINT('Ctrl Pts',(0.236112284008601,-0.0233582713521212,
-0.927642309821164));
#70921=CARTESIAN_POINT('Ctrl Pts',(0.235379691727672,-0.0298501543828239,
-0.928113639368944));
#70922=CARTESIAN_POINT('Ctrl Pts',(0.233820005480452,-0.0399195723492457,
-0.928834569811754));
#70923=CARTESIAN_POINT('Ctrl Pts',(0.23317633530627,-0.0435220347792475,
-0.929090421032869));
#70924=CARTESIAN_POINT('Ctrl Pts',(0.232228258072067,-0.04820018402496,
-0.92941875252416));
#70925=CARTESIAN_POINT('Ctrl Pts',(0.23199930031482,-0.0492904287267528,
-0.92949499035349));
#70926=CARTESIAN_POINT('Ctrl Pts',(0.231612997582235,-0.0510675673676237,
-0.929618758705851));
#70927=CARTESIAN_POINT('Ctrl Pts',(0.23146026149432,-0.0517554293574698,
-0.929666541447195));
#70928=CARTESIAN_POINT('Ctrl Pts',(0.231155848484703,-0.0530980796224711,
-0.929759554835466));
#70929=CARTESIAN_POINT('Ctrl Pts',(0.231004450496414,-0.0537529182126418,
-0.929804799778456));
#70930=CARTESIAN_POINT('Ctrl Pts',(0.230659085670137,-0.0552183068566771,
-0.929905797733753));
#70931=CARTESIAN_POINT('Ctrl Pts',(0.230463623988872,-0.0560285042132525,
-0.929961466372759));
#70932=CARTESIAN_POINT('Ctrl Pts',(0.229767125872025,-0.058850195678461,
-0.930154798252433));
#70933=CARTESIAN_POINT('Ctrl Pts',(0.22924397581814,-0.0608562070148542,
-0.930291272187157));
#70934=CARTESIAN_POINT('Ctrl Pts',(0.225526156661754,-0.0743832543932445,
-0.931206576529402));
#70935=CARTESIAN_POINT('Ctrl Pts',(0.22149018180792,-0.0856568064272036,
-0.931945360217781));
#70936=CARTESIAN_POINT('Ctrl Pts',(0.212414385578742,-0.106013231292959,
-0.933313766200487));
#70937=CARTESIAN_POINT('Ctrl Pts',(0.207596432549409,-0.115162452881432,
-0.933943121080449));
#70938=CARTESIAN_POINT('Ctrl Pts',(0.197111836728112,-0.132263289676667,
-0.935190640158037));
#70939=CARTESIAN_POINT('Ctrl Pts',(0.191521031177732,-0.140236636150888,
-0.935806124119797));
#70940=CARTESIAN_POINT('Ctrl Pts',(0.184071548074278,-0.149581365839802,
-0.936585454645904));
#70941=CARTESIAN_POINT('Ctrl Pts',(0.182661874630053,-0.15129956649896,
-0.936731303705609));
#70942=CARTESIAN_POINT('Ctrl Pts',(0.180380265645049,-0.154002170779592,
-0.936964975076122));
#70943=CARTESIAN_POINT('Ctrl Pts',(0.179523906744151,-0.154999598800187,
-0.937052161959542));
#70944=CARTESIAN_POINT('Ctrl Pts',(0.177889168217858,-0.156871908342234,
-0.937217658990402));
#70945=CARTESIAN_POINT('Ctrl Pts',(0.177112512271686,-0.157748247876709,
-0.937295896048207));
#70946=CARTESIAN_POINT('Ctrl Pts',(0.175336643204878,-0.159722402086563,
-0.937473935853399));
#70947=CARTESIAN_POINT('Ctrl Pts',(0.17433355682885,-0.160816650156586,
-0.937573900328392));
#70948=CARTESIAN_POINT('Ctrl Pts',(0.171240014871982,-0.164128379446678,
-0.937880431710378));
#70949=CARTESIAN_POINT('Ctrl Pts',(0.169117106064412,-0.166314973956369,
-0.93808838259582));
#70950=CARTESIAN_POINT('Ctrl Pts',(0.153723388880565,-0.181570961590509,
-0.939580208981506));
#70951=CARTESIAN_POINT('Ctrl Pts',(0.138998050013537,-0.193075566900732,
-0.940932097277406));
#70952=CARTESIAN_POINT('Ctrl Pts',(0.120169865004178,-0.204506227491978,
-0.942540648653914));
#70953=CARTESIAN_POINT('Ctrl Pts',(0.117219085135308,-0.206211736119834,
-0.942789348548752));
#70954=CARTESIAN_POINT('Ctrl Pts',(0.108470413237395,-0.211019858714152,
-0.943515336048037));
#70955=CARTESIAN_POINT('Ctrl Pts',(0.102578675609848,-0.213945876994352,
-0.943990026136453));
#70956=CARTESIAN_POINT('Ctrl Pts',(0.0943143489417772,-0.217630184991644,
-0.944630302189163));
#70957=CARTESIAN_POINT('Ctrl Pts',(0.0920403978783554,-0.218601601234483,
-0.944803888317525));
#70958=CARTESIAN_POINT('Ctrl Pts',(0.0880698977227582,-0.220224827040807,
-0.945102036667528));
#70959=CARTESIAN_POINT('Ctrl Pts',(0.0863803108074465,-0.220893014237281,
-0.945227379437528));
#70960=CARTESIAN_POINT('Ctrl Pts',(0.0838880503226851,-0.221845667501571,
-0.945409861681743));
#70961=CARTESIAN_POINT('Ctrl Pts',(0.0830913053079532,-0.222145313286607,
-0.945467840780107));
#70962=CARTESIAN_POINT('Ctrl Pts',(0.0816767430518859,-0.222668637101217,
-0.945570123309403));
#70963=CARTESIAN_POINT('Ctrl Pts',(0.0810595901001707,-0.222894044771368,
-0.945614526701023));
#70964=CARTESIAN_POINT('Ctrl Pts',(0.0797158809203744,-0.223378499169898,
-0.945710722059338));
#70965=CARTESIAN_POINT('Ctrl Pts',(0.0789889929723276,-0.223636568105714,
-0.94576245659595));
#70966=CARTESIAN_POINT('Ctrl Pts',(0.0769578537991184,-0.224346550219677,
-0.94590620885446));
#70967=CARTESIAN_POINT('Ctrl Pts',(0.0756508718645457,-0.224790639636685,
-0.945997782050744));
#70968=CARTESIAN_POINT('Ctrl Pts',(0.0679709130172216,-0.227325583848626,
-0.946530871254124));
#70969=CARTESIAN_POINT('Ctrl Pts',(0.0615147943001458,-0.229156965023907,
-0.946958932703432));
#70970=CARTESIAN_POINT('Ctrl Pts',(0.0425628447169863,-0.233674064546939,
-0.94818102258841));
#70971=CARTESIAN_POINT('Ctrl Pts',(0.0299170545174869,-0.235627178748956,
-0.948954790919051));
#70972=CARTESIAN_POINT('Ctrl Pts',(0.00455840076217602,-0.23746835211797,
-0.950518932029374));
#70973=CARTESIAN_POINT('Ctrl Pts',(-0.00810964606314755,-0.237373485922798,
-0.951306786860958));
#70974=CARTESIAN_POINT('Ctrl Pts',(-0.0235052764053285,-0.236024073138651,
-0.95230879777316));
#70975=CARTESIAN_POINT('Ctrl Pts',(-0.0262971030402953,-0.235729341411989,
-0.95249223432027));
#70976=CARTESIAN_POINT('Ctrl Pts',(-0.0305093869968351,-0.235208893797576,
-0.952771931227015));
#70977=CARTESIAN_POINT('Ctrl Pts',(-0.0319341677832795,-0.235019691070726,
-0.952867045352051));
#70978=CARTESIAN_POINT('Ctrl Pts',(-0.0345125437591595,-0.234653418693272,
-0.953040132162558));
#70979=CARTESIAN_POINT('Ctrl Pts',(-0.0356667273097581,-0.234480760533774,
-0.953117963171087));
#70980=CARTESIAN_POINT('Ctrl Pts',(-0.0381498545167648,-0.23409054354817,
-0.95328618760446));
#70981=CARTESIAN_POINT('Ctrl Pts',(-0.0394783079627051,-0.233870171353125,
-0.953376667707197));
#70982=CARTESIAN_POINT('Ctrl Pts',(-0.0430791132751796,-0.23324129340404,
-0.953623260599664));
#70983=CARTESIAN_POINT('Ctrl Pts',(-0.0453474429961468,-0.232810909764799,
-0.953780061256431));
#70984=CARTESIAN_POINT('Ctrl Pts',(-0.0579202964877048,-0.230234674793777,
-0.954657577256476));
#70985=CARTESIAN_POINT('Ctrl Pts',(-0.0680779628848821,-0.227438125226631,
-0.955398826434814));
#70986=CARTESIAN_POINT('Ctrl Pts',(-0.0935899451340671,-0.218551838399711,
-0.957341115739239));
#70987=CARTESIAN_POINT('Ctrl Pts',(-0.108555294300177,-0.211517587295821,
-0.958561658576663));
#70988=CARTESIAN_POINT('Ctrl Pts',(-0.127874261312718,-0.199842781203762,
-0.960182906412191));
#70989=CARTESIAN_POINT('Ctrl Pts',(-0.132956690940827,-0.196498082804704,
-0.960613718117229));
#70990=CARTESIAN_POINT('Ctrl Pts',(-0.138969314717727,-0.192200989555981,
-0.96112375663454));
#70991=CARTESIAN_POINT('Ctrl Pts',(-0.140026995637415,-0.191431793357643,
-0.961213490212237));
#70992=CARTESIAN_POINT('Ctrl Pts',(-0.14167898339549,-0.190209370689018,
-0.961353596017911));
#70993=CARTESIAN_POINT('Ctrl Pts',(-0.142277583313108,-0.189762030869195,
-0.961404353337906));
#70994=CARTESIAN_POINT('Ctrl Pts',(-0.143401970381736,-0.18891345352853,
-0.961499659026405));
#70995=CARTESIAN_POINT('Ctrl Pts',(-0.143928190488795,-0.188512848442116,
-0.961544246149591));
#70996=CARTESIAN_POINT('Ctrl Pts',(-0.145146637811149,-0.187577182968247,
-0.961647459769384));
#70997=CARTESIAN_POINT('Ctrl Pts',(-0.145837588595359,-0.187040487199312,
-0.961705970887468));
#70998=CARTESIAN_POINT('Ctrl Pts',(-0.14809659034468,-0.185265679869789,
-0.96189726505498));
#70999=CARTESIAN_POINT('Ctrl Pts',(-0.149652018717732,-0.184011538098165,
-0.962028975795085));
#71000=CARTESIAN_POINT('Ctrl Pts',(-0.163184060984271,-0.172815556800203,
-0.963176686354874));
#71001=CARTESIAN_POINT('Ctrl Pts',(-0.174172574861356,-0.161735307621267,
-0.964123156633538));
#71002=CARTESIAN_POINT('Ctrl Pts',(-0.192878880287221,-0.138736626027903,
-0.965940364174387));
#71003=CARTESIAN_POINT('Ctrl Pts',(-0.200770081893458,-0.127048921675544,
-0.966806396292655));
#71004=CARTESIAN_POINT('Ctrl Pts',(-0.209432803016603,-0.111375851952022,
-0.967957522600417));
#71005=CARTESIAN_POINT('Ctrl Pts',(-0.211205691895818,-0.107976073297876,
-0.968206502517116));
#71006=CARTESIAN_POINT('Ctrl Pts',(-0.213611330031101,-0.103076764245542,
-0.968565082982564));
#71007=CARTESIAN_POINT('Ctrl Pts',(-0.214312315697623,-0.101611272827068,
-0.968672313312657));
#71008=CARTESIAN_POINT('Ctrl Pts',(-0.215500954733855,-0.0990592608693048,
-0.96885905256649));
#71009=CARTESIAN_POINT('Ctrl Pts',(-0.215995587462027,-0.0979760417834671,
-0.968938317680023));
#71010=CARTESIAN_POINT('Ctrl Pts',(-0.21693233594426,-0.0958830396748749,
-0.969091500454952));
#71011=CARTESIAN_POINT('Ctrl Pts',(-0.217375611252159,-0.094873806907852,
-0.969165375882945));
#71012=CARTESIAN_POINT('Ctrl Pts',(-0.218525319312046,-0.0922058341951418,
-0.969360721377472));
#71013=CARTESIAN_POINT('Ctrl Pts',(-0.219219890042996,-0.0905420926222624,
-0.969482590404888));
#71014=CARTESIAN_POINT('Ctrl Pts',(-0.221643848481839,-0.0845444158636322,
-0.969922203026356));
#71015=CARTESIAN_POINT('Ctrl Pts',(-0.223264120855246,-0.0801678291482114,
-0.970243547301865));
#71016=CARTESIAN_POINT('Ctrl Pts',(-0.230550808716873,-0.0585468673434822,
-0.971834709272483));
#71017=CARTESIAN_POINT('Ctrl Pts',(-0.234353117220915,-0.0407409133868043,
-0.973162881150796));
#71018=CARTESIAN_POINT('Ctrl Pts',(-0.236815238704013,-0.0151108211956559,
-0.975040153881166));
#71019=CARTESIAN_POINT('Ctrl Pts',(-0.237177979124535,-0.00751103452780264,
-0.975591560863526));
#71020=CARTESIAN_POINT('Ctrl Pts',(-0.23717341925525,0.00405703612768345,
-0.976412327064179));
#71021=CARTESIAN_POINT('Ctrl Pts',(-0.237072501648943,0.00802021022546458,
-0.976690172081095));
#71022=CARTESIAN_POINT('Ctrl Pts',(-0.23681222175655,0.0131668618294169,
-0.977045118598729));
#71023=CARTESIAN_POINT('Ctrl Pts',(-0.236743229618205,0.0143540239169615,
-0.977126585744526));
#71024=CARTESIAN_POINT('Ctrl Pts',(-0.236618055843411,0.0162602694370274,
-0.977256691299954));
#71025=CARTESIAN_POINT('Ctrl Pts',(-0.236567519063765,0.0169796841155333,
-0.977305630899871));
#71026=CARTESIAN_POINT('Ctrl Pts',(-0.236463665996791,0.0183674944257257,
-0.977399712172109));
#71027=CARTESIAN_POINT('Ctrl Pts',(-0.236410796068062,0.0190359055978749,
-0.977444876293001));
#71028=CARTESIAN_POINT('Ctrl Pts',(-0.236276304141768,0.0206491671213104,
-0.977553542393236));
#71029=CARTESIAN_POINT('Ctrl Pts',(-0.236191847094369,0.0215937825472487,
-0.977616887838891));
#71030=CARTESIAN_POINT('Ctrl Pts',(-0.23587539342549,0.0249088785907314,
-0.977838286255811));
#71031=CARTESIAN_POINT('Ctrl Pts',(-0.235613349289118,0.0272764397316798,
-0.977994767868042));
#71032=CARTESIAN_POINT('Ctrl Pts',(-0.234873154622818,0.0331529851254552,
-0.978379998279816));
#71033=CARTESIAN_POINT('Ctrl Pts',(-0.234351991205659,0.0366560516767475,
-0.978606813908757));
#71034=CARTESIAN_POINT('Ctrl Pts',(-0.231694589361973,0.0521288149137847,
-0.979601275661725));
#71035=CARTESIAN_POINT('Ctrl Pts',(-0.228718167234694,0.0639362140585172,
-0.980341240432557));
#71036=CARTESIAN_POINT('Ctrl Pts',(-0.22029906712413,0.0890213911591812,
-0.98196390218881));
#71037=CARTESIAN_POINT('Ctrl Pts',(-0.214532710494641,0.102137819548313,
-0.982846475214743));
#71038=CARTESIAN_POINT('Ctrl Pts',(-0.206066284837678,0.117469173681874,
-0.983977904960187));
#71039=CARTESIAN_POINT('Ctrl Pts',(-0.204454805785503,0.120252032366676,
-0.984187477297886));
#71040=CARTESIAN_POINT('Ctrl Pts',(-0.202009423067353,0.124283641202035,
-0.984497783625189));
#71041=CARTESIAN_POINT('Ctrl Pts',(-0.201219401356263,0.125558682784296,
-0.984596925679337));
#71042=CARTESIAN_POINT('Ctrl Pts',(-0.199788645343749,0.127819639217326,
-0.984774575967432));
#71043=CARTESIAN_POINT('Ctrl Pts',(-0.199152567878596,0.128808453138365,
-0.984852910233782));
#71044=CARTESIAN_POINT('Ctrl Pts',(-0.197802024741819,0.130874021185105,
-0.985017917780456));
#71045=CARTESIAN_POINT('Ctrl Pts',(-0.197086060533356,0.131949744379605,
-0.985104645390105));
#71046=CARTESIAN_POINT('Ctrl Pts',(-0.19517277257943,0.134774109871154,
-0.985334491345755));
#71047=CARTESIAN_POINT('Ctrl Pts',(-0.193960763210803,0.136512613607017,
-0.985478161702391));
#71048=CARTESIAN_POINT('Ctrl Pts',(-0.187952134022555,0.144889800166391,
-0.98618140782895));
#71049=CARTESIAN_POINT('Ctrl Pts',(-0.182837651666947,0.151292512650184,
-0.986753136973753));
#71050=CARTESIAN_POINT('Ctrl Pts',(-0.171006308713623,0.164625947888223,
-0.988021253903538));
#71051=CARTESIAN_POINT('Ctrl Pts',(-0.164176844776914,0.171437443073787,
-0.988720780043092));
#71052=CARTESIAN_POINT('Ctrl Pts',(-0.146098651911036,0.1873946586456,-0.990480792377981));
#71053=CARTESIAN_POINT('Ctrl Pts',(-0.134389409107557,0.195962074328455,
-0.991543566052026));
#71054=CARTESIAN_POINT('Ctrl Pts',(-0.120206017873164,0.204466939118223,
-0.992696362932122));
#71055=CARTESIAN_POINT('Ctrl Pts',(-0.118427250529332,0.205502318665864,
-0.992838653405654));
#71056=CARTESIAN_POINT('Ctrl Pts',(-0.115933143261656,0.206910939637112,
-0.993034777413625));
#71057=CARTESIAN_POINT('Ctrl Pts',(-0.115229098919506,0.207303848150714,
-0.993089768922433));
#71058=CARTESIAN_POINT('Ctrl Pts',(-0.113940556034504,0.208014357150275,
-0.99318972040096));
#71059=CARTESIAN_POINT('Ctrl Pts',(-0.113356698997806,0.208333103290601,
-0.993234751479036));
#71060=CARTESIAN_POINT('Ctrl Pts',(-0.112141232300572,0.208990042608169,
-0.99332795060113));
#71061=CARTESIAN_POINT('Ctrl Pts',(-0.111509421706876,0.209327835694194,
-0.993376093772336));
#71062=CARTESIAN_POINT('Ctrl Pts',(-0.109843883916734,0.210208622987748,
-0.993502237787409));
#71063=CARTESIAN_POINT('Ctrl Pts',(-0.108807644909484,0.210746863704373,
-0.993579946470265));
#71064=CARTESIAN_POINT('Ctrl Pts',(-0.104029808169605,0.213183921150094,
-0.993934897645398));
#71065=CARTESIAN_POINT('Ctrl Pts',(-0.10024195600675,0.214991024718669,
-0.994206940668382));
#71066=CARTESIAN_POINT('Ctrl Pts',(-0.08901178210802,0.219987301671365,
-0.994992187864485));
#71067=CARTESIAN_POINT('Ctrl Pts',(-0.0814514880749731,0.22289725267806,
-0.995494193889456));
#71068=CARTESIAN_POINT('Ctrl Pts',(-0.0633377977123513,0.228824121685867,
-0.996666873125569));
#71069=CARTESIAN_POINT('Ctrl Pts',(-0.0527062750104053,0.231503131401166,
-0.997332618169306));
#71070=CARTESIAN_POINT('Ctrl Pts',(-0.0419392532630309,0.233437528389801,
-0.998011590250681));
#71071=CARTESIAN_POINT('Ctrl Pts',(-0.0419392742985056,0.233437524610579,
-1.01798096863704));
#71072=CARTESIAN_POINT('Ctrl Pts',(-0.0422632750598508,0.233379314788377,
-1.01796023613685));
#71073=CARTESIAN_POINT('Ctrl Pts',(-0.0425871672563835,0.233320428150497,
-1.01793948734342));
#71074=CARTESIAN_POINT('Ctrl Pts',(-0.0473194747750942,0.232449867177383,
-1.01763598461243));
#71075=CARTESIAN_POINT('Ctrl Pts',(-0.0517039011818453,0.231514095318814,
-1.01735036103975));
#71076=CARTESIAN_POINT('Ctrl Pts',(-0.0592873197805651,0.22966939969849,
-1.01684661972613));
#71077=CARTESIAN_POINT('Ctrl Pts',(-0.0624986542337207,0.228816380287551,
-1.01663021966578));
#71078=CARTESIAN_POINT('Ctrl Pts',(-0.0671663671439948,0.227470916108471,
-1.0163106386793));
#71079=CARTESIAN_POINT('Ctrl Pts',(-0.0686376517744219,0.227031299875507,
-1.01620916568142));
#71080=CARTESIAN_POINT('Ctrl Pts',(-0.0712287148892143,0.226229608063533,
-1.01602910377622));
#71081=CARTESIAN_POINT('Ctrl Pts',(-0.0723502724684468,0.225873423353623,
-1.01595070975655));
#71082=CARTESIAN_POINT('Ctrl Pts',(-0.0746923032457631,0.225110407255202,
-1.01578603468581));
#71083=CARTESIAN_POINT('Ctrl Pts',(-0.0759122066295384,0.224701963476534,
-1.01569970269944));
#71084=CARTESIAN_POINT('Ctrl Pts',(-0.0791090446185606,0.223602605549567,
-1.01547196511786));
#71085=CARTESIAN_POINT('Ctrl Pts',(-0.0810802188927643,0.222895409917599,
-1.01533002530775));
#71086=CARTESIAN_POINT('Ctrl Pts',(-0.0896255789672378,0.219701251374851,
-1.01470788662115));
#71087=CARTESIAN_POINT('Ctrl Pts',(-0.0960961343688778,0.216949071271681,
-1.01421896402477));
#71088=CARTESIAN_POINT('Ctrl Pts',(-0.116885251584624,0.206994033960744,
-1.01258795180993));
#71089=CARTESIAN_POINT('Ctrl Pts',(-0.130596445140514,0.198628173673593,
-1.01141158036202));
#71090=CARTESIAN_POINT('Ctrl Pts',(-0.148937457192227,0.184712392760167,
-1.00973525680361));
#71091=CARTESIAN_POINT('Ctrl Pts',(-0.15432719730745,0.180233635958996,
-1.00922862296121));
#71092=CARTESIAN_POINT('Ctrl Pts',(-0.16234499092282,0.172947240356999,
-1.00846109676939));
#71093=CARTESIAN_POINT('Ctrl Pts',(-0.165116290032456,0.170303431902368,
-1.00819304784337));
#71094=CARTESIAN_POINT('Ctrl Pts',(-0.168622161676673,0.166792768966254,
-1.00785166048578));
#71095=CARTESIAN_POINT('Ctrl Pts',(-0.169416070386828,0.165986313929055,
-1.00777419554823));
#71096=CARTESIAN_POINT('Ctrl Pts',(-0.170697487361878,0.164665874277494,
-1.00764895093927));
#71097=CARTESIAN_POINT('Ctrl Pts',(-0.171188507094944,0.164155345375798,
-1.0076009077662));
#71098=CARTESIAN_POINT('Ctrl Pts',(-0.172139045734287,0.163158136612783,
-1.007507817032));
#71099=CARTESIAN_POINT('Ctrl Pts',(-0.172598801116911,0.162671701525592,
-1.00746275224699));
#71100=CARTESIAN_POINT('Ctrl Pts',(-0.17372603000911,0.161468900399427,
-1.0073521475783));
#71101=CARTESIAN_POINT('Ctrl Pts',(-0.174391148484324,0.160750324147314,
-1.00728678514286));
#71102=CARTESIAN_POINT('Ctrl Pts',(-0.176308383773,0.15865308941284,-1.00709800823569));
#71103=CARTESIAN_POINT('Ctrl Pts',(-0.177548768929553,0.15726374070451,
-1.00697541594042));
#71104=CARTESIAN_POINT('Ctrl Pts',(-0.188198145901443,0.145048807572277,
-1.00591733091284));
#71105=CARTESIAN_POINT('Ctrl Pts',(-0.196624849652758,0.133403456028322,
-1.00504051789584));
#71106=CARTESIAN_POINT('Ctrl Pts',(-0.208910129077674,0.112707710516761,
-1.00356551431451));
#71107=CARTESIAN_POINT('Ctrl Pts',(-0.213353283056393,0.104052072676631,
-1.0029702915832));
#71108=CARTESIAN_POINT('Ctrl Pts',(-0.220553071413563,0.0876128100012291,
-1.00184685787184));
#71109=CARTESIAN_POINT('Ctrl Pts',(-0.223458837487953,0.0799111213121292,
-1.00132325796295));
#71110=CARTESIAN_POINT('Ctrl Pts',(-0.226603190950512,0.0700533768727471,
-1.00064775456286));
#71111=CARTESIAN_POINT('Ctrl Pts',(-0.22722074820045,0.0680236199171196,
-1.0005084062185));
#71112=CARTESIAN_POINT('Ctrl Pts',(-0.228170550501307,0.0647445045977041,
-1.000282741197));
#71113=CARTESIAN_POINT('Ctrl Pts',(-0.228519965163453,0.0635002078815756,
-1.00019698524257));
#71114=CARTESIAN_POINT('Ctrl Pts',(-0.229167638749663,0.0611191865430806,
-1.00003261998377));
#71115=CARTESIAN_POINT('Ctrl Pts',(-0.229467653717758,0.0599829761287445,
-0.999954070378719));
#71116=CARTESIAN_POINT('Ctrl Pts',(-0.230130903694588,0.0573933113487352,
-0.999774754521618));
#71117=CARTESIAN_POINT('Ctrl Pts',(-0.2304888327643,0.0559385628560676,
-0.999673820441227));
#71118=CARTESIAN_POINT('Ctrl Pts',(-0.231569691542354,0.0513589868288608,
-0.999355388131359));
#71119=CARTESIAN_POINT('Ctrl Pts',(-0.232243005732384,0.0482229416530763,
-0.999136318961076));
#71120=CARTESIAN_POINT('Ctrl Pts',(-0.235741875918895,0.0301478970315594,
-0.99786730918976));
#71121=CARTESIAN_POINT('Ctrl Pts',(-0.23718885865161,0.0149807892051603,
-0.99677423853755));
#71122=CARTESIAN_POINT('Ctrl Pts',(-0.237160804066701,-0.0155658577260233,
-0.994546359668472));
#71123=CARTESIAN_POINT('Ctrl Pts',(-0.235656959168687,-0.0308774600742672,
-0.993416922705108));
#71124=CARTESIAN_POINT('Ctrl Pts',(-0.232295131637977,-0.0479059383490672,
-0.99220773276186));
#71125=CARTESIAN_POINT('Ctrl Pts',(-0.231881496679346,-0.0498696228094154,
-0.992069056025991));
#71126=CARTESIAN_POINT('Ctrl Pts',(-0.231251497611235,-0.0526829502750557,
-0.991871702225889));
#71127=CARTESIAN_POINT('Ctrl Pts',(-0.231055282365642,-0.0535369493875011,
-0.991811970958411));
#71128=CARTESIAN_POINT('Ctrl Pts',(-0.230702670997574,-0.055033586171341,
-0.991707625006668));
#71129=CARTESIAN_POINT('Ctrl Pts',(-0.230548313206057,-0.0556766857324453,
-0.991662897021047));
#71130=CARTESIAN_POINT('Ctrl Pts',(-0.230214100137423,-0.0570438896833402,
-0.991568046389226));
#71131=CARTESIAN_POINT('Ctrl Pts',(-0.230033516827469,-0.057767797491483,
-0.991517965559326));
#71132=CARTESIAN_POINT('Ctrl Pts',(-0.229528177706717,-0.0597536114390435,
-0.991380940869361));
#71133=CARTESIAN_POINT('Ctrl Pts',(-0.229196428287493,-0.0610137352814793,
-0.991294386288601));
#71134=CARTESIAN_POINT('Ctrl Pts',(-0.227277292079897,-0.0680668080809355,
-0.990811823552627));
#71135=CARTESIAN_POINT('Ctrl Pts',(-0.225480532240527,-0.0738010928991041,
-0.990426664875811));
#71136=CARTESIAN_POINT('Ctrl Pts',(-0.219501066704819,-0.0906170137375754,
-0.989301710464295));
#71137=CARTESIAN_POINT('Ctrl Pts',(-0.214704342650741,-0.101460542304057,
-0.988581661577075));
#71138=CARTESIAN_POINT('Ctrl Pts',(-0.201993096294056,-0.12521497060818,
-0.9869287246401));
#71139=CARTESIAN_POINT('Ctrl Pts',(-0.193614532709966,-0.13781627147034,
-0.985994080111688));
#71140=CARTESIAN_POINT('Ctrl Pts',(-0.182585173905853,-0.151394769359509,
-0.984855698777855));
#71141=CARTESIAN_POINT('Ctrl Pts',(-0.181046422256745,-0.15323157057933,
-0.984698714351303));
#71142=CARTESIAN_POINT('Ctrl Pts',(-0.178587195222643,-0.156078378414233,
-0.984450462203051));
#71143=CARTESIAN_POINT('Ctrl Pts',(-0.177685342284982,-0.157104314106395,
-0.984359959979965));
#71144=CARTESIAN_POINT('Ctrl Pts',(-0.176005143178681,-0.15898271154365,
-0.984192296755484));
#71145=CARTESIAN_POINT('Ctrl Pts',(-0.17522933475977,-0.15983739597996,
-0.984115243700795));
#71146=CARTESIAN_POINT('Ctrl Pts',(-0.173493757411195,-0.16172160578393,
-0.983943644413476));
#71147=CARTESIAN_POINT('Ctrl Pts',(-0.172531006784746,-0.162748312394476,
-0.98384897256605));
#71148=CARTESIAN_POINT('Ctrl Pts',(-0.169721164621445,-0.165691860892384,
-0.983574104686601));
#71149=CARTESIAN_POINT('Ctrl Pts',(-0.16785091928829,-0.167586199831108,
-0.983392910382637));
#71150=CARTESIAN_POINT('Ctrl Pts',(-0.163543715356715,-0.17180445416408,
-0.982979375615308));
#71151=CARTESIAN_POINT('Ctrl Pts',(-0.16108839611643,-0.174108713060005,
-0.982746248495182));
#71152=CARTESIAN_POINT('Ctrl Pts',(-0.152744288566874,-0.181611838868939,
-0.981962351513645));
#71153=CARTESIAN_POINT('Ctrl Pts',(-0.146646863960116,-0.186569970889694,
-0.981402701759877));
#71154=CARTESIAN_POINT('Ctrl Pts',(-0.126838149790874,-0.201105693858329,
-0.97962899273299));
#71155=CARTESIAN_POINT('Ctrl Pts',(-0.112353844013378,-0.209542397726592,
-0.97839061099793));
#71156=CARTESIAN_POINT('Ctrl Pts',(-0.0928283945638343,-0.218304426649075,
-0.976864740841788));
#71157=CARTESIAN_POINT('Ctrl Pts',(-0.0884974225334974,-0.220095767430514,
-0.976534964445998));
#71158=CARTESIAN_POINT('Ctrl Pts',(-0.0829399755530145,-0.222203786656368,
-0.976125087641337));
#71159=CARTESIAN_POINT('Ctrl Pts',(-0.0817605003251482,-0.222640479497394,
-0.976038845094655));
#71160=CARTESIAN_POINT('Ctrl Pts',(-0.0798852242868947,-0.223317875375292,
-0.975902968521636));
#71161=CARTESIAN_POINT('Ctrl Pts',(-0.0791917009999208,-0.22356474912591,
-0.975852985742669));
#71162=CARTESIAN_POINT('Ctrl Pts',(-0.0778702180974649,-0.224028237013831,
-0.97575826896684));
#71163=CARTESIAN_POINT('Ctrl Pts',(-0.0772425018772638,-0.224245440890856,
-0.975713503234853));
#71164=CARTESIAN_POINT('Ctrl Pts',(-0.0757510904633691,-0.224754497198856,
-0.975607663183514));
#71165=CARTESIAN_POINT('Ctrl Pts',(-0.0748866124927424,-0.225044011374408,
-0.975546725734796));
#71166=CARTESIAN_POINT('Ctrl Pts',(-0.0719713575833915,-0.226001673176092,
-0.975342541745212));
#71167=CARTESIAN_POINT('Ctrl Pts',(-0.0699130701676077,-0.226646853097484,
-0.975200559821209));
#71168=CARTESIAN_POINT('Ctrl Pts',(-0.0648761958635684,-0.228150535336097,
-0.974857748172062));
#71169=CARTESIAN_POINT('Ctrl Pts',(-0.0618889669489348,-0.228978918793727,
-0.974658346055567));
#71170=CARTESIAN_POINT('Ctrl Pts',(-0.0496557984955409,-0.232114368294907,
-0.973854390514675));
#71171=CARTESIAN_POINT('Ctrl Pts',(-0.0402904612524984,-0.233921963185723,
-0.973267805165594));
#71172=CARTESIAN_POINT('Ctrl Pts',(-0.013140511722014,-0.237482649289191,
-0.971588115014542));
#71173=CARTESIAN_POINT('Ctrl Pts',(0.00476343443951824,-0.237798036803507,
-0.970501087327765));
#71174=CARTESIAN_POINT('Ctrl Pts',(0.0256294445630077,-0.235806680392451,
-0.969145752847856));
#71175=CARTESIAN_POINT('Ctrl Pts',(0.0287201338560649,-0.235450231237663,
-0.96894286461842));
#71176=CARTESIAN_POINT('Ctrl Pts',(0.0332855492847619,-0.234832475645031,
-0.968639582100633));
#71177=CARTESIAN_POINT('Ctrl Pts',(0.0347663322284696,-0.234617819825169,
-0.968540652489463));
#71178=CARTESIAN_POINT('Ctrl Pts',(0.0374030827439788,-0.23421008380084,
-0.968363447729816));
#71179=CARTESIAN_POINT('Ctrl Pts',(0.0385598470780688,-0.23402241786087,
-0.968285346194934));
#71180=CARTESIAN_POINT('Ctrl Pts',(0.0410036341392827,-0.233607342956876,
-0.968119563176141));
#71181=CARTESIAN_POINT('Ctrl Pts',(0.0422902588698042,-0.233377853666517,
-0.968031818023431));
#71182=CARTESIAN_POINT('Ctrl Pts',(0.0457259822764512,-0.232735695528596,
-0.967796237429406));
#71183=CARTESIAN_POINT('Ctrl Pts',(0.0478713325317403,-0.2323039052402,
-0.967647799221991));
#71184=CARTESIAN_POINT('Ctrl Pts',(0.0589868929277687,-0.22990618720785,
-0.96687152110211));
#71185=CARTESIAN_POINT('Ctrl Pts',(0.0678422587878289,-0.227450429768159,
-0.966228215971281));
#71186=CARTESIAN_POINT('Ctrl Pts',(0.0867347737370395,-0.221009622340344,
-0.964801699505761));
#71187=CARTESIAN_POINT('Ctrl Pts',(0.096687818041288,-0.216840054389063,
-0.964015046504671));
#71188=CARTESIAN_POINT('Ctrl Pts',(0.117153519969759,-0.206576523521615,
-0.962342996905235));
#71189=CARTESIAN_POINT('Ctrl Pts',(0.127553886433173,-0.20032192077999,
-0.961459783662889));
#71190=CARTESIAN_POINT('Ctrl Pts',(0.139121343601995,-0.192097713732959,
-0.960469725050554));
#71191=CARTESIAN_POINT('Ctrl Pts',(0.140795473045375,-0.190874082495373,
-0.960326260233319));
#71192=CARTESIAN_POINT('Ctrl Pts',(0.143119696163081,-0.189128072120037,
-0.960127077284734));
#71193=CARTESIAN_POINT('Ctrl Pts',(0.14378335307408,-0.188624024252106,
-0.960070201847991));
#71194=CARTESIAN_POINT('Ctrl Pts',(0.144977289078083,-0.187707266119526,
-0.959967900467953));
#71195=CARTESIAN_POINT('Ctrl Pts',(0.145508496235768,-0.187295781229081,
-0.959922391389542));
#71196=CARTESIAN_POINT('Ctrl Pts',(0.14659287862366,-0.186448396449807,
-0.959829517357495));
#71197=CARTESIAN_POINT('Ctrl Pts',(0.147145872341527,-0.186012281550627,
-0.959782168182981));
#71198=CARTESIAN_POINT('Ctrl Pts',(0.148567881318607,-0.184880513690316,
-0.959660420593631));
#71199=CARTESIAN_POINT('Ctrl Pts',(0.149433968766053,-0.184181184713478,
-0.959586278429204));
#71200=CARTESIAN_POINT('Ctrl Pts',(0.153121109439434,-0.181160844395393,
-0.959270519023305));
#71201=CARTESIAN_POINT('Ctrl Pts',(0.155893427207424,-0.178780783684352,
-0.959032801968887));
#71202=CARTESIAN_POINT('Ctrl Pts',(0.163453716880564,-0.171980548463517,
-0.958380054589196));
#71203=CARTESIAN_POINT('Ctrl Pts',(0.168116387363714,-0.167425563167802,
-0.957972226309055));
#71204=CARTESIAN_POINT('Ctrl Pts',(0.175401344259383,-0.15969720461835,
-0.957314605920151));
#71205=CARTESIAN_POINT('Ctrl Pts',(0.178138859186959,-0.156637724683934,
-0.957062307469217));
#71206=CARTESIAN_POINT('Ctrl Pts',(0.192394688370421,-0.139847849756836,
-0.955711128555238));
#71207=CARTESIAN_POINT('Ctrl Pts',(0.202406772513173,-0.124918175022821,
-0.954620202215843));
#71208=CARTESIAN_POINT('Ctrl Pts',(0.212069582634607,-0.106245570056992,
-0.953260683489908));
#71209=CARTESIAN_POINT('Ctrl Pts',(0.213442780007141,-0.103459205666825,
-0.953058102930902));
#71210=CARTESIAN_POINT('Ctrl Pts',(0.215395371141649,-0.0992927528531827,
-0.952755192476975));
#71211=CARTESIAN_POINT('Ctrl Pts',(0.216017098140839,-0.0979327821360431,
-0.952656321932976));
#71212=CARTESIAN_POINT('Ctrl Pts',(0.217103011861908,-0.0954967850498731,
-0.952479182739508));
#71213=CARTESIAN_POINT('Ctrl Pts',(0.21757216621149,-0.0944230168963909,
-0.952401087211313));
#71214=CARTESIAN_POINT('Ctrl Pts',(0.218547916015378,-0.0921439008375314,
-0.952235274611943));
#71215=CARTESIAN_POINT('Ctrl Pts',(0.21905253813811,-0.0909377560345294,
-0.952147493556511));
#71216=CARTESIAN_POINT('Ctrl Pts',(0.220375945279911,-0.0876996160912122,
-0.951911713440981));
#71217=CARTESIAN_POINT('Ctrl Pts',(0.221176575303429,-0.0856603869688508,
-0.95176310982777));
#71218=CARTESIAN_POINT('Ctrl Pts',(0.225199245897759,-0.0749819690119696,
-0.950984097357312));
#71219=CARTESIAN_POINT('Ctrl Pts',(0.227943338882066,-0.0661724373596597,
-0.950338090622313));
#71220=CARTESIAN_POINT('Ctrl Pts',(0.23276215463758,-0.0467909504527406,
-0.948910530272376));
#71221=CARTESIAN_POINT('Ctrl Pts',(0.234643870559066,-0.0361916739412844,
-0.94812573917053));
#71222=CARTESIAN_POINT('Ctrl Pts',(0.237100979435463,-0.0134725561905994,
-0.9464568731755));
#71223=CARTESIAN_POINT('Ctrl Pts',(0.237479669791776,-0.0013598095768279,
-0.945574978278472));
#71224=CARTESIAN_POINT('Ctrl Pts',(0.236838306904382,0.0128023731972036,
-0.944586050413844));
#71225=CARTESIAN_POINT('Ctrl Pts',(0.236717261995422,0.0148735665785085,
-0.94444250902019));
#71226=CARTESIAN_POINT('Ctrl Pts',(0.236509505708998,0.0177743948449892,
-0.944243237905769));
#71227=CARTESIAN_POINT('Ctrl Pts',(0.236445577289121,0.018605494777037,
-0.944186349579088));
#71228=CARTESIAN_POINT('Ctrl Pts',(0.236322200189586,0.0201059659386397,
-0.944084031909984));
#71229=CARTESIAN_POINT('Ctrl Pts',(0.236264285828072,0.0207754530972834,
-0.944038519350998));
#71230=CARTESIAN_POINT('Ctrl Pts',(0.236139855148863,0.0221459998558341,
-0.943945646638725));
#71231=CARTESIAN_POINT('Ctrl Pts',(0.236073060823819,0.0228470235599321,
-0.943898302206605));
#71232=CARTESIAN_POINT('Ctrl Pts',(0.235892659926479,0.0246550594524117,
-0.943776581278541));
#71233=CARTESIAN_POINT('Ctrl Pts',(0.235774381250001,0.0257616038244113,
-0.943702460819372));
#71234=CARTESIAN_POINT('Ctrl Pts',(0.235234841335179,0.0304938122672807,
-0.943386925731097));
#71235=CARTESIAN_POINT('Ctrl Pts',(0.234737678756236,0.0341105393039,-0.943149404421166));
#71236=CARTESIAN_POINT('Ctrl Pts',(0.23312252522281,0.0441384857335257,
-0.942497373591188));
#71237=CARTESIAN_POINT('Ctrl Pts',(0.231823865979681,0.050517572243762,
-0.942090047033668));
#71238=CARTESIAN_POINT('Ctrl Pts',(0.229264014485041,0.0608885851818783,
-0.941428583205499));
#71239=CARTESIAN_POINT('Ctrl Pts',(0.228156772355307,0.0649145333826267,
-0.941172008810144));
#71240=CARTESIAN_POINT('Ctrl Pts',(0.221755992724638,0.0859946927190393,
-0.939820612327463));
#71241=CARTESIAN_POINT('Ctrl Pts',(0.21465613250109,0.102437625490528,-0.938733384620454));
#71242=CARTESIAN_POINT('Ctrl Pts',(0.204232409683695,0.120626615106908,
-0.937377835292395));
#71243=CARTESIAN_POINT('Ctrl Pts',(0.202632798481718,0.123294788816971,
-0.937174962572818));
#71244=CARTESIAN_POINT('Ctrl Pts',(0.200186804129414,0.127198516986609,
-0.936871698809996));
#71245=CARTESIAN_POINT('Ctrl Pts',(0.199380410858223,0.128458829453395,
-0.936772772175208));
#71246=CARTESIAN_POINT('Ctrl Pts',(0.197921256173277,0.130692502828194,
-0.936595570720357));
#71247=CARTESIAN_POINT('Ctrl Pts',(0.19727309747168,0.131668822695496,-0.93651746948908));
#71248=CARTESIAN_POINT('Ctrl Pts',(0.195886822648927,0.133723750608847,
-0.936351684984267));
#71249=CARTESIAN_POINT('Ctrl Pts',(0.195146975242471,0.13480113760411,-0.936263938026059));
#71250=CARTESIAN_POINT('Ctrl Pts',(0.193144556673796,0.137666082180563,
-0.936028347398848));
#71251=CARTESIAN_POINT('Ctrl Pts',(0.19186611102136,0.139442335167609,-0.935879900873936));
#71252=CARTESIAN_POINT('Ctrl Pts',(0.18509513999362,0.148580389047212,-0.935103485643365));
#71253=CARTESIAN_POINT('Ctrl Pts',(0.179203618055949,0.155635367887134,
-0.934460045082522));
#71254=CARTESIAN_POINT('Ctrl Pts',(0.165541784759199,0.170188318229843,
-0.933033475763687));
#71255=CARTESIAN_POINT('Ctrl Pts',(0.157638376022508,0.177533821537695,
-0.932246915570011));
#71256=CARTESIAN_POINT('Ctrl Pts',(0.139847595845537,0.191941230324709,
-0.930575025435195));
#71257=CARTESIAN_POINT('Ctrl Pts',(0.129860184425608,0.198834546880914,
-0.929691878683497));
#71258=CARTESIAN_POINT('Ctrl Pts',(0.117597138135601,0.205978623132566,
-0.928701877267359));
#71259=CARTESIAN_POINT('Ctrl Pts',(0.115791797110284,0.206998890187272,
-0.928558408743856));
#71260=CARTESIAN_POINT('Ctrl Pts',(0.113242403523329,0.208395856851519,
-0.928359221527935));
#71261=CARTESIAN_POINT('Ctrl Pts',(0.112509454963556,0.208792475211763,
-0.928302345467193));
#71262=CARTESIAN_POINT('Ctrl Pts',(0.111181789978038,0.209501889449674,
-0.928200043298646));
#71263=CARTESIAN_POINT('Ctrl Pts',(0.110587806970969,0.209816036316492,
-0.92815453405178));
#71264=CARTESIAN_POINT('Ctrl Pts',(0.109368542918671,0.210454266805773,
-0.928061660083809));
#71265=CARTESIAN_POINT('Ctrl Pts',(0.108743140915312,0.210778096427793,
-0.928014311139019));
#71266=CARTESIAN_POINT('Ctrl Pts',(0.107125553759385,0.211606558021915,
-0.927892564841113));
#71267=CARTESIAN_POINT('Ctrl Pts',(0.106131227891892,0.2121070066123,-0.927818423728058));
#71268=CARTESIAN_POINT('Ctrl Pts',(0.101858944189285,0.214219700527968,
-0.927502675191723));
#71269=CARTESIAN_POINT('Ctrl Pts',(0.0985473039358211,0.215763196712221,
-0.927264967622557));
#71270=CARTESIAN_POINT('Ctrl Pts',(0.0892343110721986,0.219844624805761,
-0.926612254974379));
#71271=CARTESIAN_POINT('Ctrl Pts',(0.0831618549986136,0.222212824765676,
-0.926204451014928));
#71272=CARTESIAN_POINT('Ctrl Pts',(0.0731135138158255,0.225661853215844,
-0.925546634472915));
#71273=CARTESIAN_POINT('Ctrl Pts',(0.0691937742389778,0.226894426384592,
-0.925294119016022));
#71274=CARTESIAN_POINT('Ctrl Pts',(0.0480177070501756,0.232953465762329,
-0.923942931490136));
#71275=CARTESIAN_POINT('Ctrl Pts',(0.0302905814593938,0.235913994694997,
-0.922852194973547));
#71276=CARTESIAN_POINT('Ctrl Pts',(0.00929778192120318,0.237013041345022,
-0.921492879808453));
#71277=CARTESIAN_POINT('Ctrl Pts',(0.00619283613492947,0.237114482550914,
-0.92129028400685));
#71278=CARTESIAN_POINT('Ctrl Pts',(0.00159164458882926,0.237174373576065,
-0.92098735511916));
#71279=CARTESIAN_POINT('Ctrl Pts',(9.62610957998343E-5,0.237179694272432,
-0.920888481647647));
#71280=CARTESIAN_POINT('Ctrl Pts',(-0.00257081801484389,0.237163961471575,
-0.920711339205475));
#71281=CARTESIAN_POINT('Ctrl Pts',(-0.00374250585806567,0.237148365567761,
-0.920633243380491));
#71282=CARTESIAN_POINT('Ctrl Pts',(-0.00622115791677948,0.237096999523045,
-0.920467432251684));
#71283=CARTESIAN_POINT('Ctrl Pts',(-0.00752803400164977,0.237059103545626,
-0.920379652979261));
#71284=CARTESIAN_POINT('Ctrl Pts',(-0.011023597810831,0.23692880721959,
-0.920143882772886));
#71285=CARTESIAN_POINT('Ctrl Pts',(-0.0132113858183241,0.236816887324553,
-0.919995287374625));
#71286=CARTESIAN_POINT('Ctrl Pts',(-0.0242996886663794,0.236095520178203,
-0.919236704472944));
#71287=CARTESIAN_POINT('Ctrl Pts',(-0.0331610130045195,0.235014622843947,
-0.918612203568901));
#71288=CARTESIAN_POINT('Ctrl Pts',(-0.0419392742314872,0.23343752462262,
-0.917975447697368));
#71289=CARTESIAN_POINT('Origin',(0.,0.,-2.1456589891905));
#71290=CARTESIAN_POINT('',(-0.0419215622832511,0.233346034556857,-0.798097588861634));
#71291=CARTESIAN_POINT('',(-0.0419392746656718,0.233437524544614,-0.817620397237267));
#71292=CARTESIAN_POINT('',(-0.0419392741328076,0.233437524640348,-2.1456589891905));
#71293=CARTESIAN_POINT('',(-0.236887575109366,0.0001513332746742,-0.875941010809498));
#71294=CARTESIAN_POINT('Ctrl Pts',(-0.236887575109366,0.0001513332746742,
-0.875941010809498));
#71295=CARTESIAN_POINT('Ctrl Pts',(-0.236597463890264,-0.049544091138451,
-0.872615461822126));
#71296=CARTESIAN_POINT('Ctrl Pts',(-0.197039124271961,-0.178782761335024,
-0.863995269476757));
#71297=CARTESIAN_POINT('Ctrl Pts',(0.0151527372976048,-0.279961252852672,
-0.850080433773393));
#71298=CARTESIAN_POINT('Ctrl Pts',(0.243491146154017,-0.138996295961623,
-0.834196503699405));
#71299=CARTESIAN_POINT('Ctrl Pts',(0.248777094918733,0.129297585399898,
-0.818312573625418));
#71300=CARTESIAN_POINT('Ctrl Pts',(0.0801384244127168,0.242817063678148,
-0.806279602012826));
#71301=CARTESIAN_POINT('Ctrl Pts',(-0.0207684499901398,0.237356879304441,
-0.799541273758231));
#71302=CARTESIAN_POINT('Ctrl Pts',(-0.0419215622832843,0.23334603455685,
-0.798097588861632));
#71303=CARTESIAN_POINT('Ctrl Pts',(-0.237174943862191,0.000163183843552357,
-0.875775716082648));
#71304=CARTESIAN_POINT('Ctrl Pts',(-0.237164001431015,0.0160671510705129,
-0.876898264731405));
#71305=CARTESIAN_POINT('Ctrl Pts',(-0.23555337892694,0.0319287061283791,
-0.878063892272444));
#71306=CARTESIAN_POINT('Ctrl Pts',(-0.230191123282688,0.05815630739297,
-0.880015174976474));
#71307=CARTESIAN_POINT('Ctrl Pts',(-0.227284381721771,0.06864383126262,
-0.880800959270579));
#71308=CARTESIAN_POINT('Ctrl Pts',(-0.22317710950521,0.0802878359840086,
-0.881655268879182));
#71309=CARTESIAN_POINT('Ctrl Pts',(-0.222673166825975,0.0816750871891151,
-0.881756738959431));
#71310=CARTESIAN_POINT('Ctrl Pts',(-0.221881986312466,0.0837912783102711,
-0.881910953095896));
#71311=CARTESIAN_POINT('Ctrl Pts',(-0.221604043232464,0.0845236194126831,
-0.881964215306016));
#71312=CARTESIAN_POINT('Ctrl Pts',(-0.221086712469624,0.0858666196223114,
-0.882061677303563));
#71313=CARTESIAN_POINT('Ctrl Pts',(-0.220848419197361,0.086477665059888,
-0.882105937922297));
#71314=CARTESIAN_POINT('Ctrl Pts',(-0.220300894102182,0.0878646362973995,
-0.882206218569208));
#71315=CARTESIAN_POINT('Ctrl Pts',(-0.219990095949804,0.088639923236142,
-0.882262144307547));
#71316=CARTESIAN_POINT('Ctrl Pts',(-0.219167969423675,0.0906597600180472,
-0.88240754970554));
#71317=CARTESIAN_POINT('Ctrl Pts',(-0.218650126633838,0.0919016498037438,
-0.882496656322477));
#71318=CARTESIAN_POINT('Ctrl Pts',(-0.21346446456841,0.104045911106359,
-0.883365749288355));
#71319=CARTESIAN_POINT('Ctrl Pts',(-0.207994990040098,0.114589673315482,
-0.884102710142617));
#71320=CARTESIAN_POINT('Ctrl Pts',(-0.194505403633626,0.136418491898445,
-0.885681107506964));
#71321=CARTESIAN_POINT('Ctrl Pts',(-0.186242013125466,0.147500012570092,
-0.886517886675148));
#71322=CARTESIAN_POINT('Ctrl Pts',(-0.173704334038675,0.161568122803833,
-0.887701048702306));
#71323=CARTESIAN_POINT('Ctrl Pts',(-0.170227095552165,0.165227675753513,
-0.88802134979542));
#71324=CARTESIAN_POINT('Ctrl Pts',(-0.164856467158617,0.170530288170809,
-0.888507248162344));
#71325=CARTESIAN_POINT('Ctrl Pts',(-0.16304937825703,0.172258914019895,
-0.888669333539511));
#71326=CARTESIAN_POINT('Ctrl Pts',(-0.159694356380409,0.175368165492342,
-0.888968016245174));
#71327=CARTESIAN_POINT('Ctrl Pts',(-0.158154985913881,0.176757689816749,
-0.889104228035403));
#71328=CARTESIAN_POINT('Ctrl Pts',(-0.155655164803658,0.178955371660737,
-0.889324228000585));
#71329=CARTESIAN_POINT('Ctrl Pts',(-0.154706152071789,0.179776421659302,
-0.889407476701386));
#71330=CARTESIAN_POINT('Ctrl Pts',(-0.152858375717605,0.181349582148963,
-0.889569074240294));
#71331=CARTESIAN_POINT('Ctrl Pts',(-0.151960463588417,0.18210263972164,
-0.889647380893023));
#71332=CARTESIAN_POINT('Ctrl Pts',(-0.149905857687856,0.183800011029056,
-0.889826087082309));
#71333=CARTESIAN_POINT('Ctrl Pts',(-0.148745762514662,0.18474010982933,
-0.889926653043626));
#71334=CARTESIAN_POINT('Ctrl Pts',(-0.145155401372374,0.187593864836568,
-0.890236917869707));
#71335=CARTESIAN_POINT('Ctrl Pts',(-0.142696596690058,0.189470917000551,
-0.890448050370114));
#71336=CARTESIAN_POINT('Ctrl Pts',(-0.122424523898745,0.204328175881824,
-0.892178777537975));
#71337=CARTESIAN_POINT('Ctrl Pts',(-0.102920510350732,0.214813236436444,
-0.893797282936546));
#71338=CARTESIAN_POINT('Ctrl Pts',(-0.0761309472811355,0.224719190371577,
-0.895874150753232));
#71339=CARTESIAN_POINT('Ctrl Pts',(-0.0699138555546477,0.226730456611347,
-0.89634557233232));
#71340=CARTESIAN_POINT('Ctrl Pts',(-0.0600961714632879,0.229464203586896,
-0.8970666250601));
#71341=CARTESIAN_POINT('Ctrl Pts',(-0.0565485654291269,0.23036413336333,
-0.897322508838198));
#71342=CARTESIAN_POINT('Ctrl Pts',(-0.0518954407814253,0.231430518562675,
-0.897650875322841));
#71343=CARTESIAN_POINT('Ctrl Pts',(-0.0508077912922736,0.231671729314368,
-0.897727116551379));
#71344=CARTESIAN_POINT('Ctrl Pts',(-0.0490295008634744,0.23205297917948,
-0.897850889022003));
#71345=CARTESIAN_POINT('Ctrl Pts',(-0.0483398795537936,0.232197616651937,
-0.897898672513225));
#71346=CARTESIAN_POINT('Ctrl Pts',(-0.0469912196344658,0.232474208495938,
-0.897991686176618));
#71347=CARTESIAN_POINT('Ctrl Pts',(-0.0463322502967748,0.232606437869259,
-0.898036930652904));
#71348=CARTESIAN_POINT('Ctrl Pts',(-0.0448549261492183,0.232896351987323,
-0.898137926342285));
#71349=CARTESIAN_POINT('Ctrl Pts',(-0.0440362759893075,0.233052529739542,
-0.898193593194436));
#71350=CARTESIAN_POINT('Ctrl Pts',(-0.0427911751582108,0.233283268442541,
-0.898277827287995));
#71351=CARTESIAN_POINT('Ctrl Pts',(-0.0423653301735287,0.233360979615656,
-0.898306560340943));
#71352=CARTESIAN_POINT('Ctrl Pts',(-0.0419392741323876,0.233437524640424,
-0.898335233456629));
#71353=CARTESIAN_POINT('',(-0.237175039616951,9.57688685589552E-5,-0.895455268706531));
#71354=CARTESIAN_POINT('Ctrl Pts',(-0.0419392742314872,0.23343752462262,
-0.917975447697368));
#71355=CARTESIAN_POINT('Ctrl Pts',(-0.0422317674705741,0.23338497542692,
-0.917954230877481));
#71356=CARTESIAN_POINT('Ctrl Pts',(-0.0425241685212188,0.233331875316163,
-0.917933000919219));
#71357=CARTESIAN_POINT('Ctrl Pts',(-0.0533943627192033,0.231336732356517,
-0.917143030107916));
#71358=CARTESIAN_POINT('Ctrl Pts',(-0.0638272696291555,0.228678138260806,
-0.916358145743216));
#71359=CARTESIAN_POINT('Ctrl Pts',(-0.0855467442851248,0.221540880198969,
-0.91468851198947));
#71360=CARTESIAN_POINT('Ctrl Pts',(-0.0967452791403489,0.216884800320748,
-0.913805944742864));
#71361=CARTESIAN_POINT('Ctrl Pts',(-0.10938401095843,0.210455217868708,
-0.912816840148667));
#71362=CARTESIAN_POINT('Ctrl Pts',(-0.111215657362555,0.20949305207031,
-0.912673703246731));
#71363=CARTESIAN_POINT('Ctrl Pts',(-0.113766474859567,0.208110218314762,
-0.912474897913189));
#71364=CARTESIAN_POINT('Ctrl Pts',(-0.114496314222815,0.207709575732239,
-0.912418077737528));
#71365=CARTESIAN_POINT('Ctrl Pts',(-0.115811156719384,0.206978761707875,
-0.912315846172132));
#71366=CARTESIAN_POINT('Ctrl Pts',(-0.116396894586063,0.206649932954719,
-0.912270351996501));
#71367=CARTESIAN_POINT('Ctrl Pts',(-0.117581841461388,0.205978076185156,
-0.912178426812099));
#71368=CARTESIAN_POINT('Ctrl Pts',(-0.118180961532467,0.205634913554832,
-0.912132004748522));
#71369=CARTESIAN_POINT('Ctrl Pts',(-0.119710439793986,0.204749970162841,
-0.912013616531119));
#71370=CARTESIAN_POINT('Ctrl Pts',(-0.120638635615156,0.204204454859977,
-0.911941885861967));
#71371=CARTESIAN_POINT('Ctrl Pts',(-0.122667272340464,0.202993533162125,
-0.911785294841027));
#71372=CARTESIAN_POINT('Ctrl Pts',(-0.12376608829564,0.202325455069047,
-0.911700595303086));
#71373=CARTESIAN_POINT('Ctrl Pts',(-0.126990354928992,0.200329009624858,
-0.911452243230933));
#71374=CARTESIAN_POINT('Ctrl Pts',(-0.129100309564777,0.198975811340943,
-0.911289958096488));
#71375=CARTESIAN_POINT('Ctrl Pts',(-0.136784929296316,0.193873645076855,
-0.910698238012091));
#71376=CARTESIAN_POINT('Ctrl Pts',(-0.142221386774673,0.189921556086763,
-0.910278270154202));
#71377=CARTESIAN_POINT('Ctrl Pts',(-0.159571933858356,0.176144982267166,
-0.908907836013511));
#71378=CARTESIAN_POINT('Ctrl Pts',(-0.170694589517402,0.165389283027187,
-0.907977124595711));
#71379=CARTESIAN_POINT('Ctrl Pts',(-0.185794422945062,0.147629369350368,
-0.906516310329683));
#71380=CARTESIAN_POINT('Ctrl Pts',(-0.190593045301499,0.141379876733652,
-0.906014762462898));
#71381=CARTESIAN_POINT('Ctrl Pts',(-0.196306168349518,0.133118667085378,
-0.905359382638094));
#71382=CARTESIAN_POINT('Ctrl Pts',(-0.19751608245608,0.131316746517983,
-0.905216887022205));
#71383=CARTESIAN_POINT('Ctrl Pts',(-0.199412528136862,0.128406861776938,
-0.904987355298596));
#71384=CARTESIAN_POINT('Ctrl Pts',(-0.200114970670058,0.127309374862874,
-0.904900915670784));
#71385=CARTESIAN_POINT('Ctrl Pts',(-0.201432334216918,0.125213300194608,
-0.904736041753284));
#71386=CARTESIAN_POINT('Ctrl Pts',(-0.202048963888699,0.124215827976891,
-0.90465767375895));
#71387=CARTESIAN_POINT('Ctrl Pts',(-0.203439091119634,0.121929391396564,
-0.90447822155915));
#71388=CARTESIAN_POINT('Ctrl Pts',(-0.20420777564749,0.120637574850504,
-0.904376965374131));
#71389=CARTESIAN_POINT('Ctrl Pts',(-0.20654799872374,0.116618239176673,
-0.904062273333156));
#71390=CARTESIAN_POINT('Ctrl Pts',(-0.208077500133248,0.113866771990018,
-0.903847343333906));
#71391=CARTESIAN_POINT('Ctrl Pts',(-0.215474078728602,0.0999139000285166,
-0.902759367325248));
#71392=CARTESIAN_POINT('Ctrl Pts',(-0.220492620940013,0.0882880516295587,
-0.901857447206898));
#71393=CARTESIAN_POINT('Ctrl Pts',(-0.229261579111557,0.0624864779643527,
-0.899878788967944));
#71394=CARTESIAN_POINT('Ctrl Pts',(-0.232674680326883,0.0482487333022393,
-0.898800453416702));
#71395=CARTESIAN_POINT('Ctrl Pts',(-0.235411728918039,0.0292315402947884,
-0.897431290780465));
#71396=CARTESIAN_POINT('Ctrl Pts',(-0.235934711108775,0.0246573299949662,
-0.897107475104667));
#71397=CARTESIAN_POINT('Ctrl Pts',(-0.23643022784052,0.0188227514627737,
-0.896703719396755));
#71398=CARTESIAN_POINT('Ctrl Pts',(-0.236526312246819,0.017574196914112,
-0.896617858352744));
#71399=CARTESIAN_POINT('Ctrl Pts',(-0.236663091987083,0.0155917170641874,
-0.896482443259699));
#71400=CARTESIAN_POINT('Ctrl Pts',(-0.236710270532387,0.0148582842783356,
-0.896432544350279));
#71401=CARTESIAN_POINT('Ctrl Pts',(-0.236791755443785,0.0134924516889735,
-0.896340005136011));
#71402=CARTESIAN_POINT('Ctrl Pts',(-0.236826938044166,0.0128601370356045,
-0.896297319035144));
#71403=CARTESIAN_POINT('Ctrl Pts',(-0.236893394091507,0.0115728309164111,
-0.896210721248901));
#71404=CARTESIAN_POINT('Ctrl Pts',(-0.236924484243125,0.0109178464712578,
-0.896166820274818));
#71405=CARTESIAN_POINT('Ctrl Pts',(-0.236990819385654,0.00938625604526191,
-0.896064520674928));
#71406=CARTESIAN_POINT('Ctrl Pts',(-0.237023918043973,0.00850955986828271,
-0.896006236543748));
#71407=CARTESIAN_POINT('Ctrl Pts',(-0.237133017466511,0.00512120341351875,
-0.89578195832203));
#71408=CARTESIAN_POINT('Ctrl Pts',(-0.237173968865591,0.00260849225459629,
-0.895617730207301));
#71409=CARTESIAN_POINT('Ctrl Pts',(-0.237174980771817,9.55033420706099E-5,
-0.895455149390825));
#71410=CARTESIAN_POINT('Ctrl Pts',(-0.237174980662101,9.5775424050204E-5,
-0.8954551669935));
#71411=CARTESIAN_POINT('Ctrl Pts',(-0.2371833279887,-0.0205752583428094,
-0.89411782880804));
#71412=CARTESIAN_POINT('Ctrl Pts',(-0.234489360101835,-0.041162614077105,
-0.892892067334419));
#71413=CARTESIAN_POINT('Ctrl Pts',(-0.226502289821164,-0.0710973627577832,
-0.890969390586061));
#71414=CARTESIAN_POINT('Ctrl Pts',(-0.223200885745565,-0.0808668486431776,
-0.890319190464305));
#71415=CARTESIAN_POINT('Ctrl Pts',(-0.218416242996458,-0.0924738090747347,
-0.889500763002097));
#71416=CARTESIAN_POINT('Ctrl Pts',(-0.217527632660627,-0.0945451692293766,
-0.889352888167248));
#71417=CARTESIAN_POINT('Ctrl Pts',(-0.21607154873807,-0.0978100806068398,
-0.889116746347139));
#71418=CARTESIAN_POINT('Ctrl Pts',(-0.215523372865828,-0.0990121289090137,
-0.889029139052045));
#71419=CARTESIAN_POINT('Ctrl Pts',(-0.214471084072819,-0.101269454115096,
-0.888863328947414));
#71420=CARTESIAN_POINT('Ctrl Pts',(-0.213969151054201,-0.102325708171585,
-0.888785203332076));
#71421=CARTESIAN_POINT('Ctrl Pts',(-0.212817548923232,-0.104703582438074,
-0.888608079379626));
#71422=CARTESIAN_POINT('Ctrl Pts',(-0.212163345773567,-0.106022940182293,
-0.888508925476395));
#71423=CARTESIAN_POINT('Ctrl Pts',(-0.210144695538564,-0.110000523779266,
-0.88820727898241));
#71424=CARTESIAN_POINT('Ctrl Pts',(-0.208742308037355,-0.11263905054928,
-0.888003465609751));
#71425=CARTESIAN_POINT('Ctrl Pts',(-0.19796257661731,-0.132027601974797,
-0.886477268126378));
#71426=CARTESIAN_POINT('Ctrl Pts',(-0.186633985986837,-0.147607381284134,
-0.885081975229611));
#71427=CARTESIAN_POINT('Ctrl Pts',(-0.171297000813657,-0.164074074110974,
-0.883438992480977));
#71428=CARTESIAN_POINT('Ctrl Pts',(-0.168987590417036,-0.166451672001164,
-0.883197267798034));
#71429=CARTESIAN_POINT('Ctrl Pts',(-0.162136577340472,-0.173215371798461,
-0.882497743174002));
#71430=CARTESIAN_POINT('Ctrl Pts',(-0.157468459187152,-0.177469799783668,
-0.882042539813931));
#71431=CARTESIAN_POINT('Ctrl Pts',(-0.15079225631944,-0.183083253596495,
-0.881425790475272));
#71432=CARTESIAN_POINT('Ctrl Pts',(-0.148925079541231,-0.184605265342825,
-0.88125679631911));
#71433=CARTESIAN_POINT('Ctrl Pts',(-0.146053459246999,-0.186874108374204,
-0.881002533941513));
#71434=CARTESIAN_POINT('Ctrl Pts',(-0.145065810896337,-0.187641829050827,
-0.880916073844857));
#71435=CARTESIAN_POINT('Ctrl Pts',(-0.143253360462092,-0.189027822546557,
-0.880759272098043));
#71436=CARTESIAN_POINT('Ctrl Pts',(-0.142430519645353,-0.189648596493712,
-0.880688774197995));
#71437=CARTESIAN_POINT('Ctrl Pts',(-0.141052432602468,-0.190674235289257,
-0.880571883656095));
#71438=CARTESIAN_POINT('Ctrl Pts',(-0.140499436805848,-0.191082079311968,
-0.880525290836942));
#71439=CARTESIAN_POINT('Ctrl Pts',(-0.139402358511907,-0.191883856139328,
-0.880433485513471));
#71440=CARTESIAN_POINT('Ctrl Pts',(-0.138858363857907,-0.192277889028762,
-0.880388267233697));
#71441=CARTESIAN_POINT('Ctrl Pts',(-0.137636427864242,-0.193155086334715,
-0.880287357921831));
#71442=CARTESIAN_POINT('Ctrl Pts',(-0.136957594889835,-0.193637008100672,
-0.880231750910971));
#71443=CARTESIAN_POINT('Ctrl Pts',(-0.134583351586567,-0.195303815536937,
-0.880038778703969));
#71444=CARTESIAN_POINT('Ctrl Pts',(-0.132874932123937,-0.196470130081977,
-0.879902597292944));
#71445=CARTESIAN_POINT('Ctrl Pts',(-0.120926123331054,-0.204400251875899,
-0.878966866343392));
#71446=CARTESIAN_POINT('Ctrl Pts',(-0.110188147934243,-0.210383555639259,
-0.878209602267129));
#71447=CARTESIAN_POINT('Ctrl Pts',(-0.0889697948786052,-0.220134127059846,
-0.876776498883495));
#71448=CARTESIAN_POINT('Ctrl Pts',(-0.0785941490472483,-0.224048224029627,
-0.876101581428695));
#71449=CARTESIAN_POINT('Ctrl Pts',(-0.0595644883586007,-0.2297417577492,
-0.874861369663294));
#71450=CARTESIAN_POINT('Ctrl Pts',(-0.0510129591517752,-0.231790541007762,
-0.87430336439305));
#71451=CARTESIAN_POINT('Ctrl Pts',(-0.040240880356109,-0.233746286773871,
-0.873588939578593));
#71452=CARTESIAN_POINT('Ctrl Pts',(-0.0381084973051501,-0.234103389461559,
-0.873446983013624));
#71453=CARTESIAN_POINT('Ctrl Pts',(-0.0346854202018894,-0.234628632998662,
-0.873218113645547));
#71454=CARTESIAN_POINT('Ctrl Pts',(-0.0333976735292816,-0.234815393630019,
-0.873131791133101));
#71455=CARTESIAN_POINT('Ctrl Pts',(-0.0309462015268082,-0.235150354752359,
-0.872967006604323));
#71456=CARTESIAN_POINT('Ctrl Pts',(-0.0297827825134924,-0.235300536568753,
-0.872888609765996));
#71457=CARTESIAN_POINT('Ctrl Pts',(-0.0271227830617879,-0.23562386323407,
-0.872708901944158));
#71458=CARTESIAN_POINT('Ctrl Pts',(-0.0256255838670595,-0.235791389909411,
-0.87260741719276));
#71459=CARTESIAN_POINT('Ctrl Pts',(-0.0209778235715432,-0.236266654534565,
-0.872291286249288));
#71460=CARTESIAN_POINT('Ctrl Pts',(-0.0178227363863988,-0.236525578968084,
-0.872075126129018));
#71461=CARTESIAN_POINT('Ctrl Pts',(0.0021219000778639,-0.237761036115639,
-0.870698229641039));
#71462=CARTESIAN_POINT('Ctrl Pts',(0.0189673367611407,-0.237012354393224,
-0.869483519007522));
#71463=CARTESIAN_POINT('Ctrl Pts',(0.0495866263073657,-0.232365231578005,
-0.867222016049639));
#71464=CARTESIAN_POINT('Ctrl Pts',(0.0633675483631206,-0.228991414833525,
-0.866184927746579));
#71465=CARTESIAN_POINT('Ctrl Pts',(0.0784383708613653,-0.223835934910005,
-0.865078497175109));
#71466=CARTESIAN_POINT('Ctrl Pts',(0.0801041033765616,-0.223245239295858,
-0.864956629477448));
#71467=CARTESIAN_POINT('Ctrl Pts',(0.0825531662542952,-0.222345820042513,
-0.864778236736914));
#71468=CARTESIAN_POINT('Ctrl Pts',(0.0833416595325406,-0.222051473290209,
-0.864720922990878));
#71469=CARTESIAN_POINT('Ctrl Pts',(0.0847419942105739,-0.221520214585848,
-0.86461937278853));
#71470=CARTESIAN_POINT('Ctrl Pts',(0.0853544366467714,-0.22128495482819,
-0.864575041685921));
#71471=CARTESIAN_POINT('Ctrl Pts',(0.0866908465595962,-0.220765220878756,
-0.864478489163186));
#71472=CARTESIAN_POINT('Ctrl Pts',(0.0874143955017434,-0.22047972498516,
-0.864426329192201));
#71473=CARTESIAN_POINT('Ctrl Pts',(0.0894455470287741,-0.219666708394509,
-0.864280193266529));
#71474=CARTESIAN_POINT('Ctrl Pts',(0.0907498953274171,-0.219131068992247,
-0.864186685863723));
#71475=CARTESIAN_POINT('Ctrl Pts',(0.0987440397171926,-0.215764596382242,
-0.863615211447208));
#71476=CARTESIAN_POINT('Ctrl Pts',(0.105306345368305,-0.212638996443293,
-0.86315305719111));
#71477=CARTESIAN_POINT('Ctrl Pts',(0.125148109955444,-0.202044089890315,
-0.861746542527685));
#71478=CARTESIAN_POINT('Ctrl Pts',(0.137859132259978,-0.193594320187097,
-0.860830153603925));
#71479=CARTESIAN_POINT('Ctrl Pts',(0.157835757106226,-0.177343140849288,
-0.859233297960712));
#71480=CARTESIAN_POINT('Ctrl Pts',(0.165546872520648,-0.170167291408317,
-0.858569765083902));
#71481=CARTESIAN_POINT('Ctrl Pts',(0.174307683228324,-0.160853796874688,
-0.857736316400822));
#71482=CARTESIAN_POINT('Ctrl Pts',(0.175836049154033,-0.1591816435297,-0.857587702763485));
#71483=CARTESIAN_POINT('Ctrl Pts',(0.178219093141709,-0.156498202685523,
-0.857350653165804));
#71484=CARTESIAN_POINT('Ctrl Pts',(0.179089683945134,-0.155501181950484,
-0.857262885786001));
#71485=CARTESIAN_POINT('Ctrl Pts',(0.180713421334071,-0.153609917489975,
-0.857096941533867));
#71486=CARTESIAN_POINT('Ctrl Pts',(0.181468392684931,-0.152717287081412,
-0.857018843319827));
#71487=CARTESIAN_POINT('Ctrl Pts',(0.183156911309922,-0.150690689120273,
-0.856842010223158));
#71488=CARTESIAN_POINT('Ctrl Pts',(0.18408657883312,-0.149553566566187,
-0.856743121844801));
#71489=CARTESIAN_POINT('Ctrl Pts',(0.186802034108475,-0.146168474290219,
-0.856449668282114));
#71490=CARTESIAN_POINT('Ctrl Pts',(0.188557579829598,-0.143896701320385,
-0.856253914229598));
#71491=CARTESIAN_POINT('Ctrl Pts',(0.20213780965615,-0.125647802440641,
-0.854690062659708));
#71492=CARTESIAN_POINT('Ctrl Pts',(0.211950444148434,-0.108276300980372,
-0.853242877107898));
#71493=CARTESIAN_POINT('Ctrl Pts',(0.222615336530566,-0.0822362210983325,
-0.851189165810966));
#71494=CARTESIAN_POINT('Ctrl Pts',(0.225347647827582,-0.0744233774972007,
-0.850587838837127));
#71495=CARTESIAN_POINT('Ctrl Pts',(0.228857953258422,-0.0624026419056772,
-0.849697986252965));
#71496=CARTESIAN_POINT('Ctrl Pts',(0.229939759067294,-0.0582903524159181,
-0.84939968204986));
#71497=CARTESIAN_POINT('Ctrl Pts',(0.231178202201684,-0.0530093784162907,
-0.849026176563722));
#71498=CARTESIAN_POINT('Ctrl Pts',(0.23143744068887,-0.0518658516146378,
-0.848945866513497));
#71499=CARTESIAN_POINT('Ctrl Pts',(0.231841600007677,-0.0500196732296625,
-0.848817173739897));
#71500=CARTESIAN_POINT('Ctrl Pts',(0.231991827861597,-0.0493182222347262,
-0.848768500860114));
#71501=CARTESIAN_POINT('Ctrl Pts',(0.232275057373258,-0.0479658185022591,
-0.848675103592373));
#71502=CARTESIAN_POINT('Ctrl Pts',(0.232408508817347,-0.0473149771561448,
-0.848630355573465));
#71503=CARTESIAN_POINT('Ctrl Pts',(0.232697317105471,-0.045875754963413,
-0.848531827302156));
#71504=CARTESIAN_POINT('Ctrl Pts',(0.232851407355918,-0.0450871203437479,
-0.848478118062628));
#71505=CARTESIAN_POINT('Ctrl Pts',(0.233382838095572,-0.0422918478131074,
-0.848288690510409));
#71506=CARTESIAN_POINT('Ctrl Pts',(0.233738284786237,-0.0402810678347254,
-0.848154141446342));
#71507=CARTESIAN_POINT('Ctrl Pts',(0.236453887863799,-0.0236700479544012,
-0.847054862999609));
#71508=CARTESIAN_POINT('Ctrl Pts',(0.237469927377849,-0.00888087333447466,
-0.846152508716175));
#71509=CARTESIAN_POINT('Ctrl Pts',(0.236815643676436,0.0173756426311385,
-0.844542863002117));
#71510=CARTESIAN_POINT('Ctrl Pts',(0.235698359733893,0.0288065878120799,
-0.843839540075188));
#71511=CARTESIAN_POINT('Ctrl Pts',(0.233039238763601,0.0443033384358003,
-0.842845799544846));
#71512=CARTESIAN_POINT('Ctrl Pts',(0.232207282796865,0.0484752224073258,
-0.842574303528889));
#71513=CARTESIAN_POINT('Ctrl Pts',(0.230555508365567,0.0557344136510711,
-0.842093256594152));
#71514=CARTESIAN_POINT('Ctrl Pts',(0.229784653622529,0.0588317829199541,
-0.84188521201821));
#71515=CARTESIAN_POINT('Ctrl Pts',(0.228557015864354,0.0633715674101596,
-0.841575700214298));
#71516=CARTESIAN_POINT('Ctrl Pts',(0.228148538908001,0.064826762013574,
-0.841475788334233));
#71517=CARTESIAN_POINT('Ctrl Pts',(0.227398212510716,0.0674048296048628,
-0.8412974877106));
#71518=CARTESIAN_POINT('Ctrl Pts',(0.227061880769916,0.0685292661815689,
-0.841219280777512));
#71519=CARTESIAN_POINT('Ctrl Pts',(0.226335864440256,0.0708924780171649,
-0.84105396276005));
#71520=CARTESIAN_POINT('Ctrl Pts',(0.225944324798897,0.0721306380538118,
-0.840966793114157));
#71521=CARTESIAN_POINT('Ctrl Pts',(0.224877595502658,0.0754100125288046,
-0.840734408415306));
#71522=CARTESIAN_POINT('Ctrl Pts',(0.224184798069977,0.0774453273721836,
-0.840588618926588));
#71523=CARTESIAN_POINT('Ctrl Pts',(0.220944960016308,0.0865554387302815,
-0.839928819321502));
#71524=CARTESIAN_POINT('Ctrl Pts',(0.21809026665488,0.0935154180634417,
-0.839404751213831));
#71525=CARTESIAN_POINT('Ctrl Pts',(0.208295972394384,0.114495646493638,
-0.837761968967058));
#71526=CARTESIAN_POINT('Ctrl Pts',(0.200297381014247,0.127973940981892,
-0.836613311660793));
#71527=CARTESIAN_POINT('Ctrl Pts',(0.186969679747982,0.146086642333035,
-0.834976586780541));
#71528=CARTESIAN_POINT('Ctrl Pts',(0.182669372368285,0.151429459658708,
-0.83448106533778));
#71529=CARTESIAN_POINT('Ctrl Pts',(0.17565028083982,0.159415245438648,-0.833728148827456));
#71530=CARTESIAN_POINT('Ctrl Pts',(0.173089616222914,0.162191955302024,
-0.833463886762648));
#71531=CARTESIAN_POINT('Ctrl Pts',(0.169680542239703,0.165715908868075,
-0.833126549843501));
#71532=CARTESIAN_POINT('Ctrl Pts',(0.1688917528536,0.166519743009972,-0.833049464633647));
#71533=CARTESIAN_POINT('Ctrl Pts',(0.167598402441187,0.167819117331175,
-0.832924680193496));
#71534=CARTESIAN_POINT('Ctrl Pts',(0.167097309497062,0.168318061523262,
-0.832876720949228));
#71535=CARTESIAN_POINT('Ctrl Pts',(0.166117052787265,0.169285422822658,
-0.832783665329727));
#71536=CARTESIAN_POINT('Ctrl Pts',(0.165638125573272,0.16975406027289,-0.832738552611137));
#71537=CARTESIAN_POINT('Ctrl Pts',(0.164564218738812,0.170796022240532,
-0.832638160610473));
#71538=CARTESIAN_POINT('Ctrl Pts',(0.163968210096285,0.17136828595456,-0.832582962528883));
#71539=CARTESIAN_POINT('Ctrl Pts',(0.161896021252461,0.173337210642539,
-0.832392783827761));
#71540=CARTESIAN_POINT('Ctrl Pts',(0.160404840309692,0.174718053373907,
-0.832258942536074));
#71541=CARTESIAN_POINT('Ctrl Pts',(0.148502535299551,0.185458814417964,
-0.831212371159709));
#71542=CARTESIAN_POINT('Ctrl Pts',(0.137297497147454,0.193900696884352,
-0.830355239188223));
#71543=CARTESIAN_POINT('Ctrl Pts',(0.11200086852914,0.209660297054008,-0.828528525171795));
#71544=CARTESIAN_POINT('Ctrl Pts',(0.0977902934622816,0.216653231324984,
-0.827561605299581));
#71545=CARTESIAN_POINT('Ctrl Pts',(0.0795799210739103,0.223455306973142,
-0.826310146657614));
#71546=CARTESIAN_POINT('Ctrl Pts',(0.076140300878525,0.224650596085608,
-0.826073434051857));
#71547=CARTESIAN_POINT('Ctrl Pts',(0.0711594475923189,0.226253944631179,
-0.825729499993171));
#71548=CARTESIAN_POINT('Ctrl Pts',(0.0696393805797029,0.226726423048257,
-0.825624386809163));
#71549=CARTESIAN_POINT('Ctrl Pts',(0.0669795384547398,0.227523903116119,
-0.825440141227738));
#71550=CARTESIAN_POINT('Ctrl Pts',(0.0658418566889726,0.227855732605556,
-0.825361234559976));
#71551=CARTESIAN_POINT('Ctrl Pts',(0.0634870072887151,0.228523466593681,
-0.825197678987938));
#71552=CARTESIAN_POINT('Ctrl Pts',(0.0622695509014142,0.2288582045767,-0.825112995027067));
#71553=CARTESIAN_POINT('Ctrl Pts',(0.0591322035722137,0.229693926764797,
-0.824894414979077));
#71554=CARTESIAN_POINT('Ctrl Pts',(0.0572086265134711,0.230180559836876,
-0.824760060662697));
#71555=CARTESIAN_POINT('Ctrl Pts',(0.0494064273457805,0.23205054724841,
-0.824213606799371));
#71556=CARTESIAN_POINT('Ctrl Pts',(0.0434825218316268,0.23323316758651,
-0.823795197737063));
#71557=CARTESIAN_POINT('Ctrl Pts',(0.0208489583708216,0.236859393391516,
-0.822182413451291));
#71558=CARTESIAN_POINT('Ctrl Pts',(0.00394170992783503,0.23774223495821,
-0.82094419783548));
#71559=CARTESIAN_POINT('Ctrl Pts',(-0.0226485214267444,0.236292375576695,
-0.819004074324007));
#71560=CARTESIAN_POINT('Ctrl Pts',(-0.0323423762680234,0.235161698747638,
-0.818299570554947));
#71561=CARTESIAN_POINT('Ctrl Pts',(-0.0419392746656718,0.233437524544614,
-0.817620397237267));
#71562=CARTESIAN_POINT('Origin',(0.,0.,-2.1456589891905));
#71563=CARTESIAN_POINT('',(-0.0419392741328079,0.233437524640348,-0.698115075114807));
#71564=CARTESIAN_POINT('',(-0.0419393227885566,0.233437515898874,-0.717844391575082));
#71565=CARTESIAN_POINT('',(-0.0419392741328076,0.233437524640348,-2.1456589891905));
#71566=CARTESIAN_POINT('',(-0.237174928456985,-0.000184218414099613,-0.775941010809497));
#71567=CARTESIAN_POINT('Ctrl Pts',(-0.237174928456985,-0.000184218414099613,
-0.775941010809497));
#71568=CARTESIAN_POINT('Ctrl Pts',(-0.237162061016635,-0.0167506092354838,
-0.774832628374937));
#71569=CARTESIAN_POINT('Ctrl Pts',(-0.235409393017015,-0.0332436070647559,
-0.773724245940377));
#71570=CARTESIAN_POINT('Ctrl Pts',(-0.23198655433952,-0.0493378073152505,
-0.772615863505817));
#71571=CARTESIAN_POINT('Ctrl Pts',(-0.229974034838635,-0.0588006815278866,
-0.771964170138362));
#71572=CARTESIAN_POINT('Ctrl Pts',(-0.227385071187055,-0.0681260551951133,
-0.771312476770907));
#71573=CARTESIAN_POINT('Ctrl Pts',(-0.224241480738865,-0.077251142004771,
-0.770660783403453));
#71574=CARTESIAN_POINT('Ctrl Pts',(-0.219669392181079,-0.0905228151692113,
-0.76971295007795));
#71575=CARTESIAN_POINT('Ctrl Pts',(-0.213899560933309,-0.103431980680553,
-0.768765116752448));
#71576=CARTESIAN_POINT('Ctrl Pts',(-0.207011145932222,-0.115751311374119,
-0.767817283426946));
#71577=CARTESIAN_POINT('Ctrl Pts',(-0.200136684144792,-0.128045687959483,
-0.766871370038164));
#71578=CARTESIAN_POINT('Ctrl Pts',(-0.192148477163569,-0.139751845841727,
-0.765925456649382));
#71579=CARTESIAN_POINT('Ctrl Pts',(-0.183172969367591,-0.150664010029136,
-0.764979543260599));
#71580=CARTESIAN_POINT('Ctrl Pts',(-0.174198898800311,-0.161574426875236,
-0.764033781338887));
#71581=CARTESIAN_POINT('Ctrl Pts',(-0.164238331879677,-0.171690427447469,
-0.763088019417175));
#71582=CARTESIAN_POINT('Ctrl Pts',(-0.153459453442516,-0.180837431894296,
-0.762142257495463));
#71583=CARTESIAN_POINT('Ctrl Pts',(-0.142682378474369,-0.189982905909254,
-0.761196653813992));
#71584=CARTESIAN_POINT('Ctrl Pts',(-0.131087912400795,-0.198159179364291,
-0.76025105013252));
#71585=CARTESIAN_POINT('Ctrl Pts',(-0.118877396065784,-0.20523193058006,
-0.759305446451049));
#71586=CARTESIAN_POINT('Ctrl Pts',(-0.10663829229987,-0.212321240619481,
-0.758357628909069));
#71587=CARTESIAN_POINT('Ctrl Pts',(-0.0937810050099268,-0.21830148975904,
-0.757409811367089));
#71588=CARTESIAN_POINT('Ctrl Pts',(-0.0805311358005377,-0.223084550768706,
-0.756461993825109));
#71589=CARTESIAN_POINT('Ctrl Pts',(-0.0726787485432168,-0.225919178547271,
-0.755900280326561));
#71590=CARTESIAN_POINT('Ctrl Pts',(-0.0646888594965764,-0.228334261078944,
-0.755338566828013));
#71591=CARTESIAN_POINT('Ctrl Pts',(-0.0566104850057974,-0.230319850669473,
-0.754776853329465));
#71592=CARTESIAN_POINT('Ctrl Pts',(-0.0429790651128494,-0.23367032736184,
-0.753829020003963));
#71593=CARTESIAN_POINT('Ctrl Pts',(-0.029003155145229,-0.235817755452354,
-0.752881186678461));
#71594=CARTESIAN_POINT('Ctrl Pts',(-0.0149167021231715,-0.236705455414041,
-0.751933353352959));
#71595=CARTESIAN_POINT('Ctrl Pts',(-0.000858782702629119,-0.237591357245501,
-0.750987439964177));
#71596=CARTESIAN_POINT('Ctrl Pts',(0.0133084155970279,-0.237222473148615,
-0.750041526575395));
#71597=CARTESIAN_POINT('Ctrl Pts',(0.0273434308589045,-0.235593542810206,
-0.749095613186613));
#71598=CARTESIAN_POINT('Ctrl Pts',(0.0413761987240736,-0.233964873308897,
-0.748149851264901));
#71599=CARTESIAN_POINT('Ctrl Pts',(0.0552759924229695,-0.231076604608448,
-0.747204089343188));
#71600=CARTESIAN_POINT('Ctrl Pts',(0.0688049442860343,-0.226975461816461,
-0.746258327421476));
#71601=CARTESIAN_POINT('Ctrl Pts',(0.0823316325513042,-0.222875005207548,
-0.745312723740004));
#71602=CARTESIAN_POINT('Ctrl Pts',(0.0954868083391503,-0.217562337221152,
-0.744367120058533));
#71603=CARTESIAN_POINT('Ctrl Pts',(0.108048467294751,-0.211133865924572,
-0.743421516377061));
#71604=CARTESIAN_POINT('Ctrl Pts',(0.120639535781249,-0.204690344201461,
-0.742473698835081));
#71605=CARTESIAN_POINT('Ctrl Pts',(0.132633588921921,-0.197126224590689,
-0.741525881293101));
#71606=CARTESIAN_POINT('Ctrl Pts',(0.14383429546831,-0.188583339858363,
-0.740578063751121));
#71607=CARTESIAN_POINT('Ctrl Pts',(0.150472269320576,-0.183520494470776,
-0.740016350252573));
#71608=CARTESIAN_POINT('Ctrl Pts',(0.156832180133812,-0.178114711913168,
-0.739454636754024));
#71609=CARTESIAN_POINT('Ctrl Pts',(0.162879102495285,-0.172401794060649,
-0.738892923255476));
#71610=CARTESIAN_POINT('Ctrl Pts',(0.173082657413835,-0.162761837142276,
-0.737945089929974));
#71611=CARTESIAN_POINT('Ctrl Pts',(0.182461876269478,-0.152180355181562,
-0.736997256604472));
#71612=CARTESIAN_POINT('Ctrl Pts',(0.190842333428052,-0.140823238127577,
-0.73604942327897));
#71613=CARTESIAN_POINT('Ctrl Pts',(0.199205815083659,-0.129489126116228,
-0.735103509890188));
#71614=CARTESIAN_POINT('Ctrl Pts',(0.206574003311319,-0.11738311994654,
-0.734157596501406));
#71615=CARTESIAN_POINT('Ctrl Pts',(0.212811612220942,-0.104705292745512,
-0.733211683112624));
#71616=CARTESIAN_POINT('Ctrl Pts',(0.21904822231571,-0.0920294956175973,
-0.732265921190912));
#71617=CARTESIAN_POINT('Ctrl Pts',(0.224154200017897,-0.0787827846045709,
-0.731320159269199));
#71618=CARTESIAN_POINT('Ctrl Pts',(0.228039895844241,-0.0651903867786343,
-0.730374397347487));
#71619=CARTESIAN_POINT('Ctrl Pts',(0.231924941535039,-0.0516002631659596,
-0.729428793666016));
#71620=CARTESIAN_POINT('Ctrl Pts',(0.234589898825739,-0.0376653755172719,
-0.728483189984544));
#71621=CARTESIAN_POINT('Ctrl Pts',(0.235995469124175,-0.0236245460879286,
-0.727537586303073));
#71622=CARTESIAN_POINT('Ctrl Pts',(0.237404330163369,-0.00955084407317458,
-0.726589768761093));
#71623=CARTESIAN_POINT('Ctrl Pts',(0.237547878768334,0.00462845809672525,
-0.725641951219113));
#71624=CARTESIAN_POINT('Ctrl Pts',(0.236438905218546,0.01867149496038,-0.724694133677133));
#71625=CARTESIAN_POINT('Ctrl Pts',(0.235781684408782,0.0269939441845676,
-0.724132420178585));
#71626=CARTESIAN_POINT('Ctrl Pts',(0.234685558114345,0.0352685715332205,
-0.723570706680036));
#71627=CARTESIAN_POINT('Ctrl Pts',(0.233161685622907,0.0434466222218101,
-0.723008993181488));
#71628=CARTESIAN_POINT('Ctrl Pts',(0.230590308693327,0.0572462353703723,
-0.722061159855986));
#71629=CARTESIAN_POINT('Ctrl Pts',(0.226780910724152,0.0708633567232648,
-0.721113326530485));
#71630=CARTESIAN_POINT('Ctrl Pts',(0.221778371785606,0.0840614919753727,
-0.720165493204983));
#71631=CARTESIAN_POINT('Ctrl Pts',(0.216785966019151,0.0972328930076286,
-0.719219579816201));
#71632=CARTESIAN_POINT('Ctrl Pts',(0.210605442854837,0.10998619518997,-0.718273666427419));
#71633=CARTESIAN_POINT('Ctrl Pts',(0.203331622400047,0.122099270911684,
-0.717327753038637));
#71634=CARTESIAN_POINT('Ctrl Pts',(0.19605896668643,0.13421040699272,-0.716381991116925));
#71635=CARTESIAN_POINT('Ctrl Pts',(0.187693747281197,0.145680780363284,
-0.715436229195212));
#71636=CARTESIAN_POINT('Ctrl Pts',(0.178376657178569,0.156312983462025,
-0.7144904672735));
#71637=CARTESIAN_POINT('Ctrl Pts',(0.169061125965707,0.166943407632751,
-0.713544863592029));
#71638=CARTESIAN_POINT('Ctrl Pts',(0.158794604413171,0.176735324010771,
-0.712599259910558));
#71639=CARTESIAN_POINT('Ctrl Pts',(0.147756499553455,0.185526271629411,
-0.711653656229086));
#71640=CARTESIAN_POINT('Ctrl Pts',(0.13669255212891,0.194337800737049,-0.710705838687106));
#71641=CARTESIAN_POINT('Ctrl Pts',(0.124854097086247,0.20214319620622,-0.709758021145126));
#71642=CARTESIAN_POINT('Ctrl Pts',(0.11245132957152,0.208822123115817,-0.708810203603146));
#71643=CARTESIAN_POINT('Ctrl Pts',(0.105100967688763,0.212780314681992,
-0.708248490104597));
#71644=CARTESIAN_POINT('Ctrl Pts',(0.0975529215632221,0.21634373302667,
-0.707686776606049));
#71645=CARTESIAN_POINT('Ctrl Pts',(0.0898542126077082,0.219495332755958,
-0.707125063107501));
#71646=CARTESIAN_POINT('Ctrl Pts',(0.0768636571902303,0.224813241404485,
-0.706177245704115));
#71647=CARTESIAN_POINT('Ctrl Pts',(0.0633555145593011,0.228991853235572,
-0.705229428300729));
#71648=CARTESIAN_POINT('Ctrl Pts',(0.0495528462405892,0.231940716680915,
-0.704281610897343));
#71649=CARTESIAN_POINT('Ctrl Pts',(0.0357780041000708,0.234883635217795,
-0.703335704293765));
#71650=CARTESIAN_POINT('Ctrl Pts',(0.0217106075155237,0.236601484212659,
-0.702389797690186));
#71651=CARTESIAN_POINT('Ctrl Pts',(0.00758871636857107,0.237053563586117,
-0.701443891086607));
#71652=CARTESIAN_POINT('Ctrl Pts',(-0.0065210615412059,0.237505255182569,
-0.700498795846812));
#71653=CARTESIAN_POINT('Ctrl Pts',(-0.0206844113366518,0.236693274397738,
-0.699553700607018));
#71654=CARTESIAN_POINT('Ctrl Pts',(-0.0346596912665034,0.234628826929494,
-0.698608605367223));
#71655=CARTESIAN_POINT('Ctrl Pts',(-0.0370923291428906,0.234269474334751,
-0.698444095283084));
#71656=CARTESIAN_POINT('Ctrl Pts',(-0.039519276226885,0.233872300307772,
-0.698279585198946));
#71657=CARTESIAN_POINT('Ctrl Pts',(-0.0419392741328079,0.233437524640348,
-0.698115075114807));
#71658=CARTESIAN_POINT('Ctrl Pts',(-0.0419215622832843,0.23334603455685,
-0.798097588861632));
#71659=CARTESIAN_POINT('Ctrl Pts',(-0.0983464490172812,0.2226473034456,
-0.794246630400235));
#71660=CARTESIAN_POINT('Ctrl Pts',(-0.200199235814832,0.163360521026062,
-0.786861104382857));
#71661=CARTESIAN_POINT('Ctrl Pts',(-0.236573687440461,0.0525967050833675,
-0.779475578365479));
#71662=CARTESIAN_POINT('Ctrl Pts',(-0.236955669095664,-0.000184048111057593,
-0.775941010809497));
#71663=CARTESIAN_POINT('Ctrl Pts',(-0.0419392746656718,0.233437524544614,
-0.817620397237267));
#71664=CARTESIAN_POINT('Ctrl Pts',(-0.0427439480341241,0.233292957309841,
-0.817563450434388));
#71665=CARTESIAN_POINT('Ctrl Pts',(-0.0435479399485291,0.233144217572963,
-0.817506684327751));
#71666=CARTESIAN_POINT('Ctrl Pts',(-0.0457952628982983,0.232716426896028,
-0.817348411761257));
#71667=CARTESIAN_POINT('Ctrl Pts',(-0.0472367674736412,0.232428116896829,
-0.81724735352858));
#71668=CARTESIAN_POINT('Ctrl Pts',(-0.0494407928101261,0.231965945750991,
-0.817093643268754));
#71669=CARTESIAN_POINT('Ctrl Pts',(-0.0502052580879215,0.231801691293878,
-0.817040477952749));
#71670=CARTESIAN_POINT('Ctrl Pts',(-0.0516093200306797,0.231492740042138,
-0.816943123131538));
#71671=CARTESIAN_POINT('Ctrl Pts',(-0.0522491310536985,0.231349171016976,
-0.816898873505168));
#71672=CARTESIAN_POINT('Ctrl Pts',(-0.0537036484141713,0.231016445826355,
-0.816798531125211));
#71673=CARTESIAN_POINT('Ctrl Pts',(-0.0545179561465916,0.23082563247276,
-0.816742533375943));
#71674=CARTESIAN_POINT('Ctrl Pts',(-0.0566436695176156,0.230315646246639,
-0.81659678032813));
#71675=CARTESIAN_POINT('Ctrl Pts',(-0.0579534118856586,0.229989574678711,
-0.816507401155402));
#71676=CARTESIAN_POINT('Ctrl Pts',(-0.0689112921291509,0.227161962753133,
-0.81576263758787));
#71677=CARTESIAN_POINT('Ctrl Pts',(-0.0783969782197981,0.224065367249695,
-0.815137441683313));
#71678=CARTESIAN_POINT('Ctrl Pts',(-0.101823092521564,0.214747169635626,
-0.813578980107706));
#71679=CARTESIAN_POINT('Ctrl Pts',(-0.115409133106069,0.207761930697755,
-0.812659435693295));
#71680=CARTESIAN_POINT('Ctrl Pts',(-0.134955309620725,0.19519973824423,
-0.811203347655245));
#71681=CARTESIAN_POINT('Ctrl Pts',(-0.141456188803627,0.190541332177932,
-0.810694120162893));
#71682=CARTESIAN_POINT('Ctrl Pts',(-0.149354899955749,0.184253953979465,
-0.810034902534873));
#71683=CARTESIAN_POINT('Ctrl Pts',(-0.150983182973067,0.182922069986648,
-0.80989671526072));
#71684=CARTESIAN_POINT('Ctrl Pts',(-0.153579910783673,0.180739735242425,
-0.809672476306788));
#71685=CARTESIAN_POINT('Ctrl Pts',(-0.154559540091236,0.179902721900582,
-0.809586972385282));
#71686=CARTESIAN_POINT('Ctrl Pts',(-0.156420261271962,0.178286471474932,
-0.809422786141139));
#71687=CARTESIAN_POINT('Ctrl Pts',(-0.157302474240647,0.177508578832443,
-0.809344161038006));
#71688=CARTESIAN_POINT('Ctrl Pts',(-0.159300830895344,0.175719928401452,
-0.809164248558111));
#71689=CARTESIAN_POINT('Ctrl Pts',(-0.160413198509322,0.174705047217267,
-0.809062789319625));
#71690=CARTESIAN_POINT('Ctrl Pts',(-0.163895048885713,0.171467052294824,
-0.808740974528823));
#71691=CARTESIAN_POINT('Ctrl Pts',(-0.166228466807851,0.169205886629669,
-0.808519000051947));
#71692=CARTESIAN_POINT('Ctrl Pts',(-0.18587961973296,0.149364341245727,
-0.806593439920735));
#71693=CARTESIAN_POINT('Ctrl Pts',(-0.200399580666512,0.129230042450441,
-0.804762652866216));
#71694=CARTESIAN_POINT('Ctrl Pts',(-0.213645103211607,0.103098002229832,
-0.802650700491467));
#71695=CARTESIAN_POINT('Ctrl Pts',(-0.215617582829886,0.0989064786785701,
-0.802319892744766));
#71696=CARTESIAN_POINT('Ctrl Pts',(-0.218249638930465,0.0928597287886012,
-0.801856286021236));
#71697=CARTESIAN_POINT('Ctrl Pts',(-0.21901076420458,0.0910500953094566,
-0.80171923952589));
#71698=CARTESIAN_POINT('Ctrl Pts',(-0.220320986606933,0.0878234136081048,
-0.801478129327539));
#71699=CARTESIAN_POINT('Ctrl Pts',(-0.220879090816275,0.0864101652535897,
-0.801373618372736));
#71700=CARTESIAN_POINT('Ctrl Pts',(-0.221707476869052,0.0842520201662678,
-0.801215781523344));
#71701=CARTESIAN_POINT('Ctrl Pts',(-0.221987658619029,0.0835110032798849,
-0.801161900226131));
#71702=CARTESIAN_POINT('Ctrl Pts',(-0.222492744930583,0.0821546605187406,
-0.801063866257287));
#71703=CARTESIAN_POINT('Ctrl Pts',(-0.222718814786106,0.0815398022730665,
-0.80101964736757));
#71704=CARTESIAN_POINT('Ctrl Pts',(-0.223223458488964,0.0801495291375546,
-0.800920158752538));
#71705=CARTESIAN_POINT('Ctrl Pts',(-0.223500541595484,0.079373593837259,
-0.800864977050514));
#71706=CARTESIAN_POINT('Ctrl Pts',(-0.224207063465765,0.07736203479027,
-0.800722773509264));
#71707=CARTESIAN_POINT('Ctrl Pts',(-0.224630340348941,0.0761242544753688,
-0.800636098483587));
#71708=CARTESIAN_POINT('Ctrl Pts',(-0.227522305359091,0.0674331292638725,
-0.800032864484715));
#71709=CARTESIAN_POINT('Ctrl Pts',(-0.229630071510987,0.0598638830467814,
-0.799534926892895));
#71710=CARTESIAN_POINT('Ctrl Pts',(-0.235212554831166,0.0351229649092346,
-0.797953706516104));
#71711=CARTESIAN_POINT('Ctrl Pts',(-0.237163286780622,0.0176685248323082,
-0.796904759483021));
#71712=CARTESIAN_POINT('Ctrl Pts',(-0.237180144425426,-0.00764632315616661,
-0.795317854475676));
#71713=CARTESIAN_POINT('Ctrl Pts',(-0.23680014498452,-0.0154453587996077,
-0.794820676130295));
#71714=CARTESIAN_POINT('Ctrl Pts',(-0.235824625894277,-0.0253656065722973,
-0.794170228461875));
#71715=CARTESIAN_POINT('Ctrl Pts',(-0.235583254857002,-0.0275172254358308,
-0.794028076089512));
#71716=CARTESIAN_POINT('Ctrl Pts',(-0.235149632666643,-0.0309568372463856,
-0.793798966127605));
#71717=CARTESIAN_POINT('Ctrl Pts',(-0.234976167756467,-0.0322471081999229,
-0.793712601073455));
#71718=CARTESIAN_POINT('Ctrl Pts',(-0.234626242819097,-0.0346970110183,
-0.793547784177764));
#71719=CARTESIAN_POINT('Ctrl Pts',(-0.234451785053246,-0.0358568932435544,
-0.79346939792067));
#71720=CARTESIAN_POINT('Ctrl Pts',(-0.23403380056031,-0.0385022963889381,
-0.793289783459555));
#71721=CARTESIAN_POINT('Ctrl Pts',(-0.233784721948673,-0.0399868757635025,
-0.793188382140547));
#71722=CARTESIAN_POINT('Ctrl Pts',(-0.232969186852884,-0.0445793476358548,
-0.792872776912732));
#71723=CARTESIAN_POINT('Ctrl Pts',(-0.232354777014379,-0.0476782568799442,
-0.792657066319692));
#71724=CARTESIAN_POINT('Ctrl Pts',(-0.230780367643786,-0.0548636285042661,
-0.792150248702046));
#71725=CARTESIAN_POINT('Ctrl Pts',(-0.22977343644788,-0.0589386120441784,
-0.791857745655845));
#71726=CARTESIAN_POINT('Ctrl Pts',(-0.225682199945196,-0.0737914333972743,
-0.790772796770028));
#71727=CARTESIAN_POINT('Ctrl Pts',(-0.221943348726598,-0.0843725728000726,
-0.789962176969947));
#71728=CARTESIAN_POINT('Ctrl Pts',(-0.21140519444329,-0.108585723379124,
-0.788035927796551));
#71729=CARTESIAN_POINT('Ctrl Pts',(-0.204013255533633,-0.121908505732966,
-0.786917862671433));
#71730=CARTESIAN_POINT('Ctrl Pts',(-0.194254849949772,-0.136092212219059,
-0.785718376341118));
#71731=CARTESIAN_POINT('Ctrl Pts',(-0.193092140386242,-0.137736933875552,
-0.785579177629066));
#71732=CARTESIAN_POINT('Ctrl Pts',(-0.191392931678547,-0.140076751716148,
-0.785381220564546));
#71733=CARTESIAN_POINT('Ctrl Pts',(-0.190873343445992,-0.140783939039688,
-0.785321399383733));
#71734=CARTESIAN_POINT('Ctrl Pts',(-0.189955189132845,-0.142019169039291,
-0.785216950935694));
#71735=CARTESIAN_POINT('Ctrl Pts',(-0.189558321272216,-0.142548451881185,
-0.785172209657846));
#71736=CARTESIAN_POINT('Ctrl Pts',(-0.188709587452447,-0.14367055299265,
-0.785077392645125));
#71737=CARTESIAN_POINT('Ctrl Pts',(-0.1882571376529,-0.144262907065752,
-0.78502735826662));
#71738=CARTESIAN_POINT('Ctrl Pts',(-0.187008078339073,-0.145882310860354,
-0.784890594596281));
#71739=CARTESIAN_POINT('Ctrl Pts',(-0.186205792651359,-0.146904979354377,
-0.784804252124217));
#71740=CARTESIAN_POINT('Ctrl Pts',(-0.181682688967277,-0.152573959247149,
-0.784325439745302));
#71741=CARTESIAN_POINT('Ctrl Pts',(-0.177796047330419,-0.15708593701531,
-0.783943621767476));
#71742=CARTESIAN_POINT('Ctrl Pts',(-0.16565224695839,-0.17015462988163,
-0.782818741546131));
#71743=CARTESIAN_POINT('Ctrl Pts',(-0.156917501334763,-0.178241965996434,
-0.782095878856134));
#71744=CARTESIAN_POINT('Ctrl Pts',(-0.135783087408427,-0.195047055222898,
-0.780439296513251));
#71745=CARTESIAN_POINT('Ctrl Pts',(-0.123083164659989,-0.203299894677737,
-0.779503880942169));
#71746=CARTESIAN_POINT('Ctrl Pts',(-0.107560955247797,-0.211396223314265,
-0.778364632025009));
#71747=CARTESIAN_POINT('Ctrl Pts',(-0.10541980478391,-0.212472083811336,
-0.778207642154079));
#71748=CARTESIAN_POINT('Ctrl Pts',(-0.102033058506635,-0.214110022020128,
-0.777959383267467));
#71749=CARTESIAN_POINT('Ctrl Pts',(-0.100798240656284,-0.214694110552981,
-0.777868879819812));
#71750=CARTESIAN_POINT('Ctrl Pts',(-0.0985108045338502,-0.215752020577913,
-0.777701215433239));
#71751=CARTESIAN_POINT('Ctrl Pts',(-0.0974596344063058,-0.216228889313234,
-0.777624162451613));
#71752=CARTESIAN_POINT('Ctrl Pts',(-0.0951190938234653,-0.217270153421073,
-0.777452564706434));
#71753=CARTESIAN_POINT('Ctrl Pts',(-0.0938281044018087,-0.217830778939077,
-0.777357894339669));
#71754=CARTESIAN_POINT('Ctrl Pts',(-0.0900813404126108,-0.21941836303876,
-0.777083035097977));
#71755=CARTESIAN_POINT('Ctrl Pts',(-0.0876132378049596,-0.220415483766243,
-0.776901848048038));
#71756=CARTESIAN_POINT('Ctrl Pts',(-0.0819864812091353,-0.222579273663771,
-0.776488332456942));
#71757=CARTESIAN_POINT('Ctrl Pts',(-0.0788187701944008,-0.223720619645481,
-0.776255217364598));
#71758=CARTESIAN_POINT('Ctrl Pts',(-0.068183827309296,-0.227298556717051,
-0.775471375879996));
#71759=CARTESIAN_POINT('Ctrl Pts',(-0.0606205702085482,-0.229431457529129,
-0.774911770987888));
#71760=CARTESIAN_POINT('Ctrl Pts',(-0.0366642910276418,-0.234920003276817,
-0.773137545533251));
#71761=CARTESIAN_POINT('Ctrl Pts',(-0.0200138367804017,-0.236920051691439,
-0.771898566770572));
#71762=CARTESIAN_POINT('Ctrl Pts',(0.00138735010707077,-0.237217102158682,
-0.77037261576576));
#71763=CARTESIAN_POINT('Ctrl Pts',(0.00606768302189341,-0.237143561159798,
-0.770043264992721));
#71764=CARTESIAN_POINT('Ctrl Pts',(0.0119989879116246,-0.236874619439597,
-0.769633834273039));
#71765=CARTESIAN_POINT('Ctrl Pts',(0.0132544077875595,-0.236807689686453,
-0.769547627852372));
#71766=CARTESIAN_POINT('Ctrl Pts',(0.0152439140481402,-0.236685752503537,
-0.769411794975062));
#71767=CARTESIAN_POINT('Ctrl Pts',(0.0159783568812277,-0.236637305813183,
-0.769361820135098));
#71768=CARTESIAN_POINT('Ctrl Pts',(0.0173752056995839,-0.236538631353395,
-0.769267108875787));
#71769=CARTESIAN_POINT('Ctrl Pts',(0.018037622085949,-0.236489040117381,
-0.769222340795759));
#71770=CARTESIAN_POINT('Ctrl Pts',(0.0196088924895617,-0.23636476788746,
-0.76911648222918));
#71771=CARTESIAN_POINT('Ctrl Pts',(0.020517537455653,-0.236287627455589,
-0.769055528749612));
#71772=CARTESIAN_POINT('Ctrl Pts',(0.0235752021646285,-0.236010272441571,
-0.768851233137706));
#71773=CARTESIAN_POINT('Ctrl Pts',(0.025722002965479,-0.235785958505809,
-0.768709157500939));
#71774=CARTESIAN_POINT('Ctrl Pts',(0.0309463351775337,-0.235167874391955,
-0.768366076001241));
#71775=CARTESIAN_POINT('Ctrl Pts',(0.0340198437549295,-0.234742959341649,
-0.768166500696405));
#71776=CARTESIAN_POINT('Ctrl Pts',(0.0465105498680658,-0.232765613220388,
-0.767361448000405));
#71777=CARTESIAN_POINT('Ctrl Pts',(0.0558389099304648,-0.230705669643688,
-0.76677398915997));
#71778=CARTESIAN_POINT('Ctrl Pts',(0.0821653963619249,-0.223201121231705,
-0.765094776298149));
#71779=CARTESIAN_POINT('Ctrl Pts',(0.0987045106109589,-0.216395996570317,
-0.764009004681878));
#71780=CARTESIAN_POINT('Ctrl Pts',(0.117051434692432,-0.206302278211669,
-0.762655019819878));
#71781=CARTESIAN_POINT('Ctrl Pts',(0.119748577671364,-0.204748492142824,
-0.762452034871108));
#71782=CARTESIAN_POINT('Ctrl Pts',(0.123696065740999,-0.2023697200352,-0.76214863539994));
#71783=CARTESIAN_POINT('Ctrl Pts',(0.12497050124483,-0.201585202613731,
-0.762049687231038));
#71784=CARTESIAN_POINT('Ctrl Pts',(0.127229534549637,-0.200164930909991,
-0.761872461863766));
#71785=CARTESIAN_POINT('Ctrl Pts',(0.128217013836075,-0.199533834991098,
-0.76179435843368));
#71786=CARTESIAN_POINT('Ctrl Pts',(0.130295619607261,-0.198183601191193,
-0.761628584669387));
#71787=CARTESIAN_POINT('Ctrl Pts',(0.131385557361585,-0.197462714121037,
-0.761540850765289));
#71788=CARTESIAN_POINT('Ctrl Pts',(0.13428402856137,-0.195511037583469,
-0.76130533267886));
#71789=CARTESIAN_POINT('Ctrl Pts',(0.136081547192064,-0.194264196644445,
-0.761156946289835));
#71790=CARTESIAN_POINT('Ctrl Pts',(0.145324380039627,-0.187661714471184,
-0.760381521457689));
#71791=CARTESIAN_POINT('Ctrl Pts',(0.15247079473486,-0.181903031942176,
-0.759739059063353));
#71792=CARTESIAN_POINT('Ctrl Pts',(0.167258594018503,-0.168501960438982,
-0.758312872807955));
#71793=CARTESIAN_POINT('Ctrl Pts',(0.174747960349115,-0.160721707881131,
-0.757525643633148));
#71794=CARTESIAN_POINT('Ctrl Pts',(0.189473955934466,-0.143173183720772,
-0.755852602057995));
#71795=CARTESIAN_POINT('Ctrl Pts',(0.196543959832642,-0.133302179247616,
-0.754968974044639));
#71796=CARTESIAN_POINT('Ctrl Pts',(0.203903224972589,-0.12116003208253,
-0.753978558229908));
#71797=CARTESIAN_POINT('Ctrl Pts',(0.204954532321896,-0.119373024341003,
-0.75383511614973));
#71798=CARTESIAN_POINT('Ctrl Pts',(0.206395395817321,-0.116848686716007,
-0.753635959380549));
#71799=CARTESIAN_POINT('Ctrl Pts',(0.206804666710838,-0.116122800866511,
-0.75357908777217));
#71800=CARTESIAN_POINT('Ctrl Pts',(0.207537019219195,-0.114807742493401,
-0.753476791229729));
#71801=CARTESIAN_POINT('Ctrl Pts',(0.207861438405948,-0.114219326504537,
-0.753431283184742));
#71802=CARTESIAN_POINT('Ctrl Pts',(0.208520776711208,-0.113011337095497,
-0.753338408759164));
#71803=CARTESIAN_POINT('Ctrl Pts',(0.208855443643762,-0.112391638148354,
-0.753291058174916));
#71804=CARTESIAN_POINT('Ctrl Pts',(0.209711971748914,-0.110788577148183,
-0.753169302660511));
#71805=CARTESIAN_POINT('Ctrl Pts',(0.210229686168149,-0.109803001310291,
-0.753095154044283));
#71806=CARTESIAN_POINT('Ctrl Pts',(0.212416881293943,-0.105567044785309,
-0.752779327927861));
#71807=CARTESIAN_POINT('Ctrl Pts',(0.214018166330394,-0.102281769879419,
-0.752541552658432));
#71808=CARTESIAN_POINT('Ctrl Pts',(0.218262422481726,-0.0930374869733026,
-0.751888592095682));
#71809=CARTESIAN_POINT('Ctrl Pts',(0.220736748892215,-0.0870043621872726,
-0.751480614530072));
#71810=CARTESIAN_POINT('Ctrl Pts',(0.224351678549712,-0.0770387673838556,
-0.75082422009093));
#71811=CARTESIAN_POINT('Ctrl Pts',(0.225644509273265,-0.0731655928764686,
-0.750573275346606));
#71812=CARTESIAN_POINT('Ctrl Pts',(0.23207617779094,-0.0521012059392833,
-0.749222144811371));
#71813=CARTESIAN_POINT('Ctrl Pts',(0.235351080179665,-0.0344045320088943,
-0.748130029713232));
#71814=CARTESIAN_POINT('Ctrl Pts',(0.236815860574844,-0.0134114833652199,
-0.746769236584495));
#71815=CARTESIAN_POINT('Ctrl Pts',(0.236971119992029,-0.0103105061208107,
-0.746566752093371));
#71816=CARTESIAN_POINT('Ctrl Pts',(0.237110894074801,-0.00571311970649749,
-0.746263957822327));
#71817=CARTESIAN_POINT('Ctrl Pts',(0.237142195492225,-0.00421838483763519,
-0.746165105732175));
#71818=CARTESIAN_POINT('Ctrl Pts',(0.237172817898998,-0.00155180218573925,
-0.745987987014976));
#71819=CARTESIAN_POINT('Ctrl Pts',(0.237177589818882,-0.000380056957058218,
-0.745909893355406));
#71820=CARTESIAN_POINT('Ctrl Pts',(0.237169314132987,0.00209926562713611,
-0.745744071475447));
#71821=CARTESIAN_POINT('Ctrl Pts',(0.237154135813141,0.00340679178762933,
-0.745656279172044));
#71822=CARTESIAN_POINT('Ctrl Pts',(0.237084588507573,0.00690515043165489,
-0.745420436544233));
#71823=CARTESIAN_POINT('Ctrl Pts',(0.237010666314697,0.00909542197051881,
-0.745271781106377));
#71824=CARTESIAN_POINT('Ctrl Pts',(0.236467160639718,0.0205059716707322,
-0.74449190855852));
#71825=CARTESIAN_POINT('Ctrl Pts',(0.23548992133616,0.0296929439342925,
-0.743845051711116));
#71826=CARTESIAN_POINT('Ctrl Pts',(0.232222271285833,0.0493989180236857,
-0.742417167169648));
#71827=CARTESIAN_POINT('Ctrl Pts',(0.229746314823503,0.0598668264034082,
-0.741632966265385));
#71828=CARTESIAN_POINT('Ctrl Pts',(0.222993397439967,0.0816835169848657,
-0.739965103043221));
#71829=CARTESIAN_POINT('Ctrl Pts',(0.218538399404636,0.0929477197894774,
-0.739083619651619));
#71830=CARTESIAN_POINT('Ctrl Pts',(0.212334754689178,0.105689345775776,
-0.738095043383589));
#71831=CARTESIAN_POINT('Ctrl Pts',(0.211401979785314,0.107542965995895,
-0.737951476823557));
#71832=CARTESIAN_POINT('Ctrl Pts',(0.210060509430596,0.110123829765267,
-0.737752176735345));
#71833=CARTESIAN_POINT('Ctrl Pts',(0.20967215492571,0.110861458613419,-0.737695284173697));
#71834=CARTESIAN_POINT('Ctrl Pts',(0.208963725047883,0.112189989770339,
-0.737592961152486));
#71835=CARTESIAN_POINT('Ctrl Pts',(0.208645012611117,0.112781607292701,
-0.737547447449598));
#71836=CARTESIAN_POINT('Ctrl Pts',(0.20798718759458,0.113990377936833,-0.737454575169175));
#71837=CARTESIAN_POINT('Ctrl Pts',(0.207647834352599,0.114607388013562,
-0.737407232293775));
#71838=CARTESIAN_POINT('Ctrl Pts',(0.20676516858516,0.116195455081041,-0.737285520117831));
#71839=CARTESIAN_POINT('Ctrl Pts',(0.206217753878216,0.117164230158201,
-0.737211406783946));
#71840=CARTESIAN_POINT('Ctrl Pts',(0.203846083520035,0.121293322195744,
-0.736895945296159));
#71841=CARTESIAN_POINT('Ctrl Pts',(0.201955735872948,0.12441535305541,-0.736658488209435));
#71842=CARTESIAN_POINT('Ctrl Pts',(0.196497789346405,0.132977068637876,
-0.736006692388246));
#71843=CARTESIAN_POINT('Ctrl Pts',(0.192777233486394,0.138315698649986,
-0.735599530363658));
#71844=CARTESIAN_POINT('Ctrl Pts',(0.186302966032496,0.146835937303549,
-0.734936899362414));
#71845=CARTESIAN_POINT('Ctrl Pts',(0.183676008044094,0.150109003713227,
-0.73467901485996));
#71846=CARTESIAN_POINT('Ctrl Pts',(0.169434227018847,0.166919593031269,
-0.733327529406232));
#71847=CARTESIAN_POINT('Ctrl Pts',(0.156408104585745,0.179182944241944,
-0.732241415382019));
#71848=CARTESIAN_POINT('Ctrl Pts',(0.139639943991141,0.191735108537672,
-0.730887062536924));
#71849=CARTESIAN_POINT('Ctrl Pts',(0.137112189406538,0.193550799147673,
-0.730684103838247));
#71850=CARTESIAN_POINT('Ctrl Pts',(0.133317178915064,0.196165108620653,
-0.730380736108378));
#71851=CARTESIAN_POINT('Ctrl Pts',(0.132076840821975,0.197002355264635,
-0.730281792975631));
#71852=CARTESIAN_POINT('Ctrl Pts',(0.129851192166905,0.198474234852637,
-0.730104573201188));
#71853=CARTESIAN_POINT('Ctrl Pts',(0.128868935627575,0.199113413292776,
-0.730026470285796));
#71854=CARTESIAN_POINT('Ctrl Pts',(0.126781418701622,0.200449894630835,
-0.729860694011883));
#71855=CARTESIAN_POINT('Ctrl Pts',(0.125675054844796,0.201145392332424,
-0.729772957056639));
#71856=CARTESIAN_POINT('Ctrl Pts',(0.122701251540261,0.202980713135329,
-0.729537422015438));
#71857=CARTESIAN_POINT('Ctrl Pts',(0.120823731666818,0.20410387634948,-0.729389021571073));
#71858=CARTESIAN_POINT('Ctrl Pts',(0.110993313989625,0.209801422119215,
-0.728613365447377));
#71859=CARTESIAN_POINT('Ctrl Pts',(0.102796405199097,0.213936937621227,
-0.727970674637133));
#71860=CARTESIAN_POINT('Ctrl Pts',(0.0844870568284945,0.221878881640529,
-0.72654439865347));
#71861=CARTESIAN_POINT('Ctrl Pts',(0.0743120169870806,0.225490563302023,
-0.725757325414621));
#71862=CARTESIAN_POINT('Ctrl Pts',(0.0522547619520863,0.23166429202892,
-0.724084552656099));
#71863=CARTESIAN_POINT('Ctrl Pts',(0.0403476740833811,0.234032109241221,
-0.723201037244923));
#71864=CARTESIAN_POINT('Ctrl Pts',(0.0262523252851681,0.235726736509283,
-0.722210718470013));
#71865=CARTESIAN_POINT('Ctrl Pts',(0.0241906777440488,0.235947220220347,
-0.722067270279137));
#71866=CARTESIAN_POINT('Ctrl Pts',(0.0212966450340585,0.236218390344216,
-0.721868106474055));
#71867=CARTESIAN_POINT('Ctrl Pts',(0.0204665518706763,0.236291758920337,
-0.721811233836736));
#71868=CARTESIAN_POINT('Ctrl Pts',(0.0189664703592798,0.236416380756957,
-0.721708935994121));
#71869=CARTESIAN_POINT('Ctrl Pts',(0.0182966193840366,0.236469164686944,
-0.721663427671397));
#71870=CARTESIAN_POINT('Ctrl Pts',(0.0169242129664499,0.236571442992661,
-0.721570553351657));
#71871=CARTESIAN_POINT('Ctrl Pts',(0.016221647217112,0.236620655942528,
-0.721523203146354));
#71872=CARTESIAN_POINT('Ctrl Pts',(0.0144080362414379,0.236739579187792,
-0.721401449762246));
#71873=CARTESIAN_POINT('Ctrl Pts',(0.0132966850958709,0.236804599088722,
-0.721327302880291));
#71874=CARTESIAN_POINT('Ctrl Pts',(0.00853595339270665,0.237049505589593,
-0.721011494697443));
#71875=CARTESIAN_POINT('Ctrl Pts',(0.00488291993516837,0.237152885832268,
-0.720773735077856));
#71876=CARTESIAN_POINT('Ctrl Pts',(-0.00528807153497601,0.237205578827938,
-0.720120831828304));
#71877=CARTESIAN_POINT('Ctrl Pts',(-0.0118039747893253,0.236970734068871,
-0.71971289439808));
#71878=CARTESIAN_POINT('Ctrl Pts',(-0.0195876596812752,0.236368284890876,
-0.719229498985646));
#71879=CARTESIAN_POINT('Ctrl Pts',(-0.0208721358349881,0.236258325801489,
-0.719149858254532));
#71880=CARTESIAN_POINT('Ctrl Pts',(-0.0287900959476827,0.235515422430361,
-0.718659407888492));
#71881=CARTESIAN_POINT('Ctrl Pts',(-0.0353904170704665,0.234614090579963,
-0.718252580103505));
#71882=CARTESIAN_POINT('Ctrl Pts',(-0.04193932278856,0.233437515898874,
-0.717844391575082));
#71883=CARTESIAN_POINT('Origin',(0.,0.,-2.1456589891905));
#71884=CARTESIAN_POINT('',(-0.0419766262164045,0.23365534329502,-0.598123480850464));
#71885=CARTESIAN_POINT('',(-0.0418741542966648,0.233068851607476,-0.617833934840082));
#71886=CARTESIAN_POINT('',(-0.0419392741328076,0.233437524640348,-2.1456589891905));
#71887=CARTESIAN_POINT('',(-0.237249110971816,-5.32523605593984E-5,-0.675941014918504));
#71888=CARTESIAN_POINT('Ctrl Pts',(-0.237550249404384,-5.3380897644477E-5,
-0.675941010809497));
#71889=CARTESIAN_POINT('Ctrl Pts',(-0.237559050867073,-0.00294060675479713,
-0.675746408192839));
#71890=CARTESIAN_POINT('Ctrl Pts',(-0.236202859689124,-0.084373458259399,
-0.670257162218186));
#71891=CARTESIAN_POINT('Ctrl Pts',(-0.143209357946364,-0.241037317324593,
-0.659473272885537));
#71892=CARTESIAN_POINT('Ctrl Pts',(0.124952039551137,-0.250987841057003,
-0.643589342811547));
#71893=CARTESIAN_POINT('Ctrl Pts',(0.278649891841477,-0.0310184835734619,
-0.62770541273756));
#71894=CARTESIAN_POINT('Ctrl Pts',(0.181746723461027,0.20597154716017,-0.612550125417199));
#71895=CARTESIAN_POINT('Ctrl Pts',(0.0249201733156075,0.245060147532978,
-0.602689481454833));
#71896=CARTESIAN_POINT('Ctrl Pts',(-0.0419766262164012,0.23365534329502,
-0.598123480850464));
#71897=CARTESIAN_POINT('Ctrl Pts',(-0.0419392741328079,0.233437524640348,
-0.698115075114807));
#71898=CARTESIAN_POINT('Ctrl Pts',(-0.0558502647186398,0.230938282718824,
-0.697169413870174));
#71899=CARTESIAN_POINT('Ctrl Pts',(-0.0695303812972798,0.227192518435731,
-0.696223752625541));
#71900=CARTESIAN_POINT('Ctrl Pts',(-0.0827484893710936,0.222271608919812,
-0.695278091380908));
#71901=CARTESIAN_POINT('Ctrl Pts',(-0.0959969028860838,0.217339417128622,
-0.694330261998364));
#71902=CARTESIAN_POINT('Ctrl Pts',(-0.108780430948953,0.211227046017747,
-0.69338243261582));
#71903=CARTESIAN_POINT('Ctrl Pts',(-0.120888672191277,0.204053692838012,
-0.692434603233277));
#71904=CARTESIAN_POINT('Ctrl Pts',(-0.125970748973033,0.201042889624525,
-0.692036779833355));
#71905=CARTESIAN_POINT('Ctrl Pts',(-0.130934198668081,0.197845717141427,
-0.691638956433434));
#71906=CARTESIAN_POINT('Ctrl Pts',(-0.135765095923163,0.194473184151375,
-0.691241133033512));
#71907=CARTESIAN_POINT('Ctrl Pts',(-0.147207302363418,0.186485181786356,
-0.690298869675731));
#71908=CARTESIAN_POINT('Ctrl Pts',(-0.157982935539225,0.177455254709155,
-0.689356606317951));
#71909=CARTESIAN_POINT('Ctrl Pts',(-0.167896362767565,0.167519527203315,
-0.68841434296017));
#71910=CARTESIAN_POINT('Ctrl Pts',(-0.177789727932494,0.157603906890545,
-0.687473986485529));
#71911=CARTESIAN_POINT('Ctrl Pts',(-0.186823707031258,0.146786664065463,
-0.686533630010888));
#71912=CARTESIAN_POINT('Ctrl Pts',(-0.194836192693097,0.135243626991657,
-0.685593273536246));
#71913=CARTESIAN_POINT('Ctrl Pts',(-0.202847293896005,0.123702584412623,
-0.684653079543633));
#71914=CARTESIAN_POINT('Ctrl Pts',(-0.209836731309494,0.111436662316105,
-0.683712885551019));
#71915=CARTESIAN_POINT('Ctrl Pts',(-0.215683815247096,0.0986532942453341,
-0.682772691558406));
#71916=CARTESIAN_POINT('Ctrl Pts',(-0.221530259604519,0.085871324476509,
-0.681832600408414));
#71917=CARTESIAN_POINT('Ctrl Pts',(-0.226234267631766,0.0725727996398668,
-0.680892509258422));
#71918=CARTESIAN_POINT('Ctrl Pts',(-0.22972296895733,0.0589859149155935,
-0.67995241810843));
#71919=CARTESIAN_POINT('Ctrl Pts',(-0.233219408844369,0.0453688920588515,
-0.679010241668677));
#71920=CARTESIAN_POINT('Ctrl Pts',(-0.235495005835672,0.031463065700045,
-0.678068065228924));
#71921=CARTESIAN_POINT('Ctrl Pts',(-0.236527988038831,0.0175068986203395,
-0.677125888789171));
#71922=CARTESIAN_POINT('Ctrl Pts',(-0.236961011170192,0.0116565140230217,
-0.676730931169388));
#71923=CARTESIAN_POINT('Ctrl Pts',(-0.237176306855964,0.0057973155111871,
-0.676335973549606));
#71924=CARTESIAN_POINT('Ctrl Pts',(-0.237174994028786,-5.32207246910343E-5,
-0.675941015929823));
#71925=CARTESIAN_POINT('',(-0.236922073620166,-0.000171722348330205,-0.695658869404682));
#71926=CARTESIAN_POINT('Ctrl Pts',(-0.0419393227885598,0.233437515898874,
-0.717844391575082));
#71927=CARTESIAN_POINT('Ctrl Pts',(-0.0525772381988217,0.231526310810564,
-0.717181338047711));
#71928=CARTESIAN_POINT('Ctrl Pts',(-0.0630794614327931,0.228888870292117,
-0.716514194660857));
#71929=CARTESIAN_POINT('Ctrl Pts',(-0.0784769135198977,0.223879812165597,
-0.715485132150475));
#71930=CARTESIAN_POINT('Ctrl Pts',(-0.0835234147063496,0.222046455704396,
-0.715139446381879));
#71931=CARTESIAN_POINT('Ctrl Pts',(-0.0902667636855455,0.219334232894479,
-0.714663706665366));
#71932=CARTESIAN_POINT('Ctrl Pts',(-0.0920217966268213,0.218603712097245,
-0.714538598478205));
#71933=CARTESIAN_POINT('Ctrl Pts',(-0.094911247513511,0.217360036274781,
-0.714330382191779));
#71934=CARTESIAN_POINT('Ctrl Pts',(-0.096050766332457,0.216858895275677,
-0.714247684029168));
#71935=CARTESIAN_POINT('Ctrl Pts',(-0.0982536957775581,0.215869315121601,
-0.714086649331944));
#71936=CARTESIAN_POINT('Ctrl Pts',(-0.0993175423839966,0.215381929685326,
-0.714008350839327));
#71937=CARTESIAN_POINT('Ctrl Pts',(-0.101816139978379,0.214214786549096,
-0.713823177228744));
#71938=CARTESIAN_POINT('Ctrl Pts',(-0.103247743320399,0.213528462791111,
-0.713716077567042));
#71939=CARTESIAN_POINT('Ctrl Pts',(-0.106274126753787,0.212040036360264,
-0.713487490500992));
#71940=CARTESIAN_POINT('Ctrl Pts',(-0.107866950573482,0.211234201083342,
-0.713365878117769));
#71941=CARTESIAN_POINT('Ctrl Pts',(-0.112194423789506,0.208983153241751,
-0.713031836171442));
#71942=CARTESIAN_POINT('Ctrl Pts',(-0.114910058565981,0.20750234689232,
-0.712818188320758));
#71943=CARTESIAN_POINT('Ctrl Pts',(-0.12359230955118,0.202545304209228,
-0.712121831197764));
#71944=CARTESIAN_POINT('Ctrl Pts',(-0.129435881053669,0.198861753509653,
-0.711632298097665));
#71945=CARTESIAN_POINT('Ctrl Pts',(-0.146848509522171,0.18679262807147,
-0.710110421114418));
#71946=CARTESIAN_POINT('Ctrl Pts',(-0.157827755137984,0.177612865934884,
-0.709058205538637));
#71947=CARTESIAN_POINT('Ctrl Pts',(-0.173745697236007,0.161655828076908,
-0.707424676793536));
#71948=CARTESIAN_POINT('Ctrl Pts',(-0.179269133818743,0.15550814152815,
-0.706833561518333));
#71949=CARTESIAN_POINT('Ctrl Pts',(-0.185293390317587,0.148054359499175,
-0.706170516244241));
#71950=CARTESIAN_POINT('Ctrl Pts',(-0.186117081652261,0.147017570306768,
-0.706079431164925));
#71951=CARTESIAN_POINT('Ctrl Pts',(-0.18744211413612,0.145320752922566,
-0.70593227814894));
#71952=CARTESIAN_POINT('Ctrl Pts',(-0.187948741383397,0.144664916433839,
-0.705875860986625));
#71953=CARTESIAN_POINT('Ctrl Pts',(-0.188849815647416,0.143485738603242,
-0.705775263015471));
#71954=CARTESIAN_POINT('Ctrl Pts',(-0.189245540363652,0.142963406288722,
-0.70573099489097));
#71955=CARTESIAN_POINT('Ctrl Pts',(-0.190112414923563,0.141809278297383,
-0.70563382567623));
#71956=CARTESIAN_POINT('Ctrl Pts',(-0.190582583682373,0.141176770615792,
-0.705580992101311));
#71957=CARTESIAN_POINT('Ctrl Pts',(-0.191938226311698,0.139333939792885,
-0.705428233490907));
#71958=CARTESIAN_POINT('Ctrl Pts',(-0.192815404662887,0.138117520644432,
-0.705328858763159));
#71959=CARTESIAN_POINT('Ctrl Pts',(-0.201067174873499,0.126442612019581,
-0.70438802949425));
#71960=CARTESIAN_POINT('Ctrl Pts',(-0.20759658571956,0.115410124225476,
-0.703596580294805));
#71961=CARTESIAN_POINT('Ctrl Pts',(-0.217379569366901,0.0953358954136322,
-0.702225297712208));
#71962=CARTESIAN_POINT('Ctrl Pts',(-0.221034511834627,0.0865248539457959,
-0.701644391304448));
#71963=CARTESIAN_POINT('Ctrl Pts',(-0.226821574066829,0.0697911174599313,
-0.700546583455936));
#71964=CARTESIAN_POINT('Ctrl Pts',(-0.229092241183086,0.0619318411730688,
-0.70003312872163));
#71965=CARTESIAN_POINT('Ctrl Pts',(-0.231791079607705,0.0503830929441907,
-0.699270354435328));
#71966=CARTESIAN_POINT('Ctrl Pts',(-0.232545876430116,0.0467757801607365,
-0.69903099573463));
#71967=CARTESIAN_POINT('Ctrl Pts',(-0.233485612826743,0.0416970049545228,
-0.698691768909176));
#71968=CARTESIAN_POINT('Ctrl Pts',(-0.233741289376611,0.0402390493665929,
-0.698594133513378));
#71969=CARTESIAN_POINT('Ctrl Pts',(-0.234162304802007,0.0376987304661087,
-0.69842352928938));
#71970=CARTESIAN_POINT('Ctrl Pts',(-0.234333828634087,0.0366174269717644,
-0.698350757995416));
#71971=CARTESIAN_POINT('Ctrl Pts',(-0.234664109538308,0.0344378804321751,
-0.698203750531822));
#71972=CARTESIAN_POINT('Ctrl Pts',(-0.234822657843481,0.0333396341469533,
-0.698129509741804));
#71973=CARTESIAN_POINT('Ctrl Pts',(-0.235132043495524,0.0310847743760905,
-0.69797672650977));
#71974=CARTESIAN_POINT('Ctrl Pts',(-0.235282066727623,0.0299280815974099,
-0.697898160479516));
#71975=CARTESIAN_POINT('Ctrl Pts',(-0.235611435984668,0.0272329010515647,
-0.697714631259476));
#71976=CARTESIAN_POINT('Ctrl Pts',(-0.23578425320844,0.0256936841795304,
-0.69760946604402));
#71977=CARTESIAN_POINT('Ctrl Pts',(-0.236260645939362,0.0210399586476515,
-0.697290399551302));
#71978=CARTESIAN_POINT('Ctrl Pts',(-0.236517661084166,0.0179211345203719,
-0.697075070043448));
#71979=CARTESIAN_POINT('Ctrl Pts',(-0.237024664985002,0.00981110428418152,
-0.696511086020329));
#71980=CARTESIAN_POINT('Ctrl Pts',(-0.237178732709955,0.00481571997640742,
-0.696159699629818));
#71981=CARTESIAN_POINT('Ctrl Pts',(-0.237174931349867,-0.000180455495009113,
-0.695804408402709));
#71982=CARTESIAN_POINT('Ctrl Pts',(-0.236922073620166,-0.000171722348330205,
-0.695658869404682));
#71983=CARTESIAN_POINT('Ctrl Pts',(-0.23710552994315,-0.0279230387667656,
-0.693801110963438));
#71984=CARTESIAN_POINT('Ctrl Pts',(-0.219763942386725,-0.134543724728559,
-0.686648709164199));
#71985=CARTESIAN_POINT('Ctrl Pts',(-0.0618944900249994,-0.273453815725051,
-0.674201664006962));
#71986=CARTESIAN_POINT('Ctrl Pts',(0.196265018423904,-0.200219778676104,
-0.658317733932975));
#71987=CARTESIAN_POINT('Ctrl Pts',(0.274634025736058,0.056427556548666,
-0.642433803858986));
#71988=CARTESIAN_POINT('Ctrl Pts',(0.127477169071532,0.230553445971132,
-0.628939204161356));
#71989=CARTESIAN_POINT('Ctrl Pts',(0.000916701292335384,0.240640926964646,
-0.620739247821721));
#71990=CARTESIAN_POINT('Ctrl Pts',(-0.0418741542966648,0.233068851607476,
-0.617833934840082));
#71991=CARTESIAN_POINT('Origin',(0.,0.,-2.1456589891905));
#71992=CARTESIAN_POINT('',(-0.0419392658597717,0.233437526126678,-0.498199055407226));
#71993=CARTESIAN_POINT('',(-0.0419392867764624,0.233437522368795,-0.517737946518584));
#71994=CARTESIAN_POINT('',(-0.0419392741328076,0.233437524640348,-2.1456589891905));
#71995=CARTESIAN_POINT('',(-0.237113469260214,0.000216662027683377,-0.575941048797587));
#71996=CARTESIAN_POINT('Ctrl Pts',(-0.0419392658597717,0.233437526126678,
-0.498199055407226));
#71997=CARTESIAN_POINT('Ctrl Pts',(-0.0330765815721231,0.235029791426685,
-0.498854438470705));
#71998=CARTESIAN_POINT('Ctrl Pts',(-0.0241272490857351,0.236116612807205,
-0.499504144402303));
#71999=CARTESIAN_POINT('Ctrl Pts',(-0.0130677217538534,0.236823784124591,
-0.500277172715157));
#72000=CARTESIAN_POINT('Ctrl Pts',(-0.0109991115124832,0.236928871929854,
-0.500420471355373));
#72001=CARTESIAN_POINT('Ctrl Pts',(-0.00809678705350146,0.237038217874467,
-0.500619474195118));
#72002=CARTESIAN_POINT('Ctrl Pts',(-0.00726409450755453,0.23706519710254,
-0.500676332777726));
#72003=CARTESIAN_POINT('Ctrl Pts',(-0.00575949653870239,0.237106010941874,
-0.500778623293592));
#72004=CARTESIAN_POINT('Ctrl Pts',(-0.00508764283983578,0.237121378530362,
-0.500824138186445));
#72005=CARTESIAN_POINT('Ctrl Pts',(-0.00371111637288122,0.237147011101855,
-0.500917049062407));
#72006=CARTESIAN_POINT('Ctrl Pts',(-0.00300644900677803,0.237156991372071,
-0.500964429082569));
#72007=CARTESIAN_POINT('Ctrl Pts',(-0.00118724318088404,0.237174647232239,
-0.501086300569577));
#72008=CARTESIAN_POINT('Ctrl Pts',(-7.26606088802279E-5,0.237177607877993,
-0.501160534952242));
#72009=CARTESIAN_POINT('Ctrl Pts',(0.00470589197833913,0.23715661511272,
-0.501477101949923));
#72010=CARTESIAN_POINT('Ctrl Pts',(0.00836923808759544,0.23705561574805,
-0.501715510301296));
#72011=CARTESIAN_POINT('Ctrl Pts',(0.0185645961743475,0.236537862562508,
-0.50237074909836));
#72012=CARTESIAN_POINT('Ctrl Pts',(0.0250841369162542,0.235935591099632,
-0.502780312100465));
#72013=CARTESIAN_POINT('Ctrl Pts',(0.0353272638051378,0.234559864942448,
-0.503420156542185));
#72014=CARTESIAN_POINT('Ctrl Pts',(0.0390711110489085,0.233965371524756,
-0.503653233582996));
#72015=CARTESIAN_POINT('Ctrl Pts',(0.0607299183943161,0.229991720981356,
-0.505004501675264));
#72016=CARTESIAN_POINT('Ctrl Pts',(0.0782194597970318,0.224646267754523,
-0.506112968106125));
#72017=CARTESIAN_POINT('Ctrl Pts',(0.0977486194251004,0.216117307995706,
-0.507491241025893));
#72018=CARTESIAN_POINT('Ctrl Pts',(0.100549184772378,0.214828637353469,
-0.507692316454647));
#72019=CARTESIAN_POINT('Ctrl Pts',(0.104665970453112,0.212836178430527,
-0.50799342611889));
#72020=CARTESIAN_POINT('Ctrl Pts',(0.106002020615916,0.212173927885199,
-0.508092027097791));
#72021=CARTESIAN_POINT('Ctrl Pts',(0.10837654992391,0.210968900284615,-0.508268891060408));
#72022=CARTESIAN_POINT('Ctrl Pts',(0.109417427998987,0.210430938376974,
-0.508346983331399));
#72023=CARTESIAN_POINT('Ctrl Pts',(0.111614078733411,0.209274928684104,
-0.508513008840907));
#72024=CARTESIAN_POINT('Ctrl Pts',(0.11276879609338,0.208654970837369,-0.508601007747302));
#72025=CARTESIAN_POINT('Ctrl Pts',(0.115851424522281,0.206966871045782,
-0.508837912523622));
#72026=CARTESIAN_POINT('Ctrl Pts',(0.117769643695447,0.205881394802806,
-0.508987432739999));
#72027=CARTESIAN_POINT('Ctrl Pts',(0.127808849002608,0.200014229300171,
-0.509781371131358));
#72028=CARTESIAN_POINT('Ctrl Pts',(0.135653579611324,0.194778999945319,
-0.510442120254722));
#72029=CARTESIAN_POINT('Ctrl Pts',(0.151622159419223,0.182688849587316,
-0.511875072709876));
#72030=CARTESIAN_POINT('Ctrl Pts',(0.159639408522314,0.175726280999964,
-0.512649399976805));
#72031=CARTESIAN_POINT('Ctrl Pts',(0.175680572604679,0.159788836753034,
-0.514300754108403));
#72032=CARTESIAN_POINT('Ctrl Pts',(0.183543925188247,0.150691144616251,
-0.515175619417615));
#72033=CARTESIAN_POINT('Ctrl Pts',(0.191922873303588,0.139362565664156,
-0.516158618663595));
#72034=CARTESIAN_POINT('Ctrl Pts',(0.193138709285569,0.137672632432337,
-0.516302662351488));
#72035=CARTESIAN_POINT('Ctrl Pts',(0.194810822616322,0.1352827449943,-0.516502522896911));
#72036=CARTESIAN_POINT('Ctrl Pts',(0.195285851047047,0.134596114859929,
-0.516559506804667));
#72037=CARTESIAN_POINT('Ctrl Pts',(0.196136935793519,0.133351922700136,
-0.51666195571733));
#72038=CARTESIAN_POINT('Ctrl Pts',(0.196514264588357,0.132795243604197,
-0.516707504473968));
#72039=CARTESIAN_POINT('Ctrl Pts',(0.197281753623912,0.131652519729256,
-0.516800402628193));
#72040=CARTESIAN_POINT('Ctrl Pts',(0.197671680390599,0.131066330796504,
-0.516847736625924));
#72041=CARTESIAN_POINT('Ctrl Pts',(0.198670378150646,0.129550362863303,
-0.516969349353387));
#72042=CARTESIAN_POINT('Ctrl Pts',(0.199275243310086,0.128618012725329,
-0.517043373072305));
#72043=CARTESIAN_POINT('Ctrl Pts',(0.201829928385638,0.124618887732487,
-0.517357764837771));
#72044=CARTESIAN_POINT('Ctrl Pts',(0.203715794467464,0.121511586970772,
-0.517594275163542));
#72045=CARTESIAN_POINT('Ctrl Pts',(0.208754956328711,0.112761335227541,
-0.518242569833834));
#72046=CARTESIAN_POINT('Ctrl Pts',(0.211750261286401,0.107030787268048,
-0.51864727141038));
#72047=CARTESIAN_POINT('Ctrl Pts',(0.216390444679063,0.0971937611344773,
-0.519320912665028));
#72048=CARTESIAN_POINT('Ctrl Pts',(0.2181612670776,0.0931510321216165,-0.519592032955327));
#72049=CARTESIAN_POINT('Ctrl Pts',(0.226449597120232,0.0726940099749962,
-0.52094576261472));
#72050=CARTESIAN_POINT('Ctrl Pts',(0.231231490981726,0.0556394799885956,
-0.522021834560969));
#72051=CARTESIAN_POINT('Ctrl Pts',(0.234579677202807,0.0351299650828139,
-0.523365391825341));
#72052=CARTESIAN_POINT('Ctrl Pts',(0.235022011279658,0.0320373552576627,
-0.523569105033863));
#72053=CARTESIAN_POINT('Ctrl Pts',(0.235586009968098,0.0274492176768213,
-0.523873405027875));
#72054=CARTESIAN_POINT('Ctrl Pts',(0.235754786569311,0.0259597395952857,
-0.523972512983669));
#72055=CARTESIAN_POINT('Ctrl Pts',(0.236030398466981,0.023302499674537,
-0.524149939243159));
#72056=CARTESIAN_POINT('Ctrl Pts',(0.236142714969529,0.0221353467022232,
-0.524228082607621));
#72057=CARTESIAN_POINT('Ctrl Pts',(0.236361838665955,0.0196664133929033,
-0.524393851976311));
#72058=CARTESIAN_POINT('Ctrl Pts',(0.23646655560621,0.018364491675914,-0.524481540928238));
#72059=CARTESIAN_POINT('Ctrl Pts',(0.236717574604468,0.0148841317712658,
-0.524716722914501));
#72060=CARTESIAN_POINT('Ctrl Pts',(0.236844555280886,0.012704470974011,
-0.524864814833499));
#72061=CARTESIAN_POINT('Ctrl Pts',(0.237345114623906,0.00143407289938757,
-0.52563492584933));
#72062=CARTESIAN_POINT('Ctrl Pts',(0.237225412815,-0.00766982049385359,
-0.526272111051324));
#72063=CARTESIAN_POINT('Ctrl Pts',(0.235818250233654,-0.0275529582367287,
-0.527696140702168));
#72064=CARTESIAN_POINT('Ctrl Pts',(0.234313348873809,-0.038296678014635,
-0.528486886555703));
#72065=CARTESIAN_POINT('Ctrl Pts',(0.229573013052809,-0.0607947583794694,
-0.530166035018932));
#72066=CARTESIAN_POINT('Ctrl Pts',(0.22615542981611,-0.0724813868646703,
-0.531052247248237));
#72067=CARTESIAN_POINT('Ctrl Pts',(0.221123967869649,-0.0857931398776052,
-0.532044922880732));
#72068=CARTESIAN_POINT('Ctrl Pts',(0.220366158560588,-0.0877213138711721,
-0.532188254462476));
#72069=CARTESIAN_POINT('Ctrl Pts',(0.219268250830519,-0.0904107792497356,
-0.532387295237444));
#72070=CARTESIAN_POINT('Ctrl Pts',(0.218949282083269,-0.0911805174071922,
-0.532444159372446));
#72071=CARTESIAN_POINT('Ctrl Pts',(0.218365722168895,-0.0925680486739769,
-0.532546456902546));
#72072=CARTESIAN_POINT('Ctrl Pts',(0.218102549405499,-0.093186427322411,
-0.53259197329234));
#72073=CARTESIAN_POINT('Ctrl Pts',(0.217558037187035,-0.0944509273126081,
-0.53268488358847));
#72074=CARTESIAN_POINT('Ctrl Pts',(0.217276441023691,-0.095096926469615,
-0.532732261556894));
#72075=CARTESIAN_POINT('Ctrl Pts',(0.216542108726632,-0.0967612405080249,
-0.532854121511781));
#72076=CARTESIAN_POINT('Ctrl Pts',(0.216085060948707,-0.097777651195761,
-0.532928346506588));
#72077=CARTESIAN_POINT('Ctrl Pts',(0.214095241944681,-0.102120630047286,
-0.533244816225979));
#72078=CARTESIAN_POINT('Ctrl Pts',(0.212492598056775,-0.105414871175082,
-0.533483139675793));
#72079=CARTESIAN_POINT('Ctrl Pts',(0.20781746220006,-0.114484319665278,
-0.534138067029002));
#72080=CARTESIAN_POINT('Ctrl Pts',(0.204581327868328,-0.120171750972739,
-0.534547411826224));
#72081=CARTESIAN_POINT('Ctrl Pts',(0.199082745057949,-0.128967926221641,
-0.535189638321337));
#72082=CARTESIAN_POINT('Ctrl Pts',(0.196973004602218,-0.132167703478062,
-0.535425278661488));
#72083=CARTESIAN_POINT('Ctrl Pts',(0.18440992919682,-0.150252313283444,
-0.536776473569577));
#72084=CARTESIAN_POINT('Ctrl Pts',(0.17235087217781,-0.163944720201064,
-0.537882550175804));
#72085=CARTESIAN_POINT('Ctrl Pts',(0.156554702582462,-0.178191273166644,
-0.539258278720561));
#72086=CARTESIAN_POINT('Ctrl Pts',(0.154222944574336,-0.180213170068991,
-0.539459575203072));
#72087=CARTESIAN_POINT('Ctrl Pts',(0.150706516611133,-0.1831440745308,-0.539760952344966));
#72088=CARTESIAN_POINT('Ctrl Pts',(0.14955158437768,-0.184088374493874,
-0.539859595955209));
#72089=CARTESIAN_POINT('Ctrl Pts',(0.147473751419888,-0.185754801471623,
-0.540036507088638));
#72090=CARTESIAN_POINT('Ctrl Pts',(0.146554254562996,-0.18648110899634,
-0.540114603543847));
#72091=CARTESIAN_POINT('Ctrl Pts',(0.144595268238482,-0.188005068398782,
-0.540280606967812));
#72092=CARTESIAN_POINT('Ctrl Pts',(0.143554478672965,-0.188800976888037,
-0.540368579372874));
#72093=CARTESIAN_POINT('Ctrl Pts',(0.140746784991828,-0.190911427082562,
-0.540605336787589));
#72094=CARTESIAN_POINT('Ctrl Pts',(0.138968113812755,-0.192210023798749,
-0.54075473481482));
#72095=CARTESIAN_POINT('Ctrl Pts',(0.12950697511722,-0.198917569042661,
-0.541546585609574));
#72096=CARTESIAN_POINT('Ctrl Pts',(0.121527177528542,-0.203890558957619,
-0.542205265320451));
#72097=CARTESIAN_POINT('Ctrl Pts',(0.10393694681623,-0.213452675600637,
-0.543637474943252));
#72098=CARTESIAN_POINT('Ctrl Pts',(0.094269428020421,-0.217894882670642,
-0.544413284230555));
#72099=CARTESIAN_POINT('Ctrl Pts',(0.0731037286647757,-0.225947531162459,
-0.546067082627708));
#72100=CARTESIAN_POINT('Ctrl Pts',(0.0615602883400919,-0.229361789742797,
-0.546942907743081));
#72101=CARTESIAN_POINT('Ctrl Pts',(0.0477724683100303,-0.232323268520589,
-0.547926714424495));
#72102=CARTESIAN_POINT('Ctrl Pts',(0.045732441818632,-0.232733440503412,
-0.548070687355907));
#72103=CARTESIAN_POINT('Ctrl Pts',(0.0428667395150199,-0.233270486902231,
-0.548270466471568));
#72104=CARTESIAN_POINT('Ctrl Pts',(0.0420454607585319,-0.233419914957443,
-0.548327438500273));
#72105=CARTESIAN_POINT('Ctrl Pts',(0.0405611836494176,-0.233681884599432,
-0.548429872392408));
#72106=CARTESIAN_POINT('Ctrl Pts',(0.0398984643800055,-0.233795948188677,
-0.548475417932497));
#72107=CARTESIAN_POINT('Ctrl Pts',(0.0385408714947916,-0.234023668850306,
-0.548568317259998));
#72108=CARTESIAN_POINT('Ctrl Pts',(0.0378459627371746,-0.234137052802743,
-0.548615655594351));
#72109=CARTESIAN_POINT('Ctrl Pts',(0.0360526393801527,-0.234421465614031,
-0.548737292711659));
#72110=CARTESIAN_POINT('Ctrl Pts',(0.034953493370299,-0.234587872170292,
-0.548811336288614));
#72111=CARTESIAN_POINT('Ctrl Pts',(0.0302535385970015,-0.235265660484166,
-0.549125932414795));
#72112=CARTESIAN_POINT('Ctrl Pts',(0.0266421799854468,-0.235701941794512,
-0.549362621017553));
#72113=CARTESIAN_POINT('Ctrl Pts',(0.0165819887027716,-0.236683092486534,
-0.550011566300828));
#72114=CARTESIAN_POINT('Ctrl Pts',(0.010118507675001,-0.237047414070391,
-0.550416723019095));
#72115=CARTESIAN_POINT('Ctrl Pts',(-0.00957069677091684,-0.237350273078646,
-0.551636279247605));
#72116=CARTESIAN_POINT('Ctrl Pts',(-0.0227830231040275,-0.236448076564223,
-0.552435791141741));
#72117=CARTESIAN_POINT('Ctrl Pts',(-0.0459051610031064,-0.23291229393427,
-0.553887449154942));
#72118=CARTESIAN_POINT('Ctrl Pts',(-0.0558483846699635,-0.230730015998957,
-0.554529220835882));
#72119=CARTESIAN_POINT('Ctrl Pts',(-0.0678216978028471,-0.22728274623486,
-0.555340918633542));
#72120=CARTESIAN_POINT('Ctrl Pts',(-0.0700139261114413,-0.226617031526893,
-0.55549114269021));
#72121=CARTESIAN_POINT('Ctrl Pts',(-0.0734749932579312,-0.225510994345337,
-0.555731041137378));
#72122=CARTESIAN_POINT('Ctrl Pts',(-0.0747503648296774,-0.22509146149307,
-0.555820034219674));
#72123=CARTESIAN_POINT('Ctrl Pts',(-0.0771278627139591,-0.224286950524391,
-0.555987075459408));
#72124=CARTESIAN_POINT('Ctrl Pts',(-0.0782308465766714,-0.223904617956588,
-0.556065034150252));
#72125=CARTESIAN_POINT('Ctrl Pts',(-0.0806904646445958,-0.223031636016509,
-0.556239941390695));
#72126=CARTESIAN_POINT('Ctrl Pts',(-0.0820455254802655,-0.222536723570224,
-0.556337029223204));
#72127=CARTESIAN_POINT('Ctrl Pts',(-0.0859849170769581,-0.221057058186752,
-0.556621454261435));
#72128=CARTESIAN_POINT('Ctrl Pts',(-0.0885565659622792,-0.220039456542911,
-0.556809879573585));
#72129=CARTESIAN_POINT('Ctrl Pts',(-0.0944132911535427,-0.21760265114447,
-0.557245527579756));
#72130=CARTESIAN_POINT('Ctrl Pts',(-0.0976851517166901,-0.216153630798189,
-0.557493703058731));
#72131=CARTESIAN_POINT('Ctrl Pts',(-0.108734227334932,-0.210958188725723,
-0.55834848157885));
#72132=CARTESIAN_POINT('Ctrl Pts',(-0.116338508787639,-0.206861824114568,
-0.558965835322636));
#72133=CARTESIAN_POINT('Ctrl Pts',(-0.138958359613599,-0.193034423024834,
-0.560886196524469));
#72134=CARTESIAN_POINT('Ctrl Pts',(-0.153111160632558,-0.182012956809431,
-0.562213018963176));
#72135=CARTESIAN_POINT('Ctrl Pts',(-0.167866838853847,-0.167571916874691,
-0.563663435178786));
#72136=CARTESIAN_POINT('Ctrl Pts',(-0.16980871577917,-0.16560381822515,
-0.56385572847679));
#72137=CARTESIAN_POINT('Ctrl Pts',(-0.172430200082915,-0.162852323353281,
-0.564116745960032));
#72138=CARTESIAN_POINT('Ctrl Pts',(-0.17313965985942,-0.162097845161331,
-0.56418753390917));
#72139=CARTESIAN_POINT('Ctrl Pts',(-0.174265468734213,-0.16088477428329,
-0.564300067336537));
#72140=CARTESIAN_POINT('Ctrl Pts',(-0.174684992697594,-0.160429166731407,
-0.564342047856977));
#72141=CARTESIAN_POINT('Ctrl Pts',(-0.175561550639008,-0.15946970024006,
-0.564429849036139));
#72142=CARTESIAN_POINT('Ctrl Pts',(-0.176018209194962,-0.158965510118756,
-0.564475639678436));
#72143=CARTESIAN_POINT('Ctrl Pts',(-0.177140667371284,-0.157715453158685,
-0.56458833418918));
#72144=CARTESIAN_POINT('Ctrl Pts',(-0.177803942013721,-0.156967316647778,
-0.564655051727945));
#72145=CARTESIAN_POINT('Ctrl Pts',(-0.18020055206605,-0.154229391363479,
-0.564896677840784));
#72146=CARTESIAN_POINT('Ctrl Pts',(-0.181905453860643,-0.152214819940171,
-0.565069637428765));
#72147=CARTESIAN_POINT('Ctrl Pts',(-0.18997951233834,-0.142344764301913,
-0.565896395197436));
#72148=CARTESIAN_POINT('Ctrl Pts',(-0.195876118778367,-0.134115015891556,
-0.566524180511667));
#72149=CARTESIAN_POINT('Ctrl Pts',(-0.206845864889663,-0.116530495209853,
-0.567799129845046));
#72150=CARTESIAN_POINT('Ctrl Pts',(-0.21185140795199,-0.107161308260448,
-0.568444489340571));
#72151=CARTESIAN_POINT('Ctrl Pts',(-0.220469427169856,-0.0880480228350329,
-0.569744813863598));
#72152=CARTESIAN_POINT('Ctrl Pts',(-0.224102724212719,-0.0783399758487367,
-0.57039779297285));
#72153=CARTESIAN_POINT('Ctrl Pts',(-0.227753542249212,-0.0662238350929426,
-0.571222082154118));
#72154=CARTESIAN_POINT('Ctrl Pts',(-0.228385114451004,-0.0640118053968531,
-0.571372907803587));
#72155=CARTESIAN_POINT('Ctrl Pts',(-0.229334731862316,-0.0604927239157919,
-0.571613551645852));
#72156=CARTESIAN_POINT('Ctrl Pts',(-0.229674015584425,-0.0591915139546034,
-0.571702681224881));
#72157=CARTESIAN_POINT('Ctrl Pts',(-0.230287086205016,-0.0567556241761504,
-0.571869845054797));
#72158=CARTESIAN_POINT('Ctrl Pts',(-0.230563598619468,-0.0556216671463706,
-0.571947788629566));
#72159=CARTESIAN_POINT('Ctrl Pts',(-0.231089283680852,-0.0533945742143698,
-0.572101134728435));
#72160=CARTESIAN_POINT('Ctrl Pts',(-0.231339097560891,-0.0523016199777244,
-0.572176514314871));
#72161=CARTESIAN_POINT('Ctrl Pts',(-0.231885217019687,-0.0498318191477032,
-0.572347150390873));
#72162=CARTESIAN_POINT('Ctrl Pts',(-0.232177024488392,-0.0484540320528138,
-0.572442547989112));
#72163=CARTESIAN_POINT('Ctrl Pts',(-0.232885067724556,-0.0449576191226075,
-0.572685194325873));
#72164=CARTESIAN_POINT('Ctrl Pts',(-0.233284668193528,-0.0428357950472687,
-0.572832961562156));
#72165=CARTESIAN_POINT('Ctrl Pts',(-0.236010352359248,-0.027191284116254,
-0.57392646661218));
#72166=CARTESIAN_POINT('Ctrl Pts',(-0.237187548041389,-0.0134974807389825,
-0.574907807761886));
#72167=CARTESIAN_POINT('Ctrl Pts',(-0.237174899149993,0.00021871943419613,
-0.575905717570473));
#72168=CARTESIAN_POINT('Ctrl Pts',(-0.0419766262164012,0.23365534329502,
-0.598123480850464));
#72169=CARTESIAN_POINT('Ctrl Pts',(-0.0526520230118338,0.231835363692615,
-0.597394838096837));
#72170=CARTESIAN_POINT('Ctrl Pts',(-0.139695025652084,0.210579474520431,
-0.591371551985214));
#72171=CARTESIAN_POINT('Ctrl Pts',(-0.225519033105649,0.119811949965669,
-0.583977407967588));
#72172=CARTESIAN_POINT('Ctrl Pts',(-0.237296177544911,0.0206528429717354,
-0.57731190670359));
#72173=CARTESIAN_POINT('Ctrl Pts',(-0.237113469260214,0.000216662027683377,
-0.575941048797587));
#72174=CARTESIAN_POINT('',(-0.237522045222027,-7.70250957813517E-5,-0.595652851074302));
#72175=CARTESIAN_POINT('Ctrl Pts',(-0.0418741542966648,0.233068851607476,
-0.617833934840082));
#72176=CARTESIAN_POINT('Ctrl Pts',(-0.0770653683707668,0.226841574278908,
-0.615444604463725));
#72177=CARTESIAN_POINT('Ctrl Pts',(-0.181642156144958,0.184255516872655,
-0.608052990951751));
#72178=CARTESIAN_POINT('Ctrl Pts',(-0.237210808141337,0.0741535263668472,
-0.60066137743978));
#72179=CARTESIAN_POINT('Ctrl Pts',(-0.237532922930967,-7.74222378633504E-5,
-0.595659094304164));
#72180=CARTESIAN_POINT('Ctrl Pts',(-0.237174991269168,-6.43542539559139E-5,
-0.595453660452978));
#72181=CARTESIAN_POINT('Ctrl Pts',(-0.237174364967726,-0.00237256280265978,
-0.595291666791208));
#72182=CARTESIAN_POINT('Ctrl Pts',(-0.237140043091288,-0.00468075615503481,
-0.59513102131791));
#72183=CARTESIAN_POINT('Ctrl Pts',(-0.237046058216446,-0.0078691605257938,
-0.594911300655702));
#72184=CARTESIAN_POINT('Ctrl Pts',(-0.237015178994657,-0.0087499936839357,
-0.594850831062905));
#72185=CARTESIAN_POINT('Ctrl Pts',(-0.236952705462167,-0.0102872666538859,
-0.59474572287562));
#72186=CARTESIAN_POINT('Ctrl Pts',(-0.236923291848027,-0.0109437784665437,
-0.594700970890158));
#72187=CARTESIAN_POINT('Ctrl Pts',(-0.236860251490791,-0.0122311478259143,
-0.594613493078634));
#72188=CARTESIAN_POINT('Ctrl Pts',(-0.236826832148373,-0.0128620110159745,
-0.594570756598602));
#72189=CARTESIAN_POINT('Ctrl Pts',(-0.23674925025568,-0.0142235333722509,
-0.594478813958949));
#72190=CARTESIAN_POINT('Ctrl Pts',(-0.236704225687466,-0.0149541290827802,
-0.594429656067645));
#72191=CARTESIAN_POINT('Ctrl Pts',(-0.236573901414612,-0.0169205267247753,
-0.594297800630824));
#72192=CARTESIAN_POINT('Ctrl Pts',(-0.236482299953095,-0.0181559089434672,
-0.594215444896435));
#72193=CARTESIAN_POINT('Ctrl Pts',(-0.236015912577266,-0.0238414168202966,
-0.59383841107224));
#72194=CARTESIAN_POINT('Ctrl Pts',(-0.23552513848384,-0.0282814329169275,
-0.593549575711258));
#72195=CARTESIAN_POINT('Ctrl Pts',(-0.232875735959759,-0.0473110602734093,
-0.59232562791775));
#72196=CARTESIAN_POINT('Ctrl Pts',(-0.229484309769027,-0.0616966295445551,
-0.591434318300533));
#72197=CARTESIAN_POINT('Ctrl Pts',(-0.220737362157619,-0.0876777794383515,
-0.589749526966357));
#72198=CARTESIAN_POINT('Ctrl Pts',(-0.21574207370356,-0.0993361845106995,
-0.588962803570763));
#72199=CARTESIAN_POINT('Ctrl Pts',(-0.208372266667843,-0.113326533785409,
-0.587940689071195));
#72200=CARTESIAN_POINT('Ctrl Pts',(-0.206848709372263,-0.116084084546745,
-0.587735290429501));
#72201=CARTESIAN_POINT('Ctrl Pts',(-0.204517489273079,-0.120111773947784,
-0.587428973656753));
#72202=CARTESIAN_POINT('Ctrl Pts',(-0.203751895292275,-0.12140595804614,
-0.587329564014937));
#72203=CARTESIAN_POINT('Ctrl Pts',(-0.202367393829763,-0.123696377689382,
-0.587151824987848));
#72204=CARTESIAN_POINT('Ctrl Pts',(-0.201753300158513,-0.124695475977623,
-0.587073673219476));
#72205=CARTESIAN_POINT('Ctrl Pts',(-0.200441425995232,-0.126794765732958,
-0.586908123675633));
#72206=CARTESIAN_POINT('Ctrl Pts',(-0.199741941561339,-0.127893840883713,
-0.586820664759316));
#72207=CARTESIAN_POINT('Ctrl Pts',(-0.197853713350675,-0.130807470514853,
-0.586586674194169));
#72208=CARTESIAN_POINT('Ctrl Pts',(-0.196649093645901,-0.132611536646144,
-0.586439553943037));
#72209=CARTESIAN_POINT('Ctrl Pts',(-0.190966132320522,-0.14087473634893,
-0.585755062407461));
#72210=CARTESIAN_POINT('Ctrl Pts',(-0.186193677998158,-0.147124589577071,
-0.585206631042645));
#72211=CARTESIAN_POINT('Ctrl Pts',(-0.17114287346141,-0.164927022395434,
-0.583549892348229));
#72212=CARTESIAN_POINT('Ctrl Pts',(-0.160036533161969,-0.175724292345416,
-0.582414087636772));
#72213=CARTESIAN_POINT('Ctrl Pts',(-0.142709880293066,-0.189554765978345,
-0.580801134905494));
#72214=CARTESIAN_POINT('Ctrl Pts',(-0.137282941452883,-0.193521382241397,
-0.58031576124169));
#72215=CARTESIAN_POINT('Ctrl Pts',(-0.129609936051608,-0.198644224259631,
-0.579662659841458));
#72216=CARTESIAN_POINT('Ctrl Pts',(-0.127503286264467,-0.20000294111581,
-0.579486622933222));
#72217=CARTESIAN_POINT('Ctrl Pts',(-0.124283778770851,-0.202007863038646,
-0.579222939517429));
#72218=CARTESIAN_POINT('Ctrl Pts',(-0.123186615034183,-0.202678791308846,
-0.579134000849986));
#72219=CARTESIAN_POINT('Ctrl Pts',(-0.121160912232504,-0.203895005494751,
-0.578971551820555));
#72220=CARTESIAN_POINT('Ctrl Pts',(-0.120234018939932,-0.204442952238364,
-0.578897888497295));
#72221=CARTESIAN_POINT('Ctrl Pts',(-0.118706689585987,-0.20533187564164,
-0.578777638569231));
#72222=CARTESIAN_POINT('Ctrl Pts',(-0.118108451580459,-0.205676568921734,
-0.578730820474705));
#72223=CARTESIAN_POINT('Ctrl Pts',(-0.11692522724356,-0.206351455208957,
-0.578638790191275));
#72224=CARTESIAN_POINT('Ctrl Pts',(-0.116340331267228,-0.206681782386678,
-0.578593570604684));
#72225=CARTESIAN_POINT('Ctrl Pts',(-0.115027364560979,-0.207415956911952,
-0.5784926549391));
#72226=CARTESIAN_POINT('Ctrl Pts',(-0.114298547382574,-0.207818468615713,
-0.578437042915983));
#72227=CARTESIAN_POINT('Ctrl Pts',(-0.111751363888757,-0.209207775685885,
-0.578244036259951));
#72228=CARTESIAN_POINT('Ctrl Pts',(-0.1099221556088,-0.210174644424576,
-0.578107825966146));
#72229=CARTESIAN_POINT('Ctrl Pts',(-0.0972579440298088,-0.216658018774652,
-0.577179510633432));
#72230=CARTESIAN_POINT('Ctrl Pts',(-0.0860239447449395,-0.221358898838197,
-0.576428885493879));
#72231=CARTESIAN_POINT('Ctrl Pts',(-0.0641930178298191,-0.228579488531291,
-0.575017512308011));
#72232=CARTESIAN_POINT('Ctrl Pts',(-0.0536875482153833,-0.231272487607986,
-0.574357478384001));
#72233=CARTESIAN_POINT('Ctrl Pts',(-0.0340823292735756,-0.234889885050145,
-0.573114415965014));
#72234=CARTESIAN_POINT('Ctrl Pts',(-0.0250427285420628,-0.2360247780673,
-0.572537068560617));
#72235=CARTESIAN_POINT('Ctrl Pts',(-0.0137826979678303,-0.236784256940236,
-0.571800795587073));
#72236=CARTESIAN_POINT('Ctrl Pts',(-0.0116025592820808,-0.236901091583059,
-0.571657473194882));
#72237=CARTESIAN_POINT('Ctrl Pts',(-0.00811638441949301,-0.237039680438405,
-0.57142692553729));
#72238=CARTESIAN_POINT('Ctrl Pts',(-0.00681120873066814,-0.237080773404782,
-0.571340306293188));
#72239=CARTESIAN_POINT('Ctrl Pts',(-0.00433398712852715,-0.237138295145103,
-0.571175293579186));
#72240=CARTESIAN_POINT('Ctrl Pts',(-0.0031620251166205,-0.237156817276737,
-0.571096968108943));
#72241=CARTESIAN_POINT('Ctrl Pts',(-0.000491829408069863,-0.237179222061253,
-0.570917899582971));
#72242=CARTESIAN_POINT('Ctrl Pts',(0.00100638775418432,-0.237177596492656,
-0.570816987236155));
#72243=CARTESIAN_POINT('Ctrl Pts',(0.00562563048261394,-0.23712881668216,
-0.570504452008143));
#72244=CARTESIAN_POINT('Ctrl Pts',(0.00874570960937807,-0.23703424723826,
-0.570291364391872));
#72245=CARTESIAN_POINT('Ctrl Pts',(0.0295370486453282,-0.235993014212989,
-0.568857507091995));
#72246=CARTESIAN_POINT('Ctrl Pts',(0.0470534520428524,-0.23313276472498,
-0.56757621241717));
#72247=CARTESIAN_POINT('Ctrl Pts',(0.0682747558833584,-0.227177181415122,
-0.56596639182474));
#72248=CARTESIAN_POINT('Ctrl Pts',(0.0724310583169615,-0.225886380055069,
-0.565648588912877));
#72249=CARTESIAN_POINT('Ctrl Pts',(0.0826869346882144,-0.222389071818803,
-0.564860800502041));
#72250=CARTESIAN_POINT('Ctrl Pts',(0.088736352147564,-0.22004522166057,
-0.564392851018951));
#72251=CARTESIAN_POINT('Ctrl Pts',(0.0980214519375577,-0.216002402829693,
-0.563676433286827));
#72252=CARTESIAN_POINT('Ctrl Pts',(0.10132674335912,-0.214471764436723,
-0.563421798239548));
#72253=CARTESIAN_POINT('Ctrl Pts',(0.105593635895879,-0.21237514225777,
-0.563094790851715));
#72254=CARTESIAN_POINT('Ctrl Pts',(0.106588152603565,-0.21187775446711,
-0.563018696561857));
#72255=CARTESIAN_POINT('Ctrl Pts',(0.108206562668344,-0.21105405947461,
-0.562895112779373));
#72256=CARTESIAN_POINT('Ctrl Pts',(0.108832552105023,-0.210731943142361,
-0.562847372297404));
#72257=CARTESIAN_POINT('Ctrl Pts',(0.110053363718528,-0.210096857406963,
-0.562754401041409));
#72258=CARTESIAN_POINT('Ctrl Pts',(0.110648302977808,-0.209784140066978,
-0.562709156252696));
#72259=CARTESIAN_POINT('Ctrl Pts',(0.111978512731564,-0.20907771023795,
-0.562608118283999));
#72260=CARTESIAN_POINT('Ctrl Pts',(0.112713059494938,-0.208682635845613,
-0.562552409826735));
#72261=CARTESIAN_POINT('Ctrl Pts',(0.115269921669376,-0.207289994087695,
-0.562358739375872));
#72262=CARTESIAN_POINT('Ctrl Pts',(0.117081264603381,-0.206272331378097,
-0.56222197242369));
#72263=CARTESIAN_POINT('Ctrl Pts',(0.12930782146226,-0.199190155230564,
-0.561300133642804));
#72264=CARTESIAN_POINT('Ctrl Pts',(0.139262362439573,-0.192362417569494,
-0.560555750398351));
#72265=CARTESIAN_POINT('Ctrl Pts',(0.156976219061154,-0.178113655481915,
-0.559160198717179));
#72266=CARTESIAN_POINT('Ctrl Pts',(0.164835156615894,-0.170866526968388,
-0.558509614241831));
#72267=CARTESIAN_POINT('Ctrl Pts',(0.178592068984296,-0.156345167960695,
-0.557263537882503));
#72268=CARTESIAN_POINT('Ctrl Pts',(0.184599822741478,-0.149203931271848,
-0.556672697092615));
#72269=CARTESIAN_POINT('Ctrl Pts',(0.191484311341427,-0.139966308808759,
-0.555921193740991));
#72270=CARTESIAN_POINT('Ctrl Pts',(0.192772807237123,-0.138186299424059,
-0.555776959208841));
#72271=CARTESIAN_POINT('Ctrl Pts',(0.194789037651535,-0.135317865206395,
-0.555545290683498));
#72272=CARTESIAN_POINT('Ctrl Pts',(0.195532834493481,-0.134240844572613,
-0.55545847331205));
#72273=CARTESIAN_POINT('Ctrl Pts',(0.1969253908652,-0.132188288050696,-0.555293305184091));
#72274=CARTESIAN_POINT('Ctrl Pts',(0.197575913415688,-0.131213990939206,
-0.555215024294645));
#72275=CARTESIAN_POINT('Ctrl Pts',(0.199038908679309,-0.128987293962221,
-0.555036367636241));
#72276=CARTESIAN_POINT('Ctrl Pts',(0.199846821728958,-0.127731972658824,
-0.554935825468488));
#72277=CARTESIAN_POINT('Ctrl Pts',(0.202292085954818,-0.123852569943335,
-0.554625601978909));
#72278=CARTESIAN_POINT('Ctrl Pts',(0.203889944341918,-0.121204109427891,
-0.554414487113187));
#72279=CARTESIAN_POINT('Ctrl Pts',(0.214480468748191,-0.102847942259788,
-0.552955172454069));
#72280=CARTESIAN_POINT('Ctrl Pts',(0.221699529875901,-0.0861896030936155,
-0.551643272546658));
#72281=CARTESIAN_POINT('Ctrl Pts',(0.228091379389882,-0.0651279471798013,
-0.55003573205021));
#72282=CARTESIAN_POINT('Ctrl Pts',(0.229135979823658,-0.0613516934154544,
-0.549749713353507));
#72283=CARTESIAN_POINT('Ctrl Pts',(0.231672747531028,-0.0512098446968167,
-0.548989532873781));
#72284=CARTESIAN_POINT('Ctrl Pts',(0.232996187252141,-0.0448051156460757,
-0.548517688347433));
#72285=CARTESIAN_POINT('Ctrl Pts',(0.234645422208803,-0.0347406092982293,
-0.547796092467409));
#72286=CARTESIAN_POINT('Ctrl Pts',(0.235153761598731,-0.031114243509007,
-0.547540077025534));
#72287=CARTESIAN_POINT('Ctrl Pts',(0.235707023331009,-0.0263708316703005,
-0.547211585599379));
#72288=CARTESIAN_POINT('Ctrl Pts',(0.235828288448366,-0.0252634142876844,
-0.547135346919539));
#72289=CARTESIAN_POINT('Ctrl Pts',(0.236013493612088,-0.0234543748584933,
-0.547011588205249));
#72290=CARTESIAN_POINT('Ctrl Pts',(0.236082116669978,-0.0227532654514893,
-0.546963815873332));
#72291=CARTESIAN_POINT('Ctrl Pts',(0.236210078324722,-0.0213829567942696,
-0.546870833003076));
#72292=CARTESIAN_POINT('Ctrl Pts',(0.236269698846107,-0.0207137965562993,
-0.546825608107873));
#72293=CARTESIAN_POINT('Ctrl Pts',(0.236396864353383,-0.0192144950637545,
-0.546724666644068));
#72294=CARTESIAN_POINT('Ctrl Pts',(0.236462882146181,-0.0183842246462954,
-0.546669034272001));
#72295=CARTESIAN_POINT('Ctrl Pts',(0.236677778227756,-0.0154886265795101,
-0.546475887705503));
#72296=CARTESIAN_POINT('Ctrl Pts',(0.236803987621979,-0.0134216400827039,
-0.546339560101602));
#72297=CARTESIAN_POINT('Ctrl Pts',(0.237485492057007,0.000799090680145227,
-0.545410630885345));
#72298=CARTESIAN_POINT('Ctrl Pts',(0.23713202746367,0.0129798120500622,
-0.544659554214914));
#72299=CARTESIAN_POINT('Ctrl Pts',(0.234697959336753,0.0358682352331096,
-0.543246762281554));
#72300=CARTESIAN_POINT('Ctrl Pts',(0.232812051046232,0.0465639499299556,
-0.542585776208153));
#72301=CARTESIAN_POINT('Ctrl Pts',(0.228014886848421,0.0659063916198067,
-0.541343071473364));
#72302=CARTESIAN_POINT('Ctrl Pts',(0.225324834881934,0.0745863989112967,
-0.540767142030793));
#72303=CARTESIAN_POINT('Ctrl Pts',(0.221379776316486,0.0851336309306886,
-0.540032470055647));
#72304=CARTESIAN_POINT('Ctrl Pts',(0.220587314807362,0.0871663725392257,
-0.539889245432231));
#72305=CARTESIAN_POINT('Ctrl Pts',(0.219276024223611,0.0903975117953189,
-0.539658817914129));
#72306=CARTESIAN_POINT('Ctrl Pts',(0.218775132656203,0.0916030903061705,
-0.539572219909044));
#72307=CARTESIAN_POINT('Ctrl Pts',(0.217805659725784,0.0938831679032894,
-0.539407223712777));
#72308=CARTESIAN_POINT('Ctrl Pts',(0.217339013978693,0.0949584516607608,
-0.539328893320299));
#72309=CARTESIAN_POINT('Ctrl Pts',(0.216257571748591,0.0974006657528809,
-0.539149779944029));
#72310=CARTESIAN_POINT('Ctrl Pts',(0.215637755235712,0.098765304459563,
-0.539048827354598));
#72311=CARTESIAN_POINT('Ctrl Pts',(0.213686070078126,0.102956331492917,
-0.53873604017328));
#72312=CARTESIAN_POINT('Ctrl Pts',(0.212311299652096,0.105762248255869,
-0.538522737426246));
#72313=CARTESIAN_POINT('Ctrl Pts',(0.202805864629077,0.124230274180054,
-0.537092059582729));
#72314=CARTESIAN_POINT('Ctrl Pts',(0.193005765026251,0.138967368594582,
-0.53581454406287));
#72315=CARTESIAN_POINT('Ctrl Pts',(0.178826985613105,0.155860119530935,
-0.534203750671509));
#72316=CARTESIAN_POINT('Ctrl Pts',(0.17589509967971,0.159161497979249,-0.533881320985099));
#72317=CARTESIAN_POINT('Ctrl Pts',(0.168441890771932,0.167096363333458,
-0.533089889086122));
#72318=CARTESIAN_POINT('Ctrl Pts',(0.163819491191561,0.17163056488607,-0.532622876747621));
#72319=CARTESIAN_POINT('Ctrl Pts',(0.156318594807358,0.178408817208816,
-0.531907705975132));
#72320=CARTESIAN_POINT('Ctrl Pts',(0.153564149282636,0.180785134275456,
-0.531653404069181));
#72321=CARTESIAN_POINT('Ctrl Pts',(0.149897948038343,0.183803756890842,
-0.531326754984067));
#72322=CARTESIAN_POINT('Ctrl Pts',(0.14903496577768,0.184504186867197,-0.531250695658668));
#72323=CARTESIAN_POINT('Ctrl Pts',(0.147617445664233,0.185638266005345,
-0.531127154235261));
#72324=CARTESIAN_POINT('Ctrl Pts',(0.147065856878645,0.186075548752318,
-0.531079421464324));
#72325=CARTESIAN_POINT('Ctrl Pts',(0.145983724702753,0.186925612426653,
-0.530986452984858));
#72326=CARTESIAN_POINT('Ctrl Pts',(0.145453361590474,0.187338602745772,
-0.53094120334465));
#72327=CARTESIAN_POINT('Ctrl Pts',(0.144260796322612,0.188259128192028,
-0.530840141881582));
#72328=CARTESIAN_POINT('Ctrl Pts',(0.143597650706156,0.188765440341301,
-0.530784414909541));
#72329=CARTESIAN_POINT('Ctrl Pts',(0.141272670167787,0.190521222044709,
-0.530590616793896));
#72330=CARTESIAN_POINT('Ctrl Pts',(0.139597031901368,0.191752373634479,
-0.53045374275603));
#72331=CARTESIAN_POINT('Ctrl Pts',(0.128117934878563,0.199956237479907,
-0.529533246987873));
#72332=CARTESIAN_POINT('Ctrl Pts',(0.117811186178973,0.206197237749492,
-0.528790152173273));
#72333=CARTESIAN_POINT('Ctrl Pts',(0.0975772066812585,0.216434628539015,
-0.527398064029015));
#72334=CARTESIAN_POINT('Ctrl Pts',(0.0877677526280537,0.220594815865414,
-0.526749624709212));
#72335=CARTESIAN_POINT('Ctrl Pts',(0.0688559372362668,0.227153497815084,
-0.525502942794627));
#72336=CARTESIAN_POINT('Ctrl Pts',(0.0598261243365684,0.229696876582851,
-0.52490912582114));
#72337=CARTESIAN_POINT('Ctrl Pts',(0.0485206003293139,0.232169278467857,
-0.524154264256176));
#72338=CARTESIAN_POINT('Ctrl Pts',(0.0463645962284942,0.232609428446374,
-0.524009832921641));
#72339=CARTESIAN_POINT('Ctrl Pts',(0.0429162240681387,0.233263570410312,
-0.523777922555877));
#72340=CARTESIAN_POINT('Ctrl Pts',(0.0416276330411383,0.233496971328214,
-0.523691062443543));
#72341=CARTESIAN_POINT('Ctrl Pts',(0.0391828750733199,0.233918907047026,
-0.523525860479693));
#72342=CARTESIAN_POINT('Ctrl Pts',(0.0380271115126804,0.234109571521905,
-0.523447588896423));
#72343=CARTESIAN_POINT('Ctrl Pts',(0.0353964468609779,0.234523553845564,
-0.523269019571817));
#72344=CARTESIAN_POINT('Ctrl Pts',(0.0339207683405629,0.234741532449766,
-0.523168556045875));
#72345=CARTESIAN_POINT('Ctrl Pts',(0.0293852098264478,0.235367838586018,
-0.522858822306003));
#72346=CARTESIAN_POINT('Ctrl Pts',(0.0263194391213415,0.235730345002672,
-0.522648125112458));
#72347=CARTESIAN_POINT('Ctrl Pts',(0.00515981982593997,0.237814419393502,
-0.521184077497259));
#72348=CARTESIAN_POINT('Ctrl Pts',(-0.0130695234560479,0.237510557714901,
-0.51986641709386));
#72349=CARTESIAN_POINT('Ctrl Pts',(-0.0347144503614342,0.234649349495437,
-0.518271817473785));
#72350=CARTESIAN_POINT('Ctrl Pts',(-0.0383347093569048,0.234085119227144,
-0.518004355068976));
#72351=CARTESIAN_POINT('Ctrl Pts',(-0.0419392867764624,0.233437522368795,
-0.517737946518584));
#72352=CARTESIAN_POINT('Origin',(0.,0.,-2.1456589891905));
#72353=CARTESIAN_POINT('',(-0.0419392740612461,0.233437524653205,-0.397890210729054));
#72354=CARTESIAN_POINT('',(-0.041939274266712,0.233437524616291,-0.417694787181515));
#72355=CARTESIAN_POINT('',(-0.0419392741328076,0.233437524640348,-2.1456589891905));
#72356=CARTESIAN_POINT('Ctrl Pts',(-0.0419392740612461,0.233437524653205,
-0.397890210729054));
#72357=CARTESIAN_POINT('Ctrl Pts',(-0.0402008843706342,0.233749842913811,
-0.398010601581905));
#72358=CARTESIAN_POINT('Ctrl Pts',(-0.0384590613533141,0.234042732781722,
-0.398131602917604));
#72359=CARTESIAN_POINT('Ctrl Pts',(-0.0186066639421137,0.237153331412323,
-0.39951511916644));
#72360=CARTESIAN_POINT('Ctrl Pts',(-0.000234620402447351,0.237881494207574,
-0.400844414765493));
#72361=CARTESIAN_POINT('Ctrl Pts',(0.0217149774632429,0.236207682940379,
-0.402452128909572));
#72362=CARTESIAN_POINT('Ctrl Pts',(0.0253890361293069,0.235841063358142,
-0.402721619783982));
#72363=CARTESIAN_POINT('Ctrl Pts',(0.0355580255649566,0.23458594681924,
-0.403466707445045));
#72364=CARTESIAN_POINT('Ctrl Pts',(0.0420273580620156,0.233513709194453,
-0.403939857560636));
#72365=CARTESIAN_POINT('Ctrl Pts',(0.0520347969310622,0.231425610210343,
-0.404663206288373));
#72366=CARTESIAN_POINT('Ctrl Pts',(0.0556076302153558,0.230593209523418,
-0.404919700847363));
#72367=CARTESIAN_POINT('Ctrl Pts',(0.0602396563793955,0.229400103609189,
-0.405248723717678));
#72368=CARTESIAN_POINT('Ctrl Pts',(0.0613174160332498,0.229114378316452,
-0.405325028635298));
#72369=CARTESIAN_POINT('Ctrl Pts',(0.0630731333764691,0.228635642957073,
-0.405448878267782));
#72370=CARTESIAN_POINT('Ctrl Pts',(0.0637523010832571,0.228447196358497,
-0.405496675809539));
#72371=CARTESIAN_POINT('Ctrl Pts',(0.0650773210398278,0.228073177824649,
-0.405589694652314));
#72372=CARTESIAN_POINT('Ctrl Pts',(0.0657232388445533,0.227887884824202,
-0.405634930408187));
#72373=CARTESIAN_POINT('Ctrl Pts',(0.0671679766557816,0.227466782698395,
-0.405735883728774));
#72374=CARTESIAN_POINT('Ctrl Pts',(0.0679663677772369,0.227229503415424,
-0.405791517163645));
#72375=CARTESIAN_POINT('Ctrl Pts',(0.070744392289104,0.226387931645108,
-0.405984606915277));
#72376=CARTESIAN_POINT('Ctrl Pts',(0.0727174200606783,0.225761914790316,
-0.40612087782565));
#72377=CARTESIAN_POINT('Ctrl Pts',(0.086258118429489,0.221269679973657,
-0.407051732514566));
#72378=CARTESIAN_POINT('Ctrl Pts',(0.097522249466343,0.216541502009419,
-0.407804574319244));
#72379=CARTESIAN_POINT('Ctrl Pts',(0.116166878108451,0.206963754168709,
-0.409091080310384));
#72380=CARTESIAN_POINT('Ctrl Pts',(0.123732078996018,0.202531745948396,
-0.409625618141897));
#72381=CARTESIAN_POINT('Ctrl Pts',(0.13939916052274,0.192147233529331,-0.410789473634976));
#72382=CARTESIAN_POINT('Ctrl Pts',(0.147402540302711,0.186078321364228,
-0.411420256346053));
#72383=CARTESIAN_POINT('Ctrl Pts',(0.157127667175876,0.177681739833076,
-0.412253228564104));
#72384=CARTESIAN_POINT('Ctrl Pts',(0.159225334355741,0.175804426178106,
-0.412437159364938));
#72385=CARTESIAN_POINT('Ctrl Pts',(0.162343934824314,0.172911820551287,
-0.412717458118383));
#72386=CARTESIAN_POINT('Ctrl Pts',(0.16338990116483,0.171923793885699,-0.412812672211412));
#72387=CARTESIAN_POINT('Ctrl Pts',(0.165267913119384,0.170117194016267,
-0.412985864782996));
#72388=CARTESIAN_POINT('Ctrl Pts',(0.166103035186032,0.169301873660903,
-0.41306370075071));
#72389=CARTESIAN_POINT('Ctrl Pts',(0.167887839869451,0.167533471406042,
-0.413231849910912));
#72390=CARTESIAN_POINT('Ctrl Pts',(0.168835494180268,0.166578409743422,
-0.413322249113473));
#72391=CARTESIAN_POINT('Ctrl Pts',(0.171383487121962,0.163966421324328,
-0.41356840591792));
#72392=CARTESIAN_POINT('Ctrl Pts',(0.172967859910619,0.16229419510503,-0.413724847319821));
#72393=CARTESIAN_POINT('Ctrl Pts',(0.181583586867232,0.152931247570632,
-0.414594776761866));
#72394=CARTESIAN_POINT('Ctrl Pts',(0.188125582841696,0.1448077200227,-0.415328368871273));
#72395=CARTESIAN_POINT('Ctrl Pts',(0.203644990521002,0.122702748566535,
-0.417269428085389));
#72396=CARTESIAN_POINT('Ctrl Pts',(0.211726561384617,0.10816221640806,-0.418497393025293));
#72397=CARTESIAN_POINT('Ctrl Pts',(0.220612248233739,0.0872890464152246,
-0.420126884760523));
#72398=CARTESIAN_POINT('Ctrl Pts',(0.222783065238373,0.0815895945170851,
-0.420558761122068));
#72399=CARTESIAN_POINT('Ctrl Pts',(0.225150298159732,0.0745723561417519,
-0.42106987370135));
#72400=CARTESIAN_POINT('Ctrl Pts',(0.225558331637648,0.0733289321285298,
-0.421159667051202));
#72401=CARTESIAN_POINT('Ctrl Pts',(0.226183230348393,0.0713700611089194,
-0.421299845011767));
#72402=CARTESIAN_POINT('Ctrl Pts',(0.226407033041811,0.0706568803577203,
-0.421350615350519));
#72403=CARTESIAN_POINT('Ctrl Pts',(0.226822487521583,0.069310728799461,
-0.421445931070812));
#72404=CARTESIAN_POINT('Ctrl Pts',(0.22701486249877,0.068678018234242,-0.421490515325779));
#72405=CARTESIAN_POINT('Ctrl Pts',(0.227455498332989,0.0672067089610365,
-0.421593703890249));
#72406=CARTESIAN_POINT('Ctrl Pts',(0.227701770405727,0.0663675317168976,
-0.421652193003436));
#72407=CARTESIAN_POINT('Ctrl Pts',(0.228494851880888,0.0636087040252514,
-0.421843339050414));
#72408=CARTESIAN_POINT('Ctrl Pts',(0.229022088873881,0.06168345013147,-0.421974925963065));
#72409=CARTESIAN_POINT('Ctrl Pts',(0.233456489299866,0.0446495281187777,
-0.423125177904624));
#72410=CARTESIAN_POINT('Ctrl Pts',(0.235888469034036,0.0291939203176684,
-0.424073933576794));
#72411=CARTESIAN_POINT('Ctrl Pts',(0.237589924520497,-0.000408606105287425,
-0.425891524116123));
#72412=CARTESIAN_POINT('Ctrl Pts',(0.23714916268035,-0.0144690854275087,
-0.426755543941157));
#72413=CARTESIAN_POINT('Ctrl Pts',(0.235008687643185,-0.0322114963700264,
-0.427904329174176));
#72414=CARTESIAN_POINT('Ctrl Pts',(0.234457629580041,-0.036003902824007,
-0.428153179623342));
#72415=CARTESIAN_POINT('Ctrl Pts',(0.233542553792801,-0.0413822923748594,
-0.428511606046887));
#72416=CARTESIAN_POINT('Ctrl Pts',(0.23325369924883,-0.0429805784204745,
-0.428618814649973));
#72417=CARTESIAN_POINT('Ctrl Pts',(0.23272466247339,-0.0457452729318386,
-0.428805528409901));
#72418=CARTESIAN_POINT('Ctrl Pts',(0.232492066046093,-0.0469130861917967,
-0.428884789944866));
#72419=CARTESIAN_POINT('Ctrl Pts',(0.231996920755761,-0.0493049338275856,
-0.429047959753064));
#72420=CARTESIAN_POINT('Ctrl Pts',(0.231733455230604,-0.0505287379874477,
-0.429131895060779));
#72421=CARTESIAN_POINT('Ctrl Pts',(0.231038654738067,-0.0536363237877092,
-0.429346201667886));
#72422=CARTESIAN_POINT('Ctrl Pts',(0.230593968257228,-0.0555169940670322,
-0.429476996867895));
#72423=CARTESIAN_POINT('Ctrl Pts',(0.228768197821384,-0.062837842015074,
-0.429990571060034));
#72424=CARTESIAN_POINT('Ctrl Pts',(0.227217260567347,-0.0682333499428704,
-0.430378738217138));
#72425=CARTESIAN_POINT('Ctrl Pts',(0.220121007886839,-0.089982339936886,
-0.431984167073725));
#72426=CARTESIAN_POINT('Ctrl Pts',(0.212989736483191,-0.105760534315724,
-0.43324960033746));
#72427=CARTESIAN_POINT('Ctrl Pts',(0.200469044737067,-0.126957803020404,
-0.435043658018043));
#72428=CARTESIAN_POINT('Ctrl Pts',(0.19643382964896,-0.133116064449294,
-0.435576726327406));
#72429=CARTESIAN_POINT('Ctrl Pts',(0.189800908020513,-0.142278661390064,
-0.43637880373576));
#72430=CARTESIAN_POINT('Ctrl Pts',(0.187403414383106,-0.145422030492873,
-0.436655673345544));
#72431=CARTESIAN_POINT('Ctrl Pts',(0.184211833622378,-0.14939642008148,
-0.437006485523086));
#72432=CARTESIAN_POINT('Ctrl Pts',(0.183488897013931,-0.150283448142588,
-0.437084830715379));
#72433=CARTESIAN_POINT('Ctrl Pts',(0.182306219892668,-0.151713310929788,
-0.437211152784681));
#72434=CARTESIAN_POINT('Ctrl Pts',(0.181850418228026,-0.15225935750927,
-0.43725940123931));
#72435=CARTESIAN_POINT('Ctrl Pts',(0.180961816069301,-0.153314213045529,
-0.437352608865237));
#72436=CARTESIAN_POINT('Ctrl Pts',(0.180529314264568,-0.153823254099554,
-0.437397587223204));
#72437=CARTESIAN_POINT('Ctrl Pts',(0.179462826932491,-0.155067782685971,
-0.437507568946035));
#72438=CARTESIAN_POINT('Ctrl Pts',(0.178826454723412,-0.155801228015175,
-0.437572399658116));
#72439=CARTESIAN_POINT('Ctrl Pts',(0.176977415524469,-0.157906067508014,
-0.437758563791342));
#72440=CARTESIAN_POINT('Ctrl Pts',(0.175753321840142,-0.159267391888125,
-0.437879107303134));
#72441=CARTESIAN_POINT('Ctrl Pts',(0.164350572631791,-0.171656900411977,
-0.438978997848292));
#72442=CARTESIAN_POINT('Ctrl Pts',(0.153160949645616,-0.181711459257032,
-0.439893777391911));
#72443=CARTESIAN_POINT('Ctrl Pts',(0.138148528935538,-0.192822191159927,
-0.441038425045506));
#72444=CARTESIAN_POINT('Ctrl Pts',(0.135152405300156,-0.194933938540231,
-0.441263104408691));
#72445=CARTESIAN_POINT('Ctrl Pts',(0.122931893651822,-0.203130060792316,
-0.442168650629999));
#72446=CARTESIAN_POINT('Ctrl Pts',(0.113337284337999,-0.208635312100769,
-0.442856178370973));
#72447=CARTESIAN_POINT('Ctrl Pts',(0.100027671606413,-0.215082406365566,
-0.443807503838229));
#72448=CARTESIAN_POINT('Ctrl Pts',(0.0966228017272741,-0.216633349926769,
-0.444050583637591));
#72449=CARTESIAN_POINT('Ctrl Pts',(0.0917031371936131,-0.218735238080925,
-0.44440213740468));
#72450=CARTESIAN_POINT('Ctrl Pts',(0.0902170884414607,-0.219352334131449,
-0.444508369164063));
#72451=CARTESIAN_POINT('Ctrl Pts',(0.0876229608785047,-0.220398750486248,
-0.444693939303387));
#72452=CARTESIAN_POINT('Ctrl Pts',(0.0865177087370344,-0.220834957549538,
-0.44477304250186));
#72453=CARTESIAN_POINT('Ctrl Pts',(0.0842365786921663,-0.221715492184689,
-0.444936407309595));
#72454=CARTESIAN_POINT('Ctrl Pts',(0.0830603548880778,-0.222158812575235,
-0.445020699697912));
#72455=CARTESIAN_POINT('Ctrl Pts',(0.0800443984693883,-0.22326823129227,
-0.445237006210582));
#72456=CARTESIAN_POINT('Ctrl Pts',(0.0781998764283866,-0.223920940862848,
-0.445369460052377));
#72457=CARTESIAN_POINT('Ctrl Pts',(0.0708501825523862,-0.226419846148451,
-0.445898013209767));
#72458=CARTESIAN_POINT('Ctrl Pts',(0.0652864985862891,-0.228086295206418,
-0.446299910210928));
#72459=CARTESIAN_POINT('Ctrl Pts',(0.0411774939264183,-0.234353113480744,
-0.448050093494924));
#72460=CARTESIAN_POINT('Ctrl Pts',(0.0221759879560849,-0.236907139943528,
-0.449458710709847));
#72461=CARTESIAN_POINT('Ctrl Pts',(-0.00284066065774192,-0.237231848917687,
-0.451273932748468));
#72462=CARTESIAN_POINT('Ctrl Pts',(-0.0087607412272072,-0.237087068993664,
-0.451699909201556));
#72463=CARTESIAN_POINT('Ctrl Pts',(-0.0169756273633561,-0.236577993606905,
-0.452281181733561));
#72464=CARTESIAN_POINT('Ctrl Pts',(-0.0192795789151716,-0.236401391090274,
-0.45244312021214));
#72465=CARTESIAN_POINT('Ctrl Pts',(-0.0232979563725679,-0.236034233808542,
-0.452723260259365));
#72466=CARTESIAN_POINT('Ctrl Pts',(-0.0250135389880172,-0.235858596625228,
-0.452842126646201));
#72467=CARTESIAN_POINT('Ctrl Pts',(-0.027555335470836,-0.235570326833739,
-0.453016999107878));
#72468=CARTESIAN_POINT('Ctrl Pts',(-0.028383071328361,-0.235472029576621,
-0.453073750877317));
#72469=CARTESIAN_POINT('Ctrl Pts',(-0.0297986546241951,-0.235296349982555,
-0.453170452742688));
#72470=CARTESIAN_POINT('Ctrl Pts',(-0.0303867487670684,-0.235221125029791,
-0.453210521232329));
#72471=CARTESIAN_POINT('Ctrl Pts',(-0.0317263637550768,-0.235044662693193,
-0.453301549264324));
#72472=CARTESIAN_POINT('Ctrl Pts',(-0.0324776860982156,-0.234942025963743,
-0.453352429666835));
#72473=CARTESIAN_POINT('Ctrl Pts',(-0.0345381891891899,-0.234650471332525,
-0.453491527343151));
#72474=CARTESIAN_POINT('Ctrl Pts',(-0.035846326073275,-0.234454198758655,
-0.453579345008174));
#72475=CARTESIAN_POINT('Ctrl Pts',(-0.0427931742419882,-0.233352392536122,
-0.45404341983562));
#72476=CARTESIAN_POINT('Ctrl Pts',(-0.048399939233285,-0.232254284692115,
-0.454409982761481));
#72477=CARTESIAN_POINT('Ctrl Pts',(-0.070242644332587,-0.227150783254028,
-0.455825804021682));
#72478=CARTESIAN_POINT('Ctrl Pts',(-0.0860762115126081,-0.221635890598079,
-0.456828239404915));
#72479=CARTESIAN_POINT('Ctrl Pts',(-0.110897179275683,-0.209925670259526,
-0.45852886764447));
#72480=CARTESIAN_POINT('Ctrl Pts',(-0.120272781510286,-0.204698279790981,
-0.459204484337004));
#72481=CARTESIAN_POINT('Ctrl Pts',(-0.131170057264296,-0.197614716801845,
-0.460051577446284));
#72482=CARTESIAN_POINT('Ctrl Pts',(-0.133060212188065,-0.196346987655507,
-0.460200869375425));
#72483=CARTESIAN_POINT('Ctrl Pts',(-0.136022430203147,-0.194297807170501,
-0.46043877119538));
#72484=CARTESIAN_POINT('Ctrl Pts',(-0.137106715151686,-0.19353420351136,
-0.460526704445047));
#72485=CARTESIAN_POINT('Ctrl Pts',(-0.139134782726734,-0.192080347532853,
-0.460692820743926));
#72486=CARTESIAN_POINT('Ctrl Pts',(-0.140079979471034,-0.191392128729863,
-0.460770923843428));
#72487=CARTESIAN_POINT('Ctrl Pts',(-0.142198817739738,-0.189825251910599,
-0.460947577442449));
#72488=CARTESIAN_POINT('Ctrl Pts',(-0.143369469312758,-0.188942650374211,
-0.461046279823175));
#72489=CARTESIAN_POINT('Ctrl Pts',(-0.146796749557804,-0.186308494317819,
-0.461338566674719));
#72490=CARTESIAN_POINT('Ctrl Pts',(-0.149029933676435,-0.18452701255234,
-0.46153332556047));
#72491=CARTESIAN_POINT('Ctrl Pts',(-0.166631517953804,-0.169957717901932,
-0.463103962006038));
#72492=CARTESIAN_POINT('Ctrl Pts',(-0.180356218749445,-0.155315811630681,
-0.464560004873317));
#72493=CARTESIAN_POINT('Ctrl Pts',(-0.196891452236667,-0.132487819079628,
-0.466617053257804));
#72494=CARTESIAN_POINT('Ctrl Pts',(-0.201355788173507,-0.125599084031395,
-0.467213298114807));
#72495=CARTESIAN_POINT('Ctrl Pts',(-0.2075677115856,-0.114828213116781,
-0.468096700864029));
#72496=CARTESIAN_POINT('Ctrl Pts',(-0.209582769928244,-0.111107791776598,
-0.468393488839807));
#72497=CARTESIAN_POINT('Ctrl Pts',(-0.212027228168022,-0.106291137612642,
-0.468765412395763));
#72498=CARTESIAN_POINT('Ctrl Pts',(-0.212549361757136,-0.105243148844418,
-0.468845604880173));
#72499=CARTESIAN_POINT('Ctrl Pts',(-0.213378761086747,-0.103547086929671,
-0.468974165816297));
#72500=CARTESIAN_POINT('Ctrl Pts',(-0.213690877402603,-0.102901427804725,
-0.469022823232137));
#72501=CARTESIAN_POINT('Ctrl Pts',(-0.214286702653162,-0.101654472148345,
-0.469116235895805));
#72502=CARTESIAN_POINT('Ctrl Pts',(-0.214570816903586,-0.101053387804816,
-0.469161014465183));
#72503=CARTESIAN_POINT('Ctrl Pts',(-0.215193257597783,-0.099722064756122,
-0.469259656831312));
#72504=CARTESIAN_POINT('Ctrl Pts',(-0.215530405607414,-0.0989912754775003,
-0.469313449126351));
#72505=CARTESIAN_POINT('Ctrl Pts',(-0.216712615039491,-0.0963940899296627,
-0.469503419858634));
#72506=CARTESIAN_POINT('Ctrl Pts',(-0.217537235187122,-0.0945184114141076,
-0.469638420469324));
#72507=CARTESIAN_POINT('Ctrl Pts',(-0.224065539945921,-0.0791309594976372,
-0.470729992054561));
#72508=CARTESIAN_POINT('Ctrl Pts',(-0.228529786552498,-0.0651255177717425,
-0.471625291624658));
#72509=CARTESIAN_POINT('Ctrl Pts',(-0.23532626214526,-0.0341277841372568,
-0.473570121112919));
#72510=CARTESIAN_POINT('Ctrl Pts',(-0.237170985036829,-0.01711657282713,
-0.474617686914739));
#72511=CARTESIAN_POINT('Ctrl Pts',(-0.237175510836601,0.00214638939489631,
-0.475870955694842));
#72512=CARTESIAN_POINT('Ctrl Pts',(-0.237145359082231,0.00434834028815707,
-0.47601512181016));
#72513=CARTESIAN_POINT('Ctrl Pts',(-0.237044903180087,0.00798473490960728,
-0.476254855331902));
#72514=CARTESIAN_POINT('Ctrl Pts',(-0.236992223209531,0.00941955946395762,
-0.476349872605398));
#72515=CARTESIAN_POINT('Ctrl Pts',(-0.236873117601517,0.0120195060600362,
-0.476522857117236));
#72516=CARTESIAN_POINT('Ctrl Pts',(-0.236811113601335,0.0131847927332773,
-0.476600683486768));
#72517=CARTESIAN_POINT('Ctrl Pts',(-0.236658971904528,0.0156948426340991,
-0.476768981640673));
#72518=CARTESIAN_POINT('Ctrl Pts',(-0.236565966107027,0.0170393843122896,
-0.476859540754235));
#72519=CARTESIAN_POINT('Ctrl Pts',(-0.236277335842771,0.0207520433863723,
-0.477110764543423));
#72520=CARTESIAN_POINT('Ctrl Pts',(-0.236057579516744,0.0231180702826091,
-0.477272178452543));
#72521=CARTESIAN_POINT('Ctrl Pts',(-0.234371341527379,0.0387230070048102,
-0.478345799241754));
#72522=CARTESIAN_POINT('Ctrl Pts',(-0.231827622907716,0.051819307098901,
-0.479291876888957));
#72523=CARTESIAN_POINT('Ctrl Pts',(-0.224751972433897,0.0768019941004218,
-0.481174563573363));
#72524=CARTESIAN_POINT('Ctrl Pts',(-0.220336789296876,0.0886774573073427,
-0.482105981532162));
#72525=CARTESIAN_POINT('Ctrl Pts',(-0.21209038525342,0.106381357016382,
-0.483514374959463));
#72526=CARTESIAN_POINT('Ctrl Pts',(-0.208914736192351,0.112489897628098,
-0.484003931083776));
#72527=CARTESIAN_POINT('Ctrl Pts',(-0.204783659210171,0.119656024480095,
-0.484575659483176));
#72528=CARTESIAN_POINT('Ctrl Pts',(-0.204079126485024,0.120853720008388,
-0.484671121043142));
#72529=CARTESIAN_POINT('Ctrl Pts',(-0.202966120490294,0.122708323604762,
-0.484818713877912));
#72530=CARTESIAN_POINT('Ctrl Pts',(-0.202564904912202,0.123369518479409,
-0.484871287542501));
#72531=CARTESIAN_POINT('Ctrl Pts',(-0.201816990583711,0.124588580189074,
-0.484968117648391));
#72532=CARTESIAN_POINT('Ctrl Pts',(-0.201471208877567,0.125146969650448,
-0.485012428985358));
#72533=CARTESIAN_POINT('Ctrl Pts',(-0.200673488157288,0.126423302483734,
-0.485113625113941));
#72534=CARTESIAN_POINT('Ctrl Pts',(-0.200220013014459,0.127140263899515,
-0.485170408317801));
#72535=CARTESIAN_POINT('Ctrl Pts',(-0.198791562366065,0.129372101639205,
-0.485347025530662));
#72536=CARTESIAN_POINT('Ctrl Pts',(-0.197803140658203,0.130878355659917,
-0.485466015018669));
#72537=CARTESIAN_POINT('Ctrl Pts',(-0.18864869768923,0.144488148110305,
-0.486540663785389));
#72538=CARTESIAN_POINT('Ctrl Pts',(-0.179397232324798,0.155826553017773,
-0.487433626443334));
#72539=CARTESIAN_POINT('Ctrl Pts',(-0.15774239696061,0.177861371996881,
-0.489327073172076));
#72540=CARTESIAN_POINT('Ctrl Pts',(-0.145159473051866,0.188271021835937,
-0.490324847174287));
#72541=CARTESIAN_POINT('Ctrl Pts',(-0.129223059709154,0.198901015833218,
-0.491562713949262));
#72542=CARTESIAN_POINT('Ctrl Pts',(-0.12680748098783,0.200449681668915,
-0.491749589634421));
#72543=CARTESIAN_POINT('Ctrl Pts',(-0.12311560389951,0.202723160656437,
-0.492034416923675));
#72544=CARTESIAN_POINT('Ctrl Pts',(-0.12185964127556,0.203480611992349,
-0.492131178801979));
#72545=CARTESIAN_POINT('Ctrl Pts',(-0.119656643881099,0.204781493783321,
-0.492300710836373));
#72546=CARTESIAN_POINT('Ctrl Pts',(-0.118712722098046,0.205330129705883,
-0.492373289982694));
#72547=CARTESIAN_POINT('Ctrl Pts',(-0.116723903225186,0.206467793501117,
-0.492526104654826));
#72548=CARTESIAN_POINT('Ctrl Pts',(-0.115678261094875,0.207055449471853,
-0.492606386866096));
#72549=CARTESIAN_POINT('Ctrl Pts',(-0.113163273995616,0.208443887393663,
-0.492799359829047));
#72550=CARTESIAN_POINT('Ctrl Pts',(-0.111689840898464,0.209237090313794,
-0.492912316323004));
#72551=CARTESIAN_POINT('Ctrl Pts',(-0.106542987048353,0.211937975373904,
-0.493306621938611));
#72552=CARTESIAN_POINT('Ctrl Pts',(-0.102828297687207,0.213764943205885,
-0.493590763661581));
#72553=CARTESIAN_POINT('Ctrl Pts',(-0.0936053500143426,0.218004965719879,
-0.494295595237789));
#72554=CARTESIAN_POINT('Ctrl Pts',(-0.088049706851249,0.220307434051798,
-0.494719664064118));
#72555=CARTESIAN_POINT('Ctrl Pts',(-0.0722385820114713,0.226166534839886,
-0.495924181426436));
#72556=CARTESIAN_POINT('Ctrl Pts',(-0.0618181169873884,0.229233947684174,
-0.496715919119564));
#72557=CARTESIAN_POINT('Ctrl Pts',(-0.0481417438444124,0.232259177699159,
-0.497738874503745));
#72558=CARTESIAN_POINT('Ctrl Pts',(-0.0450458290258016,0.232879402586337,
-0.497969329421446));
#72559=CARTESIAN_POINT('Ctrl Pts',(-0.0419392658597717,0.233437526126678,
-0.498199055407226));
#72560=CARTESIAN_POINT('Ctrl Pts',(-0.0419392867764624,0.233437522368795,
-0.517737946518584));
#72561=CARTESIAN_POINT('Ctrl Pts',(-0.0514623511486289,0.231726612641677,
-0.51703411206606));
#72562=CARTESIAN_POINT('Ctrl Pts',(-0.0608759382465519,0.229433824766293,
-0.516337312495976));
#72563=CARTESIAN_POINT('Ctrl Pts',(-0.0715629283511039,0.226126043590324,
-0.515562958538504));
#72564=CARTESIAN_POINT('Ctrl Pts',(-0.0729947285602193,0.225667920181476,
-0.515459576608732));
#72565=CARTESIAN_POINT('Ctrl Pts',(-0.0751711249529407,0.224948671643561,
-0.515303087799546));
#72566=CARTESIAN_POINT('Ctrl Pts',(-0.0759189023175492,0.224697403673176,
-0.515249439445631));
#72567=CARTESIAN_POINT('Ctrl Pts',(-0.0772855192608476,0.224230592288743,
-0.515151629011857));
#72568=CARTESIAN_POINT('Ctrl Pts',(-0.0779047229749196,0.224016214068525,
-0.515107402689105));
#72569=CARTESIAN_POINT('Ctrl Pts',(-0.0793041858884918,0.223525193222377,
-0.515007647748705));
#72570=CARTESIAN_POINT('Ctrl Pts',(-0.0800838910345873,0.223247029887003,
-0.514952209355774));
#72571=CARTESIAN_POINT('Ctrl Pts',(-0.0821041079633582,0.222514362342653,
-0.514808892137006));
#72572=CARTESIAN_POINT('Ctrl Pts',(-0.0833423270342379,0.222053558208546,
-0.514721369203872));
#72573=CARTESIAN_POINT('Ctrl Pts',(-0.0922251708022917,0.218663030614834,
-0.514095341158277));
#72574=CARTESIAN_POINT('Ctrl Pts',(-0.0997183114492473,0.215349233822919,
-0.51357708992896));
#72575=CARTESIAN_POINT('Ctrl Pts',(-0.117882231037556,0.206164397940351,
-0.512310166070876));
#72576=CARTESIAN_POINT('Ctrl Pts',(-0.128300448376669,0.199847423043494,
-0.511573089755153));
#72577=CARTESIAN_POINT('Ctrl Pts',(-0.147672766592826,0.185959463134733,
-0.510103593364523));
#72578=CARTESIAN_POINT('Ctrl Pts',(-0.156641371690452,0.17847016250468,
-0.509374149377564));
#72579=CARTESIAN_POINT('Ctrl Pts',(-0.167033702916567,0.168402995036752,
-0.508435998315449));
#72580=CARTESIAN_POINT('Ctrl Pts',(-0.169010830082696,0.166418643426867,
-0.508252955764386));
#72581=CARTESIAN_POINT('Ctrl Pts',(-0.171947491464907,0.163364935657382,
-0.507973758136767));
#72582=CARTESIAN_POINT('Ctrl Pts',(-0.172933261847976,0.162321067077269,
-0.507878743396792));
#72583=CARTESIAN_POINT('Ctrl Pts',(-0.174702685431904,0.16041294584397,
-0.507705786759474));
#72584=CARTESIAN_POINT('Ctrl Pts',(-0.175489560840209,0.159551732814112,
-0.507627985883393));
#72585=CARTESIAN_POINT('Ctrl Pts',(-0.177171215091402,0.157683719433989,
-0.507459769557748));
#72586=CARTESIAN_POINT('Ctrl Pts',(-0.178063830872781,0.156675035778925,
-0.50736926704471));
#72587=CARTESIAN_POINT('Ctrl Pts',(-0.180464769243914,0.153914879862574,
-0.507122470887297));
#72588=CARTESIAN_POINT('Ctrl Pts',(-0.181956124299485,0.152148911765601,
-0.506965487148934));
#72589=CARTESIAN_POINT('Ctrl Pts',(-0.190134593628091,0.142172246476447,
-0.506083409527655));
#72590=CARTESIAN_POINT('Ctrl Pts',(-0.196290863209069,0.133543816870864,
-0.505337518261049));
#72591=CARTESIAN_POINT('Ctrl Pts',(-0.210478725735969,0.110547602358844,
-0.50339438022508));
#72592=CARTESIAN_POINT('Ctrl Pts',(-0.217630301738286,0.0957030689456048,
-0.502178219779088));
#72593=CARTESIAN_POINT('Ctrl Pts',(-0.225244129204583,0.0745247350646868,
-0.500561877307296));
#72594=CARTESIAN_POINT('Ctrl Pts',(-0.2270784659515,0.0687330955978113,
-0.500131726981203));
#72595=CARTESIAN_POINT('Ctrl Pts',(-0.229035072486159,0.0616167527717919,
-0.499622377079648));
#72596=CARTESIAN_POINT('Ctrl Pts',(-0.229371133830322,0.0603537224358601,
-0.49953270127418));
#72597=CARTESIAN_POINT('Ctrl Pts',(-0.229882831118833,0.0583645653148398,
-0.499392675940227));
#72598=CARTESIAN_POINT('Ctrl Pts',(-0.230065500234272,0.0576402998658913,
-0.499341941857678));
#72599=CARTESIAN_POINT('Ctrl Pts',(-0.230403405875435,0.0562733357002763,
-0.49924667385942));
#72600=CARTESIAN_POINT('Ctrl Pts',(-0.230559375793822,0.0556308547037943,
-0.499202101263233));
#72601=CARTESIAN_POINT('Ctrl Pts',(-0.230915453123314,0.0541368562435719,
-0.49909891527044));
#72602=CARTESIAN_POINT('Ctrl Pts',(-0.231113539158999,0.0532848737760093,
-0.499040417231651));
#72603=CARTESIAN_POINT('Ctrl Pts',(-0.231748558272797,0.0504834380976598,
-0.498849142919466));
#72604=CARTESIAN_POINT('Ctrl Pts',(-0.232165588398956,0.0485294961560803,
-0.498717438937636));
#72605=CARTESIAN_POINT('Ctrl Pts',(-0.235613769565828,0.0313103810206143,
-0.497569871360487));
#72606=CARTESIAN_POINT('Ctrl Pts',(-0.237160675224263,0.0157842829669599,
-0.496623519766758));
#72607=CARTESIAN_POINT('Ctrl Pts',(-0.237188604127509,-0.0147789281299883,
-0.494750069891481));
#72608=CARTESIAN_POINT('Ctrl Pts',(-0.23578018455968,-0.0297402292983789,
-0.493827016014195));
#72609=CARTESIAN_POINT('Ctrl Pts',(-0.23236734549757,-0.0476203715957152,
-0.492651002314969));
#72610=CARTESIAN_POINT('Ctrl Pts',(-0.231701642444954,-0.0507605193646444,
-0.492441802332666));
#72611=CARTESIAN_POINT('Ctrl Pts',(-0.230631972160886,-0.0553454584455917,
-0.492131964310255));
#72612=CARTESIAN_POINT('Ctrl Pts',(-0.230277679226126,-0.0568015548231795,
-0.492032911674053));
#72613=CARTESIAN_POINT('Ctrl Pts',(-0.229620965763451,-0.0593933820801181,
-0.491855385340801));
#72614=CARTESIAN_POINT('Ctrl Pts',(-0.229323854684311,-0.0605304166555545,
-0.491777085035815));
#72615=CARTESIAN_POINT('Ctrl Pts',(-0.228682341034493,-0.062912934223662,
-0.491612111504454));
#72616=CARTESIAN_POINT('Ctrl Pts',(-0.228336186359553,-0.064157901132294,
-0.491525383708313));
#72617=CARTESIAN_POINT('Ctrl Pts',(-0.227395156112566,-0.0674382697546252,
-0.491295450577449));
#72618=CARTESIAN_POINT('Ctrl Pts',(-0.226783138195888,-0.0694685898179573,
-0.491151692167827));
#72619=CARTESIAN_POINT('Ctrl Pts',(-0.22366841892273,-0.0793213156881715,
-0.490446793698876));
#72620=CARTESIAN_POINT('Ctrl Pts',(-0.220788051571348,-0.0870174763010837,
-0.48987342836396));
#72621=CARTESIAN_POINT('Ctrl Pts',(-0.213652113992268,-0.103434223423304,
-0.488599857345659));
#72622=CARTESIAN_POINT('Ctrl Pts',(-0.209248903577,-0.112074677576266,-0.487896429064942));
#72623=CARTESIAN_POINT('Ctrl Pts',(-0.197020347226297,-0.132824059607327,
-0.486138401879095));
#72624=CARTESIAN_POINT('Ctrl Pts',(-0.18859589810098,-0.144536876232833,
-0.485081792203671));
#72625=CARTESIAN_POINT('Ctrl Pts',(-0.177810426369258,-0.156970307311911,
-0.483934427361521));
#72626=CARTESIAN_POINT('Ctrl Pts',(-0.176440148551139,-0.158508989664251,
-0.483791980227073));
#72627=CARTESIAN_POINT('Ctrl Pts',(-0.174505815557176,-0.16062487754063,
-0.483595689220372));
#72628=CARTESIAN_POINT('Ctrl Pts',(-0.173958651448422,-0.161217302366558,
-0.483540684589748));
#72629=CARTESIAN_POINT('Ctrl Pts',(-0.172954742711665,-0.162293191194496,
-0.483440727706311));
#72630=CARTESIAN_POINT('Ctrl Pts',(-0.172498966030143,-0.162777546661928,
-0.483395704187179));
#72631=CARTESIAN_POINT('Ctrl Pts',(-0.171548327053136,-0.163779317003408,
-0.483302545048399));
#72632=CARTESIAN_POINT('Ctrl Pts',(-0.171053151864804,-0.164296416468658,
-0.483254434112858));
#72633=CARTESIAN_POINT('Ctrl Pts',(-0.169745288109525,-0.165649864728131,
-0.483128421265536));
#72634=CARTESIAN_POINT('Ctrl Pts',(-0.16892874727279,-0.166482488580105,
-0.483050810577667));
#72635=CARTESIAN_POINT('Ctrl Pts',(-0.165155689556132,-0.170273519791817,
-0.482696832755316));
#72636=CARTESIAN_POINT('Ctrl Pts',(-0.162127181963509,-0.173159624008968,
-0.482425631234877));
#72637=CARTESIAN_POINT('Ctrl Pts',(-0.153048168132241,-0.181364573800002,
-0.481643757450121));
#72638=CARTESIAN_POINT('Ctrl Pts',(-0.146800956810188,-0.186457365572262,
-0.481144171665557));
#72639=CARTESIAN_POINT('Ctrl Pts',(-0.123978034154506,-0.203203279985697,
-0.479402201908506));
#72640=CARTESIAN_POINT('Ctrl Pts',(-0.106184579874836,-0.213041973453268,
-0.478179868526611));
#72641=CARTESIAN_POINT('Ctrl Pts',(-0.0849653580669599,-0.221448622922334,
-0.476700754035614));
#72642=CARTESIAN_POINT('Ctrl Pts',(-0.0825573869965616,-0.222357553689453,
-0.476532763417803));
#72643=CARTESIAN_POINT('Ctrl Pts',(-0.078696082338833,-0.223743704105128,
-0.476262908351054));
#72644=CARTESIAN_POINT('Ctrl Pts',(-0.0772520564513907,-0.224246378103167,
-0.476161886098676));
#72645=CARTESIAN_POINT('Ctrl Pts',(-0.0746856261138126,-0.225112036978749,
-0.475982110346465));
#72646=CARTESIAN_POINT('Ctrl Pts',(-0.0735651740691968,-0.225480679923413,
-0.47590354642424));
#72647=CARTESIAN_POINT('Ctrl Pts',(-0.0712256807259108,-0.226231109220051,
-0.475739322221883));
#72648=CARTESIAN_POINT('Ctrl Pts',(-0.0700062144122565,-0.226611434412937,
-0.475653616889312));
#72649=CARTESIAN_POINT('Ctrl Pts',(-0.0668195534499327,-0.227577108437216,
-0.475429356496869));
#72650=CARTESIAN_POINT('Ctrl Pts',(-0.0648477636399524,-0.228146795061074,
-0.475290296577235));
#72651=CARTESIAN_POINT('Ctrl Pts',(-0.0557572574911122,-0.230645845931149,
-0.474647667199291));
#72652=CARTESIAN_POINT('Ctrl Pts',(-0.0485590568855369,-0.232267896181336,
-0.474134356723536));
#72653=CARTESIAN_POINT('Ctrl Pts',(-0.0284951742657086,-0.235815676410801,
-0.472690872100666));
#72654=CARTESIAN_POINT('Ctrl Pts',(-0.0155294289507012,-0.237022743404765,
-0.471742669150701));
#72655=CARTESIAN_POINT('Ctrl Pts',(0.0094366785587664,-0.237289243673352,
-0.469919356345127));
#72656=CARTESIAN_POINT('Ctrl Pts',(0.0213986745210681,-0.236510867068765,
-0.469047370412982));
#72657=CARTESIAN_POINT('Ctrl Pts',(0.035304013149444,-0.234541901188131,
-0.468067716503805));
#72658=CARTESIAN_POINT('Ctrl Pts',(0.0373524440351625,-0.234224406099606,
-0.46792430451187));
#72659=CARTESIAN_POINT('Ctrl Pts',(0.0402181788888056,-0.233741679995695,
-0.467725182387074));
#72660=CARTESIAN_POINT('Ctrl Pts',(0.0410391039769695,-0.233598944513275,
-0.467668315845569));
#72661=CARTESIAN_POINT('Ctrl Pts',(0.0425206148403899,-0.233333301031761,
-0.467566025705486));
#72662=CARTESIAN_POINT('Ctrl Pts',(0.0431814617101092,-0.233211906775567,
-0.467520519028002));
#72663=CARTESIAN_POINT('Ctrl Pts',(0.044533968352047,-0.232957511867592,
-0.467427644080444));
#72664=CARTESIAN_POINT('Ctrl Pts',(0.0452255655488018,-0.232824236123435,
-0.467380291629511));
#72665=CARTESIAN_POINT('Ctrl Pts',(0.0470088738068744,-0.232472333827784,
-0.467258525621523));
#72666=CARTESIAN_POINT('Ctrl Pts',(0.0480996729121381,-0.232249094292064,
-0.4671843684625));
#72667=CARTESIAN_POINT('Ctrl Pts',(0.0527646357164179,-0.23126010141126,
-0.466868453991817));
#72668=CARTESIAN_POINT('Ctrl Pts',(0.0563226241436127,-0.230419415123055,
-0.466630601618582));
#72669=CARTESIAN_POINT('Ctrl Pts',(0.0661697280620907,-0.227850980099421,
-0.465977358646288));
#72670=CARTESIAN_POINT('Ctrl Pts',(0.0724093857151596,-0.225945558088657,
-0.465569183306518));
#72671=CARTESIAN_POINT('Ctrl Pts',(0.0823864202456606,-0.222442978584746,
-0.464914471010075));
#72672=CARTESIAN_POINT('Ctrl Pts',(0.0861748967030278,-0.221002916982992,
-0.464665377033247));
#72673=CARTESIAN_POINT('Ctrl Pts',(0.106553528967471,-0.212652931231677,
-0.463314298453605));
#72674=CARTESIAN_POINT('Ctrl Pts',(0.122352154159339,-0.203972519875487,
-0.462220545870337));
#72675=CARTESIAN_POINT('Ctrl Pts',(0.139551044774914,-0.191799667874045,
-0.460857998384811));
#72676=CARTESIAN_POINT('Ctrl Pts',(0.142047991959621,-0.189957819576722,
-0.46065564795281));
#72677=CARTESIAN_POINT('Ctrl Pts',(0.145693190100282,-0.187156910089194,
-0.460353015817484));
#72678=CARTESIAN_POINT('Ctrl Pts',(0.146869720775871,-0.186235065395491,
-0.460254189487388));
#72679=CARTESIAN_POINT('Ctrl Pts',(0.148952883987814,-0.184570831629846,
-0.460077099347008));
#72680=CARTESIAN_POINT('Ctrl Pts',(0.149862883847405,-0.183832721508379,
-0.459999008289518));
#72681=CARTESIAN_POINT('Ctrl Pts',(0.151776956454218,-0.182256540535712,
-0.459833173423538));
#72682=CARTESIAN_POINT('Ctrl Pts',(0.152779637791821,-0.181416849371181,
-0.459745365394014));
#72683=CARTESIAN_POINT('Ctrl Pts',(0.155444549125654,-0.179147369388942,
-0.459509435362496));
#72684=CARTESIAN_POINT('Ctrl Pts',(0.157093949148122,-0.177702781040604,
-0.459360707463244));
#72685=CARTESIAN_POINT('Ctrl Pts',(0.165595322110128,-0.170046189899455,
-0.458579629646133));
#72686=CARTESIAN_POINT('Ctrl Pts',(0.172098807595499,-0.16346093926156,
-0.457931581224259));
#72687=CARTESIAN_POINT('Ctrl Pts',(0.185283715097079,-0.148449089382346,
-0.456503245439868));
#72688=CARTESIAN_POINT('Ctrl Pts',(0.191810725852447,-0.139913553763965,
-0.455719874969718));
#72689=CARTESIAN_POINT('Ctrl Pts',(0.204411021810946,-0.120889215053568,
-0.454053417957853));
#72690=CARTESIAN_POINT('Ctrl Pts',(0.210305811315452,-0.11031587462482,
-0.453172508836579));
#72691=CARTESIAN_POINT('Ctrl Pts',(0.21623846239433,-0.0974536575230821,
-0.452184422248417));
#72692=CARTESIAN_POINT('Ctrl Pts',(0.217082992328944,-0.0955576431178358,
-0.452040819644487));
#72693=CARTESIAN_POINT('Ctrl Pts',(0.218231746381074,-0.0928847701260245,
-0.451841478060546));
#72694=CARTESIAN_POINT('Ctrl Pts',(0.218556898643629,-0.0921170872198375,
-0.451784579434576));
#72695=CARTESIAN_POINT('Ctrl Pts',(0.219136826062409,-0.0907275244071472,
-0.451682248749058));
#72696=CARTESIAN_POINT('Ctrl Pts',(0.219393018375959,-0.0901062470092216,
-0.451636733407867));
#72697=CARTESIAN_POINT('Ctrl Pts',(0.21991223233453,-0.0888317875940768,
-0.451543861744528));
#72698=CARTESIAN_POINT('Ctrl Pts',(0.220174991358857,-0.0881785100269253,
-0.451496521097271));
#72699=CARTESIAN_POINT('Ctrl Pts',(0.220845399946186,-0.0864900439209981,
-0.451374821448213));
#72700=CARTESIAN_POINT('Ctrl Pts',(0.221248687831748,-0.0854531253327159,
-0.451300718312726));
#72701=CARTESIAN_POINT('Ctrl Pts',(0.222942878341639,-0.0810046801372399,
-0.450985362135807));
#72702=CARTESIAN_POINT('Ctrl Pts',(0.224162362922549,-0.0775662542901242,
-0.450747996940529));
#72703=CARTESIAN_POINT('Ctrl Pts',(0.227332931836171,-0.0679262032263988,
-0.45009653729647));
#72704=CARTESIAN_POINT('Ctrl Pts',(0.229109202077763,-0.0616702256393484,
-0.449689610618353));
#72705=CARTESIAN_POINT('Ctrl Pts',(0.231612389548724,-0.0512399843677539,
-0.449025390541219));
#72706=CARTESIAN_POINT('Ctrl Pts',(0.232488508698639,-0.0471055159063544,
-0.4487657115224));
#72707=CARTESIAN_POINT('Ctrl Pts',(0.23647883700083,-0.0254346505775926,
-0.447414084391004));
#72708=CARTESIAN_POINT('Ctrl Pts',(0.237720636882419,-0.00761416327510002,
-0.446329478342523));
#72709=CARTESIAN_POINT('Ctrl Pts',(0.236822961484322,0.0132876600504383,
-0.444976746520249));
#72710=CARTESIAN_POINT('Ctrl Pts',(0.236628102131184,0.0163956337452305,
-0.444773672864555));
#72711=CARTESIAN_POINT('Ctrl Pts',(0.236249063767338,0.0209904960157593,
-0.444470166132395));
#72712=CARTESIAN_POINT('Ctrl Pts',(0.236111891245874,0.0224810073932401,
-0.444371200947694));
#72713=CARTESIAN_POINT('Ctrl Pts',(0.23584217899795,0.0251360438902577,
-0.444193956681814));
#72714=CARTESIAN_POINT('Ctrl Pts',(0.235715097169576,0.0263010832222142,
-0.44411585151076));
#72715=CARTESIAN_POINT('Ctrl Pts',(0.235428080119742,0.0287629444071511,
-0.44395008621603));
#72716=CARTESIAN_POINT('Ctrl Pts',(0.235266052674576,0.0300594780412402,
-0.443862362613071));
#72717=CARTESIAN_POINT('Ctrl Pts',(0.234804215254474,0.0335222856539613,
-0.44362690176707));
#72718=CARTESIAN_POINT('Ctrl Pts',(0.234485148629836,0.0356858186086232,
-0.44347856282941));
#72719=CARTESIAN_POINT('Ctrl Pts',(0.23267450102878,0.0468879065362686,
-0.442703917987147));
#72720=CARTESIAN_POINT('Ctrl Pts',(0.230690270873367,0.0558378010345413,
-0.442062225799171));
#72721=CARTESIAN_POINT('Ctrl Pts',(0.225251352603745,0.0750355546668417,
-0.440636343388626));
#72722=CARTESIAN_POINT('Ctrl Pts',(0.221603480165496,0.0852078216531518,
-0.439848589708582));
#72723=CARTESIAN_POINT('Ctrl Pts',(0.212413278523452,0.106205752846442,
-0.438174641943308));
#72724=CARTESIAN_POINT('Ctrl Pts',(0.206705141033089,0.116927781852566,
-0.43729063317855));
#72725=CARTESIAN_POINT('Ctrl Pts',(0.19908986164733,0.128916656490078,-0.436299888886334));
#72726=CARTESIAN_POINT('Ctrl Pts',(0.197955516287549,0.130651795370431,
-0.436156467143259));
#72727=CARTESIAN_POINT('Ctrl Pts',(0.196333471553988,0.133063303984531,
-0.435957333790632));
#72728=CARTESIAN_POINT('Ctrl Pts',(0.195864773267705,0.133752254430053,
-0.435900465606926));
#72729=CARTESIAN_POINT('Ctrl Pts',(0.195011593591186,0.134992260630924,
-0.43579817339183));
#72730=CARTESIAN_POINT('Ctrl Pts',(0.194628383583158,0.135544178811035,
-0.435752666271157));
#72731=CARTESIAN_POINT('Ctrl Pts',(0.193838688223285,0.136671283038966,
-0.435659791492658));
#72732=CARTESIAN_POINT('Ctrl Pts',(0.193431978203111,0.137246298678765,
-0.435612439646585));
#72733=CARTESIAN_POINT('Ctrl Pts',(0.192375766403062,0.138725573051882,
-0.435490677039562));
#72734=CARTESIAN_POINT('Ctrl Pts',(0.191722439098596,0.139627098321284,
-0.435416522649381));
#72735=CARTESIAN_POINT('Ctrl Pts',(0.188897318589356,0.143468259334777,
-0.435100636820759));
#72736=CARTESIAN_POINT('Ctrl Pts',(0.186663952874782,0.146362258358951,
-0.434862809442849));
#72737=CARTESIAN_POINT('Ctrl Pts',(0.180262935483613,0.154271715467041,
-0.434209658028853));
#72738=CARTESIAN_POINT('Ctrl Pts',(0.175953889872365,0.159168869607122,
-0.43380154680976));
#72739=CARTESIAN_POINT('Ctrl Pts',(0.168641375131357,0.166818968297945,
-0.43314628192893));
#72740=CARTESIAN_POINT('Ctrl Pts',(0.165759502591866,0.169682851439624,
-0.432896580774437));
#72741=CARTESIAN_POINT('Ctrl Pts',(0.149744292150789,0.184800513316992,
-0.431545486892093));
#72742=CARTESIAN_POINT('Ctrl Pts',(0.135326600557098,0.195604725745614,
-0.430452273013452));
#72743=CARTESIAN_POINT('Ctrl Pts',(0.117150411071567,0.206245950702394,
-0.429090302541077));
#72744=CARTESIAN_POINT('Ctrl Pts',(0.114441922270815,0.207761054976932,
-0.428887907784918));
#72745=CARTESIAN_POINT('Ctrl Pts',(0.110385963612875,0.209926544454168,
-0.42858522204126));
#72746=CARTESIAN_POINT('Ctrl Pts',(0.109060741340316,0.210618065595952,
-0.428486387192704));
#72747=CARTESIAN_POINT('Ctrl Pts',(0.106685214654437,0.21182922023441,-0.428309287602884));
#72748=CARTESIAN_POINT('Ctrl Pts',(0.105637420018949,0.212353688402477,
-0.428231195685402));
#72749=CARTESIAN_POINT('Ctrl Pts',(0.1034120445917,0.213447042412632,-0.428065365116619));
#72750=CARTESIAN_POINT('Ctrl Pts',(0.102233562431806,0.214013993642643,
-0.42797756228994));
#72751=CARTESIAN_POINT('Ctrl Pts',(0.0990672143205684,0.215505158490184,
-0.427741661176857));
#72752=CARTESIAN_POINT('Ctrl Pts',(0.0970711631449704,0.216411587055149,
-0.427592957252577));
#72753=CARTESIAN_POINT('Ctrl Pts',(0.0865946862030465,0.220994970148713,
-0.42681227857495));
#72754=CARTESIAN_POINT('Ctrl Pts',(0.0779182515088997,0.224201078261169,
-0.426164624792756));
#72755=CARTESIAN_POINT('Ctrl Pts',(0.0588060693320402,0.230019816604003,
-0.424736438060719));
#72756=CARTESIAN_POINT('Ctrl Pts',(0.0483344366950005,0.232445739595188,
-0.423952792161658));
#72757=CARTESIAN_POINT('Ctrl Pts',(0.0258001242724952,0.236077280990494,
-0.422285869348412));
#72758=CARTESIAN_POINT('Ctrl Pts',(0.0137341111087947,0.237085557425128,
-0.421404770354038));
#72759=CARTESIAN_POINT('Ctrl Pts',(-0.000432393023030546,0.237183684747741,
-0.420416521983644));
#72760=CARTESIAN_POINT('Ctrl Pts',(-0.0025077789487524,0.237170822514593,
-0.420272931411953));
#72761=CARTESIAN_POINT('Ctrl Pts',(-0.00541631169140616,0.237114611884206,
-0.420073603679899));
#72762=CARTESIAN_POINT('Ctrl Pts',(-0.00624973361394499,0.237094108918329,
-0.420016707078061));
#72763=CARTESIAN_POINT('Ctrl Pts',(-0.0077547477749643,0.237049142791723,
-0.419914378950628));
#72764=CARTESIAN_POINT('Ctrl Pts',(-0.0084263757899602,0.237026218893271,
-0.419868864156181));
#72765=CARTESIAN_POINT('Ctrl Pts',(-0.00980153154737315,0.236973429761481,
-0.419775992286766));
#72766=CARTESIAN_POINT('Ctrl Pts',(-0.01050503797967,0.236943285711089,
-0.41972865089578));
#72767=CARTESIAN_POINT('Ctrl Pts',(-0.0123197623723455,0.236857429576628,
-0.419606947065551));
#72768=CARTESIAN_POINT('Ctrl Pts',(-0.0134307569198347,0.236797029923703,
-0.419532840526114));
#72769=CARTESIAN_POINT('Ctrl Pts',(-0.0181824776367429,0.236505150558754,
-0.419217449203993));
#72770=CARTESIAN_POINT('Ctrl Pts',(-0.0218182432858041,0.236197494786223,
-0.418980053342243));
#72771=CARTESIAN_POINT('Ctrl Pts',(-0.030969545985803,0.235209982859015,
-0.418389173064982));
#72772=CARTESIAN_POINT('Ctrl Pts',(-0.0364708068239119,0.23441998686729,
-0.418040077434656));
#72773=CARTESIAN_POINT('Ctrl Pts',(-0.041939274266712,0.233437524616291,
-0.417694787181515));
#72774=CARTESIAN_POINT('Origin',(0.,0.,-2.1456589891905));
#72775=CARTESIAN_POINT('',(-0.0419325474085422,0.233395695413117,-0.298126337027085));
#72776=CARTESIAN_POINT('',(-0.0418736008932845,0.233079825957759,-0.317824451239062));
#72777=CARTESIAN_POINT('',(-0.0419392741328076,0.233437524640348,-2.1456589891905));
#72778=CARTESIAN_POINT('',(-0.237369928097243,-0.000181986744939411,-0.375941010809497));
#72779=CARTESIAN_POINT('Ctrl Pts',(-0.237369928097243,-0.000181986744939411,
-0.375941010809497));
#72780=CARTESIAN_POINT('Ctrl Pts',(-0.237469999104454,-0.0119683065141777,
-0.375148184390915));
#72781=CARTESIAN_POINT('Ctrl Pts',(-0.231312589235971,-0.102360953237923,
-0.369060714614336));
#72782=CARTESIAN_POINT('Ctrl Pts',(-0.115177429001217,-0.255620947329064,
-0.357678601479762));
#72783=CARTESIAN_POINT('Ctrl Pts',(0.152400560897723,-0.235333760199054,
-0.341794671405773));
#72784=CARTESIAN_POINT('Ctrl Pts',(0.280370506222409,0.000533234281509477,
-0.325910741331786));
#72785=CARTESIAN_POINT('Ctrl Pts',(0.162276893924525,0.216235263332081,
-0.311354629872224));
#72786=CARTESIAN_POINT('Ctrl Pts',(0.0163630136312862,0.243270981762062,
-0.302093161770659));
#72787=CARTESIAN_POINT('Ctrl Pts',(-0.0419325474085123,0.233395695413122,
-0.298126337027087));
#72788=CARTESIAN_POINT('Ctrl Pts',(-0.237174924912043,-0.000188727228977812,
-0.376053073332811));
#72789=CARTESIAN_POINT('Ctrl Pts',(-0.237190585303674,0.0194918044542662,
-0.377272926375048));
#72790=CARTESIAN_POINT('Ctrl Pts',(-0.234756782705812,0.0390977061925586,
-0.378451184420277));
#72791=CARTESIAN_POINT('Ctrl Pts',(-0.229105195484696,0.0614333847607206,
-0.379919998904733));
#72792=CARTESIAN_POINT('Ctrl Pts',(-0.228212702756558,0.0646700237461788,
-0.380135849644863));
#72793=CARTESIAN_POINT('Ctrl Pts',(-0.226491614925483,0.0704314095087167,
-0.380526254875689));
#72794=CARTESIAN_POINT('Ctrl Pts',(-0.225688713936378,0.0729632685109562,
-0.380699991109408));
#72795=CARTESIAN_POINT('Ctrl Pts',(-0.224395850630544,0.0768144599800887,
-0.380967855542854));
#72796=CARTESIAN_POINT('Ctrl Pts',(-0.223936367095655,0.078143857021848,
-0.381060982329268));
#72797=CARTESIAN_POINT('Ctrl Pts',(-0.223078216687786,0.080556955284831,
-0.381231271595175));
#72798=CARTESIAN_POINT('Ctrl Pts',(-0.22268340597101,0.0816419893768781,
-0.381308304032937));
#72799=CARTESIAN_POINT('Ctrl Pts',(-0.221803655756444,0.0840058897771032,
-0.38147716554136));
#72800=CARTESIAN_POINT('Ctrl Pts',(-0.221315547558358,0.0852835241817804,
-0.381569098305943));
#72801=CARTESIAN_POINT('Ctrl Pts',(-0.219939615107987,0.0887936855495577,
-0.381823555960584));
#72802=CARTESIAN_POINT('Ctrl Pts',(-0.219028896687038,0.0910170015028857,
-0.381986843881685));
#72803=CARTESIAN_POINT('Ctrl Pts',(-0.212370799921784,0.106592354277255,
-0.383146136638752));
#72804=CARTESIAN_POINT('Ctrl Pts',(-0.205441365751811,0.119402648033143,
-0.384182916473199));
#72805=CARTESIAN_POINT('Ctrl Pts',(-0.190568615642849,0.141727634527022,
-0.386133581692759));
#72806=CARTESIAN_POINT('Ctrl Pts',(-0.182967356395915,0.151413587888032,
-0.387038167992818));
#72807=CARTESIAN_POINT('Ctrl Pts',(-0.171882058048072,0.163478649016614,
-0.388215039346255));
#72808=CARTESIAN_POINT('Ctrl Pts',(-0.169037093203672,0.166418675765035,
-0.388506147198009));
#72809=CARTESIAN_POINT('Ctrl Pts',(-0.164245486320776,0.171120655449421,
-0.388976999564615));
#72810=CARTESIAN_POINT('Ctrl Pts',(-0.162343188455039,0.172926426810922,
-0.389159183029999));
#72811=CARTESIAN_POINT('Ctrl Pts',(-0.159703418668383,0.17535028397106,
-0.389405137297903));
#72812=CARTESIAN_POINT('Ctrl Pts',(-0.158991645560508,0.175995911160324,
-0.389470791627737));
#72813=CARTESIAN_POINT('Ctrl Pts',(-0.157820416812469,0.177045391888606,
-0.389577717980516));
#72814=CARTESIAN_POINT('Ctrl Pts',(-0.157363296841877,0.177451817631253,
-0.389619177469419));
#72815=CARTESIAN_POINT('Ctrl Pts',(-0.156400609881027,0.178301098009743,
-0.389705910087934));
#72816=CARTESIAN_POINT('Ctrl Pts',(-0.155894724843367,0.178743579201823,
-0.389751153800993));
#72817=CARTESIAN_POINT('Ctrl Pts',(-0.154757371946464,0.179729883221839,
-0.389852145791806));
#72818=CARTESIAN_POINT('Ctrl Pts',(-0.154124898513095,0.180272545899769,
-0.389907809728756));
#72819=CARTESIAN_POINT('Ctrl Pts',(-0.151909575130615,0.182153113904561,
-0.390101109266142));
#72820=CARTESIAN_POINT('Ctrl Pts',(-0.150312005502342,0.183473642906006,
-0.390237556081786));
#72821=CARTESIAN_POINT('Ctrl Pts',(-0.139350334965236,0.192295112575101,
-0.391155589866821));
#72822=CARTESIAN_POINT('Ctrl Pts',(-0.129444850091223,0.199098043317687,
-0.391896836478088));
#72823=CARTESIAN_POINT('Ctrl Pts',(-0.109939702884554,0.210420035364313,
-0.393281432332941));
#72824=CARTESIAN_POINT('Ctrl Pts',(-0.100470304905444,0.21510239281493,
-0.393924314566495));
#72825=CARTESIAN_POINT('Ctrl Pts',(-0.0819504608263965,0.222769402657644,
-0.395172090841339));
#72826=CARTESIAN_POINT('Ctrl Pts',(-0.0729709057571046,0.2258700938572,
-0.395773115494786));
#72827=CARTESIAN_POINT('Ctrl Pts',(-0.0617037172939343,0.229018575852127,
-0.39653613915634));
#72828=CARTESIAN_POINT('Ctrl Pts',(-0.0595688466963732,0.229583119536072,
-0.396681071878779));
#72829=CARTESIAN_POINT('Ctrl Pts',(-0.056153956429874,0.230435313952003,
-0.396913617204924));
#72830=CARTESIAN_POINT('Ctrl Pts',(-0.0548788605507008,0.230742304933986,
-0.397000605165877));
#72831=CARTESIAN_POINT('Ctrl Pts',(-0.0524601018400909,0.231303460380716,
-0.397165942201058));
#72832=CARTESIAN_POINT('Ctrl Pts',(-0.05131697020594,0.231559758060649,
-0.397244220040114));
#72833=CARTESIAN_POINT('Ctrl Pts',(-0.048716098995227,0.232122685836553,
-0.397422653988228));
#72834=CARTESIAN_POINT('Ctrl Pts',(-0.0472572871926885,0.232424069777982,
-0.397522974605593));
#72835=CARTESIAN_POINT('Ctrl Pts',(-0.0445122365249925,0.232964273359007,
-0.397712226431447));
#72836=CARTESIAN_POINT('Ctrl Pts',(-0.04322669682703,0.233206226894684,
-0.39780105124681));
#72837=CARTESIAN_POINT('Ctrl Pts',(-0.0419392740612461,0.233437524653205,
-0.397890210729054));
#72838=CARTESIAN_POINT('',(-0.236816548519718,-4.82205570482326E-5,-0.395672065486472));
#72839=CARTESIAN_POINT('Ctrl Pts',(-0.041939274266712,0.233437524616291,
-0.417694787181515));
#72840=CARTESIAN_POINT('Ctrl Pts',(-0.0428698155356764,0.233270344016001,
-0.417636030896746));
#72841=CARTESIAN_POINT('Ctrl Pts',(-0.0437994072801449,0.233097590351859,
-0.417577385479228));
#72842=CARTESIAN_POINT('Ctrl Pts',(-0.0481263531409487,0.23226667743249,
-0.417304550759911));
#72843=CARTESIAN_POINT('Ctrl Pts',(-0.0515100750404628,0.231539776861124,
-0.417091590177645));
#72844=CARTESIAN_POINT('Ctrl Pts',(-0.0730643407221923,0.226413520843067,
-0.415731321572093));
#72845=CARTESIAN_POINT('Ctrl Pts',(-0.0906745869905617,0.219953437514709,
-0.414596511065129));
#72846=CARTESIAN_POINT('Ctrl Pts',(-0.109995505769665,0.210147130652429,
-0.413194607920678));
#72847=CARTESIAN_POINT('Ctrl Pts',(-0.112622192228822,0.208751211597952,
-0.413000569756606));
#72848=CARTESIAN_POINT('Ctrl Pts',(-0.11653627827804,0.206575743854621,
-0.412705816499035));
#72849=CARTESIAN_POINT('Ctrl Pts',(-0.117843711415678,0.205832702961808,
-0.412606397290873));
#72850=CARTESIAN_POINT('Ctrl Pts',(-0.120112899086648,0.204514370675183,
-0.412432112128609));
#72851=CARTESIAN_POINT('Ctrl Pts',(-0.121077816773909,0.203944596768285,
-0.412357447253752));
#72852=CARTESIAN_POINT('Ctrl Pts',(-0.123117521890662,0.202720594792607,
-0.412198414774323));
#72853=CARTESIAN_POINT('Ctrl Pts',(-0.124191209850555,0.202064611051853,
-0.412113984670837));
#72854=CARTESIAN_POINT('Ctrl Pts',(-0.126376271600266,0.200705624901073,
-0.411940666037161));
#72855=CARTESIAN_POINT('Ctrl Pts',(-0.127487118026636,0.20000186125685,
-0.411851751454164));
#72856=CARTESIAN_POINT('Ctrl Pts',(-0.130214875953954,0.1982417635852,-0.411631398698134));
#72857=CARTESIAN_POINT('Ctrl Pts',(-0.131824822177707,0.197174863060566,
-0.411499572145909));
#72858=CARTESIAN_POINT('Ctrl Pts',(-0.144869112648568,0.188299332280254,
-0.410416684793781));
#72859=CARTESIAN_POINT('Ctrl Pts',(-0.155610667273648,0.179524090849719,
-0.409428755865637));
#72860=CARTESIAN_POINT('Ctrl Pts',(-0.175998990922182,0.159656644566247,
-0.4073594508553));
#72861=CARTESIAN_POINT('Ctrl Pts',(-0.18550737581262,0.148502279798145,
-0.406280363932357));
#72862=CARTESIAN_POINT('Ctrl Pts',(-0.196312641385644,0.133155871578909,
-0.404947002586524));
#72863=CARTESIAN_POINT('Ctrl Pts',(-0.198608427800127,0.129706733800864,
-0.404656325229395));
#72864=CARTESIAN_POINT('Ctrl Pts',(-0.201455416163695,0.1251764926425,-0.404287669095979));
#72865=CARTESIAN_POINT('Ctrl Pts',(-0.202090188945879,0.124149082556119,
-0.404204912092669));
#72866=CARTESIAN_POINT('Ctrl Pts',(-0.203093503802128,0.122497082078524,
-0.404073254579364));
#72867=CARTESIAN_POINT('Ctrl Pts',(-0.203467066745241,0.121875588984757,
-0.404024040241966));
#72868=CARTESIAN_POINT('Ctrl Pts',(-0.20417947741013,0.120677953061953,
-0.403929823028724));
#72869=CARTESIAN_POINT('Ctrl Pts',(-0.204518745392452,0.120102082182325,
-0.403884794844485));
#72870=CARTESIAN_POINT('Ctrl Pts',(-0.205327868345856,0.118715312399557,
-0.403777004447757));
#72871=CARTESIAN_POINT('Ctrl Pts',(-0.205795366284811,0.117903037312684,
-0.403714392515051));
#72872=CARTESIAN_POINT('Ctrl Pts',(-0.207399599021535,0.115077077996875,
-0.403498296667782));
#72873=CARTESIAN_POINT('Ctrl Pts',(-0.208511734536915,0.113049480760451,
-0.403346286137321));
#72874=CARTESIAN_POINT('Ctrl Pts',(-0.211186592785501,0.107998985907927,
-0.40297427101964));
#72875=CARTESIAN_POINT('Ctrl Pts',(-0.212714293180425,0.104958038560421,
-0.402756033157679));
#72876=CARTESIAN_POINT('Ctrl Pts',(-0.219017458803409,0.0917079433893473,
-0.401825180362117));
#72877=CARTESIAN_POINT('Ctrl Pts',(-0.223127630984375,0.0811978604855395,
-0.401136796826917));
#72878=CARTESIAN_POINT('Ctrl Pts',(-0.230148509132521,0.0586229852930964,
-0.399687854717072));
#72879=CARTESIAN_POINT('Ctrl Pts',(-0.232892040678517,0.046543019007061,
-0.398928593311946));
#72880=CARTESIAN_POINT('Ctrl Pts',(-0.235454519399103,0.0290129582105658,
-0.397802477268319));
#72881=CARTESIAN_POINT('Ctrl Pts',(-0.236048799425014,0.0236968321811222,
-0.397458039662757));
#72882=CARTESIAN_POINT('Ctrl Pts',(-0.23660689132188,0.0165111704860901,
-0.396986274539072));
#72883=CARTESIAN_POINT('Ctrl Pts',(-0.236729089594629,0.0146552920532204,
-0.396863880091339));
#72884=CARTESIAN_POINT('Ctrl Pts',(-0.236896966262464,0.0115487533799083,
-0.396657999017235));
#72885=CARTESIAN_POINT('Ctrl Pts',(-0.236954596731431,0.0102988016100876,
-0.396574888504609));
#72886=CARTESIAN_POINT('Ctrl Pts',(-0.237044835434167,0.00793522221117625,
-0.39641719225462));
#72887=CARTESIAN_POINT('Ctrl Pts',(-0.237079493106086,0.00682170308155223,
-0.396342672917639));
#72888=CARTESIAN_POINT('Ctrl Pts',(-0.237130791666075,0.00469079598739136,
-0.396199618979042));
#72889=CARTESIAN_POINT('Ctrl Pts',(-0.237148732963697,0.00367346167808046,
-0.396131126857865));
#72890=CARTESIAN_POINT('Ctrl Pts',(-0.237170272980592,0.00175014714279538,
-0.396001259635131));
#72891=CARTESIAN_POINT('Ctrl Pts',(-0.237175227796383,0.000844199745607207,
-0.395939928391633));
#72892=CARTESIAN_POINT('Ctrl Pts',(-0.237174991963874,-6.17408820430942E-5,
-0.395878435029662));
#72893=CARTESIAN_POINT('Ctrl Pts',(-0.236793760552407,-4.73610052024943E-5,
-0.395658945585743));
#72894=CARTESIAN_POINT('Ctrl Pts',(-0.236858273123243,-0.036785166275623,
-0.393202937948888));
#72895=CARTESIAN_POINT('Ctrl Pts',(-0.211519713818698,-0.152637591068471,
-0.385452286954036));
#72896=CARTESIAN_POINT('Ctrl Pts',(-0.0307313623949624,-0.278681719209718,
-0.372406992601189));
#72897=CARTESIAN_POINT('Ctrl Pts',(0.217548020283183,-0.176863722360531,
-0.3565230625272));
#72898=CARTESIAN_POINT('Ctrl Pts',(0.266540396953676,0.086972027342936,
-0.340639132453212));
#72899=CARTESIAN_POINT('Ctrl Pts',(0.108036699394564,0.236534038370805,
-0.327739595357166));
#72900=CARTESIAN_POINT('Ctrl Pts',(-0.00788774517042406,0.239305024134992,
-0.320134701619114));
#72901=CARTESIAN_POINT('Ctrl Pts',(-0.0418736008932845,0.233079825957759,
-0.317824451239062));
#72902=CARTESIAN_POINT('Origin',(0.,0.,-2.1456589891905));
#72903=CARTESIAN_POINT('',(-0.0419392735105505,0.233437524752143,-0.198319131484844));
#72904=CARTESIAN_POINT('',(-0.0419392741328085,0.233437524640348,-0.217838756538471));
#72905=CARTESIAN_POINT('',(-0.0419392741328076,0.233437524640348,-2.1456589891905));
#72906=CARTESIAN_POINT('',(-0.237378208863769,0.000179012329966397,-0.275941010809497));
#72907=CARTESIAN_POINT('Ctrl Pts',(-0.0419392735105505,0.233437524752143,
-0.198319131484844));
#72908=CARTESIAN_POINT('Ctrl Pts',(-0.0408906519443126,0.233625919598782,
-0.198393501506002));
#72909=CARTESIAN_POINT('Ctrl Pts',(-0.0398406677809363,0.233807265436557,
-0.198467570847434));
#72910=CARTESIAN_POINT('Ctrl Pts',(-0.0374695049912287,0.234200356104447,
-0.198633892873104));
#72911=CARTESIAN_POINT('Ctrl Pts',(-0.0361477522691964,0.234408000749219,
-0.198725944022587));
#72912=CARTESIAN_POINT('Ctrl Pts',(-0.0340003552892332,0.234726756608232,
-0.198874348178815));
#72913=CARTESIAN_POINT('Ctrl Pts',(-0.0331757802923443,0.234844719086903,
-0.198931059852335));
#72914=CARTESIAN_POINT('Ctrl Pts',(-0.0317010447894705,0.235047770219734,
-0.199031978163518));
#72915=CARTESIAN_POINT('Ctrl Pts',(-0.0310511370933753,0.235134509259918,
-0.19907627447507));
#72916=CARTESIAN_POINT('Ctrl Pts',(-0.0296223739676866,0.235319169930043,
-0.199173264260355));
#72917=CARTESIAN_POINT('Ctrl Pts',(-0.0288433872861542,0.2354159209371,
-0.199225892132143));
#72918=CARTESIAN_POINT('Ctrl Pts',(-0.0265902388878308,0.235684412714702,
-0.199377421091112));
#72919=CARTESIAN_POINT('Ctrl Pts',(-0.0251148948729674,0.235846190417251,
-0.199475785416768));
#72920=CARTESIAN_POINT('Ctrl Pts',(-0.0123063785541186,0.237129140955931,
-0.200323103571914));
#72921=CARTESIAN_POINT('Ctrl Pts',(-0.000905972739818323,0.237446684457663,
-0.201032502145055));
#72922=CARTESIAN_POINT('Ctrl Pts',(0.0295443988519499,0.236100574073751,
-0.202909331837398));
#72923=CARTESIAN_POINT('Ctrl Pts',(0.048440995153022,0.232958724438614,
-0.204060836371404));
#72924=CARTESIAN_POINT('Ctrl Pts',(0.0703384475933215,0.226535688858469,
-0.20552794567744));
#72925=CARTESIAN_POINT('Ctrl Pts',(0.0738950040511176,0.225400624303204,
-0.205770343728593));
#72926=CARTESIAN_POINT('Ctrl Pts',(0.0788299145653848,0.22369631253669,
-0.206113198361948));
#72927=CARTESIAN_POINT('Ctrl Pts',(0.0802320547282062,0.223197251099559,
-0.206211357300669));
#72928=CARTESIAN_POINT('Ctrl Pts',(0.0826593353134839,0.222307485849543,
-0.20638262590514));
#72929=CARTESIAN_POINT('Ctrl Pts',(0.0836866449615448,0.221922800462884,
-0.206455534206672));
#72930=CARTESIAN_POINT('Ctrl Pts',(0.0858270451439506,0.22110433291032,
-0.206608340352562));
#72931=CARTESIAN_POINT('Ctrl Pts',(0.0869395982322922,0.220669240898619,
-0.2066882803394));
#72932=CARTESIAN_POINT('Ctrl Pts',(0.089578173805124,0.219614307988721,
-0.206879117937247));
#72933=CARTESIAN_POINT('Ctrl Pts',(0.0911011023744059,0.218986945736783,
-0.206990266462376));
#72934=CARTESIAN_POINT('Ctrl Pts',(0.0962753840534234,0.216792112460512,
-0.207371407883418));
#72935=CARTESIAN_POINT('Ctrl Pts',(0.0998936502034588,0.215148843663351,
-0.207643949904716));
#72936=CARTESIAN_POINT('Ctrl Pts',(0.108586211261025,0.210934490776281,
-0.208313891516673));
#72937=CARTESIAN_POINT('Ctrl Pts',(0.113612396482174,0.208270351323096,
-0.208714248660186));
#72938=CARTESIAN_POINT('Ctrl Pts',(0.137763556271179,0.194334484591581,
-0.210701628754575));
#72939=CARTESIAN_POINT('Ctrl Pts',(0.155334491883245,0.18059829748691,-0.21236254026382));
#72940=CARTESIAN_POINT('Ctrl Pts',(0.172900510626221,0.16237946676154,-0.21414609014474));
#72941=CARTESIAN_POINT('Ctrl Pts',(0.175017704239143,0.16009523201039,-0.214363227042695));
#72942=CARTESIAN_POINT('Ctrl Pts',(0.177811975682375,0.156958790154907,
-0.214652019838792));
#72943=CARTESIAN_POINT('Ctrl Pts',(0.178528972667212,0.156142776125272,
-0.214726326617835));
#72944=CARTESIAN_POINT('Ctrl Pts',(0.179652342302017,0.154846415190829,
-0.214843033014999));
#72945=CARTESIAN_POINT('Ctrl Pts',(0.180062442168332,0.154369340660612,
-0.214885699062894));
#72946=CARTESIAN_POINT('Ctrl Pts',(0.180906737906747,0.153379218042015,
-0.214973654470858));
#72947=CARTESIAN_POINT('Ctrl Pts',(0.181340656304526,0.152865950199629,
-0.215018921401336));
#72948=CARTESIAN_POINT('Ctrl Pts',(0.182387336131514,0.151617138601297,
-0.215128283732326));
#72949=CARTESIAN_POINT('Ctrl Pts',(0.182997846070875,0.150879705431736,
-0.215192217481971));
#72950=CARTESIAN_POINT('Ctrl Pts',(0.185148164527114,0.148250089331276,
-0.215418003435874));
#72951=CARTESIAN_POINT('Ctrl Pts',(0.186663288011938,0.146337793715882,
-0.215578200461039));
#72952=CARTESIAN_POINT('Ctrl Pts',(0.190375847449172,0.14150052366493,-0.215974530621141));
#72953=CARTESIAN_POINT('Ctrl Pts',(0.192535681095711,0.138547378018361,
-0.216208584079583));
#72954=CARTESIAN_POINT('Ctrl Pts',(0.208412292795654,0.115750507007908,
-0.217966155721346));
#72955=CARTESIAN_POINT('Ctrl Pts',(0.219098122065027,0.093968359373036,
-0.219383456521826));
#72956=CARTESIAN_POINT('Ctrl Pts',(0.227712964072919,0.0664877947031829,
-0.221222284110396));
#72957=CARTESIAN_POINT('Ctrl Pts',(0.228978734388096,0.0619883484522639,
-0.22152425417164));
#72958=CARTESIAN_POINT('Ctrl Pts',(0.230547735911851,0.0557043685174594,
-0.22194871340123));
#72959=CARTESIAN_POINT('Ctrl Pts',(0.230964763746884,0.0539491688019627,
-0.222067557427068));
#72960=CARTESIAN_POINT('Ctrl Pts',(0.231604332458714,0.0511138870388545,
-0.222260070633318));
#72961=CARTESIAN_POINT('Ctrl Pts',(0.231839439966796,0.0500366892163563,
-0.222333335500144));
#72962=CARTESIAN_POINT('Ctrl Pts',(0.232312822599627,0.0477927922263265,
-0.222486229520478));
#72963=CARTESIAN_POINT('Ctrl Pts',(0.232549838588974,0.0466258620923692,
-0.222565896559128));
#72964=CARTESIAN_POINT('Ctrl Pts',(0.233089278674585,0.0438634884240857,
-0.222754875469015));
#72965=CARTESIAN_POINT('Ctrl Pts',(0.233384121295515,0.0422666434468315,
-0.222864425064524));
#72966=CARTESIAN_POINT('Ctrl Pts',(0.23431914321321,0.0368942293103895,
-0.223234090724907));
#72967=CARTESIAN_POINT('Ctrl Pts',(0.234884246888271,0.033106383409515,
-0.223496551858554));
#72968=CARTESIAN_POINT('Ctrl Pts',(0.237086903605599,0.0154172038502997,
-0.224731413607685));
#72969=CARTESIAN_POINT('Ctrl Pts',(0.237583260247537,0.00140402554505526,
-0.225738242708841));
#72970=CARTESIAN_POINT('Ctrl Pts',(0.236011994139174,-0.0282037735747135,
-0.227899908143103));
#72971=CARTESIAN_POINT('Ctrl Pts',(0.233636114644562,-0.0437190768782639,
-0.229053052127985));
#72972=CARTESIAN_POINT('Ctrl Pts',(0.22925320235401,-0.0608187706105084,
-0.230282619571909));
#72973=CARTESIAN_POINT('Ctrl Pts',(0.228733960281828,-0.062743363942219,
-0.230420356199139));
#72974=CARTESIAN_POINT('Ctrl Pts',(0.227952183963314,-0.0655022635516871,
-0.230616638709787));
#72975=CARTESIAN_POINT('Ctrl Pts',(0.22770922049643,-0.0663419600718826,
-0.230676223086176));
#72976=CARTESIAN_POINT('Ctrl Pts',(0.227274304100026,-0.0678145163145308,
-0.230780417146112));
#72977=CARTESIAN_POINT('Ctrl Pts',(0.22708433872812,-0.0684479442741014,
-0.230825138860422));
#72978=CARTESIAN_POINT('Ctrl Pts',(0.22667392167327,-0.0697959383767032,
-0.230920095263616));
#72979=CARTESIAN_POINT('Ctrl Pts',(0.22645273827191,-0.0705102627194792,
-0.230970287213825));
#72980=CARTESIAN_POINT('Ctrl Pts',(0.225834787739539,-0.0724730662974802,
-0.231107884305723));
#72981=CARTESIAN_POINT('Ctrl Pts',(0.225431042509389,-0.0737193458962792,
-0.23119489495115));
#72982=CARTESIAN_POINT('Ctrl Pts',(0.223082868363784,-0.0807679476473073,
-0.231685317642865));
#72983=CARTESIAN_POINT('Ctrl Pts',(0.220924596420078,-0.0864971953561818,
-0.232077461834929));
#72984=CARTESIAN_POINT('Ctrl Pts',(0.212040151735574,-0.107570886020958,
-0.233517943615066));
#72985=CARTESIAN_POINT('Ctrl Pts',(0.203916569277001,-0.122272738137984,
-0.234522017734836));
#72986=CARTESIAN_POINT('Ctrl Pts',(0.188434147729298,-0.144393928146496,
-0.23619724329017));
#72987=CARTESIAN_POINT('Ctrl Pts',(0.18201955647348,-0.152400382984631,
-0.236843800015503));
#72988=CARTESIAN_POINT('Ctrl Pts',(0.173559932183318,-0.161660748833739,
-0.237660872086531));
#72989=CARTESIAN_POINT('Ctrl Pts',(0.171987549801099,-0.163332574466902,
-0.237811353683865));
#72990=CARTESIAN_POINT('Ctrl Pts',(0.169456642744818,-0.165946472877133,
-0.238051571146007));
#72991=CARTESIAN_POINT('Ctrl Pts',(0.168513919737545,-0.166903697860553,
-0.238140622580898));
#72992=CARTESIAN_POINT('Ctrl Pts',(0.166737020919909,-0.168677529749143,
-0.238307715990569));
#72993=CARTESIAN_POINT('Ctrl Pts',(0.165904846725866,-0.169496091212868,
-0.238385667980301));
#72994=CARTESIAN_POINT('Ctrl Pts',(0.164031656499945,-0.171311628022471,
-0.238560485292351));
#72995=CARTESIAN_POINT('Ctrl Pts',(0.162987533467228,-0.172305316239645,
-0.238657489243466));
#72996=CARTESIAN_POINT('Ctrl Pts',(0.159868385752157,-0.175220078545677,
-0.238946027794434));
#72997=CARTESIAN_POINT('Ctrl Pts',(0.157768053294167,-0.177113570464016,
-0.239138719367062));
#72998=CARTESIAN_POINT('Ctrl Pts',(0.147992014620262,-0.185614978290297,
-0.240028755909638));
#72999=CARTESIAN_POINT('Ctrl Pts',(0.1399327717453,-0.191763726430454,-0.240744257494194));
#73000=CARTESIAN_POINT('Ctrl Pts',(0.120110858059246,-0.204970391008402,
-0.242459265759643));
#73001=CARTESIAN_POINT('Ctrl Pts',(0.108079532206323,-0.211561490916474,
-0.243467770606852));
#73002=CARTESIAN_POINT('Ctrl Pts',(0.0880773396988655,-0.220365566623388,
-0.24505117752501));
#73003=CARTESIAN_POINT('Ctrl Pts',(0.0804412308386572,-0.223266295351193,
-0.245635194754938));
#73004=CARTESIAN_POINT('Ctrl Pts',(0.0714131627912768,-0.226172244112975,
-0.246291307043648));
#73005=CARTESIAN_POINT('Ctrl Pts',(0.0701529690250268,-0.2265662926427,
-0.246382126756864));
#73006=CARTESIAN_POINT('Ctrl Pts',(0.0680974913850215,-0.227190222925519,
-0.246528947435672));
#73007=CARTESIAN_POINT('Ctrl Pts',(0.0673041993674203,-0.227426494775398,
-0.246585294980196));
#73008=CARTESIAN_POINT('Ctrl Pts',(0.0658805072608992,-0.227842421469994,
-0.246685833461541));
#73009=CARTESIAN_POINT('Ctrl Pts',(0.0652505854859661,-0.228023620233389,
-0.246730111046778));
#73010=CARTESIAN_POINT('Ctrl Pts',(0.0638603168994318,-0.228417301824784,
-0.246827379129658));
#73011=CARTESIAN_POINT('Ctrl Pts',(0.063099655717341,-0.228628601319358,
-0.246880301429568));
#73012=CARTESIAN_POINT('Ctrl Pts',(0.0608854961345036,-0.229231767276363,
-0.247033527987953));
#73013=CARTESIAN_POINT('Ctrl Pts',(0.0594292719137986,-0.229613607387583,
-0.247133276936913));
#73014=CARTESIAN_POINT('Ctrl Pts',(0.0446346667033431,-0.233342755548294,
-0.24813723621359));
#73015=CARTESIAN_POINT('Ctrl Pts',(0.0310306665192168,-0.235538335204974,
-0.248983660376269));
#73016=CARTESIAN_POINT('Ctrl Pts',(-0.000352386463949084,-0.237835097405011,
-0.250913660966725));
#73017=CARTESIAN_POINT('Ctrl Pts',(-0.0181031180450091,-0.237145208320164,
-0.251992654571631));
#73018=CARTESIAN_POINT('Ctrl Pts',(-0.0386961959379133,-0.234017784850299,
-0.253339363571248));
#73019=CARTESIAN_POINT('Ctrl Pts',(-0.0417718169183226,-0.233488400218571,
-0.253542869799111));
#73020=CARTESIAN_POINT('Ctrl Pts',(-0.0463073460652319,-0.232615251997926,
-0.253846918526893));
#73021=CARTESIAN_POINT('Ctrl Pts',(-0.0477759604003386,-0.23231806472192,
-0.253945985761868));
#73022=CARTESIAN_POINT('Ctrl Pts',(-0.0503885426558618,-0.231763564979018,
-0.254123365508268));
#73023=CARTESIAN_POINT('Ctrl Pts',(-0.0515336141072254,-0.231511645096038,
-0.254201503408333));
#73024=CARTESIAN_POINT('Ctrl Pts',(-0.0539505652592379,-0.230961087467525,
-0.254367288842436));
#73025=CARTESIAN_POINT('Ctrl Pts',(-0.0552219354157915,-0.230660410877781,
-0.254454999528943));
#73026=CARTESIAN_POINT('Ctrl Pts',(-0.0586126931778994,-0.229828863144447,
-0.254690306866756));
#73027=CARTESIAN_POINT('Ctrl Pts',(-0.0607272951177369,-0.229279194882732,
-0.254838503549516));
#73028=CARTESIAN_POINT('Ctrl Pts',(-0.071629987061836,-0.226283751568062,
-0.25561034665026));
#73029=CARTESIAN_POINT('Ctrl Pts',(-0.0802781627260963,-0.223361971272003,
-0.256249242590259));
#73030=CARTESIAN_POINT('Ctrl Pts',(-0.09877060054596,-0.215901452667303,
-0.257673979071009));
#73031=CARTESIAN_POINT('Ctrl Pts',(-0.108515986908028,-0.211171300074533,
-0.258463592668211));
#73032=CARTESIAN_POINT('Ctrl Pts',(-0.128441729312765,-0.199755361036593,
-0.260140711265932));
#73033=CARTESIAN_POINT('Ctrl Pts',(-0.138501535037477,-0.192916732527656,
-0.261026027896984));
#73034=CARTESIAN_POINT('Ctrl Pts',(-0.149613458168704,-0.184043714414448,
-0.262017946315261));
#73035=CARTESIAN_POINT('Ctrl Pts',(-0.15121599525498,-0.182729305778164,
-0.262161340208199));
#73036=CARTESIAN_POINT('Ctrl Pts',(-0.153438505119097,-0.180857126524833,
-0.262360452283735));
#73037=CARTESIAN_POINT('Ctrl Pts',(-0.154073024968241,-0.18031688245355,
-0.262417326486901));
#73038=CARTESIAN_POINT('Ctrl Pts',(-0.155214106493161,-0.179334919751906,
-0.262519636310813));
#73039=CARTESIAN_POINT('Ctrl Pts',(-0.155721662199803,-0.178894371793139,
-0.262565154993845));
#73040=CARTESIAN_POINT('Ctrl Pts',(-0.156746873733782,-0.177996839768093,
-0.262657108873602));
#73041=CARTESIAN_POINT('Ctrl Pts',(-0.157264416946585,-0.177539743680831,
-0.262703535262519));
#73042=CARTESIAN_POINT('Ctrl Pts',(-0.158542445501955,-0.176401010562457,
-0.262818219573316));
#73043=CARTESIAN_POINT('Ctrl Pts',(-0.159300547407176,-0.17571670166335,
-0.262886282046332));
#73044=CARTESIAN_POINT('Ctrl Pts',(-0.162356336224479,-0.172922329931214,
-0.26316088556557));
#73045=CARTESIAN_POINT('Ctrl Pts',(-0.164616828546704,-0.170771818953241,
-0.263364610678865));
#73046=CARTESIAN_POINT('Ctrl Pts',(-0.1705318051301,-0.164917994784074,
-0.263901461125042));
#73047=CARTESIAN_POINT('Ctrl Pts',(-0.174108111644666,-0.16113787333786,
-0.264230066746408));
#73048=CARTESIAN_POINT('Ctrl Pts',(-0.185178561386462,-0.148637214531152,
-0.26527232113807));
#73049=CARTESIAN_POINT('Ctrl Pts',(-0.192164247961001,-0.139488506833902,
-0.265970144835793));
#73050=CARTESIAN_POINT('Ctrl Pts',(-0.205900771978131,-0.118497051428662,
-0.26751258562063));
#73051=CARTESIAN_POINT('Ctrl Pts',(-0.212350238620743,-0.10650813398858,
-0.268358706109745));
#73052=CARTESIAN_POINT('Ctrl Pts',(-0.218688355073152,-0.0918321107238223,
-0.26939897385841));
#73053=CARTESIAN_POINT('Ctrl Pts',(-0.219605797813507,-0.0896159923442804,
-0.269556109723826));
#73054=CARTESIAN_POINT('Ctrl Pts',(-0.220993037739358,-0.0861157709838005,
-0.269804568529628));
#73055=CARTESIAN_POINT('Ctrl Pts',(-0.221485625389237,-0.0848408295278547,
-0.269895124200468));
#73056=CARTESIAN_POINT('Ctrl Pts',(-0.222373976181857,-0.0824810804611815,
-0.270062867421355));
#73057=CARTESIAN_POINT('Ctrl Pts',(-0.222772891684219,-0.0813974972983083,
-0.270139946763227));
#73058=CARTESIAN_POINT('Ctrl Pts',(-0.223640514567448,-0.0789865954731762,
-0.270311581284186));
#73059=CARTESIAN_POINT('Ctrl Pts',(-0.224105346713349,-0.0776579387204261,
-0.270406261968071));
#73060=CARTESIAN_POINT('Ctrl Pts',(-0.225414692289538,-0.0738056821353131,
-0.270681084056492));
#73061=CARTESIAN_POINT('Ctrl Pts',(-0.226228571654414,-0.0712719760977893,
-0.270862222809807));
#73062=CARTESIAN_POINT('Ctrl Pts',(-0.227974805574555,-0.065504158222808,
-0.271275591665741));
#73063=CARTESIAN_POINT('Ctrl Pts',(-0.228881277717332,-0.062262873832811,
-0.271508607248377));
#73064=CARTESIAN_POINT('Ctrl Pts',(-0.234684897256532,-0.039667644587641,
-0.273138252610976));
#73065=CARTESIAN_POINT('Ctrl Pts',(-0.237189270172021,-0.0197850128759254,
-0.274608699299126));
#73066=CARTESIAN_POINT('Ctrl Pts',(-0.23717493883632,0.000170331993290248,
-0.27605765282612));
#73067=CARTESIAN_POINT('Ctrl Pts',(-0.0419325474085123,0.233395695413122,
-0.298126337027087));
#73068=CARTESIAN_POINT('Ctrl Pts',(-0.061445870050903,0.230090132428982,
-0.296798518412659));
#73069=CARTESIAN_POINT('Ctrl Pts',(-0.156420177455278,0.201614181129484,
-0.290176056440238));
#73070=CARTESIAN_POINT('Ctrl Pts',(-0.23149538472674,0.101752851827335,
-0.282780947701042));
#73071=CARTESIAN_POINT('Ctrl Pts',(-0.23747464009092,0.0116642938095829,
-0.276713657576272));
#73072=CARTESIAN_POINT('Ctrl Pts',(-0.237378208863769,0.000179012329966397,
-0.275941010809497));
#73073=CARTESIAN_POINT('',(-0.237174920140862,-0.000194630870780877,-0.2956589891905));
#73074=CARTESIAN_POINT('Ctrl Pts',(-0.0418736008932845,0.233079825957759,
-0.317824451239062));
#73075=CARTESIAN_POINT('Ctrl Pts',(-0.0857766990355478,0.22503808386485,
-0.314840058261121));
#73076=CARTESIAN_POINT('Ctrl Pts',(-0.189385050560669,0.175933016957098,
-0.307451603093063));
#73077=CARTESIAN_POINT('Ctrl Pts',(-0.236747464188876,0.0653079928409343,
-0.300063147925004));
#73078=CARTESIAN_POINT('Ctrl Pts',(-0.237328574752462,-0.000193321075562004,
-0.295659085734888));
#73079=CARTESIAN_POINT('Ctrl Pts',(-0.237174920140862,-0.000194630870780877,
-0.2956589891905));
#73080=CARTESIAN_POINT('Ctrl Pts',(-0.237164058071819,-0.013431022135193,
-0.294768440204083));
#73081=CARTESIAN_POINT('Ctrl Pts',(-0.236044766251475,-0.0266231619079329,
-0.293877891217663));
#73082=CARTESIAN_POINT('Ctrl Pts',(-0.233841221537961,-0.0396265534034244,
-0.292987342231242));
#73083=CARTESIAN_POINT('Ctrl Pts',(-0.231495933747312,-0.0534663884312158,
-0.292039508655633));
#73084=CARTESIAN_POINT('Ctrl Pts',(-0.227909804592804,-0.0671440084078081,
-0.291091675080023));
#73085=CARTESIAN_POINT('Ctrl Pts',(-0.223123839459559,-0.0804222163946304,
-0.290143841504413));
#73086=CARTESIAN_POINT('Ctrl Pts',(-0.218347568795678,-0.0936735279923352,
-0.289197927864136));
#73087=CARTESIAN_POINT('Ctrl Pts',(-0.212376499564324,-0.106526232553001,
-0.288252014223859));
#73088=CARTESIAN_POINT('Ctrl Pts',(-0.20530180552342,-0.118756680965005,
-0.287306100583582));
#73089=CARTESIAN_POINT('Ctrl Pts',(-0.198228244350353,-0.130985170920353,
-0.286360338412066));
#73090=CARTESIAN_POINT('Ctrl Pts',(-0.19005178309994,-0.142590856550964,
-0.28541457624055));
#73091=CARTESIAN_POINT('Ctrl Pts',(-0.180909866664417,-0.153374055069503,
-0.284468814069034));
#73092=CARTESIAN_POINT('Ctrl Pts',(-0.171769479814827,-0.164155449389886,
-0.283523210138355));
#73093=CARTESIAN_POINT('Ctrl Pts',(-0.161664512499544,-0.174114004722382,
-0.282577606207676));
#73094=CARTESIAN_POINT('Ctrl Pts',(-0.15077169015199,-0.183084346883376,
-0.281632002276998));
#73095=CARTESIAN_POINT('Ctrl Pts',(-0.139853365450954,-0.192075690473508,
-0.280684184491643));
#73096=CARTESIAN_POINT('Ctrl Pts',(-0.128144177315514,-0.200073704553567,
-0.279736366706287));
#73097=CARTESIAN_POINT('Ctrl Pts',(-0.115852324306153,-0.206954631689803,
-0.278788548920932));
#73098=CARTESIAN_POINT('Ctrl Pts',(-0.108567712671679,-0.211032526359908,
-0.278226836666376));
#73099=CARTESIAN_POINT('Ctrl Pts',(-0.101078986156344,-0.214718936239686,
-0.27766512441182));
#73100=CARTESIAN_POINT('Ctrl Pts',(-0.0934328807077565,-0.217996049110185,
-0.277103412157264));
#73101=CARTESIAN_POINT('Ctrl Pts',(-0.0805308487538358,-0.223525846633392,
-0.276155579367627));
#73102=CARTESIAN_POINT('Ctrl Pts',(-0.0670926434824372,-0.227924930145413,
-0.275207746577991));
#73103=CARTESIAN_POINT('Ctrl Pts',(-0.0533398279857906,-0.231099206782382,
-0.274259913788354));
#73104=CARTESIAN_POINT('Ctrl Pts',(-0.0396148702701166,-0.234267053586615,
-0.273314000934184));
#73105=CARTESIAN_POINT('Ctrl Pts',(-0.0255773559771039,-0.236214763200705,
-0.272368088080015));
#73106=CARTESIAN_POINT('Ctrl Pts',(-0.0114646524321514,-0.23689774665372,
-0.271422175225845));
#73107=CARTESIAN_POINT('Ctrl Pts',(0.00264579141979539,-0.237580620749025,
-0.270476413829025));
#73108=CARTESIAN_POINT('Ctrl Pts',(0.0168305710547536,-0.236999080620268,
-0.269530652432204));
#73109=CARTESIAN_POINT('Ctrl Pts',(0.0308473827951734,-0.235160412484091,
-0.268584891035384));
#73110=CARTESIAN_POINT('Ctrl Pts',(0.0448618493803064,-0.233322051975811,
-0.267639287874072));
#73111=CARTESIAN_POINT('Ctrl Pts',(0.0587075782799197,-0.230227107852141,
-0.26669368471276));
#73112=CARTESIAN_POINT('Ctrl Pts',(0.0721498098128534,-0.225934471847412,
-0.265748081551449));
#73113=CARTESIAN_POINT('Ctrl Pts',(0.0856235127516525,-0.221631785778481,
-0.264800264512121));
#73114=CARTESIAN_POINT('Ctrl Pts',(0.0986910490096823,-0.21612610661674,
-0.263852447472793));
#73115=CARTESIAN_POINT('Ctrl Pts',(0.111135576046833,-0.209525331074166,
-0.262904630433465));
#73116=CARTESIAN_POINT('Ctrl Pts',(0.118510724532073,-0.205613434736209,
-0.262342914316732));
#73117=CARTESIAN_POINT('Ctrl Pts',(0.125667491310397,-0.201317822332404,
-0.2617811982));
#73118=CARTESIAN_POINT('Ctrl Pts',(0.132565576710731,-0.196668117640738,
-0.261219482083267));
#73119=CARTESIAN_POINT('Ctrl Pts',(0.144205329226883,-0.188822257703783,
-0.260271648560825));
#73120=CARTESIAN_POINT('Ctrl Pts',(0.155185420939559,-0.179912984470352,
-0.259323815038384));
#73121=CARTESIAN_POINT('Ctrl Pts',(0.16530669567106,-0.170075503795566,
-0.258375981515942));
#73122=CARTESIAN_POINT('Ctrl Pts',(0.17540746861187,-0.160257950054399,
-0.257430067937875));
#73123=CARTESIAN_POINT('Ctrl Pts',(0.184652235968526,-0.149516445600452,
-0.256484154359809));
#73124=CARTESIAN_POINT('Ctrl Pts',(0.192874879116141,-0.138026307749407,
-0.255538240781742));
#73125=CARTESIAN_POINT('Ctrl Pts',(0.201096205468579,-0.126538009958528,
-0.254592478684703));
#73126=CARTESIAN_POINT('Ctrl Pts',(0.208295207260659,-0.114301965120842,
-0.253646716587665));
#73127=CARTESIAN_POINT('Ctrl Pts',(0.214346686308301,-0.101525753844288,
-0.252700954490626));
#73128=CARTESIAN_POINT('Ctrl Pts',(0.220397152803617,-0.0887516803232042,
-0.251755350641448));
#73129=CARTESIAN_POINT('Ctrl Pts',(0.225300136886879,-0.0754383823506948,
-0.25080974679227));
#73130=CARTESIAN_POINT('Ctrl Pts',(0.228977898146495,-0.0618150692421615,
-0.249864142943091));
#73131=CARTESIAN_POINT('Ctrl Pts',(0.232664269772247,-0.0481598612645623,
-0.248916325248373));
#73132=CARTESIAN_POINT('Ctrl Pts',(0.235119516839297,-0.0341940083580267,
-0.247968507553655));
#73133=CARTESIAN_POINT('Ctrl Pts',(0.236316793157245,-0.0201582215702607,
-0.247020689858938));
#73134=CARTESIAN_POINT('Ctrl Pts',(0.237026344389551,-0.0118400834242511,
-0.246458977242387));
#73135=CARTESIAN_POINT('Ctrl Pts',(0.237295070610515,-0.00349751050045388,
-0.245897264625838));
#73136=CARTESIAN_POINT('Ctrl Pts',(0.237126026238738,0.0048195752121259,
-0.245335552009287));
#73137=CARTESIAN_POINT('Ctrl Pts',(0.236840780463713,0.0188538405064866,
-0.244387717136319));
#73138=CARTESIAN_POINT('Ctrl Pts',(0.235304324253603,0.0329100654086107,
-0.24343988226335));
#73139=CARTESIAN_POINT('Ctrl Pts',(0.232522348153217,0.046747601374982,
-0.242492047390382));
#73140=CARTESIAN_POINT('Ctrl Pts',(0.22974600719756,0.0605571081581194,
-0.241546132442853));
#73141=CARTESIAN_POINT('Ctrl Pts',(0.225729247348527,0.0741479816775976,
-0.240600217495324));
#73142=CARTESIAN_POINT('Ctrl Pts',(0.220529374087023,0.0872855989827991,
-0.239654302547795));
#73143=CARTESIAN_POINT('Ctrl Pts',(0.215330333504744,0.100421112501918,
-0.238708539073906));
#73144=CARTESIAN_POINT('Ctrl Pts',(0.208948815794916,0.113102721053147,
-0.237762775600016));
#73145=CARTESIAN_POINT('Ctrl Pts',(0.201491418064631,0.12511270547512,-0.236817012126127));
#73146=CARTESIAN_POINT('Ctrl Pts',(0.194035268079209,0.137120680429863,
-0.235871406893967));
#73147=CARTESIAN_POINT('Ctrl Pts',(0.185504051561946,0.148456554616219,
-0.234925801661806));
#73148=CARTESIAN_POINT('Ctrl Pts',(0.176048263005386,0.158930770204472,
-0.233980196429646));
#73149=CARTESIAN_POINT('Ctrl Pts',(0.166570336790122,0.169429507767649,
-0.233032377369864));
#73150=CARTESIAN_POINT('Ctrl Pts',(0.15616411072589,0.179061968283412,-0.232084558310081));
#73151=CARTESIAN_POINT('Ctrl Pts',(0.145017328464764,0.187675131730186,
-0.231136739250299));
#73152=CARTESIAN_POINT('Ctrl Pts',(0.138411413689159,0.192779548623317,
-0.23057503347863));
#73153=CARTESIAN_POINT('Ctrl Pts',(0.131546056594898,0.197526748657646,
-0.23001332770696));
#73154=CARTESIAN_POINT('Ctrl Pts',(0.124464865211157,0.201892243419524,
-0.229451621935291));
#73155=CARTESIAN_POINT('Ctrl Pts',(0.112264984280593,0.209413367113511,
-0.228483883152223));
#73156=CARTESIAN_POINT('Ctrl Pts',(0.0993388589516617,0.215850597682492,
-0.227516144369154));
#73157=CARTESIAN_POINT('Ctrl Pts',(0.0859053425306205,0.221070696270891,
-0.226548405586086));
#73158=CARTESIAN_POINT('Ctrl Pts',(0.0727733693233782,0.226173618890218,
-0.225602389712613));
#73159=CARTESIAN_POINT('Ctrl Pts',(0.0591573674941752,0.230113191175845,
-0.22465637383914));
#73160=CARTESIAN_POINT('Ctrl Pts',(0.0452860359781853,0.232811416323132,
-0.223710357965667));
#73161=CARTESIAN_POINT('Ctrl Pts',(0.0309369233451853,0.235602578548833,
-0.222731757727801));
#73162=CARTESIAN_POINT('Ctrl Pts',(0.016315423833323,0.237064855767117,
-0.221753157489935));
#73163=CARTESIAN_POINT('Ctrl Pts',(0.00168848205185222,0.237168989653708,
-0.220774557252068));
#73164=CARTESIAN_POINT('Ctrl Pts',(-0.0129384597296185,0.237273123540299,
-0.219795957014202));
#73165=CARTESIAN_POINT('Ctrl Pts',(-0.0275698529512033,0.236019127983656,
-0.218817356776337));
#73166=CARTESIAN_POINT('Ctrl Pts',(-0.0419392741328085,0.233437524640348,
-0.217838756538471));
#73167=CARTESIAN_POINT('Origin',(0.,0.,-2.1456589891905));
#73168=CARTESIAN_POINT('',(-0.0419392282806928,0.233437532878113,-0.0979609479953583));
#73169=CARTESIAN_POINT('',(-0.0419392741328228,0.233437524640346,-0.117607182502807));
#73170=CARTESIAN_POINT('',(-0.0419392741328076,0.233437524640348,-2.1456589891905));
#73171=CARTESIAN_POINT('Ctrl Pts',(-0.0419392282806931,0.233437532878113,
-0.0979609479953583));
#73172=CARTESIAN_POINT('Ctrl Pts',(-0.0317635392632918,0.235265690241466,
-0.0986991702520308));
#73173=CARTESIAN_POINT('Ctrl Pts',(-0.0214726811650525,0.23642772405573,
-0.0994531880114252));
#73174=CARTESIAN_POINT('Ctrl Pts',(-0.00136646084210373,0.237372473734899,
-0.100924066052501));
#73175=CARTESIAN_POINT('Ctrl Pts',(0.00841873030292184,0.237227116043163,
-0.101638678885694));
#73176=CARTESIAN_POINT('Ctrl Pts',(0.0213076755559574,0.236236920560851,
-0.102560202574135));
#73177=CARTESIAN_POINT('Ctrl Pts',(0.0244429230897771,0.235933137185549,
-0.102782765074389));
#73178=CARTESIAN_POINT('Ctrl Pts',(0.0297406827468052,0.235313074254126,
-0.103155166051736));
#73179=CARTESIAN_POINT('Ctrl Pts',(0.0319065096461671,0.235029203762183,
-0.103306364786636));
#73180=CARTESIAN_POINT('Ctrl Pts',(0.0349757976741866,0.23458370635857,
-0.10351886394209));
#73181=CARTESIAN_POINT('Ctrl Pts',(0.0358826423319724,0.234446705589172,
-0.103581428036273));
#73182=CARTESIAN_POINT('Ctrl Pts',(0.0374456242908962,0.234201298140421,
-0.10368885301994));
#73183=CARTESIAN_POINT('Ctrl Pts',(0.0381021378283496,0.234095386469795,
-0.103733851438361));
#73184=CARTESIAN_POINT('Ctrl Pts',(0.0394782195698376,0.23386744842694,
-0.103827898609573));
#73185=CARTESIAN_POINT('Ctrl Pts',(0.0401976813562165,0.23374486027367,
-0.103876915329461));
#73186=CARTESIAN_POINT('Ctrl Pts',(0.0421387178844203,0.233404902524112,
-0.104008768952267));
#73187=CARTESIAN_POINT('Ctrl Pts',(0.0433591924056388,0.233181261401142,
-0.104091258861908));
#73188=CARTESIAN_POINT('Ctrl Pts',(0.0490415825753238,0.232093856033384,
-0.104473619026303));
#73189=CARTESIAN_POINT('Ctrl Pts',(0.05348016031268,0.231111474826344,-0.104767380930168));
#73190=CARTESIAN_POINT('Ctrl Pts',(0.0621535256294052,0.228928517752236,
-0.105336649232027));
#73191=CARTESIAN_POINT('Ctrl Pts',(0.0663884748542621,0.227736472978143,
-0.105612325596284));
#73192=CARTESIAN_POINT('Ctrl Pts',(0.0912801443464492,0.21997657121836,
-0.107232006774772));
#73193=CARTESIAN_POINT('Ctrl Pts',(0.110989247272626,0.210720560787885,
-0.108522448033418));
#73194=CARTESIAN_POINT('Ctrl Pts',(0.132540244981078,0.196726297267704,
-0.110171268580961));
#73195=CARTESIAN_POINT('Ctrl Pts',(0.135856563976942,0.194450876843222,
-0.110432086465231));
#73196=CARTESIAN_POINT('Ctrl Pts',(0.140447843833548,0.191125871940096,
-0.110804269739766));
#73197=CARTESIAN_POINT('Ctrl Pts',(0.141772263293761,0.190145525565056,
-0.110912974506636));
#73198=CARTESIAN_POINT('Ctrl Pts',(0.1440340085122,0.188434596153315,-0.111101002614679));
#73199=CARTESIAN_POINT('Ctrl Pts',(0.144976268251543,0.187710612888308,
-0.111180064330605));
#73200=CARTESIAN_POINT('Ctrl Pts',(0.14676948991735,0.186311238702517,-0.111331950162483));
#73201=CARTESIAN_POINT('Ctrl Pts',(0.147621331739057,0.18563701997331,-0.111404726089653));
#73202=CARTESIAN_POINT('Ctrl Pts',(0.149830301012876,0.18386383818349,-0.111595104158352));
#73203=CARTESIAN_POINT('Ctrl Pts',(0.151179955263766,0.182755713817817,
-0.111713075262875));
#73204=CARTESIAN_POINT('Ctrl Pts',(0.155838073374351,0.178844288287787,
-0.112126128294458));
#73205=CARTESIAN_POINT('Ctrl Pts',(0.159081622531094,0.175965387535873,
-0.112424298257366));
#73206=CARTESIAN_POINT('Ctrl Pts',(0.175792944629793,0.160292981960417,
-0.114018569877111));
#73207=CARTESIAN_POINT('Ctrl Pts',(0.187800063385754,0.146040767498145,
-0.115378112400515));
#73208=CARTESIAN_POINT('Ctrl Pts',(0.204197668210822,0.121166335832178,
-0.117552510211982));
#73209=CARTESIAN_POINT('Ctrl Pts',(0.209703168483444,0.111367009378906,
-0.11836556833137));
#73210=CARTESIAN_POINT('Ctrl Pts',(0.215123329420001,0.0998804605168641,
-0.119244528014781));
#73211=CARTESIAN_POINT('Ctrl Pts',(0.215739926291081,0.09854155335073,-0.119345881672176));
#73212=CARTESIAN_POINT('Ctrl Pts',(0.216663241156643,0.0964864100011733,
-0.119499682372998));
#73213=CARTESIAN_POINT('Ctrl Pts',(0.216978965820279,0.0957742962353528,
-0.119552652571218));
#73214=CARTESIAN_POINT('Ctrl Pts',(0.217553184764051,0.0944617369030223,
-0.119649677852005));
#73215=CARTESIAN_POINT('Ctrl Pts',(0.217812704576054,0.0938617796454056,
-0.119693792594117));
#73216=CARTESIAN_POINT('Ctrl Pts',(0.21839693045004,0.0924956957159582,
-0.119793718175686));
#73217=CARTESIAN_POINT('Ctrl Pts',(0.21872008856859,0.0917289260012577,
-0.119849435273378));
#73218=CARTESIAN_POINT('Ctrl Pts',(0.219550943832558,0.0897281677865304,
-0.11999389835299));
#73219=CARTESIAN_POINT('Ctrl Pts',(0.22005228305086,0.0884915473765325,
-0.120082279464231));
#73220=CARTESIAN_POINT('Ctrl Pts',(0.223871299255121,0.0788382415558933,
-0.120765655145308));
#73221=CARTESIAN_POINT('Ctrl Pts',(0.226715789494457,0.070241141679544,
-0.121335839871748));
#73222=CARTESIAN_POINT('Ctrl Pts',(0.232587774936777,0.0483709533665607,
-0.12274029999639));
#73223=CARTESIAN_POINT('Ctrl Pts',(0.234977717149941,0.0349615070469867,
-0.123561780396935));
#73224=CARTESIAN_POINT('Ctrl Pts',(0.237139121633588,0.0111280437616441,
-0.125046799678374));
#73225=CARTESIAN_POINT('Ctrl Pts',(0.237398690208547,0.000786308062397829,
-0.1256990214052));
#73226=CARTESIAN_POINT('Ctrl Pts',(0.236892216344357,-0.0117968966932127,
-0.126519987660863));
#73227=CARTESIAN_POINT('Ctrl Pts',(0.236769044922754,-0.0140537441573658,
-0.126668275838954));
#73228=CARTESIAN_POINT('Ctrl Pts',(0.236522534332127,-0.0176302863716958,
-0.126905090297152));
#73229=CARTESIAN_POINT('Ctrl Pts',(0.236420352132248,-0.0189513382505818,
-0.126992954605069));
#73230=CARTESIAN_POINT('Ctrl Pts',(0.236206847835148,-0.0214401884444225,
-0.127159263198825));
#73231=CARTESIAN_POINT('Ctrl Pts',(0.236097920001129,-0.0226081562903602,
-0.12723763008589));
#73232=CARTESIAN_POINT('Ctrl Pts',(0.235832225310229,-0.02524529875237,
-0.127415323371018));
#73233=CARTESIAN_POINT('Ctrl Pts',(0.235670386127033,-0.0267139015321142,
-0.127514806058743));
#73234=CARTESIAN_POINT('Ctrl Pts',(0.235150194295314,-0.0310609107078595,
-0.127810882168602));
#73235=CARTESIAN_POINT('Ctrl Pts',(0.234752759183562,-0.0339342719189924,
-0.128008689105845));
#73236=CARTESIAN_POINT('Ctrl Pts',(0.231275530909281,-0.0560738064319622,
-0.12954971415502));
#73237=CARTESIAN_POINT('Ctrl Pts',(0.225882086601258,-0.0748974520192039,
-0.130968446756744));
#73238=CARTESIAN_POINT('Ctrl Pts',(0.214960827071432,-0.100569957832654,
-0.1330036856912));
#73239=CARTESIAN_POINT('Ctrl Pts',(0.211266000785236,-0.108116455798295,
-0.133614122015012));
#73240=CARTESIAN_POINT('Ctrl Pts',(0.205089425930616,-0.119200361663949,
-0.134515751058621));
#73241=CARTESIAN_POINT('Ctrl Pts',(0.202898816247151,-0.122892126758162,
-0.134816909096948));
#73242=CARTESIAN_POINT('Ctrl Pts',(0.199979768200804,-0.127520447391947,
-0.135193689043195));
#73243=CARTESIAN_POINT('Ctrl Pts',(0.199343025299983,-0.128513542483922,
-0.135274486758466));
#73244=CARTESIAN_POINT('Ctrl Pts',(0.198305132959889,-0.130106014060527,
-0.135403920471898));
#73245=CARTESIAN_POINT('Ctrl Pts',(0.197908623051454,-0.130708368553989,
-0.135452848881824));
#73246=CARTESIAN_POINT('Ctrl Pts',(0.197140680941502,-0.131863474879834,
-0.135546604232513));
#73247=CARTESIAN_POINT('Ctrl Pts',(0.196769662478786,-0.132416479442879,
-0.135591455544656));
#73248=CARTESIAN_POINT('Ctrl Pts',(0.195945035774624,-0.133634469811613,
-0.135690180169615));
#73249=CARTESIAN_POINT('Ctrl Pts',(0.195490357401895,-0.134298729616357,
-0.13574398258863));
#73250=CARTESIAN_POINT('Ctrl Pts',(0.193868397689006,-0.136642631146042,
-0.13593373893578));
#73251=CARTESIAN_POINT('Ctrl Pts',(0.192682740122091,-0.138309531927601,
-0.136068521644786));
#73252=CARTESIAN_POINT('Ctrl Pts',(0.1827836108456,-0.15185217967709,-0.137164068017958));
#73253=CARTESIAN_POINT('Ctrl Pts',(0.17300149511792,-0.162909600824409,
-0.138063104962052));
#73254=CARTESIAN_POINT('Ctrl Pts',(0.153872711728283,-0.180851474159983,
-0.139670676231541));
#73255=CARTESIAN_POINT('Ctrl Pts',(0.144930104029103,-0.188093876450735,
-0.140375369078716));
#73256=CARTESIAN_POINT('Ctrl Pts',(0.132003548327169,-0.197091793980823,
-0.141370829727221));
#73257=CARTESIAN_POINT('Ctrl Pts',(0.128444046254087,-0.199429776545429,
-0.141642628895989));
#73258=CARTESIAN_POINT('Ctrl Pts',(0.122107333326926,-0.203351875156971,
-0.142124177396081));
#73259=CARTESIAN_POINT('Ctrl Pts',(0.119357391255386,-0.20497804163141,
-0.142332417952089));
#73260=CARTESIAN_POINT('Ctrl Pts',(0.115258162000108,-0.207291642524837,
-0.142642215903759));
#73261=CARTESIAN_POINT('Ctrl Pts',(0.11393371946252,-0.20802253810478,-0.142742216090707));
#73262=CARTESIAN_POINT('Ctrl Pts',(0.111568572310416,-0.20929838535573,
-0.142920673804633));
#73263=CARTESIAN_POINT('Ctrl Pts',(0.110530630974945,-0.209848373763131,
-0.142998949300023));
#73264=CARTESIAN_POINT('Ctrl Pts',(0.108335743067134,-0.210990607864978,
-0.143164412619173));
#73265=CARTESIAN_POINT('Ctrl Pts',(0.107177931467915,-0.211581097271691,
-0.143251659075141));
#73266=CARTESIAN_POINT('Ctrl Pts',(0.104090466951129,-0.213123873866501,
-0.143484250993119));
#73267=CARTESIAN_POINT('Ctrl Pts',(0.102152646038065,-0.214059448044098,
-0.143630171686381));
#73268=CARTESIAN_POINT('Ctrl Pts',(0.0933807409431472,-0.218148261529492,
-0.144290612805715));
#73269=CARTESIAN_POINT('Ctrl Pts',(0.0864123022932157,-0.221001174729244,
-0.144815208604353));
#73270=CARTESIAN_POINT('Ctrl Pts',(0.064578534578444,-0.228749412997202,
-0.146459115906403));
#73271=CARTESIAN_POINT('Ctrl Pts',(0.0493560779889504,-0.232509276452619,
-0.147608394117222));
#73272=CARTESIAN_POINT('Ctrl Pts',(0.0239346547052643,-0.236177926863205,
-0.149478070160238));
#73273=CARTESIAN_POINT('Ctrl Pts',(0.0139103833567047,-0.236979809411012,
-0.150202021012649));
#73274=CARTESIAN_POINT('Ctrl Pts',(0.0024051977859521,-0.237167294413206,
-0.150998016541098));
#73275=CARTESIAN_POINT('Ctrl Pts',(0.000945742120645826,-0.237177605090394,
-0.151098340038964));
#73276=CARTESIAN_POINT('Ctrl Pts',(-0.00129349645152199,-0.237172754510377,
-0.151251175640611));
#73277=CARTESIAN_POINT('Ctrl Pts',(-0.00207323299373263,-0.237167220256647,
-0.15130419241869));
#73278=CARTESIAN_POINT('Ctrl Pts',(-0.0035086113051823,-0.237149953059226,
-0.151401397571196));
#73279=CARTESIAN_POINT('Ctrl Pts',(-0.00416423374441061,-0.237139346727902,
-0.15144564493904));
#73280=CARTESIAN_POINT('Ctrl Pts',(-0.00565833808986251,-0.237108977521131,
-0.151546140231133));
#73281=CARTESIAN_POINT('Ctrl Pts',(-0.00649676585406703,-0.237087486170394,
-0.151602291692027));
#73282=CARTESIAN_POINT('Ctrl Pts',(-0.00869278053640779,-0.2370195378284,
-0.151748770809671));
#73283=CARTESIAN_POINT('Ctrl Pts',(-0.0100501360724432,-0.236965864044813,
-0.151838715524392));
#73284=CARTESIAN_POINT('Ctrl Pts',(-0.0230833179739347,-0.236338303478938,
-0.152697294297803));
#73285=CARTESIAN_POINT('Ctrl Pts',(-0.0347038318256782,-0.234913503793368,
-0.153424178222884));
#73286=CARTESIAN_POINT('Ctrl Pts',(-0.0602796956831921,-0.229837268003803,
-0.15502840576495));
#73287=CARTESIAN_POINT('Ctrl Pts',(-0.074101590421285,-0.225760377299027,
-0.155899790937294));
#73288=CARTESIAN_POINT('Ctrl Pts',(-0.0919352750746342,-0.218684646942566,
-0.157106642431737));
#73289=CARTESIAN_POINT('Ctrl Pts',(-0.0963465458354181,-0.216777324111726,
-0.157412086840691));
#73290=CARTESIAN_POINT('Ctrl Pts',(-0.103867642789056,-0.213250462402792,
-0.157947437397418));
#73291=CARTESIAN_POINT('Ctrl Pts',(-0.107005170831192,-0.211693500796118,
-0.158175300989801));
#73292=CARTESIAN_POINT('Ctrl Pts',(-0.111494957946378,-0.209340179707107,
-0.158508607580227));
#73293=CARTESIAN_POINT('Ctrl Pts',(-0.112875693782438,-0.208598931067458,
-0.158612119598968));
#73294=CARTESIAN_POINT('Ctrl Pts',(-0.11528358032905,-0.207275349768651,
-0.158794469453041));
#73295=CARTESIAN_POINT('Ctrl Pts',(-0.116313928072974,-0.206698922505567,
-0.15887309467931));
#73296=CARTESIAN_POINT('Ctrl Pts',(-0.118444549876502,-0.205485972561805,
-0.159036948065097));
#73297=CARTESIAN_POINT('Ctrl Pts',(-0.1195440939656,-0.204848250673099,
-0.159122217643613));
#73298=CARTESIAN_POINT('Ctrl Pts',(-0.122382674859691,-0.203171271887754,
-0.159344230093433));
#73299=CARTESIAN_POINT('Ctrl Pts',(-0.12411358575642,-0.202118535053269,
-0.159481460259121));
#73300=CARTESIAN_POINT('Ctrl Pts',(-0.131269589973405,-0.19763968279577,
-0.160056726445009));
#73301=CARTESIAN_POINT('Ctrl Pts',(-0.136567555451433,-0.194016593814558,
-0.160501955461516));
#73302=CARTESIAN_POINT('Ctrl Pts',(-0.154994307295865,-0.180286238218627,
-0.16212242874649));
#73303=CARTESIAN_POINT('Ctrl Pts',(-0.167202170236288,-0.169025639410055,
-0.163337922385332));
#73304=CARTESIAN_POINT('Ctrl Pts',(-0.185031388432316,-0.148742907379374,
-0.165305156860093));
#73305=CARTESIAN_POINT('Ctrl Pts',(-0.191402175016785,-0.140450442205517,
-0.166059085705771));
#73306=CARTESIAN_POINT('Ctrl Pts',(-0.198020970858295,-0.130544350485439,
-0.166883324480858));
#73307=CARTESIAN_POINT('Ctrl Pts',(-0.198824594959166,-0.129317102719204,
-0.166984167750053));
#73308=CARTESIAN_POINT('Ctrl Pts',(-0.200038509967097,-0.127425213109616,
-0.167137595701303));
#73309=CARTESIAN_POINT('Ctrl Pts',(-0.200456973158922,-0.126765895895795,
-0.167190691833981));
#73310=CARTESIAN_POINT('Ctrl Pts',(-0.201220830419954,-0.125549145830893,
-0.167287977667876));
#73311=CARTESIAN_POINT('Ctrl Pts',(-0.201567169900439,-0.124992346368357,
-0.167332226924011));
#73312=CARTESIAN_POINT('Ctrl Pts',(-0.202350456624617,-0.123721357341604,
-0.167432627053454));
#73313=CARTESIAN_POINT('Ctrl Pts',(-0.202785935199133,-0.123006284789944,
-0.167488682374463));
#73314=CARTESIAN_POINT('Ctrl Pts',(-0.203914684663908,-0.121130548129553,
-0.167634641480022));
#73315=CARTESIAN_POINT('Ctrl Pts',(-0.204601845898348,-0.119966216808555,
-0.16772416768257));
#73316=CARTESIAN_POINT('Ctrl Pts',(-0.210346950344549,-0.11003870169986,
-0.168478985290338));
#73317=CARTESIAN_POINT('Ctrl Pts',(-0.214849973970703,-0.100964833240656,
-0.169113162522728));
#73318=CARTESIAN_POINT('Ctrl Pts',(-0.219517946093408,-0.0898203819165326,
-0.169859698398523));
#73319=CARTESIAN_POINT('Ctrl Pts',(-0.220253428481769,-0.0880014605055449,
-0.169980543942454));
#73320=CARTESIAN_POINT('Ctrl Pts',(-0.221250697507531,-0.0854442644068944,
-0.170149299073959));
#73321=CARTESIAN_POINT('Ctrl Pts',(-0.221531518372763,-0.0847135162836387,
-0.170197393619803));
#73322=CARTESIAN_POINT('Ctrl Pts',(-0.225436883741637,-0.0743988014777939,
-0.170874601171089));
#73323=CARTESIAN_POINT('Ctrl Pts',(-0.228440214760001,-0.0645912679262485,
-0.171498899042203));
#73324=CARTESIAN_POINT('Ctrl Pts',(-0.233067808386633,-0.0450373123278173,
-0.172748038565983));
#73325=CARTESIAN_POINT('Ctrl Pts',(-0.234736445492843,-0.0353231998860428,
-0.173370695311321));
#73326=CARTESIAN_POINT('Ctrl Pts',(-0.236036555603795,-0.0233173233311289,
-0.174158148960352));
#73327=CARTESIAN_POINT('Ctrl Pts',(-0.236245343936131,-0.0210971576527419,
-0.174304481991065));
#73328=CARTESIAN_POINT('Ctrl Pts',(-0.236527566576646,-0.0175620133324477,
-0.174538772081519));
#73329=CARTESIAN_POINT('Ctrl Pts',(-0.236621410058296,-0.0162487613803373,
-0.174626088405674));
#73330=CARTESIAN_POINT('Ctrl Pts',(-0.236778066356169,-0.0137658907706906,
-0.174791732887196));
#73331=CARTESIAN_POINT('Ctrl Pts',(-0.236843158614524,-0.0125964514341567,
-0.174869987076174));
#73332=CARTESIAN_POINT('Ctrl Pts',(-0.236971023209236,-0.00994552459101086,
-0.175047931581799));
#73333=CARTESIAN_POINT('Ctrl Pts',(-0.237028568816733,-0.0084638461175782,
-0.175147782463482));
#73334=CARTESIAN_POINT('Ctrl Pts',(-0.237141608843325,-0.00462546271417778,
-0.17540751224517));
#73335=CARTESIAN_POINT('Ctrl Pts',(-0.237175866105723,-0.00226834485232048,
-0.175568045190495));
#73336=CARTESIAN_POINT('Ctrl Pts',(-0.23717374932495,0.00338407696309937,
-0.175955600589388));
#73337=CARTESIAN_POINT('Ctrl Pts',(-0.237103840333012,0.00667880153782812,
-0.176183619433192));
#73338=CARTESIAN_POINT('Ctrl Pts',(-0.236645877390351,0.0175626458177593,
-0.176944017009669));
#73339=CARTESIAN_POINT('Ctrl Pts',(-0.235961820736989,0.0251339961851816,
-0.177484688742312));
#73340=CARTESIAN_POINT('Ctrl Pts',(-0.233645105216224,0.0417981664330959,
-0.178697684000097));
#73341=CARTESIAN_POINT('Ctrl Pts',(-0.231842309578179,0.0508552074570876,
-0.179372493758461));
#73342=CARTESIAN_POINT('Ctrl Pts',(-0.228880033345431,0.0622277197680743,
-0.18023024885811));
#73343=CARTESIAN_POINT('Ctrl Pts',(-0.228204439465065,0.0646613703820853,
-0.180414394828264));
#73344=CARTESIAN_POINT('Ctrl Pts',(-0.224772007709468,0.0763012057397664,
-0.181296935440569));
#73345=CARTESIAN_POINT('Ctrl Pts',(-0.221495882486234,0.0853460401025865,
-0.181988494429987));
#73346=CARTESIAN_POINT('Ctrl Pts',(-0.217145550247915,0.0954023019437799,
-0.182746764247662));
#73347=CARTESIAN_POINT('Ctrl Pts',(-0.216601092375262,0.0966320661011829,
-0.182839298312313));
#73348=CARTESIAN_POINT('Ctrl Pts',(-0.215701529202356,0.098618095325905,
-0.18298834609361));
#73349=CARTESIAN_POINT('Ctrl Pts',(-0.215352845971618,0.0993772117321909,
-0.183045222763101));
#73350=CARTESIAN_POINT('Ctrl Pts',(-0.214723124938131,0.100729294572572,
-0.183146339223));
#73351=CARTESIAN_POINT('Ctrl Pts',(-0.214443630171735,0.101322952392927,
-0.183190669843936));
#73352=CARTESIAN_POINT('Ctrl Pts',(-0.213824830519985,0.102623276746964,
-0.183287622092679));
#73353=CARTESIAN_POINT('Ctrl Pts',(-0.213484484020065,0.103329425646501,
-0.183340178991159));
#73354=CARTESIAN_POINT('Ctrl Pts',(-0.212492233791753,0.105362309849602,
-0.18349124804005));
#73355=CARTESIAN_POINT('Ctrl Pts',(-0.211831405379961,0.106684683662526,
-0.18358922882327));
#73356=CARTESIAN_POINT('Ctrl Pts',(-0.206151449967395,0.117789869820153,
-0.184410350524637));
#73357=CARTESIAN_POINT('Ctrl Pts',(-0.200469284858491,0.127220304297074,
-0.185096652792071));
#73358=CARTESIAN_POINT('Ctrl Pts',(-0.183813048715642,0.150959598894989,
-0.186884163567184));
#73359=CARTESIAN_POINT('Ctrl Pts',(-0.171830478782721,0.164469721334244,
-0.187969515819806));
#73360=CARTESIAN_POINT('Ctrl Pts',(-0.154851828792529,0.179711103260258,
-0.189424900495335));
#73361=CARTESIAN_POINT('Ctrl Pts',(-0.15117145590068,0.18281782001336,-0.189735834443007));
#73362=CARTESIAN_POINT('Ctrl Pts',(-0.145969417315702,0.18694448614643,
-0.19017086984896));
#73363=CARTESIAN_POINT('Ctrl Pts',(-0.14452655033769,0.188062190857791,
-0.190291076608971));
#73364=CARTESIAN_POINT('Ctrl Pts',(-0.142188513756844,0.189830533241875,
-0.190485212410213));
#73365=CARTESIAN_POINT('Ctrl Pts',(-0.141301420632521,0.190491766887114,
-0.190558723771199));
#73366=CARTESIAN_POINT('Ctrl Pts',(-0.139452258873633,0.191850096648846,
-0.190711675294912));
#73367=CARTESIAN_POINT('Ctrl Pts',(-0.138489515924331,0.192546217774897,
-0.190791150379207));
#73368=CARTESIAN_POINT('Ctrl Pts',(-0.136211587036532,0.194167374996316,
-0.190978850828351));
#73369=CARTESIAN_POINT('Ctrl Pts',(-0.134892157681595,0.195086318151782,
-0.191087305076769));
#73370=CARTESIAN_POINT('Ctrl Pts',(-0.130477949500889,0.198094491417262,
-0.191449333368615));
#73371=CARTESIAN_POINT('Ctrl Pts',(-0.127343321667718,0.200123957843785,
-0.191705122435571));
#73372=CARTESIAN_POINT('Ctrl Pts',(-0.115042864309425,0.207681676565704,
-0.192704482667673));
#73373=CARTESIAN_POINT('Ctrl Pts',(-0.105555866580389,0.212660396015786,
-0.193466874231611));
#73374=CARTESIAN_POINT('Ctrl Pts',(-0.086051537853299,0.221268782257148,
-0.195010864836056));
#73375=CARTESIAN_POINT('Ctrl Pts',(-0.0760598859657186,0.224899145862902,
-0.195790513614848));
#73376=CARTESIAN_POINT('Ctrl Pts',(-0.0579878194108664,0.230122849107711,
-0.197157622533095));
#73377=CARTESIAN_POINT('Ctrl Pts',(-0.0500038365085975,0.231988649239616,
-0.19774717899015));
#73378=CARTESIAN_POINT('Ctrl Pts',(-0.0419392735105505,0.233437524752143,
-0.198319131484844));
#73379=CARTESIAN_POINT('',(-0.237174944070688,0.000162880526358662,-0.1956589891905));
#73380=CARTESIAN_POINT('Ctrl Pts',(-0.0419392741328085,0.233437524640348,
-0.217838756538471));
#73381=CARTESIAN_POINT('Ctrl Pts',(-0.0558566731803301,0.230937131377658,
-0.216890940349756));
#73382=CARTESIAN_POINT('Ctrl Pts',(-0.0695275470206164,0.227191865779455,
-0.215943124161042));
#73383=CARTESIAN_POINT('Ctrl Pts',(-0.082723246704858,0.222281004765606,
-0.214995307972327));
#73384=CARTESIAN_POINT('Ctrl Pts',(-0.0893484389765401,0.219815398604902,
-0.214519435935322));
#73385=CARTESIAN_POINT('Ctrl Pts',(-0.0958541374193577,0.21705674966462,
-0.214043563898317));
#73386=CARTESIAN_POINT('Ctrl Pts',(-0.102213610392895,0.214019528257235,
-0.213567691861312));
#73387=CARTESIAN_POINT('Ctrl Pts',(-0.114880326844257,0.207970029733153,
-0.212619856060302));
#73388=CARTESIAN_POINT('Ctrl Pts',(-0.12705087675837,0.200771692096791,
-0.211672020259292));
#73389=CARTESIAN_POINT('Ctrl Pts',(-0.138508390745754,0.192528975268715,
-0.210724184458281));
#73390=CARTESIAN_POINT('Ctrl Pts',(-0.149942695774464,0.184302955332691,
-0.209778268644623));
#73391=CARTESIAN_POINT('Ctrl Pts',(-0.160666120031039,0.175037180079499,
-0.208832352830964));
#73392=CARTESIAN_POINT('Ctrl Pts',(-0.170488576055934,0.16488064185774,
-0.207886437017305));
#73393=CARTESIAN_POINT('Ctrl Pts',(-0.180309458097597,0.154725731153661,
-0.206940672780363));
#73394=CARTESIAN_POINT('Ctrl Pts',(-0.189229043617759,0.143680904924962,
-0.20599490854342));
#73395=CARTESIAN_POINT('Ctrl Pts',(-0.197092978050972,0.131933083902405,
-0.205049144306477));
#73396=CARTESIAN_POINT('Ctrl Pts',(-0.204955596245962,0.120187229189613,
-0.204103538368291));
#73397=CARTESIAN_POINT('Ctrl Pts',(-0.211762464883004,0.10773931743606,
-0.203157932430105));
#73398=CARTESIAN_POINT('Ctrl Pts',(-0.217402991910532,0.0948046398302793,
-0.202212326491919));
#73399=CARTESIAN_POINT('Ctrl Pts',(-0.223056723787191,0.081839681283462,
-0.201264506827304));
#73400=CARTESIAN_POINT('Ctrl Pts',(-0.227538369305371,0.0683864664481,-0.200316687162689));
#73401=CARTESIAN_POINT('Ctrl Pts',(-0.230785986797566,0.0546791452280835,
-0.199368867498074));
#73402=CARTESIAN_POINT('Ctrl Pts',(-0.232710607055604,0.0465558400152984,
-0.198807165594489));
#73403=CARTESIAN_POINT('Ctrl Pts',(-0.234202800191289,0.0383435642722978,
-0.198245463690903));
#73404=CARTESIAN_POINT('Ctrl Pts',(-0.235258248560059,0.0300921436500207,
-0.197683761787317));
#73405=CARTESIAN_POINT('Ctrl Pts',(-0.236526443736657,0.0201774835464205,
-0.197008837588379));
#73406=CARTESIAN_POINT('Ctrl Pts',(-0.237168064099412,0.0101810014103574,
-0.19633391338944));
#73407=CARTESIAN_POINT('Ctrl Pts',(-0.237174944070688,0.000162880526358662,
-0.1956589891905));
#73408=CARTESIAN_POINT('Ctrl Pts',(-0.0419392741328228,0.233437524640346,
-0.117607182502807));
#73409=CARTESIAN_POINT('Ctrl Pts',(-0.0419233069101264,0.233440393303946,
-0.117608254364183));
#73410=CARTESIAN_POINT('Ctrl Pts',(-0.0419073393854834,0.233443260337026,
-0.11760932631259));
#73411=CARTESIAN_POINT('Ctrl Pts',(-0.0406613141794025,0.233666856699471,
-0.11769298041077));
#73412=CARTESIAN_POINT('Ctrl Pts',(-0.0394295655190218,0.233877856112213,
-0.117776051018579));
#73413=CARTESIAN_POINT('Ctrl Pts',(-0.0374715243177032,0.23419736268533,
-0.117908781232462));
#73414=CARTESIAN_POINT('Ctrl Pts',(-0.0367462751363644,0.234312251173553,
-0.117958091049391));
#73415=CARTESIAN_POINT('Ctrl Pts',(-0.0353639204475622,0.234524657664918,
-0.118052377902706));
#73416=CARTESIAN_POINT('Ctrl Pts',(-0.0347069258778216,0.234622784854061,
-0.11809732065703));
#73417=CARTESIAN_POINT('Ctrl Pts',(-0.033144621262886,0.234849421577537,
-0.118204493981608));
#73418=CARTESIAN_POINT('Ctrl Pts',(-0.0322389705330159,0.234975457107885,
-0.118266860235112));
#73419=CARTESIAN_POINT('Ctrl Pts',(-0.0291755708059842,0.235383734052467,
-0.118478572780337));
#73420=CARTESIAN_POINT('Ctrl Pts',(-0.0270147491157533,0.235641504566257,
-0.11862917365776));
#73421=CARTESIAN_POINT('Ctrl Pts',(-0.0217308353624622,0.236198208205375,
-0.119000041144256));
#73422=CARTESIAN_POINT('Ctrl Pts',(-0.0186048258583135,0.2364649682449,
-0.119221657036352));
#73423=CARTESIAN_POINT('Ctrl Pts',(-0.00576030112902554,0.237304805753033,
-0.120138982690224));
#73424=CARTESIAN_POINT('Ctrl Pts',(0.00398336794439466,0.237341239431457,
-0.120850203430668));
#73425=CARTESIAN_POINT('Ctrl Pts',(0.0312231769978453,0.235765020726392,
-0.122843171008102));
#73426=CARTESIAN_POINT('Ctrl Pts',(0.0485818250559329,0.232809063584704,
-0.124114015434344));
#73427=CARTESIAN_POINT('Ctrl Pts',(0.0684646634710677,0.227099886388252,
-0.125538943349998));
#73428=CARTESIAN_POINT('Ctrl Pts',(0.0714544569375792,0.226176989894679,
-0.12575255085971));
#73429=CARTESIAN_POINT('Ctrl Pts',(0.0758482204165325,0.22472488538814,
-0.126065631322679));
#73430=CARTESIAN_POINT('Ctrl Pts',(0.0772667352360214,0.224241116789075,
-0.126166579372806));
#73431=CARTESIAN_POINT('Ctrl Pts',(0.0797853948396371,0.223355418355039,
-0.12634561859638));
#73432=CARTESIAN_POINT('Ctrl Pts',(0.0808873155438912,0.222958728035803,
-0.126423879998563));
#73433=CARTESIAN_POINT('Ctrl Pts',(0.0832092110477833,0.22210336866464,
-0.126588662580306));
#73434=CARTESIAN_POINT('Ctrl Pts',(0.0844284380617033,0.221642771452417,
-0.126675116542418));
#73435=CARTESIAN_POINT('Ctrl Pts',(0.0876725020877363,0.220386582223038,
-0.126904995179905));
#73436=CARTESIAN_POINT('Ctrl Pts',(0.0896903257542046,0.219573129572948,
-0.127047818471099));
#73437=CARTESIAN_POINT('Ctrl Pts',(0.100002505295372,0.215250062541782,
-0.127777335077885));
#73438=CARTESIAN_POINT('Ctrl Pts',(0.108103802279133,0.211297626187242,
-0.128348759130919));
#73439=CARTESIAN_POINT('Ctrl Pts',(0.125487704905034,0.201554150426609,
-0.129591715403383));
#73440=CARTESIAN_POINT('Ctrl Pts',(0.134634101961298,0.195563055040453,
-0.130257032561207));
#73441=CARTESIAN_POINT('Ctrl Pts',(0.153053908972181,0.181590975116401,
-0.131675820923081));
#73442=CARTESIAN_POINT('Ctrl Pts',(0.162188224000305,0.173481077428067,
-0.132428506538101));
#73443=CARTESIAN_POINT('Ctrl Pts',(0.172094245765931,0.163217135574412,
-0.133359207778695));
#73444=CARTESIAN_POINT('Ctrl Pts',(0.173511686439202,0.161709482481619,
-0.133495434229795));
#73445=CARTESIAN_POINT('Ctrl Pts',(0.175471221910759,0.159569807570801,
-0.133688433008307));
#73446=CARTESIAN_POINT('Ctrl Pts',(0.17603003968329,0.158953132350848,-0.133744018966581));
#73447=CARTESIAN_POINT('Ctrl Pts',(0.177033678867831,0.157833797705537,
-0.133844873059607));
#73448=CARTESIAN_POINT('Ctrl Pts',(0.177479639748936,0.157332160127695,
-0.133890057060902));
#73449=CARTESIAN_POINT('Ctrl Pts',(0.178389254654472,0.156300194070775,
-0.133982995760833));
#73450=CARTESIAN_POINT('Ctrl Pts',(0.178852682950757,0.155769684505577,
-0.134030764903502));
#73451=CARTESIAN_POINT('Ctrl Pts',(0.180042616421704,0.154395197507338,
-0.134154489362849));
#73452=CARTESIAN_POINT('Ctrl Pts',(0.180765542867942,0.153548165504204,
-0.134230696644829));
#73453=CARTESIAN_POINT('Ctrl Pts',(0.183836621162676,0.149898125592831,
-0.134558810662025));
#73454=CARTESIAN_POINT('Ctrl Pts',(0.186125606477016,0.147046272714128,
-0.134814469141503));
#73455=CARTESIAN_POINT('Ctrl Pts',(0.192312433121669,0.138962112472606,
-0.135534700329734));
#73456=CARTESIAN_POINT('Ctrl Pts',(0.196061568367257,0.133620322461467,
-0.136005510592295));
#73457=CARTESIAN_POINT('Ctrl Pts',(0.201770372409919,0.124727917694376,
-0.136773861340206));
#73458=CARTESIAN_POINT('Ctrl Pts',(0.203867807946244,0.121269339854454,
-0.13706916217845));
#73459=CARTESIAN_POINT('Ctrl Pts',(0.214800835754819,0.102155319502525,
-0.138677422479804));
#73460=CARTESIAN_POINT('Ctrl Pts',(0.221924778514198,0.0855846835914042,
-0.139980412817154));
#73461=CARTESIAN_POINT('Ctrl Pts',(0.228002525397906,0.0653946144547187,
-0.141432465470148));
#73462=CARTESIAN_POINT('Ctrl Pts',(0.228838519214608,0.0624062569083836,
-0.141644271690046));
#73463=CARTESIAN_POINT('Ctrl Pts',(0.229990116612161,0.0579548277846998,
-0.141955332757995));
#73464=CARTESIAN_POINT('Ctrl Pts',(0.230350876387253,0.0565038912700911,
-0.142056031237064));
#73465=CARTESIAN_POINT('Ctrl Pts',(0.230969966771371,0.0539094523898376,
-0.142234891463863));
#73466=CARTESIAN_POINT('Ctrl Pts',(0.231233581824808,0.0527672751700546,
-0.142313220550652));
#73467=CARTESIAN_POINT('Ctrl Pts',(0.231773529879102,0.0503460391445611,
-0.14247841560043));
#73468=CARTESIAN_POINT('Ctrl Pts',(0.232047768050413,0.0490665493941061,
-0.142565212226774));
#73469=CARTESIAN_POINT('Ctrl Pts',(0.232753444964353,0.0456358207419901,
-0.14279664962511));
#73470=CARTESIAN_POINT('Ctrl Pts',(0.233165652926233,0.0434807210531672,
-0.142940676721724));
#73471=CARTESIAN_POINT('Ctrl Pts',(0.235161830736234,0.0321980141257359,
-0.143688117149105));
#73472=CARTESIAN_POINT('Ctrl Pts',(0.236240042013914,0.0229885135371988,
-0.144275337543931));
#73473=CARTESIAN_POINT('Ctrl Pts',(0.237397162333193,0.00304624986000087,
-0.145520097420657));
#73474=CARTESIAN_POINT('Ctrl Pts',(0.237292600406242,-0.00767613580710551,
-0.14617274365936));
#73475=CARTESIAN_POINT('Ctrl Pts',(0.235529536730651,-0.0303895884491641,
-0.147571376429492));
#73476=CARTESIAN_POINT('Ctrl Pts',(0.233678080003207,-0.0423340270988234,
-0.148316746171546));
#73477=CARTESIAN_POINT('Ctrl Pts',(0.230452728613299,-0.056105537690637,
-0.14923956944462));
#73478=CARTESIAN_POINT('Ctrl Pts',(0.229952765032285,-0.0581207073085242,
-0.149376249136292));
#73479=CARTESIAN_POINT('Ctrl Pts',(0.229214966752837,-0.0609358300574998,
-0.149569833449145));
#73480=CARTESIAN_POINT('Ctrl Pts',(0.228999250339493,-0.0617415553740832,
-0.149625545766298));
#73481=CARTESIAN_POINT('Ctrl Pts',(0.228601967178426,-0.0631947258300784,
-0.149726607456939));
#73482=CARTESIAN_POINT('Ctrl Pts',(0.228421886341667,-0.0638425766452738,
-0.149771872254705));
#73483=CARTESIAN_POINT('Ctrl Pts',(0.228047528574421,-0.0651674879565829,
-0.149864888607596));
#73484=CARTESIAN_POINT('Ctrl Pts',(0.227852987027905,-0.0658444610035887,
-0.149912654281116));
#73485=CARTESIAN_POINT('Ctrl Pts',(0.227343197449048,-0.0675891305191501,
-0.150036351909273));
#73486=CARTESIAN_POINT('Ctrl Pts',(0.22702344669927,-0.0686554769580445,
-0.150112535588346));
#73487=CARTESIAN_POINT('Ctrl Pts',(0.225622343033365,-0.0732112305367457,
-0.15044038472327));
#73488=CARTESIAN_POINT('Ctrl Pts',(0.224468018572885,-0.0766774475920768,
-0.150695794277266));
#73489=CARTESIAN_POINT('Ctrl Pts',(0.221033683606676,-0.0862469084447028,
-0.151415094649121));
#73490=CARTESIAN_POINT('Ctrl Pts',(0.218581626439671,-0.0922847747616836,
-0.151885204845275));
#73491=CARTESIAN_POINT('Ctrl Pts',(0.21417117132057,-0.101979441210671,
-0.152659601789109));
#73492=CARTESIAN_POINT('Ctrl Pts',(0.212359743947641,-0.105699741909095,
-0.152961708599504));
#73493=CARTESIAN_POINT('Ctrl Pts',(0.202207528789262,-0.125234711837627,
-0.15456962969795));
#73494=CARTESIAN_POINT('Ctrl Pts',(0.192194200116681,-0.140118666259069,
-0.155865231049579));
#73495=CARTESIAN_POINT('Ctrl Pts',(0.178586406111427,-0.156104250519835,
-0.157311032985161));
#73496=CARTESIAN_POINT('Ctrl Pts',(0.17652525903678,-0.158431297410584,
-0.15752322418723));
#73497=CARTESIAN_POINT('Ctrl Pts',(0.173405317849516,-0.161817222802482,
-0.157834711247489));
#73498=CARTESIAN_POINT('Ctrl Pts',(0.172381357010381,-0.162907598925841,
-0.157935457524008));
#73499=CARTESIAN_POINT('Ctrl Pts',(0.170536897323632,-0.16483482783265,
-0.158114343254752));
#73500=CARTESIAN_POINT('Ctrl Pts',(0.169720390364434,-0.1656754145761,-0.158192650681002));
#73501=CARTESIAN_POINT('Ctrl Pts',(0.167979939349333,-0.167440823588724,
-0.158357738947634));
#73502=CARTESIAN_POINT('Ctrl Pts',(0.167054508930708,-0.168364130948288,
-0.158444450935687));
#73503=CARTESIAN_POINT('Ctrl Pts',(0.164558690474189,-0.170813384518051,
-0.158675514807385));
#73504=CARTESIAN_POINT('Ctrl Pts',(0.162974700843463,-0.172325338686806,
-0.158819255828806));
#73505=CARTESIAN_POINT('Ctrl Pts',(0.154626504230812,-0.180075801523522,
-0.159562374211088));
#73506=CARTESIAN_POINT('Ctrl Pts',(0.147523963190298,-0.185939130802494,
-0.160145780548163));
#73507=CARTESIAN_POINT('Ctrl Pts',(0.131409680509794,-0.197735720883886,
-0.161390469743401));
#73508=CARTESIAN_POINT('Ctrl Pts',(0.12229817477599,-0.20349713804708,-0.162046523425559));
#73509=CARTESIAN_POINT('Ctrl Pts',(0.102170866704393,-0.214382491576574,
-0.163451090007482));
#73510=CARTESIAN_POINT('Ctrl Pts',(0.0910904829798847,-0.219319828080074,
-0.164198943852727));
#73511=CARTESIAN_POINT('Ctrl Pts',(0.0777298910860151,-0.224085576513676,
-0.16512444955251));
#73512=CARTESIAN_POINT('Ctrl Pts',(0.0757675930409317,-0.224756652171625,
-0.165260973505059));
#73513=CARTESIAN_POINT('Ctrl Pts',(0.0730048228234889,-0.225661186261036,
-0.165454351537729));
#73514=CARTESIAN_POINT('Ctrl Pts',(0.0722114685927882,-0.225916309485954,
-0.165510015129837));
#73515=CARTESIAN_POINT('Ctrl Pts',(0.070776085624787,-0.226369560184181,
-0.165610993478031));
#73516=CARTESIAN_POINT('Ctrl Pts',(0.070134520061887,-0.226569153135777,
-0.165656223794456));
#73517=CARTESIAN_POINT('Ctrl Pts',(0.0688188774111642,-0.226972329940867,
-0.165749190140842));
#73518=CARTESIAN_POINT('Ctrl Pts',(0.0681447300253172,-0.227175641704029,
-0.165796940352851));
#73519=CARTESIAN_POINT('Ctrl Pts',(0.0664028052847694,-0.22769252636039,
-0.165920596091726));
#73520=CARTESIAN_POINT('Ctrl Pts',(0.0653337233026107,-0.228001586806835,
-0.165996753232333));
#73521=CARTESIAN_POINT('Ctrl Pts',(0.0607476486542171,-0.229292470577999,
-0.1663244637223));
#73522=CARTESIAN_POINT('Ctrl Pts',(0.0572106174746963,-0.230200468094717,
-0.166579758981892));
#73523=CARTESIAN_POINT('Ctrl Pts',(0.0473125528260156,-0.232499225371961,
-0.16729866916973));
#73524=CARTESIAN_POINT('Ctrl Pts',(0.0409132710682016,-0.233710205763855,
-0.167768498715436));
#73525=CARTESIAN_POINT('Ctrl Pts',(0.0303334731170175,-0.235264456523317,
-0.168546003443792));
#73526=CARTESIAN_POINT('Ctrl Pts',(0.0261788674989858,-0.235762911008172,
-0.16885152753961));
#73527=CARTESIAN_POINT('Ctrl Pts',(0.00425317270159916,-0.237806758298755,
-0.170459880130942));
#73528=CARTESIAN_POINT('Ctrl Pts',(-0.0136404184221096,-0.237453816122117,
-0.171752365742219));
#73529=CARTESIAN_POINT('Ctrl Pts',(-0.0344117743366196,-0.234685940736986,
-0.173195578486813));
#73530=CARTESIAN_POINT('Ctrl Pts',(-0.0374875775764345,-0.234214312381348,
-0.173407987406293));
#73531=CARTESIAN_POINT('Ctrl Pts',(-0.0420274952558084,-0.233426452746969,
-0.173719719009552));
#73532=CARTESIAN_POINT('Ctrl Pts',(-0.0434992233954118,-0.233156678956929,
-0.173820495945463));
#73533=CARTESIAN_POINT('Ctrl Pts',(-0.046118792410249,-0.232650833931493,
-0.173999404302277));
#73534=CARTESIAN_POINT('Ctrl Pts',(-0.0472676101201849,-0.232420151150761,
-0.174077704045024));
#73535=CARTESIAN_POINT('Ctrl Pts',(-0.0496937718187097,-0.231914244619261,
-0.17424274363375));
#73536=CARTESIAN_POINT('Ctrl Pts',(-0.0509706498374841,-0.231636959024393,
-0.174329414883327));
#73537=CARTESIAN_POINT('Ctrl Pts',(-0.0543788447542903,-0.230867291978971,
-0.174560292661675));
#73538=CARTESIAN_POINT('Ctrl Pts',(-0.0565057846285708,-0.230355946508815,
-0.174703889831387));
#73539=CARTESIAN_POINT('Ctrl Pts',(-0.0675119475841352,-0.227548296392982,
-0.175444886714059));
#73540=CARTESIAN_POINT('Ctrl Pts',(-0.0762601508909911,-0.224767678651007,
-0.176026426779777));
#73541=CARTESIAN_POINT('Ctrl Pts',(-0.0948988896575572,-0.217629324586893,
-0.177270529810449));
#73542=CARTESIAN_POINT('Ctrl Pts',(-0.104696979828549,-0.213088887619416,
-0.177927729059481));
#73543=CARTESIAN_POINT('Ctrl Pts',(-0.124784407854769,-0.202059301641824,
-0.179334359043513));
#73544=CARTESIAN_POINT('Ctrl Pts',(-0.134951920443454,-0.195414976646931,
-0.180083115762509));
#73545=CARTESIAN_POINT('Ctrl Pts',(-0.146206861234186,-0.186761402787457,
-0.181009436949204));
#73546=CARTESIAN_POINT('Ctrl Pts',(-0.147831657988762,-0.185477944843892,
-0.181145746290077));
#73547=CARTESIAN_POINT('Ctrl Pts',(-0.150086069528746,-0.183648702460812,
-0.181338867702054));
#73548=CARTESIAN_POINT('Ctrl Pts',(-0.150729983689493,-0.183120578163806,
-0.181394493315748));
#73549=CARTESIAN_POINT('Ctrl Pts',(-0.151888226556527,-0.182160364754587,
-0.181495422619538));
#73550=CARTESIAN_POINT('Ctrl Pts',(-0.152403532942728,-0.181729455465044,
-0.181540642127857));
#73551=CARTESIAN_POINT('Ctrl Pts',(-0.15344467486292,-0.18085128951155,
-0.181632663444296));
#73552=CARTESIAN_POINT('Ctrl Pts',(-0.153970397898302,-0.180403918199303,
-0.18167947256891));
#73553=CARTESIAN_POINT('Ctrl Pts',(-0.155271847595331,-0.179286598938222,
-0.181796189931273));
#73554=CARTESIAN_POINT('Ctrl Pts',(-0.156045189387923,-0.178613913195304,
-0.181866292779184));
#73555=CARTESIAN_POINT('Ctrl Pts',(-0.157750947807456,-0.177110638746918,
-0.182022538978979));
#73556=CARTESIAN_POINT('Ctrl Pts',(-0.158681208070373,-0.176277661476834,
-0.18210884060396));
#73557=CARTESIAN_POINT('Ctrl Pts',(-0.16138203919936,-0.173820570363269,
-0.182362501518714));
#73558=CARTESIAN_POINT('Ctrl Pts',(-0.163134509806404,-0.172176897345417,
-0.182531046370922));
#73559=CARTESIAN_POINT('Ctrl Pts',(-0.169382400913826,-0.166135868117174,
-0.183145505707788));
#73560=CARTESIAN_POINT('Ctrl Pts',(-0.173727248986793,-0.16158699430277,
-0.183598815142674));
#73561=CARTESIAN_POINT('Ctrl Pts',(-0.179598737349793,-0.154928952377287,
-0.184243778871834));
#73562=CARTESIAN_POINT('Ctrl Pts',(-0.181279606378228,-0.152958787757367,
-0.184432490648436));
#73563=CARTESIAN_POINT('Ctrl Pts',(-0.195745765150561,-0.135429397117074,
-0.186090913059738));
#73564=CARTESIAN_POINT('Ctrl Pts',(-0.206536204325546,-0.118324348639466,
-0.187558681570756));
#73565=CARTESIAN_POINT('Ctrl Pts',(-0.216232155612315,-0.09748682807027,
-0.18913822938638));
#73566=CARTESIAN_POINT('Ctrl Pts',(-0.217382649080613,-0.0948936871644106,
-0.18933161298771));
#73567=CARTESIAN_POINT('Ctrl Pts',(-0.219055091062853,-0.0909339547118214,
-0.189622243280102));
#73568=CARTESIAN_POINT('Ctrl Pts',(-0.219611343117681,-0.0895822258077033,
-0.18972064484483));
#73569=CARTESIAN_POINT('Ctrl Pts',(-0.220589739889991,-0.0871407636020019,
-0.189896951656467));
#73570=CARTESIAN_POINT('Ctrl Pts',(-0.221016390015588,-0.0860528991643905,
-0.18997500655894));
#73571=CARTESIAN_POINT('Ctrl Pts',(-0.221910859804268,-0.0837216555441437,
-0.19014122259533));
#73572=CARTESIAN_POINT('Ctrl Pts',(-0.222376309620995,-0.0824774050709694,
-0.190229302283899));
#73573=CARTESIAN_POINT('Ctrl Pts',(-0.223614668619061,-0.079080291306097,
-0.190468106229765));
#73574=CARTESIAN_POINT('Ctrl Pts',(-0.224366941078171,-0.076920015894052,
-0.190618144707412));
#73575=CARTESIAN_POINT('Ctrl Pts',(-0.228545521215175,-0.06433729207203,
-0.191482158114994));
#73576=CARTESIAN_POINT('Ctrl Pts',(-0.231276852359328,-0.0536973565629997,
-0.192172821148151));
#73577=CARTESIAN_POINT('Ctrl Pts',(-0.235875800516865,-0.0286944258220648,
-0.193746838634687));
#73578=CARTESIAN_POINT('Ctrl Pts',(-0.237185388115221,-0.0142756234224376,
-0.194617895383358));
#73579=CARTESIAN_POINT('Ctrl Pts',(-0.237174937953315,0.000171557107381939,
-0.195520038937142));
#73580=CARTESIAN_POINT('Origin',(0.,0.,-0.9775));
#73581=CARTESIAN_POINT('',(-0.29419993969113,0.000188376579435279,-1.92858238829104));
#73582=CARTESIAN_POINT('',(0.12894108841962,0.264438718264107,-1.96079706282707));
#73583=CARTESIAN_POINT('Ctrl Pts',(-0.29419993969113,0.000188376579435279,
-1.92858238829104));
#73584=CARTESIAN_POINT('Ctrl Pts',(-0.294193636363906,0.0100326921233836,
-1.92911748512889));
#73585=CARTESIAN_POINT('Ctrl Pts',(-0.293693265724678,0.019862149828654,
-1.92965258196674));
#73586=CARTESIAN_POINT('Ctrl Pts',(-0.292703045250943,0.0296406359720001,
-1.93018767880459));
#73587=CARTESIAN_POINT('Ctrl Pts',(-0.291037817615491,0.0460848580323184,
-1.93108753703381));
#73588=CARTESIAN_POINT('Ctrl Pts',(-0.287977283616911,0.0624400269542837,
-1.93198739526302));
#73589=CARTESIAN_POINT('Ctrl Pts',(-0.28354685905932,0.078452652712285,
-1.93288725349224));
#73590=CARTESIAN_POINT('Ctrl Pts',(-0.279125085348672,0.0944340122174017,
-1.93378535465829));
#73591=CARTESIAN_POINT('Ctrl Pts',(-0.273338875571435,0.110073387857488,
-1.93468345582433));
#73592=CARTESIAN_POINT('Ctrl Pts',(-0.266264720315519,0.125126890456442,
-1.93558155699038));
#73593=CARTESIAN_POINT('Ctrl Pts',(-0.259192119958031,0.140177084297433,
-1.9364794607539));
#73594=CARTESIAN_POINT('Ctrl Pts',(-0.250832423035421,0.15464092744763,
-1.93737736451743));
#73595=CARTESIAN_POINT('Ctrl Pts',(-0.241310388426852,0.168294196089116,
-1.93827526828095));
#73596=CARTESIAN_POINT('Ctrl Pts',(-0.2317911197368,0.181943498789488,-1.93917291122536));
#73597=CARTESIAN_POINT('Ctrl Pts',(-0.221110642536091,0.194782053275159,
-1.94007055416976));
#73598=CARTESIAN_POINT('Ctrl Pts',(-0.20943635480893,0.206615714030535,
-1.94096819711417));
#73599=CARTESIAN_POINT('Ctrl Pts',(-0.197734962313328,0.218476849578557,
-1.94186792416038));
#73600=CARTESIAN_POINT('Ctrl Pts',(-0.185035724332008,0.229327885384296,
-1.9427676512066));
#73601=CARTESIAN_POINT('Ctrl Pts',(-0.171542350944017,0.239012262933515,
-1.94366737825281));
#73602=CARTESIAN_POINT('Ctrl Pts',(-0.159523453405146,0.247638389117453,
-1.9444687884614));
#73603=CARTESIAN_POINT('Ctrl Pts',(-0.146875316353266,0.255339274278587,
-1.94527019866999));
#73604=CARTESIAN_POINT('Ctrl Pts',(-0.133759077941881,0.262034633337156,
-1.94607160887857));
#73605=CARTESIAN_POINT('Ctrl Pts',(-0.119199316029112,0.269466858244615,
-1.94696121925813));
#73606=CARTESIAN_POINT('Ctrl Pts',(-0.103967986147468,0.275707332434235,
-1.94785082963768));
#73607=CARTESIAN_POINT('Ctrl Pts',(-0.0882868080160081,0.280640480918816,
-1.94874044001724));
#73608=CARTESIAN_POINT('Ctrl Pts',(-0.0726355375993347,0.285564220722709,
-1.94962835369944));
#73609=CARTESIAN_POINT('Ctrl Pts',(-0.0565368624984817,0.28918527751626,
-1.95051626738163));
#73610=CARTESIAN_POINT('Ctrl Pts',(-0.040232402904419,0.291436088631001,
-1.95140418106383));
#73611=CARTESIAN_POINT('Ctrl Pts',(-0.0239311430304607,0.293686458028214,
-1.95229192049461));
#73612=CARTESIAN_POINT('Ctrl Pts',(-0.00742497013263192,0.294566957618438,
-1.95317965992538));
#73613=CARTESIAN_POINT('Ctrl Pts',(0.00903488855945793,0.294061236460568,
-1.95406739935616));
#73614=CARTESIAN_POINT('Ctrl Pts',(0.0254921775252421,0.29355559425629,
-1.95495500019235));
#73615=CARTESIAN_POINT('Ctrl Pts',(0.0419023600789404,0.291664204113601,
-1.95584260102853));
#73616=CARTESIAN_POINT('Ctrl Pts',(0.0580166101801649,0.288422802398151,
-1.95673020186472));
#73617=CARTESIAN_POINT('Ctrl Pts',(0.0741645751101561,0.285174618902406,
-1.95761965977213));
#73618=CARTESIAN_POINT('Ctrl Pts',(0.0900145886645593,0.280570990771778,
-1.95850911767955));
#73619=CARTESIAN_POINT('Ctrl Pts',(0.105330521385611,0.274698236733757,
-1.95939857558696));
#73620=CARTESIAN_POINT('Ctrl Pts',(0.113357559091118,0.271620342689892,
-1.95986473800033));
#73621=CARTESIAN_POINT('Ctrl Pts',(0.121238206880903,0.268194665714199,
-1.9603309004137));
#73622=CARTESIAN_POINT('Ctrl Pts',(0.12894108841962,0.264438718264107,-1.96079706282707));
#73623=CARTESIAN_POINT('',(-0.128892185405333,0.264462557919712,-1.9608));
#73624=CARTESIAN_POINT('Origin',(0.,0.,-1.9608));
#73625=CARTESIAN_POINT('',(-0.294199832726378,0.000313725630257716,-1.94301761170573));
#73626=CARTESIAN_POINT('Ctrl Pts',(-0.128892185405333,0.264462557919712,
-1.9608));
#73627=CARTESIAN_POINT('Ctrl Pts',(-0.144172453258884,0.257015352036523,
-1.95988042553177));
#73628=CARTESIAN_POINT('Ctrl Pts',(-0.158823731371776,0.248230991355156,
-1.95896085106354));
#73629=CARTESIAN_POINT('Ctrl Pts',(-0.17261306769371,0.238240149557892,
-1.95804127659531));
#73630=CARTESIAN_POINT('Ctrl Pts',(-0.186392524158092,0.228256466052477,
-1.95712236098871));
#73631=CARTESIAN_POINT('Ctrl Pts',(-0.199310661850408,0.217068438626958,
-1.95620344538212));
#73632=CARTESIAN_POINT('Ctrl Pts',(-0.211164165757333,0.204849542591654,
-1.95528452977553));
#73633=CARTESIAN_POINT('Ctrl Pts',(-0.223031084542253,0.192616818155832,
-1.9543645742114));
#73634=CARTESIAN_POINT('Ctrl Pts',(-0.233830441426606,0.179351418393509,
-1.95344461864728));
#73635=CARTESIAN_POINT('Ctrl Pts',(-0.243395958708843,0.165263569137917,
-1.95252466308315));
#73636=CARTESIAN_POINT('Ctrl Pts',(-0.252965853013338,0.151169273515868,
-1.95160428656259));
#73637=CARTESIAN_POINT('Ctrl Pts',(-0.261300398891812,0.136252410350624,
-1.95068391004203));
#73638=CARTESIAN_POINT('Ctrl Pts',(-0.268277579228135,0.120750902619781,
-1.94976353352148));
#73639=CARTESIAN_POINT('Ctrl Pts',(-0.275274713264632,0.105205062877639,
-1.94884052486068));
#73640=CARTESIAN_POINT('Ctrl Pts',(-0.280906460402522,0.0890719304062782,
-1.94791751619988));
#73641=CARTESIAN_POINT('Ctrl Pts',(-0.28509924002603,0.0726089755924176,
-1.94699450753908));
#73642=CARTESIAN_POINT('Ctrl Pts',(-0.28824635057256,0.0602518418114619,
-1.94630169500139));
#73643=CARTESIAN_POINT('Ctrl Pts',(-0.290583772810123,0.0477093161032033,
-1.9456088824637));
#73644=CARTESIAN_POINT('Ctrl Pts',(-0.292099501141714,0.0350930396626186,
-1.94491606992601));
#73645=CARTESIAN_POINT('Ctrl Pts',(-0.293483977099918,0.0235692520220445,
-1.94428325052032));
#73646=CARTESIAN_POINT('Ctrl Pts',(-0.294187418228296,0.0119555623629466,
-1.94365043111464));
#73647=CARTESIAN_POINT('Ctrl Pts',(-0.294199832726315,0.000313725689767731,
-1.94301761170896));
#73648=CARTESIAN_POINT('',(-0.294181798577116,0.000133869447550703,-1.84301761781353));
#73649=CARTESIAN_POINT('Ctrl Pts',(-0.294199832726378,0.000313725630257912,
-1.94301761170573));
#73650=CARTESIAN_POINT('Ctrl Pts',(-0.294217035041623,-0.0158179441453529,
-1.94214073686488));
#73651=CARTESIAN_POINT('Ctrl Pts',(-0.292903174616159,-0.0320111324691114,
-1.94126386202403));
#73652=CARTESIAN_POINT('Ctrl Pts',(-0.290254358978592,-0.0480213191606245,
-1.94038698718318));
#73653=CARTESIAN_POINT('Ctrl Pts',(-0.287610259166518,-0.0640030020765365,
-1.93951167348863));
#73654=CARTESIAN_POINT('Ctrl Pts',(-0.283635983382084,-0.0798015088650099,
-1.93863635979408));
#73655=CARTESIAN_POINT('Ctrl Pts',(-0.278379474364989,-0.0951761958279081,
-1.93776104609953));
#73656=CARTESIAN_POINT('Ctrl Pts',(-0.273122876603055,-0.110551142359301,
-1.93688571762719));
#73657=CARTESIAN_POINT('Ctrl Pts',(-0.266584228486466,-0.125501456989427,
-1.93601038915485));
#73658=CARTESIAN_POINT('Ctrl Pts',(-0.25886143281037,-0.139801282552637,
-1.93513506068251));
#73659=CARTESIAN_POINT('Ctrl Pts',(-0.251138408936953,-0.154101530654787,
-1.9342597063455));
#73660=CARTESIAN_POINT('Ctrl Pts',(-0.242231590358653,-0.167750537452882,
-1.93338435200848));
#73661=CARTESIAN_POINT('Ctrl Pts',(-0.232283958546599,-0.180548615618957,
-1.93250899767147));
#73662=CARTESIAN_POINT('Ctrl Pts',(-0.22231468153334,-0.193374541315195,
-1.93163173863783));
#73663=CARTESIAN_POINT('Ctrl Pts',(-0.211300636300945,-0.205345235053099,
-1.93075447960419));
#73664=CARTESIAN_POINT('Ctrl Pts',(-0.199423466513676,-0.216295910741902,
-1.92987722057055));
#73665=CARTESIAN_POINT('Ctrl Pts',(-0.195609630161698,-0.21981224382198,
-1.92959552699771));
#73666=CARTESIAN_POINT('Ctrl Pts',(-0.191707050176684,-0.223223717710466,
-1.92931383342487));
#73667=CARTESIAN_POINT('Ctrl Pts',(-0.187722398853854,-0.22652580640747,
-1.92903213985203));
#73668=CARTESIAN_POINT('Ctrl Pts',(-0.174999249451123,-0.237069506327294,
-1.92813268112336));
#73669=CARTESIAN_POINT('Ctrl Pts',(-0.161345053520292,-0.246571091634817,
-1.92723322239468));
#73670=CARTESIAN_POINT('Ctrl Pts',(-0.146955739436558,-0.254867908232195,
-1.92633376366601));
#73671=CARTESIAN_POINT('Ctrl Pts',(-0.132594367936121,-0.263148613256254,
-1.92543605159464));
#73672=CARTESIAN_POINT('Ctrl Pts',(-0.117501354938071,-0.270228747692943,
-1.92453833952326));
#73673=CARTESIAN_POINT('Ctrl Pts',(-0.101902268212067,-0.275988347096822,
-1.92364062745189));
#73674=CARTESIAN_POINT('Ctrl Pts',(-0.0863062601140787,-0.281746809789021,
-1.92274309255253));
#73675=CARTESIAN_POINT('Ctrl Pts',(-0.0702050961063534,-0.286184933517517,
-1.92184555765316));
#73676=CARTESIAN_POINT('Ctrl Pts',(-0.0538449204140348,-0.289230642473453,
-1.92094802275379));
#73677=CARTESIAN_POINT('Ctrl Pts',(-0.0374893075748574,-0.292275501981135,
-1.92005073817692));
#73678=CARTESIAN_POINT('Ctrl Pts',(-0.0208756039515256,-0.293928583288013,
-1.91915345360005));
#73679=CARTESIAN_POINT('Ctrl Pts',(-0.00425919539984884,-0.294169167749691,
-1.91825616902317));
#73680=CARTESIAN_POINT('Ctrl Pts',(0.0123962441238195,-0.294410317330201,
-1.9173567767773));
#73681=CARTESIAN_POINT('Ctrl Pts',(0.0290536088470616,-0.293232357194632,
-1.91645738453142));
#73682=CARTESIAN_POINT('Ctrl Pts',(0.0454580461426138,-0.290666829963269,
-1.91555799228555));
#73683=CARTESIAN_POINT('Ctrl Pts',(0.0601090975319945,-0.288375518738729,
-1.91475473144971));
#73684=CARTESIAN_POINT('Ctrl Pts',(0.0745580725981294,-0.284978244983199,
-1.91395147061387));
#73685=CARTESIAN_POINT('Ctrl Pts',(0.0886326038546962,-0.280531462645345,
-1.91314820977803));
#73686=CARTESIAN_POINT('Ctrl Pts',(0.104397103171186,-0.275550742801266,
-1.91224849918258));
#73687=CARTESIAN_POINT('Ctrl Pts',(0.119788857198775,-0.269221776581918,
-1.91134878858713));
#73688=CARTESIAN_POINT('Ctrl Pts',(0.134564982691761,-0.261621683797743,
-1.91044907799168));
#73689=CARTESIAN_POINT('Ctrl Pts',(0.149313219172654,-0.25403593571304,
-1.90955106554366));
#73690=CARTESIAN_POINT('Ctrl Pts',(0.163447411623416,-0.245184124227383,
-1.90865305309565));
#73691=CARTESIAN_POINT('Ctrl Pts',(0.176744624805868,-0.235191363791771,
-1.90775504064764));
#73692=CARTESIAN_POINT('Ctrl Pts',(0.19004026610177,-0.225199784617638,
-1.90685713435523));
#73693=CARTESIAN_POINT('Ctrl Pts',(0.202498465489455,-0.214067955634066,
-1.90595922806282));
#73694=CARTESIAN_POINT('Ctrl Pts',(0.213925481031022,-0.201964176441383,
-1.90506132177041));
#73695=CARTESIAN_POINT('Ctrl Pts',(0.225349814876871,-0.189863237767531,
-1.90416362619895));
#73696=CARTESIAN_POINT('Ctrl Pts',(0.235742912830622,-0.176791383399317,
-1.90326593062748));
#73697=CARTESIAN_POINT('Ctrl Pts',(0.244949280141027,-0.162952416853487,
-1.90236823505601));
#73698=CARTESIAN_POINT('Ctrl Pts',(0.254177861619886,-0.149080058077724,
-1.90146837342273));
#73699=CARTESIAN_POINT('Ctrl Pts',(0.262213577408823,-0.134437564321108,
-1.90056851178945));
#73700=CARTESIAN_POINT('Ctrl Pts',(0.268945203200768,-0.119256520472877,
-1.89966865015617));
#73701=CARTESIAN_POINT('Ctrl Pts',(0.274940688710376,-0.105735607215682,
-1.8988671933388));
#73702=CARTESIAN_POINT('Ctrl Pts',(0.2799022483917,-0.0917882161141617,
-1.89806573652142));
#73703=CARTESIAN_POINT('Ctrl Pts',(0.283784549488893,-0.0775884622310952,
-1.89726427970405));
#73704=CARTESIAN_POINT('Ctrl Pts',(0.288129241563922,-0.061697485045494,
-1.89636736753888));
#73705=CARTESIAN_POINT('Ctrl Pts',(0.291149258518538,-0.0453882981460449,
-1.8954704553737));
#73706=CARTESIAN_POINT('Ctrl Pts',(0.292776608790061,-0.0289049709460469,
-1.89457354320853));
#73707=CARTESIAN_POINT('Ctrl Pts',(0.294400747119029,-0.0124541773075123,
-1.89367840130168));
#73708=CARTESIAN_POINT('Ctrl Pts',(0.294637529594483,0.00416930050062396,
-1.89278325939482));
#73709=CARTESIAN_POINT('Ctrl Pts',(0.293470035720682,0.0207117873227185,
-1.89188811748797));
#73710=CARTESIAN_POINT('Ctrl Pts',(0.292302769717584,0.0372510453928779,
-1.89099315029434));
#73711=CARTESIAN_POINT('Ctrl Pts',(0.289731772884849,0.0537085506239803,
-1.8900981831007));
#73712=CARTESIAN_POINT('Ctrl Pts',(0.285792240943256,0.069831475830259,
-1.88920321590707));
#73713=CARTESIAN_POINT('Ctrl Pts',(0.281853825128017,0.0859498331787345,
-1.88830850227058));
#73714=CARTESIAN_POINT('Ctrl Pts',(0.276547842355274,0.101733029589139,
-1.88741378863409));
#73715=CARTESIAN_POINT('Ctrl Pts',(0.269960107105045,0.116940927702121,
-1.8865190749976));
#73716=CARTESIAN_POINT('Ctrl Pts',(0.263356487414368,0.132185495314217,
-1.88562220401493));
#73717=CARTESIAN_POINT('Ctrl Pts',(0.255465283571869,0.146851272710017,
-1.88472533303226));
#73718=CARTESIAN_POINT('Ctrl Pts',(0.246419722265722,0.160720130906133,
-1.8838284620496));
#73719=CARTESIAN_POINT('Ctrl Pts',(0.23818942255219,0.173339011678179,-1.88301242457642));
#73720=CARTESIAN_POINT('Ctrl Pts',(0.229004329318591,0.185298117620465,
-1.88219638710324));
#73721=CARTESIAN_POINT('Ctrl Pts',(0.218993716856664,0.19645709958488,-1.88138034963006));
#73722=CARTESIAN_POINT('Ctrl Pts',(0.207972888625727,0.208742184431554,
-1.88048196215816));
#73723=CARTESIAN_POINT('Ctrl Pts',(0.19587999043407,0.220136142643117,-1.87958357468625));
#73724=CARTESIAN_POINT('Ctrl Pts',(0.182884332901883,0.230449475545147,
-1.87868518721435));
#73725=CARTESIAN_POINT('Ctrl Pts',(0.169913911101314,0.24074278141118,-1.87778854428404));
#73726=CARTESIAN_POINT('Ctrl Pts',(0.156044781088644,0.249959089577038,
-1.87689190135373));
#73727=CARTESIAN_POINT('Ctrl Pts',(0.141481890185821,0.257946728510844,
-1.87599525842342));
#73728=CARTESIAN_POINT('Ctrl Pts',(0.126921552086915,0.265932967250411,
-1.87509877267025));
#73729=CARTESIAN_POINT('Ctrl Pts',(0.11166836044177,0.272690538754484,-1.87420228691709));
#73730=CARTESIAN_POINT('Ctrl Pts',(0.0959546917773066,0.278112094533701,
-1.87330580116392));
#73731=CARTESIAN_POINT('Ctrl Pts',(0.0802452495683534,0.283532192094294,
-1.87240955653568));
#73732=CARTESIAN_POINT('Ctrl Pts',(0.064076327662526,0.287616739394745,
-1.87151331190743));
#73733=CARTESIAN_POINT('Ctrl Pts',(0.0476969939611587,0.290307831046751,
-1.87061706727919));
#73734=CARTESIAN_POINT('Ctrl Pts',(0.0312784436967652,0.293005365901351,
-1.86971867679846));
#73735=CARTESIAN_POINT('Ctrl Pts',(0.0146492636034039,0.29430267865183,
-1.86882028631773));
#73736=CARTESIAN_POINT('Ctrl Pts',(-0.0019343336099744,0.294193640912725,
-1.867921895837));
#73737=CARTESIAN_POINT('Ctrl Pts',(-0.0168584757494519,0.294095514149513,
-1.86711340374336));
#73738=CARTESIAN_POINT('Ctrl Pts',(-0.0317452363588749,0.292859161753257,
-1.86630491164972));
#73739=CARTESIAN_POINT('Ctrl Pts',(-0.0464121480238433,0.290516010773611,
-1.86549641955607));
#73740=CARTESIAN_POINT('Ctrl Pts',(-0.0627085619740153,0.287912534378286,
-1.86459810352783));
#73741=CARTESIAN_POINT('Ctrl Pts',(-0.0788370821054864,0.283925291532679,
-1.86369978749959));
#73742=CARTESIAN_POINT('Ctrl Pts',(-0.0945467246718159,0.2785938923484,
-1.86280147147135));
#73743=CARTESIAN_POINT('Ctrl Pts',(-0.110225942020353,0.273272818604731,
-1.86190489523195));
#73744=CARTESIAN_POINT('Ctrl Pts',(-0.125487130426198,0.266612944882,-1.86100831899255));
#73745=CARTESIAN_POINT('Ctrl Pts',(-0.140091790292761,0.258704329868228,
-1.86011174275314));
#73746=CARTESIAN_POINT('Ctrl Pts',(-0.154694026867372,0.250797027098856,
-1.859215315279));
#73747=CARTESIAN_POINT('Ctrl Pts',(-0.168639232467807,0.241641723459449,
-1.85831888780486));
#73748=CARTESIAN_POINT('Ctrl Pts',(-0.181711297679933,0.231375548179739,
-1.85742246033071));
#73749=CARTESIAN_POINT('Ctrl Pts',(-0.194779912490204,0.221112082680745,
-1.85652626947067));
#73750=CARTESIAN_POINT('Ctrl Pts',(-0.206975228840357,0.209738825049817,
-1.85563007861063));
#73751=CARTESIAN_POINT('Ctrl Pts',(-0.218113653404721,0.197433721026691,
-1.8547338877506));
#73752=CARTESIAN_POINT('Ctrl Pts',(-0.229278857310927,0.185099032695198,
-1.85383554224101));
#73753=CARTESIAN_POINT('Ctrl Pts',(-0.239381580730588,0.171828630164055,
-1.85293719673143));
#73754=CARTESIAN_POINT('Ctrl Pts',(-0.248277879238832,0.157834516759384,
-1.85203885122185));
#73755=CARTESIAN_POINT('Ctrl Pts',(-0.256287283970732,0.145235510777484,
-1.85123006397526));
#73756=CARTESIAN_POINT('Ctrl Pts',(-0.263319194239916,0.132050695847513,
-1.85042127672867));
#73757=CARTESIAN_POINT('Ctrl Pts',(-0.269301100085867,0.118450654251219,
-1.84961248948208));
#73758=CARTESIAN_POINT('Ctrl Pts',(-0.276605475269511,0.101843939118829,
-1.84862489695806));
#73759=CARTESIAN_POINT('Ctrl Pts',(-0.282384365359411,0.0845267189773186,
-1.84763730443405));
#73760=CARTESIAN_POINT('Ctrl Pts',(-0.286520638407411,0.0667799653085389,
-1.84664971191003));
#73761=CARTESIAN_POINT('Ctrl Pts',(-0.290628292530723,0.0491560016492214,
-1.84566895255097));
#73762=CARTESIAN_POINT('Ctrl Pts',(-0.29311574621684,0.0311089028882957,
-1.84468819319192));
#73763=CARTESIAN_POINT('Ctrl Pts',(-0.29391554915533,0.0129340621894621,
-1.84370743383287));
#73764=CARTESIAN_POINT('Ctrl Pts',(-0.294103062588117,0.00867297910787347,
-1.84347749525012));
#73765=CARTESIAN_POINT('Ctrl Pts',(-0.294198025887685,0.0044049446360574,
-1.84324755666737));
#73766=CARTESIAN_POINT('Ctrl Pts',(-0.294199969536726,0.000133882744709338,
-1.84301761808462));
#73767=CARTESIAN_POINT('',(-0.294199886788754,-0.00025809588161594,-1.74301760920454));
#73768=CARTESIAN_POINT('Ctrl Pts',(-0.293772605452732,0.000133570007895117,
-1.84301761170896));
#73769=CARTESIAN_POINT('Ctrl Pts',(-0.293541789016053,-0.0572970795812668,
-1.83992126094201));
#73770=CARTESIAN_POINT('Ctrl Pts',(-0.249523258593931,-0.213261476144942,
-1.83153026681705));
#73771=CARTESIAN_POINT('Ctrl Pts',(0.0037807816485258,-0.347758850054799,
-1.81784462933411));
#73772=CARTESIAN_POINT('Ctrl Pts',(0.294305938288256,-0.185300865244264,
-1.80196069926011));
#73773=CARTESIAN_POINT('Ctrl Pts',(0.315230872436925,0.146908278444259,
-1.78607676918614));
#73774=CARTESIAN_POINT('Ctrl Pts',(0.0473846120171572,0.344538303459251,
-1.77019283911214));
#73775=CARTESIAN_POINT('Ctrl Pts',(-0.233870088077291,0.23792327169595,
-1.75583978661975));
#73776=CARTESIAN_POINT('Ctrl Pts',(-0.29345314308191,0.0693924262310005,
-1.74678137748536));
#73777=CARTESIAN_POINT('Ctrl Pts',(-0.294038510274165,-0.000257907963998623,
-1.74301761170896));
#73778=CARTESIAN_POINT('',(-0.294199999759564,1.18942342969988E-5,-1.64301761170595));
#73779=CARTESIAN_POINT('Ctrl Pts',(-0.294199886788754,-0.00025809588161594,
-1.74301760920454));
#73780=CARTESIAN_POINT('Ctrl Pts',(-0.294182004219665,-0.0206421863546536,
-1.74191668866673));
#73781=CARTESIAN_POINT('Ctrl Pts',(-0.292041631426675,-0.0409317727345108,
-1.74081576812892));
#73782=CARTESIAN_POINT('Ctrl Pts',(-0.287860331974439,-0.060745940403997,
-1.73971484759111));
#73783=CARTESIAN_POINT('Ctrl Pts',(-0.286227357023594,-0.0684842140784187,
-1.73928489138213));
#73784=CARTESIAN_POINT('Ctrl Pts',(-0.284283610133334,-0.0761502155981999,
-1.73885493517315));
#73785=CARTESIAN_POINT('Ctrl Pts',(-0.282035889300632,-0.0837221425096234,
-1.73842497896416));
#73786=CARTESIAN_POINT('Ctrl Pts',(-0.277340653829632,-0.0995390443690926,
-1.73752684890547));
#73787=CARTESIAN_POINT('Ctrl Pts',(-0.271295716406367,-0.115010317437608,
-1.73662871884677));
#73788=CARTESIAN_POINT('Ctrl Pts',(-0.263972782043712,-0.129892302851643,
-1.73573058878808));
#73789=CARTESIAN_POINT('Ctrl Pts',(-0.256664082356794,-0.144745359939108,
-1.73483420455825));
#73790=CARTESIAN_POINT('Ctrl Pts',(-0.248082602783536,-0.159010671921717,
-1.73393782032842));
#73791=CARTESIAN_POINT('Ctrl Pts',(-0.238348459422095,-0.172463479876506,
-1.73304143609858));
#73792=CARTESIAN_POINT('Ctrl Pts',(-0.228616002021185,-0.18591395779542,
-1.73214520712314));
#73793=CARTESIAN_POINT('Ctrl Pts',(-0.217731696690339,-0.198551540690138,
-1.73124897814769));
#73794=CARTESIAN_POINT('Ctrl Pts',(-0.205859437392401,-0.21017976124376,
-1.73035274917224));
#73795=CARTESIAN_POINT('Ctrl Pts',(-0.193990364349679,-0.221804861036838,
-1.72945676072508));
#73796=CARTESIAN_POINT('Ctrl Pts',(-0.181134436886301,-0.232420589967314,
-1.72856077227793));
#73797=CARTESIAN_POINT('Ctrl Pts',(-0.16749181297899,-0.241868006534579,
-1.72766478383077));
#73798=CARTESIAN_POINT('Ctrl Pts',(-0.153816416765014,-0.251338117682815,
-1.72676664304046));
#73799=CARTESIAN_POINT('Ctrl Pts',(-0.139351218207657,-0.259633880163493,
-1.72586850225015));
#73800=CARTESIAN_POINT('Ctrl Pts',(-0.12432501040221,-0.266640079111319,
-1.72497036145984));
#73801=CARTESIAN_POINT('Ctrl Pts',(-0.110777262324531,-0.272956923624333,
-1.72416059060329));
#73802=CARTESIAN_POINT('Ctrl Pts',(-0.0967742142943387,-0.278225957041598,
-1.72335081974673));
#73803=CARTESIAN_POINT('Ctrl Pts',(-0.0824951304211087,-0.282397226361741,
-1.72254104889018));
#73804=CARTESIAN_POINT('Ctrl Pts',(-0.0666579885938232,-0.287023642482648,
-1.72164292012949));
#73805=CARTESIAN_POINT('Ctrl Pts',(-0.050379814436038,-0.290328456021256,
-1.72074479136879));
#73806=CARTESIAN_POINT('Ctrl Pts',(-0.0339042395189861,-0.292239871582642,
-1.7198466626081));
#73807=CARTESIAN_POINT('Ctrl Pts',(-0.0174606908866978,-0.294147571611225,
-1.718950279688));
#73808=CARTESIAN_POINT('Ctrl Pts',(-0.000821272637496952,-0.294667094103919,
-1.7180538967679));
#73809=CARTESIAN_POINT('Ctrl Pts',(0.0157600296568049,-0.293777571412824,
-1.7171575138478));
#73810=CARTESIAN_POINT('Ctrl Pts',(0.0323384600825974,-0.292888202786358,
-1.71626128618052));
#73811=CARTESIAN_POINT('Ctrl Pts',(0.0488580037869914,-0.290590262706318,
-1.71536505851323));
#73812=CARTESIAN_POINT('Ctrl Pts',(0.0650647250257694,-0.286915007549834,
-1.71446883084595));
#73813=CARTESIAN_POINT('Ctrl Pts',(0.0812670967009878,-0.28324073875917,
-1.71357284370845));
#73814=CARTESIAN_POINT('Ctrl Pts',(0.0971560428253877,-0.278190074333859,
-1.71267685657095));
#73815=CARTESIAN_POINT('Ctrl Pts',(0.112489510217748,-0.271845084728364,
-1.71178086943345));
#73816=CARTESIAN_POINT('Ctrl Pts',(0.127859812149806,-0.265484852988423,
-1.71088272992735));
#73817=CARTESIAN_POINT('Ctrl Pts',(0.142671245731315,-0.257824414314113,
-1.70998459042125));
#73818=CARTESIAN_POINT('Ctrl Pts',(0.156702986152284,-0.248993602590422,
-1.70908645091515));
#73819=CARTESIAN_POINT('Ctrl Pts',(0.169354234344561,-0.241031597343466,
-1.70827667354883));
#73820=CARTESIAN_POINT('Ctrl Pts',(0.18137165371886,-0.232119060944684,
-1.70746689618251));
#73821=CARTESIAN_POINT('Ctrl Pts',(0.192616104667109,-0.222379576901453,
-1.70665711881619));
#73822=CARTESIAN_POINT('Ctrl Pts',(0.20508738163451,-0.211577466279802,
-1.70575899067603));
#73823=CARTESIAN_POINT('Ctrl Pts',(0.21668701521377,-0.199688445134471,
-1.70486086253587));
#73824=CARTESIAN_POINT('Ctrl Pts',(0.227222627668846,-0.186878349402131,
-1.70396273439571));
#73825=CARTESIAN_POINT('Ctrl Pts',(0.237737760048888,-0.174093155090843,
-1.70306635211814));
#73826=CARTESIAN_POINT('Ctrl Pts',(0.247192428763082,-0.160391002328869,
-1.70216996984057));
#73827=CARTESIAN_POINT('Ctrl Pts',(0.255431444012423,-0.145974029915354,
-1.701273587563));
#73828=CARTESIAN_POINT('Ctrl Pts',(0.263669032044348,-0.131559554906379,
-1.70037736056278));
#73829=CARTESIAN_POINT('Ctrl Pts',(0.270690947064961,-0.116431164783314,
-1.69948113356255));
#73830=CARTESIAN_POINT('Ctrl Pts',(0.276385831152967,-0.100819206195466,
-1.69858490656233));
#73831=CARTESIAN_POINT('Ctrl Pts',(0.282079186752439,-0.0852114378069836,
-1.69768892010654));
#73832=CARTESIAN_POINT('Ctrl Pts',(0.286445957303159,-0.0691211061119678,
-1.69679293365075));
#73833=CARTESIAN_POINT('Ctrl Pts',(0.289423928892626,-0.0527961114510928,
-1.69589694719497));
#73834=CARTESIAN_POINT('Ctrl Pts',(0.292409054230803,-0.0364319005297542,
-1.69499880838085));
#73835=CARTESIAN_POINT('Ctrl Pts',(0.293998600557534,-0.0198326875387263,
-1.69410066956674));
#73836=CARTESIAN_POINT('Ctrl Pts',(0.294181999376833,-0.00325441894184345,
-1.69320253075262));
#73837=CARTESIAN_POINT('Ctrl Pts',(0.29434735557396,0.0116928934815336,
-1.69239275008248));
#73838=CARTESIAN_POINT('Ctrl Pts',(0.293370361575628,0.0266226975162987,
-1.69158296941234));
#73839=CARTESIAN_POINT('Ctrl Pts',(0.291279467561646,0.0413510795143722,
-1.6907731887422));
#73840=CARTESIAN_POINT('Ctrl Pts',(0.288960454152482,0.0576863481221683,
-1.68987505989398));
#73841=CARTESIAN_POINT('Ctrl Pts',(0.285255596600586,0.0738781613795155,
-1.68897693104575));
#73842=CARTESIAN_POINT('Ctrl Pts',(0.280200000512142,0.0896749670364913,
-1.68807880219753));
#73843=CARTESIAN_POINT('Ctrl Pts',(0.27515423185183,0.105441065736345,-1.6871824191962));
#73844=CARTESIAN_POINT('Ctrl Pts',(0.268763111840153,0.120812915685593,
-1.68628603619486));
#73845=CARTESIAN_POINT('Ctrl Pts',(0.26111240966032,0.135550542313122,-1.68538965319353));
#73846=CARTESIAN_POINT('Ctrl Pts',(0.253463032670157,0.1502856162141,-1.68449342545605));
#73847=CARTESIAN_POINT('Ctrl Pts',(0.24455482305236,0.164385960117459,-1.68359719771857));
#73848=CARTESIAN_POINT('Ctrl Pts',(0.234521011344578,0.177633147914223,
-1.68270096998109));
#73849=CARTESIAN_POINT('Ctrl Pts',(0.224489892579616,0.190876780340376,
-1.68180498277932));
#73850=CARTESIAN_POINT('Ctrl Pts',(0.213334258091221,0.203267086599783,
-1.68090899557755));
#73851=CARTESIAN_POINT('Ctrl Pts',(0.201228725053308,0.214617427562209,
-1.68001300837578));
#73852=CARTESIAN_POINT('Ctrl Pts',(0.189094111877945,0.225995034525584,
-1.67911486881683));
#73853=CARTESIAN_POINT('Ctrl Pts',(0.17600564058815,0.236327162035444,-1.67821672925788));
#73854=CARTESIAN_POINT('Ctrl Pts',(0.162172680545946,0.245466212918484,
-1.67731858969893));
#73855=CARTESIAN_POINT('Ctrl Pts',(0.149700662234219,0.253706127558396,
-1.67650881268869));
#73856=CARTESIAN_POINT('Ctrl Pts',(0.136624244377117,0.260976533262224,
-1.67569903567845));
#73857=CARTESIAN_POINT('Ctrl Pts',(0.123113404217359,0.267201664856365,
-1.67488925866821));
#73858=CARTESIAN_POINT('Ctrl Pts',(0.108128449066995,0.274105996240668,
-1.67399113005173));
#73859=CARTESIAN_POINT('Ctrl Pts',(0.0925129675321822,0.279767919567134,
-1.67309300143525));
#73860=CARTESIAN_POINT('Ctrl Pts',(0.0764973896053433,0.28408060367362,
-1.67219487281876));
#73861=CARTESIAN_POINT('Ctrl Pts',(0.0605129439601607,0.288384904461258,
-1.67129849005205));
#73862=CARTESIAN_POINT('Ctrl Pts',(0.0441306838838317,0.291344904687799,
-1.67040210728534));
#73863=CARTESIAN_POINT('Ctrl Pts',(0.0275987676766963,0.292902625496474,
-1.66950572451862));
#73864=CARTESIAN_POINT('Ctrl Pts',(0.011069715005662,0.294460076488286,
-1.66860949701669));
#73865=CARTESIAN_POINT('Ctrl Pts',(-0.00560816175754345,0.294615603373687,
-1.66771326951477));
#73866=CARTESIAN_POINT('Ctrl Pts',(-0.0221790909419616,0.293362792332273,
-1.66681704201284));
#73867=CARTESIAN_POINT('Ctrl Pts',(-0.0387455726889244,0.292110317530226,
-1.66592105504756));
#73868=CARTESIAN_POINT('Ctrl Pts',(-0.0552043751603669,0.289450325616551,
-1.66502506808228));
#73869=CARTESIAN_POINT('Ctrl Pts',(-0.0713040100637426,0.285428411600579,
-1.664129081117));
#73870=CARTESIAN_POINT('Ctrl Pts',(-0.0874423198831428,0.281396836049563,
-1.66323094179107));
#73871=CARTESIAN_POINT('Ctrl Pts',(-0.103218974013307,0.275997022269512,
-1.66233280246514));
#73872=CARTESIAN_POINT('Ctrl Pts',(-0.118396460284086,0.269324930506255,
-1.66143466313921));
#73873=CARTESIAN_POINT('Ctrl Pts',(-0.13208074832238,0.263309255454575,
-1.66062488495755));
#73874=CARTESIAN_POINT('Ctrl Pts',(-0.145277828378794,0.256260196441748,
-1.65981510677589));
#73875=CARTESIAN_POINT('Ctrl Pts',(-0.157831904283623,0.248279540015292,
-1.65900532859422));
#73876=CARTESIAN_POINT('Ctrl Pts',(-0.171755685256082,0.239428158763435,
-1.65810720004034));
#73877=CARTESIAN_POINT('Ctrl Pts',(-0.184977075898487,0.229373536686353,
-1.65720907148646));
#73878=CARTESIAN_POINT('Ctrl Pts',(-0.197281409381263,0.218251427286381,
-1.65631094293258));
#73879=CARTESIAN_POINT('Ctrl Pts',(-0.209561824739444,0.207150937911481,
-1.65541456023114));
#73880=CARTESIAN_POINT('Ctrl Pts',(-0.220928096626076,0.194987555580086,
-1.6545181775297));
#73881=CARTESIAN_POINT('Ctrl Pts',(-0.231197005359185,0.181938409119529,
-1.65362179482826));
#73882=CARTESIAN_POINT('Ctrl Pts',(-0.241464135351528,0.168891522981793,
-1.65272556739477));
#73883=CARTESIAN_POINT('Ctrl Pts',(-0.250633749860754,0.154959764532739,
-1.65182933996128));
#73884=CARTESIAN_POINT('Ctrl Pts',(-0.258561838122118,0.140354607572789,
-1.6509331125278));
#73885=CARTESIAN_POINT('Ctrl Pts',(-0.266487798563621,0.125753370491381,
-1.65003712563282));
#73886=CARTESIAN_POINT('Ctrl Pts',(-0.273172526015679,0.11047979467552,
-1.64914113873785));
#73887=CARTESIAN_POINT('Ctrl Pts',(-0.278518039277829,0.0947699414204417,
-1.64824515184287));
#73888=CARTESIAN_POINT('Ctrl Pts',(-0.283876393646943,0.079022349617882,
-1.6473470125889));
#73889=CARTESIAN_POINT('Ctrl Pts',(-0.287888877285267,0.0628371482372673,
-1.64644887333492));
#73890=CARTESIAN_POINT('Ctrl Pts',(-0.29050741046383,0.0464659495286565,
-1.64555073408095));
#73891=CARTESIAN_POINT('Ctrl Pts',(-0.292868327118073,0.0317053820485487,
-1.64474095556071));
#73892=CARTESIAN_POINT('Ctrl Pts',(-0.294096737055979,0.0167941996829556,
-1.64393117704048));
#73893=CARTESIAN_POINT('Ctrl Pts',(-0.294193744601594,0.00191849870784247,
-1.64312139852024));
#73894=CARTESIAN_POINT('Ctrl Pts',(-0.294197888987406,0.00128297449510215,
-1.64308680291648));
#73895=CARTESIAN_POINT('Ctrl Pts',(-0.294199974065043,0.000647436838625386,
-1.64305220731272));
#73896=CARTESIAN_POINT('Ctrl Pts',(-0.294199999759561,1.18942896398017E-5,
-1.64301761170896));
#73897=CARTESIAN_POINT('',(-0.294199892933704,0.000250993619749801,-1.54301761464762));
#73898=CARTESIAN_POINT('Ctrl Pts',(-0.294199999759564,1.18942342971948E-5,
-1.64301761170595));
#73899=CARTESIAN_POINT('Ctrl Pts',(-0.29420066603068,-0.0164681041648284,
-1.64212052700963));
#73900=CARTESIAN_POINT('Ctrl Pts',(-0.292812289007885,-0.0330014442052797,
-1.64122344231331));
#73901=CARTESIAN_POINT('Ctrl Pts',(-0.290034021661079,-0.0493346356944172,
-1.640326357617));
#73902=CARTESIAN_POINT('Ctrl Pts',(-0.287261151236874,-0.0656360991461516,
-1.63943101555235));
#73903=CARTESIAN_POINT('Ctrl Pts',(-0.283103815236798,-0.081737401346229,
-1.63853567348771));
#73904=CARTESIAN_POINT('Ctrl Pts',(-0.277612958384786,-0.0973893491961362,
-1.63764033142306));
#73905=CARTESIAN_POINT('Ctrl Pts',(-0.272123042715187,-0.113038614160944,
-1.63674514282813));
#73906=CARTESIAN_POINT('Ctrl Pts',(-0.26530027190556,-0.128237913644052,
-1.63584995423319));
#73907=CARTESIAN_POINT('Ctrl Pts',(-0.257245611679783,-0.142752706704617,
-1.63495476563826));
#73908=CARTESIAN_POINT('Ctrl Pts',(-0.249193019905193,-0.157263772340298,
-1.63405980692936));
#73909=CARTESIAN_POINT('Ctrl Pts',(-0.239909561963817,-0.17108999201756,
-1.63316484822046));
#73910=CARTESIAN_POINT('Ctrl Pts',(-0.229541638621305,-0.184022488134049,
-1.63226988951156));
#73911=CARTESIAN_POINT('Ctrl Pts',(-0.219148990372253,-0.196985825022335,
-1.63137279654977));
#73912=CARTESIAN_POINT('Ctrl Pts',(-0.207667232146339,-0.209050577778784,
-1.63047570358797));
#73913=CARTESIAN_POINT('Ctrl Pts',(-0.195282607322232,-0.220041685317648,
-1.62957861062618));
#73914=CARTESIAN_POINT('Ctrl Pts',(-0.184509228273474,-0.22960284436474,
-1.62879822989954));
#73915=CARTESIAN_POINT('Ctrl Pts',(-0.173053501126384,-0.238351936559686,
-1.62801784917289));
#73916=CARTESIAN_POINT('Ctrl Pts',(-0.161056510020361,-0.246200001178029,
-1.62723746844625));
#73917=CARTESIAN_POINT('Ctrl Pts',(-0.147249350738978,-0.255232222447381,
-1.62633933983237));
#73918=CARTESIAN_POINT('Ctrl Pts',(-0.132635872021187,-0.263128226214613,
-1.62544121121848));
#73919=CARTESIAN_POINT('Ctrl Pts',(-0.11742829531282,-0.269748467020528,
-1.6245430826046));
#73920=CARTESIAN_POINT('Ctrl Pts',(-0.102250280248761,-0.276355838898824,
-1.62364669984142));
#73921=CARTESIAN_POINT('Ctrl Pts',(-0.0864811503842343,-0.281691997354744,
-1.62275031707825));
#73922=CARTESIAN_POINT('Ctrl Pts',(-0.0703578445262541,-0.285663112273215,
-1.62185393431508));
#73923=CARTESIAN_POINT('Ctrl Pts',(-0.0542373314533323,-0.289633539338307,
-1.6209577068181));
#73924=CARTESIAN_POINT('Ctrl Pts',(-0.0377635176204008,-0.292239152005272,
-1.62006147932112));
#73925=CARTESIAN_POINT('Ctrl Pts',(-0.0211884529455285,-0.293436005735109,
-1.61916525182415));
#73926=CARTESIAN_POINT('Ctrl Pts',(-0.00461783683253826,-0.294632538242799,
-1.6182692648646));
#73927=CARTESIAN_POINT('Ctrl Pts',(0.0120531857089837,-0.294421016148064,
-1.61737327790506));
#73928=CARTESIAN_POINT('Ctrl Pts',(0.0285691559034124,-0.292809568373314,
-1.61647729094551));
#73929=CARTESIAN_POINT('Ctrl Pts',(0.0451248011221824,-0.291194249543522,
-1.61557915162652));
#73930=CARTESIAN_POINT('Ctrl Pts',(0.0615238614247141,-0.288172391760294,
-1.61468101230753));
#73931=CARTESIAN_POINT('Ctrl Pts',(0.0775172982348087,-0.283803996579287,
-1.61378287298854));
#73932=CARTESIAN_POINT('Ctrl Pts',(0.0919372621366972,-0.279865374657852,
-1.61297309478312));
#73933=CARTESIAN_POINT('Ctrl Pts',(0.106027226741348,-0.274832972739917,
-1.61216331657769));
#73934=CARTESIAN_POINT('Ctrl Pts',(0.119618125126485,-0.26878456827211,
-1.61135353837226));
#73935=CARTESIAN_POINT('Ctrl Pts',(0.134691850967059,-0.262076255978323,
-1.61045540976337));
#73936=CARTESIAN_POINT('Ctrl Pts',(0.14924770316629,-0.254074518741827,
-1.60955728115447));
#73937=CARTESIAN_POINT('Ctrl Pts',(0.163053390356407,-0.244882077525656,
-1.60865915254558));
#73938=CARTESIAN_POINT('Ctrl Pts',(0.176832240996848,-0.23570750527913,
-1.6077627697877));
#73939=CARTESIAN_POINT('Ctrl Pts',(0.18986313325126,-0.225347201834048,
-1.60686638702982));
#73940=CARTESIAN_POINT('Ctrl Pts',(0.201938798754428,-0.213949436918209,
-1.60597000427194));
#73941=CARTESIAN_POINT('Ctrl Pts',(0.214012372575882,-0.202553646261796,
-1.60507377678066));
#73942=CARTESIAN_POINT('Ctrl Pts',(0.225130437864743,-0.190121253866431,
-1.60417754928937));
#73943=CARTESIAN_POINT('Ctrl Pts',(0.235119460212498,-0.176840265294371,
-1.60328132179808));
#73944=CARTESIAN_POINT('Ctrl Pts',(0.245105801615888,-0.163562841194412,
-1.60238533484446));
#73945=CARTESIAN_POINT('Ctrl Pts',(0.253963234353235,-0.149437912289678,
-1.60148934789083));
#73946=CARTESIAN_POINT('Ctrl Pts',(0.261560138938136,-0.134684571197532,
-1.6005933609372));
#73947=CARTESIAN_POINT('Ctrl Pts',(0.269175292971096,-0.119895789311185,
-1.59969522162438));
#73948=CARTESIAN_POINT('Ctrl Pts',(0.275523530465425,-0.104476299009142,
-1.59879708231157));
#73949=CARTESIAN_POINT('Ctrl Pts',(0.280520305136338,-0.0886679108032643,
-1.59789894299876));
#73950=CARTESIAN_POINT('Ctrl Pts',(0.285025485244197,-0.0744147893853603,
-1.59708916476526));
#73951=CARTESIAN_POINT('Ctrl Pts',(0.288432605244778,-0.0598462025816209,
-1.59627938653177));
#73952=CARTESIAN_POINT('Ctrl Pts',(0.290715399914207,-0.0451463869287753,
-1.59546960829827));
#73953=CARTESIAN_POINT('Ctrl Pts',(0.293247257584567,-0.0288427563342436,
-1.59457147967584));
#73954=CARTESIAN_POINT('Ctrl Pts',(0.294411451733629,-0.0122733479877298,
-1.5936733510534));
#73955=CARTESIAN_POINT('Ctrl Pts',(0.294168413866012,0.00431094926375149,
-1.59277522243096));
#73956=CARTESIAN_POINT('Ctrl Pts',(0.293925848433877,0.0208630086975991,
-1.59187883965921));
#73957=CARTESIAN_POINT('Ctrl Pts',(0.292281426022063,0.0374291163790788,
-1.59098245688746));
#73958=CARTESIAN_POINT('Ctrl Pts',(0.289247418934938,0.0537547266710246,
-1.59008607411571));
#73959=CARTESIAN_POINT('Ctrl Pts',(0.28621393738113,0.0700775091343299,
-1.58918984661024));
#73960=CARTESIAN_POINT('Ctrl Pts',(0.281791440950735,0.0861590914506403,
-1.58829361910478));
#73961=CARTESIAN_POINT('Ctrl Pts',(0.276043878650335,0.101751742293089,
-1.58739739159931));
#73962=CARTESIAN_POINT('Ctrl Pts',(0.270297858931542,0.117340208241988,
-1.58650140463131));
#73963=CARTESIAN_POINT('Ctrl Pts',(0.263227763301797,0.132439264070395,
-1.58560541766331));
#73964=CARTESIAN_POINT('Ctrl Pts',(0.254946382893199,0.146819555406201,
-1.58470943069531));
#73965=CARTESIAN_POINT('Ctrl Pts',(0.246645108774087,0.161234391387805,
-1.5838112913681));
#73966=CARTESIAN_POINT('Ctrl Pts',(0.2371271578167,0.174926338578149,-1.5829131520409));
#73967=CARTESIAN_POINT('Ctrl Pts',(0.226549925487755,0.187693290400836,
-1.58201501271369));
#73968=CARTESIAN_POINT('Ctrl Pts',(0.217013307385266,0.199204197987944,
-1.58120523455056));
#73969=CARTESIAN_POINT('Ctrl Pts',(0.206616457308168,0.209963271222389,
-1.58039545638742));
#73970=CARTESIAN_POINT('Ctrl Pts',(0.19549997222728,0.219848586211358,-1.57958567822428));
#73971=CARTESIAN_POINT('Ctrl Pts',(0.18317062844361,0.230812433688506,-1.57868754960816));
#73972=CARTESIAN_POINT('Ctrl Pts',(0.169876692927069,0.240770943386101,
-1.57778942099204));
#73973=CARTESIAN_POINT('Ctrl Pts',(0.155807567163121,0.249554887779642,
-1.57689129237592));
#73974=CARTESIAN_POINT('Ctrl Pts',(0.141765790037109,0.258321757273228,
-1.5759949096106));
#73975=CARTESIAN_POINT('Ctrl Pts',(0.126952442259669,0.265918123021017,
-1.57509852684527));
#73976=CARTESIAN_POINT('Ctrl Pts',(0.111588094637542,0.272216342520362,
-1.57420214407994));
#73977=CARTESIAN_POINT('Ctrl Pts',(0.0962264083407792,0.27851347107776,
-1.57330591658096));
#73978=CARTESIAN_POINT('Ctrl Pts',(0.0803146216090893,0.283512551370949,
-1.57240968908198));
#73979=CARTESIAN_POINT('Ctrl Pts',(0.0640955857448739,0.287133063035279,
-1.571513461583));
#73980=CARTESIAN_POINT('Ctrl Pts',(0.0478809028898535,0.290752602994466,
-1.57061747462154));
#73981=CARTESIAN_POINT('Ctrl Pts',(0.0313599096841066,0.292994146872166,
-1.56972148766007));
#73982=CARTESIAN_POINT('Ctrl Pts',(0.0147864844490515,0.293828180877257,
-1.56882550069861));
#73983=CARTESIAN_POINT('Ctrl Pts',(-0.00182675382671472,0.294664218416882,
-1.56792736137788));
#73984=CARTESIAN_POINT('Ctrl Pts',(-0.0184918804152472,0.294085979362492,
-1.56702922205715));
#73985=CARTESIAN_POINT('Ctrl Pts',(-0.0349537417671605,0.292116202796892,
-1.56613108273642));
#73986=CARTESIAN_POINT('Ctrl Pts',(-0.0497960452610043,0.290340217628707,
-1.56532130454104));
#73987=CARTESIAN_POINT('Ctrl Pts',(-0.0644727288162011,0.287433823600362,
-1.56451152634567));
#73988=CARTESIAN_POINT('Ctrl Pts',(-0.0788051284892848,0.28344909899978,
-1.5637017481503));
#73989=CARTESIAN_POINT('Ctrl Pts',(-0.0947012570288975,0.279029623134566,
-1.5628036195343));
#73990=CARTESIAN_POINT('Ctrl Pts',(-0.110275281788735,0.273254643519861,
-1.56190549091831));
#73991=CARTESIAN_POINT('Ctrl Pts',(-0.125282334394243,0.266191616488441,
-1.56100736230232));
#73992=CARTESIAN_POINT('Ctrl Pts',(-0.140260215147669,0.259142319107021,
-1.56011097953715));
#73993=CARTESIAN_POINT('Ctrl Pts',(-0.154672575358626,0.250810217452463,
-1.55921459677198));
#73994=CARTESIAN_POINT('Ctrl Pts',(-0.168292601773028,0.241311500323679,
-1.55831821400681));
#73995=CARTESIAN_POINT('Ctrl Pts',(-0.181910269002808,0.231814428509427,
-1.55742198650804));
#73996=CARTESIAN_POINT('Ctrl Pts',(-0.194735197328667,0.221151550187561,
-1.55652575900927));
#73997=CARTESIAN_POINT('Ctrl Pts',(-0.206568099474672,0.209483317425092,
-1.5556295315105));
#73998=CARTESIAN_POINT('Ctrl Pts',(-0.218397825800741,0.197818216287121,
-1.55473354454926));
#73999=CARTESIAN_POINT('Ctrl Pts',(-0.229235498322907,0.185148859962291,
-1.55383755758803));
#74000=CARTESIAN_POINT('Ctrl Pts',(-0.238918719262039,0.171672611636763,
-1.5529415706268));
#74001=CARTESIAN_POINT('Ctrl Pts',(-0.248625201443618,0.158163990376493,
-1.55204343130634));
#74002=CARTESIAN_POINT('Ctrl Pts',(-0.257171250626507,0.143845266693222,
-1.55114529198588));
#74003=CARTESIAN_POINT('Ctrl Pts',(-0.264437691095471,0.128943194966219,
-1.55024715266542));
#74004=CARTESIAN_POINT('Ctrl Pts',(-0.270989241531935,0.115507225189233,
-1.54943737446905));
#74005=CARTESIAN_POINT('Ctrl Pts',(-0.276501037815482,0.101597794258325,
-1.54862759627268));
#74006=CARTESIAN_POINT('Ctrl Pts',(-0.280920015911495,0.0873932758299257,
-1.54781781807631));
#74007=CARTESIAN_POINT('Ctrl Pts',(-0.286835222818169,0.0683792269507376,
-1.54673385579455));
#74008=CARTESIAN_POINT('Ctrl Pts',(-0.290823615892637,0.0487388113954715,
-1.54564989351278));
#74009=CARTESIAN_POINT('Ctrl Pts',(-0.292784009127529,0.0288299150052643,
-1.54456593123101));
#74010=CARTESIAN_POINT('Ctrl Pts',(-0.293717408566058,0.0193507184942863,
-1.54404982570322));
#74011=CARTESIAN_POINT('Ctrl Pts',(-0.294191736941937,0.00981096533160225,
-1.54353372017542));
#74012=CARTESIAN_POINT('Ctrl Pts',(-0.294199892933704,0.000250993619749801,
-1.54301761464762));
#74013=CARTESIAN_POINT('',(-0.29418954747297,-0.000149745958145899,-1.44301760831983));
#74014=CARTESIAN_POINT('Ctrl Pts',(-0.294003481567088,0.000250771656118091,
-1.54301761170896));
#74015=CARTESIAN_POINT('Ctrl Pts',(-0.293449673493068,-0.0681397340478563,
-1.53932303714008));
#74016=CARTESIAN_POINT('Ctrl Pts',(-0.23560419086501,-0.235384398412292,
-1.5303338192132));
#74017=CARTESIAN_POINT('Ctrl Pts',(0.0428872820869395,-0.345127335346264,
-1.51604995792834));
#74018=CARTESIAN_POINT('Ctrl Pts',(0.313287870803062,-0.151006313006851,
-1.50016602785434));
#74019=CARTESIAN_POINT('Ctrl Pts',(0.296698023090229,0.181445528060777,
-1.48428209778035));
#74020=CARTESIAN_POINT('Ctrl Pts',(0.00831503218110857,0.347682407955339,
-1.46839816770636));
#74021=CARTESIAN_POINT('Ctrl Pts',(-0.248008816545998,0.21583064906809,
-1.45464333901591));
#74022=CARTESIAN_POINT('Ctrl Pts',(-0.293521943642023,0.0585543023250566,
-1.44618315368343));
#74023=CARTESIAN_POINT('Ctrl Pts',(-0.293791839002738,-0.000149480667589675,
-1.44301761170896));
#74024=CARTESIAN_POINT('',(-0.294199947499254,-0.000175759597173832,-1.34301761171257));
#74025=CARTESIAN_POINT('Ctrl Pts',(-0.294199961886584,-0.000149752905057487,
-1.44301760823108));
#74026=CARTESIAN_POINT('Ctrl Pts',(-0.294190615311062,-0.0185117483628317,
-1.44202882723622));
#74027=CARTESIAN_POINT('Ctrl Pts',(-0.292458066504274,-0.0368137300704296,
-1.44104004624135));
#74028=CARTESIAN_POINT('Ctrl Pts',(-0.289060276751152,-0.0547521360729214,
-1.44005126524649));
#74029=CARTESIAN_POINT('Ctrl Pts',(-0.285636324511361,-0.0728286651913199,
-1.43905487078185));
#74030=CARTESIAN_POINT('Ctrl Pts',(-0.280521610325117,-0.0905355406692512,
-1.43805847631721));
#74031=CARTESIAN_POINT('Ctrl Pts',(-0.273824486776581,-0.10758155251502,
-1.43706208185257));
#74032=CARTESIAN_POINT('Ctrl Pts',(-0.272857116959456,-0.110043773383792,
-1.43691815708784));
#74033=CARTESIAN_POINT('Ctrl Pts',(-0.271856810329458,-0.11249224522753,
-1.43677423232312));
#74034=CARTESIAN_POINT('Ctrl Pts',(-0.270823972658315,-0.114926132074338,
-1.4366303075584));
#74035=CARTESIAN_POINT('Ctrl Pts',(-0.264378792282731,-0.130114230049183,
-1.43573217894141));
#74036=CARTESIAN_POINT('Ctrl Pts',(-0.256631377181344,-0.144807024088557,
-1.43483405032443));
#74037=CARTESIAN_POINT('Ctrl Pts',(-0.247680393466925,-0.158770471725914,
-1.43393592170744));
#74038=CARTESIAN_POINT('Ctrl Pts',(-0.238746809356209,-0.172706776150528,
-1.43303953894125));
#74039=CARTESIAN_POINT('Ctrl Pts',(-0.22861466703219,-0.18591585399038,
-1.43214315617505));
#74040=CARTESIAN_POINT('Ctrl Pts',(-0.217428609611005,-0.198187889949475,
-1.43124677340886));
#74041=CARTESIAN_POINT('Ctrl Pts',(-0.206244489775594,-0.210457800215719,
-1.43035054590903));
#74042=CARTESIAN_POINT('Ctrl Pts',(-0.194007309544396,-0.221790371912111,
-1.42945431840921));
#74043=CARTESIAN_POINT('Ctrl Pts',(-0.180902028460652,-0.232008827631238,
-1.42855809090938));
#74044=CARTESIAN_POINT('Ctrl Pts',(-0.167800264688979,-0.242224540830199,
-1.42766210394707));
#74045=CARTESIAN_POINT('Ctrl Pts',(-0.153831493606305,-0.251326253328425,
-1.42676611698477));
#74046=CARTESIAN_POINT('Ctrl Pts',(-0.13921248597049,-0.259178555729281,
-1.42587013002246));
#74047=CARTESIAN_POINT('Ctrl Pts',(-0.124558360238736,-0.267049721100588,
-1.42497199070091));
#74048=CARTESIAN_POINT('Ctrl Pts',(-0.109251590984753,-0.273665128883298,
-1.42407385137937));
#74049=CARTESIAN_POINT('Ctrl Pts',(-0.093532481983476,-0.278936040722619,
-1.42317571205783));
#74050=CARTESIAN_POINT('Ctrl Pts',(-0.0793598571488876,-0.283688387438252,
-1.42236593386669));
#74051=CARTESIAN_POINT('Ctrl Pts',(-0.0648527204541803,-0.287348325831189,
-1.42155615567554));
#74052=CARTESIAN_POINT('Ctrl Pts',(-0.0501948238207512,-0.289886390956188,
-1.4207463774844));
#74053=CARTESIAN_POINT('Ctrl Pts',(-0.0339376850445119,-0.29270137034867,
-1.41984824886741));
#74054=CARTESIAN_POINT('Ctrl Pts',(-0.0173910263376684,-0.294153514652302,
-1.41895012025042));
#74055=CARTESIAN_POINT('Ctrl Pts',(-0.000805010551057393,-0.294198898634942,
-1.41805199163343));
#74056=CARTESIAN_POINT('Ctrl Pts',(0.0157487640751522,-0.29424419439674,
-1.41715560886723));
#74057=CARTESIAN_POINT('Ctrl Pts',(0.0323409617841025,-0.292888089443892,
-1.41625922610103));
#74058=CARTESIAN_POINT('Ctrl Pts',(0.0487168620251309,-0.290138427917476,
-1.41536284333484));
#74059=CARTESIAN_POINT('Ctrl Pts',(0.0650899257250815,-0.287389242671921,
-1.41446661583501));
#74060=CARTESIAN_POINT('Ctrl Pts',(0.0812459793976757,-0.28324705834533,
-1.41357038833518));
#74061=CARTESIAN_POINT('Ctrl Pts',(0.096936217163283,-0.277771506461827,
-1.41267416083535));
#74062=CARTESIAN_POINT('Ctrl Pts',(0.112622243843119,-0.272297424155712,
-1.41177817387303));
#74063=CARTESIAN_POINT('Ctrl Pts',(0.127841958827308,-0.265490955779006,
-1.41088218691072));
#74064=CARTESIAN_POINT('Ctrl Pts',(0.142364081094165,-0.257460887154173,
-1.40998619994841));
#74065=CARTESIAN_POINT('Ctrl Pts',(0.156921088716833,-0.249411528525028,
-1.40908806062687));
#74066=CARTESIAN_POINT('Ctrl Pts',(0.170776473709852,-0.240133106685944,
-1.40818992130532));
#74067=CARTESIAN_POINT('Ctrl Pts',(0.183725423100417,-0.229779478863045,
-1.40729178198377));
#74068=CARTESIAN_POINT('Ctrl Pts',(0.195400423362444,-0.220444466121908,
-1.40648200379265));
#74069=CARTESIAN_POINT('Ctrl Pts',(0.206338661513041,-0.210236277728869,
-1.40567222560153));
#74070=CARTESIAN_POINT('Ctrl Pts',(0.216415787233943,-0.199293369272318,
-1.40486244741041));
#74071=CARTESIAN_POINT('Ctrl Pts',(0.227592372484364,-0.187156540513847,
-1.40396431879342));
#74072=CARTESIAN_POINT('Ctrl Pts',(0.23778054528921,-0.174037784004933,
-1.40306619017643));
#74073=CARTESIAN_POINT('Ctrl Pts',(0.246807810200392,-0.160123529888917,
-1.40216806155943));
#74074=CARTESIAN_POINT('Ctrl Pts',(0.255817527226674,-0.146236323359531,
-1.40127167879323));
#74075=CARTESIAN_POINT('Ctrl Pts',(0.263670334362132,-0.131557308898357,
-1.40037529602703));
#74076=CARTESIAN_POINT('Ctrl Pts',(0.270234772888155,-0.116304804380935,
-1.39947891326083));
#74077=CARTESIAN_POINT('Ctrl Pts',(0.276798074359162,-0.101054941816316,
-1.398582685761));
#74078=CARTESIAN_POINT('Ctrl Pts',(0.282073089550326,-0.0852324901730909,
-1.39768645826116));
#74079=CARTESIAN_POINT('Ctrl Pts',(0.285975087319612,-0.0690788638625486,
-1.39679023076133));
#74080=CARTESIAN_POINT('Ctrl Pts',(0.289876037835979,-0.0529295730061226,
-1.39589424379901));
#74081=CARTESIAN_POINT('Ctrl Pts',(0.292404527066775,-0.0364500560782893,
-1.3949982568367));
#74082=CARTESIAN_POINT('Ctrl Pts',(0.29352663098193,-0.019893639797628,
-1.39410226987438));
#74083=CARTESIAN_POINT('Ctrl Pts',(0.294651430439349,-0.00329745133613088,
-1.39320413055283));
#74084=CARTESIAN_POINT('Ctrl Pts',(0.294363069428234,0.0133752105106759,
-1.39230599123128));
#74085=CARTESIAN_POINT('Ctrl Pts',(0.292679846716762,0.0298688353615089,
-1.39140785190973));
#74086=CARTESIAN_POINT('Ctrl Pts',(0.291162223548715,0.0447397772921781,
-1.39059807371863));
#74087=CARTESIAN_POINT('Ctrl Pts',(0.288511482478781,0.0594647810571047,
-1.38978829552753));
#74088=CARTESIAN_POINT('Ctrl Pts',(0.284776587124312,0.0738643041382596,
-1.38897851733643));
#74089=CARTESIAN_POINT('Ctrl Pts',(0.280634197966181,0.089834879651773,
-1.38808038871944));
#74090=CARTESIAN_POINT('Ctrl Pts',(0.275130908931858,0.105506971000544,
-1.38718226010245));
#74091=CARTESIAN_POINT('Ctrl Pts',(0.268329908128366,0.120634573832806,
-1.38628413148546));
#74092=CARTESIAN_POINT('Ctrl Pts',(0.261542127628087,0.135732770478817,
-1.38538774871926));
#74093=CARTESIAN_POINT('Ctrl Pts',(0.253461902951509,0.150287838827411,
-1.38449136595306));
#74094=CARTESIAN_POINT('Ctrl Pts',(0.244201461264651,0.164070979506459,
-1.38359498318686));
#74095=CARTESIAN_POINT('Ctrl Pts',(0.234942623619273,0.177851732747617,
-1.38269875568703));
#74096=CARTESIAN_POINT('Ctrl Pts',(0.2245043707634,0.190860139205912,-1.3818025281872));
#74097=CARTESIAN_POINT('Ctrl Pts',(0.213043665088906,0.202894151629578,
-1.38090630068737));
#74098=CARTESIAN_POINT('Ctrl Pts',(0.201586035340687,0.214924934257797,
-1.38001031372506));
#74099=CARTESIAN_POINT('Ctrl Pts',(0.189107051380983,0.225981276116504,
-1.37911432676275));
#74100=CARTESIAN_POINT('Ctrl Pts',(0.175801222612858,0.235897372023989,
-1.37821833980044));
#74101=CARTESIAN_POINT('Ctrl Pts',(0.162463430295437,0.245837288591269,
-1.37732020047889));
#74102=CARTESIAN_POINT('Ctrl Pts',(0.148295479221592,0.254631034522214,
-1.37642206115735));
#74103=CARTESIAN_POINT('Ctrl Pts',(0.133522017133855,0.26215550907907,-1.3755239218358));
#74104=CARTESIAN_POINT('Ctrl Pts',(0.120202004170434,0.268939707532015,
-1.37471414364468));
#74105=CARTESIAN_POINT('Ctrl Pts',(0.106390521317145,0.274692542094154,
-1.37390436545356));
#74106=CARTESIAN_POINT('Ctrl Pts',(0.0922649925235385,0.27935785500793,
-1.37309458726244));
#74107=CARTESIAN_POINT('Ctrl Pts',(0.0765983053012701,0.284532174446308,
-1.37219645864545));
#74108=CARTESIAN_POINT('Ctrl Pts',(0.0604448964933684,0.288401027160595,
-1.37129833002846));
#74109=CARTESIAN_POINT('Ctrl Pts',(0.0440457536748395,0.290884189297417,
-1.37040020141147));
#74110=CARTESIAN_POINT('Ctrl Pts',(0.0276784887588075,0.293362524474601,
-1.36950381864527));
#74111=CARTESIAN_POINT('Ctrl Pts',(0.011067201584773,0.294460333145734,
-1.36860743587907));
#74112=CARTESIAN_POINT('Ctrl Pts',(-0.005535001596226,0.294147928358045,
-1.36771105311288));
#74113=CARTESIAN_POINT('Ctrl Pts',(-0.0221343290372297,0.293835577683352,
-1.36681482561304));
#74114=CARTESIAN_POINT('Ctrl Pts',(-0.038723785711801,0.29211346023372,
-1.36591859811321));
#74115=CARTESIAN_POINT('Ctrl Pts',(-0.0550485026375527,0.289003983289787,
-1.36502237061338));
#74116=CARTESIAN_POINT('Ctrl Pts',(-0.0713688381903642,0.285895340894973,
-1.36412638365107));
#74117=CARTESIAN_POINT('Ctrl Pts',(-0.0874237993062656,0.28140023694395,
-1.36323039668875));
#74118=CARTESIAN_POINT('Ctrl Pts',(-0.102968625401473,0.275592275259905,
-1.36233440972644));
#74119=CARTESIAN_POINT('Ctrl Pts',(-0.118550793613721,0.26977036156484,
-1.36143627040489));
#74120=CARTESIAN_POINT('Ctrl Pts',(-0.133619643773714,0.262629594100133,
-1.36053813108334));
#74121=CARTESIAN_POINT('Ctrl Pts',(-0.147949969939373,0.254292049413541,
-1.3596399917618));
#74122=CARTESIAN_POINT('Ctrl Pts',(-0.16087044377021,0.246774772647384,
-1.35883021357068));
#74123=CARTESIAN_POINT('Ctrl Pts',(-0.173190523650776,0.238285497304914,
-1.35802043537957));
#74124=CARTESIAN_POINT('Ctrl Pts',(-0.184766856253945,0.228942894255388,
-1.35721065718845));
#74125=CARTESIAN_POINT('Ctrl Pts',(-0.197440381985434,0.218714808711713,
-1.35632412903712));
#74126=CARTESIAN_POINT('Ctrl Pts',(-0.2093075580526,0.207394171215443,-1.35543760088579));
#74127=CARTESIAN_POINT('Ctrl Pts',(-0.220172996192097,0.195134547806878,
-1.35455107273446));
#74128=CARTESIAN_POINT('Ctrl Pts',(-0.231017282860132,0.1828987898947,-1.35366627036488));
#74129=CARTESIAN_POINT('Ctrl Pts',(-0.240863114080798,0.169728227077772,
-1.3527814679953));
#74130=CARTESIAN_POINT('Ctrl Pts',(-0.249550676841476,0.155814311563351,
-1.35189666562572));
#74131=CARTESIAN_POINT('Ctrl Pts',(-0.258235555527538,0.141904694836574,
-1.35101213662115));
#74132=CARTESIAN_POINT('Ctrl Pts',(-0.265762406856247,0.127252844514462,
-1.35012760761657));
#74133=CARTESIAN_POINT('Ctrl Pts',(-0.27201421930744,0.112079902277633,
-1.34924307861199));
#74134=CARTESIAN_POINT('Ctrl Pts',(-0.278265017748795,0.0969094210091772,
-1.34835869307318));
#74135=CARTESIAN_POINT('Ctrl Pts',(-0.283240895905996,0.0812187746302049,
-1.34747430753438));
#74136=CARTESIAN_POINT('Ctrl Pts',(-0.286873342468991,0.0652481829683322,
-1.34658992199557));
#74137=CARTESIAN_POINT('Ctrl Pts',(-0.29051252747974,0.0492479647185263,
-1.34570389585845));
#74138=CARTESIAN_POINT('Ctrl Pts',(-0.292803179103319,0.0329675687853759,
-1.34481786972132));
#74139=CARTESIAN_POINT('Ctrl Pts',(-0.293728134706627,0.0166560163834503,
-1.34393184358419));
#74140=CARTESIAN_POINT('Ctrl Pts',(-0.294046268245785,0.0110457450620725,
-1.34362709962698));
#74141=CARTESIAN_POINT('Ctrl Pts',(-0.294203297540194,0.0054317968864524,
-1.34332235566977));
#74142=CARTESIAN_POINT('Ctrl Pts',(-0.294199947499254,-0.000175759597174776,
-1.34301761171257));
#74143=CARTESIAN_POINT('',(-0.29419988923003,0.000255297940232041,-1.24301761170896));
#74144=CARTESIAN_POINT('Ctrl Pts',(-0.294199947499215,-0.00017575966358228,
-1.34301761170896));
#74145=CARTESIAN_POINT('Ctrl Pts',(-0.294193751549442,-0.010547013571074,
-1.3424539835108));
#74146=CARTESIAN_POINT('Ctrl Pts',(-0.293639176427434,-0.0209017185291566,
-1.34189035531263));
#74147=CARTESIAN_POINT('Ctrl Pts',(-0.292541208478424,-0.0311974572999702,
-1.34132672711446));
#74148=CARTESIAN_POINT('Ctrl Pts',(-0.290791621714033,-0.0476034810816983,
-1.34042859849746));
#74149=CARTESIAN_POINT('Ctrl Pts',(-0.287652041311442,-0.0639143263184607,
-1.33953046988046));
#74150=CARTESIAN_POINT('Ctrl Pts',(-0.28314880433921,-0.0798773722732269,
-1.33863234126347));
#74151=CARTESIAN_POINT('Ctrl Pts',(-0.278654321101896,-0.0958093880437881,
-1.33773595849726));
#74152=CARTESIAN_POINT('Ctrl Pts',(-0.2728015916199,-0.111394175596688,
-1.33683957573106));
#74153=CARTESIAN_POINT('Ctrl Pts',(-0.265667988492458,-0.126388923131623,
-1.33594319296486));
#74154=CARTESIAN_POINT('Ctrl Pts',(-0.258535621007514,-0.141381073360964,
-1.33504696546503));
#74155=CARTESIAN_POINT('Ctrl Pts',(-0.250123111352777,-0.155782651141836,
-1.33415073796519));
#74156=CARTESIAN_POINT('Ctrl Pts',(-0.240556014087382,-0.169370729721494,
-1.33325451046536));
#74157=CARTESIAN_POINT('Ctrl Pts',(-0.230991484524771,-0.182955161411586,
-1.33235852350305));
#74158=CARTESIAN_POINT('Ctrl Pts',(-0.220273447152277,-0.195725886169684,
-1.33146253654073));
#74159=CARTESIAN_POINT('Ctrl Pts',(-0.208569923466897,-0.207490305857919,
-1.33056654957842));
#74160=CARTESIAN_POINT('Ctrl Pts',(-0.196838285324102,-0.219282986289262,
-1.32966841025687));
#74161=CARTESIAN_POINT('Ctrl Pts',(-0.18411701195124,-0.230063988510944,
-1.32877027093533));
#74162=CARTESIAN_POINT('Ctrl Pts',(-0.170610213622442,-0.239678524293907,
-1.32787213161378));
#74163=CARTESIAN_POINT('Ctrl Pts',(-0.158432246957576,-0.248347158666972,
-1.32706235342268));
#74164=CARTESIAN_POINT('Ctrl Pts',(-0.145616531664977,-0.256067884386416,
-1.32625257523158));
#74165=CARTESIAN_POINT('Ctrl Pts',(-0.132330308425864,-0.262759071150581,
-1.32544279704048));
#74166=CARTESIAN_POINT('Ctrl Pts',(-0.117594498751165,-0.270180296346038,
-1.32454466842349));
#74167=CARTESIAN_POINT('Ctrl Pts',(-0.102185341950397,-0.2763817900475,
-1.3236465398065));
#74168=CARTESIAN_POINT('Ctrl Pts',(-0.0863294138337773,-0.281248772987753,
-1.32274841118951));
#74169=CARTESIAN_POINT('Ctrl Pts',(-0.0705043076775544,-0.286106295115977,
-1.32185202842331));
#74170=CARTESIAN_POINT('Ctrl Pts',(-0.0542348825185319,-0.28963416280787,
-1.32095564565711));
#74171=CARTESIAN_POINT('Ctrl Pts',(-0.0377671304889351,-0.29176580309322,
-1.32005926289092));
#74172=CARTESIAN_POINT('Ctrl Pts',(-0.0213022309104615,-0.293897074147864,
-1.31916303539108));
#74173=CARTESIAN_POINT('Ctrl Pts',(-0.00463984835274561,-0.294632443965077,
-1.31826680789125));
#74174=CARTESIAN_POINT('Ctrl Pts',(0.0119646232211581,-0.293956608687704,
-1.31737058039142));
#74175=CARTESIAN_POINT('Ctrl Pts',(0.0285646383390764,-0.293280954797022,
-1.3164745934291));
#74176=CARTESIAN_POINT('Ctrl Pts',(0.0451059826769823,-0.291194890690062,
-1.31557860646679));
#74177=CARTESIAN_POINT('Ctrl Pts',(0.0613357345627556,-0.287735238831894,
-1.31468261950448));
#74178=CARTESIAN_POINT('Ctrl Pts',(0.077604473909099,-0.284267276123298,
-1.31378448018293));
#74179=CARTESIAN_POINT('Ctrl Pts',(0.0935593538175207,-0.27941932684169,
-1.31288634086138));
#74180=CARTESIAN_POINT('Ctrl Pts',(0.108959668941943,-0.273279034219719,
-1.31198820153983));
#74181=CARTESIAN_POINT('Ctrl Pts',(0.122844863615938,-0.267742838517063,
-1.31117842334871));
#74182=CARTESIAN_POINT('Ctrl Pts',(0.136279078635207,-0.261156942152836,
-1.3103686451576));
#74183=CARTESIAN_POINT('Ctrl Pts',(0.149103072629811,-0.253617652643402,
-1.30955886696648));
#74184=CARTESIAN_POINT('Ctrl Pts',(0.163326221779837,-0.245255792896507,
-1.30866073834949));
#74185=CARTESIAN_POINT('Ctrl Pts',(0.176889245284057,-0.235666995742333,
-1.3077626097325));
#74186=CARTESIAN_POINT('Ctrl Pts',(0.189572885590776,-0.224979468060502,
-1.30686448111551));
#74187=CARTESIAN_POINT('Ctrl Pts',(0.202231870471692,-0.214312715608763,
-1.30596809834931));
#74188=CARTESIAN_POINT('Ctrl Pts',(0.214014224319459,-0.202551925530603,
-1.30507171558311));
#74189=CARTESIAN_POINT('Ctrl Pts',(0.224730678981851,-0.189867748510262,
-1.30417533281691));
#74190=CARTESIAN_POINT('Ctrl Pts',(0.23544527740041,-0.177185768571524,
-1.30327910531708));
#74191=CARTESIAN_POINT('Ctrl Pts',(0.245093793381539,-0.163581287668909,
-1.30238287781725));
#74192=CARTESIAN_POINT('Ctrl Pts',(0.253524949710887,-0.149260644089768,
-1.30148665031742));
#74193=CARTESIAN_POINT('Ctrl Pts',(0.261953843211399,-0.134943844012512,
-1.30059066335511));
#74194=CARTESIAN_POINT('Ctrl Pts',(0.269165633287289,-0.119911950590032,
-1.29969467639279));
#74195=CARTESIAN_POINT('Ctrl Pts',(0.275054189477498,-0.104397475308919,
-1.29879868943048));
#74196=CARTESIAN_POINT('Ctrl Pts',(0.280956891284591,-0.0888457308201479,
-1.29790055010894));
#74197=CARTESIAN_POINT('Ctrl Pts',(0.28552975301188,-0.0728098416726041,
-1.29700241078739));
#74198=CARTESIAN_POINT('Ctrl Pts',(0.288715974741864,-0.0565395961150734,
-1.29610427146584));
#74199=CARTESIAN_POINT('Ctrl Pts',(0.291588728230211,-0.0418700568793609,
-1.29529449327473));
#74200=CARTESIAN_POINT('Ctrl Pts',(0.29333489813115,-0.027010613592972,
-1.29448471508361));
#74201=CARTESIAN_POINT('Ctrl Pts',(0.293949117009706,-0.0121472881423871,
-1.2936749368925));
#74202=CARTESIAN_POINT('Ctrl Pts',(0.294630349917656,0.00433769265518017,
-1.29277680827551));
#74203=CARTESIAN_POINT('Ctrl Pts',(0.293922699000598,0.0209328686897962,
-1.29187867965852));
#74204=CARTESIAN_POINT('Ctrl Pts',(0.291815078002818,0.0373844921084808,
-1.29098055104153));
#74205=CARTESIAN_POINT('Ctrl Pts',(0.289711553959215,0.0538041356088827,
-1.29008416827533));
#74206=CARTESIAN_POINT('Ctrl Pts',(0.286213495329414,0.0700799959941093,
-1.28918778550913));
#74207=CARTESIAN_POINT('Ctrl Pts',(0.281361738894204,0.085960525163762,
-1.28829140274293));
#74208=CARTESIAN_POINT('Ctrl Pts',(0.276510822852879,0.101838303597721,
-1.2873951752431));
#74209=CARTESIAN_POINT('Ctrl Pts',(0.270306854263215,0.117320116637753,
-1.28649894774327));
#74210=CARTESIAN_POINT('Ctrl Pts',(0.262841251640155,0.132167002070247,
-1.28560272024343));
#74211=CARTESIAN_POINT('Ctrl Pts',(0.255377652702027,0.14700990276338,-1.28470673328112));
#74212=CARTESIAN_POINT('Ctrl Pts',(0.246653457261611,0.161217511636139,
-1.28381074631881));
#74213=CARTESIAN_POINT('Ctrl Pts',(0.236806547921958,0.174574622615332,
-1.2829147593565));
#74214=CARTESIAN_POINT('Ctrl Pts',(0.226935984123979,0.187963820335056,
-1.28201662003495));
#74215=CARTESIAN_POINT('Ctrl Pts',(0.21593781269343,0.200497815321246,-1.2811184807134));
#74216=CARTESIAN_POINT('Ctrl Pts',(0.203991171264655,0.211993495291894,
-1.28022034139185));
#74217=CARTESIAN_POINT('Ctrl Pts',(0.19321986946998,0.222358202313284,-1.27941056320074));
#74218=CARTESIAN_POINT('Ctrl Pts',(0.18167839813468,0.231879053300413,-1.27860078500963));
#74219=CARTESIAN_POINT('Ctrl Pts',(0.169520180650363,0.240450719176026,
-1.27779100681851));
#74220=CARTESIAN_POINT('Ctrl Pts',(0.1560354472084,0.249957592172443,-1.27689287820152));
#74221=CARTESIAN_POINT('Ctrl Pts',(0.141705372455059,0.258356972804593,
-1.27599474958453));
#74222=CARTESIAN_POINT('Ctrl Pts',(0.126737197104228,0.265502020463431,
-1.27509662096754));
#74223=CARTESIAN_POINT('Ctrl Pts',(0.111798118032371,0.272633179034582,
-1.27420023820134));
#74224=CARTESIAN_POINT('Ctrl Pts',(0.0962240779494825,0.278514447686267,
-1.27330385543514));
#74225=CARTESIAN_POINT('Ctrl Pts',(0.0802486096345411,0.283043814014232,
-1.27240747266894));
#74226=CARTESIAN_POINT('Ctrl Pts',(0.0642759085001157,0.287572395790908,
-1.27151124516911));
#74227=CARTESIAN_POINT('Ctrl Pts',(0.0479026618057446,0.290749273810779,
-1.27061501766928));
#74228=CARTESIAN_POINT('Ctrl Pts',(0.031379238965604,0.29252176562085,-1.26971879016945));
#74229=CARTESIAN_POINT('Ctrl Pts',(0.0148602508288663,0.294293781713781,
-1.26882280320714));
#74230=CARTESIAN_POINT('Ctrl Pts',(-0.00180804505916306,0.294662086143294,
-1.26792681624482));
#74231=CARTESIAN_POINT('Ctrl Pts',(-0.0183700617464465,0.293625919890312,
-1.26703082928251));
#74232=CARTESIAN_POINT('Ctrl Pts',(-0.0349718640679828,0.292587264536374,
-1.26613268996096));
#74233=CARTESIAN_POINT('Ctrl Pts',(-0.0514660855087487,0.290137475934808,
-1.26523455063941));
#74234=CARTESIAN_POINT('Ctrl Pts',(-0.0676017516749918,0.286327859577919,
-1.26433641131787));
#74235=CARTESIAN_POINT('Ctrl Pts',(-0.0821499517671537,0.282893042541959,
-1.26352663312675));
#74236=CARTESIAN_POINT('Ctrl Pts',(-0.0964063859679396,0.278353632009501,
-1.26271685493564));
#74237=CARTESIAN_POINT('Ctrl Pts',(-0.110199385066545,0.272781479450045,
-1.26190707674452));
#74238=CARTESIAN_POINT('Ctrl Pts',(-0.125497262115504,0.26660138010086,
-1.26100894812753));
#74239=CARTESIAN_POINT('Ctrl Pts',(-0.140322554736792,0.25911063006276,
-1.26011081951054));
#74240=CARTESIAN_POINT('Ctrl Pts',(-0.154439540141873,0.250403810755282,
-1.25921269089355));
#74241=CARTESIAN_POINT('Ctrl Pts',(-0.168529083875808,0.24171391642614,
-1.25831630812735));
#74242=CARTESIAN_POINT('Ctrl Pts',(-0.181912352764208,0.231812999331368,
-1.25741992536115));
#74243=CARTESIAN_POINT('Ctrl Pts',(-0.194377048029768,0.22084203222945,
-1.25652354259495));
#74244=CARTESIAN_POINT('Ctrl Pts',(-0.206839584231116,0.209872965456575,
-1.25562731509512));
#74245=CARTESIAN_POINT('Ctrl Pts',(-0.218383235302948,0.197834698089562,
-1.25473108759529));
#74246=CARTESIAN_POINT('Ctrl Pts',(-0.22882803429704,0.18490908771543,-1.25383486009546));
#74247=CARTESIAN_POINT('Ctrl Pts',(-0.239270030022942,0.171986946431744,
-1.25293887313314));
#74248=CARTESIAN_POINT('Ctrl Pts',(-0.248613269914563,0.158178557521689,
-1.25204288617083));
#74249=CARTESIAN_POINT('Ctrl Pts',(-0.256718595612957,0.143698304327195,
-1.25114689920852));
#74250=CARTESIAN_POINT('Ctrl Pts',(-0.264843392099831,0.12918326635568,
-1.25024875988697));
#74251=CARTESIAN_POINT('Ctrl Pts',(-0.271723969716891,0.11399384711777,
-1.24935062056542));
#74252=CARTESIAN_POINT('Ctrl Pts',(-0.277267424873653,0.0983687709790725,
-1.24845248124387));
#74253=CARTESIAN_POINT('Ctrl Pts',(-0.282265501432228,0.0842809278259624,
-1.24764270305276));
#74254=CARTESIAN_POINT('Ctrl Pts',(-0.286177151682841,0.0698396274544479,
-1.24683292486165));
#74255=CARTESIAN_POINT('Ctrl Pts',(-0.288969719865065,0.055228081635216,
-1.24602314667053));
#74256=CARTESIAN_POINT('Ctrl Pts',(-0.2924246417998,0.0371509043356214,
-1.24502130168334));
#74257=CARTESIAN_POINT('Ctrl Pts',(-0.294183848952715,0.0187397706500721,
-1.24401945669615));
#74258=CARTESIAN_POINT('Ctrl Pts',(-0.29419988923003,0.000255297940232041,
-1.24301761170896));
#74259=CARTESIAN_POINT('',(-0.294152882452219,2.44525333549389E-5,-1.14301761352535));
#74260=CARTESIAN_POINT('Ctrl Pts',(-0.294329728545196,0.000254154008116347,
-1.2430175436321));
#74261=CARTESIAN_POINT('Ctrl Pts',(-0.293605515756253,-0.0789850627824231,
-1.23872476795359));
#74262=CARTESIAN_POINT('Ctrl Pts',(-0.219727723116684,-0.257146121866797,
-1.22913734891706));
#74263=CARTESIAN_POINT('Ctrl Pts',(0.081449915577503,-0.338109609170002,
-1.21425528652256));
#74264=CARTESIAN_POINT('Ctrl Pts',(0.328289982877296,-0.114794963753201,
-1.19837135644858));
#74265=CARTESIAN_POINT('Ctrl Pts',(0.274396781387414,0.213678737652817,
-1.18248742637458));
#74266=CARTESIAN_POINT('Ctrl Pts',(-0.030860291423648,0.34640992909257,
-1.16660349630059));
#74267=CARTESIAN_POINT('Ctrl Pts',(-0.260287732143521,0.193505598037348,
-1.15344689759982));
#74268=CARTESIAN_POINT('Ctrl Pts',(-0.293753616556347,0.047664275140288,
-1.14558494225705));
#74269=CARTESIAN_POINT('Ctrl Pts',(-0.293718471850348,2.47272304220616E-5,
-1.14301763027227));
#74270=CARTESIAN_POINT('',(-0.294199878709568,-0.000267146542919366,-1.04301761170896));
#74271=CARTESIAN_POINT('Ctrl Pts',(-0.294199998986285,2.44227394832766E-5,
-1.14301761170896));
#74272=CARTESIAN_POINT('Ctrl Pts',(-0.294201439091654,-0.0173233034906427,
-1.1420842667241));
#74273=CARTESIAN_POINT('Ctrl Pts',(-0.292664192110059,-0.0346450682093256,
-1.14115092173924));
#74274=CARTESIAN_POINT('Ctrl Pts',(-0.289627608697573,-0.0516670908811927,
-1.14021757675438));
#74275=CARTESIAN_POINT('Ctrl Pts',(-0.286578246409207,-0.068760747453864,
-1.13928030396709));
#74276=CARTESIAN_POINT('Ctrl Pts',(-0.282017105962231,-0.0855514630817754,
-1.13834303117979));
#74277=CARTESIAN_POINT('Ctrl Pts',(-0.276034546441971,-0.101777056209027,
-1.1374057583925));
#74278=CARTESIAN_POINT('Ctrl Pts',(-0.27056623117564,-0.116607942270845,
-1.13654905097921));
#74279=CARTESIAN_POINT('Ctrl Pts',(-0.263911154304513,-0.130966526867975,
-1.13569234356592));
#74280=CARTESIAN_POINT('Ctrl Pts',(-0.256172065381413,-0.14467035950125,
-1.13483563615262));
#74281=CARTESIAN_POINT('Ctrl Pts',(-0.248058796926603,-0.159036762849026,
-1.13393750753563));
#74282=CARTESIAN_POINT('Ctrl Pts',(-0.238707297624362,-0.172764475631579,
-1.13303937891864));
#74283=CARTESIAN_POINT('Ctrl Pts',(-0.228241942290027,-0.185632044054026,
-1.13214125030165));
#74284=CARTESIAN_POINT('Ctrl Pts',(-0.217796930310254,-0.1984745995172,
-1.13124486753545));
#74285=CARTESIAN_POINT('Ctrl Pts',(-0.206242802347557,-0.210459680763422,
-1.13034848476925));
#74286=CARTESIAN_POINT('Ctrl Pts',(-0.193746892091351,-0.221395080805654,
-1.12945210200305));
#74287=CARTESIAN_POINT('Ctrl Pts',(-0.181253146306246,-0.232328586679565,
-1.12855587450322));
#74288=CARTESIAN_POINT('Ctrl Pts',(-0.167818500885398,-0.242212212718823,
-1.12765964700339));
#74289=CARTESIAN_POINT('Ctrl Pts',(-0.153646632351437,-0.250891116556689,
-1.12676341950355));
#74290=CARTESIAN_POINT('Ctrl Pts',(-0.13947856738979,-0.259567691073036,
-1.12586743254124));
#74291=CARTESIAN_POINT('Ctrl Pts',(-0.124574352940194,-0.267039780981758,
-1.12497144557893));
#74292=CARTESIAN_POINT('Ctrl Pts',(-0.109164619826008,-0.273197228716258,
-1.12407545861661));
#74293=CARTESIAN_POINT('Ctrl Pts',(-0.0937178691180572,-0.279369468004716,
-1.12317731929506));
#74294=CARTESIAN_POINT('Ctrl Pts',(-0.077763922306269,-0.284220487099293,
-1.12227917997351));
#74295=CARTESIAN_POINT('Ctrl Pts',(-0.0615515421749449,-0.28768915109174,
-1.12138104065197));
#74296=CARTESIAN_POINT('Ctrl Pts',(-0.046934175424128,-0.290816559485957,
-1.12057126246085));
#74297=CARTESIAN_POINT('Ctrl Pts',(-0.032107343124302,-0.292820856883143,
-1.11976148426974));
#74298=CARTESIAN_POINT('Ctrl Pts',(-0.0172569457007118,-0.293693441917048,
-1.11895170607862));
#74299=CARTESIAN_POINT('Ctrl Pts',(-0.000786303435730034,-0.294661229884554,
-1.11805357746163));
#74300=CARTESIAN_POINT('Ctrl Pts',(0.015818668767146,-0.294242260217352,
-1.11715544884464));
#74301=CARTESIAN_POINT('Ctrl Pts',(0.0323044542012235,-0.292421035903303,
-1.11625732022765));
#74302=CARTESIAN_POINT('Ctrl Pts',(0.0487581933102811,-0.290603351823752,
-1.11536093746145));
#74303=CARTESIAN_POINT('Ctrl Pts',(0.0650924206680926,-0.287388843761867,
-1.11446455469525));
#74304=CARTESIAN_POINT('Ctrl Pts',(0.0810549160959561,-0.282813968142801,
-1.11356817192905));
#74305=CARTESIAN_POINT('Ctrl Pts',(0.0970146465904034,-0.278239884957885,
-1.11267194442922));
#74306=CARTESIAN_POINT('Ctrl Pts',(0.112601999852034,-0.272306068347537,
-1.11177571692939));
#74307=CARTESIAN_POINT('Ctrl Pts',(0.127576460117915,-0.265099767679608,
-1.11087948942956));
#74308=CARTESIAN_POINT('Ctrl Pts',(0.142546901404766,-0.257895401102841,
-1.10998350246725));
#74309=CARTESIAN_POINT('Ctrl Pts',(0.156904067496427,-0.249419581509413,
-1.10908751550494));
#74310=CARTESIAN_POINT('Ctrl Pts',(0.170430387212349,-0.239806428426448,
-1.10819152854263));
#74311=CARTESIAN_POINT('Ctrl Pts',(0.183989200145682,-0.230170182419487,
-1.10729338922108));
#74312=CARTESIAN_POINT('Ctrl Pts',(0.19671254767203,-0.219391628116924,
-1.10639524989953));
#74313=CARTESIAN_POINT('Ctrl Pts',(0.208414230163847,-0.207646691919739,
-1.10549711057798));
#74314=CARTESIAN_POINT('Ctrl Pts',(0.218964672677452,-0.197057251105479,
-1.10468733238687));
#74315=CARTESIAN_POINT('Ctrl Pts',(0.228684779260871,-0.18568308335087,
-1.10387755419576));
#74316=CARTESIAN_POINT('Ctrl Pts',(0.237466568876532,-0.173675757277771,
-1.10306777600465));
#74317=CARTESIAN_POINT('Ctrl Pts',(0.247206491053715,-0.160358378175512,
-1.10216964738766));
#74318=CARTESIAN_POINT('Ctrl Pts',(0.255853787998005,-0.146176527344347,
-1.10127151877066));
#74319=CARTESIAN_POINT('Ctrl Pts',(0.263258037584813,-0.131334860745323,
-1.10037339015367));
#74320=CARTESIAN_POINT('Ctrl Pts',(0.27064789422749,-0.116522044507928,
-1.09947700738747));
#74321=CARTESIAN_POINT('Ctrl Pts',(0.276799091300331,-0.101052628874886,
-1.09858062462128));
#74322=CARTESIAN_POINT('Ctrl Pts',(0.281605570911589,-0.0851583374165925,
-1.09768424185508));
#74323=CARTESIAN_POINT('Ctrl Pts',(0.286411217971558,-0.0692667990778169,
-1.09678801435524));
#74324=CARTESIAN_POINT('Ctrl Pts',(0.289872330758011,-0.0529512709053253,
-1.09589178685541));
#74325=CARTESIAN_POINT('Ctrl Pts',(0.291931881098733,-0.0364611683597093,
-1.09499555935558));
#74326=CARTESIAN_POINT('Ctrl Pts',(0.29399087867899,-0.0199754915746974,
-1.09409957239327));
#74327=CARTESIAN_POINT('Ctrl Pts',(0.294648973157355,-0.00331612040945406,
-1.09320358543095));
#74328=CARTESIAN_POINT('Ctrl Pts',(0.293900961216667,0.0132614100275669,
-1.09230759846864));
#74329=CARTESIAN_POINT('Ctrl Pts',(0.293151152385537,0.0298787633663042,
-1.09140945914709));
#74330=CARTESIAN_POINT('Ctrl Pts',(0.290988552942633,0.0464130903492512,
-1.09051131982554));
#74331=CARTESIAN_POINT('Ctrl Pts',(0.287460096417958,0.0626125623767172,
-1.08961318050399));
#74332=CARTESIAN_POINT('Ctrl Pts',(0.284278778026232,0.0772182909543078,
-1.08880340231288));
#74333=CARTESIAN_POINT('Ctrl Pts',(0.279987959623469,0.0915515055811006,
-1.08799362412177));
#74334=CARTESIAN_POINT('Ctrl Pts',(0.27465649665164,0.105439313574433,-1.08718384593065));
#74335=CARTESIAN_POINT('Ctrl Pts',(0.268743347201612,0.120842343592982,
-1.08628571731366));
#74336=CARTESIAN_POINT('Ctrl Pts',(0.261511527442603,0.135795651602018,
-1.08538758869667));
#74337=CARTESIAN_POINT('Ctrl Pts',(0.253051505499328,0.150061905773996,
-1.08448946007968));
#74338=CARTESIAN_POINT('Ctrl Pts',(0.244607928790882,0.164300428114831,
-1.08359307731348));
#74339=CARTESIAN_POINT('Ctrl Pts',(0.234941230979866,0.177853840928105,
-1.08269669454728));
#74340=CARTESIAN_POINT('Ctrl Pts',(0.224188671836702,0.190507426154718,
-1.08180031178108));
#74341=CARTESIAN_POINT('Ctrl Pts',(0.213437975191185,0.20315881959867,-1.08090408428125));
#74342=CARTESIAN_POINT('Ctrl Pts',(0.201602261081292,0.214910059225903,
-1.08000785678142));
#74343=CARTESIAN_POINT('Ctrl Pts',(0.188860230143771,0.225578042969704,
-1.07911162928159));
#74344=CARTESIAN_POINT('Ctrl Pts',(0.176121619026007,0.236243163545008,
-1.07821564231928));
#74345=CARTESIAN_POINT('Ctrl Pts',(0.162477787969324,0.24582510541816,-1.07731965535696));
#74346=CARTESIAN_POINT('Ctrl Pts',(0.148140668069825,0.254181003349632,
-1.07642366839465));
#74347=CARTESIAN_POINT('Ctrl Pts',(0.133769107231204,0.262556973999614,
-1.0755255290731));
#74348=CARTESIAN_POINT('Ctrl Pts',(0.11870163131608,0.269700640752514,-1.07462738975156));
#74349=CARTESIAN_POINT('Ctrl Pts',(0.103175313090077,0.275514962876365,
-1.07372925043001));
#74350=CARTESIAN_POINT('Ctrl Pts',(0.0891765118060444,0.280757257851153,
-1.07291947223889));
#74351=CARTESIAN_POINT('Ctrl Pts',(0.0748054148313669,0.284919437069828,
-1.07210969404778));
#74352=CARTESIAN_POINT('Ctrl Pts',(0.0602446383824871,0.287965663831929,
-1.07129991585666));
#74353=CARTESIAN_POINT('Ctrl Pts',(0.044095216037158,0.291344247571163,
-1.07040178723967));
#74354=CARTESIAN_POINT('Ctrl Pts',(0.0276090592174151,0.293370887834,-1.06950365862268));
#74355=CARTESIAN_POINT('Ctrl Pts',(0.0110346520815367,0.293992987082072,
-1.06860553000569));
#74356=CARTESIAN_POINT('Ctrl Pts',(-0.00550753645972035,0.294613877046257,
-1.06770914723949));
#74357=CARTESIAN_POINT('Ctrl Pts',(-0.0221368555162454,0.293835549883038,
-1.06681276447329));
#74358=CARTESIAN_POINT('Ctrl Pts',(-0.0385984658186121,0.291656987635218,
-1.06591638170709));
#74359=CARTESIAN_POINT('Ctrl Pts',(-0.0550572247336882,0.289478802745662,
-1.06502015420726));
#74360=CARTESIAN_POINT('Ctrl Pts',(-0.0713475433805044,0.285900915149179,
-1.06412392670743));
#74361=CARTESIAN_POINT('Ctrl Pts',(-0.0872186927898397,0.280974268622647,
-1.0632276992076));
#74362=CARTESIAN_POINT('Ctrl Pts',(-0.103085582558728,0.276048944353394,
-1.06233171224529));
#74363=CARTESIAN_POINT('Ctrl Pts',(-0.118532773472252,0.269775824806875,
-1.06143572528297));
#74364=CARTESIAN_POINT('Ctrl Pts',(-0.13332534158677,0.262255587720779,
-1.06053973832066));
#74365=CARTESIAN_POINT('Ctrl Pts',(-0.148153444727958,0.254717285358705,
-1.05964159899911));
#74366=CARTESIAN_POINT('Ctrl Pts',(-0.162323087557588,0.245926265667551,
-1.05874345967756));
#74367=CARTESIAN_POINT('Ctrl Pts',(-0.175624230913873,0.236029170900358,
-1.05784532035602));
#74368=CARTESIAN_POINT('Ctrl Pts',(-0.187616775442742,0.227105776382856,
-1.0570355421649));
#74369=CARTESIAN_POINT('Ctrl Pts',(-0.19890336621151,0.217284114969341,
-1.05622576397379));
#74370=CARTESIAN_POINT('Ctrl Pts',(-0.209354913611055,0.206698234503606,
-1.05541598578268));
#74371=CARTESIAN_POINT('Ctrl Pts',(-0.220789690983753,0.195116486673142,
-1.05453002765775));
#74372=CARTESIAN_POINT('Ctrl Pts',(-0.231301783831298,0.182540831427682,
-1.05364406953283));
#74373=CARTESIAN_POINT('Ctrl Pts',(-0.240714390826723,0.169145564674099,
-1.05275811140791));
#74374=CARTESIAN_POINT('Ctrl Pts',(-0.250111460747171,0.155772409038507,
-1.05187361570437));
#74375=CARTESIAN_POINT('Ctrl Pts',(-0.258412117491872,0.14158293958677,
-1.05098912000084));
#74376=CARTESIAN_POINT('Ctrl Pts',(-0.265479047062119,0.126785312915138,
-1.05010462429731));
#74377=CARTESIAN_POINT('Ctrl Pts',(-0.272538744393056,0.112002830016518,
-1.04922103377962));
#74378=CARTESIAN_POINT('Ctrl Pts',(-0.278366846345738,0.0966141464632306,
-1.04833744326193));
#74379=CARTESIAN_POINT('Ctrl Pts',(-0.282872149058977,0.0808516375020071,
-1.04745385274424));
#74380=CARTESIAN_POINT('Ctrl Pts',(-0.287382011663733,0.0650731750443189,
-1.04656936792995));
#74381=CARTESIAN_POINT('Ctrl Pts',(-0.290566177837302,0.0489209165269241,
-1.04568488311565));
#74382=CARTESIAN_POINT('Ctrl Pts',(-0.292383595975706,0.0326415809101696,
-1.04480039830136));
#74383=CARTESIAN_POINT('Ctrl Pts',(-0.293604671656364,0.0217039213816084,
-1.04420613610389));
#74384=CARTESIAN_POINT('Ctrl Pts',(-0.294209845691427,0.0107091693839332,
-1.04361187390643));
#74385=CARTESIAN_POINT('Ctrl Pts',(-0.294199878709568,-0.000267146542919366,
-1.04301761170896));
#74386=CARTESIAN_POINT('',(-0.294610924535095,0.000132059026951131,-0.943017611708961));
#74387=CARTESIAN_POINT('Ctrl Pts',(-0.294240133891941,-0.000267183096411164,
-1.04301761170896));
#74388=CARTESIAN_POINT('Ctrl Pts',(-0.294438591321936,-0.0217302969209736,
-1.04185575970887));
#74389=CARTESIAN_POINT('Ctrl Pts',(-0.282496855002347,-0.140783416643142,
-1.03539926435079));
#74390=CARTESIAN_POINT('Ctrl Pts',(-0.120486255734729,-0.32624417043023,
-1.0236481256347));
#74391=CARTESIAN_POINT('Ctrl Pts',(0.208874931436236,-0.278070961407654,
-1.00776419556071));
#74392=CARTESIAN_POINT('Ctrl Pts',(0.346894182589261,0.0248318876930918,
-0.991880265486725));
#74393=CARTESIAN_POINT('Ctrl Pts',(0.167137604763724,0.30498724175696,-0.975996335412736));
#74394=CARTESIAN_POINT('Ctrl Pts',(-0.165727020336765,0.305756032305122,
-0.96011240533875));
#74395=CARTESIAN_POINT('Ctrl Pts',(-0.291026760911973,0.112443587052818,
-0.94911949743749));
#74396=CARTESIAN_POINT('Ctrl Pts',(-0.294652539398193,0.00756385498649065,
-0.943421232894227));
#74397=CARTESIAN_POINT('Ctrl Pts',(-0.294610924535095,0.000132059026951131,
-0.943017611708961));
#74398=CARTESIAN_POINT('',(-0.294199939966062,0.0001879467097956,-0.843017611708961));
#74399=CARTESIAN_POINT('Ctrl Pts',(-0.294610924535095,0.000132059026951131,
-0.943017611708961));
#74400=CARTESIAN_POINT('Ctrl Pts',(-0.294106641743307,-0.0899253516050796,
-0.938126589536231));
#74401=CARTESIAN_POINT('Ctrl Pts',(-0.201793630053243,-0.278365916406644,
-0.927940924005507));
#74402=CARTESIAN_POINT('Ctrl Pts',(0.118977978713689,-0.326797241637504,
-0.912460615116783));
#74403=CARTESIAN_POINT('Ctrl Pts',(0.339122181698526,-0.0771254979932333,
-0.896576685042796));
#74404=CARTESIAN_POINT('Ctrl Pts',(0.248610173587816,0.243197816909012,
-0.880692754968808));
#74405=CARTESIAN_POINT('Ctrl Pts',(-0.0696436300603406,0.340737378860454,
-0.864808824894819));
#74406=CARTESIAN_POINT('Ctrl Pts',(-0.270824704599013,0.171070735517887,
-0.852250483857469));
#74407=CARTESIAN_POINT('Ctrl Pts',(-0.294056291535214,0.0366892411458219,
-0.844986786178113));
#74408=CARTESIAN_POINT('Ctrl Pts',(-0.293843481306506,0.000189946096159861,
-0.843017731856754));
#74409=CARTESIAN_POINT('',(-0.294199911255592,-0.000228510835546836,-0.743017611708961));
#74410=CARTESIAN_POINT('Ctrl Pts',(-0.294199939966062,0.0001879467097956,
-0.843017611708961));
#74411=CARTESIAN_POINT('Ctrl Pts',(-0.294210637410069,-0.0165571582630485,
-0.84211534212027));
#74412=CARTESIAN_POINT('Ctrl Pts',(-0.292787354432935,-0.0333086725148639,
-0.841213072531579));
#74413=CARTESIAN_POINT('Ctrl Pts',(-0.289953095943817,-0.0498080530897905,
-0.840310802942887));
#74414=CARTESIAN_POINT('Ctrl Pts',(-0.287118308400922,-0.0663105135036494,
-0.839408364933025));
#74415=CARTESIAN_POINT('Ctrl Pts',(-0.282872182508555,-0.0825599868555481,
-0.838505926923162));
#74416=CARTESIAN_POINT('Ctrl Pts',(-0.277288867949126,-0.0983083094732686,
-0.837603488913299));
#74417=CARTESIAN_POINT('Ctrl Pts',(-0.271690760042274,-0.114098358274486,
-0.83669865983647));
#74418=CARTESIAN_POINT('Ctrl Pts',(-0.264748691178075,-0.12938388715599,
-0.83579383075964));
#74419=CARTESIAN_POINT('Ctrl Pts',(-0.25658515980724,-0.143936429602423,
-0.834889001682811));
#74420=CARTESIAN_POINT('Ctrl Pts',(-0.251027385457895,-0.153843875712752,
-0.834272989370822));
#74421=CARTESIAN_POINT('Ctrl Pts',(-0.24490447653641,-0.163412053346357,
-0.833656977058833));
#74422=CARTESIAN_POINT('Ctrl Pts',(-0.238266280902253,-0.172576995526659,
-0.833040964746843));
#74423=CARTESIAN_POINT('Ctrl Pts',(-0.228587978458964,-0.185939223334441,
-0.832142836129852));
#74424=CARTESIAN_POINT('Ctrl Pts',(-0.217751176956386,-0.198527486544028,
-0.831244707512861));
#74425=CARTESIAN_POINT('Ctrl Pts',(-0.2059043801134,-0.210135732920692,
-0.83034657889587));
#74426=CARTESIAN_POINT('Ctrl Pts',(-0.194080611976174,-0.221721414304158,
-0.829450196129672));
#74427=CARTESIAN_POINT('Ctrl Pts',(-0.18125125798943,-0.232330265407811,
-0.828553813363473));
#74428=CARTESIAN_POINT('Ctrl Pts',(-0.167604216956642,-0.241790128951434,
-0.827657430597274));
#74429=CARTESIAN_POINT('Ctrl Pts',(-0.15395953978733,-0.251248353910849,
-0.826761203097442));
#74430=CARTESIAN_POINT('Ctrl Pts',(-0.139498074974674,-0.259557493260994,
-0.825864975597611));
#74431=CARTESIAN_POINT('Ctrl Pts',(-0.124439628937701,-0.266586606471232,
-0.824968748097779));
#74432=CARTESIAN_POINT('Ctrl Pts',(-0.109385224420607,-0.273613833145455,
-0.824072761135466));
#74433=CARTESIAN_POINT('Ctrl Pts',(-0.0937348787508753,-0.279361390572878,
-0.823176774173154));
#74434=CARTESIAN_POINT('Ctrl Pts',(-0.077730153362982,-0.283745772229592,
-0.822280787210842));
#74435=CARTESIAN_POINT('Ctrl Pts',(-0.0616869810780328,-0.288140686142631,
-0.821382647889294));
#74436=CARTESIAN_POINT('Ctrl Pts',(-0.0452885024722155,-0.291165699290351,
-0.820484508567746));
#74437=CARTESIAN_POINT('Ctrl Pts',(-0.0287887795740931,-0.292788056741791,
-0.819586369246198));
#74438=CARTESIAN_POINT('Ctrl Pts',(-0.013912339536594,-0.294250802722118,
-0.818776591055083));
#74439=CARTESIAN_POINT('Ctrl Pts',(0.00104585912408567,-0.294574000697571,
-0.817966812863969));
#74440=CARTESIAN_POINT('Ctrl Pts',(0.0159001287712503,-0.293770022134761,
-0.817157034672855));
#74441=CARTESIAN_POINT('Ctrl Pts',(0.032375065736724,-0.292878325911485,
-0.816258906055864));
#74442=CARTESIAN_POINT('Ctrl Pts',(0.0488274363991952,-0.290593563992844,
-0.815360777438873));
#74443=CARTESIAN_POINT('Ctrl Pts',(0.0650035903451627,-0.286928864428517,
-0.814462648821881));
#74444=CARTESIAN_POINT('Ctrl Pts',(0.0811482998513748,-0.283271288586248,
-0.813566266055683));
#74445=CARTESIAN_POINT('Ctrl Pts',(0.0970170808011161,-0.278239207841102,
-0.812669883289484));
#74446=CARTESIAN_POINT('Ctrl Pts',(0.112363417068298,-0.271897227835695,
-0.811773500523286));
#74447=CARTESIAN_POINT('Ctrl Pts',(0.127707095129677,-0.26555634635229,
-0.810877273023454));
#74448=CARTESIAN_POINT('Ctrl Pts',(0.142527758658779,-0.257906268324901,
-0.809981045523622));
#74449=CARTESIAN_POINT('Ctrl Pts',(0.156596237021465,-0.249060752730568,
-0.80908481802379));
#74450=CARTESIAN_POINT('Ctrl Pts',(0.170660939560616,-0.2402176111745,-0.808188831061478));
#74451=CARTESIAN_POINT('Ctrl Pts',(0.183973193177795,-0.230180099550807,
-0.807292844099165));
#74452=CARTESIAN_POINT('Ctrl Pts',(0.196331900105423,-0.219105967515707,
-0.806396857136852));
#74453=CARTESIAN_POINT('Ctrl Pts',(0.2087202953858,-0.208005232961414,-0.805498717815304));
#74454=CARTESIAN_POINT('Ctrl Pts',(0.220149994497017,-0.195863454534986,
-0.804600578493756));
#74455=CARTESIAN_POINT('Ctrl Pts',(0.230455776249653,-0.182876393209102,
-0.803702439172208));
#74456=CARTESIAN_POINT('Ctrl Pts',(0.239747650133175,-0.171167030556742,
-0.802892660981095));
#74457=CARTESIAN_POINT('Ctrl Pts',(0.248126161128695,-0.158771357214758,
-0.802082882789981));
#74458=CARTESIAN_POINT('Ctrl Pts',(0.255501069045883,-0.145852129625902,
-0.801273104598868));
#74459=CARTESIAN_POINT('Ctrl Pts',(0.263680612432935,-0.131523356470108,
-0.800374975981877));
#74460=CARTESIAN_POINT('Ctrl Pts',(0.270677196238584,-0.116458548058095,
-0.799476847364886));
#74461=CARTESIAN_POINT('Ctrl Pts',(0.276364382311608,-0.100877986644874,
-0.798578718747895));
#74462=CARTESIAN_POINT('Ctrl Pts',(0.2820405131993,-0.0853277119132891,
-0.797682335981696));
#74463=CARTESIAN_POINT('Ctrl Pts',(0.286411968193491,-0.0692643863955023,
-0.796785953215497));
#74464=CARTESIAN_POINT('Ctrl Pts',(0.289399437368199,-0.0529301960224028,
-0.795889570449299));
#74465=CARTESIAN_POINT('Ctrl Pts',(0.292386389070347,-0.0365988349656295,
-0.794993342949467));
#74466=CARTESIAN_POINT('Ctrl Pts',(0.293989636672718,-0.0199974688051808,
-0.794097115449635));
#74467=CARTESIAN_POINT('Ctrl Pts',(0.294180579340224,-0.00338034599560538,
-0.793200887949803));
#74468=CARTESIAN_POINT('Ctrl Pts',(0.294371470760837,0.0132323169625333,
-0.792304900987491));
#74469=CARTESIAN_POINT('Ctrl Pts',(0.293150811423026,0.0298599363575227,
-0.791408914025179));
#74470=CARTESIAN_POINT('Ctrl Pts',(0.290542184814657,0.0462480144776586,
-0.790512927062866));
#74471=CARTESIAN_POINT('Ctrl Pts',(0.287927291707098,0.0626754603930689,
-0.789614787741318));
#74472=CARTESIAN_POINT('Ctrl Pts',(0.283917922998519,0.0788614348057531,
-0.78871664841977));
#74473=CARTESIAN_POINT('Ctrl Pts',(0.278589050834782,0.0945609896044634,
-0.787818509098222));
#74474=CARTESIAN_POINT('Ctrl Pts',(0.27378444607258,0.108715984025915,-0.787008730907108));
#74475=CARTESIAN_POINT('Ctrl Pts',(0.267908051971126,0.122475350162049,
-0.786198952715993));
#74476=CARTESIAN_POINT('Ctrl Pts',(0.261047741200663,0.135675041234678,
-0.785389174524879));
#74477=CARTESIAN_POINT('Ctrl Pts',(0.253438939812809,0.150314877695889,
-0.784491045907888));
#74478=CARTESIAN_POINT('Ctrl Pts',(0.244570447328582,0.164359466636021,
-0.783592917290896));
#74479=CARTESIAN_POINT('Ctrl Pts',(0.234558862771465,0.177583163321744,
-0.782694788673905));
#74480=CARTESIAN_POINT('Ctrl Pts',(0.224566739494724,0.190781154778953,
-0.781798405907706));
#74481=CARTESIAN_POINT('Ctrl Pts',(0.213436354176119,0.203160757685192,
-0.780902023141507));
#74482=CARTESIAN_POINT('Ctrl Pts',(0.201328255727785,0.214524062626102,
-0.780005640375309));
#74483=CARTESIAN_POINT('Ctrl Pts',(0.189222254575975,0.225885399279419,
-0.779109412875477));
#74484=CARTESIAN_POINT('Ctrl Pts',(0.176139415511457,0.23623020876436,-0.778213185375645));
#74485=CARTESIAN_POINT('Ctrl Pts',(0.162277907574574,0.245396659947152,
-0.777316957875813));
#74486=CARTESIAN_POINT('Ctrl Pts',(0.148420119912662,0.254560650956125,
-0.776420970913501));
#74487=CARTESIAN_POINT('Ctrl Pts',(0.133784744616074,0.262546483780045,
-0.775524983951189));
#74488=CARTESIAN_POINT('Ctrl Pts',(0.118598442542028,0.269236047784477,
-0.774628996988877));
#74489=CARTESIAN_POINT('Ctrl Pts',(0.103375659605088,0.275941681604068,
-0.773730857667329));
#74490=CARTESIAN_POINT('Ctrl Pts',(0.0876000447295265,0.28134453089193,
-0.77283271834578));
#74491=CARTESIAN_POINT('Ctrl Pts',(0.0715180844246416,0.285374847525548,
-0.771934579024232));
#74492=CARTESIAN_POINT('Ctrl Pts',(0.0570183064805997,0.289008651808344,
-0.771124800833118));
#74493=CARTESIAN_POINT('Ctrl Pts',(0.0422701359153877,0.291527308014146,
-0.770315022642004));
#74494=CARTESIAN_POINT('Ctrl Pts',(0.0274590616356825,0.292915755694513,
-0.76950524445089));
#74495=CARTESIAN_POINT('Ctrl Pts',(0.0110320328456341,0.294455689232631,
-0.768607115833899));
#74496=CARTESIAN_POINT('Ctrl Pts',(-0.00557746613309338,0.294614374820569,
-0.767708987216908));
#74497=CARTESIAN_POINT('Ctrl Pts',(-0.0221166107849677,0.293367509324714,
-0.766810858599917));
#74498=CARTESIAN_POINT('Ctrl Pts',(-0.0386236053881212,0.292123067580951,
-0.765914475833718));
#74499=CARTESIAN_POINT('Ctrl Pts',(-0.0550597320389343,0.289478490833111,
-0.765018093067519));
#74500=CARTESIAN_POINT('Ctrl Pts',(-0.0711716553977228,0.285461443049579,
-0.76412171030132));
#74501=CARTESIAN_POINT('Ctrl Pts',(-0.087280787940025,0.281445091076406,
-0.763225482801488));
#74502=CARTESIAN_POINT('Ctrl Pts',(-0.10306505022713,0.276056879376787,
-0.762329255301656));
#74503=CARTESIAN_POINT('Ctrl Pts',(-0.118281038042414,0.269375641140043,
-0.761433027801824));
#74504=CARTESIAN_POINT('Ctrl Pts',(-0.133492942055352,0.262696196073529,
-0.760537040839512));
#74505=CARTESIAN_POINT('Ctrl Pts',(-0.148136153775957,0.254724741597121,
-0.759641053877199));
#74506=CARTESIAN_POINT('Ctrl Pts',(-0.161988569885976,0.245587750562393,
-0.758745066914886));
#74507=CARTESIAN_POINT('Ctrl Pts',(-0.175874262569211,0.236428810450427,
-0.757846927593338));
#74508=CARTESIAN_POINT('Ctrl Pts',(-0.188964716392098,0.226099201365837,
-0.75694878827179));
#74509=CARTESIAN_POINT('Ctrl Pts',(-0.201067726873874,0.214768268628709,
-0.756050648950241));
#74510=CARTESIAN_POINT('Ctrl Pts',(-0.211980013753884,0.204552100607387,
-0.755240870759128));
#74511=CARTESIAN_POINT('Ctrl Pts',(-0.222089754032483,0.193522807085033,
-0.754431092568016));
#74512=CARTESIAN_POINT('Ctrl Pts',(-0.231283761504503,0.181828110214918,
-0.753621314376903));
#74513=CARTESIAN_POINT('Ctrl Pts',(-0.241474226249487,0.168865928432832,
-0.752723771479215));
#74514=CARTESIAN_POINT('Ctrl Pts',(-0.250605506517791,0.155001277538237,
-0.751826228581528));
#74515=CARTESIAN_POINT('Ctrl Pts',(-0.258519464715208,0.140432639950129,
-0.750928685683841));
#74516=CARTESIAN_POINT('Ctrl Pts',(-0.266417571192186,0.125893183457555,
-0.750032940571629));
#74517=CARTESIAN_POINT('Ctrl Pts',(-0.273102759340644,0.110653192248535,
-0.749137195459416));
#74518=CARTESIAN_POINT('Ctrl Pts',(-0.278460120528183,0.0949399877576883,
-0.748241450347204));
#74519=CARTESIAN_POINT('Ctrl Pts',(-0.283815402235698,0.0792328824066407,
-0.747346052921848));
#74520=CARTESIAN_POINT('Ctrl Pts',(-0.28784357491228,0.06305365788728,-0.746450655496491));
#74521=CARTESIAN_POINT('Ctrl Pts',(-0.29047804426146,0.0466491779352817,
-0.745555258071135));
#74522=CARTESIAN_POINT('Ctrl Pts',(-0.292966827964608,0.031151862555292,
-0.74470937595041));
#74523=CARTESIAN_POINT('Ctrl Pts',(-0.294212092345077,0.015454226645856,
-0.743863493829685));
#74524=CARTESIAN_POINT('Ctrl Pts',(-0.294199911255592,-0.000228510835546836,
-0.743017611708961));
#74525=CARTESIAN_POINT('',(-0.294239083931547,-6.59995884866487E-5,-0.643017618234341));
#74526=CARTESIAN_POINT('Ctrl Pts',(-0.293927949640422,-0.000230402592847965,
-0.743017498174503));
#74527=CARTESIAN_POINT('Ctrl Pts',(-0.294163664674453,-0.0328317124483067,
-0.741257460217307));
#74528=CARTESIAN_POINT('Ctrl Pts',(-0.274118262007807,-0.163224061780253,
-0.734202778902116));
#74529=CARTESIAN_POINT('Ctrl Pts',(-0.0830108472164328,-0.33772976742521,
-0.721853454228924));
#74530=CARTESIAN_POINT('Ctrl Pts',(0.2388379518494,-0.252801561144413,-0.70596952415494));
#74531=CARTESIAN_POINT('Ctrl Pts',(0.341896895248078,0.0637080024832001,
-0.690085594080949));
#74532=CARTESIAN_POINT('Ctrl Pts',(0.131757823904318,0.321857223626676,
-0.674201664006963));
#74533=CARTESIAN_POINT('Ctrl Pts',(-0.195025494420267,0.28561555261962,
-0.658512362449674));
#74534=CARTESIAN_POINT('Ctrl Pts',(-0.294378853579128,0.0937945108140465,
-0.648117704250382));
#74535=CARTESIAN_POINT('Ctrl Pts',(-0.294665467861281,-6.47855231172667E-5,
-0.643017689409085));
#74536=CARTESIAN_POINT('',(-0.294199877779988,0.000268168305674158,-0.543017614213059));
#74537=CARTESIAN_POINT('Ctrl Pts',(-0.294199992571974,-6.61108953689901E-5,
-0.64301761170896));
#74538=CARTESIAN_POINT('Ctrl Pts',(-0.294199189049575,-0.00364186466996765,
-0.642823009092302));
#74539=CARTESIAN_POINT('Ctrl Pts',(-0.294133197574971,-0.00721680678781066,
-0.642628406475644));
#74540=CARTESIAN_POINT('Ctrl Pts',(-0.294002091898632,-0.0107893447080197,
-0.642433803858986));
#74541=CARTESIAN_POINT('Ctrl Pts',(-0.293397013910515,-0.0272772963938953,
-0.641535675242002));
#74542=CARTESIAN_POINT('Ctrl Pts',(-0.291398688453342,-0.0437669092700093,
-0.640637546625017));
#74543=CARTESIAN_POINT('Ctrl Pts',(-0.288015830853521,-0.0600043429907858,
-0.639739418008031));
#74544=CARTESIAN_POINT('Ctrl Pts',(-0.284639549109885,-0.076210213151524,
-0.638843035241837));
#74545=CARTESIAN_POINT('Ctrl Pts',(-0.2798841721558,-0.0921640978031815,
-0.637946652475643));
#74546=CARTESIAN_POINT('Ctrl Pts',(-0.273810009185595,-0.107618394662737,
-0.637050269709449));
#74547=CARTESIAN_POINT('Ctrl Pts',(-0.267736898347642,-0.123070014616149,
-0.636154042209622));
#74548=CARTESIAN_POINT('Ctrl Pts',(-0.260345694194456,-0.138021464794339,
-0.635257814709794));
#74549=CARTESIAN_POINT('Ctrl Pts',(-0.251746153444292,-0.152241631054067,
-0.634361587209967));
#74550=CARTESIAN_POINT('Ctrl Pts',(-0.243148920715475,-0.16645798077891,
-0.633465600247659));
#74551=CARTESIAN_POINT('Ctrl Pts',(-0.233344414141136,-0.179942764306823,
-0.63256961328535));
#74552=CARTESIAN_POINT('Ctrl Pts',(-0.222486862627603,-0.192492171160612,
-0.631673626323042));
#74553=CARTESIAN_POINT('Ctrl Pts',(-0.211603228869283,-0.205071724470632,
-0.630775487001498));
#74554=CARTESIAN_POINT('Ctrl Pts',(-0.199662037835341,-0.216710829325282,
-0.629877347679954));
#74555=CARTESIAN_POINT('Ctrl Pts',(-0.186856147860634,-0.227240885420482,
-0.62897920835841));
#74556=CARTESIAN_POINT('Ctrl Pts',(-0.175310132480963,-0.236734968991724,
-0.628169430167271));
#74557=CARTESIAN_POINT('Ctrl Pts',(-0.163062027674604,-0.245327762063203,
-0.627359651976133));
#74558=CARTESIAN_POINT('Ctrl Pts',(-0.150272996084734,-0.25292620790997,
-0.626549873784995));
#74559=CARTESIAN_POINT('Ctrl Pts',(-0.136088623894679,-0.261353678215219,
-0.625651745168002));
#74560=CARTESIAN_POINT('Ctrl Pts',(-0.121147757200918,-0.268611166753299,
-0.624753616551009));
#74561=CARTESIAN_POINT('Ctrl Pts',(-0.105668446312975,-0.27456842399264,
-0.623855487934016));
#74562=CARTESIAN_POINT('Ctrl Pts',(-0.0902192252881835,-0.280514101061752,
-0.622959105167816));
#74563=CARTESIAN_POINT('Ctrl Pts',(-0.074234343983909,-0.285164220968364,
-0.622062722401616));
#74564=CARTESIAN_POINT('Ctrl Pts',(-0.0579545725884968,-0.288435274396327,
-0.621166339635415));
#74565=CARTESIAN_POINT('Ctrl Pts',(-0.0416776210832624,-0.291705761230865,
-0.620270112135582));
#74566=CARTESIAN_POINT('Ctrl Pts',(-0.0251066440073686,-0.293597448313603,
-0.619373884635749));
#74567=CARTESIAN_POINT('Ctrl Pts',(-0.00849535403158956,-0.294077317996268,
-0.618477657135916));
#74568=CARTESIAN_POINT('Ctrl Pts',(0.00811147765822207,-0.294557058887232,
-0.617581670173603));
#74569=CARTESIAN_POINT('Ctrl Pts',(0.0247578090422277,-0.293625722525604,
-0.616685683211289));
#74570=CARTESIAN_POINT('Ctrl Pts',(0.0411887707946803,-0.291302463361406,
-0.615789696248976));
#74571=CARTESIAN_POINT('Ctrl Pts',(0.057659203358391,-0.288973623213857,
-0.614891556927427));
#74572=CARTESIAN_POINT('Ctrl Pts',(0.0739124495281757,-0.285246319352522,
-0.613993417605877));
#74573=CARTESIAN_POINT('Ctrl Pts',(0.0897022945351791,-0.280191253173835,
-0.613095278284328));
#74574=CARTESIAN_POINT('Ctrl Pts',(0.103938696194503,-0.275633516698123,
-0.612285500093223));
#74575=CARTESIAN_POINT('Ctrl Pts',(0.11779816678023,-0.269997273340848,
-0.611475721902117));
#74576=CARTESIAN_POINT('Ctrl Pts',(0.131115156296434,-0.26336752986912,
-0.610665943711012));
#74577=CARTESIAN_POINT('Ctrl Pts',(0.145885088986696,-0.25601445170442,
-0.609767815094021));
#74578=CARTESIAN_POINT('Ctrl Pts',(0.160081768982187,-0.247391522124171,
-0.608869686477029));
#74579=CARTESIAN_POINT('Ctrl Pts',(0.173477558121661,-0.237611398775702,
-0.607971557860038));
#74580=CARTESIAN_POINT('Ctrl Pts',(0.186847307506206,-0.227850286775689,
-0.607075175093839));
#74581=CARTESIAN_POINT('Ctrl Pts',(0.199418585369986,-0.216936853845187,
-0.60617879232764));
#74582=CARTESIAN_POINT('Ctrl Pts',(0.210990720430563,-0.205028183165612,
-0.60528240956144));
#74583=CARTESIAN_POINT('Ctrl Pts',(0.222560851031175,-0.193121575238805,
-0.604386182061608));
#74584=CARTESIAN_POINT('Ctrl Pts',(0.233131594441001,-0.180220600661988,
-0.603489954561776));
#74585=CARTESIAN_POINT('Ctrl Pts',(0.242537698025042,-0.166520584423409,
-0.602593727061943));
#74586=CARTESIAN_POINT('Ctrl Pts',(0.251941277115219,-0.15282424511722,
-0.601697740099631));
#74587=CARTESIAN_POINT('Ctrl Pts',(0.260180397664757,-0.138329948703318,
-0.600801753137317));
#74588=CARTESIAN_POINT('Ctrl Pts',(0.26713302548195,-0.123262267936543,
-0.599905766175004));
#74589=CARTESIAN_POINT('Ctrl Pts',(0.274102355051873,-0.108158391261543,
-0.599007626853456));
#74590=CARTESIAN_POINT('Ctrl Pts',(0.279778710291323,-0.0924791120585587,
-0.598109487531907));
#74591=CARTESIAN_POINT('Ctrl Pts',(0.284088067458913,-0.076469666714718,
-0.597211348210358));
#74592=CARTESIAN_POINT('Ctrl Pts',(0.287973459589404,-0.0620352695335585,
-0.596401570019246));
#74593=CARTESIAN_POINT('Ctrl Pts',(0.290748191564568,-0.047333125929017,
-0.595591791828134));
#74594=CARTESIAN_POINT('Ctrl Pts',(0.29239397973829,-0.0325484348748805,
-0.594782013637021));
#74595=CARTESIAN_POINT('Ctrl Pts',(0.294219330769654,-0.0161506678384154,
-0.593883885020032));
#74596=CARTESIAN_POINT('Ctrl Pts',(0.294666815678933,0.000453560378974142,
-0.592985756403042));
#74597=CARTESIAN_POINT('Ctrl Pts',(0.293707738630449,0.01701188609731,-0.592087627786052));
#74598=CARTESIAN_POINT('Ctrl Pts',(0.29275052590896,0.0335380244813062,
-0.591191245019855));
#74599=CARTESIAN_POINT('Ctrl Pts',(0.290392157559051,0.0500176526379714,
-0.590294862253658));
#74600=CARTESIAN_POINT('Ctrl Pts',(0.28665588810683,0.0661969924821711,
-0.58939847948746));
#74601=CARTESIAN_POINT('Ctrl Pts',(0.282920265830129,0.0823735298323798,
-0.58850225198763));
#74602=CARTESIAN_POINT('Ctrl Pts',(0.277807342070079,0.0982491013777121,
-0.5876060244878));
#74603=CARTESIAN_POINT('Ctrl Pts',(0.271391705529629,0.113578968870645,
-0.58670979698797));
#74604=CARTESIAN_POINT('Ctrl Pts',(0.264977790874861,0.12890472199719,-0.585813810025659));
#74605=CARTESIAN_POINT('Ctrl Pts',(0.257262173147636,0.143684335627127,
-0.584917823063348));
#74606=CARTESIAN_POINT('Ctrl Pts',(0.248367443912265,0.157693540782392,
-0.584021836101037));
#74607=CARTESIAN_POINT('Ctrl Pts',(0.239451347566184,0.171736399152903,
-0.583123696779491));
#74608=CARTESIAN_POINT('Ctrl Pts',(0.229350930809813,0.185004495718582,
-0.582225557457944));
#74609=CARTESIAN_POINT('Ctrl Pts',(0.218232171105833,0.197302710306864,
-0.581327418136398));
#74610=CARTESIAN_POINT('Ctrl Pts',(0.2082073020186,0.208390996638846,-0.580517639945277));
#74611=CARTESIAN_POINT('Ctrl Pts',(0.197355474857132,0.218690997190556,
-0.579707861754155));
#74612=CARTESIAN_POINT('Ctrl Pts',(0.185822421239044,0.228086974123599,
-0.578898083563034));
#74613=CARTESIAN_POINT('Ctrl Pts',(0.173031059839962,0.238508094204016,
-0.577999954946041));
#74614=CARTESIAN_POINT('Ctrl Pts',(0.159319426709137,0.247883154434612,
-0.577101826329047));
#74615=CARTESIAN_POINT('Ctrl Pts',(0.144884055439066,0.256051265334756,
-0.576203697712053));
#74616=CARTESIAN_POINT('Ctrl Pts',(0.13047674474283,0.264203498438984,-0.575307314945851));
#74617=CARTESIAN_POINT('Ctrl Pts',(0.115349136709595,0.271152996309403,
-0.57441093217965));
#74618=CARTESIAN_POINT('Ctrl Pts',(0.0997271091365789,0.276781761868915,
-0.573514549413449));
#74619=CARTESIAN_POINT('Ctrl Pts',(0.0841077875230671,0.282409552445405,
-0.572618321913614));
#74620=CARTESIAN_POINT('Ctrl Pts',(0.0679949407084323,0.286716747448818,
-0.571722094413779));
#74621=CARTESIAN_POINT('Ctrl Pts',(0.0516346710183764,0.289633390251925,
-0.570825866913945));
#74622=CARTESIAN_POINT('Ctrl Pts',(0.0352787922432276,0.292549250260458,
-0.56992987995163));
#74623=CARTESIAN_POINT('Ctrl Pts',(0.0186764037705013,0.294075170627267,
-0.569033892989315));
#74624=CARTESIAN_POINT('Ctrl Pts',(0.00208242171189055,0.294192629954956,
-0.568137906027));
#74625=CARTESIAN_POINT('Ctrl Pts',(-0.0145514227688778,0.29431037144598,
-0.567239766705449));
#74626=CARTESIAN_POINT('Ctrl Pts',(-0.031176025375635,0.293012914973375,
-0.566341627383898));
#74627=CARTESIAN_POINT('Ctrl Pts',(-0.0475374527293351,0.290333998332965,
-0.565443488062348));
#74628=CARTESIAN_POINT('Ctrl Pts',(-0.0622892030740751,0.287918640025931,
-0.564633709871247));
#74629=CARTESIAN_POINT('Ctrl Pts',(-0.0768266663317771,0.284381080679814,
-0.563823931680146));
#74630=CARTESIAN_POINT('Ctrl Pts',(-0.0909735945032452,0.279781066377193,
-0.563014153489045));
#74631=CARTESIAN_POINT('Ctrl Pts',(-0.10666401587162,0.274679169920671,
-0.562116024872055));
#74632=CARTESIAN_POINT('Ctrl Pts',(-0.121974090607168,0.268236946000983,
-0.561217896255065));
#74633=CARTESIAN_POINT('Ctrl Pts',(-0.136662092220278,0.260532363728532,
-0.560319767638075));
#74634=CARTESIAN_POINT('Ctrl Pts',(-0.151321542177458,0.252842758209756,
-0.559423384871878));
#74635=CARTESIAN_POINT('Ctrl Pts',(-0.165360595717803,0.243895969895092,
-0.558527002105681));
#74636=CARTESIAN_POINT('Ctrl Pts',(-0.178557669351488,0.2338178750989,-0.557630619339483));
#74637=CARTESIAN_POINT('Ctrl Pts',(-0.191752457062515,0.223741525973444,
-0.556734391839652));
#74638=CARTESIAN_POINT('Ctrl Pts',(-0.204104895076259,0.212534696074499,
-0.555838164339822));
#74639=CARTESIAN_POINT('Ctrl Pts',(-0.215422811901074,0.20036629485179,
-0.554941936839991));
#74640=CARTESIAN_POINT('Ctrl Pts',(-0.226737691122558,0.188201159492991,
-0.55404594987768));
#74641=CARTESIAN_POINT('Ctrl Pts',(-0.237018069032917,0.175075552231487,
-0.553149962915369));
#74642=CARTESIAN_POINT('Ctrl Pts',(-0.246110223385262,0.16119366595886,
-0.552253975953058));
#74643=CARTESIAN_POINT('Ctrl Pts',(-0.255224219107198,0.147278432319156,
-0.551355836631511));
#74644=CARTESIAN_POINT('Ctrl Pts',(-0.263143876780439,0.132603970575454,
-0.550457697309964));
#74645=CARTESIAN_POINT('Ctrl Pts',(-0.269759925279849,0.117401970652158,
-0.549559557988417));
#74646=CARTESIAN_POINT('Ctrl Pts',(-0.275725070839879,0.103695580447476,
-0.548749779797297));
#74647=CARTESIAN_POINT('Ctrl Pts',(-0.280630983945998,0.0895610772477883,
-0.547940001606177));
#74648=CARTESIAN_POINT('Ctrl Pts',(-0.284432353931144,0.0751789600698787,
-0.547130223415058));
#74649=CARTESIAN_POINT('Ctrl Pts',(-0.289819157500309,0.0547985076411929,
-0.545982711842335));
#74650=CARTESIAN_POINT('Ctrl Pts',(-0.29301713345713,0.0338165504288796,
-0.544835200269612));
#74651=CARTESIAN_POINT('Ctrl Pts',(-0.293928020853791,0.0126474723551179,
-0.543687688696889));
#74652=CARTESIAN_POINT('Ctrl Pts',(-0.294105321143291,0.0085270029264237,
-0.543464330535613));
#74653=CARTESIAN_POINT('Ctrl Pts',(-0.29419611198676,0.00439951374748332,
-0.543240972374336));
#74654=CARTESIAN_POINT('Ctrl Pts',(-0.294199877779988,0.000268168305674158,
-0.543017614213059));
#74655=CARTESIAN_POINT('',(-0.293740379894572,-8.66858914495487E-5,-0.443017611708961));
#74656=CARTESIAN_POINT('Ctrl Pts',(-0.294123668879967,0.000268052534830647,
-0.543017611708961));
#74657=CARTESIAN_POINT('Ctrl Pts',(-0.293474798752899,-0.0722898843115431,
-0.539093838919663));
#74658=CARTESIAN_POINT('Ctrl Pts',(-0.229758782171269,-0.243774078952558,
-0.52987542277237));
#74659=CARTESIAN_POINT('Ctrl Pts',(0.0577531094952713,-0.342953021424431,
-0.515362363267081));
#74660=CARTESIAN_POINT('Ctrl Pts',(0.319517415892196,-0.137334691550856,
-0.499478433193093));
#74661=CARTESIAN_POINT('Ctrl Pts',(0.288584649791592,0.194090433725029,
-0.483594503119105));
#74662=CARTESIAN_POINT('Ctrl Pts',(-0.00670892406185214,0.347717107571907,
-0.467710573045117));
#74663=CARTESIAN_POINT('Ctrl Pts',(-0.252926720822328,0.207297382700659,
-0.454184942575068));
#74664=CARTESIAN_POINT('Ctrl Pts',(-0.293596658076772,0.0543905486936848,
-0.445953955463017));
#74665=CARTESIAN_POINT('Ctrl Pts',(-0.293740379894572,-8.66858914495487E-5,
-0.443017611708961));
#74666=CARTESIAN_POINT('',(-0.29419991353495,-0.000225557150586184,-0.343017611708961));
#74667=CARTESIAN_POINT('Ctrl Pts',(-0.293740379894572,-8.66858914495487E-5,
-0.443017611708961));
#74668=CARTESIAN_POINT('Ctrl Pts',(-0.293855808854661,-0.0438396152167057,
-0.440659312105021));
#74669=CARTESIAN_POINT('Ctrl Pts',(-0.26416141467023,-0.185673782245695,
-0.433006369143085));
#74670=CARTESIAN_POINT('Ctrl Pts',(-0.0444810415613786,-0.344925547768942,
-0.420058782823151));
#74671=CARTESIAN_POINT('Ctrl Pts',(0.265767271674193,-0.224321095562353,
-0.404174852749164));
#74672=CARTESIAN_POINT('Ctrl Pts',(0.332556860575699,0.101774903304964,
-0.388290922675176));
#74673=CARTESIAN_POINT('Ctrl Pts',(0.0947044659440234,0.334639000613301,
-0.372406992601186));
#74674=CARTESIAN_POINT('Ctrl Pts',(-0.213699718700967,0.264631837550187,
-0.357315928117542));
#74675=CARTESIAN_POINT('Ctrl Pts',(-0.293736313474251,0.0827916910960814,
-0.347519506991888));
#74676=CARTESIAN_POINT('Ctrl Pts',(-0.294441777086296,-0.000223575550274286,
-0.343017729224232));
#74677=CARTESIAN_POINT('',(-0.29419991634408,0.000221862877645845,-0.24301761170896));
#74678=CARTESIAN_POINT('Ctrl Pts',(-0.29419991353495,-0.000225557150586184,
-0.343017611708961));
#74679=CARTESIAN_POINT('Ctrl Pts',(-0.294188713844001,-0.0148335981727865,
-0.342224785290378));
#74680=CARTESIAN_POINT('Ctrl Pts',(-0.293089342069403,-0.0294007671736424,
-0.341431958871795));
#74681=CARTESIAN_POINT('Ctrl Pts',(-0.29092083917617,-0.0438030288111792,
-0.340639132453213));
#74682=CARTESIAN_POINT('Ctrl Pts',(-0.288464318379726,-0.0601181812321631,
-0.339741003798971));
#74683=CARTESIAN_POINT('Ctrl Pts',(-0.284623211539265,-0.0762782108728595,
-0.338842875144731));
#74684=CARTESIAN_POINT('Ctrl Pts',(-0.279434741703112,-0.0920318701826437,
-0.337944746490492));
#74685=CARTESIAN_POINT('Ctrl Pts',(-0.274256357608409,-0.107754906333829,
-0.337048363686894));
#74686=CARTESIAN_POINT('Ctrl Pts',(-0.267735991130414,-0.123072376354419,
-0.336151980883297));
#74687=CARTESIAN_POINT('Ctrl Pts',(-0.259961429584258,-0.13774503667468,
-0.3352555980797));
#74688=CARTESIAN_POINT('Ctrl Pts',(-0.252188214706506,-0.152415155474376,
-0.334359370542789));
#74689=CARTESIAN_POINT('Ctrl Pts',(-0.243161558549959,-0.1664399642326,
-0.333463143005878));
#74690=CARTESIAN_POINT('Ctrl Pts',(-0.233016526606927,-0.179602166824466,
-0.332566915468968));
#74691=CARTESIAN_POINT('Ctrl Pts',(-0.222874217479038,-0.192760836825726,
-0.331670928469684));
#74692=CARTESIAN_POINT('Ctrl Pts',(-0.211614620329887,-0.205056739759931,
-0.330774941470401));
#74693=CARTESIAN_POINT('Ctrl Pts',(-0.199413918088511,-0.216304713939823,
-0.329878954471117));
#74694=CARTESIAN_POINT('Ctrl Pts',(-0.18718390707091,-0.227579708233123,
-0.328980815113556));
#74695=CARTESIAN_POINT('Ctrl Pts',(-0.174008877979855,-0.237801226458742,
-0.328082675755996));
#74696=CARTESIAN_POINT('Ctrl Pts',(-0.160099435859406,-0.246823440210811,
-0.327184536398434));
#74697=CARTESIAN_POINT('Ctrl Pts',(-0.147558441841444,-0.254958024453204,
-0.326374758392032));
#74698=CARTESIAN_POINT('Ctrl Pts',(-0.134421234178903,-0.262118040987156,
-0.325564980385629));
#74699=CARTESIAN_POINT('Ctrl Pts',(-0.12085842293712,-0.268229158752646,
-0.324755202379225));
#74700=CARTESIAN_POINT('Ctrl Pts',(-0.105815845975774,-0.275007027858723,
-0.323857073830079));
#74701=CARTESIAN_POINT('Ctrl Pts',(-0.0901532297157309,-0.280537222332166,
-0.322958945280933));
#74702=CARTESIAN_POINT('Ctrl Pts',(-0.0741018957635367,-0.284714855678888,
-0.322060816731786));
#74703=CARTESIAN_POINT('Ctrl Pts',(-0.058081763614756,-0.28888436822426,
-0.321164434033202));
#74704=CARTESIAN_POINT('Ctrl Pts',(-0.041675154056802,-0.291706277349181,
-0.320268051334619));
#74705=CARTESIAN_POINT('Ctrl Pts',(-0.0251307049024998,-0.293124696453751,
-0.319371668636035));
#74706=CARTESIAN_POINT('Ctrl Pts',(-0.00858912146014023,-0.29454286986984,
-0.318475441202494));
#74707=CARTESIAN_POINT('Ctrl Pts',(0.00808947256198928,-0.294557915573295,
-0.317579213768953));
#74708=CARTESIAN_POINT('Ctrl Pts',(0.0246492605735305,-0.293165574297492,
-0.316682986335411));
#74709=CARTESIAN_POINT('Ctrl Pts',(0.0412046041325439,-0.291773606709727,
-0.315786999438783));
#74710=CARTESIAN_POINT('Ctrl Pts',(0.0576404169237435,-0.288975079092548,
-0.314891012542154));
#74711=CARTESIAN_POINT('Ctrl Pts',(0.0737056036461875,-0.284817703085941,
-0.313995025645526));
#74712=CARTESIAN_POINT('Ctrl Pts',(0.0898093825526996,-0.280650340129113,
-0.313096886387282));
#74713=CARTESIAN_POINT('Ctrl Pts',(0.105539994156818,-0.275117833834768,
-0.312198747129039));
#74714=CARTESIAN_POINT('Ctrl Pts',(0.120660743004417,-0.268318141573808,
-0.311300607870795));
#74715=CARTESIAN_POINT('Ctrl Pts',(0.134293882340815,-0.262187416636001,
-0.310490829348942));
#74716=CARTESIAN_POINT('Ctrl Pts',(0.147431126491672,-0.255027447201575,
-0.309681050827089));
#74717=CARTESIAN_POINT('Ctrl Pts',(0.159917541947552,-0.246941328613606,
-0.308871272305237));
#74718=CARTESIAN_POINT('Ctrl Pts',(0.173766275644202,-0.237972981904336,
-0.307973143683613));
#74719=CARTESIAN_POINT('Ctrl Pts',(0.186902508977528,-0.227807353077535,
-0.30707501506199));
#74720=CARTESIAN_POINT('Ctrl Pts',(0.199112726159464,-0.216581998978092,
-0.306176886440368));
#74721=CARTESIAN_POINT('Ctrl Pts',(0.211299208177787,-0.205378465589304,
-0.305280503670556));
#74722=CARTESIAN_POINT('Ctrl Pts',(0.222562626326639,-0.193119776588182,
-0.304384120900744));
#74723=CARTESIAN_POINT('Ctrl Pts',(0.232721259355089,-0.179984597797094,
-0.303487738130932));
#74724=CARTESIAN_POINT('Ctrl Pts',(0.242878132744514,-0.166851694230745,
-0.302591510629068));
#74725=CARTESIAN_POINT('Ctrl Pts',(0.251930076201204,-0.152843193943631,
-0.301695283127205));
#74726=CARTESIAN_POINT('Ctrl Pts',(0.259734865287855,-0.138171776256586,
-0.300799055625341));
#74727=CARTESIAN_POINT('Ctrl Pts',(0.267537559648178,-0.123504296229425,
-0.29990306866186));
#74728=CARTESIAN_POINT('Ctrl Pts',(0.274093401812665,-0.108174956070798,
-0.299007081698379));
#74729=CARTESIAN_POINT('Ctrl Pts',(0.279306402374615,-0.0924206340194086,
-0.298111094734898));
#74730=CARTESIAN_POINT('Ctrl Pts',(0.284531925710785,-0.0766284666204733,
-0.297212955413612));
#74731=CARTESIAN_POINT('Ctrl Pts',(0.28840793992237,-0.060410041305751,
-0.296314816092326));
#74732=CARTESIAN_POINT('Ctrl Pts',(0.290888486288432,-0.0440173664003702,
-0.295416676771039));
#74733=CARTESIAN_POINT('Ctrl Pts',(0.293124990440893,-0.0292374429135893,
-0.294606898591108));
#74734=CARTESIAN_POINT('Ctrl Pts',(0.294227760402243,-0.0143164490420228,
-0.293797120411177));
#74735=CARTESIAN_POINT('Ctrl Pts',(0.294199467913316,0.000559535094423254,
-0.292987342231246));
#74736=CARTESIAN_POINT('Ctrl Pts',(0.294168088578443,0.0170585602944459,
-0.292089213376404));
#74737=CARTESIAN_POINT('Ctrl Pts',(0.292744361366393,0.0336076926620605,
-0.291191084521562));
#74738=CARTESIAN_POINT('Ctrl Pts',(0.289928169666838,0.049952942191998,
-0.29029295566672));
#74739=CARTESIAN_POINT('Ctrl Pts',(0.287117452289695,0.0662664186129436,
-0.289396572661394));
#74740=CARTESIAN_POINT('Ctrl Pts',(0.282919710800327,0.0823760166686528,
-0.288500189656069));
#74741=CARTESIAN_POINT('Ctrl Pts',(0.277386608168404,0.0980321865961808,
-0.287603806650743));
#74742=CARTESIAN_POINT('Ctrl Pts',(0.271854463958668,0.113685644623779,
-0.286707578913342));
#74743=CARTESIAN_POINT('Ctrl Pts',(0.264987630655919,0.128885068807038,
-0.285811351175941));
#74744=CARTESIAN_POINT('Ctrl Pts',(0.256887762185586,0.143395668132903,
-0.28491512343854));
#74745=CARTESIAN_POINT('Ctrl Pts',(0.248790067633381,0.157902372968997,
-0.284019136239084));
#74746=CARTESIAN_POINT('Ctrl Pts',(0.239460390207801,0.171719933886316,
-0.283123149039629));
#74747=CARTESIAN_POINT('Ctrl Pts',(0.22904577855072,0.184639300605517,-0.282227161840174));
#74748=CARTESIAN_POINT('Ctrl Pts',(0.218606148761602,0.197589702415902,
-0.281329022287198));
#74749=CARTESIAN_POINT('Ctrl Pts',(0.207076898786055,0.20963699823115,-0.280430882734223));
#74750=CARTESIAN_POINT('Ctrl Pts',(0.194644907688949,0.220605983397461,
-0.279532743181248));
#74751=CARTESIAN_POINT('Ctrl Pts',(0.18343602537139,0.230495796132352,-0.278722966173252));
#74752=CARTESIAN_POINT('Ctrl Pts',(0.171494140039145,0.239509279579548,
-0.277913189165257));
#74753=CARTESIAN_POINT('Ctrl Pts',(0.15897708025623,0.247547829627335,-0.277103412157261));
#74754=CARTESIAN_POINT('Ctrl Pts',(0.145094340803253,0.256463429442994,
-0.276205284049544));
#74755=CARTESIAN_POINT('Ctrl Pts',(0.130414881329146,0.264236061930519,
-0.275307155941827));
#74756=CARTESIAN_POINT('Ctrl Pts',(0.115152090863427,0.270727974117528,
-0.27440902783411));
#74757=CARTESIAN_POINT('Ctrl Pts',(0.0999189693705288,0.277207266831928,
-0.27351264557611));
#74758=CARTESIAN_POINT('Ctrl Pts',(0.0841054616494478,0.282410413744088,
-0.27261626331811));
#74759=CARTESIAN_POINT('Ctrl Pts',(0.0679492881810552,0.286245583783729,
-0.27171988106011));
#74760=CARTESIAN_POINT('Ctrl Pts',(0.0517959130334674,0.290080089554932,
-0.270823654059488));
#74761=CARTESIAN_POINT('Ctrl Pts',(0.035300745405137,0.292546854929202,
-0.269927427058865));
#74762=CARTESIAN_POINT('Ctrl Pts',(0.0187161961879273,0.293604059917868,
-0.269031200058243));
#74763=CARTESIAN_POINT('Ctrl Pts',(0.00213609800764407,0.294660981169039,
-0.268135213591109));
#74764=CARTESIAN_POINT('Ctrl Pts',(-0.014532543310271,0.294309053444057,
-0.267239227123975));
#74765=CARTESIAN_POINT('Ctrl Pts',(-0.0310343467477303,0.292558557082068,
-0.266343240656841));
#74766=CARTESIAN_POINT('Ctrl Pts',(-0.0475757915097962,0.29080385560427,
-0.265445101813421));
#74767=CARTESIAN_POINT('Ctrl Pts',(-0.0639488101679096,0.287643985310027,
-0.264546962970001));
#74768=CARTESIAN_POINT('Ctrl Pts',(-0.0799048785991908,0.283141043255916,
-0.263648824126582));
#74769=CARTESIAN_POINT('Ctrl Pts',(-0.094291202113307,0.279081096945536,
-0.262839043445477));
#74770=CARTESIAN_POINT('Ctrl Pts',(-0.108338323302757,0.273930182240347,
-0.262029262764373));
#74771=CARTESIAN_POINT('Ctrl Pts',(-0.121877834764577,0.267767498761703,
-0.261219482083269));
#74772=CARTESIAN_POINT('Ctrl Pts',(-0.136894524488037,0.260932458522351,
-0.260321353279546));
#74773=CARTESIAN_POINT('Ctrl Pts',(-0.151382464382951,0.252808400843108,
-0.259423224475822));
#74774=CARTESIAN_POINT('Ctrl Pts',(-0.165110236460511,0.243499999622082,
-0.258525095672099));
#74775=CARTESIAN_POINT('Ctrl Pts',(-0.178811323349849,0.234209692847645,
-0.257628712726046));
#74776=CARTESIAN_POINT('Ctrl Pts',(-0.191754490863578,0.223739996567545,
-0.256732329779993));
#74777=CARTESIAN_POINT('Ctrl Pts',(-0.203733726773965,0.212240921065641,
-0.255835946833939));
#74778=CARTESIAN_POINT('Ctrl Pts',(-0.215710887536314,0.200743837534187,
-0.254939719167181));
#74779=CARTESIAN_POINT('Ctrl Pts',(-0.226723842192841,0.188218236884438,
-0.254043491500424));
#74780=CARTESIAN_POINT('Ctrl Pts',(-0.236600645961076,0.174853579691128,
-0.253147263833665));
#74781=CARTESIAN_POINT('Ctrl Pts',(-0.246474798830406,0.161492509524142,
-0.252251276711217));
#74782=CARTESIAN_POINT('Ctrl Pts',(-0.255212944291058,0.14729347302781,
-0.251355289588768));
#74783=CARTESIAN_POINT('Ctrl Pts',(-0.262685312828353,0.132476663696934,
-0.250459302466319));
#74784=CARTESIAN_POINT('Ctrl Pts',(-0.27017563152706,0.117624261351904,
-0.249561162999083));
#74785=CARTESIAN_POINT('Ctrl Pts',(-0.276393765841537,0.10215184385304,
-0.248663023531846));
#74786=CARTESIAN_POINT('Ctrl Pts',(-0.281257209132088,0.0863019253042985,
-0.24776488406461));
#74787=CARTESIAN_POINT('Ctrl Pts',(-0.285642169789093,0.0720113774144976,
-0.246955106712834));
#74788=CARTESIAN_POINT('Ctrl Pts',(-0.28892645453844,0.0574146248080487,
-0.246145329361058));
#74789=CARTESIAN_POINT('Ctrl Pts',(-0.291085350888058,0.0426961180715054,
-0.245335552009283));
#74790=CARTESIAN_POINT('Ctrl Pts',(-0.293145255725698,0.0286524965540629,
-0.244562905242508));
#74791=CARTESIAN_POINT('Ctrl Pts',(-0.294189181828774,0.014456301457929,
-0.243790258475734));
#74792=CARTESIAN_POINT('Ctrl Pts',(-0.29419991634408,0.000221862877645845,
-0.24301761170896));
#74793=CARTESIAN_POINT('',(-0.293744537661632,9.25662168771693E-5,-0.14301761170896));
#74794=CARTESIAN_POINT('Ctrl Pts',(-0.29445204848288,0.000219819995411468,
-0.243017490604234));
#74795=CARTESIAN_POINT('Ctrl Pts',(-0.293751335212956,-0.0831599735004281,
-0.238495534381254));
#74796=CARTESIAN_POINT('Ctrl Pts',(-0.213104386102375,-0.265350741380069,
-0.228678934800286));
#74797=CARTESIAN_POINT('Ctrl Pts',(0.0959768626644768,-0.334276361929609,
-0.213567691861301));
#74798=CARTESIAN_POINT('Ctrl Pts',(0.332941212592535,-0.100509168556688,
-0.197683761787325));
#74799=CARTESIAN_POINT('Ctrl Pts',(0.264912791059908,0.225330331614917,
-0.181799831713324));
#74800=CARTESIAN_POINT('Ctrl Pts',(-0.0457940858542747,0.344753966870199,
-0.165915901639349));
#74801=CARTESIAN_POINT('Ctrl Pts',(-0.264522476343154,0.184916985358244,
-0.152988494971215));
#74802=CARTESIAN_POINT('Ctrl Pts',(-0.293866212551352,0.0434698093785783,
-0.145355731661092));
#74803=CARTESIAN_POINT('Ctrl Pts',(-0.293744537661632,9.25662168771693E-5,
-0.14301761170896));
#74804=CARTESIAN_POINT('',(-0.294186798250996,-0.000261260174532603,-0.0430176117089603));
#74805=CARTESIAN_POINT('Ctrl Pts',(-0.293744537661632,9.25662168771693E-5,
-0.14301761170896));
#74806=CARTESIAN_POINT('Ctrl Pts',(-0.293590681286969,-0.0547574146716426,
-0.140061088303096));
#74807=CARTESIAN_POINT('Ctrl Pts',(-0.252507336188254,-0.208049626619383,
-0.131809921539239));
#74808=CARTESIAN_POINT('Ctrl Pts',(-0.00537683585382717,-0.347740876544168,
-0.118264111417372));
#74809=CARTESIAN_POINT('Ctrl Pts',(0.289302873605603,-0.192989859491775,
-0.102380181343396));
#74810=CARTESIAN_POINT('Ctrl Pts',(0.319027026718357,0.138546274126025,
-0.0864962512693962));
#74811=CARTESIAN_POINT('Ctrl Pts',(0.0563826028718357,0.343175568089735,
-0.0706123211954191));
#74812=CARTESIAN_POINT('Ctrl Pts',(-0.230176223724105,0.243028826433064,
-0.0561194413419322));
#74813=CARTESIAN_POINT('Ctrl Pts',(-0.293533328381349,0.0719298853820162,
-0.0469212048464487));
#74814=CARTESIAN_POINT('Ctrl Pts',(-0.294186798250996,-0.000261260174532603,
-0.0430176117089603));
#74815=CARTESIAN_POINT('',(-0.288932402895451,-0.0555047265699091,-0.0399922440470373));
#74816=CARTESIAN_POINT('Origin',(0.000858955019862939,0.000109716591558141,
-0.0410049673081075));
#74817=CARTESIAN_POINT('',(-0.2942,-3.60291088309151E-17,-0.04));
#74818=CARTESIAN_POINT('Origin',(0.,0.,-0.04));
#74819=CARTESIAN_POINT('',(-0.221686865784453,0.193412961144454,-0.04));
#74820=CARTESIAN_POINT('Origin',(0.,0.,-0.04));
#74821=CARTESIAN_POINT('',(-0.293768185304944,0.000119558705670028,-0.128582388291039));
#74822=CARTESIAN_POINT('Ctrl Pts',(-0.221686865784453,0.193412961144454,
-0.04));
#74823=CARTESIAN_POINT('Ctrl Pts',(-0.157343740137231,0.267162030364559,
-0.0452946433579961));
#74824=CARTESIAN_POINT('Ctrl Pts',(0.0496182053170372,0.34411773810001,
-0.0558839300739825));
#74825=CARTESIAN_POINT('Ctrl Pts',(0.316630310046587,0.144421010344727,
-0.0717678601479819));
#74826=CARTESIAN_POINT('Ctrl Pts',(0.292700980788135,-0.18764014656629,
-0.087651790221959));
#74827=CARTESIAN_POINT('Ctrl Pts',(0.00108527138476461,-0.347774759775002,
-0.103535720295958));
#74828=CARTESIAN_POINT('Ctrl Pts',(-0.250450798406577,-0.211692488319999,
-0.117179252985643));
#74829=CARTESIAN_POINT('Ctrl Pts',(-0.293565247741175,-0.0565344194021568,
-0.125528142317339));
#74830=CARTESIAN_POINT('Ctrl Pts',(-0.293768185304944,0.000119558705670028,
-0.128582388291039));
#74831=CARTESIAN_POINT('',(-0.294499934166686,0.000202248616450143,-0.228582388291039));
#74832=CARTESIAN_POINT('Ctrl Pts',(-0.293768185304944,0.000119558705670028,
-0.128582388291039));
#74833=CARTESIAN_POINT('Ctrl Pts',(-0.293917047181479,0.0416772542730101,
-0.130822785675335));
#74834=CARTESIAN_POINT('Ctrl Pts',(-0.266241884141502,0.181253034476232,
-0.13835782641764));
#74835=CARTESIAN_POINT('Ctrl Pts',(-0.0521444580392835,0.343851119474212,
-0.151187510517905));
#74836=CARTESIAN_POINT('Ctrl Pts',(0.260721659465963,0.230172071351022,
-0.167071440591914));
#74837=CARTESIAN_POINT('Ctrl Pts',(0.33473384718524,-0.0943598456158883,
-0.182955370665886));
#74838=CARTESIAN_POINT('Ctrl Pts',(0.102118851543616,-0.332451723718594,
-0.198839300739887));
#74839=CARTESIAN_POINT('Ctrl Pts',(-0.210188708599208,-0.268822006024866,
-0.214048306614925));
#74840=CARTESIAN_POINT('Ctrl Pts',(-0.293831058097356,-0.0849440524174718,
-0.223962669131982));
#74841=CARTESIAN_POINT('Ctrl Pts',(-0.294499934166686,0.000202248616450143,
-0.228582388291039));
#74842=CARTESIAN_POINT('',(-0.294199900939987,-0.000241426803754268,-0.328582388291039));
#74843=CARTESIAN_POINT('Ctrl Pts',(-0.294499934166686,0.000202248616450143,
-0.228582388291039));
#74844=CARTESIAN_POINT('Ctrl Pts',(-0.294597654532305,0.0126418141050379,
-0.229257312489979));
#74845=CARTESIAN_POINT('Ctrl Pts',(-0.288230516942064,0.122566455283741,
-0.235226880046917));
#74846=CARTESIAN_POINT('Ctrl Pts',(-0.149881191576857,0.313827796561115,
-0.246491090961838));
#74847=CARTESIAN_POINT('Ctrl Pts',(0.182509282439241,0.296044952328845,
-0.262375021035839));
#74848=CARTESIAN_POINT('Ctrl Pts',(0.347709976704713,0.00706718636026016,
-0.278258951109817));
#74849=CARTESIAN_POINT('Ctrl Pts',(0.194387712086192,-0.288384529274392,
-0.294142881183814));
#74850=CARTESIAN_POINT('Ctrl Pts',(-0.137005426269588,-0.319658767853967,
-0.310026811257793));
#74851=CARTESIAN_POINT('Ctrl Pts',(-0.285807358002809,-0.130626349168447,
-0.321506646960211));
#74852=CARTESIAN_POINT('Ctrl Pts',(-0.294536173334788,-0.0166712251748063,
-0.327691839304621));
#74853=CARTESIAN_POINT('Ctrl Pts',(-0.294390515183554,-0.000241583225926489,
-0.328582388291039));
#74854=CARTESIAN_POINT('',(-0.294157183091672,-5.80760838105538E-5,-0.42858238548701));
#74855=CARTESIAN_POINT('Ctrl Pts',(-0.294199900939987,-0.000241426803754268,
-0.328582388291039));
#74856=CARTESIAN_POINT('Ctrl Pts',(-0.294213270623952,0.0160507149000982,
-0.329466063430325));
#74857=CARTESIAN_POINT('Ctrl Pts',(-0.292869010815876,0.0323914039133056,
-0.330349738569611));
#74858=CARTESIAN_POINT('Ctrl Pts',(-0.290169337604126,0.0485324171495974,
-0.331233413708898));
#74859=CARTESIAN_POINT('Ctrl Pts',(-0.287471170605857,0.0646644249212218,
-0.332116595824287));
#74860=CARTESIAN_POINT('Ctrl Pts',(-0.283419155016342,0.0805961649708263,
-0.332999777939676));
#74861=CARTESIAN_POINT('Ctrl Pts',(-0.278067392711698,0.0960841563969761,
-0.333882960055066));
#74862=CARTESIAN_POINT('Ctrl Pts',(-0.272718393432816,0.111564151631051,
-0.334765686198235));
#74863=CARTESIAN_POINT('Ctrl Pts',(-0.26607124562374,0.126600080193668,
-0.335648412341405));
#74864=CARTESIAN_POINT('Ctrl Pts',(-0.258229490017853,0.140965139254781,
-0.336531138484574));
#74865=CARTESIAN_POINT('Ctrl Pts',(-0.250369454528004,0.155363684645478,
-0.337415922346994));
#74866=CARTESIAN_POINT('Ctrl Pts',(-0.24130966072791,0.169087525650376,
-0.338300706209414));
#74867=CARTESIAN_POINT('Ctrl Pts',(-0.231199034706483,0.181935830310553,
-0.339185490071835));
#74868=CARTESIAN_POINT('Ctrl Pts',(-0.221260465597484,0.194565489792372,
-0.340055217183148));
#74869=CARTESIAN_POINT('Ctrl Pts',(-0.210307190680362,0.206348733223679,
-0.340924944294462));
#74870=CARTESIAN_POINT('Ctrl Pts',(-0.198515397572668,0.217129631617993,
-0.341794671405776));
#74871=CARTESIAN_POINT('Ctrl Pts',(-0.186338536628284,0.228262586496369,
-0.342692799959873));
#74872=CARTESIAN_POINT('Ctrl Pts',(-0.173183301635518,0.238403611496796,
-0.34359092851397));
#74873=CARTESIAN_POINT('Ctrl Pts',(-0.159236740552278,0.247380881351584,
-0.344489057068068));
#74874=CARTESIAN_POINT('Ctrl Pts',(-0.145317289883835,0.256340700488015,
-0.345385439769729));
#74875=CARTESIAN_POINT('Ctrl Pts',(-0.130610188431077,0.264140775701221,
-0.34628182247139));
#74876=CARTESIAN_POINT('Ctrl Pts',(-0.115334224409597,0.270650432624514,
-0.347178205173051));
#74877=CARTESIAN_POINT('Ctrl Pts',(-0.100060906431591,0.277158961970183,
-0.348074432606764));
#74878=CARTESIAN_POINT('Ctrl Pts',(-0.0842196265633046,0.282377158592839,
-0.348970660040477));
#74879=CARTESIAN_POINT('Ctrl Pts',(-0.068052101713687,0.286221158289093,
-0.349866887474189));
#74880=CARTESIAN_POINT('Ctrl Pts',(-0.0518889160665153,0.290064126294161,
-0.350762874369396));
#74881=CARTESIAN_POINT('Ctrl Pts',(-0.0354004320327606,0.292533456912791,
-0.351658861264602));
#74882=CARTESIAN_POINT('Ctrl Pts',(-0.0188400964165087,0.293596135476979,
-0.352554848159809));
#74883=CARTESIAN_POINT('Ctrl Pts',(-0.00223997920574037,0.294661366830478,
-0.353452987414012));
#74884=CARTESIAN_POINT('Ctrl Pts',(0.0144315393077484,0.294313172550085,
-0.354351126668216));
#74885=CARTESIAN_POINT('Ctrl Pts',(0.0309190160886215,0.292570768266605,
-0.355249265922419));
#74886=CARTESIAN_POINT('Ctrl Pts',(0.0457844219475074,0.29099978519937,
-0.356059044441533));
#74887=CARTESIAN_POINT('Ctrl Pts',(0.0604998238938433,0.28829621433199,
-0.356868822960646));
#74888=CARTESIAN_POINT('Ctrl Pts',(0.0748858560541141,0.28450966339132,
-0.357678601479759));
#74889=CARTESIAN_POINT('Ctrl Pts',(0.0908414629000977,0.280309984324951,
-0.358576730132563));
#74890=CARTESIAN_POINT('Ctrl Pts',(0.106493703337533,0.274750485260366,
-0.359474858785367));
#74891=CARTESIAN_POINT('Ctrl Pts',(0.121596801359752,0.267895236798038,
-0.36037298743817));
#74892=CARTESIAN_POINT('Ctrl Pts',(0.13667054084219,0.261053314084136,-0.361269370240835));
#74893=CARTESIAN_POINT('Ctrl Pts',(0.151196517023994,0.252920904648086,
-0.362165753043499));
#74894=CARTESIAN_POINT('Ctrl Pts',(0.164946334766074,0.243611056085799,
-0.363062135846163));
#74895=CARTESIAN_POINT('Ctrl Pts',(0.178693770849512,0.234302820118071,
-0.363958363382926));
#74896=CARTESIAN_POINT('Ctrl Pts',(0.191664632259472,0.223817948321669,
-0.364854590919689));
#74897=CARTESIAN_POINT('Ctrl Pts',(0.203657436356593,0.212314127218752,
-0.365750818456452));
#74898=CARTESIAN_POINT('Ctrl Pts',(0.21564702172256,0.200813393609558,-0.366646805456017));
#74899=CARTESIAN_POINT('Ctrl Pts',(0.226658506983278,0.188294809460885,
-0.367542792455582));
#74900=CARTESIAN_POINT('Ctrl Pts',(0.236526786088971,0.174953477994643,
-0.368438779455147));
#74901=CARTESIAN_POINT('Ctrl Pts',(0.246418770984156,0.161580097698824,
-0.369336918813697));
#74902=CARTESIAN_POINT('Ctrl Pts',(0.25516161318444,0.14738067742214,-0.370235058172247));
#74903=CARTESIAN_POINT('Ctrl Pts',(0.262633018972394,0.132580305269848,
-0.371133197530796));
#74904=CARTESIAN_POINT('Ctrl Pts',(0.269369367887219,0.119236033292566,
-0.371942975538448));
#74905=CARTESIAN_POINT('Ctrl Pts',(0.275072596195384,0.105403996273835,
-0.372752753546101));
#74906=CARTESIAN_POINT('Ctrl Pts',(0.279687183289654,0.0912618184319138,
-0.373562531553753));
#74907=CARTESIAN_POINT('Ctrl Pts',(0.284805243636515,0.0755766621758177,
-0.374460660167658));
#74908=CARTESIAN_POINT('Ctrl Pts',(0.288616098892701,0.059409472625499,
-0.375358788781564));
#74909=CARTESIAN_POINT('Ctrl Pts',(0.291040390595721,0.0430015237159115,
-0.37625691739547));
#74910=CARTESIAN_POINT('Ctrl Pts',(0.293459969776135,0.026625469825425,
-0.377153300158664));
#74911=CARTESIAN_POINT('Ctrl Pts',(0.294498155584544,0.0100103497840362,
-0.378049682921857));
#74912=CARTESIAN_POINT('Ctrl Pts',(0.29412616962601,-0.00659062524587472,
-0.378946065685051));
#74913=CARTESIAN_POINT('Ctrl Pts',(0.293754248100716,-0.023188724751655,
-0.379842293182046));
#74914=CARTESIAN_POINT('Ctrl Pts',(0.291972604312582,-0.0397718940807069,
-0.380738520679042));
#74915=CARTESIAN_POINT('Ctrl Pts',(0.288804560090822,-0.0560853463103032,
-0.381634748176038));
#74916=CARTESIAN_POINT('Ctrl Pts',(0.285637366136683,-0.0723944201918616,
-0.382530735135603));
#74917=CARTESIAN_POINT('Ctrl Pts',(0.281084671958776,-0.088433145512489,
-0.383426722095167));
#74918=CARTESIAN_POINT('Ctrl Pts',(0.275220959321368,-0.103957027421074,
-0.384322709054731));
#74919=CARTESIAN_POINT('Ctrl Pts',(0.269343160745391,-0.119518201137842,
-0.385220848373739));
#74920=CARTESIAN_POINT('Ctrl Pts',(0.262148359134826,-0.134561326912255,
-0.386118987692747));
#74921=CARTESIAN_POINT('Ctrl Pts',(0.253759438487147,-0.148861638371637,
-0.387017127011756));
#74922=CARTESIAN_POINT('Ctrl Pts',(0.246195840097746,-0.161755050678741,
-0.387826905217082));
#74923=CARTESIAN_POINT('Ctrl Pts',(0.237662404096809,-0.17404458450177,
-0.388636683422409));
#74924=CARTESIAN_POINT('Ctrl Pts',(0.228278315073844,-0.185587313324609,
-0.389446461627736));
#74925=CARTESIAN_POINT('Ctrl Pts',(0.217870380203778,-0.198389405197028,
-0.390344590236663));
#74926=CARTESIAN_POINT('Ctrl Pts',(0.206348879583428,-0.210354172454429,
-0.391242718845589));
#74927=CARTESIAN_POINT('Ctrl Pts',(0.19387356937472,-0.22128415916623,-0.392140847454516));
#74928=CARTESIAN_POINT('Ctrl Pts',(0.181422509627243,-0.232192899334694,
-0.393037230212426));
#74929=CARTESIAN_POINT('Ctrl Pts',(0.168021865344104,-0.242070286298685,
-0.393933612970336));
#74930=CARTESIAN_POINT('Ctrl Pts',(0.153868837590726,-0.250754901883251,
-0.394829995728246));
#74931=CARTESIAN_POINT('Ctrl Pts',(0.139718261348546,-0.259438013165506,
-0.395726223219565));
#74932=CARTESIAN_POINT('Ctrl Pts',(0.124816205105695,-0.266928305295534,
-0.396622450710884));
#74933=CARTESIAN_POINT('Ctrl Pts',(0.109389430956506,-0.273107290995704,
-0.397518678202204));
#74934=CARTESIAN_POINT('Ctrl Pts',(0.0939667971847902,-0.279284618323684,
-0.398414665155865));
#74935=CARTESIAN_POINT('Ctrl Pts',(0.0780204640726392,-0.284151053523581,
-0.399310652109527));
#74936=CARTESIAN_POINT('Ctrl Pts',(0.0617962714351649,-0.287636682008244,
-0.400206639063189));
#74937=CARTESIAN_POINT('Ctrl Pts',(0.0455331046921821,-0.291130683744837,
-0.401104778376037));
#74938=CARTESIAN_POINT('Ctrl Pts',(0.0289915280435265,-0.293237112583825,
-0.402002917688885));
#74939=CARTESIAN_POINT('Ctrl Pts',(0.0124270340977167,-0.293937423312402,
-0.402901057001733));
#74940=CARTESIAN_POINT('Ctrl Pts',(-0.00250780557758506,-0.294568835807611,
-0.403710835235065));
#74941=CARTESIAN_POINT('Ctrl Pts',(-0.0174607700916445,-0.294057914770964,
-0.404520613468396));
#74942=CARTESIAN_POINT('Ctrl Pts',(-0.0322471498142642,-0.292427360773332,
-0.405330391701728));
#74943=CARTESIAN_POINT('Ctrl Pts',(-0.048646789004516,-0.290618906118236,
-0.406228520324142));
#74944=CARTESIAN_POINT('Ctrl Pts',(-0.0649462617435838,-0.287420808342489,
-0.407126648946555));
#74945=CARTESIAN_POINT('Ctrl Pts',(-0.080893043439246,-0.282860310971929,
-0.408024777568969));
#74946=CARTESIAN_POINT('Ctrl Pts',(-0.0968088265684688,-0.278308678642819,
-0.408921160340696));
#74947=CARTESIAN_POINT('Ctrl Pts',(-0.112372509131877,-0.272400054959249,
-0.409817543112423));
#74948=CARTESIAN_POINT('Ctrl Pts',(-0.12734155857147,-0.265212683445926,
-0.41071392588415));
#74949=CARTESIAN_POINT('Ctrl Pts',(-0.142308015158101,-0.258026556887908,
-0.41161015338959));
#74950=CARTESIAN_POINT('Ctrl Pts',(-0.156679308818926,-0.249562415881682,
-0.41250638089503));
#74951=CARTESIAN_POINT('Ctrl Pts',(-0.170232964834833,-0.239946614236464,
-0.41340260840047));
#74952=CARTESIAN_POINT('Ctrl Pts',(-0.183782983200655,-0.230333393365145,
-0.414298595368445));
#74953=CARTESIAN_POINT('Ctrl Pts',(-0.196515160067304,-0.219569592394035,
-0.41519458233642));
#74954=CARTESIAN_POINT('Ctrl Pts',(-0.208237501543953,-0.207823922950973,
-0.416090569304395));
#74955=CARTESIAN_POINT('Ctrl Pts',(-0.219988002681964,-0.196050037807606,
-0.416988708631577));
#74956=CARTESIAN_POINT('Ctrl Pts',(-0.230723280434877,-0.183290154585397,
-0.417886847958758));
#74957=CARTESIAN_POINT('Ctrl Pts',(-0.240289280095377,-0.169748937761759,
-0.41878498728594));
#74958=CARTESIAN_POINT('Ctrl Pts',(-0.248914153097114,-0.15753993927359,
-0.419594765449198));
#74959=CARTESIAN_POINT('Ctrl Pts',(-0.25658883481505,-0.144696598236817,
-0.420404543612457));
#74960=CARTESIAN_POINT('Ctrl Pts',(-0.263232295687335,-0.131386447197478,
-0.421214321775715));
#74961=CARTESIAN_POINT('Ctrl Pts',(-0.271109781837181,-0.115603930753049,
-0.422174516527839));
#74962=CARTESIAN_POINT('Ctrl Pts',(-0.277581946799669,-0.0990750858031063,
-0.423134711279964));
#74963=CARTESIAN_POINT('Ctrl Pts',(-0.282524234881432,-0.0820591049467478,
-0.424094906032089));
#74964=CARTESIAN_POINT('Ctrl Pts',(-0.287441843801891,-0.0651280928597843,
-0.425050306081684));
#74965=CARTESIAN_POINT('Ctrl Pts',(-0.290844538262862,-0.0477153541178306,
-0.426005706131278));
#74966=CARTESIAN_POINT('Ctrl Pts',(-0.292656388079449,-0.0300978158059859,
-0.426961106180873));
#74967=CARTESIAN_POINT('Ctrl Pts',(-0.293681269090984,-0.0201323758890031,
-0.427501532523213));
#74968=CARTESIAN_POINT('Ctrl Pts',(-0.294198011145814,-0.010101755355635,
-0.428041958865554));
#74969=CARTESIAN_POINT('Ctrl Pts',(-0.2941999942651,-5.80897158011377E-5,
-0.428582385207895));
#74970=CARTESIAN_POINT('',(-0.294177705196902,0.000269677437982729,-0.528582388291039));
#74971=CARTESIAN_POINT('Ctrl Pts',(-0.293727096099073,-5.79391349403435E-5,
-0.428582388291039));
#74972=CARTESIAN_POINT('Ctrl Pts',(-0.293634468529128,0.0526122281426488,
-0.43142100947726));
#74973=CARTESIAN_POINT('Ctrl Pts',(-0.254942151327534,0.203650636832815,
-0.439554274021477));
#74974=CARTESIAN_POINT('Ctrl Pts',(-0.0131124674156837,0.347534563923677,
-0.452982181923692));
#74975=CARTESIAN_POINT('Ctrl Pts',(0.284960711564284,0.199373024186178,
-0.468866111997679));
#74976=CARTESIAN_POINT('Ctrl Pts',(0.321992827127266,-0.131426135938866,
-0.484750042071667));
#74977=CARTESIAN_POINT('Ctrl Pts',(0.064060245340413,-0.341831091167,-0.500633972145656));
#74978=CARTESIAN_POINT('Ctrl Pts',(-0.227177597425987,-0.247332674255593,
-0.515244754218778));
#74979=CARTESIAN_POINT('Ctrl Pts',(-0.293497987656841,-0.0740605286863558,
-0.524560892933907));
#74980=CARTESIAN_POINT('Ctrl Pts',(-0.294177705196902,0.000269677437982729,
-0.528582388291039));
#74981=CARTESIAN_POINT('',(-0.294228348185738,-9.78338538022252E-5,-0.62858238829104));
#74982=CARTESIAN_POINT('Ctrl Pts',(-0.294177705196902,0.000269677437982729,
-0.528582388291039));
#74983=CARTESIAN_POINT('Ctrl Pts',(-0.294392894063339,0.0238015592200154,
-0.529855536291904));
#74984=CARTESIAN_POINT('Ctrl Pts',(-0.281052382088353,0.144954516849035,
-0.536423327650765));
#74985=CARTESIAN_POINT('Ctrl Pts',(-0.11361603957044,0.328699871423913,
-0.548285762367618));
#74986=CARTESIAN_POINT('Ctrl Pts',(0.214662148711559,0.273628163448583,
-0.564169692441609));
#74987=CARTESIAN_POINT('Ctrl Pts',(0.34629696365299,-0.0321033158226767,
-0.580053622515595));
#74988=CARTESIAN_POINT('Ctrl Pts',(0.160703037897489,-0.308426236776979,
-0.595937552589584));
#74989=CARTESIAN_POINT('Ctrl Pts',(-0.172104486846384,-0.302212268991917,
-0.611821482663572));
#74990=CARTESIAN_POINT('Ctrl Pts',(-0.29209425334131,-0.108297247891136,
-0.622703094564057));
#74991=CARTESIAN_POINT('Ctrl Pts',(-0.294667300158824,-0.00547889421475271,
-0.628290063106547));
#74992=CARTESIAN_POINT('Ctrl Pts',(-0.294643988261876,-9.79720582637844E-5,
-0.62858238829104));
#74993=CARTESIAN_POINT('',(-0.294199924273098,-0.000211086956616954,-0.728582384448469));
#74994=CARTESIAN_POINT('Ctrl Pts',(-0.294199983736203,-9.78244223404861E-5,
-0.62858238829104));
#74995=CARTESIAN_POINT('Ctrl Pts',(-0.294205426299557,0.016270297276697,
-0.629472949926511));
#74996=CARTESIAN_POINT('Ctrl Pts',(-0.292840578471788,0.0326939988902729,
-0.630363511561983));
#74997=CARTESIAN_POINT('Ctrl Pts',(-0.290103784633613,0.0489227364448709,
-0.631254073197454));
#74998=CARTESIAN_POINT('Ctrl Pts',(-0.287372108214987,0.0651211285428017,
-0.632142969607924));
#74999=CARTESIAN_POINT('Ctrl Pts',(-0.283273643069613,0.0811244831776327,
-0.633031866018394));
#75000=CARTESIAN_POINT('Ctrl Pts',(-0.277858538679389,0.0966864648384387,
-0.633920762428863));
#75001=CARTESIAN_POINT('Ctrl Pts',(-0.272443978612943,0.112246882216077,
-0.634809569487879));
#75002=CARTESIAN_POINT('Ctrl Pts',(-0.265713259877918,0.127365239426204,
-0.635698376546894));
#75003=CARTESIAN_POINT('Ctrl Pts',(-0.257766513752171,0.141809958705487,
-0.63658718360591));
#75004=CARTESIAN_POINT('Ctrl Pts',(-0.249820840153935,0.156252728462466,
-0.637475870707649));
#75005=CARTESIAN_POINT('Ctrl Pts',(-0.240659870035023,0.170021343875504,
-0.638364557809388));
#75006=CARTESIAN_POINT('Ctrl Pts',(-0.230429021010939,0.182910104357142,
-0.639253244911127));
#75007=CARTESIAN_POINT('Ctrl Pts',(-0.220175002415835,0.195828053721404,
-0.640143944602326));
#75008=CARTESIAN_POINT('Ctrl Pts',(-0.208846804315949,0.207861565752943,
-0.641034644293525));
#75009=CARTESIAN_POINT('Ctrl Pts',(-0.196629205242875,0.21883920043163,
-0.641925343984725));
#75010=CARTESIAN_POINT('Ctrl Pts',(-0.189020928018026,0.225675313436242,
-0.642480010260333));
#75011=CARTESIAN_POINT('Ctrl Pts',(-0.181068483165117,0.232102714295101,
-0.643034676535941));
#75012=CARTESIAN_POINT('Ctrl Pts',(-0.172822401357768,0.238088339884453,
-0.643589342811549));
#75013=CARTESIAN_POINT('Ctrl Pts',(-0.159470152672527,0.247780404949165,
-0.64448747142854));
#75014=CARTESIAN_POINT('Ctrl Pts',(-0.145257359119195,0.256376749337958,
-0.645385600045531));
#75015=CARTESIAN_POINT('Ctrl Pts',(-0.130389215186783,0.263727686379293,
-0.646283728662523));
#75016=CARTESIAN_POINT('Ctrl Pts',(-0.115549973084665,0.271064334109479,
-0.647180111428722));
#75017=CARTESIAN_POINT('Ctrl Pts',(-0.100058581207752,0.27715997379475,
-0.648076494194921));
#75018=CARTESIAN_POINT('Ctrl Pts',(-0.0841471422624768,0.281909379852921,
-0.648972876961119));
#75019=CARTESIAN_POINT('Ctrl Pts',(-0.0682384594069048,0.286657963245765,
-0.649869104460951));
#75020=CARTESIAN_POINT('Ctrl Pts',(-0.0519106148113616,0.290060499378108,
-0.650765331960784));
#75021=CARTESIAN_POINT('Ctrl Pts',(-0.0354132269970851,0.292060855565502,
-0.651661559460616));
#75022=CARTESIAN_POINT('Ctrl Pts',(-0.0189202668986979,0.294060674879484,
-0.652557546422929));
#75023=CARTESIAN_POINT('Ctrl Pts',(-0.00225864120250119,0.294658976746293,
-0.653453533385241));
#75024=CARTESIAN_POINT('Ctrl Pts',(0.0143160979546571,0.29385147496542,
-0.654349520347554));
#75025=CARTESIAN_POINT('Ctrl Pts',(0.0309306533082596,0.293042033386325,
-0.655247659669103));
#75026=CARTESIAN_POINT('Ctrl Pts',(0.0474571125141693,0.290820108264942,
-0.656145798990651));
#75027=CARTESIAN_POINT('Ctrl Pts',(0.0636438170329757,0.287233536609974,
-0.6570439383122));
#75028=CARTESIAN_POINT('Ctrl Pts',(0.0782380342004271,0.283999820595795,
-0.657853716503312));
#75029=CARTESIAN_POINT('Ctrl Pts',(0.0925557573170437,0.279657589733852,
-0.658663494694424));
#75030=CARTESIAN_POINT('Ctrl Pts',(0.106424341927058,0.274276319512627,
-0.659473272885536));
#75031=CARTESIAN_POINT('Ctrl Pts',(0.121806051205136,0.268307928619306,
-0.660371401502527));
#75032=CARTESIAN_POINT('Ctrl Pts',(0.136733308829178,0.261022489904615,
-0.661269530119518));
#75033=CARTESIAN_POINT('Ctrl Pts',(0.150969109178701,0.252511322664528,
-0.662167658736509));
#75034=CARTESIAN_POINT('Ctrl Pts',(0.165177236895546,0.244016700079389,
-0.663064041502708));
#75035=CARTESIAN_POINT('Ctrl Pts',(0.178695869870208,0.234301423039947,
-0.663960424268907));
#75036=CARTESIAN_POINT('Ctrl Pts',(0.191310784034313,0.223503521028588,
-0.664856807035106));
#75037=CARTESIAN_POINT('Ctrl Pts',(0.203923513114135,0.212707489368914,
-0.665753034534938));
#75038=CARTESIAN_POINT('Ctrl Pts',(0.215632200183979,0.200829677770462,
-0.66664926203477));
#75039=CARTESIAN_POINT('Ctrl Pts',(0.226254385690265,0.188049442849269,
-0.667545489534601));
#75040=CARTESIAN_POINT('Ctrl Pts',(0.236873720319788,0.175272638001366,
-0.668441476496914));
#75041=CARTESIAN_POINT('Ctrl Pts',(0.246406634503134,0.161594506435376,
-0.669337463459226));
#75042=CARTESIAN_POINT('Ctrl Pts',(0.254711024514696,0.147227490607814,
-0.670233450421538));
#75043=CARTESIAN_POINT('Ctrl Pts',(0.263035363511333,0.132825962024479,
-0.671131589743086));
#75044=CARTESIAN_POINT('Ctrl Pts',(0.270124908995877,0.117732945428985,
-0.672029729064634));
#75045=CARTESIAN_POINT('Ctrl Pts',(0.275883471685441,0.102185860327095,
-0.672927868386182));
#75046=CARTESIAN_POINT('Ctrl Pts',(0.281075492974673,0.0881683352629315,
-0.673737646577296));
#75047=CARTESIAN_POINT('Ctrl Pts',(0.28518606934168,0.0737823933043825,
-0.674547424768411));
#75048=CARTESIAN_POINT('Ctrl Pts',(0.288180019703266,0.0592107781052175,
-0.675357202959525));
#75049=CARTESIAN_POINT('Ctrl Pts',(0.291500623452659,0.0430493344534132,
-0.676255331576516));
#75050=CARTESIAN_POINT('Ctrl Pts',(0.293468083934822,0.0265560104497036,
-0.677153460193507));
#75051=CARTESIAN_POINT('Ctrl Pts',(0.294030695728291,0.00997947741802725,
-0.678051588810499));
#75052=CARTESIAN_POINT('Ctrl Pts',(0.294592213874118,-0.00656483288654887,
-0.678947971576698));
#75053=CARTESIAN_POINT('Ctrl Pts',(0.293754211203151,-0.0231912515321944,
-0.679844354342896));
#75054=CARTESIAN_POINT('Ctrl Pts',(0.291516584350613,-0.0396449372373334,
-0.680740737109095));
#75055=CARTESIAN_POINT('Ctrl Pts',(0.289279345087178,-0.0560957729278373,
-0.681636964608927));
#75056=CARTESIAN_POINT('Ctrl Pts',(0.285643016641729,-0.0723731460790802,
-0.682533192108759));
#75057=CARTESIAN_POINT('Ctrl Pts',(0.280659442297586,-0.0882265121673074,
-0.683429419608591));
#75058=CARTESIAN_POINT('Ctrl Pts',(0.275677205489516,-0.104075623387933,
-0.684325406570904));
#75059=CARTESIAN_POINT('Ctrl Pts',(0.26934868833006,-0.119500201389496,
-0.685221393533216));
#75060=CARTESIAN_POINT('Ctrl Pts',(0.261775411020823,-0.134265685060924,
-0.686117380495529));
#75061=CARTESIAN_POINT('Ctrl Pts',(0.254183941021239,-0.149066638696185,
-0.687015519817077));
#75062=CARTESIAN_POINT('Ctrl Pts',(0.245342124890783,-0.163204640416536,
-0.687913659138625));
#75063=CARTESIAN_POINT('Ctrl Pts',(0.235397357742065,-0.176470178693326,
-0.688811798460173));
#75064=CARTESIAN_POINT('Ctrl Pts',(0.226430980967861,-0.188430621056992,
-0.689621576651286));
#75065=CARTESIAN_POINT('Ctrl Pts',(0.216568876661155,-0.199681890440784,
-0.690431354842399));
#75066=CARTESIAN_POINT('Ctrl Pts',(0.205945555088724,-0.210095379147656,
-0.691241133033512));
#75067=CARTESIAN_POINT('Ctrl Pts',(0.194163181574088,-0.221645026091718,
-0.692139261650503));
#75068=CARTESIAN_POINT('Ctrl Pts',(0.181368533382261,-0.232237363656557,
-0.693037390267494));
#75069=CARTESIAN_POINT('Ctrl Pts',(0.167742570550849,-0.241694166303189,
-0.693935518884485));
#75070=CARTESIAN_POINT('Ctrl Pts',(0.154143094903518,-0.251132586096761,
-0.694831901650684));
#75071=CARTESIAN_POINT('Ctrl Pts',(0.139716117178592,-0.259439351964486,
-0.695728284416883));
#75072=CARTESIAN_POINT('Ctrl Pts',(0.124675749403214,-0.266476260688916,
-0.696624667183082));
#75073=CARTESIAN_POINT('Ctrl Pts',(0.10963798683551,-0.273511950519706,
-0.697520894682914));
#75074=CARTESIAN_POINT('Ctrl Pts',(0.0939877373242821,-0.279277837398947,
-0.698417122182746));
#75075=CARTESIAN_POINT('Ctrl Pts',(0.0779636554399853,-0.283681702671207,
-0.699313349682578));
#75076=CARTESIAN_POINT('Ctrl Pts',(0.0619438742415205,-0.288084385994878,
-0.70020933664489));
#75077=CARTESIAN_POINT('Ctrl Pts',(0.0455512261481134,-0.291125573994551,
-0.701105323607202));
#75078=CARTESIAN_POINT('Ctrl Pts',(0.0290378567090644,-0.292763458918192,
-0.702001310569515));
#75079=CARTESIAN_POINT('Ctrl Pts',(0.0124848184972283,-0.294405278404377,
-0.702899449891063));
#75080=CARTESIAN_POINT('Ctrl Pts',(-0.00418872658918546,-0.294637009672879,
-0.703797589212611));
#75081=CARTESIAN_POINT('Ctrl Pts',(-0.0207268217851637,-0.293468974269319,
-0.704695728534159));
#75082=CARTESIAN_POINT('Ctrl Pts',(-0.0356378589605347,-0.29241585302904,
-0.705505506725273));
#75083=CARTESIAN_POINT('Ctrl Pts',(-0.0504383662596673,-0.290225613820241,
-0.706315284916387));
#75084=CARTESIAN_POINT('Ctrl Pts',(-0.0649473615191108,-0.286941597248823,
-0.707125063107501));
#75085=CARTESIAN_POINT('Ctrl Pts',(-0.0810393531154373,-0.283299279767532,
-0.708023191724492));
#75086=CARTESIAN_POINT('Ctrl Pts',(-0.0968754466213217,-0.278287415851489,
-0.708921320341483));
#75087=CARTESIAN_POINT('Ctrl Pts',(-0.112207786762964,-0.271961491005174,
-0.709819448958474));
#75088=CARTESIAN_POINT('Ctrl Pts',(-0.127510322734392,-0.265647862973248,
-0.710715831724673));
#75089=CARTESIAN_POINT('Ctrl Pts',(-0.142310300624418,-0.25802548146143,
-0.711612214490872));
#75090=CARTESIAN_POINT('Ctrl Pts',(-0.156375532443047,-0.249199383733494,
-0.712508597257071));
#75091=CARTESIAN_POINT('Ctrl Pts',(-0.170438327961547,-0.24037481481243,
-0.713404824756903));
#75092=CARTESIAN_POINT('Ctrl Pts',(-0.183765933494337,-0.230347318014614,
-0.714301052256735));
#75093=CARTESIAN_POINT('Ctrl Pts',(-0.196151505051165,-0.219267478359566,
-0.715197279756567));
#75094=CARTESIAN_POINT('Ctrl Pts',(-0.20853375245797,-0.208190612410582,
-0.716093266718879));
#75095=CARTESIAN_POINT('Ctrl Pts',(-0.219973884915605,-0.196062500219674,
-0.71698925368119));
#75096=CARTESIAN_POINT('Ctrl Pts',(-0.230300111938318,-0.183072385796434,
-0.717885240643502));
#75097=CARTESIAN_POINT('Ctrl Pts',(-0.240651144846651,-0.170051066239714,
-0.71878337996505));
#75098=CARTESIAN_POINT('Ctrl Pts',(-0.249882453865169,-0.156164247347902,
-0.719681519286598));
#75099=CARTESIAN_POINT('Ctrl Pts',(-0.257863992289351,-0.141632628587475,
-0.720579658608146));
#75100=CARTESIAN_POINT('Ctrl Pts',(-0.265060287554879,-0.128530665816827,
-0.72138943679926));
#75101=CARTESIAN_POINT('Ctrl Pts',(-0.271241047516034,-0.114905308191939,
-0.722199214990374));
#75102=CARTESIAN_POINT('Ctrl Pts',(-0.276344608604166,-0.100932142033202,
-0.723008993181488));
#75103=CARTESIAN_POINT('Ctrl Pts',(-0.282853432122522,-0.0831114731023674,
-0.724041743303208));
#75104=CARTESIAN_POINT('Ctrl Pts',(-0.287644757357304,-0.0646316025977172,
-0.725074493424929));
#75105=CARTESIAN_POINT('Ctrl Pts',(-0.290611796733505,-0.0458085537790022,
-0.726107243546649));
#75106=CARTESIAN_POINT('Ctrl Pts',(-0.292982115349434,-0.0307711318352943,
-0.726932290513922));
#75107=CARTESIAN_POINT('Ctrl Pts',(-0.29418894365814,-0.0155151878871746,
-0.727757337481196));
#75108=CARTESIAN_POINT('Ctrl Pts',(-0.294199924273098,-0.000211086956616954,
-0.728582384448469));
#75109=CARTESIAN_POINT('',(-0.294199926155906,0.000208446298696108,-0.828582392147458));
#75110=CARTESIAN_POINT('Ctrl Pts',(-0.293886246767337,-0.000210790693305624,
-0.728582388291039));
#75111=CARTESIAN_POINT('Ctrl Pts',(-0.293464789150248,0.0634728800831282,
-0.732019233279185));
#75112=CARTESIAN_POINT('Ctrl Pts',(-0.241834069345054,0.225887162901957,
-0.740750721625328));
#75113=CARTESIAN_POINT('Ctrl Pts',(0.0260766885068273,0.34680284923634,
-0.754776853329467));
#75114=CARTESIAN_POINT('Ctrl Pts',(0.30558513020711,0.166041976976387,-0.770660783403452));
#75115=CARTESIAN_POINT('Ctrl Pts',(0.305159306794442,-0.166823281944281,
-0.786544713477441));
#75116=CARTESIAN_POINT('Ctrl Pts',(0.0251892979955619,-0.346868432101308,
-0.802428643551431));
#75117=CARTESIAN_POINT('Ctrl Pts',(-0.242152253072789,-0.225385360111962,
-0.816441201822627));
#75118=CARTESIAN_POINT('Ctrl Pts',(-0.29346671564659,-0.0632269917679521,
-0.825159116735832));
#75119=CARTESIAN_POINT('Ctrl Pts',(-0.293880751489893,0.000208148696046392,
-0.828582388291039));
#75120=CARTESIAN_POINT('',(-0.294226564582519,0.000102116486780654,-0.92858238829104));
#75121=CARTESIAN_POINT('Ctrl Pts',(-0.294199926155906,0.000208446298696108,
-0.828582392147458));
#75122=CARTESIAN_POINT('Ctrl Pts',(-0.294186382166594,0.0193243561534274,
-0.82961286660516));
#75123=CARTESIAN_POINT('Ctrl Pts',(-0.29230559241569,0.0383650065048286,
-0.830643341062863));
#75124=CARTESIAN_POINT('Ctrl Pts',(-0.2886255007607,0.0569996518466133,
-0.831673815520566));
#75125=CARTESIAN_POINT('Ctrl Pts',(-0.285622442753231,0.072206045098832,
-0.83251471158018));
#75126=CARTESIAN_POINT('Ctrl Pts',(-0.281422252442576,0.0871423322379511,
-0.833355607639793));
#75127=CARTESIAN_POINT('Ctrl Pts',(-0.276085466300458,0.101638847384545,
-0.834196503699406));
#75128=CARTESIAN_POINT('Ctrl Pts',(-0.270385451058139,0.117122015548989,
-0.835094632316397));
#75129=CARTESIAN_POINT('Ctrl Pts',(-0.26336068465324,0.132173702975884,
-0.835992760933389));
#75130=CARTESIAN_POINT('Ctrl Pts',(-0.255098351272925,0.146555351924913,
-0.83689088955038));
#75131=CARTESIAN_POINT('Ctrl Pts',(-0.246852078845356,0.160909044729651,
-0.83778727231658));
#75132=CARTESIAN_POINT('Ctrl Pts',(-0.237373346872821,0.174594573058873,
-0.838683655082779));
#75133=CARTESIAN_POINT('Ctrl Pts',(-0.226796438815704,0.187395345034275,
-0.839580037848979));
#75134=CARTESIAN_POINT('Ctrl Pts',(-0.216221362830944,0.200193899732153,
-0.840476265348811));
#75135=CARTESIAN_POINT('Ctrl Pts',(-0.204548950046839,0.212107360231338,
-0.841372492848643));
#75136=CARTESIAN_POINT('Ctrl Pts',(-0.191955357163281,0.222950175726141,
-0.842268720348476));
#75137=CARTESIAN_POINT('Ctrl Pts',(-0.179365144260358,0.233790081129539,
-0.843164707310788));
#75138=CARTESIAN_POINT('Ctrl Pts',(-0.165854849107379,0.243559403564761,
-0.844060694273101));
#75139=CARTESIAN_POINT('Ctrl Pts',(-0.151634410991388,0.252112366621105,
-0.844956681235414));
#75140=CARTESIAN_POINT('Ctrl Pts',(-0.13737981223177,0.260685875790062,
-0.845854820556962));
#75141=CARTESIAN_POINT('Ctrl Pts',(-0.122412358134403,0.268036802464494,
-0.84675295987851));
#75142=CARTESIAN_POINT('Ctrl Pts',(-0.106967759667312,0.274064843407096,
-0.847651099200059));
#75143=CARTESIAN_POINT('Ctrl Pts',(-0.0930426383536563,0.27949983102353,
-0.84846087739117));
#75144=CARTESIAN_POINT('Ctrl Pts',(-0.0787303505568327,0.283859943650873,
-0.849270655582282));
#75145=CARTESIAN_POINT('Ctrl Pts',(-0.0642130005341933,0.287106827787839,
-0.850080433773393));
#75146=CARTESIAN_POINT('Ctrl Pts',(-0.0481117426325573,0.290707961519855,
-0.850978562390384));
#75147=CARTESIAN_POINT('Ctrl Pts',(-0.0316551246912963,0.292961927663236,
-0.851876691007376));
#75148=CARTESIAN_POINT('Ctrl Pts',(-0.0150908813271618,0.293812704457737,
-0.852774819624367));
#75149=CARTESIAN_POINT('Ctrl Pts',(0.0014411631994639,0.294661827447524,
-0.853671202390565));
#75150=CARTESIAN_POINT('Ctrl Pts',(0.0180796399818894,0.29411306901486,
-0.854567585156764));
#75151=CARTESIAN_POINT('Ctrl Pts',(0.0345697480681757,0.292161894364243,
-0.855463967922963));
#75152=CARTESIAN_POINT('Ctrl Pts',(0.0510569998309474,0.290211057685093,
-0.856360195422795));
#75153=CARTESIAN_POINT('Ctrl Pts',(0.0673951441060099,0.28685832701963,
-0.857256422922626));
#75154=CARTESIAN_POINT('Ctrl Pts',(0.0833327727470031,0.282151181082583,
-0.858152650422458));
#75155=CARTESIAN_POINT('Ctrl Pts',(0.0992661239052585,0.27744529849129,
-0.859048637384771));
#75156=CARTESIAN_POINT('Ctrl Pts',(0.114798416563009,0.27138595688038,-0.859944624347083));
#75157=CARTESIAN_POINT('Ctrl Pts',(0.129693359735733,0.264070582307946,
-0.860840611309396));
#75158=CARTESIAN_POINT('Ctrl Pts',(0.144624083862702,0.25673763458469,-0.861738750630944));
#75159=CARTESIAN_POINT('Ctrl Pts',(0.158913698638014,0.24814300168371,-0.862636889952492));
#75160=CARTESIAN_POINT('Ctrl Pts',(0.172350161151186,0.238430413226082,
-0.86353502927404));
#75161=CARTESIAN_POINT('Ctrl Pts',(0.18446471180924,0.229673372838747,-0.864344807465154));
#75162=CARTESIAN_POINT('Ctrl Pts',(0.195885772560792,0.220008408513269,
-0.865154585656267));
#75163=CARTESIAN_POINT('Ctrl Pts',(0.206482416149396,0.209567773813408,
-0.865964363847381));
#75164=CARTESIAN_POINT('Ctrl Pts',(0.218235200992725,0.197988019127006,
-0.866862492464372));
#75165=CARTESIAN_POINT('Ctrl Pts',(0.229048423692114,0.185379496124944,
-0.867760621081363));
#75166=CARTESIAN_POINT('Ctrl Pts',(0.23874073893431,0.17192003831171,-0.868658749698355));
#75167=CARTESIAN_POINT('Ctrl Pts',(0.248414213516132,0.158486744017422,
-0.869555132464553));
#75168=CARTESIAN_POINT('Ctrl Pts',(0.256970594749501,0.144206394384238,
-0.870451515230752));
#75169=CARTESIAN_POINT('Ctrl Pts',(0.264267977109875,0.129290665843496,
-0.871347897996951));
#75170=CARTESIAN_POINT('Ctrl Pts',(0.271564095458836,0.114377520921123,
-0.872244125496783));
#75171=CARTESIAN_POINT('Ctrl Pts',(0.277601253414187,0.098829901003913,
-0.873140352996615));
#75172=CARTESIAN_POINT('Ctrl Pts',(0.282283096289123,0.0828848209832521,
-0.874036580496447));
#75173=CARTESIAN_POINT('Ctrl Pts',(0.286963682609365,0.0669440204451968,
-0.874932567458759));
#75174=CARTESIAN_POINT('Ctrl Pts',(0.290289463263858,0.0506067342873947,
-0.875828554421072));
#75175=CARTESIAN_POINT('Ctrl Pts',(0.29221425225179,0.0341243429376654,
-0.876724541383384));
#75176=CARTESIAN_POINT('Ctrl Pts',(0.294143665009407,0.0176023572313884,
-0.877622680704933));
#75177=CARTESIAN_POINT('Ctrl Pts',(0.294665298255285,0.000935362784691756,
-0.878520820026481));
#75178=CARTESIAN_POINT('Ctrl Pts',(0.293785021130875,-0.0156205428564806,
-0.879418959348029));
#75179=CARTESIAN_POINT('Ctrl Pts',(0.29299134781051,-0.0305476382421383,
-0.880228737539143));
#75180=CARTESIAN_POINT('Ctrl Pts',(0.291058806445921,-0.0453839938585814,
-0.881038515730256));
#75181=CARTESIAN_POINT('Ctrl Pts',(0.288027583983001,-0.0599479012552985,
-0.88184829392137));
#75182=CARTESIAN_POINT('Ctrl Pts',(0.284665641579156,-0.0761007961489109,
-0.882746422538361));
#75183=CARTESIAN_POINT('Ctrl Pts',(0.279929909993913,-0.0920216467478163,
-0.883644551155352));
#75184=CARTESIAN_POINT('Ctrl Pts',(0.27387155637594,-0.107461670414247,
-0.884542679772343));
#75185=CARTESIAN_POINT('Ctrl Pts',(0.267824979447033,-0.122871680587019,
-0.885439062538542));
#75186=CARTESIAN_POINT('Ctrl Pts',(0.260461107918113,-0.137801966637939,
-0.886335445304741));
#75187=CARTESIAN_POINT('Ctrl Pts',(0.25188092564397,-0.152018549186396,
-0.88723182807094));
#75188=CARTESIAN_POINT('Ctrl Pts',(0.243302229580607,-0.166232669218608,
-0.888128055570772));
#75189=CARTESIAN_POINT('Ctrl Pts',(0.233508003272942,-0.179732628192698,
-0.889024283070604));
#75190=CARTESIAN_POINT('Ctrl Pts',(0.222645212152586,-0.192308994863813,
-0.889920510570435));
#75191=CARTESIAN_POINT('Ctrl Pts',(0.211785336484869,-0.204881986177619,
-0.890816497532748));
#75192=CARTESIAN_POINT('Ctrl Pts',(0.199857991045912,-0.216531285158395,
-0.89171248449506));
#75193=CARTESIAN_POINT('Ctrl Pts',(0.187049403959069,-0.227081836522777,
-0.892608471457372));
#75194=CARTESIAN_POINT('Ctrl Pts',(0.174210047807639,-0.237657732649556,
-0.89350661077892));
#75195=CARTESIAN_POINT('Ctrl Pts',(0.160485852256959,-0.247129124396079,
-0.894404750100469));
#75196=CARTESIAN_POINT('Ctrl Pts',(0.14609522201564,-0.255362146968185,
-0.895302889422017));
#75197=CARTESIAN_POINT('Ctrl Pts',(0.133120376970759,-0.262785184759634,
-0.89611266761313));
#75198=CARTESIAN_POINT('Ctrl Pts',(0.119604557020921,-0.26920194213287,
-0.896922445804244));
#75199=CARTESIAN_POINT('Ctrl Pts',(0.105722249667185,-0.27454771156451,
-0.897732223995358));
#75200=CARTESIAN_POINT('Ctrl Pts',(0.090325320432641,-0.28047672837316,
-0.898630352612349));
#75201=CARTESIAN_POINT('Ctrl Pts',(0.0743788480752792,-0.285125454735937,
-0.89952848122934));
#75202=CARTESIAN_POINT('Ctrl Pts',(0.0581196400357285,-0.288402058664839,
-0.900426609846331));
#75203=CARTESIAN_POINT('Ctrl Pts',(0.0418920378827949,-0.291672293281533,
-0.90132299261253));
#75204=CARTESIAN_POINT('Ctrl Pts',(0.0253536605572101,-0.293575480317353,
-0.902219375378729));
#75205=CARTESIAN_POINT('Ctrl Pts',(0.008755874039357,-0.294069676556096,
-0.903115758144927));
#75206=CARTESIAN_POINT('Ctrl Pts',(-0.00783903750352962,-0.294563787192954,
-0.904011985644759));
#75207=CARTESIAN_POINT('Ctrl Pts',(-0.0244925507017758,-0.2936493149825,
-0.904908213144591));
#75208=CARTESIAN_POINT('Ctrl Pts',(-0.040949009134943,-0.291336263878815,
-0.905804440644423));
#75209=CARTESIAN_POINT('Ctrl Pts',(-0.0574010508372113,-0.289023833572388,
-0.906700427606735));
#75210=CARTESIAN_POINT('Ctrl Pts',(-0.0736553602296598,-0.285313690429837,
-0.907596414569047));
#75211=CARTESIAN_POINT('Ctrl Pts',(-0.0894638911694246,-0.280267465426912,
-0.90849240153136));
#75212=CARTESIAN_POINT('Ctrl Pts',(-0.105310397703702,-0.275209118273279,
-0.909390540852908));
#75213=CARTESIAN_POINT('Ctrl Pts',(-0.120708237687313,-0.268808545723231,
-0.910288680174456));
#75214=CARTESIAN_POINT('Ctrl Pts',(-0.135426542626646,-0.261176743896147,
-0.911186819496004));
#75215=CARTESIAN_POINT('Ctrl Pts',(-0.148696824935961,-0.254295777290848,
-0.911996597687118));
#75216=CARTESIAN_POINT('Ctrl Pts',(-0.161414623626742,-0.246414802696017,
-0.912806375878232));
#75217=CARTESIAN_POINT('Ctrl Pts',(-0.173430991634858,-0.237645389478841,
-0.913616154069346));
#75218=CARTESIAN_POINT('Ctrl Pts',(-0.186644434147676,-0.228002364453471,
-0.914506602628278));
#75219=CARTESIAN_POINT('Ctrl Pts',(-0.199096911507697,-0.217220371107064,
-0.915397051187209));
#75220=CARTESIAN_POINT('Ctrl Pts',(-0.210584816913836,-0.205445065371174,
-0.916287499746141));
#75221=CARTESIAN_POINT('Ctrl Pts',(-0.222050403937057,-0.193692636371566,
-0.917176218366393));
#75222=CARTESIAN_POINT('Ctrl Pts',(-0.232554531148838,-0.180951245852864,
-0.918064936986646));
#75223=CARTESIAN_POINT('Ctrl Pts',(-0.241927388344893,-0.167406029666256,
-0.918953655606898));
#75224=CARTESIAN_POINT('Ctrl Pts',(-0.251298231000653,-0.153863724799348,
-0.919842183211814));
#75225=CARTESIAN_POINT('Ctrl Pts',(-0.259537787311925,-0.139518569562698,
-0.92073071081673));
#75226=CARTESIAN_POINT('Ctrl Pts',(-0.266517539952699,-0.124587482908844,
-0.921619238421645));
#75227=CARTESIAN_POINT('Ctrl Pts',(-0.273495931809403,-0.109659307244236,
-0.922507592797756));
#75228=CARTESIAN_POINT('Ctrl Pts',(-0.279214680733987,-0.0941461641430382,
-0.923395947173867));
#75229=CARTESIAN_POINT('Ctrl Pts',(-0.283592790252211,-0.0782864567914893,
-0.924284301549977));
#75230=CARTESIAN_POINT('Ctrl Pts',(-0.287980331297603,-0.0623925837206593,
-0.925174569660406));
#75231=CARTESIAN_POINT('Ctrl Pts',(-0.291021293038947,-0.0461514454841997,
-0.926064837770835));
#75232=CARTESIAN_POINT('Ctrl Pts',(-0.292685522236561,-0.0298131694576637,
-0.926955105881264));
#75233=CARTESIAN_POINT('Ctrl Pts',(-0.293699512991103,-0.0198584944286457,
-0.927497533351189));
#75234=CARTESIAN_POINT('Ctrl Pts',(-0.294203442548764,-0.00986790586406562,
-0.928039960821115));
#75235=CARTESIAN_POINT('Ctrl Pts',(-0.294199982280943,0.000102107260926923,
-0.92858238829104));
#75236=CARTESIAN_POINT('',(-0.294185285097018,-0.000269622437996053,-1.02858238829104));
#75237=CARTESIAN_POINT('Ctrl Pts',(-0.294640422509188,0.00010226012342875,
-0.92858238829104));
#75238=CARTESIAN_POINT('Ctrl Pts',(-0.294665749914346,0.00573321420193211,
-0.928888286908471));
#75239=CARTESIAN_POINT('Ctrl Pts',(-0.29196650606935,0.108802724357824,
-0.934488828883914));
#75240=CARTESIAN_POINT('Ctrl Pts',(-0.17133070467475,0.302651614166351,
-0.945384014217309));
#75241=CARTESIAN_POINT('Ctrl Pts',(0.161491629393738,0.308014063895984,
-0.961267944291316));
#75242=CARTESIAN_POINT('Ctrl Pts',(0.346377967474509,0.0312171999089644,
-0.977151874365297));
#75243=CARTESIAN_POINT('Ctrl Pts',(0.213961360511507,-0.274176487193874,
-0.993035804439286));
#75244=CARTESIAN_POINT('Ctrl Pts',(-0.114456655868126,-0.32840810563904,
-1.00891973451328));
#75245=CARTESIAN_POINT('Ctrl Pts',(-0.281231284280514,-0.144445699392593,
-1.0207685957972));
#75246=CARTESIAN_POINT('Ctrl Pts',(-0.294398628936313,-0.0235490913753662,
-1.02732281372311));
#75247=CARTESIAN_POINT('Ctrl Pts',(-0.294185285097018,-0.000269622437996053,
-1.02858238829104));
#75248=CARTESIAN_POINT('',(-0.294156470823094,5.4011646819036E-5,-1.12858239090245));
#75249=CARTESIAN_POINT('Ctrl Pts',(-0.294185285097018,-0.000269622437996053,
-1.02858238829104));
#75250=CARTESIAN_POINT('Ctrl Pts',(-0.293501834438824,0.0743065566550019,
-1.03261745708111));
#75251=CARTESIAN_POINT('Ctrl Pts',(-0.226814830045291,0.247826008594651,
-1.04194716922918));
#75252=CARTESIAN_POINT('Ctrl Pts',(0.0649346204485502,0.341666072341295,
-1.05657152473523));
#75253=CARTESIAN_POINT('Ctrl Pts',(0.322328030805379,0.130601877777676,
-1.07245545480923));
#75254=CARTESIAN_POINT('Ctrl Pts',(0.284449677226377,-0.20010145188811,
-1.08833938488322));
#75255=CARTESIAN_POINT('Ctrl Pts',(-0.0140016018153781,-0.347499877796429,
-1.10422331495721));
#75256=CARTESIAN_POINT('Ctrl Pts',(-0.25521828530379,-0.203143761611344,
-1.11763764942648));
#75257=CARTESIAN_POINT('Ctrl Pts',(-0.293639961408326,-0.0523650648297256,
-1.12575734053776));
#75258=CARTESIAN_POINT('Ctrl Pts',(-0.293725670975061,5.38840834055088E-5,
-1.12858238829104));
#75259=CARTESIAN_POINT('',(-0.294199899345979,0.000243361492577376,-1.22858238829104));
#75260=CARTESIAN_POINT('Ctrl Pts',(-0.294199995039683,5.40245347011106E-5,
-1.12858239116628));
#75261=CARTESIAN_POINT('Ctrl Pts',(-0.294196741129914,0.0177737558262076,
-1.1295358325691));
#75262=CARTESIAN_POINT('Ctrl Pts',(-0.292588338013046,0.0354528612017167,
-1.13048927397193));
#75263=CARTESIAN_POINT('Ctrl Pts',(-0.289421898081706,0.0528072429765333,
-1.13144271537476));
#75264=CARTESIAN_POINT('Ctrl Pts',(-0.286238793401952,0.0702529596297707,
-1.13240117467196));
#75265=CARTESIAN_POINT('Ctrl Pts',(-0.281481430394538,0.0873699267563183,
-1.13335963396916));
#75266=CARTESIAN_POINT('Ctrl Pts',(-0.275247570906157,0.103886547301661,
-1.13431809326636));
#75267=CARTESIAN_POINT('Ctrl Pts',(-0.271620306077327,0.113496991185887,
-1.13487578721264));
#75268=CARTESIAN_POINT('Ctrl Pts',(-0.267494065615411,0.122904544285773,
-1.13543348115891));
#75269=CARTESIAN_POINT('Ctrl Pts',(-0.262895278083352,0.132059504623776,
-1.13599117510519));
#75270=CARTESIAN_POINT('Ctrl Pts',(-0.255489239854686,0.146802952928902,
-1.13688930372218));
#75271=CARTESIAN_POINT('Ctrl Pts',(-0.246815415719676,0.160968594895102,
-1.13778743233917));
#75272=CARTESIAN_POINT('Ctrl Pts',(-0.236987279564667,0.174329198141156,
-1.13868556095616));
#75273=CARTESIAN_POINT('Ctrl Pts',(-0.227178248089065,0.187663830029297,
-1.13958194372236));
#75274=CARTESIAN_POINT('Ctrl Pts',(-0.216219768717126,0.200195860004963,
-1.14047832648855));
#75275=CARTESIAN_POINT('Ctrl Pts',(-0.204269643802464,0.211725181829688,
-1.14137470925475));
#75276=CARTESIAN_POINT('Ctrl Pts',(-0.192321588821037,0.223252506610316,
-1.14227093675458));
#75277=CARTESIAN_POINT('Ctrl Pts',(-0.179382760267418,0.23377688198026,
-1.14316716425441));
#75278=CARTESIAN_POINT('Ctrl Pts',(-0.165649074942735,0.243133757365398,
-1.14406339175424));
#75279=CARTESIAN_POINT('Ctrl Pts',(-0.151919075586849,0.252488121468976,
-1.14495937871655));
#75280=CARTESIAN_POINT('Ctrl Pts',(-0.137395303356355,0.260675170764054,
-1.14585536567886));
#75281=CARTESIAN_POINT('Ctrl Pts',(-0.122302767525096,0.267573677808006,
-1.14675135264117));
#75282=CARTESIAN_POINT('Ctrl Pts',(-0.10717397607824,0.274488756594597,
-1.14764949196272));
#75283=CARTESIAN_POINT('Ctrl Pts',(-0.0914744261301407,0.280108804330703,
-1.14854763128427));
#75284=CARTESIAN_POINT('Ctrl Pts',(-0.0754496181504297,0.284360677873989,
-1.14944577060581));
#75285=CARTESIAN_POINT('Ctrl Pts',(-0.0610013697467702,0.288194241758942,
-1.15025554879693));
#75286=CARTESIAN_POINT('Ctrl Pts',(-0.0462893626626646,0.290916191733231,
-1.15106532698805));
#75287=CARTESIAN_POINT('Ctrl Pts',(-0.0314988602969082,0.292508908924149,
-1.15187510517916));
#75288=CARTESIAN_POINT('Ctrl Pts',(-0.0150946479087731,0.294275398690888,
-1.15277323379615));
#75289=CARTESIAN_POINT('Ctrl Pts',(0.00151107934364759,0.294663290245999,
-1.15367136241314));
#75290=CARTESIAN_POINT('Ctrl Pts',(0.0180658564198836,0.293644793639894,
-1.15456949103014));
#75291=CARTESIAN_POINT('Ctrl Pts',(0.0345884530599,0.292628276865045,-1.15546587379634));
#75292=CARTESIAN_POINT('Ctrl Pts',(0.0510595112019997,0.290210780404567,
-1.15636225656253));
#75293=CARTESIAN_POINT('Ctrl Pts',(0.067225337852934,0.286416469412216,
-1.15725863932873));
#75294=CARTESIAN_POINT('Ctrl Pts',(0.0833883643505557,0.282622815649015,
-1.15815486682857));
#75295=CARTESIAN_POINT('Ctrl Pts',(0.0992454840209208,0.277452949400478,
-1.1590510943284));
#75296=CARTESIAN_POINT('Ctrl Pts',(0.114552227882036,0.27098233722378,-1.15994732182823));
#75297=CARTESIAN_POINT('Ctrl Pts',(0.12985486358289,0.264513461687614,-1.16084330879055));
#75298=CARTESIAN_POINT('Ctrl Pts',(0.144606691656802,0.256744851487481,
-1.16173929575286));
#75299=CARTESIAN_POINT('Ctrl Pts',(0.158583884535607,0.247799902271162,
-1.16263528271517));
#75300=CARTESIAN_POINT('Ctrl Pts',(0.172594653729077,0.238833465304609,
-1.16353342203672));
#75301=CARTESIAN_POINT('Ctrl Pts',(0.185826415731223,0.228685496076821,
-1.16443156135827));
#75302=CARTESIAN_POINT('Ctrl Pts',(0.198084647298157,0.217522671243171,
-1.16532970067982));
#75303=CARTESIAN_POINT('Ctrl Pts',(0.20913688423552,0.207458072261,-1.16613947887093));
#75304=CARTESIAN_POINT('Ctrl Pts',(0.219397872621403,0.196569349588083,
-1.16694925706205));
#75305=CARTESIAN_POINT('Ctrl Pts',(0.228752398375091,0.18500264927196,-1.16775903525316));
#75306=CARTESIAN_POINT('Ctrl Pts',(0.239127544766995,0.17217397016936,-1.16865716387015));
#75307=CARTESIAN_POINT('Ctrl Pts',(0.248453335307034,0.158428779437926,
-1.16955529248714));
#75308=CARTESIAN_POINT('Ctrl Pts',(0.256569586884884,0.143964186816444,
-1.17045342110413));
#75309=CARTESIAN_POINT('Ctrl Pts',(0.264670061474919,0.129527711571482,
-1.17134980387033));
#75310=CARTESIAN_POINT('Ctrl Pts',(0.271565223520873,0.1143752600927,-1.17224618663653));
#75311=CARTESIAN_POINT('Ctrl Pts',(0.277137887352363,0.0987331321992221,
-1.17314256940273));
#75312=CARTESIAN_POINT('Ctrl Pts',(0.282709585918454,0.0830937137469134,
-1.17403879690256));
#75313=CARTESIAN_POINT('Ctrl Pts',(0.286958926216699,0.0669655127220728,
-1.17493502440239));
#75314=CARTESIAN_POINT('Ctrl Pts',(0.289816835300472,0.0505948809309715,
-1.17583125190223));
#75315=CARTESIAN_POINT('Ctrl Pts',(0.292673977353148,0.0342286428358504,
-1.17672723886454));
#75316=CARTESIAN_POINT('Ctrl Pts',(0.29414030402327,0.0176208849480362,
-1.17762322582685));
#75317=CARTESIAN_POINT('Ctrl Pts',(0.294198208894361,0.00102658820850397,
-1.17851921278916));
#75318=CARTESIAN_POINT('Ctrl Pts',(0.294256252865784,-0.01560757170912,
-1.17941735211071));
#75319=CARTESIAN_POINT('Ctrl Pts',(0.292899141155415,-0.0322274108459776,
-1.18031549143226));
#75320=CARTESIAN_POINT('Ctrl Pts',(0.290161522676543,-0.048579118539039,
-1.18121363075381));
#75321=CARTESIAN_POINT('Ctrl Pts',(0.287693237760616,-0.0633221054672461,
-1.18202340894492));
#75322=CARTESIAN_POINT('Ctrl Pts',(0.284103528081797,-0.0778467792510078,
-1.18283318713603));
#75323=CARTESIAN_POINT('Ctrl Pts',(0.27945277186965,-0.0919771074472861,
-1.18364296532715));
#75324=CARTESIAN_POINT('Ctrl Pts',(0.274294597334179,-0.107649117708652,
-1.18454109394414));
#75325=CARTESIAN_POINT('Ctrl Pts',(0.267797468983183,-0.122935973521103,
-1.18543922256113));
#75326=CARTESIAN_POINT('Ctrl Pts',(0.260040222950703,-0.137596229773017,
-1.18633735117812));
#75327=CARTESIAN_POINT('Ctrl Pts',(0.252298056043723,-0.152227988302547,
-1.18723373394432));
#75328=CARTESIAN_POINT('Ctrl Pts',(0.243300940961319,-0.166234842540761,
-1.18813011671052));
#75329=CARTESIAN_POINT('Ctrl Pts',(0.233175548442287,-0.179395662178991,
-1.18902649947671));
#75330=CARTESIAN_POINT('Ctrl Pts',(0.223051909786638,-0.192554202174274,
-1.18992272697655));
#75331=CARTESIAN_POINT('Ctrl Pts',(0.211800820724213,-0.204866340744693,
-1.19081895447638));
#75332=CARTESIAN_POINT('Ctrl Pts',(0.199591879296107,-0.216140513830814,
-1.19171518197621));
#75333=CARTESIAN_POINT('Ctrl Pts',(0.187386214612451,-0.227411661053939,
-1.19261116893852));
#75334=CARTESIAN_POINT('Ctrl Pts',(0.174223796905752,-0.237644866616127,
-1.19350715590083));
#75335=CARTESIAN_POINT('Ctrl Pts',(0.160309369442262,-0.246687142082891,
-1.19440314286315));
#75336=CARTESIAN_POINT('Ctrl Pts',(0.146361516440544,-0.255751139099109,
-1.19530128218469));
#75337=CARTESIAN_POINT('Ctrl Pts',(0.131658726552284,-0.263618080984681,
-1.19619942150624));
#75338=CARTESIAN_POINT('Ctrl Pts',(0.116433080370029,-0.270179528823977,
-1.19709756082779));
#75339=CARTESIAN_POINT('Ctrl Pts',(0.102705370282942,-0.276095445469563,
-1.19790733901891));
#75340=CARTESIAN_POINT('Ctrl Pts',(0.0885533514090525,-0.280950600039411,
-1.19871711721002));
#75341=CARTESIAN_POINT('Ctrl Pts',(0.0741576842169672,-0.284700329946378,
-1.19952689540113));
#75342=CARTESIAN_POINT('Ctrl Pts',(0.0581913852875117,-0.288859172173035,
-1.20042502401813));
#75343=CARTESIAN_POINT('Ctrl Pts',(0.0418230963952611,-0.291684018395409,
-1.20132315263512));
#75344=CARTESIAN_POINT('Ctrl Pts',(0.0252984543023825,-0.293110266299068,
-1.20222128125211));
#75345=CARTESIAN_POINT('Ctrl Pts',(0.00880593406704758,-0.294533741753452,
-1.20311766401831));
#75346=CARTESIAN_POINT('Ctrl Pts',(-0.00784156235179397,-0.294563882115743,
-1.2040140467845));
#75347=CARTESIAN_POINT('Ctrl Pts',(-0.024389545782722,-0.29318729518264,
-1.2049104295507));
#75348=CARTESIAN_POINT('Ctrl Pts',(-0.0409346628652968,-0.291810946694161,
-1.20580665705053));
#75349=CARTESIAN_POINT('Ctrl Pts',(-0.0573795104557058,-0.289028367136229,
-1.20670288455037));
#75350=CARTESIAN_POINT('Ctrl Pts',(-0.0734711814793199,-0.284878264337652,
-1.2075991120502));
#75351=CARTESIAN_POINT('Ctrl Pts',(-0.0895585336769281,-0.280729275380631,
-1.20849509901251));
#75352=CARTESIAN_POINT('Ctrl Pts',(-0.105292133518021,-0.275213699979629,
-1.20939108597482));
#75353=CARTESIAN_POINT('Ctrl Pts',(-0.120432445137094,-0.26842068876728,
-1.21028707293713));
#75354=CARTESIAN_POINT('Ctrl Pts',(-0.135609127139796,-0.261611359236656,
-1.21118521225868));
#75355=CARTESIAN_POINT('Ctrl Pts',(-0.150188959871209,-0.253518814355502,
-1.21208335158023));
#75356=CARTESIAN_POINT('Ctrl Pts',(-0.163955030769725,-0.24427932349116,
-1.21298149090178));
#75357=CARTESIAN_POINT('Ctrl Pts',(-0.17636676213866,-0.235948836205473,
-1.21379126909289));
#75358=CARTESIAN_POINT('Ctrl Pts',(-0.18811699407947,-0.226686859448853,
-1.214601047284));
#75359=CARTESIAN_POINT('Ctrl Pts',(-0.199070279684257,-0.216621014092428,
-1.21541082547512));
#75360=CARTESIAN_POINT('Ctrl Pts',(-0.211037652827153,-0.205623243037651,
-1.21629557532331));
#75361=CARTESIAN_POINT('Ctrl Pts',(-0.222134545065787,-0.193590312477439,
-1.2171803251715));
#75362=CARTESIAN_POINT('Ctrl Pts',(-0.232176184747201,-0.180687186142885,
-1.21806507501969));
#75363=CARTESIAN_POINT('Ctrl Pts',(-0.242203172990491,-0.167802886350917,
-1.21894853395743));
#75364=CARTESIAN_POINT('Ctrl Pts',(-0.251177400380996,-0.154051495304126,
-1.21983199289516));
#75365=CARTESIAN_POINT('Ctrl Pts',(-0.258951788135257,-0.139633847693004,
-1.2207154518329));
#75366=CARTESIAN_POINT('Ctrl Pts',(-0.266718384557415,-0.125230649152887,
-1.22159802538619));
#75367=CARTESIAN_POINT('Ctrl Pts',(-0.273287117552961,-0.110163223906686,
-1.22248059893948));
#75368=CARTESIAN_POINT('Ctrl Pts',(-0.278555812509406,-0.0946588575740512,
-1.22336317249277));
#75369=CARTESIAN_POINT('Ctrl Pts',(-0.283832396389795,-0.0791312762388782,
-1.22424706754137));
#75370=CARTESIAN_POINT('Ctrl Pts',(-0.287804785773448,-0.0631662223080026,
-1.22513096258996));
#75371=CARTESIAN_POINT('Ctrl Pts',(-0.290420181564497,-0.0470080646277298,
-1.22601485763856));
#75372=CARTESIAN_POINT('Ctrl Pts',(-0.292952574549606,-0.0313627059780524,
-1.22687070118938));
#75373=CARTESIAN_POINT('Ctrl Pts',(-0.294212952872461,-0.0155370569154584,
-1.22772654474021));
#75374=CARTESIAN_POINT('Ctrl Pts',(-0.294199899345979,0.000243361492577376,
-1.22858238829104));
#75375=CARTESIAN_POINT('',(-0.294199932671572,-0.000199037792005543,-1.32858238829104));
#75376=CARTESIAN_POINT('Ctrl Pts',(-0.294383220786406,0.000243513135659165,
-1.22858238829104));
#75377=CARTESIAN_POINT('Ctrl Pts',(-0.294531804372818,0.0169246405636604,
-1.2294865107104));
#75378=CARTESIAN_POINT('Ctrl Pts',(-0.285648723188225,0.131134112473027,
-1.23568527648771));
#75379=CARTESIAN_POINT('Ctrl Pts',(-0.136187107091055,0.320008252681217,
-1.24717868562313));
#75380=CARTESIAN_POINT('Ctrl Pts',(0.195124888317045,0.287886241215498,
-1.26306261569707));
#75381=CARTESIAN_POINT('Ctrl Pts',(0.347690809990289,-0.00795679396688126,
-1.27894654577109));
#75382=CARTESIAN_POINT('Ctrl Pts',(0.181751144316383,-0.296510929750662,
-1.29483047584506));
#75383=CARTESIAN_POINT('Ctrl Pts',(-0.150683445319157,-0.313443311028766,
-1.31071440591904));
#75384=CARTESIAN_POINT('Ctrl Pts',(-0.288377247002049,-0.122059486604382,
-1.32196504340104));
#75385=CARTESIAN_POINT('Ctrl Pts',(-0.294601083516667,-0.0123879459390851,
-1.32792103752504));
#75386=CARTESIAN_POINT('Ctrl Pts',(-0.294506364479898,-0.000199245105141105,
-1.32858238829104));
#75387=CARTESIAN_POINT('',(-0.294199973927967,-0.00012385791773357,-1.42858238828812));
#75388=CARTESIAN_POINT('Ctrl Pts',(-0.294199932671572,-0.000199037792005543,
-1.32858238829104));
#75389=CARTESIAN_POINT('Ctrl Pts',(-0.29421095546823,0.0160938782514552,
-1.32946735688903));
#75390=CARTESIAN_POINT('Ctrl Pts',(-0.292864222061912,0.0324398188035349,
-1.33035232548702));
#75391=CARTESIAN_POINT('Ctrl Pts',(-0.290159642085904,0.0485903499120993,
-1.33123729408502));
#75392=CARTESIAN_POINT('Ctrl Pts',(-0.287459443285101,0.0647147186194478,
-1.33212082911384));
#75393=CARTESIAN_POINT('Ctrl Pts',(-0.283405838901624,0.0806434996177015,
-1.33300436414265));
#75394=CARTESIAN_POINT('Ctrl Pts',(-0.278050516457775,0.0961329823607096,
-1.33388789917147));
#75395=CARTESIAN_POINT('Ctrl Pts',(-0.272694507482042,0.111624450796248,
-1.33477154746611));
#75396=CARTESIAN_POINT('Ctrl Pts',(-0.266036680896201,0.126675727872778,
-1.33565519576074));
#75397=CARTESIAN_POINT('Ctrl Pts',(-0.258178495635449,0.14105851406922,
-1.33653884405538));
#75398=CARTESIAN_POINT('Ctrl Pts',(-0.250319312112871,0.155443127377896,
-1.33742260460397));
#75399=CARTESIAN_POINT('Ctrl Pts',(-0.241259888122196,0.169158383239423,
-1.33830636515255));
#75400=CARTESIAN_POINT('Ctrl Pts',(-0.231146528751372,0.182002533625747,
-1.33919012570114));
#75401=CARTESIAN_POINT('Ctrl Pts',(-0.221011611213856,0.194874063275963,
-1.34007577012002));
#75402=CARTESIAN_POINT('Ctrl Pts',(-0.209818833944237,0.206870188509988,
-1.34096141453889));
#75403=CARTESIAN_POINT('Ctrl Pts',(-0.197752936199888,0.217824278317002,
-1.34184705895777));
#75404=CARTESIAN_POINT('Ctrl Pts',(-0.19486827810482,0.220443130598484,
-1.34205879466085));
#75405=CARTESIAN_POINT('Ctrl Pts',(-0.191933860052037,0.22300260765447,
-1.34227053036394));
#75406=CARTESIAN_POINT('Ctrl Pts',(-0.188952462317281,0.225500791537938,
-1.34248226606702));
#75407=CARTESIAN_POINT('Ctrl Pts',(-0.176306136803009,0.236097447668901,
-1.34338039468402));
#75408=CARTESIAN_POINT('Ctrl Pts',(-0.162725190941781,0.245660843872892,
-1.34427852330101));
#75409=CARTESIAN_POINT('Ctrl Pts',(-0.148403919238009,0.254027393709416,
-1.345176651918));
#75410=CARTESIAN_POINT('Ctrl Pts',(-0.134110486312648,0.262377680009309,
-1.3460730346842));
#75411=CARTESIAN_POINT('Ctrl Pts',(-0.119080226176381,0.269535286151918,
-1.3469694174504));
#75412=CARTESIAN_POINT('Ctrl Pts',(-0.103537366684782,0.275379109047838,
-1.34786580021659));
#75413=CARTESIAN_POINT('Ctrl Pts',(-0.0879971994396348,0.281221919709718,
-1.34876202771643));
#75414=CARTESIAN_POINT('Ctrl Pts',(-0.0719453289797071,0.285751071507304,
-1.34965825521626));
#75415=CARTESIAN_POINT('Ctrl Pts',(-0.0556268687501311,0.288893218115372,
-1.35055448271609));
#75416=CARTESIAN_POINT('Ctrl Pts',(-0.039312788214266,0.292034521406144,
-1.3514504696784));
#75417=CARTESIAN_POINT('Ctrl Pts',(-0.0227330394533085,0.29378941940524,
-1.35234645664072));
#75418=CARTESIAN_POINT('Ctrl Pts',(-0.00614225869613748,0.294135874483392,
-1.35324244360303));
#75419=CARTESIAN_POINT('Ctrl Pts',(0.0104883767929551,0.294483161823417,
-1.35414058292458));
#75420=CARTESIAN_POINT('Ctrl Pts',(0.0271293018715402,0.293415258429718,
-1.35503872224613));
#75421=CARTESIAN_POINT('Ctrl Pts',(0.0435261417414881,0.290962394451757,
-1.35593686156767));
#75422=CARTESIAN_POINT('Ctrl Pts',(0.0583098206332988,0.288750849196508,
-1.35674663975879));
#75423=CARTESIAN_POINT('Ctrl Pts',(0.072894719894761,0.285414252481799,
-1.3575564179499));
#75424=CARTESIAN_POINT('Ctrl Pts',(0.0871037837793806,0.281009912371993,
-1.35836619614102));
#75425=CARTESIAN_POINT('Ctrl Pts',(0.102863120145144,0.276125039038795,
-1.35926432475801));
#75426=CARTESIAN_POINT('Ctrl Pts',(0.118260643424989,0.269894716873243,
-1.360162453375));
#75427=CARTESIAN_POINT('Ctrl Pts',(0.133053574128968,0.262393571589525,
-1.36106058199199));
#75428=CARTESIAN_POINT('Ctrl Pts',(0.147817749207858,0.254907007603174,
-1.36195696475819));
#75429=CARTESIAN_POINT('Ctrl Pts',(0.161978936831009,0.246154818702195,
-1.36285334752439));
#75430=CARTESIAN_POINT('Ctrl Pts',(0.175313837441747,0.236259811227912,
-1.36374973029059));
#75431=CARTESIAN_POINT('Ctrl Pts',(0.188646428256217,0.226366517711012,
-1.36464595779042));
#75432=CARTESIAN_POINT('Ctrl Pts',(0.201152350907598,0.215331226146877,
-1.36554218529025));
#75433=CARTESIAN_POINT('Ctrl Pts',(0.212637121153248,0.203320177817301,
-1.36643841279008));
#75434=CARTESIAN_POINT('Ctrl Pts',(0.224118809013962,0.191312353119861,
-1.36733439975239));
#75435=CARTESIAN_POINT('Ctrl Pts',(0.234579349172184,0.178329871247663,
-1.36823038671471));
#75436=CARTESIAN_POINT('Ctrl Pts',(0.243862216035669,0.164574784186924,
-1.36912637367702));
#75437=CARTESIAN_POINT('Ctrl Pts',(0.253167382402457,0.150786654358918,
-1.37002451299857));
#75438=CARTESIAN_POINT('Ctrl Pts',(0.261288802265385,0.136222886146696,
-1.37092265232011));
#75439=CARTESIAN_POINT('Ctrl Pts',(0.26811401744516,0.121113639402903,-1.37182079164166));
#75440=CARTESIAN_POINT('Ctrl Pts',(0.274267751358872,0.10749087709448,-1.37263056983277));
#75441=CARTESIAN_POINT('Ctrl Pts',(0.27936826190931,0.0934254245163044,
-1.37344034802389));
#75442=CARTESIAN_POINT('Ctrl Pts',(0.283367751749445,0.0790971381812571,
-1.374250126215));
#75443=CARTESIAN_POINT('Ctrl Pts',(0.28780360383611,0.0632055716619879,
-1.37514825483199));
#75444=CARTESIAN_POINT('Ctrl Pts',(0.290912651841137,0.0468888790454422,
-1.37604638344899));
#75445=CARTESIAN_POINT('Ctrl Pts',(0.292626031829465,0.0303915365807849,
-1.37694451206598));
#75446=CARTESIAN_POINT('Ctrl Pts',(0.294336081219308,0.0139262629065766,
-1.37784089483218));
#75447=CARTESIAN_POINT('Ctrl Pts',(0.294655701078259,-0.00271819228434685,
-1.37873727759837));
#75448=CARTESIAN_POINT('Ctrl Pts',(0.293567075904432,-0.0192876111771652,
-1.37963366036457));
#75449=CARTESIAN_POINT('Ctrl Pts',(0.292478639296118,-0.035854160008702,
-1.38052988786441));
#75450=CARTESIAN_POINT('Ctrl Pts',(0.289982440651052,-0.0523449075233701,
-1.38142611536424));
#75451=CARTESIAN_POINT('Ctrl Pts',(0.286112784133044,-0.0685063117941561,
-1.38232234286407));
#75452=CARTESIAN_POINT('Ctrl Pts',(0.282244166187922,-0.0846633785233022,
-1.38321832982638));
#75453=CARTESIAN_POINT('Ctrl Pts',(0.277003017012444,-0.100490510015907,
-1.38411431678869));
#75454=CARTESIAN_POINT('Ctrl Pts',(0.270474308459799,-0.11574665638019,
-1.38501030375101));
#75455=CARTESIAN_POINT('Ctrl Pts',(0.263929916502435,-0.13103945138883,
-1.38590844307255));
#75456=CARTESIAN_POINT('Ctrl Pts',(0.256092124579347,-0.145757801258977,
-1.3868065823941));
#75457=CARTESIAN_POINT('Ctrl Pts',(0.247093409551672,-0.159682456632311,
-1.38770472171565));
#75458=CARTESIAN_POINT('Ctrl Pts',(0.238980009990367,-0.172237170549782,
-1.38851449990676));
#75459=CARTESIAN_POINT('Ctrl Pts',(0.229923758957237,-0.184146682770158,
-1.38932427809787));
#75460=CARTESIAN_POINT('Ctrl Pts',(0.22004990273473,-0.195273347660237,
-1.39013405628899));
#75461=CARTESIAN_POINT('Ctrl Pts',(0.2090987645949,-0.207613981501867,-1.39103218490598));
#75462=CARTESIAN_POINT('Ctrl Pts',(0.197071263310841,-0.219069977761558,
-1.39193031352297));
#75463=CARTESIAN_POINT('Ctrl Pts',(0.184135533987629,-0.22945096452857,
-1.39282844213996));
#75464=CARTESIAN_POINT('Ctrl Pts',(0.17122495012004,-0.239811771943064,
-1.39372482490616));
#75465=CARTESIAN_POINT('Ctrl Pts',(0.157410211298321,-0.249101176485043,
-1.39462120767236));
#75466=CARTESIAN_POINT('Ctrl Pts',(0.142895306141158,-0.257166427596653,
-1.39551759043856));
#75467=CARTESIAN_POINT('Ctrl Pts',(0.128382915174002,-0.265230281690954,
-1.39641381793839));
#75468=CARTESIAN_POINT('Ctrl Pts',(0.113171262560871,-0.272069973646394,
-1.39731004543822));
#75469=CARTESIAN_POINT('Ctrl Pts',(0.0974920162052542,-0.277576920467525,
-1.39820627293805));
#75470=CARTESIAN_POINT('Ctrl Pts',(0.081816977985442,-0.283082389285213,
-1.39910225990037));
#75471=CARTESIAN_POINT('Ctrl Pts',(0.0656753457450195,-0.287255570874658,
-1.39999824686268));
#75472=CARTESIAN_POINT('Ctrl Pts',(0.0493157494804751,-0.290037233563519,
-1.40089423382499));
#75473=CARTESIAN_POINT('Ctrl Pts',(0.0329168538403857,-0.29282557842258,
-1.40179237314654));
#75474=CARTESIAN_POINT('Ctrl Pts',(0.016299736536797,-0.294215620741398,
-1.40269051246809));
#75475=CARTESIAN_POINT('Ctrl Pts',(-0.00027954726078042,-0.294199867187817,
-1.40358865178963));
#75476=CARTESIAN_POINT('Ctrl Pts',(-0.0152277208029774,-0.294185663507144,
-1.40439842998075));
#75477=CARTESIAN_POINT('Ctrl Pts',(-0.0301446655582793,-0.293029409525153,
-1.40520820817186));
#75478=CARTESIAN_POINT('Ctrl Pts',(-0.0448468247040668,-0.290761762124876,
-1.40601798636298));
#75479=CARTESIAN_POINT('Ctrl Pts',(-0.0611530552314759,-0.288246704241395,
-1.40691611497997));
#75480=CARTESIAN_POINT('Ctrl Pts',(-0.07729919491733,-0.284347626057459,
-1.40781424359696));
#75481=CARTESIAN_POINT('Ctrl Pts',(-0.0930341314336671,-0.279102652062611,
-1.40871237221395));
#75482=CARTESIAN_POINT('Ctrl Pts',(-0.108738481182302,-0.273867873647582,
-1.40960875498015));
#75483=CARTESIAN_POINT('Ctrl Pts',(-0.124032451266787,-0.267292577113482,
-1.41050513774635));
#75484=CARTESIAN_POINT('Ctrl Pts',(-0.138677114729015,-0.259465407810821,
-1.41140152051254));
#75485=CARTESIAN_POINT('Ctrl Pts',(-0.153319241525229,-0.251639594286284,
-1.41229774801237));
#75486=CARTESIAN_POINT('Ctrl Pts',(-0.167311564065965,-0.242562663572469,
-1.41319397551221));
#75487=CARTESIAN_POINT('Ctrl Pts',(-0.180437272370374,-0.232370460126797,
-1.41409020301204));
#75488=CARTESIAN_POINT('Ctrl Pts',(-0.193559457880269,-0.222180992155474,
-1.41498618997435));
#75489=CARTESIAN_POINT('Ctrl Pts',(-0.205814872157734,-0.210877339787728,
-1.41588217693666));
#75490=CARTESIAN_POINT('Ctrl Pts',(-0.217018987017479,-0.198636349326873,
-1.41677816389897));
#75491=CARTESIAN_POINT('Ctrl Pts',(-0.228250016643971,-0.186365953294303,
-1.41767630322052));
#75492=CARTESIAN_POINT('Ctrl Pts',(-0.238424185529855,-0.173154326119332,
-1.41857444254206));
#75493=CARTESIAN_POINT('Ctrl Pts',(-0.24739642205455,-0.159212594836611,
-1.41947258186361));
#75494=CARTESIAN_POINT('Ctrl Pts',(-0.255485948132456,-0.146642484979129,
-1.42028236005473));
#75495=CARTESIAN_POINT('Ctrl Pts',(-0.26259877260222,-0.133479662631015,
-1.42109213824585));
#75496=CARTESIAN_POINT('Ctrl Pts',(-0.26866117713439,-0.119895003652211,
-1.42190191643696));
#75497=CARTESIAN_POINT('Ctrl Pts',(-0.276031327328041,-0.103379943254638,
-1.4228863751382));
#75498=CARTESIAN_POINT('Ctrl Pts',(-0.281889563048866,-0.0861502897819955,
-1.42387083383943));
#75499=CARTESIAN_POINT('Ctrl Pts',(-0.286117995118731,-0.0684845447472487,
-1.42485529254066));
#75500=CARTESIAN_POINT('Ctrl Pts',(-0.290318258654323,-0.0509364835575405,
-1.42583319307607));
#75501=CARTESIAN_POINT('Ctrl Pts',(-0.292910121610845,-0.0329586072094055,
-1.42681109361149));
#75502=CARTESIAN_POINT('Ctrl Pts',(-0.293825270581318,-0.0148442031721232,
-1.4277889941469));
#75503=CARTESIAN_POINT('Ctrl Pts',(-0.294072764678868,-0.00994531979409522,
-1.42805345886064));
#75504=CARTESIAN_POINT('Ctrl Pts',(-0.294197905692056,-0.00503654304993215,
-1.42831792357438));
#75505=CARTESIAN_POINT('Ctrl Pts',(-0.294199973927967,-0.000123857917735108,
-1.42858238828812));
#75506=CARTESIAN_POINT('',(-0.294199884656848,0.000260514677417675,-1.52858238829104));
#75507=CARTESIAN_POINT('Ctrl Pts',(-0.294199973927989,-0.000123857863553138,
-1.42858238829104));
#75508=CARTESIAN_POINT('Ctrl Pts',(-0.29420711687311,0.0168428022082966,
-1.42949575496899));
#75509=CARTESIAN_POINT('Ctrl Pts',(-0.292742206137062,0.0338023587179249,
-1.43040912164694));
#75510=CARTESIAN_POINT('Ctrl Pts',(-0.289834972294292,0.050490878732371,
-1.43132248832489));
#75511=CARTESIAN_POINT('Ctrl Pts',(-0.286925430138747,0.0671926492543543,
-1.43223658020628));
#75512=CARTESIAN_POINT('Ctrl Pts',(-0.282571464413671,0.0836222276575034,
-1.43315067208766));
#75513=CARTESIAN_POINT('Ctrl Pts',(-0.276853623498289,0.0995274392108404,
-1.43406476396905));
#75514=CARTESIAN_POINT('Ctrl Pts',(-0.271119421515831,0.115478162039664,
-1.43498147143887));
#75515=CARTESIAN_POINT('Ctrl Pts',(-0.264013865578162,0.130900841221588,
-1.4358981789087));
#75516=CARTESIAN_POINT('Ctrl Pts',(-0.255665255464979,0.14556413414034,
-1.43681488637852));
#75517=CARTESIAN_POINT('Ctrl Pts',(-0.252717689366375,0.150741166546365,
-1.437138539756));
#75518=CARTESIAN_POINT('Ctrl Pts',(-0.249615575581539,0.155823795936581,
-1.43746219313348));
#75519=CARTESIAN_POINT('Ctrl Pts',(-0.246365814950903,0.160802752537317,
-1.43778584651096));
#75520=CARTESIAN_POINT('Ctrl Pts',(-0.2373478246445,0.174619210875247,-1.43868397512795));
#75521=CARTESIAN_POINT('Ctrl Pts',(-0.227135117003751,0.187718876523039,
-1.43958210374494));
#75522=CARTESIAN_POINT('Ctrl Pts',(-0.215866014277897,0.199888728746207,
-1.44048023236193));
#75523=CARTESIAN_POINT('Ctrl Pts',(-0.20461881729199,0.21203492428397,-1.44137661512813));
#75524=CARTESIAN_POINT('Ctrl Pts',(-0.19231978425414,0.22325427505796,-1.44227299789432));
#75525=CARTESIAN_POINT('Ctrl Pts',(-0.179148232018249,0.233365702203078,
-1.44316938066052));
#75526=CARTESIAN_POINT('Ctrl Pts',(-0.165978961284344,0.243475377903818,
-1.44406560816035));
#75527=CARTESIAN_POINT('Ctrl Pts',(-0.151938064932521,0.252476988365536,
-1.44496183566018));
#75528=CARTESIAN_POINT('Ctrl Pts',(-0.137238731345518,0.260229073353983,
-1.44585806316001));
#75529=CARTESIAN_POINT('Ctrl Pts',(-0.122543342896592,0.267979077768812,
-1.44675405012232));
#75530=CARTESIAN_POINT('Ctrl Pts',(-0.107190573388433,0.274479862674681,
-1.44765003708463));
#75531=CARTESIAN_POINT('Ctrl Pts',(-0.0914176440317826,0.279636289418377,
-1.44854602404694));
#75532=CARTESIAN_POINT('Ctrl Pts',(-0.0756068246035106,0.284805103041784,
-1.44944416336849));
#75533=CARTESIAN_POINT('Ctrl Pts',(-0.059374593239593,0.288622886440156,
-1.45034230269004));
#75534=CARTESIAN_POINT('Ctrl Pts',(-0.0429731215838286,0.291044585624508,
-1.45124044201158));
#75535=CARTESIAN_POINT('Ctrl Pts',(-0.0281852665924153,0.293228032154346,
-1.4520502202027));
#75536=CARTESIAN_POINT('Ctrl Pts',(-0.0132604109650671,0.29427724548344,
-1.45285999839382));
#75537=CARTESIAN_POINT('Ctrl Pts',(0.0016153759589386,0.294195565161189,
-1.45366977658494));
#75538=CARTESIAN_POINT('Ctrl Pts',(0.0181141778322444,0.294104973150113,
-1.45456790520193));
#75539=CARTESIAN_POINT('Ctrl Pts',(0.0346580897687213,0.292621863149287,
-1.45546603381891));
#75540=CARTESIAN_POINT('Ctrl Pts',(0.0509931230950487,0.289747030005509,
-1.4563641624359));
#75541=CARTESIAN_POINT('Ctrl Pts',(0.0672964031397914,0.286877785181295,
-1.45726054520209));
#75542=CARTESIAN_POINT('Ctrl Pts',(0.0833908285708099,0.282622257540847,
-1.45815692796828));
#75543=CARTESIAN_POINT('Ctrl Pts',(0.0990270367417756,0.277033005243316,
-1.45905331073447));
#75544=CARTESIAN_POINT('Ctrl Pts',(0.114660536496952,0.271444721084543,
-1.4599495382343));
#75545=CARTESIAN_POINT('Ctrl Pts',(0.129835215689528,0.264523386482975,
-1.46084576573413));
#75546=CARTESIAN_POINT('Ctrl Pts',(0.144316649727445,0.256371497268019,
-1.46174199323395));
#75547=CARTESIAN_POINT('Ctrl Pts',(0.158794197109105,0.248221795929702,
-1.46263798019626));
#75548=CARTESIAN_POINT('Ctrl Pts',(0.172578184052074,0.238842593409423,
-1.46353396715856));
#75549=CARTESIAN_POINT('Ctrl Pts',(0.185460089444515,0.228381687582942,
-1.46442995412087));
#75550=CARTESIAN_POINT('Ctrl Pts',(0.198372940028361,0.217895652342511,
-1.46532809344241));
#75551=CARTESIAN_POINT('Ctrl Pts',(0.210378780468628,0.206323245486166,
-1.46622623276395));
#75552=CARTESIAN_POINT('Ctrl Pts',(0.221303078006792,0.193851973589953,
-1.4671243720855));
#75553=CARTESIAN_POINT('Ctrl Pts',(0.231152616589269,0.182607655748445,
-1.46793415027664));
#75554=CARTESIAN_POINT('Ctrl Pts',(0.240123198351401,0.170633482417109,
-1.46874392846778));
#75555=CARTESIAN_POINT('Ctrl Pts',(0.248116785828277,0.158087635791812,
-1.46955370665893));
#75556=CARTESIAN_POINT('Ctrl Pts',(0.256982509484536,0.144172981134509,
-1.47045183527593));
#75557=CARTESIAN_POINT('Ctrl Pts',(0.264702412415536,0.129465712993,-1.47134996389294));
#75558=CARTESIAN_POINT('Ctrl Pts',(0.27113950834701,0.114179713668155,-1.47224809250995));
#75559=CARTESIAN_POINT('Ctrl Pts',(0.277564091361269,0.098923428432728,
-1.47314447527617));
#75560=CARTESIAN_POINT('Ctrl Pts',(0.282710452419854,0.083091340341732,
-1.47404085804238));
#75561=CARTESIAN_POINT('Ctrl Pts',(0.286487614189603,0.0669214981597798,
-1.4749372408086));
#75562=CARTESIAN_POINT('Ctrl Pts',(0.290264121700693,0.0507544568266919,
-1.47583346830845));
#75563=CARTESIAN_POINT('Ctrl Pts',(0.292671669559208,0.0342505338207423,
-1.4767296958083));
#75564=CARTESIAN_POINT('Ctrl Pts',(0.29366934391778,0.0176622887220424,
-1.47762592330815));
#75565=CARTESIAN_POINT('Ctrl Pts',(0.29466675051162,0.00107849572432326,
-1.47852191027048));
#75566=CARTESIAN_POINT('Ctrl Pts',(0.294254998032437,-0.0155887834738292,
-1.47941789723281));
#75567=CARTESIAN_POINT('Ctrl Pts',(0.292445283283392,-0.032084206165911,
-1.48031388419514));
#75568=CARTESIAN_POINT('Ctrl Pts',(0.290631221198485,-0.048619254518705,
-1.4812120235167));
#75569=CARTESIAN_POINT('Ctrl Pts',(0.287412602456615,-0.0649808344709505,
-1.48211016283827));
#75570=CARTESIAN_POINT('Ctrl Pts',(0.28285241563517,-0.0809206461253819,
-1.48300830215983));
#75571=CARTESIAN_POINT('Ctrl Pts',(0.278740871082607,-0.0952922603470733,
-1.48381808035086));
#75572=CARTESIAN_POINT('Ctrl Pts',(0.273539589296867,-0.109320761045354,
-1.48462785854189));
#75573=CARTESIAN_POINT('Ctrl Pts',(0.267328372871686,-0.122838027734805,
-1.48543763673292));
#75574=CARTESIAN_POINT('Ctrl Pts',(0.260439484927435,-0.137830088735717,
-1.48633576534989));
#75575=CARTESIAN_POINT('Ctrl Pts',(0.252263485818446,-0.152288777334707,
-1.48723389396687));
#75576=CARTESIAN_POINT('Ctrl Pts',(0.242905879293824,-0.165983052762908,
-1.48813202258385));
#75577=CARTESIAN_POINT('Ctrl Pts',(0.233566462797283,-0.179650708215805,
-1.48902840535003));
#75578=CARTESIAN_POINT('Ctrl Pts',(0.223050384801855,-0.192556216692559,
-1.48992478811622));
#75579=CARTESIAN_POINT('Ctrl Pts',(0.211508393968693,-0.204494105736044,
-1.4908211708824));
#75580=CARTESIAN_POINT('Ctrl Pts',(0.199968402374078,-0.216429926965726,
-1.49171739838222));
#75581=CARTESIAN_POINT('Ctrl Pts',(0.187403360995642,-0.227397857327417,
-1.49261362588204));
#75582=CARTESIAN_POINT('Ctrl Pts',(0.174003346263128,-0.237226633178558,
-1.49350985338186));
#75583=CARTESIAN_POINT('Ctrl Pts',(0.160606927945919,-0.247052771095292,
-1.49440584034416));
#75584=CARTESIAN_POINT('Ctrl Pts',(0.146376625954696,-0.255739901875646,
-1.49530182730646));
#75585=CARTESIAN_POINT('Ctrl Pts',(0.131533098065914,-0.263159047180945,
-1.49619781426876));
#75586=CARTESIAN_POINT('Ctrl Pts',(0.116653912733785,-0.270596014917365,
-1.49709595359029));
#75587=CARTESIAN_POINT('Ctrl Pts',(0.101159282176131,-0.276758581671856,
-1.49799409291183));
#75588=CARTESIAN_POINT('Ctrl Pts',(0.0852920150001993,-0.281565111789806,
-1.49889223223336));
#75589=CARTESIAN_POINT('Ctrl Pts',(0.0709858081516357,-0.285898763787268,
-1.49970201042454));
#75590=CARTESIAN_POINT('Ctrl Pts',(0.056377348170839,-0.289130645766822,
-1.50051178861573));
#75591=CARTESIAN_POINT('Ctrl Pts',(0.0416511737591101,-0.291236707378188,
-1.50132156680691));
#75592=CARTESIAN_POINT('Ctrl Pts',(0.0253183077946819,-0.29357254973952,
-1.50221969542386));
#75593=CARTESIAN_POINT('Ctrl Pts',(0.00873611107200796,-0.294537634849432,
-1.50311782404082));
#75594=CARTESIAN_POINT('Ctrl Pts',(-0.00784407038384531,-0.294095410640515,
-1.50401595265778));
#75595=CARTESIAN_POINT('Ctrl Pts',(-0.0243920220204992,-0.293654046060688,
-1.50491233542394));
#75596=CARTESIAN_POINT('Ctrl Pts',(-0.0409371823563882,-0.29181075690919,
-1.50580871819011));
#75597=CARTESIAN_POINT('Ctrl Pts',(-0.0572251715302886,-0.288580872102309,
-1.50670510095627));
#75598=CARTESIAN_POINT('Ctrl Pts',(-0.0735103393905747,-0.285351546757855,
-1.50760132845607));
#75599=CARTESIAN_POINT('Ctrl Pts',(-0.0895376402263333,-0.280736203957116,
-1.50849755595587));
#75600=CARTESIAN_POINT('Ctrl Pts',(-0.105060128714307,-0.274801763739852,
-1.50939378345567));
#75601=CARTESIAN_POINT('Ctrl Pts',(-0.12057845113855,-0.268868916260516,
-1.51028977041794));
#75602=CARTESIAN_POINT('Ctrl Pts',(-0.135591494493943,-0.261617967001758,
-1.51118575738022));
#75603=CARTESIAN_POINT('Ctrl Pts',(-0.149871275757871,-0.253164453868841,
-1.5120817443425));
#75604=CARTESIAN_POINT('Ctrl Pts',(-0.164185360220829,-0.244690633524058,
-1.51297988366401));
#75605=CARTESIAN_POINT('Ctrl Pts',(-0.177761993823932,-0.235008907174037,
-1.51387802298553));
#75606=CARTESIAN_POINT('Ctrl Pts',(-0.190400975143691,-0.224279086551403,
-1.51477616230704));
#75607=CARTESIAN_POINT('Ctrl Pts',(-0.201796502750187,-0.214604891770623,
-1.51558594049833));
#75608=CARTESIAN_POINT('Ctrl Pts',(-0.212429917431785,-0.20407955774231,
-1.51639571868961));
#75609=CARTESIAN_POINT('Ctrl Pts',(-0.222180992872592,-0.192845135811483,
-1.5172054968809));
#75610=CARTESIAN_POINT('Ctrl Pts',(-0.232910731838629,-0.180483174765868,
-1.51809654819781));
#75611=CARTESIAN_POINT('Ctrl Pts',(-0.242642934871774,-0.167179753567899,
-1.51898759951473));
#75612=CARTESIAN_POINT('Ctrl Pts',(-0.251211342293677,-0.153122504887457,
-1.51987865083165));
#75613=CARTESIAN_POINT('Ctrl Pts',(-0.259762998908044,-0.139092737424413,
-1.52076796018785));
#75614=CARTESIAN_POINT('Ctrl Pts',(-0.267154899328252,-0.124312709262806,
-1.52165726954405));
#75615=CARTESIAN_POINT('Ctrl Pts',(-0.273262529657102,-0.109001054515089,
-1.52254657890025));
#75616=CARTESIAN_POINT('Ctrl Pts',(-0.27936345814298,-0.0937062010962422,
-1.523434912426));
#75617=CARTESIAN_POINT('Ctrl Pts',(-0.284182590563843,-0.0778816129895165,
-1.52432324595175));
#75618=CARTESIAN_POINT('Ctrl Pts',(-0.287642940184411,-0.061767134967291,
-1.5252115794775));
#75619=CARTESIAN_POINT('Ctrl Pts',(-0.291104585625806,-0.0456466224460921,
-1.52610024566359));
#75620=CARTESIAN_POINT('Ctrl Pts',(-0.293206265845959,-0.0292367899534084,
-1.52698891184968));
#75621=CARTESIAN_POINT('Ctrl Pts',(-0.293921926337035,-0.0127883235150905,
-1.52787757803577));
#75622=CARTESIAN_POINT('Ctrl Pts',(-0.294111125559157,-0.00843984110753895,
-1.52811251478753));
#75623=CARTESIAN_POINT('Ctrl Pts',(-0.294203735878343,-0.00408867950520032,
-1.52834745153928));
#75624=CARTESIAN_POINT('Ctrl Pts',(-0.294199884656848,0.000260514677417675,
-1.52858238829104));
#75625=CARTESIAN_POINT('',(-0.294247201503143,-2.16877952208041E-5,-1.62858238829104));
#75626=CARTESIAN_POINT('Ctrl Pts',(-0.294053336475258,0.000261715132789226,
-1.52858246018345));
#75627=CARTESIAN_POINT('Ctrl Pts',(-0.29428999687239,0.0280593677207072,
-1.53008478244059));
#75628=CARTESIAN_POINT('Ctrl Pts',(-0.27791468735522,0.153550929214129,
-1.53688174805573));
#75629=CARTESIAN_POINT('Ctrl Pts',(-0.0993136717012497,0.333300171830814,
-1.54897335702887));
#75630=CARTESIAN_POINT('Ctrl Pts',(0.226279686422242,0.264101710371244,
-1.56485728710286));
#75631=CARTESIAN_POINT('Ctrl Pts',(0.34458731149564,-0.0470297212362109,
-1.58074121717685));
#75632=CARTESIAN_POINT('Ctrl Pts',(0.147232339525018,-0.315079114138717,
-1.59662514725084));
#75633=CARTESIAN_POINT('Ctrl Pts',(-0.184996265602307,-0.294497184254118,
-1.61250907732483));
#75634=CARTESIAN_POINT('Ctrl Pts',(-0.294150424933899,-0.0997705721318655,
-1.6231614910049));
#75635=CARTESIAN_POINT('Ctrl Pts',(-0.294682912919936,-0.00118332006191642,
-1.62851926132696));
#75636=CARTESIAN_POINT('Ctrl Pts',(-0.294681679645924,-2.17198188829926E-5,
-1.62858238829104));
#75637=CARTESIAN_POINT('',(-0.294199895814294,-0.000247594141307502,-1.72858238519529));
#75638=CARTESIAN_POINT('Ctrl Pts',(-0.294199999200868,-2.1684316126153E-5,
-1.62858238829104));
#75639=CARTESIAN_POINT('Ctrl Pts',(-0.29420121277264,0.0164433410297652,
-1.6294786423153));
#75640=CARTESIAN_POINT('Ctrl Pts',(-0.292815900108825,0.0329621383935221,
-1.63037489633957));
#75641=CARTESIAN_POINT('Ctrl Pts',(-0.290043036332427,0.0492816099074137,
-1.63127115036383));
#75642=CARTESIAN_POINT('Ctrl Pts',(-0.2872755512891,0.0655694253111555,
-1.63216566585655));
#75643=CARTESIAN_POINT('Ctrl Pts',(-0.283125922858897,0.0816578962341241,
-1.63306018134926));
#75644=CARTESIAN_POINT('Ctrl Pts',(-0.277644920689935,0.097298191222036,
-1.63395469684197));
#75645=CARTESIAN_POINT('Ctrl Pts',(-0.27216484128538,0.112935853058729,
-1.63484906173685));
#75646=CARTESIAN_POINT('Ctrl Pts',(-0.265354045538873,0.128124723155489,
-1.63574342663173));
#75647=CARTESIAN_POINT('Ctrl Pts',(-0.25731332445106,0.142630617540357,
-1.63663779152661));
#75648=CARTESIAN_POINT('Ctrl Pts',(-0.249274583937638,0.157132938862234,
-1.63753193612331));
#75649=CARTESIAN_POINT('Ctrl Pts',(-0.240006915751063,0.170951928661847,
-1.63842608072001));
#75650=CARTESIAN_POINT('Ctrl Pts',(-0.229656536750084,0.183879077461133,
-1.63932022531671));
#75651=CARTESIAN_POINT('Ctrl Pts',(-0.21928162150504,0.196836870904251,
-1.64021648954111));
#75652=CARTESIAN_POINT('Ctrl Pts',(-0.207819391914967,0.208897996777179,
-1.64111275376552));
#75653=CARTESIAN_POINT('Ctrl Pts',(-0.195455862100078,0.219887803142228,
-1.64200901798992));
#75654=CARTESIAN_POINT('Ctrl Pts',(-0.18502757939023,0.229157389531967,
-1.64276499115088));
#75655=CARTESIAN_POINT('Ctrl Pts',(-0.173958958957302,0.237665280750663,
-1.64352096431184));
#75656=CARTESIAN_POINT('Ctrl Pts',(-0.162378246516628,0.245330277499915,
-1.6442769374728));
#75657=CARTESIAN_POINT('Ctrl Pts',(-0.148619862282732,0.254436623155937,
-1.64517506608728));
#75658=CARTESIAN_POINT('Ctrl Pts',(-0.134049059683587,0.262411104138865,
-1.64607319470175));
#75659=CARTESIAN_POINT('Ctrl Pts',(-0.11887730661778,0.269113035677022,
-1.64697132331623));
#75660=CARTESIAN_POINT('Ctrl Pts',(-0.103735045563376,0.275801939489215,
-1.64786770607977));
#75661=CARTESIAN_POINT('Ctrl Pts',(-0.0879948416570457,0.281222827286779,
-1.64876408884331));
#75662=CARTESIAN_POINT('Ctrl Pts',(-0.0718931256591281,0.285280596050557,
-1.64966047160685));
#75663=CARTESIAN_POINT('Ctrl Pts',(-0.0557941987129142,0.28933766194969,
-1.65055669910384));
#75664=CARTESIAN_POINT('Ctrl Pts',(-0.0393346361284934,0.29203183324509,
-1.65145292660083));
#75665=CARTESIAN_POINT('Ctrl Pts',(-0.0227662478442387,0.293317810504399,
-1.65234915409782));
#75666=CARTESIAN_POINT('Ctrl Pts',(-0.00620230633356539,0.294603442621525,
-1.65324514105718));
#75667=CARTESIAN_POINT('Ctrl Pts',(0.0104696126877779,0.294481580486408,
-1.65414112801655));
#75668=CARTESIAN_POINT('Ctrl Pts',(0.0269940104210207,0.2929589790421,-1.65503711497591));
#75669=CARTESIAN_POINT('Ctrl Pts',(0.043558103417585,0.291432719971885,
-1.6559352542944));
#75670=CARTESIAN_POINT('Ctrl Pts',(0.0599731781454324,0.288499100173501,
-1.6568333936129));
#75671=CARTESIAN_POINT('Ctrl Pts',(0.0759898769403874,0.284216781001025,
-1.65773153293139));
#75672=CARTESIAN_POINT('Ctrl Pts',(0.09043081425966,0.280355766721958,-1.65854131113652));
#75673=CARTESIAN_POINT('Ctrl Pts',(0.104547639415254,0.275399213522471,
-1.65935108934165));
#75674=CARTESIAN_POINT('Ctrl Pts',(0.118170869641054,0.26942398847964,-1.66016086754679));
#75675=CARTESIAN_POINT('Ctrl Pts',(0.133280455635432,0.262796839475768,
-1.66105899620086));
#75676=CARTESIAN_POINT('Ctrl Pts',(0.147879131436968,0.254873498987716,
-1.66195712485493));
#75677=CARTESIAN_POINT('Ctrl Pts',(0.161734056589533,0.24575543725235,-1.662855253509));
#75678=CARTESIAN_POINT('Ctrl Pts',(0.175562049487036,0.236655099897421,
-1.66375163631243));
#75679=CARTESIAN_POINT('Ctrl Pts',(0.188648471582833,0.226365025870775,
-1.66464801911586));
#75680=CARTESIAN_POINT('Ctrl Pts',(0.200785260103042,0.215032368087583,
-1.66554440191929));
#75681=CARTESIAN_POINT('Ctrl Pts',(0.212919946352997,0.203701673287377,
-1.66644062945604));
#75682=CARTESIAN_POINT('Ctrl Pts',(0.224104712626763,0.191329252934774,
-1.66733685699279));
#75683=CARTESIAN_POINT('Ctrl Pts',(0.23416501592168,0.178102176624541,-1.66823308452953));
#75684=CARTESIAN_POINT('Ctrl Pts',(0.244222619141691,0.16487865031631,-1.66912907152865));
#75685=CARTESIAN_POINT('Ctrl Pts',(0.253155887786595,0.150801560128604,
-1.67002505852777));
#75686=CARTESIAN_POINT('Ctrl Pts',(0.260832025983922,0.136089287679533,
-1.67092104552689));
#75687=CARTESIAN_POINT('Ctrl Pts',(0.268526603957315,0.121341673108887,
-1.67181918488429));
#75688=CARTESIAN_POINT('Ctrl Pts',(0.274957675540732,0.105956545726213,
-1.67271732424169));
#75689=CARTESIAN_POINT('Ctrl Pts',(0.280039395205683,0.090175257875071,
-1.67361546359909));
#75690=CARTESIAN_POINT('Ctrl Pts',(0.284621161709583,0.0759465752967122,
-1.67442524160632));
#75691=CARTESIAN_POINT('Ctrl Pts',(0.288106581174604,0.0613965267213745,
-1.67523501961355));
#75692=CARTESIAN_POINT('Ctrl Pts',(0.290468397946582,0.0467092045998036,
-1.67604479762078));
#75693=CARTESIAN_POINT('Ctrl Pts',(0.293087899899455,0.0304194274094599,
-1.67694292617016));
#75694=CARTESIAN_POINT('Ctrl Pts',(0.294341187685413,0.0138565209953559,
-1.67784105471955));
#75695=CARTESIAN_POINT('Ctrl Pts',(0.294187344085231,-0.00272884225966128,
-1.67873918326893));
#75696=CARTESIAN_POINT('Ctrl Pts',(0.294033799537936,-0.0192819656244967,
-1.67963556596775));
#75697=CARTESIAN_POINT('Ctrl Pts',(0.292478494041894,-0.0358566762777647,
-1.68053194866657));
#75698=CARTESIAN_POINT('Ctrl Pts',(0.289532330761364,-0.0521983662952416,
-1.68142833136539));
#75699=CARTESIAN_POINT('Ctrl Pts',(0.286586677794322,-0.0685372257211849,
-1.68232455879916));
#75700=CARTESIAN_POINT('Ctrl Pts',(0.282250733049956,-0.0846423586988476,
-1.68322078623293));
#75701=CARTESIAN_POINT('Ctrl Pts',(0.276587112295275,-0.100265693595371,
-1.6841170136667));
#75702=CARTESIAN_POINT('Ctrl Pts',(0.270925011589871,-0.115884835372345,
-1.68501300056356));
#75703=CARTESIAN_POINT('Ctrl Pts',(0.263936222243119,-0.131021695103706,
-1.68590898746042));
#75704=CARTESIAN_POINT('Ctrl Pts',(0.255732300272781,-0.145446315172273,
-1.68680497435728));
#75705=CARTESIAN_POINT('Ctrl Pts',(0.247508670640721,-0.159905586415461,
-1.68770311361574));
#75706=CARTESIAN_POINT('Ctrl Pts',(0.238064494217003,-0.173648522751832,
-1.6886012528742));
#75707=CARTESIAN_POINT('Ctrl Pts',(0.227556077247711,-0.186472174084054,
-1.68949939213267));
#75708=CARTESIAN_POINT('Ctrl Pts',(0.218081499371173,-0.198034208933238,
-1.69030917065337));
#75709=CARTESIAN_POINT('Ctrl Pts',(0.207742657805406,-0.20884904599276,
-1.69111894917406));
#75710=CARTESIAN_POINT('Ctrl Pts',(0.196679491990959,-0.21879400684246,
-1.69192872769476));
#75711=CARTESIAN_POINT('Ctrl Pts',(0.184409290188552,-0.229824003010781,
-1.69282685631643));
#75712=CARTESIAN_POINT('Ctrl Pts',(0.171169103881296,-0.239853863539452,
-1.6937249849381));
#75713=CARTESIAN_POINT('Ctrl Pts',(0.157147421701379,-0.248713344741711,
-1.69462311355977));
#75714=CARTESIAN_POINT('Ctrl Pts',(0.143152995950657,-0.257555604199888,
-1.69551949632964));
#75715=CARTESIAN_POINT('Ctrl Pts',(0.128380715715764,-0.265231526367482,
-1.6964158790995));
#75716=CARTESIAN_POINT('Ctrl Pts',(0.11305046214597,-0.271612284347713,
-1.69731226186936));
#75717=CARTESIAN_POINT('Ctrl Pts',(0.0977228640231671,-0.277991937077823,
-1.69820848937128));
#75718=CARTESIAN_POINT('Ctrl Pts',(0.0818381924911331,-0.283076518770903,
-1.6991047168732));
#75719=CARTESIAN_POINT('Ctrl Pts',(0.0656388622976581,-0.286784204161019,
-1.70000094437512));
#75720=CARTESIAN_POINT('Ctrl Pts',(0.0494438798402572,-0.290490894445947,
-1.70089693133866));
#75721=CARTESIAN_POINT('Ctrl Pts',(0.0329351805694026,-0.292821255920828,
-1.7017929183022));
#75722=CARTESIAN_POINT('Ctrl Pts',(0.0163664804088447,-0.293744409851536,
-1.70268890526574));
#75723=CARTESIAN_POINT('Ctrl Pts',(-0.000242021414697736,-0.294669781401083,
-1.70358704458708));
#75724=CARTESIAN_POINT('Ctrl Pts',(-0.0169100168106484,-0.294181175863316,
-1.70448518390843));
#75725=CARTESIAN_POINT('Ctrl Pts',(-0.0333822336270742,-0.292299959764054,
-1.70538332322978));
#75726=CARTESIAN_POINT('Ctrl Pts',(-0.0482338734912188,-0.290603822302761,
-1.70619310140944));
#75727=CARTESIAN_POINT('Ctrl Pts',(-0.0629259751805142,-0.287776401659202,
-1.70700287958909));
#75728=CARTESIAN_POINT('Ctrl Pts',(-0.0772795972649593,-0.283868814501639,
-1.70781265776875));
#75729=CARTESIAN_POINT('Ctrl Pts',(-0.0931992682033539,-0.279534890886712,
-1.70871078662273));
#75730=CARTESIAN_POINT('Ctrl Pts',(-0.108804129565062,-0.273843750169649,
-1.70960891547671));
#75731=CARTESIAN_POINT('Ctrl Pts',(-0.123848953646058,-0.266861530912151,
-1.71050704433069));
#75732=CARTESIAN_POINT('Ctrl Pts',(-0.138864532481465,-0.259892884210625,
-1.71140342733516));
#75733=CARTESIAN_POINT('Ctrl Pts',(-0.153321497429455,-0.251638409840476,
-1.71229981033962));
#75734=CARTESIAN_POINT('Ctrl Pts',(-0.166992413577997,-0.242213075219723,
-1.71319619334408));
#75735=CARTESIAN_POINT('Ctrl Pts',(-0.180660961704508,-0.232789373218159,
-1.71409242108062));
#75736=CARTESIAN_POINT('Ctrl Pts',(-0.193543051582717,-0.222195617746181,
-1.71498864881717));
#75737=CARTESIAN_POINT('Ctrl Pts',(-0.205438535842917,-0.210591186878081,
-1.71588487655371));
#75738=CARTESIAN_POINT('Ctrl Pts',(-0.217330827482302,-0.198989870515176,
-1.71678086375231));
#75739=CARTESIAN_POINT('Ctrl Pts',(-0.228236479969677,-0.186378977846106,
-1.71767685095091));
#75740=CARTESIAN_POINT('Ctrl Pts',(-0.237992036393236,-0.172954995919171,
-1.71857283814951));
#75741=CARTESIAN_POINT('Ctrl Pts',(-0.247771027756986,-0.159498766706699,
-1.71947097770165));
#75742=CARTESIAN_POINT('Ctrl Pts',(-0.256393959006673,-0.145226205702012,
-1.72036911725379));
#75743=CARTESIAN_POINT('Ctrl Pts',(-0.263740436603473,-0.130363423168501,
-1.72126725680593));
#75744=CARTESIAN_POINT('Ctrl Pts',(-0.27036413852692,-0.116962900270577,
-1.7220770338182));
#75745=CARTESIAN_POINT('Ctrl Pts',(-0.275950650625105,-0.103083332767034,
-1.72288681083047));
#75746=CARTESIAN_POINT('Ctrl Pts',(-0.280445950538711,-0.0889028055037576,
-1.72369658784274));
#75747=CARTESIAN_POINT('Ctrl Pts',(-0.28642702932571,-0.0700353545143065,
-1.72477401097431));
#75748=CARTESIAN_POINT('Ctrl Pts',(-0.290508007507302,-0.0505380932922465,
-1.72585143410589));
#75749=CARTESIAN_POINT('Ctrl Pts',(-0.292587171686153,-0.0307634030090615,
-1.72692885723746));
#75750=CARTESIAN_POINT('Ctrl Pts',(-0.29365080707009,-0.0206472897624244,
-1.7274800332234));
#75751=CARTESIAN_POINT('Ctrl Pts',(-0.294191302124979,-0.0104589120974399,
-1.72803120920935));
#75752=CARTESIAN_POINT('Ctrl Pts',(-0.294199895814294,-0.000247594141307502,
-1.72858238519529));
#75753=CARTESIAN_POINT('',(-0.293800095830876,0.000157032384922304,-1.82858238829104));
#75754=CARTESIAN_POINT('Ctrl Pts',(-0.293989435543949,-0.000247359708936523,
-1.72858238829104));
#75755=CARTESIAN_POINT('Ctrl Pts',(-0.293449229871738,0.0676232139930559,
-1.7322484314996));
#75756=CARTESIAN_POINT('Ctrl Pts',(-0.23631160546398,0.234336140108229,
-1.74120911806615));
#75757=CARTESIAN_POINT('Ctrl Pts',(0.0410305566082919,0.345352959227952,
-1.75546444799072));
#75758=CARTESIAN_POINT('Ctrl Pts',(0.312471262641183,0.152689102424562,
-1.7713483780647));
#75759=CARTESIAN_POINT('Ctrl Pts',(0.297669529109044,-0.179847460151632,
-1.7872323081387));
#75760=CARTESIAN_POINT('Ctrl Pts',(0.0101848190520429,-0.347632316485115,
-1.80311623821267));
#75761=CARTESIAN_POINT('Ctrl Pts',(-0.247377757960732,-0.216891255039904,
-1.81689959826346));
#75762=CARTESIAN_POINT('Ctrl Pts',(-0.293514181780463,-0.059071809807225,
-1.82538831495625));
#75763=CARTESIAN_POINT('Ctrl Pts',(-0.293800095830876,0.000157032384922304,
-1.82858238829104));
#75764=CARTESIAN_POINT('Ctrl Pts',(-0.293800095830876,0.000157032384922304,
-1.82858238829104));
#75765=CARTESIAN_POINT('Ctrl Pts',(-0.293988126104624,0.0391086522688038,
-1.83068295831425));
#75766=CARTESIAN_POINT('Ctrl Pts',(-0.268652541760571,0.176005752497631,
-1.83807817169543));
#75767=CARTESIAN_POINT('Ctrl Pts',(-0.0611792324801312,0.342355999552018,
-1.85076802843466));
#75768=CARTESIAN_POINT('Ctrl Pts',(0.254561196731867,0.23696743080658,-1.86665195850863));
#75769=CARTESIAN_POINT('Ctrl Pts',(0.337105175546461,-0.0855145454749233,
-1.88253588858261));
#75770=CARTESIAN_POINT('Ctrl Pts',(0.110846680674492,-0.32962749086264,
-1.89841981865661));
#75771=CARTESIAN_POINT('Ctrl Pts',(-0.205921254452606,-0.273790960216194,
-1.91376860488588));
#75772=CARTESIAN_POINT('Ctrl Pts',(-0.293956888266034,-0.0874827880384833,
-1.92382274775716));
#75773=CARTESIAN_POINT('Ctrl Pts',(-0.29455814428141,0.000186008385503332,
-1.92858224727044));
#75774=CARTESIAN_POINT('Origin',(0.,0.,-2.1456589891905));
#75775=CARTESIAN_POINT('',(0.223395701213113,0.0796639272475426,-0.0400000000000001));
#75776=CARTESIAN_POINT('Ctrl Pts',(0.223395701213113,0.0796639272475426,
-0.0400000000000001));
#75777=CARTESIAN_POINT('Ctrl Pts',(0.229242148634165,0.0632691640673004,
-0.0412368761336291));
#75778=CARTESIAN_POINT('Ctrl Pts',(0.233267330333748,0.0462771952834835,
-0.0425283651739515));
#75779=CARTESIAN_POINT('Ctrl Pts',(0.236585845934182,0.0193347385838108,
-0.0444885583085567));
#75780=CARTESIAN_POINT('Ctrl Pts',(0.237180042016459,0.00961060863350905,
-0.0451798378362018));
#75781=CARTESIAN_POINT('Ctrl Pts',(0.237173010784732,-0.00387785704994729,
-0.0461134218510738));
#75782=CARTESIAN_POINT('Ctrl Pts',(0.237081916435321,-0.00763167680734785,
-0.0463705998105068));
#75783=CARTESIAN_POINT('Ctrl Pts',(0.236823643821842,-0.0130073167037052,
-0.0467353421644926));
#75784=CARTESIAN_POINT('Ctrl Pts',(0.236728825808623,-0.0146318767989615,
-0.0468451067693097));
#75785=CARTESIAN_POINT('Ctrl Pts',(0.236534578904014,-0.0174593844560919,
-0.0470353811864949));
#75786=CARTESIAN_POINT('Ctrl Pts',(0.236442674242972,-0.0186627707240716,
-0.0471161192616475));
#75787=CARTESIAN_POINT('Ctrl Pts',(0.236234211652528,-0.0211428780630218,
-0.0472820379831441));
#75788=CARTESIAN_POINT('Ctrl Pts',(0.236116479399246,-0.0224194627869977,
-0.047367179761603));
#75789=CARTESIAN_POINT('Ctrl Pts',(0.23578782996851,-0.0256926126158978,
-0.0475848505698601));
#75790=CARTESIAN_POINT('Ctrl Pts',(0.235561899772033,-0.0276875943320591,
-0.0477169157953027));
#75791=CARTESIAN_POINT('Ctrl Pts',(0.234548202232191,-0.0357245793533611,
-0.0482467916099474));
#75792=CARTESIAN_POINT('Ctrl Pts',(0.23355304297225,-0.0417383567309479,
-0.0486382574837735));
#75793=CARTESIAN_POINT('Ctrl Pts',(0.229072898625128,-0.063555865774956,
-0.0500497146380798));
#75794=CARTESIAN_POINT('Ctrl Pts',(0.224205536799736,-0.0790293111931186,
-0.0510307340489809));
#75795=CARTESIAN_POINT('Ctrl Pts',(0.217490502406841,-0.0946069579237412,
-0.0520824257994189));
#75796=CARTESIAN_POINT('Ctrl Pts',(0.217176625344077,-0.0953252774328842,
-0.0521310789593419));
#75797=CARTESIAN_POINT('Ctrl Pts',(0.213357409630695,-0.103948919518178,
-0.0527172112680231));
#75798=CARTESIAN_POINT('Ctrl Pts',(0.209426160764464,-0.111657573027881,
-0.0532616566732872));
#75799=CARTESIAN_POINT('Ctrl Pts',(0.20409553990101,-0.120834012840443,
-0.0539559133176723));
#75800=CARTESIAN_POINT('Ctrl Pts',(0.203086648436724,-0.1225220824665,-0.0540856382508694));
#75801=CARTESIAN_POINT('Ctrl Pts',(0.201608761797323,-0.124926459356141,
-0.0542736095376432));
#75802=CARTESIAN_POINT('Ctrl Pts',(0.201156666043024,-0.125653128619482,
-0.054330845175309));
#75803=CARTESIAN_POINT('Ctrl Pts',(0.200697140094571,-0.126382904802808,
-0.0543887726460091));
#75804=CARTESIAN_POINT('Ctrl Pts',(0.200693624082134,-0.126388488088569,
-0.054389215857151));
#75805=CARTESIAN_POINT('Ctrl Pts',(0.200686565097341,-0.126399696434068,
-0.0543901056486725));
#75806=CARTESIAN_POINT('Ctrl Pts',(0.200683022120862,-0.126405321492537,
-0.0543905522293519));
#75807=CARTESIAN_POINT('Ctrl Pts',(0.200675908027464,-0.126416615234073,
-0.0543914489080991));
#75808=CARTESIAN_POINT('Ctrl Pts',(0.20067233690698,-0.126422283914579,
-0.0543918990063852));
#75809=CARTESIAN_POINT('Ctrl Pts',(0.200665165308133,-0.126433666807838,
-0.0543928028731065));
#75810=CARTESIAN_POINT('Ctrl Pts',(0.200661564825264,-0.126439381019095,
-0.0543932566418665));
#75811=CARTESIAN_POINT('Ctrl Pts',(0.200654333244772,-0.126450856942442,
-0.0543941680072206));
#75812=CARTESIAN_POINT('Ctrl Pts',(0.200650702143052,-0.12645661865194,
-0.0543946256040756));
#75813=CARTESIAN_POINT('Ctrl Pts',(0.200643408026221,-0.126468191604891,
-0.0543955447885196));
#75814=CARTESIAN_POINT('Ctrl Pts',(0.200639745007662,-0.126474002844255,
-0.0543960063762747));
#75815=CARTESIAN_POINT('Ctrl Pts',(0.200632385716146,-0.126485676955469,
-0.0543969337107085));
#75816=CARTESIAN_POINT('Ctrl Pts',(0.20062868943874,-0.126491539824327,
-0.0543973994576657));
#75817=CARTESIAN_POINT('Ctrl Pts',(0.200621262243384,-0.126503319362767,
-0.0543983352843283));
#75818=CARTESIAN_POINT('Ctrl Pts',(0.2006175313199,-0.126509236030559,-0.0543988053644348));
#75819=CARTESIAN_POINT('Ctrl Pts',(0.200610033396785,-0.126521125411547,
-0.0543997500373972));
#75820=CARTESIAN_POINT('Ctrl Pts',(0.200606266392381,-0.126527098121203,
-0.0544002246305432));
#75821=CARTESIAN_POINT('Ctrl Pts',(0.200598694821391,-0.126539101908473,
-0.0544011785158827));
#75822=CARTESIAN_POINT('Ctrl Pts',(0.200594890249154,-0.126545132983368,
-0.0544016578084608));
#75823=CARTESIAN_POINT('Ctrl Pts',(0.200587242002331,-0.126557255907287,
-0.0544026212857213));
#75824=CARTESIAN_POINT('Ctrl Pts',(0.200583398322663,-0.126563347752089,
-0.0544031054707));
#75825=CARTESIAN_POINT('Ctrl Pts',(0.200575670264262,-0.126575594709312,
-0.0544040789328784));
#75826=CARTESIAN_POINT('Ctrl Pts',(0.200571785880057,-0.126581749817493,
-0.0544045682104059));
#75827=CARTESIAN_POINT('Ctrl Pts',(0.200563974756709,-0.126594125886275,
-0.0544055520651835));
#75828=CARTESIAN_POINT('Ctrl Pts',(0.200560048011122,-0.126600346843506,
-0.0544060466428653));
#75829=CARTESIAN_POINT('Ctrl Pts',(0.200552150445225,-0.126612857293882,
-0.0544070413134324));
#75830=CARTESIAN_POINT('Ctrl Pts',(0.200548179618808,-0.126619146782418,
-0.0544075414066874));
#75831=CARTESIAN_POINT('Ctrl Pts',(0.200540192105282,-0.126631797081026,
-0.0544085473321432));
#75832=CARTESIAN_POINT('Ctrl Pts',(0.200536175410803,-0.126638157887745,
-0.0544090531648523));
#75833=CARTESIAN_POINT('Ctrl Pts',(0.200528094304026,-0.126650953718181,
-0.0544100708018415));
#75834=CARTESIAN_POINT('Ctrl Pts',(0.200524029884712,-0.126657388737192,
-0.0544105826065634));
#75835=CARTESIAN_POINT('Ctrl Pts',(0.20051585139652,-0.126670336002805,
-0.0544116124295171));
#75836=CARTESIAN_POINT('Ctrl Pts',(0.200511737320095,-0.126676848244705,
-0.0544121304482347));
#75837=CARTESIAN_POINT('Ctrl Pts',(0.200503457507019,-0.126689953088422,
-0.0544131729509683));
#75838=CARTESIAN_POINT('Ctrl Pts',(0.20049929176263,-0.126696545684953,
-0.0544136974354696));
#75839=CARTESIAN_POINT('Ctrl Pts',(0.200490906519636,-0.126709814498762,
-0.0544147531319586));
#75840=CARTESIAN_POINT('Ctrl Pts',(0.20048668701253,-0.12671649071102,-0.0544152843445016));
#75841=CARTESIAN_POINT('Ctrl Pts',(0.200478192061428,-0.126729930153859,
-0.0544163537703289));
#75842=CARTESIAN_POINT('Ctrl Pts',(0.200473916608742,-0.12673669337872,
-0.0544168919841648));
#75843=CARTESIAN_POINT('Ctrl Pts',(0.200465307489914,-0.126750310389085,
-0.0544179756975492));
#75844=CARTESIAN_POINT('Ctrl Pts',(0.200460973814824,-0.126757164168214,
-0.0544185211976525));
#75845=CARTESIAN_POINT('Ctrl Pts',(0.2004537838742,-0.126768533887821,-0.054419426193448));
#75846=CARTESIAN_POINT('Ctrl Pts',(0.200450927806819,-0.126773049955175,
-0.0544197856764443));
#75847=CARTESIAN_POINT('Ctrl Pts',(0.200445019548975,-0.126782391504547,
-0.0544205293083176));
#75848=CARTESIAN_POINT('Ctrl Pts',(0.200441967336429,-0.126787216973569,
-0.0544209134586418));
#75849=CARTESIAN_POINT('Ctrl Pts',(0.200435650221673,-0.126797203370224,
-0.0544217085061467));
#75850=CARTESIAN_POINT('Ctrl Pts',(0.200432385295043,-0.126802364280933,
-0.0544221194048575));
#75851=CARTESIAN_POINT('Ctrl Pts',(0.200425624369565,-0.126813050447579,
-0.0544229702578859));
#75852=CARTESIAN_POINT('Ctrl Pts',(0.200422128340668,-0.12681857568648,
-0.0544234102141926));
#75853=CARTESIAN_POINT('Ctrl Pts',(0.200414884750506,-0.12683002264666,
-0.0544243217517066));
#75854=CARTESIAN_POINT('Ctrl Pts',(0.200411137156593,-0.126835944344308,
-0.0544247933349339));
#75855=CARTESIAN_POINT('Ctrl Pts',(0.200403367596856,-0.126848220079705,
-0.0544257709939155));
#75856=CARTESIAN_POINT('Ctrl Pts',(0.200399345590891,-0.126854574092906,
-0.05442627707228));
#75857=CARTESIAN_POINT('Ctrl Pts',(0.200391001625303,-0.126867754602532,
-0.0544273269329174));
#75858=CARTESIAN_POINT('Ctrl Pts',(0.200386679619657,-0.126874581068429,
-0.0544278707181186));
#75859=CARTESIAN_POINT('Ctrl Pts',(0.200377706901994,-0.126888751578943,
-0.0544289996012303));
#75860=CARTESIAN_POINT('Ctrl Pts',(0.200373056134776,-0.126896095589163,
-0.0544295847027166));
#75861=CARTESIAN_POINT('Ctrl Pts',(0.200363393455383,-0.126911352036645,
-0.054430800289052));
#75862=CARTESIAN_POINT('Ctrl Pts',(0.200358381478679,-0.126919264432039,
-0.054431430778038));
#75863=CARTESIAN_POINT('Ctrl Pts',(0.200347959637473,-0.126935715211567,
-0.0544327417492392));
#75864=CARTESIAN_POINT('Ctrl Pts',(0.200342549696038,-0.126944253546433,
-0.0544334222364082));
#75865=CARTESIAN_POINT('Ctrl Pts',(0.200331290129024,-0.126962021642882,
-0.0544348384467625));
#75866=CARTESIAN_POINT('Ctrl Pts',(0.200325440411186,-0.126971251346402,
-0.0544355741759215));
#75867=CARTESIAN_POINT('Ctrl Pts',(0.20031325352696,-0.126990476912724,
-0.054437106860315));
#75868=CARTESIAN_POINT('Ctrl Pts',(0.200306916249913,-0.127000472705921,
-0.0544379038227216));
#75869=CARTESIAN_POINT('Ctrl Pts',(0.20029369939146,-0.127021316219308,
-0.0544395658513579));
#75870=CARTESIAN_POINT('Ctrl Pts',(0.200286819678411,-0.127032163852739,
-0.0544404309260182));
#75871=CARTESIAN_POINT('Ctrl Pts',(0.200272454615401,-0.127054809993787,
-0.0544422371177047));
#75872=CARTESIAN_POINT('Ctrl Pts',(0.200264969103648,-0.127066608399492,
-0.054443178245233));
#75873=CARTESIAN_POINT('Ctrl Pts',(0.200249318899478,-0.127091270893961,
-0.0544451457586584));
#75874=CARTESIAN_POINT('Ctrl Pts',(0.200241154010927,-0.127104134856105,
-0.0544461721572159));
#75875=CARTESIAN_POINT('Ctrl Pts',(0.200226318960041,-0.127127502829,-0.0544480369171733));
#75876=CARTESIAN_POINT('Ctrl Pts',(0.200219649209185,-0.127138007103998,
-0.0544488752519425));
#75877=CARTESIAN_POINT('Ctrl Pts',(0.200202513634127,-0.127164989445355,
-0.0544510289288671));
#75878=CARTESIAN_POINT('Ctrl Pts',(0.200192046604907,-0.127181466740238,
-0.0544523443491516));
#75879=CARTESIAN_POINT('Ctrl Pts',(0.200155105019507,-0.127239604668286,
-0.0544569864645531));
#75880=CARTESIAN_POINT('Ctrl Pts',(0.200128619517845,-0.127281258288021,
-0.0544603138702484));
#75881=CARTESIAN_POINT('Ctrl Pts',(0.199748158275235,-0.127879195497085,
-0.0545081004141175));
#75882=CARTESIAN_POINT('Ctrl Pts',(0.199391891122265,-0.12843398729936,
-0.0545527101709068));
#75883=CARTESIAN_POINT('Ctrl Pts',(0.198536343300947,-0.129754136959971,
-0.0546595072140715));
#75884=CARTESIAN_POINT('Ctrl Pts',(0.198034952730123,-0.130518094905958,
-0.0547218290234923));
#75885=CARTESIAN_POINT('Ctrl Pts',(0.196382370235541,-0.133004653682108,
-0.0549263310661629));
#75886=CARTESIAN_POINT('Ctrl Pts',(0.195213056526881,-0.134715014307767,
-0.0550696094276162));
#75887=CARTESIAN_POINT('Ctrl Pts',(0.187132358221273,-0.146208542816238,
-0.0560491591106425));
#75888=CARTESIAN_POINT('Ctrl Pts',(0.179511437687025,-0.155470396876478,
-0.0569208452468902));
#75889=CARTESIAN_POINT('Ctrl Pts',(0.163902810340877,-0.171755093499542,
-0.0585664861289188));
#75890=CARTESIAN_POINT('Ctrl Pts',(0.156077517866197,-0.178896002122403,
-0.0593382776378411));
#75891=CARTESIAN_POINT('Ctrl Pts',(0.140491598256113,-0.191315033070328,
-0.0607630397227132));
#75892=CARTESIAN_POINT('Ctrl Pts',(0.132843524769311,-0.196702742587695,
-0.0614182504510669));
#75893=CARTESIAN_POINT('Ctrl Pts',(0.123021585651424,-0.202786917464426,
-0.0622071770197591));
#75894=CARTESIAN_POINT('Ctrl Pts',(0.121130583050321,-0.203922109763472,
-0.0623568184425714));
#75895=CARTESIAN_POINT('Ctrl Pts',(0.118087165740926,-0.205691835519322,
-0.0625941627852089));
#75896=CARTESIAN_POINT('Ctrl Pts',(0.11694486925447,-0.206343421478318,
-0.0626824751914192));
#75897=CARTESIAN_POINT('Ctrl Pts',(0.114769190859445,-0.207560595958415,
-0.0628492485818871));
#75898=CARTESIAN_POINT('Ctrl Pts',(0.11373690363406,-0.208128049532983,
-0.0629277742163327));
#75899=CARTESIAN_POINT('Ctrl Pts',(0.111378467038472,-0.209401707059572,
-0.063105837232709));
#75900=CARTESIAN_POINT('Ctrl Pts',(0.110049740122914,-0.210103052600945,
-0.0632052009302801));
#75901=CARTESIAN_POINT('Ctrl Pts',(0.105943058826969,-0.212221045683783,
-0.0635094563079053));
#75902=CARTESIAN_POINT('Ctrl Pts',(0.103143688473451,-0.213595610785489,
-0.0637128835617589));
#75903=CARTESIAN_POINT('Ctrl Pts',(0.0839101043146858,-0.222573469144085,
-0.0650857066937842));
#75904=CARTESIAN_POINT('Ctrl Pts',(0.0666790650596363,-0.228328368378285,
-0.066187684147284));
#75905=CARTESIAN_POINT('Ctrl Pts',(0.0448381780651893,-0.232936169444844,
-0.0675569835304955));
#75906=CARTESIAN_POINT('Ctrl Pts',(0.0406945805117616,-0.233695680349334,
-0.0678158930163265));
#75907=CARTESIAN_POINT('Ctrl Pts',(0.0301696114994126,-0.235336466706992,
-0.0684757787806644));
#75908=CARTESIAN_POINT('Ctrl Pts',(0.023768856740451,-0.236068819383293,
-0.0688791336764089));
#75909=CARTESIAN_POINT('Ctrl Pts',(0.0137275642480068,-0.2368052015335,
-0.069525711002115));
#75910=CARTESIAN_POINT('Ctrl Pts',(0.0101030129709715,-0.236987499939797,
-0.0697619087733305));
#75911=CARTESIAN_POINT('Ctrl Pts',(0.00536486025256381,-0.237116921263174,
-0.0700759910807173));
#75912=CARTESIAN_POINT('Ctrl Pts',(0.00425359434382207,-0.237139458734659,
-0.0701500362865578));
#75913=CARTESIAN_POINT('Ctrl Pts',(0.00243782708816929,-0.237163517233428,
-0.0702717067319259));
#75914=CARTESIAN_POINT('Ctrl Pts',(0.00173338935264927,-0.237169711885553,
-0.0703190775162847));
#75915=CARTESIAN_POINT('Ctrl Pts',(0.000360142134917721,-0.237175669557212,
-0.0704117688757194));
#75916=CARTESIAN_POINT('Ctrl Pts',(-0.000308651197940893,-0.237175742058156,
-0.0704570724444562));
#75917=CARTESIAN_POINT('Ctrl Pts',(-0.0018068708919154,-0.237169567694617,
-0.0705589109484881));
#75918=CARTESIAN_POINT('Ctrl Pts',(-0.00263628093352684,-0.237161798343516,
-0.0706155284544852));
#75919=CARTESIAN_POINT('Ctrl Pts',(-0.0055295702210324,-0.237119516888802,
-0.0708138289541566));
#75920=CARTESIAN_POINT('Ctrl Pts',(-0.00759295480567648,-0.237062413190828,
-0.0709566652065116));
#75921=CARTESIAN_POINT('Ctrl Pts',(-0.0218368899586364,-0.236482070691389,
-0.0719512896540136));
#75922=CARTESIAN_POINT('Ctrl Pts',(-0.0339609371229547,-0.235047260827278,
-0.0728403779867142));
#75923=CARTESIAN_POINT('Ctrl Pts',(-0.0566183719172663,-0.230575934993547,
-0.0745278089015591));
#75924=CARTESIAN_POINT('Ctrl Pts',(-0.0671595412626176,-0.227729073102524,
-0.0753239494707382));
#75925=CARTESIAN_POINT('Ctrl Pts',(-0.0831163325583045,-0.22221469410172,
-0.0765299836855675));
#75926=CARTESIAN_POINT('Ctrl Pts',(-0.0886892828642959,-0.220049804104411,
-0.0769515524117712));
#75927=CARTESIAN_POINT('Ctrl Pts',(-0.0979515320207506,-0.216042612797609,
-0.0776522300415399));
#75928=CARTESIAN_POINT('Ctrl Pts',(-0.101685187203332,-0.214310614720927,
-0.07793470630629));
#75929=CARTESIAN_POINT('Ctrl Pts',(-0.106861138388362,-0.211743808067834,
-0.0783265852228423));
#75930=CARTESIAN_POINT('Ctrl Pts',(-0.108342409660623,-0.210989728822862,
-0.078438770424016));
#75931=CARTESIAN_POINT('Ctrl Pts',(-0.110870918714153,-0.209668875711607,
-0.0786303687796769));
#75932=CARTESIAN_POINT('Ctrl Pts',(-0.11192202284175,-0.2091096816309,-0.0787100465633688));
#75933=CARTESIAN_POINT('Ctrl Pts',(-0.113921145129769,-0.208026743964054,
-0.0788616646966255));
#75934=CARTESIAN_POINT('Ctrl Pts',(-0.11486987053429,-0.20750437687515,
-0.0789336517283876));
#75935=CARTESIAN_POINT('Ctrl Pts',(-0.117083562742454,-0.20626568566774,
-0.0791017204709229));
#75936=CARTESIAN_POINT('Ctrl Pts',(-0.11834559751945,-0.205544188569614,
-0.0791976134647109));
#75937=CARTESIAN_POINT('Ctrl Pts',(-0.122052534778528,-0.203379495597458,
-0.0794795748395817));
#75938=CARTESIAN_POINT('Ctrl Pts',(-0.124478304401009,-0.201903921032023,
-0.0796644700421166));
#75939=CARTESIAN_POINT('Ctrl Pts',(-0.141419652375891,-0.191177230968593,
-0.0809600374885441));
#75940=CARTESIAN_POINT('Ctrl Pts',(-0.154917030248592,-0.18041355612816,
-0.0820098088353067));
#75941=CARTESIAN_POINT('Ctrl Pts',(-0.177082386753192,-0.158399797967705,
-0.0839226617382625));
#75942=CARTESIAN_POINT('Ctrl Pts',(-0.186135571550302,-0.147655340394726,
-0.0847823218684297));
#75943=CARTESIAN_POINT('Ctrl Pts',(-0.195164671528303,-0.134779969224629,
-0.0858137660865564));
#75944=CARTESIAN_POINT('Ctrl Pts',(-0.196128736414607,-0.133373188654349,
-0.0859264932023624));
#75945=CARTESIAN_POINT('Ctrl Pts',(-0.197536819723423,-0.131270206098783,
-0.0860952504988646));
#75946=CARTESIAN_POINT('Ctrl Pts',(-0.197992533731215,-0.13058184671035,
-0.0861505270739946));
#75947=CARTESIAN_POINT('Ctrl Pts',(-0.198767589085154,-0.12939773528402,
-0.0862457044692087));
#75948=CARTESIAN_POINT('Ctrl Pts',(-0.19908868897228,-0.128903150745055,
-0.0862854866995572));
#75949=CARTESIAN_POINT('Ctrl Pts',(-0.199818486361409,-0.127769824842621,
-0.0863767129294122));
#75950=CARTESIAN_POINT('Ctrl Pts',(-0.200225961271355,-0.127130326925791,
-0.0864282347117256));
#75951=CARTESIAN_POINT('Ctrl Pts',(-0.201335775554544,-0.125369995082972,
-0.086570159368804));
#75952=CARTESIAN_POINT('Ctrl Pts',(-0.20203180324681,-0.124245243209492,
-0.0866609536062306));
#75953=CARTESIAN_POINT('Ctrl Pts',(-0.205680085236808,-0.118238053191723,
-0.0871462310204833));
#75954=CARTESIAN_POINT('Ctrl Pts',(-0.208464601193013,-0.113256490952333,
-0.0875498545609662));
#75955=CARTESIAN_POINT('Ctrl Pts',(-0.218702192169865,-0.0932822322136545,
-0.0891595544137602));
#75956=CARTESIAN_POINT('Ctrl Pts',(-0.224739209200121,-0.0776179879845412,
-0.0903992235482619));
#75957=CARTESIAN_POINT('Ctrl Pts',(-0.231860148189455,-0.0510712781021315,
-0.0923759712771183));
#75958=CARTESIAN_POINT('Ctrl Pts',(-0.233935662075728,-0.0405162896788951,
-0.0931327866834833));
#75959=CARTESIAN_POINT('Ctrl Pts',(-0.235575466598854,-0.0275931283719011,
-0.0940229323734671));
#75960=CARTESIAN_POINT('Ctrl Pts',(-0.235829896139041,-0.025326703617522,
-0.0941777402842617));
#75961=CARTESIAN_POINT('Ctrl Pts',(-0.236180811944037,-0.0217341013475974,
-0.0944211502360611));
#75962=CARTESIAN_POINT('Ctrl Pts',(-0.236298899455012,-0.020410226184335,
-0.0945104225554074));
#75963=CARTESIAN_POINT('Ctrl Pts',(-0.236500159912637,-0.0179172661765964,
-0.0946777558405602));
#75964=CARTESIAN_POINT('Ctrl Pts',(-0.236585807552514,-0.0167484272430532,
-0.094755891744372));
#75965=CARTESIAN_POINT('Ctrl Pts',(-0.236759334094774,-0.0141123582010645,
-0.0949314150996178));
#75966=CARTESIAN_POINT('Ctrl Pts',(-0.236842245196064,-0.0126448404025159,
-0.0950286449075528));
#75967=CARTESIAN_POINT('Ctrl Pts',(-0.237046527478915,-0.00831465553332598,
-0.0953141800904135));
#75968=CARTESIAN_POINT('Ctrl Pts',(-0.23712967786779,-0.0054503862617585,
-0.0955012980030014));
#75969=CARTESIAN_POINT('Ctrl Pts',(-0.237376655468488,0.0172067421768256,
-0.0969693134541154));
#75970=CARTESIAN_POINT('Ctrl Pts',(-0.235114231299932,0.0369476174326382,
-0.0981666877287926));
#75971=CARTESIAN_POINT('Ctrl Pts',(-0.228475771996707,0.0641759067051366,
-0.0998914917931622));
#75972=CARTESIAN_POINT('Ctrl Pts',(-0.226111375753752,0.072064906198731,
-0.100401685561311));
#75973=CARTESIAN_POINT('Ctrl Pts',(-0.221915157252005,0.0838070436925666,
-0.101198195648931));
#75974=CARTESIAN_POINT('Ctrl Pts',(-0.220381630715368,0.0877604072705071,
-0.101473017725974));
#75975=CARTESIAN_POINT('Ctrl Pts',(-0.218289092861059,0.0927536110717456,
-0.101831289357));
#75976=CARTESIAN_POINT('Ctrl Pts',(-0.217827049540407,0.0938335589011456,
-0.101909456485216));
#75977=CARTESIAN_POINT('Ctrl Pts',(-0.217068943362879,0.095569726766183,
-0.102036289503191));
#75978=CARTESIAN_POINT('Ctrl Pts',(-0.216777874180959,0.0962281251897154,
-0.10208466075129));
#75979=CARTESIAN_POINT('Ctrl Pts',(-0.216211674285649,0.097493263140531,
-0.102178153874216));
#75980=CARTESIAN_POINT('Ctrl Pts',(-0.215936979035774,0.0981001809090765,
-0.102223249815646));
#75981=CARTESIAN_POINT('Ctrl Pts',(-0.215323984791063,0.0994394944572594,
-0.102323297345094));
#75982=CARTESIAN_POINT('Ctrl Pts',(-0.214984498814626,0.100171336747408,
-0.102378319591914));
#75983=CARTESIAN_POINT('Ctrl Pts',(-0.21376578858428,0.102763822962466,
-0.102574451244748));
#75984=CARTESIAN_POINT('Ctrl Pts',(-0.212866119242487,0.104614675065719,
-0.102716716532706));
#75985=CARTESIAN_POINT('Ctrl Pts',(-0.205445213885111,0.119389250731872,
-0.10386912587332));
#75986=CARTESIAN_POINT('Ctrl Pts',(-0.197777874960259,0.131701813606501,
-0.104931439576513));
#75987=CARTESIAN_POINT('Ctrl Pts',(-0.183224240622791,0.150908902640768,
-0.106690099009823));
#75988=CARTESIAN_POINT('Ctrl Pts',(-0.176949469730423,0.158219882939297,
-0.107388731877561));
#75989=CARTESIAN_POINT('Ctrl Pts',(-0.164550925129815,0.171002670601748,
-0.108655484035029));
#75990=CARTESIAN_POINT('Ctrl Pts',(-0.158553968031887,0.176577425116427,
-0.109226722000924));
#75991=CARTESIAN_POINT('Ctrl Pts',(-0.150655810034008,0.183191966493385,
-0.109929483977509));
#75992=CARTESIAN_POINT('Ctrl Pts',(-0.149013265636112,0.184530530962521,
-0.110073129790207));
#75993=CARTESIAN_POINT('Ctrl Pts',(-0.146340408514578,0.186649766243898,
-0.110302956417574));
#75994=CARTESIAN_POINT('Ctrl Pts',(-0.145321298795663,0.187444313421689,
-0.110389688551851));
#75995=CARTESIAN_POINT('Ctrl Pts',(-0.143362477055389,0.18894592767337,
-0.110554717314766));
#75996=CARTESIAN_POINT('Ctrl Pts',(-0.14242390371116,0.189654409779722,
-0.11063306816178));
#75997=CARTESIAN_POINT('Ctrl Pts',(-0.140275849388458,0.191250929349737,
-0.110810772765256));
#75998=CARTESIAN_POINT('Ctrl Pts',(-0.139063124681192,0.192134534705682,
-0.110909952406068));
#75999=CARTESIAN_POINT('Ctrl Pts',(-0.135223831944562,0.194876493255582,
-0.111220438940319));
#76000=CARTESIAN_POINT('Ctrl Pts',(-0.132567716955189,0.196692995271332,
-0.111430151941891));
#76001=CARTESIAN_POINT('Ctrl Pts',(-0.117474710265588,0.206570347662989,
-0.112595452893011));
#76002=CARTESIAN_POINT('Ctrl Pts',(-0.10434021716574,0.213505990716383,
-0.113508436933499));
#76003=CARTESIAN_POINT('Ctrl Pts',(-0.0797631594554744,0.223670365562725,
-0.115138736986617));
#76004=CARTESIAN_POINT('Ctrl Pts',(-0.0685643471672252,0.227353212336554,
-0.115856262258257));
#76005=CARTESIAN_POINT('Ctrl Pts',(-0.0521091052626759,0.231437863805961,
-0.116930921805025));
#76006=CARTESIAN_POINT('Ctrl Pts',(-0.0470396628855004,0.232521191234172,
-0.117264799246147));
#76007=CARTESIAN_POINT('Ctrl Pts',(-0.0419392741328228,0.233437524640346,
-0.117607182502807));
#76008=CARTESIAN_POINT('',(0.150502666328431,-0.18330555925294,-0.04));
#76009=CARTESIAN_POINT('Origin',(0.,0.,-0.04));
#76010=CARTESIAN_POINT('',(-0.237174906472556,-0.000210629376151607,-0.0759410108039518));
#76011=CARTESIAN_POINT('Ctrl Pts',(-0.237174906472556,-0.000210629376151607,
-0.0759410108039518));
#76012=CARTESIAN_POINT('Ctrl Pts',(-0.237158621928716,-0.0185475073215331,
-0.0747111264345429));
#76013=CARTESIAN_POINT('Ctrl Pts',(-0.235011944072667,-0.0367877728492129,
-0.073481242065133));
#76014=CARTESIAN_POINT('Ctrl Pts',(-0.230823636693189,-0.0545199905422847,
-0.0722513576957233));
#76015=CARTESIAN_POINT('Ctrl Pts',(-0.23027479475933,-0.0568436463221744,
-0.0720901918464742));
#76016=CARTESIAN_POINT('Ctrl Pts',(-0.229690959325625,-0.0591586106164768,
-0.071929025997225));
#76017=CARTESIAN_POINT('Ctrl Pts',(-0.229072388495109,-0.0614639850168034,
-0.0717678601479759));
#76018=CARTESIAN_POINT('Ctrl Pts',(-0.225473876565801,-0.0748754116018108,
-0.0708302840410715));
#76019=CARTESIAN_POINT('Ctrl Pts',(-0.220679734069817,-0.0880206305498771,
-0.0698927079341669));
#76020=CARTESIAN_POINT('Ctrl Pts',(-0.214749523310849,-0.100670864021142,
-0.0689551318272628));
#76021=CARTESIAN_POINT('Ctrl Pts',(-0.208831413436207,-0.113295284073934,
-0.0680194688901394));
#76022=CARTESIAN_POINT('Ctrl Pts',(-0.201782122092558,-0.125425925126062,
-0.0670838059530158));
#76023=CARTESIAN_POINT('Ctrl Pts',(-0.193710062291085,-0.136851716803933,
-0.0661481430158926));
#76024=CARTESIAN_POINT('Ctrl Pts',(-0.185637996783948,-0.148277516558024,
-0.0652124794174042));
#76025=CARTESIAN_POINT('Ctrl Pts',(-0.176543608234863,-0.158997737682083,
-0.0642768158189159));
#76026=CARTESIAN_POINT('Ctrl Pts',(-0.166579315386946,-0.168829240092516,
-0.0633411522204277));
#76027=CARTESIAN_POINT('Ctrl Pts',(-0.156616017366152,-0.178659760933518,
-0.0624055820378537));
#76028=CARTESIAN_POINT('Ctrl Pts',(-0.145783612815802,-0.187601155783707,
-0.0614700118552792));
#76029=CARTESIAN_POINT('Ctrl Pts',(-0.134270399414448,-0.195508159589529,
-0.0605344416727052));
#76030=CARTESIAN_POINT('Ctrl Pts',(-0.122726310093654,-0.203436368249634,
-0.0595963624955889));
#76031=CARTESIAN_POINT('Ctrl Pts',(-0.110498503346432,-0.210324207770786,
-0.0586582833184732));
#76032=CARTESIAN_POINT('Ctrl Pts',(-0.0978025802286634,-0.216070904856753,
-0.0577202041413569));
#76033=CARTESIAN_POINT('Ctrl Pts',(-0.0895185622228277,-0.219820592192808,
-0.0571081127855693));
#76034=CARTESIAN_POINT('Ctrl Pts',(-0.0810357512357401,-0.223085405507269,
-0.0564960214297812));
#76035=CARTESIAN_POINT('Ctrl Pts',(-0.0724175090206001,-0.225848810074907,
-0.0558839300739935));
#76036=CARTESIAN_POINT('Ctrl Pts',(-0.058700685419742,-0.230247054176878,
-0.054909723391777));
#76037=CARTESIAN_POINT('Ctrl Pts',(-0.0445441512454388,-0.233403639176892,
-0.0539355167095605));
#76038=CARTESIAN_POINT('Ctrl Pts',(-0.0301891542800366,-0.235245819492836,
-0.0529613100273441));
#76039=CARTESIAN_POINT('Ctrl Pts',(-0.0158683657925657,-0.237083609826336,
-0.0519894249149523));
#76040=CARTESIAN_POINT('Ctrl Pts',(-0.00135080955263697,-0.237613054939815,
-0.0510175398025608));
#76041=CARTESIAN_POINT('Ctrl Pts',(0.0131117876559467,-0.236812292015143,
-0.0500456546901691));
#76042=CARTESIAN_POINT('Ctrl Pts',(0.0275557422064152,-0.236012561294384,
-0.0490750223625722));
#76043=CARTESIAN_POINT('Ctrl Pts',(0.0419441028805848,-0.233886027421871,
-0.0481043900349758));
#76044=CARTESIAN_POINT('Ctrl Pts',(0.056025401347839,-0.23046287125872,
-0.0471337577073792));
#76045=CARTESIAN_POINT('Ctrl Pts',(0.0700949748608359,-0.22704256542571,
-0.046163933587894));
#76046=CARTESIAN_POINT('Ctrl Pts',(0.0838572370641301,-0.222327955504268,
-0.0451941094684088));
#76047=CARTESIAN_POINT('Ctrl Pts',(0.0970721910482277,-0.216400023914269,
-0.0442242853489239));
#76048=CARTESIAN_POINT('Ctrl Pts',(0.110296407387627,-0.210467937439687,
-0.04325378148015));
#76049=CARTESIAN_POINT('Ctrl Pts',(0.122971840732214,-0.203321153059231,
-0.0422832776113755));
#76050=CARTESIAN_POINT('Ctrl Pts',(0.134879909857446,-0.195088160947422,
-0.0413127737426016));
#76051=CARTESIAN_POINT('Ctrl Pts',(0.140249148447719,-0.191375980702644,
-0.0408751824950676));
#76052=CARTESIAN_POINT('Ctrl Pts',(0.145462740656309,-0.187443580242826,
-0.0404375912475343));
#76053=CARTESIAN_POINT('Ctrl Pts',(0.150502666328431,-0.18330555925294,
-0.0400000000000005));
#76054=CARTESIAN_POINT('Ctrl Pts',(-0.237174906802781,-0.000210257205037135,
-0.0759349427062525));
#76055=CARTESIAN_POINT('Ctrl Pts',(-0.237184871465481,0.0110301088355765,
-0.0766243420965755));
#76056=CARTESIAN_POINT('Ctrl Pts',(-0.236395779708201,0.0222563389972307,
-0.0773177921882711));
#76057=CARTESIAN_POINT('Ctrl Pts',(-0.234160303454425,0.0379800345014828,
-0.0783290024312435));
#76058=CARTESIAN_POINT('Ctrl Pts',(-0.233372123243744,0.0425555912896126,
-0.0786279996175695));
#76059=CARTESIAN_POINT('Ctrl Pts',(-0.232138852293334,0.0486414640296778,
-0.0790334908787454));
#76060=CARTESIAN_POINT('Ctrl Pts',(-0.231812242696509,0.0501749211471305,
-0.0791363285688339));
#76061=CARTESIAN_POINT('Ctrl Pts',(-0.231151157611951,0.0531344351987663,
-0.0793361544101244));
#76062=CARTESIAN_POINT('Ctrl Pts',(-0.230818627185992,0.0545608564178603,
-0.0794330779268147));
#76063=CARTESIAN_POINT('Ctrl Pts',(-0.230192614039309,0.0571380010832394,
-0.0796093424027828));
#76064=CARTESIAN_POINT('Ctrl Pts',(-0.229903657821878,0.0582897826325445,
-0.0796885374281201));
#76065=CARTESIAN_POINT('Ctrl Pts',(-0.22926304781756,0.060764372255098,
-0.0798596117821293));
#76066=CARTESIAN_POINT('Ctrl Pts',(-0.228908569309991,0.0620863978056552,
-0.079951578523863));
#76067=CARTESIAN_POINT('Ctrl Pts',(-0.22791578960818,0.0656648475377874,
-0.0802021039836467));
#76068=CARTESIAN_POINT('Ctrl Pts',(-0.227255448984399,0.0679149437704475,
-0.0803613582399107));
#76069=CARTESIAN_POINT('Ctrl Pts',(-0.223314490021691,0.0806420971034408,
-0.0812722542829496));
#76070=CARTESIAN_POINT('Ctrl Pts',(-0.21934334157729,0.090889749731291,
-0.0820458021824909));
#76071=CARTESIAN_POINT('Ctrl Pts',(-0.209585964487055,0.111665367466873,
-0.0836949756063555));
#76072=CARTESIAN_POINT('Ctrl Pts',(-0.203680656515842,0.122104880727242,
-0.0845712972506596));
#76073=CARTESIAN_POINT('Ctrl Pts',(-0.192340692450215,0.139023187812856,
-0.086044737919071));
#76074=CARTESIAN_POINT('Ctrl Pts',(-0.187301726833644,0.145741140601818,
-0.0866455770107887));
#76075=CARTESIAN_POINT('Ctrl Pts',(-0.180822706082521,0.153486276444645,
-0.0873459029039126));
#76076=CARTESIAN_POINT('Ctrl Pts',(-0.179714534521033,0.154782345818205,
-0.0874633599572446));
#76077=CARTESIAN_POINT('Ctrl Pts',(-0.178024842028212,0.156715922302783,
-0.0876388503564303));
#76078=CARTESIAN_POINT('Ctrl Pts',(-0.177453690138022,0.157362360798179,
-0.0876975651350682));
#76079=CARTESIAN_POINT('Ctrl Pts',(-0.176431219120985,0.158506963088898,
-0.0878015841051318));
#76080=CARTESIAN_POINT('Ctrl Pts',(-0.175981287427686,0.159006348771741,
-0.0878469862438275));
#76081=CARTESIAN_POINT('Ctrl Pts',(-0.174995754780171,0.160090898153959,
-0.0879456209862042));
#76082=CARTESIAN_POINT('Ctrl Pts',(-0.174459333737651,0.160675296110486,
-0.0879987922362712));
#76083=CARTESIAN_POINT('Ctrl Pts',(-0.172930307121767,0.162324392126888,
-0.0881489377149598));
#76084=CARTESIAN_POINT('Ctrl Pts',(-0.171930797592166,0.16338268114712,
-0.0882454148530343));
#76085=CARTESIAN_POINT('Ctrl Pts',(-0.165292232081609,0.170283259705127,
-0.0888758498991717));
#76086=CARTESIAN_POINT('Ctrl Pts',(-0.159365443180029,0.175842531747045,
-0.0893902801404555));
#76087=CARTESIAN_POINT('Ctrl Pts',(-0.140071327184596,0.192161582258995,
-0.0909649355060656));
#76088=CARTESIAN_POINT('Ctrl Pts',(-0.125815890111833,0.201783142663815,
-0.0919949081816021));
#76089=CARTESIAN_POINT('Ctrl Pts',(-0.103740430807673,0.213426518917386,
-0.0935611549519308));
#76090=CARTESIAN_POINT('Ctrl Pts',(-0.0966585351981046,0.216725781169569,
-0.0940591087956679));
#76091=CARTESIAN_POINT('Ctrl Pts',(-0.087521784953452,0.220445346438063,
-0.0947033806385633));
#76092=CARTESIAN_POINT('Ctrl Pts',(-0.085606255171609,0.221196252788198,
-0.094838536730929));
#76093=CARTESIAN_POINT('Ctrl Pts',(-0.082453235290099,0.222385177215646,
-0.0950612662435626));
#76094=CARTESIAN_POINT('Ctrl Pts',(-0.0812214226796713,0.222838020624795,
-0.0951483451909119));
#76095=CARTESIAN_POINT('Ctrl Pts',(-0.078876005780729,0.223678220611693,
-0.095314298212735));
#76096=CARTESIAN_POINT('Ctrl Pts',(-0.0777631440224593,0.224067543409303,
-0.095393104370899));
#76097=CARTESIAN_POINT('Ctrl Pts',(-0.0752199078727373,0.224936038884836,
-0.0955733702939126));
#76098=CARTESIAN_POINT('Ctrl Pts',(-0.0737877840137135,0.225409890815699,
-0.0956750013880507));
#76099=CARTESIAN_POINT('Ctrl Pts',(-0.0693527254060101,0.226830540068804,
-0.095990165247697));
#76100=CARTESIAN_POINT('Ctrl Pts',(-0.0663354882016132,0.227731191929472,
-0.0962051840564345));
#76101=CARTESIAN_POINT('Ctrl Pts',(-0.0562535680305483,0.230523312114176,
-0.0969260105663089));
#76102=CARTESIAN_POINT('Ctrl Pts',(-0.0491251218842478,0.232146520123974,
-0.0974396283497645));
#76103=CARTESIAN_POINT('Ctrl Pts',(-0.0419392282806928,0.233437532878113,
-0.0979609479953583));
#76104=CARTESIAN_POINT('Origin',(3.51939854619125E-17,0.,-0.04));
#76105=CARTESIAN_POINT('',(-0.287838815064698,-0.060847814604559,-0.04));
#76106=CARTESIAN_POINT('Origin',(0.,0.,-0.04));
#76107=CARTESIAN_POINT('Ctrl Pts',(-0.287838815064696,-0.0608478146045586,
-0.0399999999999992));
#76108=CARTESIAN_POINT('Ctrl Pts',(-0.286283540210113,-0.0659045633072947,
-0.0399999999999988));
#76109=CARTESIAN_POINT('Ctrl Pts',(-0.284582373527586,-0.0709112958269072,
-0.0399999999999993));
#76110=CARTESIAN_POINT('Ctrl Pts',(-0.28273331426505,-0.0758621163637482,
-0.0399999999999997));
#76111=CARTESIAN_POINT('Ctrl Pts',(-0.278025520183387,-0.0884671442798089,
-0.0400000000000001));
#76112=CARTESIAN_POINT('Ctrl Pts',(-0.272360008650186,-0.100710598371884,
-0.0400000000000012));
#76113=CARTESIAN_POINT('Ctrl Pts',(-0.265818480752146,-0.112520517868452,
-0.0400000000000015));
#76114=CARTESIAN_POINT('Ctrl Pts',(-0.260688658964569,-0.121781776596889,
-0.0400000000000017));
#76115=CARTESIAN_POINT('Ctrl Pts',(-0.255013694239099,-0.130782755603393,
-0.0400000000000012));
#76116=CARTESIAN_POINT('Ctrl Pts',(-0.248864487923652,-0.139437457683636,
-0.0400000000000016));
#76117=CARTESIAN_POINT('Ctrl Pts',(-0.240894471708758,-0.150654859145894,
-0.0400000000000022));
#76118=CARTESIAN_POINT('Ctrl Pts',(-0.23212064683322,-0.161308101360409,
-0.0400000000000023));
#76119=CARTESIAN_POINT('Ctrl Pts',(-0.222626939812443,-0.171314385878302,
-0.0400000000000022));
#76120=CARTESIAN_POINT('Ctrl Pts',(-0.21832455164424,-0.175849065537495,
-0.0400000000000022));
#76121=CARTESIAN_POINT('Ctrl Pts',(-0.213872397622076,-0.180252249579648,
-0.0400000000000026));
#76122=CARTESIAN_POINT('Ctrl Pts',(-0.209283584109627,-0.184509529763357,
-0.0400000000000031));
#76123=CARTESIAN_POINT('Ctrl Pts',(-0.204476924871702,-0.188968916719908,
-0.0400000000000036));
#76124=CARTESIAN_POINT('Ctrl Pts',(-0.199527853480205,-0.193261361732437,
-0.0400000000000041));
#76125=CARTESIAN_POINT('Ctrl Pts',(-0.194449905572787,-0.197375579987002,
-0.0400000000000039));
#76126=CARTESIAN_POINT('Ctrl Pts',(-0.18165053109359,-0.207745796674809,
-0.0400000000000036));
#76127=CARTESIAN_POINT('Ctrl Pts',(-0.168024374394842,-0.216995232927637,
-0.0400000000000015));
#76128=CARTESIAN_POINT('Ctrl Pts',(-0.153712907451332,-0.224968312253503,
-0.0400000000000022));
#76129=CARTESIAN_POINT('Ctrl Pts',(-0.143239782181528,-0.230803008228101,
-0.0400000000000027));
#76130=CARTESIAN_POINT('Ctrl Pts',(-0.132399065183417,-0.235953385843509,
-0.0400000000000035));
#76131=CARTESIAN_POINT('Ctrl Pts',(-0.121243795560285,-0.240340769520388,
-0.0400000000000029));
#76132=CARTESIAN_POINT('Ctrl Pts',(-0.109335780392514,-0.245024209108684,
-0.0400000000000027));
#76133=CARTESIAN_POINT('Ctrl Pts',(-0.0971496399731909,-0.248806596857885,
-0.040000000000001));
#76134=CARTESIAN_POINT('Ctrl Pts',(-0.0847601082121804,-0.251609660970604,
-0.0400000000000014));
#76135=CARTESIAN_POINT('Ctrl Pts',(-0.0834902268297793,-0.25189696472018,
-0.0400000000000015));
#76136=CARTESIAN_POINT('Ctrl Pts',(-0.0822181843381618,-0.252173969867375,
-0.0400000000000012));
#76137=CARTESIAN_POINT('Ctrl Pts',(-0.0809440531687431,-0.252440581539771,
-0.0400000000000011));
#76138=CARTESIAN_POINT('Ctrl Pts',(-0.0684659059362601,-0.255051631156887,
-0.04));
#76139=CARTESIAN_POINT('Ctrl Pts',(-0.0557870915798686,-0.256667486014179,
-0.0399999999999995));
#76140=CARTESIAN_POINT('Ctrl Pts',(-0.0430126701052795,-0.257314032850501,
-0.0399999999999991));
#76141=CARTESIAN_POINT('Ctrl Pts',(-0.037129326557397,-0.257611804234156,
-0.0399999999999989));
#76142=CARTESIAN_POINT('Ctrl Pts',(-0.0312252572910126,-0.257703706671377,
-0.0399999999999976));
#76143=CARTESIAN_POINT('Ctrl Pts',(-0.0253118328480331,-0.257590874842292,
-0.039999999999998));
#76144=CARTESIAN_POINT('Ctrl Pts',(-0.0194836856989803,-0.257479670157198,
-0.0399999999999984));
#76145=CARTESIAN_POINT('Ctrl Pts',(-0.0136532337202037,-0.257169362129647,
-0.0399999999999976));
#76146=CARTESIAN_POINT('Ctrl Pts',(-0.00784763512537938,-0.256664290536718,
-0.0399999999999974));
#76147=CARTESIAN_POINT('Ctrl Pts',(0.00781580971746332,-0.255301612613277,
-0.0399999999999969));
#76148=CARTESIAN_POINT('Ctrl Pts',(0.0233323927142078,-0.252524616633121,
-0.0399999999999976));
#76149=CARTESIAN_POINT('Ctrl Pts',(0.0385007003554855,-0.248383008519942,
-0.0399999999999976));
#76150=CARTESIAN_POINT('Ctrl Pts',(0.0491632350559369,-0.245471672511548,
-0.0399999999999976));
#76151=CARTESIAN_POINT('Ctrl Pts',(0.059653511041483,-0.241884935280662,
-0.0399999999999978));
#76152=CARTESIAN_POINT('Ctrl Pts',(0.0698923366418034,-0.237627597582937,
-0.0399999999999982));
#76153=CARTESIAN_POINT('Ctrl Pts',(0.0737978347774825,-0.236003678484158,
-0.0399999999999983));
#76154=CARTESIAN_POINT('Ctrl Pts',(0.0776663307490886,-0.234281976313234,
-0.0399999999999973));
#76155=CARTESIAN_POINT('Ctrl Pts',(0.0814808838935122,-0.232468982961978,
-0.0399999999999975));
#76156=CARTESIAN_POINT('Ctrl Pts',(0.0948711124254617,-0.226104831151508,
-0.0399999999999976));
#76157=CARTESIAN_POINT('Ctrl Pts',(0.107640202715245,-0.218602145131227,
-0.0399999999999986));
#76158=CARTESIAN_POINT('Ctrl Pts',(0.119605438277537,-0.209989258535857,
-0.0399999999999986));
#76159=CARTESIAN_POINT('Ctrl Pts',(0.130647229961905,-0.202041090771666,
-0.0399999999999991));
#76160=CARTESIAN_POINT('Ctrl Pts',(0.141004945256145,-0.193146676236034,
-0.0399999999999997));
#76161=CARTESIAN_POINT('Ctrl Pts',(0.150502666328436,-0.183305559252936,
-0.0399999999999996));
#76162=CARTESIAN_POINT('',(0.22249458563984,0.0827040654021107,-0.0398874406537738));
#76163=CARTESIAN_POINT('Ctrl Pts',(0.223395701213113,0.0796639272475427,
-0.04));
#76164=CARTESIAN_POINT('Ctrl Pts',(0.2230414864133,0.0806572257995756,-0.0399624802179247));
#76165=CARTESIAN_POINT('Ctrl Pts',(0.222680646665404,0.081648161864277,
-0.039924960435849));
#76166=CARTESIAN_POINT('Ctrl Pts',(0.222313214070923,0.0826366472847004,
-0.0398874406537737));
#76167=CARTESIAN_POINT('Ctrl Pts',(0.222674980869761,0.0827832056464219,
-0.0400000000000007));
#76168=CARTESIAN_POINT('Ctrl Pts',(0.221331052085945,0.0884148732654746,
-0.0400000000000008));
#76169=CARTESIAN_POINT('Ctrl Pts',(0.219769833377309,0.0939831708252383,
-0.0400000000000001));
#76170=CARTESIAN_POINT('Ctrl Pts',(0.217990451664176,0.099475512510641,
-0.04));
#76171=CARTESIAN_POINT('Ctrl Pts',(0.214256976699871,0.110999470538598,
-0.0399999999999994));
#76172=CARTESIAN_POINT('Ctrl Pts',(0.209564791763102,0.122189312126664,
-0.0400000000000003));
#76173=CARTESIAN_POINT('Ctrl Pts',(0.204016432957559,0.132986817060258,
-0.0399999999999988));
#76174=CARTESIAN_POINT('Ctrl Pts',(0.200496467614902,0.139836922557307,
-0.0399999999999993));
#76175=CARTESIAN_POINT('Ctrl Pts',(0.196628495701105,0.146532151765652,
-0.0399999999999984));
#76176=CARTESIAN_POINT('Ctrl Pts',(0.19245580578463,0.153026708431451,-0.039999999999998));
#76177=CARTESIAN_POINT('Ctrl Pts',(0.186915308542496,0.161650180104644,
-0.0399999999999974));
#76178=CARTESIAN_POINT('Ctrl Pts',(0.180832662499186,0.169931866194158,
-0.0399999999999965));
#76179=CARTESIAN_POINT('Ctrl Pts',(0.174264480746233,0.177837483950101,
-0.0399999999999971));
#76180=CARTESIAN_POINT('Ctrl Pts',(0.16975483858615,0.183265395124708,-0.0399999999999975));
#76181=CARTESIAN_POINT('Ctrl Pts',(0.165014946191758,0.188517133640017,
-0.0399999999999955));
#76182=CARTESIAN_POINT('Ctrl Pts',(0.160064174348171,0.193576884039022,
-0.0399999999999964));
#76183=CARTESIAN_POINT('Ctrl Pts',(0.156162208776054,0.197564741384135,
-0.0399999999999971));
#76184=CARTESIAN_POINT('Ctrl Pts',(0.152134390718043,0.201427900135178,
-0.0399999999999966));
#76185=CARTESIAN_POINT('Ctrl Pts',(0.147995497593573,0.205155973605731,
-0.0399999999999967));
#76186=CARTESIAN_POINT('Ctrl Pts',(0.136081349924499,0.215887542774968,
-0.0399999999999971));
#76187=CARTESIAN_POINT('Ctrl Pts',(0.123234372878606,0.225517729201755,
-0.0399999999999972));
#76188=CARTESIAN_POINT('Ctrl Pts',(0.109642260298283,0.233917545345877,
-0.0399999999999972));
#76189=CARTESIAN_POINT('Ctrl Pts',(0.100917414355191,0.239309429894705,
-0.0399999999999972));
#76190=CARTESIAN_POINT('Ctrl Pts',(0.09188516178185,0.24419367893778,-0.0399999999999965));
#76191=CARTESIAN_POINT('Ctrl Pts',(0.0825842917960279,0.248529743097262,
-0.0399999999999971));
#76192=CARTESIAN_POINT('Ctrl Pts',(0.0772852871455863,0.251000138251773,
-0.0399999999999974));
#76193=CARTESIAN_POINT('Ctrl Pts',(0.0719034015557044,0.253289849721424,
-0.0399999999999972));
#76194=CARTESIAN_POINT('Ctrl Pts',(0.0664655282955866,0.255384798311809,
-0.0399999999999977));
#76195=CARTESIAN_POINT('Ctrl Pts',(0.0572749031145685,0.258925500043301,
-0.0399999999999985));
#76196=CARTESIAN_POINT('Ctrl Pts',(0.0479118585129067,0.261916421959981,
-0.0399999999999984));
#76197=CARTESIAN_POINT('Ctrl Pts',(0.0384166442040826,0.264327757183461,
-0.0399999999999985));
#76198=CARTESIAN_POINT('Ctrl Pts',(0.0229887101002665,0.268245722562663,
-0.0399999999999994));
#76199=CARTESIAN_POINT('Ctrl Pts',(0.00721254038154319,0.270636624867907,
-0.0399999999999979));
#76200=CARTESIAN_POINT('Ctrl Pts',(-0.0087328601544421,0.271586817233884,
-0.0400000000000007));
#76201=CARTESIAN_POINT('Ctrl Pts',(-0.0117870319733156,0.271768816471854,
-0.0400000000000012));
#76202=CARTESIAN_POINT('Ctrl Pts',(-0.0148474612088789,0.271897813973021,
-0.0400000000000012));
#76203=CARTESIAN_POINT('Ctrl Pts',(-0.017912944060836,0.271974210463001,
-0.0400000000000013));
#76204=CARTESIAN_POINT('Ctrl Pts',(-0.023389560269392,0.2721106960594,-0.0400000000000013));
#76205=CARTESIAN_POINT('Ctrl Pts',(-0.0288790425251526,0.272078878082152,
-0.0400000000000002));
#76206=CARTESIAN_POINT('Ctrl Pts',(-0.034355927104671,0.271882901390066,
-0.0400000000000005));
#76207=CARTESIAN_POINT('Ctrl Pts',(-0.0515834758169103,0.271266456409283,
-0.0400000000000017));
#76208=CARTESIAN_POINT('Ctrl Pts',(-0.0687348278204772,0.269032047713159,
-0.0400000000000022));
#76209=CARTESIAN_POINT('Ctrl Pts',(-0.0855927959851901,0.265288603456289,
-0.0400000000000021));
#76210=CARTESIAN_POINT('Ctrl Pts',(-0.0939029519891339,0.263443268036106,
-0.040000000000002));
#76211=CARTESIAN_POINT('Ctrl Pts',(-0.102142100636434,0.261230327336921,
-0.0400000000000021));
#76212=CARTESIAN_POINT('Ctrl Pts',(-0.110284812020322,0.258657679335378,
-0.0400000000000021));
#76213=CARTESIAN_POINT('Ctrl Pts',(-0.11652245142853,0.256686929077716,
-0.040000000000002));
#76214=CARTESIAN_POINT('Ctrl Pts',(-0.122706184972723,0.254503953011045,
-0.0400000000000007));
#76215=CARTESIAN_POINT('Ctrl Pts',(-0.128815207409699,0.252114660253398,
-0.0400000000000013));
#76216=CARTESIAN_POINT('Ctrl Pts',(-0.135399388890598,0.24953952858714,
-0.0400000000000019));
#76217=CARTESIAN_POINT('Ctrl Pts',(-0.141881668799996,0.246730834774574,
-0.0400000000000011));
#76218=CARTESIAN_POINT('Ctrl Pts',(-0.148245421000419,0.243696854595293,
-0.0400000000000011));
#76219=CARTESIAN_POINT('Ctrl Pts',(-0.16393852661808,0.236215015281659,
-0.0400000000000013));
#76220=CARTESIAN_POINT('Ctrl Pts',(-0.178918800966714,0.227363679838949,
-0.0399999999999997));
#76221=CARTESIAN_POINT('Ctrl Pts',(-0.192978433199048,0.217213213525256,
-0.0399999999999996));
#76222=CARTESIAN_POINT('Ctrl Pts',(-0.203047642906921,0.209943665342464,
-0.0399999999999995));
#76223=CARTESIAN_POINT('Ctrl Pts',(-0.212644773119861,0.202006682473912,
-0.0399999999999999));
#76224=CARTESIAN_POINT('Ctrl Pts',(-0.221686865784453,0.193412961144454,
-0.04));
#76225=CARTESIAN_POINT('Ctrl Pts',(-0.103676804647749,0.212843510916694,
-1.99397142723206));
#76226=CARTESIAN_POINT('Ctrl Pts',(-0.174500313671441,0.178346644274193,
-1.98867562368504));
#76227=CARTESIAN_POINT('Ctrl Pts',(-0.277757662224097,0.0337041756151036,
-1.97808517678002));
#76228=CARTESIAN_POINT('Ctrl Pts',(-0.178659324738769,-0.215666118176939,
-1.96220008651701));
#76229=CARTESIAN_POINT('Ctrl Pts',(0.0843322378632243,-0.266777789429326,
-1.94631615644302));
#76230=CARTESIAN_POINT('Ctrl Pts',(0.269948356849218,-0.0738434778211555,
-1.93043222636904));
#76231=CARTESIAN_POINT('Ctrl Pts',(0.208339268208791,0.18691124507345,-1.91454829629505));
#76232=CARTESIAN_POINT('Ctrl Pts',(-0.0441543487728196,0.276352467078339,
-1.89866436622106));
#76233=CARTESIAN_POINT('Ctrl Pts',(-0.256182511614628,0.112686240256283,
-1.88278043614707));
#76234=CARTESIAN_POINT('Ctrl Pts',(-0.233541289554458,-0.154232428936108,
-1.86689650607308));
#76235=CARTESIAN_POINT('Ctrl Pts',(0.00304250668361687,-0.279851820056704,
-1.8510125759991));
#76236=CARTESIAN_POINT('Ctrl Pts',(0.236836682863679,-0.149117080380604,
-1.8351286459251));
#76237=CARTESIAN_POINT('Ctrl Pts',(0.253675595533036,0.118221431597056,
-1.81924471585112));
#76238=CARTESIAN_POINT('Ctrl Pts',(0.0381317971162815,0.277260151070568,
-1.80336078577713));
#76239=CARTESIAN_POINT('Ctrl Pts',(-0.212342650053903,0.182312969274217,
-1.78747685570314));
#76240=CARTESIAN_POINT('Ctrl Pts',(-0.268298711511727,-0.0796443191042248,
-1.77159292562915));
#76241=CARTESIAN_POINT('Ctrl Pts',(-0.0784770000832964,-0.268642374478244,
-1.75570899555517));
#76242=CARTESIAN_POINT('Ctrl Pts',(0.183234287828566,-0.21154808143558,
-1.73982506548118));
#76243=CARTESIAN_POINT('Ctrl Pts',(0.277092030570221,0.0393369872510852,
-1.72394113540719));
#76244=CARTESIAN_POINT('Ctrl Pts',(0.117116878322258,0.254186982850244,
-1.7080572053332));
#76245=CARTESIAN_POINT('Ctrl Pts',(-0.150144335198661,0.236186512280278,
-1.69217327525921));
#76246=CARTESIAN_POINT('Ctrl Pts',(-0.279864357098656,0.00182505268549074,
-1.67628934518523));
#76247=CARTESIAN_POINT('Ctrl Pts',(-0.153211879123455,-0.234208258795446,
-1.66040541511124));
#76248=CARTESIAN_POINT('Ctrl Pts',(0.113791847079068,-0.255692793405017,
-1.64452148503725));
#76249=CARTESIAN_POINT('Ctrl Pts',(0.27655543274757,-0.0429474273786092,
-1.62863755496326));
#76250=CARTESIAN_POINT('Ctrl Pts',(0.185977692986568,0.209140351247083,
-1.61275362488927));
#76251=CARTESIAN_POINT('Ctrl Pts',(-0.0749667420769754,0.269643053845345,
-1.59686969481528));
#76252=CARTESIAN_POINT('Ctrl Pts',(-0.26723715555904,0.0831365837885122,
-1.5809857647413));
#76253=CARTESIAN_POINT('Ctrl Pts',(-0.214702343360205,-0.179527971695799,
-1.56510183466731));
#76254=CARTESIAN_POINT('Ctrl Pts',(0.0345126628622819,-0.277734162431102,
-1.54921790459332));
#76255=CARTESIAN_POINT('Ctrl Pts',(0.252112004718534,-0.121519241072826,
-1.53333397451933));
#76256=CARTESIAN_POINT('Ctrl Pts',(0.238761664170276,0.146014576655516,
-1.51745004444534));
#76257=CARTESIAN_POINT('Ctrl Pts',(0.00669135203703449,0.279790304841033,
-1.50156611437136));
#76258=CARTESIAN_POINT('Ctrl Pts',(-0.231508638966162,0.157261371475424,
-1.48568218429737));
#76259=CARTESIAN_POINT('Ctrl Pts',(-0.257632863479559,-0.109328388488873,
-1.46979825422338));
#76260=CARTESIAN_POINT('Ctrl Pts',(-0.0477499686083177,-0.275766802520549,
-1.45391432414939));
#76261=CARTESIAN_POINT('Ctrl Pts',(0.205874754808538,-0.189586323892037,
-1.4380303940754));
#76262=CARTESIAN_POINT('Ctrl Pts',(0.270905883525229,0.0702665720367265,
-1.42214646400142));
#76263=CARTESIAN_POINT('Ctrl Pts',(0.0877710122536518,0.265751083313652,
-1.40626253392743));
#76264=CARTESIAN_POINT('Ctrl Pts',(-0.175767358353134,0.217791700052944,
-1.39037860385344));
#76265=CARTESIAN_POINT('Ctrl Pts',(-0.278292311003068,-0.0296779128471706,
-1.37449467377945));
#76266=CARTESIAN_POINT('Ctrl Pts',(-0.125884854100124,-0.249960781689022,
-1.35861074370546));
#76267=CARTESIAN_POINT('Ctrl Pts',(0.141840661955398,-0.241264617153963,
-1.34272681363148));
#76268=CARTESIAN_POINT('Ctrl Pts',(0.27963164408674,-0.0115556263240567,
-1.32684288355749));
#76269=CARTESIAN_POINT('Ctrl Pts',(0.161263307416486,0.228739009693342,
-1.3109589534835));
#76270=CARTESIAN_POINT('Ctrl Pts',(-0.10483186864783,0.259495025366958,
-1.29507502340951));
#76271=CARTESIAN_POINT('Ctrl Pts',(-0.274894780018969,0.0525380699371205,
-1.27919109333552));
#76272=CARTESIAN_POINT('Ctrl Pts',(-0.193137623522783,-0.202546901369451,
-1.26330716326153));
#76273=CARTESIAN_POINT('Ctrl Pts',(0.0655451532412157,-0.272086790860894,
-1.24742323318755));
#76274=CARTESIAN_POINT('Ctrl Pts',(0.264184647493857,-0.0923788985804749,
-1.23153930311356));
#76275=CARTESIAN_POINT('Ctrl Pts',(0.220815196153506,0.171953592640814,
-1.21565537303957));
#76276=CARTESIAN_POINT('Ctrl Pts',(-0.0248341881767495,0.278766303508864,
-1.19977144296558));
#76277=CARTESIAN_POINT('Ctrl Pts',(-0.247733970089428,0.130212399325583,
-1.18388751289159));
#76278=CARTESIAN_POINT('Ctrl Pts',(-0.24369461130014,-0.137623854391846,
-1.16800358281761));
#76279=CARTESIAN_POINT('Ctrl Pts',(-0.0164164061701999,-0.279388422241956,
-1.15211965274362));
#76280=CARTESIAN_POINT('Ctrl Pts',(0.225900209349461,-0.165216477054391,
-1.13623572266963));
#76281=CARTESIAN_POINT('Ctrl Pts',(0.261278715510704,0.10030364746843,-1.12035179259564));
#76282=CARTESIAN_POINT('Ctrl Pts',(0.0573102836629663,0.273939628861662,
-1.10446786252165));
#76283=CARTESIAN_POINT('Ctrl Pts',(-0.199157797397855,0.196630518002749,
-1.08858393244767));
#76284=CARTESIAN_POINT('Ctrl Pts',(-0.273185418681399,-0.0608039134781932,
-1.07270000237368));
#76285=CARTESIAN_POINT('Ctrl Pts',(-0.0969588493689412,-0.262538321780736,
-1.05681607229969));
#76286=CARTESIAN_POINT('Ctrl Pts',(0.168087827865316,-0.223771917357639,
-1.0409321422257));
#76287=CARTESIAN_POINT('Ctrl Pts',(0.279155996603362,0.019982953604956,
-1.02504821215171));
#76288=CARTESIAN_POINT('Ctrl Pts',(0.134500568096756,0.245432243309726,
-1.00916428207772));
#76289=CARTESIAN_POINT('Ctrl Pts',(-0.133365429137207,0.246050911775273,
-0.993280352003735));
#76290=CARTESIAN_POINT('Ctrl Pts',(-0.279060712856098,0.0212722216667855,
-0.977396421929748));
#76291=CARTESIAN_POINT('Ctrl Pts',(-0.169119684944492,-0.2229930963924,
-0.961512491855758));
#76292=CARTESIAN_POINT('Ctrl Pts',(0.0957450942929234,-0.262983394519946,
-0.945628561781772));
#76293=CARTESIAN_POINT('Ctrl Pts',(0.272901637887803,-0.062065166660125,
-0.929744631707783));
#76294=CARTESIAN_POINT('Ctrl Pts',(0.200063951074714,0.195708467764605,
-0.913860701633795));
#76295=CARTESIAN_POINT('Ctrl Pts',(-0.0560442865067918,0.274201434759812,
-0.897976771559806));
#76296=CARTESIAN_POINT('Ctrl Pts',(-0.260812604026003,0.101509479634023,
-0.88209284148582));
#76297=CARTESIAN_POINT('Ctrl Pts',(-0.226660969547766,-0.164171233040571,
-0.86620891141183));
#76298=CARTESIAN_POINT('Ctrl Pts',(0.0151256761535035,-0.279461272442701,
-0.850324981337842));
#76299=CARTESIAN_POINT('Ctrl Pts',(0.243056297396063,-0.138748063664006,
-0.834441051263854));
#76300=CARTESIAN_POINT('Ctrl Pts',(0.248332806030034,0.129066673946625,
-0.818557121189867));
#76301=CARTESIAN_POINT('Ctrl Pts',(0.0261216044068271,0.27864861502905,
-0.802673191115877));
#76302=CARTESIAN_POINT('Ctrl Pts',(-0.220018549938132,0.172971750749988,
-0.786789261041891));
#76303=CARTESIAN_POINT('Ctrl Pts',(-0.264608546896811,-0.0911575876356607,
-0.770905330967901));
#76304=CARTESIAN_POINT('Ctrl Pts',(-0.0668012810437667,-0.271781120987654,
-0.755021400893914));
#76305=CARTESIAN_POINT('Ctrl Pts',(0.192199955552935,-0.203436884462588,
-0.739137470819925));
#76306=CARTESIAN_POINT('Ctrl Pts',(0.275134531851118,0.0512677116464285,
-0.723253540745937));
#76307=CARTESIAN_POINT('Ctrl Pts',(0.106029413257268,0.259008016089684,
-0.70736961067195));
#76308=CARTESIAN_POINT('Ctrl Pts',(-0.160204992551617,0.229481479069509,
-0.69148568059796));
#76309=CARTESIAN_POINT('Ctrl Pts',(-0.279682038710943,-0.0102638246714771,
-0.675601750523973));
#76310=CARTESIAN_POINT('Ctrl Pts',(-0.142953601577338,-0.240606850838584,
-0.659717820449986));
#76311=CARTESIAN_POINT('Ctrl Pts',(0.124728888771074,-0.25053960401566,
-0.643833890375996));
#76312=CARTESIAN_POINT('Ctrl Pts',(0.278152253379934,-0.0309630879286156,
-0.627949960302009));
#76313=CARTESIAN_POINT('Ctrl Pts',(0.176771509599478,0.216977469494643,
-0.612066030228021));
#76314=CARTESIAN_POINT('Ctrl Pts',(-0.0865425147664667,0.266153681192405,
-0.596182100154032));
#76315=CARTESIAN_POINT('Ctrl Pts',(-0.270578417007657,0.071517194604748,
-0.580298170080044));
#76316=CARTESIAN_POINT('Ctrl Pts',(-0.206748298185121,-0.188633321743026,
-0.564414240006056));
#76317=CARTESIAN_POINT('Ctrl Pts',(0.0464756333408657,-0.275984427785086,
-0.548530309932067));
#76318=CARTESIAN_POINT('Ctrl Pts',(0.25712510368365,-0.110517283403066,
-0.53264637985808));
#76319=CARTESIAN_POINT('Ctrl Pts',(0.232232592993323,0.156190305796638,
-0.516762449784092));
#76320=CARTESIAN_POINT('Ctrl Pts',(-0.00539886938617793,0.279818228647572,
-0.500878519710104));
#76321=CARTESIAN_POINT('Ctrl Pts',(-0.238084644363667,0.147115910075619,
-0.484994589636116));
#76322=CARTESIAN_POINT('Ctrl Pts',(-0.25267063837447,-0.1203533853658,-0.469110659562128));
#76323=CARTESIAN_POINT('Ctrl Pts',(-0.0357952081938611,-0.277571778006463,
-0.453226729488138));
#76324=CARTESIAN_POINT('Ctrl Pts',(0.21387077475615,-0.180517812444876,
-0.437342799414151));
#76325=CARTESIAN_POINT('Ctrl Pts',(0.267618330028949,0.0819012713019475,
-0.421458869340163));
#76326=CARTESIAN_POINT('Ctrl Pts',(0.0762114814842632,0.269293889627319,
-0.405574939266175));
#76327=CARTESIAN_POINT('Ctrl Pts',(-0.185009645352496,0.20999719090376,
-0.389691009192186));
#76328=CARTESIAN_POINT('Ctrl Pts',(-0.276750864670533,-0.0416695007967132,
-0.373807079118198));
#76329=CARTESIAN_POINT('Ctrl Pts',(-0.114971734614638,-0.255164436062807,
-0.357923149044211));
#76330=CARTESIAN_POINT('Ctrl Pts',(0.152128390037859,-0.234913479646994,
-0.342039218970221));
#76331=CARTESIAN_POINT('Ctrl Pts',(0.279869794930341,0.000532281982961198,
-0.326155288896234));
#76332=CARTESIAN_POINT('Ctrl Pts',(0.151233742192331,0.235490439708333,
-0.310271358822245));
#76333=CARTESIAN_POINT('Ctrl Pts',(-0.115941509278813,0.254725266554512,
-0.294387428748259));
#76334=CARTESIAN_POINT('Ctrl Pts',(-0.276907321688116,0.0406165003772714,
-0.27850349867427));
#76335=CARTESIAN_POINT('Ctrl Pts',(-0.184209608056035,-0.210699398348146,
-0.262619568600281));
#76336=CARTESIAN_POINT('Ctrl Pts',(0.0772354167140077,-0.269002063565523,
-0.246735638526293));
#76337=CARTESIAN_POINT('Ctrl Pts',(0.267927629451405,-0.0808826971579307,
-0.230851708452305));
#76338=CARTESIAN_POINT('Ctrl Pts',(0.213183148962925,0.18132997451097,-0.214967778378317));
#76339=CARTESIAN_POINT('Ctrl Pts',(-0.0368518537260703,0.277433701788479,
-0.199083848304329));
#76340=CARTESIAN_POINT('Ctrl Pts',(-0.253124531452511,0.119391245964334,
-0.183199918230341));
#76341=CARTESIAN_POINT('Ctrl Pts',(-0.237527290585313,-0.148020141499362,
-0.167315988156352));
#76342=CARTESIAN_POINT('Ctrl Pts',(-0.00432689865297213,-0.279837356241662,
-0.151432058082364));
#76343=CARTESIAN_POINT('Ctrl Pts',(0.232810568914152,-0.155304641198214,
-0.135548128008376));
#76344=CARTESIAN_POINT('Ctrl Pts',(0.256730473028442,0.111492279693591,
-0.119664197934388));
#76345=CARTESIAN_POINT('Ctrl Pts',(0.0453727461737449,0.276163517661131,
-0.1037802678604));
#76346=CARTESIAN_POINT('Ctrl Pts',(-0.207363196613034,0.187837216669757,
-0.0878963377864122));
#76347=CARTESIAN_POINT('Ctrl Pts',(-0.270500560251008,-0.0725291372450606,
-0.0720124077124241));
#76348=CARTESIAN_POINT('Ctrl Pts',(-0.0850981096593689,-0.266552231679603,
-0.0561258829081893));
#76349=CARTESIAN_POINT('Ctrl Pts',(0.0894476313883584,-0.232940382224155,
-0.0455340014619504));
#76350=CARTESIAN_POINT('Ctrl Pts',(0.150323359639724,-0.182904692841898,
-0.0402367633737074));
#76351=CARTESIAN_POINT('Ctrl Pts',(-0.112118529268456,0.230173966967767,
-1.98284177580134));
#76352=CARTESIAN_POINT('Ctrl Pts',(-0.188708733763536,0.192868245929506,
-1.97754597225432));
#76353=CARTESIAN_POINT('Ctrl Pts',(-0.300373653368441,0.0364484863611533,
-1.9669555253493));
#76354=CARTESIAN_POINT('Ctrl Pts',(-0.193206385920782,-0.233226400690007,
-1.95107043508629));
#76355=CARTESIAN_POINT('Ctrl Pts',(0.0911988608374564,-0.288499761291163,
-1.9351865050123));
#76356=CARTESIAN_POINT('Ctrl Pts',(0.291928487294752,-0.0798560696146595,
-1.91930257493831));
#76357=CARTESIAN_POINT('Ctrl Pts',(0.225302973213726,0.202130206197729,
-1.90341864486432));
#76358=CARTESIAN_POINT('Ctrl Pts',(-0.0477495488217895,0.298854042365646,
-1.88753471479033));
#76359=CARTESIAN_POINT('Ctrl Pts',(-0.277041779249657,0.121861544337256,
-1.87165078471634));
#76360=CARTESIAN_POINT('Ctrl Pts',(-0.252557030449273,-0.166790567635357,
-1.85576685464236));
#76361=CARTESIAN_POINT('Ctrl Pts',(0.00329023811850059,-0.302638324786948,
-1.83988292456837));
#76362=CARTESIAN_POINT('Ctrl Pts',(0.256120746098554,-0.16125870967844,
-1.82399899449438));
#76363=CARTESIAN_POINT('Ctrl Pts',(0.274330741375541,0.127847430133554,
-1.80811506442039));
#76364=CARTESIAN_POINT('Ctrl Pts',(0.041236620144366,0.299835633133174,
-1.7922311343464));
#76365=CARTESIAN_POINT('Ctrl Pts',(-0.229632324278302,0.197157522852288,
-1.77634720427242));
#76366=CARTESIAN_POINT('Ctrl Pts',(-0.29014452211872,-0.0861292354918946,
-1.76046327419843));
#76367=CARTESIAN_POINT('Ctrl Pts',(-0.0848668693121321,-0.290516167314583,
-1.74457934412444));
#76368=CARTESIAN_POINT('Ctrl Pts',(0.198153858355219,-0.228773059130311,
-1.72869541405045));
#76369=CARTESIAN_POINT('Ctrl Pts',(0.29965382367924,0.0425399410352991,
-1.71281148397646));
#76370=CARTESIAN_POINT('Ctrl Pts',(0.126652940304422,0.274883767619805,
-1.69692755390248));
#76371=CARTESIAN_POINT('Ctrl Pts',(-0.162369607142684,0.255417636373752,
-1.68104362382849));
#76372=CARTESIAN_POINT('Ctrl Pts',(-0.302651882638292,0.00197365479800523,
-1.6651596937545));
#76373=CARTESIAN_POINT('Ctrl Pts',(-0.165686921121286,-0.253278306636561,
-1.64927576368051));
#76374=CARTESIAN_POINT('Ctrl Pts',(0.123057173497901,-0.276512186486802,
-1.63339183360652));
#76375=CARTESIAN_POINT('Ctrl Pts',(0.299073534202835,-0.0464443557063105,
-1.61750790353254));
#76376=CARTESIAN_POINT('Ctrl Pts',(0.201120641065663,0.226169283208327,
-1.60162397345855));
#76377=CARTESIAN_POINT('Ctrl Pts',(-0.081070793937711,0.291598325462588,
-1.58574004338456));
#76378=CARTESIAN_POINT('Ctrl Pts',(-0.288996530602623,0.0899058524656643,
-1.56985611331057));
#76379=CARTESIAN_POINT('Ctrl Pts',(-0.232184151988719,-0.194145761122461,
-1.55397218323658));
#76380=CARTESIAN_POINT('Ctrl Pts',(0.0373228034409807,-0.300348240140887,
-1.5380882531626));
#76381=CARTESIAN_POINT('Ctrl Pts',(0.27263983757989,-0.131413758682043,
-1.52220432308861));
#76382=CARTESIAN_POINT('Ctrl Pts',(0.258202466052199,0.157903589351488,
-1.50632039301462));
#76383=CARTESIAN_POINT('Ctrl Pts',(0.00723618510195202,0.302571800789299,
-1.49043646294063));
#76384=CARTESIAN_POINT('Ctrl Pts',(-0.250358874407996,0.170066137169941,
-1.47455253286664));
#76385=CARTESIAN_POINT('Ctrl Pts',(-0.278610223788148,-0.118230284645726,
-1.45866860279265));
#76386=CARTESIAN_POINT('Ctrl Pts',(-0.0516379364812537,-0.298220690970535,
-1.44278467271867));
#76387=CARTESIAN_POINT('Ctrl Pts',(0.222637790594162,-0.205023099201488,
-1.42690074264468));
#76388=CARTESIAN_POINT('Ctrl Pts',(0.292963979110057,0.075987919769137,
-1.41101681257069));
#76389=CARTESIAN_POINT('Ctrl Pts',(0.094917632152324,0.287389457206547,
-1.3951328824967));
#76390=CARTESIAN_POINT('Ctrl Pts',(-0.190078945612864,0.235525054806396,
-1.37924895242271));
#76391=CARTESIAN_POINT('Ctrl Pts',(-0.300951835103278,-0.0320943913297411,
-1.36336502234873));
#76392=CARTESIAN_POINT('Ctrl Pts',(-0.136134835046605,-0.270313454518445,
-1.34748109227474));
#76393=CARTESIAN_POINT('Ctrl Pts',(0.15338982005604,-0.260909218139248,
-1.33159716220075));
#76394=CARTESIAN_POINT('Ctrl Pts',(0.302400221326715,-0.0124965254536081,
-1.31571323212676));
#76395=CARTESIAN_POINT('Ctrl Pts',(0.174393924599955,0.247363732324456,
-1.29982930205277));
#76396=CARTESIAN_POINT('Ctrl Pts',(-0.113367642581119,0.280624009347843,
-1.28394537197879));
#76397=CARTESIAN_POINT('Ctrl Pts',(-0.297277665375771,0.0568159016085323,
-1.2680614419048));
#76398=CARTESIAN_POINT('Ctrl Pts',(-0.208863557951579,-0.21903897179878,
-1.25217751183081));
#76399=CARTESIAN_POINT('Ctrl Pts',(0.0708820666980315,-0.294241040012223,
-1.23629358175682));
#76400=CARTESIAN_POINT('Ctrl Pts',(0.285695476755416,-0.0999007085478101,
-1.22040965168283));
#76401=CARTESIAN_POINT('Ctrl Pts',(0.23879473443431,0.18595464988353,-1.20452572160884));
#76402=CARTESIAN_POINT('Ctrl Pts',(-0.0268562738156637,0.301464421721033,
-1.18864179153486));
#76403=CARTESIAN_POINT('Ctrl Pts',(-0.267905328203665,0.140814743997017,
-1.17275786146087));
#76404=CARTESIAN_POINT('Ctrl Pts',(-0.263537070827475,-0.148829665411615,
-1.15687393138688));
#76405=CARTESIAN_POINT('Ctrl Pts',(-0.0177530868349023,-0.302137195516692,
-1.14099000131289));
#76406=CARTESIAN_POINT('Ctrl Pts',(0.244293787021608,-0.178668975005457,
-1.1251060712389));
#76407=CARTESIAN_POINT('Ctrl Pts',(0.282552933722652,0.108470717945358,
-1.10922214116491));
#76408=CARTESIAN_POINT('Ctrl Pts',(0.0619766855091786,0.296244742502134,
-1.09333821109093));
#76409=CARTESIAN_POINT('Ctrl Pts',(-0.215373915240332,0.212640856001168,
-1.07745428101694));
#76410=CARTESIAN_POINT('Ctrl Pts',(-0.295429121916048,-0.0657547787675702,
-1.06157035094295));
#76411=CARTESIAN_POINT('Ctrl Pts',(-0.104853574796624,-0.283915101499071,
-1.04568642086896));
#76412=CARTESIAN_POINT('Ctrl Pts',(0.181774121147142,-0.241992202122388,
-1.02980249079498));
#76413=CARTESIAN_POINT('Ctrl Pts',(0.30188584497737,0.0216100349180264,
-1.01391856072098));
#76414=CARTESIAN_POINT('Ctrl Pts',(0.145452070325817,0.265416186855271,
-0.998034630647006));
#76415=CARTESIAN_POINT('Ctrl Pts',(-0.144224504419512,0.266085229450651,
-0.982150700573014));
#76416=CARTESIAN_POINT('Ctrl Pts',(-0.301782802897294,0.0230042796520985,
-0.966266770499029));
#76417=CARTESIAN_POINT('Ctrl Pts',(-0.182889995604558,-0.241149966855945,
-0.950382840425037));
#76418=CARTESIAN_POINT('Ctrl Pts',(0.103540991577281,-0.284396413602654,
-0.934498910351052));
#76419=CARTESIAN_POINT('Ctrl Pts',(0.295122234707084,-0.0671187275531662,
-0.918614980277062));
#76420=CARTESIAN_POINT('Ctrl Pts',(0.216353851088915,0.211643729238206,
-0.902731050203075));
#76421=CARTESIAN_POINT('Ctrl Pts',(-0.0606076064785213,0.296527865543533,
-0.886847120129086));
#76422=CARTESIAN_POINT('Ctrl Pts',(-0.28204886982603,0.10977473314346,-0.870963190055099));
#76423=CARTESIAN_POINT('Ctrl Pts',(-0.245116490950899,-0.177538623602801,
-0.85507925998111));
#76424=CARTESIAN_POINT('Ctrl Pts',(0.0163572611085327,-0.30221597743317,
-0.839195329907123));
#76425=CARTESIAN_POINT('Ctrl Pts',(0.262846783193899,-0.15004541169752,
-0.823311399833134));
#76426=CARTESIAN_POINT('Ctrl Pts',(0.268552923441213,0.139575729688357,
-0.807427469759146));
#76427=CARTESIAN_POINT('Ctrl Pts',(0.0282485159354271,0.301337150637463,
-0.791543539685159));
#76428=CARTESIAN_POINT('Ctrl Pts',(-0.237933222524112,0.187055709953346,
-0.77565960961117));
#76429=CARTESIAN_POINT('Ctrl Pts',(-0.286153891516353,-0.0985799542346567,
-0.759775679537182));
#76430=CARTESIAN_POINT('Ctrl Pts',(-0.0722404727781009,-0.293910481438916,
-0.743891749463194));
#76431=CARTESIAN_POINT('Ctrl Pts',(0.20784954180709,-0.220001420398691,
-0.728007819389205));
#76432=CARTESIAN_POINT('Ctrl Pts',(0.29753693863271,0.0554421063446759,
-0.712123889315217));
#76433=CARTESIAN_POINT('Ctrl Pts',(0.114662695421532,0.280097346087977,
-0.696239959241229));
#76434=CARTESIAN_POINT('Ctrl Pts',(-0.173249438072272,0.248166656129505,
-0.680356029167241));
#76435=CARTESIAN_POINT('Ctrl Pts',(-0.302454719255812,-0.0110995408350489,
-0.664472099093253));
#76436=CARTESIAN_POINT('Ctrl Pts',(-0.154593379077758,-0.260197894211651,
-0.648588169019265));
#76437=CARTESIAN_POINT('Ctrl Pts',(0.13488474701564,-0.270939406564237,
-0.632704238945277));
#76438=CARTESIAN_POINT('Ctrl Pts',(0.30080037350324,-0.0334842098187864,
-0.616820308871289));
#76439=CARTESIAN_POINT('Ctrl Pts',(0.191164858332551,0.234644526775151,
-0.600936378797301));
#76440=CARTESIAN_POINT('Ctrl Pts',(-0.0935891061436223,0.287824835999382,
-0.585052448723312));
#76441=CARTESIAN_POINT('Ctrl Pts',(-0.292609849134122,0.0773403723594089,
-0.569168518649325));
#76442=CARTESIAN_POINT('Ctrl Pts',(-0.223582460898843,-0.203992500315843,
-0.553284588575336));
#76443=CARTESIAN_POINT('Ctrl Pts',(0.0502598404214115,-0.298456036038071,
-0.537400658501348));
#76444=CARTESIAN_POINT('Ctrl Pts',(0.278061120430529,-0.119515983502741,
-0.52151672842736));
#76445=CARTESIAN_POINT('Ctrl Pts',(0.251141775280176,0.168907861612897,
-0.505632798353372));
#76446=CARTESIAN_POINT('Ctrl Pts',(-0.00583846403587734,0.302601998248909,
-0.489748868279384));
#76447=CARTESIAN_POINT('Ctrl Pts',(-0.257470320947409,0.159094597154208,
-0.473864938205395));
#76448=CARTESIAN_POINT('Ctrl Pts',(-0.27324395712347,-0.130152974964262,
-0.457981008131408));
#76449=CARTESIAN_POINT('Ctrl Pts',(-0.038709778056815,-0.300172633813816,
-0.442097078057419));
#76450=CARTESIAN_POINT('Ctrl Pts',(0.231284874187964,-0.195216198134616,
-0.426213147983432));
#76451=CARTESIAN_POINT('Ctrl Pts',(0.289408741618445,0.0885699565567235,
-0.410329217909442));
#76452=CARTESIAN_POINT('Ctrl Pts',(0.0824168843399205,0.291220731084257,
-0.394445287835456));
#76453=CARTESIAN_POINT('Ctrl Pts',(-0.20007377163944,0.22709588971836,-0.378561357761467));
#76454=CARTESIAN_POINT('Ctrl Pts',(-0.299284878870036,-0.0450623759147606,
-0.362677427687479));
#76455=CARTESIAN_POINT('Ctrl Pts',(-0.124333131564319,-0.275940808459303,
-0.34679349761349));
#76456=CARTESIAN_POINT('Ctrl Pts',(0.164515210600611,-0.254040949013069,
-0.330909567539503));
#76457=CARTESIAN_POINT('Ctrl Pts',(0.302657763237072,0.000575622226092337,
-0.315025637465514));
#76458=CARTESIAN_POINT('Ctrl Pts',(0.163547717428012,0.254664887161466,
-0.299141707391526));
#76459=CARTESIAN_POINT('Ctrl Pts',(-0.125381868641413,0.27546588024815,
-0.283257777317538));
#76460=CARTESIAN_POINT('Ctrl Pts',(-0.299454075160033,0.0439236365530725,
-0.26737384724355));
#76461=CARTESIAN_POINT('Ctrl Pts',(-0.19920859253459,-0.227855273325648,
-0.251489917169562));
#76462=CARTESIAN_POINT('Ctrl Pts',(0.08352419192347,-0.290905143533485,
-0.235605987095574));
#76463=CARTESIAN_POINT('Ctrl Pts',(0.289743225271439,-0.0874684465770746,
-0.219722057021586));
#76464=CARTESIAN_POINT('Ctrl Pts',(0.230541259520392,0.196094489249849,
-0.203838126947598));
#76465=CARTESIAN_POINT('Ctrl Pts',(-0.0398524593289804,0.300023314951801,
-0.18795419687361));
#76466=CARTESIAN_POINT('Ctrl Pts',(-0.273734807748427,0.129112494839419,
-0.172070266799621));
#76467=CARTESIAN_POINT('Ctrl Pts',(-0.256867585493483,-0.160072454233161,
-0.156186336725633));
#76468=CARTESIAN_POINT('Ctrl Pts',(-0.00467920973175626,-0.302622683277977,
-0.140302406651645));
#76469=CARTESIAN_POINT('Ctrl Pts',(0.251766812002862,-0.167950083134505,
-0.124418476577657));
#76470=CARTESIAN_POINT('Ctrl Pts',(0.277634357580187,0.120570367369091,
-0.108534546503669));
#76471=CARTESIAN_POINT('Ctrl Pts',(0.0490671523602165,0.298649708032275,
-0.0926506164296805));
#76472=CARTESIAN_POINT('Ctrl Pts',(-0.224247426487058,0.203131573609421,
-0.0767666863556922));
#76473=CARTESIAN_POINT('Ctrl Pts',(-0.292525653010615,-0.078434710875347,
-0.0608827562817043));
#76474=CARTESIAN_POINT('Ctrl Pts',(-0.0920270925685949,-0.288255837848017,
-0.0449962314774693));
#76475=CARTESIAN_POINT('Ctrl Pts',(0.0967307674255891,-0.251907195162304,
-0.0344043500312305));
#76476=CARTESIAN_POINT('Ctrl Pts',(0.162563208373966,-0.197797426602863,
-0.0291071119429875));
#76477=CARTESIAN_POINT('Ctrl Pts',(-0.120560253889163,0.247504423018841,
-1.97171212437062));
#76478=CARTESIAN_POINT('Ctrl Pts',(-0.202917153855632,0.207389847584819,
-1.9664163208236));
#76479=CARTESIAN_POINT('Ctrl Pts',(-0.322989644512786,0.0391927971072032,
-1.95582587391858));
#76480=CARTESIAN_POINT('Ctrl Pts',(-0.207753447102797,-0.250786683203076,
-1.93994078365557));
#76481=CARTESIAN_POINT('Ctrl Pts',(0.0980654838116881,-0.310221733153001,
-1.92405685358158));
#76482=CARTESIAN_POINT('Ctrl Pts',(0.313908617740286,-0.0858686614081634,
-1.90817292350759));
#76483=CARTESIAN_POINT('Ctrl Pts',(0.242266678218659,0.217349167322007,
-1.89228899343361));
#76484=CARTESIAN_POINT('Ctrl Pts',(-0.0513447488707591,0.321355617652953,
-1.87640506335962));
#76485=CARTESIAN_POINT('Ctrl Pts',(-0.297901046884685,0.131036848418228,
-1.86052113328563));
#76486=CARTESIAN_POINT('Ctrl Pts',(-0.271572771344087,-0.179348706334606,
-1.84463720321164));
#76487=CARTESIAN_POINT('Ctrl Pts',(0.00353796955338376,-0.325424829517193,
-1.82875327313765));
#76488=CARTESIAN_POINT('Ctrl Pts',(0.27540480933343,-0.173400338976277,
-1.81286934306366));
#76489=CARTESIAN_POINT('Ctrl Pts',(0.294985887218045,0.137473428670053,
-1.79698541298968));
#76490=CARTESIAN_POINT('Ctrl Pts',(0.0443414431724512,0.32241111519578,
-1.78110148291569));
#76491=CARTESIAN_POINT('Ctrl Pts',(-0.246921998502703,0.212002076430359,
-1.7652175528417));
#76492=CARTESIAN_POINT('Ctrl Pts',(-0.311990332725711,-0.0926141518795645,
-1.74933362276771));
#76493=CARTESIAN_POINT('Ctrl Pts',(-0.0912567385409681,-0.312389960150921,
-1.73344969269373));
#76494=CARTESIAN_POINT('Ctrl Pts',(0.213073428881872,-0.245998036825041,
-1.71756576261974));
#76495=CARTESIAN_POINT('Ctrl Pts',(0.322215616788258,0.0457428948195131,
-1.70168183254575));
#76496=CARTESIAN_POINT('Ctrl Pts',(0.136189002286588,0.295580552389366,
-1.68579790247176));
#76497=CARTESIAN_POINT('Ctrl Pts',(-0.174594879086708,0.274648760467226,
-1.66991397239777));
#76498=CARTESIAN_POINT('Ctrl Pts',(-0.325439408177928,0.00212225691052003,
-1.65403004232379));
#76499=CARTESIAN_POINT('Ctrl Pts',(-0.178161963119117,-0.272348354477677,
-1.63814611224979));
#76500=CARTESIAN_POINT('Ctrl Pts',(0.132322499916734,-0.297331579568586,
-1.62226218217581));
#76501=CARTESIAN_POINT('Ctrl Pts',(0.321591635658101,-0.0499412840340122,
-1.60637825210182));
#76502=CARTESIAN_POINT('Ctrl Pts',(0.216263589144758,0.243198215169573,
-1.59049432202783));
#76503=CARTESIAN_POINT('Ctrl Pts',(-0.087174845798447,0.313553597079832,
-1.57461039195384));
#76504=CARTESIAN_POINT('Ctrl Pts',(-0.310755905646206,0.0966751211428172,
-1.55872646187986));
#76505=CARTESIAN_POINT('Ctrl Pts',(-0.249665960617232,-0.208763550549125,
-1.54284253180586));
#76506=CARTESIAN_POINT('Ctrl Pts',(0.0401329440196797,-0.322962317850671,
-1.52695860173188));
#76507=CARTESIAN_POINT('Ctrl Pts',(0.293167670441246,-0.14130827629126,
-1.51107467165789));
#76508=CARTESIAN_POINT('Ctrl Pts',(0.27764326793412,0.169792602047461,-1.4951907415839));
#76509=CARTESIAN_POINT('Ctrl Pts',(0.00778101816686971,0.325353296737565,
-1.47930681150992));
#76510=CARTESIAN_POINT('Ctrl Pts',(-0.269209109849831,0.182870902864458,
-1.46342288143592));
#76511=CARTESIAN_POINT('Ctrl Pts',(-0.299587584096736,-0.12713218080258,
-1.44753895136194));
#76512=CARTESIAN_POINT('Ctrl Pts',(-0.0555259043541897,-0.320674579420522,
-1.43165502128795));
#76513=CARTESIAN_POINT('Ctrl Pts',(0.239400826379785,-0.220459874510939,
-1.41577109121396));
#76514=CARTESIAN_POINT('Ctrl Pts',(0.315022074694887,0.0817092675015477,
-1.39988716113997));
#76515=CARTESIAN_POINT('Ctrl Pts',(0.102064252050996,0.309027831099441,
-1.38400323106599));
#76516=CARTESIAN_POINT('Ctrl Pts',(-0.204390532872595,0.253258409559849,
-1.368119300992));
#76517=CARTESIAN_POINT('Ctrl Pts',(-0.323611359203487,-0.0345108698123119,
-1.35223537091801));
#76518=CARTESIAN_POINT('Ctrl Pts',(-0.146384815993087,-0.290666127347867,
-1.33635144084402));
#76519=CARTESIAN_POINT('Ctrl Pts',(0.164938978156682,-0.280553819124534,
-1.32046751077003));
#76520=CARTESIAN_POINT('Ctrl Pts',(0.32516879856669,-0.0134374245831591,
-1.30458358069605));
#76521=CARTESIAN_POINT('Ctrl Pts',(0.187524541783422,0.26598845495557,-1.28869965062206));
#76522=CARTESIAN_POINT('Ctrl Pts',(-0.12190341651441,0.301752993328728,
-1.27281572054807));
#76523=CARTESIAN_POINT('Ctrl Pts',(-0.319660550732573,0.0610937332799438,
-1.25693179047408));
#76524=CARTESIAN_POINT('Ctrl Pts',(-0.224589492380374,-0.235531042228108,
-1.24104786040009));
#76525=CARTESIAN_POINT('Ctrl Pts',(0.0762189801548472,-0.316395289163552,
-1.2251639303261));
#76526=CARTESIAN_POINT('Ctrl Pts',(0.307206306016977,-0.107422518515145,
-1.20928000025212));
#76527=CARTESIAN_POINT('Ctrl Pts',(0.256774272715115,0.199955707126246,
-1.19339607017813));
#76528=CARTESIAN_POINT('Ctrl Pts',(-0.0288783594545779,0.324162539933202,
-1.17751214010414));
#76529=CARTESIAN_POINT('Ctrl Pts',(-0.288076686317903,0.151417088668452,
-1.16162821003015));
#76530=CARTESIAN_POINT('Ctrl Pts',(-0.28337953035481,-0.160035476431385,
-1.14574427995616));
#76531=CARTESIAN_POINT('Ctrl Pts',(-0.0190897674996043,-0.324885968791427,
-1.12986034988218));
#76532=CARTESIAN_POINT('Ctrl Pts',(0.262687364693754,-0.192121472956523,
-1.11397641980818));
#76533=CARTESIAN_POINT('Ctrl Pts',(0.303827151934601,0.116637788422287,
-1.0980924897342));
#76534=CARTESIAN_POINT('Ctrl Pts',(0.0666430873553909,0.318549856142606,
-1.08220855966021));
#76535=CARTESIAN_POINT('Ctrl Pts',(-0.231590033082807,0.228651193999587,
-1.06632462958623));
#76536=CARTESIAN_POINT('Ctrl Pts',(-0.317672825150698,-0.0707056440569471,
-1.05044069951223));
#76537=CARTESIAN_POINT('Ctrl Pts',(-0.112748300224307,-0.305291881217406,
-1.03455676943825));
#76538=CARTESIAN_POINT('Ctrl Pts',(0.19546041442897,-0.260212486887136,
-1.01867283936426));
#76539=CARTESIAN_POINT('Ctrl Pts',(0.324615693351377,0.0232371162310966,
-1.00278890929027));
#76540=CARTESIAN_POINT('Ctrl Pts',(0.156403572554879,0.285400130400817,
-0.986904979216284));
#76541=CARTESIAN_POINT('Ctrl Pts',(-0.155083579701816,0.286119547126029,
-0.971021049142295));
#76542=CARTESIAN_POINT('Ctrl Pts',(-0.32450489293849,0.0247363376374115,
-0.955137119068307));
#76543=CARTESIAN_POINT('Ctrl Pts',(-0.196660306264625,-0.259306837319491,
-0.939253188994319));
#76544=CARTESIAN_POINT('Ctrl Pts',(0.111336888861641,-0.305809432685363,
-0.92336925892033));
#76545=CARTESIAN_POINT('Ctrl Pts',(0.317342831526365,-0.0721722884462076,
-0.907485328846344));
#76546=CARTESIAN_POINT('Ctrl Pts',(0.232643751103116,0.227578990711806,
-0.891601398772354));
#76547=CARTESIAN_POINT('Ctrl Pts',(-0.0651709264502512,0.318854296327255,
-0.875717468698368));
#76548=CARTESIAN_POINT('Ctrl Pts',(-0.303285135626059,0.118039986652897,
-0.859833538624378));
#76549=CARTESIAN_POINT('Ctrl Pts',(-0.263572012354034,-0.19090601416503,
-0.843949608550391));
#76550=CARTESIAN_POINT('Ctrl Pts',(0.017588846063562,-0.324970682423638,
-0.828065678476401));
#76551=CARTESIAN_POINT('Ctrl Pts',(0.282637268991736,-0.161342759731034,
-0.812181748402415));
#76552=CARTESIAN_POINT('Ctrl Pts',(0.288773040852392,0.15008478543009,-0.796297818328426));
#76553=CARTESIAN_POINT('Ctrl Pts',(0.0303754274640274,0.324025686245876,
-0.780413888254438));
#76554=CARTESIAN_POINT('Ctrl Pts',(-0.255847895110093,0.201139669156703,
-0.76452995818045));
#76555=CARTESIAN_POINT('Ctrl Pts',(-0.307699236135894,-0.106002320833652,
-0.748646028106462));
#76556=CARTESIAN_POINT('Ctrl Pts',(-0.0776796645124351,-0.316039841890178,
-0.732762098032473));
#76557=CARTESIAN_POINT('Ctrl Pts',(0.223499128061244,-0.236565956334796,
-0.716878167958486));
#76558=CARTESIAN_POINT('Ctrl Pts',(0.319939345414303,0.0596165010429236,
-0.700994237884497));
#76559=CARTESIAN_POINT('Ctrl Pts',(0.123295977585797,0.30118667608627,-0.68511030781051));
#76560=CARTESIAN_POINT('Ctrl Pts',(-0.186293883592927,0.2668518331895,-0.669226377736521));
#76561=CARTESIAN_POINT('Ctrl Pts',(-0.325227399800682,-0.011935256998621,
-0.653342447662532));
#76562=CARTESIAN_POINT('Ctrl Pts',(-0.16623315657818,-0.279788937584717,
-0.637458517588546));
#76563=CARTESIAN_POINT('Ctrl Pts',(0.145040605260206,-0.291339209112815,
-0.621574587514556));
#76564=CARTESIAN_POINT('Ctrl Pts',(0.323448493626547,-0.0360053317089568,
-0.605690657440569));
#76565=CARTESIAN_POINT('Ctrl Pts',(0.205558207065626,0.252311584055658,
-0.58980672736658));
#76566=CARTESIAN_POINT('Ctrl Pts',(-0.100635697520777,0.30949599080636,
-0.573922797292592));
#76567=CARTESIAN_POINT('Ctrl Pts',(-0.314641281260587,0.0831635501140697,
-0.558038867218604));
#76568=CARTESIAN_POINT('Ctrl Pts',(-0.240416623612565,-0.21935167888866,
-0.542154937144616));
#76569=CARTESIAN_POINT('Ctrl Pts',(0.0540440475019573,-0.320927644291056,
-0.526271007070628));
#76570=CARTESIAN_POINT('Ctrl Pts',(0.298997137177409,-0.128514683602414,
-0.51038707699664));
#76571=CARTESIAN_POINT('Ctrl Pts',(0.27005095756703,0.181625417429157,-0.494503146922652));
#76572=CARTESIAN_POINT('Ctrl Pts',(-0.00627805868557644,0.325385767850246,
-0.478619216848664));
#76573=CARTESIAN_POINT('Ctrl Pts',(-0.276855997531152,0.171073284232798,
-0.462735286774675));
#76574=CARTESIAN_POINT('Ctrl Pts',(-0.293817275872469,-0.139952564562724,
-0.446851356700688));
#76575=CARTESIAN_POINT('Ctrl Pts',(-0.0416243479197691,-0.322773489621168,
-0.430967426626699));
#76576=CARTESIAN_POINT('Ctrl Pts',(0.248698973619779,-0.209914583824356,
-0.415083496552711));
#76577=CARTESIAN_POINT('Ctrl Pts',(0.311199153207941,0.0952386418114992,
-0.399199566478723));
#76578=CARTESIAN_POINT('Ctrl Pts',(0.0886222871955774,0.313147572541195,
-0.383315636404735));
#76579=CARTESIAN_POINT('Ctrl Pts',(-0.215137897926383,0.24419458853296,
-0.367431706330747));
#76580=CARTESIAN_POINT('Ctrl Pts',(-0.32181889306954,-0.0484552510328077,
-0.351547776256759));
#76581=CARTESIAN_POINT('Ctrl Pts',(-0.133694528514001,-0.296717180855799,
-0.33566384618277));
#76582=CARTESIAN_POINT('Ctrl Pts',(0.176902031163362,-0.273168418379144,
-0.319779916108783));
#76583=CARTESIAN_POINT('Ctrl Pts',(0.325445731543802,0.000618962469223088,
-0.303895986034794));
#76584=CARTESIAN_POINT('Ctrl Pts',(0.175861692663694,0.2738393346146,-0.288012055960806));
#76585=CARTESIAN_POINT('Ctrl Pts',(-0.134822228004013,0.296206493941789,
-0.272128125886818));
#76586=CARTESIAN_POINT('Ctrl Pts',(-0.32200082863195,0.0472307727288739,
-0.25624419581283));
#76587=CARTESIAN_POINT('Ctrl Pts',(-0.214207577013145,-0.245011148303151,
-0.240360265738842));
#76588=CARTESIAN_POINT('Ctrl Pts',(0.0898129671329327,-0.312808223501447,
-0.224476335664854));
#76589=CARTESIAN_POINT('Ctrl Pts',(0.311558821091472,-0.0940541959962185,
-0.208592405590866));
#76590=CARTESIAN_POINT('Ctrl Pts',(0.247899370077859,0.210859003988727,
-0.192708475516877));
#76591=CARTESIAN_POINT('Ctrl Pts',(-0.0428530649318907,0.322612928115123,
-0.17682454544289));
#76592=CARTESIAN_POINT('Ctrl Pts',(-0.294345084044343,0.138833743714504,
-0.160940615368901));
#76593=CARTESIAN_POINT('Ctrl Pts',(-0.276207880401654,-0.17212476696696,
-0.145056685294913));
#76594=CARTESIAN_POINT('Ctrl Pts',(-0.00503152081054036,-0.325408010314291,
-0.129172755220925));
#76595=CARTESIAN_POINT('Ctrl Pts',(0.270723055091573,-0.180595525070797,
-0.113288825146937));
#76596=CARTESIAN_POINT('Ctrl Pts',(0.298538242131932,0.129648455044593,
-0.0974048950729486));
#76597=CARTESIAN_POINT('Ctrl Pts',(0.0527615585466883,0.321135898403419,
-0.0815209649989606));
#76598=CARTESIAN_POINT('Ctrl Pts',(-0.241131656361081,0.218425930549086,
-0.0656370349249724));
#76599=CARTESIAN_POINT('Ctrl Pts',(-0.314550745770222,-0.0843402845056338,
-0.0497531048509844));
#76600=CARTESIAN_POINT('Ctrl Pts',(-0.098956075477821,-0.309959444016429,
-0.0338665800467495));
#76601=CARTESIAN_POINT('Ctrl Pts',(0.104013903462819,-0.270874008100452,
-0.0232746986005106));
#76602=CARTESIAN_POINT('Ctrl Pts',(0.174803057108209,-0.212690160363829,
-0.0179774605122677));
#76603=CARTESIAN_POINT('Ctrl Pts',(-0.129001978509869,0.264834879069913,
-1.9605824729399));
#76604=CARTESIAN_POINT('Ctrl Pts',(-0.217125573947727,0.221911449240131,
-1.95528666939287));
#76605=CARTESIAN_POINT('Ctrl Pts',(-0.34560563565713,0.0419371078532527,
-1.94469622248786));
#76606=CARTESIAN_POINT('Ctrl Pts',(-0.222300508284811,-0.268346965716144,
-1.92881113222485));
#76607=CARTESIAN_POINT('Ctrl Pts',(0.10493210678592,-0.331943705014839,
-1.91292720215086));
#76608=CARTESIAN_POINT('Ctrl Pts',(0.33588874818582,-0.0918812532016676,
-1.89704327207688));
#76609=CARTESIAN_POINT('Ctrl Pts',(0.259230383223593,0.232568128446287,
-1.88115934200289));
#76610=CARTESIAN_POINT('Ctrl Pts',(-0.0549399489197289,0.343857192940258,
-1.8652754119289));
#76611=CARTESIAN_POINT('Ctrl Pts',(-0.318760314519713,0.140212152499201,
-1.84939148185491));
#76612=CARTESIAN_POINT('Ctrl Pts',(-0.290588512238902,-0.191906845033854,
-1.83350755178092));
#76613=CARTESIAN_POINT('Ctrl Pts',(0.00378570098826755,-0.348211334247439,
-1.81762362170694));
#76614=CARTESIAN_POINT('Ctrl Pts',(0.294688872568306,-0.185541968274115,
-1.80173969163295));
#76615=CARTESIAN_POINT('Ctrl Pts',(0.31564103306055,0.14709942720655,-1.78585576155896));
#76616=CARTESIAN_POINT('Ctrl Pts',(0.0474462662005358,0.344986597258388,
-1.76997183148497));
#76617=CARTESIAN_POINT('Ctrl Pts',(-0.264211672727102,0.22684663000843,
-1.75408790141098));
#76618=CARTESIAN_POINT('Ctrl Pts',(-0.333836143332704,-0.0990990682672344,
-1.73820397133699));
#76619=CARTESIAN_POINT('Ctrl Pts',(-0.0976466077698041,-0.33426375298726,
-1.72232004126301));
#76620=CARTESIAN_POINT('Ctrl Pts',(0.227992999408525,-0.263223014519772,
-1.70643611118902));
#76621=CARTESIAN_POINT('Ctrl Pts',(0.344777409897277,0.0489458486037273,
-1.69055218111503));
#76622=CARTESIAN_POINT('Ctrl Pts',(0.145725064268752,0.316277337158927,
-1.67466825104104));
#76623=CARTESIAN_POINT('Ctrl Pts',(-0.186820151030732,0.2938798845607,-1.65878432096705));
#76624=CARTESIAN_POINT('Ctrl Pts',(-0.348226933717562,0.00227085902303463,
-1.64290039089307));
#76625=CARTESIAN_POINT('Ctrl Pts',(-0.190637005116948,-0.291418402318793,
-1.62701646081908));
#76626=CARTESIAN_POINT('Ctrl Pts',(0.141587826335567,-0.31815097265037,
-1.61113253074509));
#76627=CARTESIAN_POINT('Ctrl Pts',(0.344109737113365,-0.0534382123617138,
-1.5952486006711));
#76628=CARTESIAN_POINT('Ctrl Pts',(0.231406537223853,0.260227147130818,
-1.57936467059712));
#76629=CARTESIAN_POINT('Ctrl Pts',(-0.0932788976591828,0.335508868697075,
-1.56348074052312));
#76630=CARTESIAN_POINT('Ctrl Pts',(-0.33251528068979,0.10344438981997,-1.54759681044914));
#76631=CARTESIAN_POINT('Ctrl Pts',(-0.267147769245746,-0.223381339975787,
-1.53171288037515));
#76632=CARTESIAN_POINT('Ctrl Pts',(0.0429430845983787,-0.345576395560456,
-1.51582895030116));
#76633=CARTESIAN_POINT('Ctrl Pts',(0.313695503302601,-0.151202793900476,
-1.49994502022717));
#76634=CARTESIAN_POINT('Ctrl Pts',(0.297084069816041,0.181681614743433,
-1.48406109015319));
#76635=CARTESIAN_POINT('Ctrl Pts',(0.00832585123178702,0.348134792685833,
-1.4681771600792));
#76636=CARTESIAN_POINT('Ctrl Pts',(-0.288059345291665,0.195675668558975,
-1.45229323000521));
#76637=CARTESIAN_POINT('Ctrl Pts',(-0.320564944405325,-0.136034076959434,
-1.43640929993122));
#76638=CARTESIAN_POINT('Ctrl Pts',(-0.0594138722271255,-0.343128467870509,
-1.42052536985723));
#76639=CARTESIAN_POINT('Ctrl Pts',(0.256163862165409,-0.23589664982039,
-1.40464143978325));
#76640=CARTESIAN_POINT('Ctrl Pts',(0.337080170279715,0.0874306152339582,
-1.38875750970926));
#76641=CARTESIAN_POINT('Ctrl Pts',(0.109210871949668,0.330666204992337,
-1.37287357963527));
#76642=CARTESIAN_POINT('Ctrl Pts',(-0.218702120132325,0.270991764313301,
-1.35698964956128));
#76643=CARTESIAN_POINT('Ctrl Pts',(-0.346270883303697,-0.0369273482948824,
-1.34110571948729));
#76644=CARTESIAN_POINT('Ctrl Pts',(-0.156634796939567,-0.311018800177289,
-1.32522178941331));
#76645=CARTESIAN_POINT('Ctrl Pts',(0.176488136257323,-0.300198420109819,
-1.30933785933932));
#76646=CARTESIAN_POINT('Ctrl Pts',(0.347937375806666,-0.0143783237127102,
-1.29345392926533));
#76647=CARTESIAN_POINT('Ctrl Pts',(0.20065515896689,0.284613177586684,-1.27756999919134));
#76648=CARTESIAN_POINT('Ctrl Pts',(-0.130439190447699,0.322881977309613,
-1.26168606911735));
#76649=CARTESIAN_POINT('Ctrl Pts',(-0.342043436089377,0.0653715649513554,
-1.24580213904337));
#76650=CARTESIAN_POINT('Ctrl Pts',(-0.240315426809168,-0.252023112657438,
-1.22991820896938));
#76651=CARTESIAN_POINT('Ctrl Pts',(0.0815558936116627,-0.338549538314881,
-1.21403427889539));
#76652=CARTESIAN_POINT('Ctrl Pts',(0.328717135278538,-0.114944328482481,
-1.1981503488214));
#76653=CARTESIAN_POINT('Ctrl Pts',(0.274753810995919,0.213956764368961,
-1.18226641874741));
#76654=CARTESIAN_POINT('Ctrl Pts',(-0.030900445093492,0.346860658145371,
-1.16638248867342));
#76655=CARTESIAN_POINT('Ctrl Pts',(-0.30824804443214,0.162019433339887,
-1.15049855859943));
#76656=CARTESIAN_POINT('Ctrl Pts',(-0.303221989882145,-0.171241287451154,
-1.13461462852545));
#76657=CARTESIAN_POINT('Ctrl Pts',(-0.0204264481643065,-0.347634742066163,
-1.11873069845146));
#76658=CARTESIAN_POINT('Ctrl Pts',(0.2810809423659,-0.205573970907589,-1.10284676837747));
#76659=CARTESIAN_POINT('Ctrl Pts',(0.32510137014655,0.124804858899214,-1.08696283830348));
#76660=CARTESIAN_POINT('Ctrl Pts',(0.0713094892016032,0.340854969783078,
-1.0710789082295));
#76661=CARTESIAN_POINT('Ctrl Pts',(-0.247806150925284,0.244661531998007,
-1.05519497815551));
#76662=CARTESIAN_POINT('Ctrl Pts',(-0.339916528385347,-0.0756565093463238,
-1.03931104808152));
#76663=CARTESIAN_POINT('Ctrl Pts',(-0.12064302565199,-0.32666866093574,
-1.02342711800753));
#76664=CARTESIAN_POINT('Ctrl Pts',(0.209146707710798,-0.278432771651885,
-1.00754318793354));
#76665=CARTESIAN_POINT('Ctrl Pts',(0.347345541725384,0.0248641975441668,
-0.991659257859552));
#76666=CARTESIAN_POINT('Ctrl Pts',(0.16735507478394,0.305384073946364,-0.975775327785563));
#76667=CARTESIAN_POINT('Ctrl Pts',(-0.16594265498412,0.306153864801407,
-0.959891397711576));
#76668=CARTESIAN_POINT('Ctrl Pts',(-0.347226982979686,0.0264683956227249,
-0.944007467637586));
#76669=CARTESIAN_POINT('Ctrl Pts',(-0.21043061692469,-0.277463707783037,
-0.928123537563599));
#76670=CARTESIAN_POINT('Ctrl Pts',(0.119132786145999,-0.327222451768071,
-0.912239607489611));
#76671=CARTESIAN_POINT('Ctrl Pts',(0.339563428345645,-0.0772258493392489,
-0.896355677415623));
#76672=CARTESIAN_POINT('Ctrl Pts',(0.248933651117318,0.243514252185408,
-0.880471747341634));
#76673=CARTESIAN_POINT('Ctrl Pts',(-0.0697342464219807,0.341180727110977,
-0.864587817267647));
#76674=CARTESIAN_POINT('Ctrl Pts',(-0.324521401426087,0.126305240162334,
-0.848703887193659));
#76675=CARTESIAN_POINT('Ctrl Pts',(-0.282027533757167,-0.204273404727259,
-0.83281995711967));
#76676=CARTESIAN_POINT('Ctrl Pts',(0.018820431018591,-0.347725387414107,
-0.816936027045682));
#76677=CARTESIAN_POINT('Ctrl Pts',(0.302427754789573,-0.172640107764547,
-0.801052096971694));
#76678=CARTESIAN_POINT('Ctrl Pts',(0.308993158263571,0.160593841171823,
-0.785168166897706));
#76679=CARTESIAN_POINT('Ctrl Pts',(0.0325023389926279,0.346714221854288,
-0.769284236823718));
#76680=CARTESIAN_POINT('Ctrl Pts',(-0.273762567696073,0.215223628360061,
-0.75340030674973));
#76681=CARTESIAN_POINT('Ctrl Pts',(-0.329244580755436,-0.113424687432649,
-0.737516376675742));
#76682=CARTESIAN_POINT('Ctrl Pts',(-0.0831188562467696,-0.338169202341438,
-0.721632446601753));
#76683=CARTESIAN_POINT('Ctrl Pts',(0.239148714315398,-0.253130492270901,
-0.705748516527766));
#76684=CARTESIAN_POINT('Ctrl Pts',(0.342341752195895,0.0637908957411709,
-0.689864586453776));
#76685=CARTESIAN_POINT('Ctrl Pts',(0.131929259750061,0.322276006084563,
-0.67398065637979));
#76686=CARTESIAN_POINT('Ctrl Pts',(-0.199338329113583,0.285537010249495,
-0.658096726305801));
#76687=CARTESIAN_POINT('Ctrl Pts',(-0.348000080345551,-0.012770973162193,
-0.642212796231813));
#76688=CARTESIAN_POINT('Ctrl Pts',(-0.177872934078603,-0.299379980957783,
-0.626328866157825));
#76689=CARTESIAN_POINT('Ctrl Pts',(0.155196463504772,-0.311739011661393,
-0.610444936083836));
#76690=CARTESIAN_POINT('Ctrl Pts',(0.346096613749853,-0.0385264535991275,
-0.594561006009849));
#76691=CARTESIAN_POINT('Ctrl Pts',(0.219951555798699,0.269978641336165,
-0.578677075935861));
#76692=CARTESIAN_POINT('Ctrl Pts',(-0.107682288897933,0.331167145613336,
-0.562793145861872));
#76693=CARTESIAN_POINT('Ctrl Pts',(-0.336672713387052,0.0889867278687308,
-0.546909215787884));
#76694=CARTESIAN_POINT('Ctrl Pts',(-0.257250786326287,-0.234710857461478,
-0.531025285713896));
#76695=CARTESIAN_POINT('Ctrl Pts',(0.0578282545825028,-0.34339925254404,
-0.515141355639908));
#76696=CARTESIAN_POINT('Ctrl Pts',(0.319933153924289,-0.13751338370209,
-0.49925742556592));
#76697=CARTESIAN_POINT('Ctrl Pts',(0.288960139853882,0.194342973245417,
-0.483373495491932));
#76698=CARTESIAN_POINT('Ctrl Pts',(-0.00671765333527564,0.348169537451584,
-0.467489565417944));
#76699=CARTESIAN_POINT('Ctrl Pts',(-0.296241674114894,0.183051971311387,
-0.451605635343955));
#76700=CARTESIAN_POINT('Ctrl Pts',(-0.314390594621468,-0.149752154161186,
-0.435721705269968));
#76701=CARTESIAN_POINT('Ctrl Pts',(-0.0445389177827234,-0.345374345428521,
-0.419837775195979));
#76702=CARTESIAN_POINT('Ctrl Pts',(0.266113073051594,-0.224612969514096,
-0.403953845121992));
#76703=CARTESIAN_POINT('Ctrl Pts',(0.332989564797437,0.101907327066275,
-0.388069915048003));
#76704=CARTESIAN_POINT('Ctrl Pts',(0.0948276900512347,0.335074413998132,
-0.372185984974015));
#76705=CARTESIAN_POINT('Ctrl Pts',(-0.230202024213326,0.26129328734756,
-0.356302054900027));
#76706=CARTESIAN_POINT('Ctrl Pts',(-0.344352907269043,-0.0518481261508553,
-0.340418124826038));
#76707=CARTESIAN_POINT('Ctrl Pts',(-0.143055925463681,-0.317493553252295,
-0.324534194752051));
#76708=CARTESIAN_POINT('Ctrl Pts',(0.189288851726114,-0.292295887745218,
-0.308650264678062));
#76709=CARTESIAN_POINT('Ctrl Pts',(0.348233699850533,0.000662302712354398,
-0.292766334604074));
#76710=CARTESIAN_POINT('Ctrl Pts',(0.188175667899375,0.293013782067735,
-0.276882404530086));
#76711=CARTESIAN_POINT('Ctrl Pts',(-0.144262587366613,0.316947107635427,
-0.260998474456099));
#76712=CARTESIAN_POINT('Ctrl Pts',(-0.344547582103868,0.050537908904675,
-0.24511454438211));
#76713=CARTESIAN_POINT('Ctrl Pts',(-0.2292065614917,-0.262167023280654,
-0.229230614308122));
#76714=CARTESIAN_POINT('Ctrl Pts',(0.0961017423423954,-0.334711303469409,
-0.213346684234133));
#76715=CARTESIAN_POINT('Ctrl Pts',(0.333374416911505,-0.100639945415362,
-0.197462754160146));
#76716=CARTESIAN_POINT('Ctrl Pts',(0.265257480635327,0.225623518727604,
-0.181578824086157));
#76717=CARTESIAN_POINT('Ctrl Pts',(-0.0458536705348012,0.345202541278447,
-0.16569489401217));
#76718=CARTESIAN_POINT('Ctrl Pts',(-0.314955360340258,0.148554992589589,
-0.149810963938181));
#76719=CARTESIAN_POINT('Ctrl Pts',(-0.295548175309825,-0.18417707970076,
-0.133927033864193));
#76720=CARTESIAN_POINT('Ctrl Pts',(-0.00538383188932432,-0.348193337350606,
-0.118043103790205));
#76721=CARTESIAN_POINT('Ctrl Pts',(0.289679298180285,-0.193240967007088,
-0.102159173716217));
#76722=CARTESIAN_POINT('Ctrl Pts',(0.319442126683677,0.138726542720093,
-0.0862752436422287));
#76723=CARTESIAN_POINT('Ctrl Pts',(0.05645596473316,0.343622088774564,-0.0703913135682407));
#76724=CARTESIAN_POINT('Ctrl Pts',(-0.258015886235105,0.23372028748875,
-0.0545073834942526));
#76725=CARTESIAN_POINT('Ctrl Pts',(-0.336575838529829,-0.0902458581359205,
-0.0386234534202645));
#76726=CARTESIAN_POINT('Ctrl Pts',(-0.105885058387047,-0.331663050184843,
-0.0227369286160296));
#76727=CARTESIAN_POINT('Ctrl Pts',(0.11129703950005,-0.289840821038601,
-0.0121450471697907));
#76728=CARTESIAN_POINT('Ctrl Pts',(0.187042905842451,-0.227582894124795,
-0.00684780908154777));
#76729=CARTESIAN_POINT('Ctrl Pts',(-0.289034808525452,-0.0555371045866529,
-0.04));
#76730=CARTESIAN_POINT('Ctrl Pts',(-0.288636144038534,-0.0573073412592883,
-0.04));
#76731=CARTESIAN_POINT('Ctrl Pts',(-0.288237479551616,-0.0590775779319236,
-0.04));
#76732=CARTESIAN_POINT('Ctrl Pts',(-0.287838815064698,-0.060847814604559,
-0.04));
#76733=CARTESIAN_POINT('Ctrl Pts',(-0.138000239402477,-0.193373078029398,
-1.9608));
#76734=CARTESIAN_POINT('Ctrl Pts',(-0.143086395765402,-0.190606700707026,
-1.9608));
#76735=CARTESIAN_POINT('Ctrl Pts',(-0.148054697801646,-0.187647084738665,
-1.9608));
#76736=CARTESIAN_POINT('Ctrl Pts',(-0.152892767683467,-0.184496670108783,
-1.9608));
#76737=CARTESIAN_POINT('Ctrl Pts',(-0.163043940938266,-0.177886512439802,
-1.9608));
#76738=CARTESIAN_POINT('Ctrl Pts',(-0.172622493969985,-0.170437982864818,
-1.9608));
#76739=CARTESIAN_POINT('Ctrl Pts',(-0.181598967428321,-0.162265254850832,
-1.9608));
#76740=CARTESIAN_POINT('Ctrl Pts',(-0.187293781374843,-0.157080349476667,
-1.9608));
#76741=CARTESIAN_POINT('Ctrl Pts',(-0.192748306396003,-0.151599882545997,
-1.9608));
#76742=CARTESIAN_POINT('Ctrl Pts',(-0.197929623010393,-0.145877589802222,
-1.9608));
#76743=CARTESIAN_POINT('Ctrl Pts',(-0.2048094626486,-0.138279432930144,
-1.9608));
#76744=CARTESIAN_POINT('Ctrl Pts',(-0.21121792230437,-0.130247035676296,
-1.9608));
#76745=CARTESIAN_POINT('Ctrl Pts',(-0.217136672188152,-0.121843996423096,
-1.9608));
#76746=CARTESIAN_POINT('Ctrl Pts',(-0.221200409818485,-0.116074577628095,
-1.9608));
#76747=CARTESIAN_POINT('Ctrl Pts',(-0.225034010493672,-0.110128828935726,
-1.9608));
#76748=CARTESIAN_POINT('Ctrl Pts',(-0.228627257789668,-0.10402957803314,
-1.9608));
#76749=CARTESIAN_POINT('Ctrl Pts',(-0.231459374288426,-0.0992222859966238,
-1.9608));
#76750=CARTESIAN_POINT('Ctrl Pts',(-0.234138268440307,-0.0943260187649396,
-1.9608));
#76751=CARTESIAN_POINT('Ctrl Pts',(-0.236657767742044,-0.0893577521864006,
-1.9608));
#76752=CARTESIAN_POINT('Ctrl Pts',(-0.243910061937438,-0.0750567635558887,
-1.9608));
#76753=CARTESIAN_POINT('Ctrl Pts',(-0.249855778463453,-0.060142531185048,
-1.9608));
#76754=CARTESIAN_POINT('Ctrl Pts',(-0.25441935181254,-0.0448298972586075,
-1.9608));
#76755=CARTESIAN_POINT('Ctrl Pts',(-0.257348678655569,-0.0350008211888239,
-1.9608));
#76756=CARTESIAN_POINT('Ctrl Pts',(-0.259707778490682,-0.0250074014029279,
-1.9608));
#76757=CARTESIAN_POINT('Ctrl Pts',(-0.261467624497603,-0.0148976599763562,
-1.9608));
#76758=CARTESIAN_POINT('Ctrl Pts',(-0.262470243263279,-0.00913794212005506,
-1.9608));
#76759=CARTESIAN_POINT('Ctrl Pts',(-0.26327682977629,-0.00334534667317961,
-1.9608));
#76760=CARTESIAN_POINT('Ctrl Pts',(-0.263880808002415,0.00245049521744596,
-1.9608));
#76761=CARTESIAN_POINT('Ctrl Pts',(-0.264901640441406,0.012246516261413,
-1.9608));
#76762=CARTESIAN_POINT('Ctrl Pts',(-0.265346751527308,0.0220655810592102,
-1.9608));
#76763=CARTESIAN_POINT('Ctrl Pts',(-0.265197864941953,0.0318610581547499,
-1.9608));
#76764=CARTESIAN_POINT('Ctrl Pts',(-0.265021292489645,0.0434780309543282,
-1.9608));
#76765=CARTESIAN_POINT('Ctrl Pts',(-0.264009847886286,0.0550619824997758,
-1.9608));
#76766=CARTESIAN_POINT('Ctrl Pts',(-0.262216867534709,0.0665542493180926,
-1.9608));
#76767=CARTESIAN_POINT('Ctrl Pts',(-0.261115413480366,0.0736141169120082,
-1.9608));
#76768=CARTESIAN_POINT('Ctrl Pts',(-0.259718714489693,0.0806394477428598,
-1.9608));
#76769=CARTESIAN_POINT('Ctrl Pts',(-0.258036389767163,0.0876167385651326,
-1.9608));
#76770=CARTESIAN_POINT('Ctrl Pts',(-0.256725636355855,0.0930529707172855,
-1.9608));
#76771=CARTESIAN_POINT('Ctrl Pts',(-0.255241512393281,0.0984579649283385,
-1.9608));
#76772=CARTESIAN_POINT('Ctrl Pts',(-0.253595547443031,0.103805521125184,
-1.9608));
#76773=CARTESIAN_POINT('Ctrl Pts',(-0.248517117827109,0.120304771463862,
-1.9608));
#76774=CARTESIAN_POINT('Ctrl Pts',(-0.241891167152933,0.13630805743798,
-1.9608));
#76775=CARTESIAN_POINT('Ctrl Pts',(-0.233880496481478,0.151633352688369,
-1.9608));
#76776=CARTESIAN_POINT('Ctrl Pts',(-0.229912443575941,0.159224674918506,
-1.9608));
#76777=CARTESIAN_POINT('Ctrl Pts',(-0.225603661083085,0.166649682158028,
-1.9608));
#76778=CARTESIAN_POINT('Ctrl Pts',(-0.220968694610218,0.173885464859617,
-1.9608));
#76779=CARTESIAN_POINT('Ctrl Pts',(-0.217449048122994,0.17938008867557,
-1.9608));
#76780=CARTESIAN_POINT('Ctrl Pts',(-0.213739562626335,0.184767816744313,
-1.9608));
#76781=CARTESIAN_POINT('Ctrl Pts',(-0.209851120783383,0.190030463551426,
-1.9608));
#76782=CARTESIAN_POINT('Ctrl Pts',(-0.205687585120815,0.1956654244293,-1.9608));
#76783=CARTESIAN_POINT('Ctrl Pts',(-0.201328524903064,0.201144177852673,
-1.9608));
#76784=CARTESIAN_POINT('Ctrl Pts',(-0.196786165510293,0.206452912344335,
-1.9608));
#76785=CARTESIAN_POINT('Ctrl Pts',(-0.18548209900297,0.219664171642526,
-1.9608));
#76786=CARTESIAN_POINT('Ctrl Pts',(-0.173040875473831,0.231830875283052,
-1.9608));
#76787=CARTESIAN_POINT('Ctrl Pts',(-0.15958491798273,0.24277084955155,-1.9608));
#76788=CARTESIAN_POINT('Ctrl Pts',(-0.149872809851103,0.250666996155991,
-1.9608));
#76789=CARTESIAN_POINT('Ctrl Pts',(-0.139630976873493,0.257923930314965,
-1.9608));
#76790=CARTESIAN_POINT('Ctrl Pts',(-0.128892185405331,0.264462557919713,
-1.9608));
#76791=CARTESIAN_POINT('Origin',(-3.51939854619125E-17,0.,-1.9608));
#76792=CARTESIAN_POINT('',(-0.2942,-3.60291088309151E-17,-1.9608));
#76793=CARTESIAN_POINT('Origin',(0.,0.,-1.9608));
#76794=CARTESIAN_POINT('',(0.133821547094406,0.262002735736212,-1.9608));
#76795=CARTESIAN_POINT('Origin',(0.,0.,-1.9608));
#76796=CARTESIAN_POINT('Ctrl Pts',(0.133821547094406,0.262002735736212,
-1.9608));
#76797=CARTESIAN_POINT('Ctrl Pts',(0.138297615113376,0.259182261595568,
-1.9608));
#76798=CARTESIAN_POINT('Ctrl Pts',(0.142687341570814,0.256233989666448,
-1.9608));
#76799=CARTESIAN_POINT('Ctrl Pts',(0.146984512649617,0.253157526346722,
-1.9608));
#76800=CARTESIAN_POINT('Ctrl Pts',(0.156416973582358,0.246404567355291,
-1.9608));
#76801=CARTESIAN_POINT('Ctrl Pts',(0.165404046449669,0.239034332280283,
-1.9608));
#76802=CARTESIAN_POINT('Ctrl Pts',(0.173915563696922,0.231109827924898,
-1.9608));
#76803=CARTESIAN_POINT('Ctrl Pts',(0.178983715958836,0.226391210373337,
-1.9608));
#76804=CARTESIAN_POINT('Ctrl Pts',(0.183884248765666,0.221474694998783,
-1.9608));
#76805=CARTESIAN_POINT('Ctrl Pts',(0.188605652765418,0.216376747084418,
-1.9608));
#76806=CARTESIAN_POINT('Ctrl Pts',(0.194496179098994,0.210016436372108,
-1.9608));
#76807=CARTESIAN_POINT('Ctrl Pts',(0.200097635413564,0.203384895024988,
-1.9608));
#76808=CARTESIAN_POINT('Ctrl Pts',(0.205392638302791,0.196515230368162,
-1.9608));
#76809=CARTESIAN_POINT('Ctrl Pts',(0.212203122093379,0.187679401423239,
-1.9608));
#76810=CARTESIAN_POINT('Ctrl Pts',(0.218510175211099,0.178446116869452,
-1.9608));
#76811=CARTESIAN_POINT('Ctrl Pts',(0.224281484638061,0.168869554768253,
-1.9608));
#76812=CARTESIAN_POINT('Ctrl Pts',(0.22751782490307,0.163499367305478,-1.9608));
#76813=CARTESIAN_POINT('Ctrl Pts',(0.230586998760227,0.158018286713927,
-1.9608));
#76814=CARTESIAN_POINT('Ctrl Pts',(0.233476785545442,0.152446119292306,
-1.9608));
#76815=CARTESIAN_POINT('Ctrl Pts',(0.237406871706289,0.144868017620003,
-1.9608));
#76816=CARTESIAN_POINT('Ctrl Pts',(0.240998077474448,0.137136337286731,
-1.9608));
#76817=CARTESIAN_POINT('Ctrl Pts',(0.244237996620259,0.129277760874839,
-1.9608));
#76818=CARTESIAN_POINT('Ctrl Pts',(0.250537692111831,0.113997552893049,
-1.9608));
#76819=CARTESIAN_POINT('Ctrl Pts',(0.255513873420495,0.0982344656391996,
-1.9608));
#76820=CARTESIAN_POINT('Ctrl Pts',(0.259043884351174,0.0821679460335087,
-1.9608));
#76821=CARTESIAN_POINT('Ctrl Pts',(0.260467944208438,0.0756864687617066,
-1.9608));
#76822=CARTESIAN_POINT('Ctrl Pts',(0.261656067894151,0.0691556200203403,
-1.9608));
#76823=CARTESIAN_POINT('Ctrl Pts',(0.262597734038404,0.0625875582041159,
-1.9608));
#76824=CARTESIAN_POINT('Ctrl Pts',(0.263470407024643,0.0565007193027163,
-1.9608));
#76825=CARTESIAN_POINT('Ctrl Pts',(0.264131287375213,0.0503777548586035,
-1.9608));
#76826=CARTESIAN_POINT('Ctrl Pts',(0.26456994765883,0.0442583426162408,
-1.9608));
#76827=CARTESIAN_POINT('Ctrl Pts',(0.265334619145271,0.0335909988190579,
-1.9608));
#76828=CARTESIAN_POINT('Ctrl Pts',(0.265427901586744,0.022920104419746,
-1.9608));
#76829=CARTESIAN_POINT('Ctrl Pts',(0.264815004423569,0.0122950415847356,
-1.9608));
#76830=CARTESIAN_POINT('Ctrl Pts',(0.263869571843309,-0.00409478883881043,
-1.9608));
#76831=CARTESIAN_POINT('Ctrl Pts',(0.261245615493676,-0.0203764095907301,
-1.9608));
#76832=CARTESIAN_POINT('Ctrl Pts',(0.257049826563265,-0.0363442073303925,
-1.9608));
#76833=CARTESIAN_POINT('Ctrl Pts',(0.25528111713989,-0.0430753358025595,
-1.9608));
#76834=CARTESIAN_POINT('Ctrl Pts',(0.253229675597862,-0.0497567776443664,
-1.9608));
#76835=CARTESIAN_POINT('Ctrl Pts',(0.250916504864508,-0.0563328026274767,
-1.9608));
#76836=CARTESIAN_POINT('Ctrl Pts',(0.245894613969703,-0.0706093449987376,
-1.9608));
#76837=CARTESIAN_POINT('Ctrl Pts',(0.239635781072895,-0.0844231946567744,
-1.9608));
#76838=CARTESIAN_POINT('Ctrl Pts',(0.232232690107956,-0.097615126217959,
-1.9608));
#76839=CARTESIAN_POINT('Ctrl Pts',(0.226848422394677,-0.107209617426709,
-1.9608));
#76840=CARTESIAN_POINT('Ctrl Pts',(0.220857960469645,-0.11647482010455,
-1.9608));
#76841=CARTESIAN_POINT('Ctrl Pts',(0.214287232483329,-0.125338313944058,
-1.9608));
#76842=CARTESIAN_POINT('Ctrl Pts',(0.210193048601064,-0.130861107414408,
-1.9608));
#76843=CARTESIAN_POINT('Ctrl Pts',(0.205869486213015,-0.136231200486207,
-1.9608));
#76844=CARTESIAN_POINT('Ctrl Pts',(0.201350239334785,-0.141399126486128,
-1.9608));
#76845=CARTESIAN_POINT('Ctrl Pts',(0.191610974505686,-0.152536336133355,
-1.9608));
#76846=CARTESIAN_POINT('Ctrl Pts',(0.180942748192052,-0.162770241399539,
-1.9608));
#76847=CARTESIAN_POINT('Ctrl Pts',(0.169418754522685,-0.17192999128596,
-1.9608));
#76848=CARTESIAN_POINT('Ctrl Pts',(0.159472693097453,-0.179835534938963,
-1.9608));
#76849=CARTESIAN_POINT('Ctrl Pts',(0.148888342042439,-0.186940774148992,
-1.9608));
#76850=CARTESIAN_POINT('Ctrl Pts',(0.137702479013108,-0.19310620885576,
-1.9608));
#76851=CARTESIAN_POINT('Ctrl Pts',(0.170904093888077,-0.23991444519679,
-1.99394055716378));
#76852=CARTESIAN_POINT('Ctrl Pts',(0.250758961454554,-0.183034120394509,
-1.9886433188887));
#76853=CARTESIAN_POINT('Ctrl Pts',(0.347776689926164,0.0157071971072416,
-1.97805143725563));
#76854=CARTESIAN_POINT('Ctrl Pts',(0.174902784065685,0.301363500003521,
-1.96216491226457));
#76855=CARTESIAN_POINT('Ctrl Pts',(-0.158317247439313,0.310026665536666,
-1.94628098219058));
#76856=CARTESIAN_POINT('Ctrl Pts',(-0.346428810985269,0.035126883458298,
-1.9303970521166));
#76857=CARTESIAN_POINT('Ctrl Pts',(-0.217232984403476,-0.272179277325897,
-1.91451312204261));
#76858=CARTESIAN_POINT('Ctrl Pts',(0.110983315678744,-0.330033805723321,
-1.89862919196862));
#76859=CARTESIAN_POINT('Ctrl Pts',(0.337520707764598,-0.0856199548585268,
-1.88274526189463));
#76860=CARTESIAN_POINT('Ctrl Pts',(0.254874981231195,0.237259528375207,
-1.86686133182064));
#76861=CARTESIAN_POINT('Ctrl Pts',(-0.0612546449745717,0.342778004190948,
-1.85097740174666));
#76862=CARTESIAN_POINT('Ctrl Pts',(-0.321269693814492,0.134300259451662,
-1.83509347167267));
#76863=CARTESIAN_POINT('Ctrl Pts',(-0.28698334628375,-0.197209240948837,
-1.81920954159868));
#76864=CARTESIAN_POINT('Ctrl Pts',(0.0101973733548513,-0.34806082496865,
-1.80332561152469));
#76865=CARTESIAN_POINT('Ctrl Pts',(0.298036451033343,-0.180069148869172,
-1.7874416814507));
#76866=CARTESIAN_POINT('Ctrl Pts',(0.312856429901399,0.152877314430839,
-1.77155775137671));
#76867=CARTESIAN_POINT('Ctrl Pts',(0.041081132865898,0.345778658064987,
-1.75567382130273));
#76868=CARTESIAN_POINT('Ctrl Pts',(-0.268326906005064,0.22192624403291,
-1.73978989122873));
#76869=CARTESIAN_POINT('Ctrl Pts',(-0.331931460478688,-0.105223985707714,
-1.72390596115475));
#76870=CARTESIAN_POINT('Ctrl Pts',(-0.0914669254283658,-0.335982697609461,
-1.70802203108076));
#76871=CARTESIAN_POINT('Ctrl Pts',(0.232786781689362,-0.258961180118152,
-1.69213810100677));
#76872=CARTESIAN_POINT('Ctrl Pts',(0.34379386966368,0.0552842881121883,
-1.67625417093279));
#76873=CARTESIAN_POINT('Ctrl Pts',(0.139865199476729,0.31888603304783,-1.6603702408588));
#76874=CARTESIAN_POINT('Ctrl Pts',(-0.192188362092366,0.290369093748387,
-1.64448631078481));
#76875=CARTESIAN_POINT('Ctrl Pts',(-0.348185884034223,-0.00414331274272311,
-1.62860238071082));
#76876=CARTESIAN_POINT('Ctrl Pts',(-0.18522430098761,-0.294860195792014,
-1.61271845063683));
#76877=CARTESIAN_POINT('Ctrl Pts',(0.14741382526022,-0.315467495963393,
-1.59683452056285));
#76878=CARTESIAN_POINT('Ctrl Pts',(0.345012066558079,-0.0470876923556176,
-1.58095059048886));
#76879=CARTESIAN_POINT('Ctrl Pts',(0.226558609757863,0.264427254971228,
-1.56506666041487));
#76880=CARTESIAN_POINT('Ctrl Pts',(-0.0994360905582914,0.333711013816492,
-1.54918273034088));
#76881=CARTESIAN_POINT('Ctrl Pts',(-0.334341381795663,0.0972955151030245,
-1.53329880026689));
#76882=CARTESIAN_POINT('Ctrl Pts',(-0.26296996072181,-0.228248497468949,
-1.5174148701929));
#76883=CARTESIAN_POINT('Ctrl Pts',(0.0492976801743824,-0.344703228257538,
-1.50153094011892));
#76884=CARTESIAN_POINT('Ctrl Pts',(0.316405696118587,-0.145389175333612,
-1.48564701004493));
#76885=CARTESIAN_POINT('Ctrl Pts',(0.29366716108482,0.187110062104603,-1.46976307997094));
#76886=CARTESIAN_POINT('Ctrl Pts',(0.00191193381121215,0.34820528621762,
-1.45387914989695));
#76887=CARTESIAN_POINT('Ctrl Pts',(-0.291594739241419,0.190323631972808,
-1.43799521982296));
#76888=CARTESIAN_POINT('Ctrl Pts',(-0.317983182473595,-0.141905857893761,
-1.42211128974898));
#76889=CARTESIAN_POINT('Ctrl Pts',(-0.0530800028323548,-0.344141090455598,
-1.40622735967499));
#76890=CARTESIAN_POINT('Ctrl Pts',(0.260447635646281,-0.231122491174878,
-1.390343429601));
#76891=CARTESIAN_POINT('Ctrl Pts',(0.335389655002547,0.0936181401112829,
-1.37445949952701));
#76892=CARTESIAN_POINT('Ctrl Pts',(0.103094681066654,0.332598953059679,
-1.35857556945302));
#76893=CARTESIAN_POINT('Ctrl Pts',(-0.223641189786869,0.266899222687776,
-1.34269163937903));
#76894=CARTESIAN_POINT('Ctrl Pts',(-0.345508348378294,-0.0432961665916229,
-1.32680770930505));
#76895=CARTESIAN_POINT('Ctrl Pts',(-0.150869185055043,-0.313829676483047,
-1.31092377923106));
#76896=CARTESIAN_POINT('Ctrl Pts',(0.181975179607525,-0.296876423529109,
-1.29503984915707));
#76897=CARTESIAN_POINT('Ctrl Pts',(0.348119390575748,-0.00796660189769713,
-1.27915591908308));
#76898=CARTESIAN_POINT('Ctrl Pts',(0.195365408734829,0.288241103783793,
-1.26327198900909));
#76899=CARTESIAN_POINT('Ctrl Pts',(-0.136354977936102,0.320402710401569,
-1.24738805893511));
#76900=CARTESIAN_POINT('Ctrl Pts',(-0.343166045501201,0.0590562617822472,
-1.23150412886112));
#76901=CARTESIAN_POINT('Ctrl Pts',(-0.235616480747601,-0.25638925648463,
-1.21562019878713));
#76902=CARTESIAN_POINT('Ctrl Pts',(0.0877718793749992,-0.336966873789705,
-1.19973626871314));
#76903=CARTESIAN_POINT('Ctrl Pts',(0.330755945827384,-0.10886267101472,
-1.18385233863915));
#76904=CARTESIAN_POINT('Ctrl Pts',(0.270747773867585,0.218966252619836,
-1.16796840856517));
#76905=CARTESIAN_POINT('Ctrl Pts',(-0.0372815601730543,0.346208986179863,
-1.15208447849118));
#76906=CARTESIAN_POINT('Ctrl Pts',(-0.31115875421187,0.156303571673662,
-1.13620054841719));
#76907=CARTESIAN_POINT('Ctrl Pts',(-0.299995910030472,-0.176785267501611,
-1.1203166183432));
#76908=CARTESIAN_POINT('Ctrl Pts',(-0.0140188608700629,-0.347928223029595,
-1.10443268826921));
#76909=CARTESIAN_POINT('Ctrl Pts',(0.284800303718939,-0.200348106659949,
-1.08854875819523));
#76910=CARTESIAN_POINT('Ctrl Pts',(0.322725347996934,0.130762863997715,
-1.07266482812124));
#76911=CARTESIAN_POINT('Ctrl Pts',(0.0650146620166612,0.34208722654242,
-1.05678089804725));
#76912=CARTESIAN_POINT('Ctrl Pts',(-0.252253344769326,0.240039219489886,
-1.04089696797326));
#76913=CARTESIAN_POINT('Ctrl Pts',(-0.338442193212666,-0.0818990762708986,
-1.02501303789927));
#76914=CARTESIAN_POINT('Ctrl Pts',(-0.114597740703191,-0.328812917426232,
-1.00912910782529));
#76915=CARTESIAN_POINT('Ctrl Pts',(0.214225099680103,-0.274514450453299,
-0.993245177751293));
#76916=CARTESIAN_POINT('Ctrl Pts',(0.346804929786502,0.0312556797463465,
-0.977361247677308));
#76917=CARTESIAN_POINT('Ctrl Pts',(0.161690691822444,0.308393736996402,
-0.961477317603318));
#76918=CARTESIAN_POINT('Ctrl Pts',(-0.171541895225696,0.303024677250884,
-0.94559338752933));
#76919=CARTESIAN_POINT('Ctrl Pts',(-0.347631841388322,0.020066880514706,
-0.929709457455343));
#76920=CARTESIAN_POINT('Ctrl Pts',(-0.205270218971837,-0.281273379550714,
-0.913825527381354));
#76921=CARTESIAN_POINT('Ctrl Pts',(0.125131207143578,-0.324950392890079,
-0.897941597307366));
#76922=CARTESIAN_POINT('Ctrl Pts',(0.340904959815935,-0.070953401705074,
-0.882057667233379));
#76923=CARTESIAN_POINT('Ctrl Pts',(0.244389369957919,0.248041151207208,
-0.866173737159389));
#76924=CARTESIAN_POINT('Ctrl Pts',(-0.0760015067447896,0.339815167132293,
-0.850289807085402));
#76925=CARTESIAN_POINT('Ctrl Pts',(-0.326770455431364,0.12029815583709,
-0.834405877011414));
#76926=CARTESIAN_POINT('Ctrl Pts',(-0.278198113395417,-0.209419164700504,
-0.818521946937425));
#76927=CARTESIAN_POINT('Ctrl Pts',(0.025220347548139,-0.347295998983832,
-0.802638016863437));
#76928=CARTESIAN_POINT('Ctrl Pts',(0.305535460982617,-0.167028916426965,
-0.78675408678945));
#76929=CARTESIAN_POINT('Ctrl Pts',(0.305961809285915,0.166246648384607,
-0.77087015671546));
#76930=CARTESIAN_POINT('Ctrl Pts',(0.0261088319000491,0.347230335278244,
-0.754986226641474));
#76931=CARTESIAN_POINT('Ctrl Pts',(-0.27766139782707,0.210130257215241,
-0.739102296567485));
#76932=CARTESIAN_POINT('Ctrl Pts',(-0.327077172223595,-0.119461710396439,
-0.723218366493496));
#76933=CARTESIAN_POINT('Ctrl Pts',(-0.0768706849623521,-0.339619602841245,
-0.70733443641951));
#76934=CARTESIAN_POINT('Ctrl Pts',(0.243753949572878,-0.248665616658693,
-0.69145050634552));
#76935=CARTESIAN_POINT('Ctrl Pts',(0.341085380358906,0.0700809542318726,
-0.675566576271533));
#76936=CARTESIAN_POINT('Ctrl Pts',(0.125962192601037,0.324629177486809,
-0.659682646197544));
#76937=CARTESIAN_POINT('Ctrl Pts',(-0.204549901004051,0.281797648747914,
-0.643798716123556));
#76938=CARTESIAN_POINT('Ctrl Pts',(-0.347682045271716,-0.0191773886733094,
-0.627914786049569));
#76939=CARTESIAN_POINT('Ctrl Pts',(-0.172316631198822,-0.302584790518111,
-0.61203085597558));
#76940=CARTESIAN_POINT('Ctrl Pts',(0.160901128269999,-0.30880641794178,
-0.596146925901592));
#76941=CARTESIAN_POINT('Ctrl Pts',(0.346723826115746,-0.032142887929545,
-0.580262995827604));
#76942=CARTESIAN_POINT('Ctrl Pts',(0.214926751705743,0.273965450817477,
-0.564379065753616));
#76943=CARTESIAN_POINT('Ctrl Pts',(-0.113756088221019,0.329105042855812,
-0.548495135679626));
#76944=CARTESIAN_POINT('Ctrl Pts',(-0.338231544314204,0.082764722391689,
-0.532611205605641));
#76945=CARTESIAN_POINT('Ctrl Pts',(-0.252866666444601,-0.239393036323237,
-0.51672727553165));
#76946=CARTESIAN_POINT('Ctrl Pts',(0.0641392091112833,-0.342252448778347,
-0.500843345457664));
#76947=CARTESIAN_POINT('Ctrl Pts',(0.322389731130484,-0.131588138179558,
-0.484959415383675));
#76948=CARTESIAN_POINT('Ctrl Pts',(0.285311967982603,0.199618781062624,
-0.469075485309687));
#76949=CARTESIAN_POINT('Ctrl Pts',(-0.0131286304801114,0.347962951912657,
-0.453191555235699));
#76950=CARTESIAN_POINT('Ctrl Pts',(-0.299542617972748,0.177552237117127,
-0.437307625161711));
#76951=CARTESIAN_POINT('Ctrl Pts',(-0.311557642847234,-0.155506951363366,
-0.421423695087722));
#76952=CARTESIAN_POINT('Ctrl Pts',(-0.0381672241935123,-0.346112467094931,
-0.405539765013735));
#76953=CARTESIAN_POINT('Ctrl Pts',(0.270186656754355,-0.219658251927647,
-0.389655834939746));
#76954=CARTESIAN_POINT('Ctrl Pts',(0.331033390463177,0.108016065916605,
-0.373771904865758));
#76955=CARTESIAN_POINT('Ctrl Pts',(0.0886337337118425,0.336741204159362,
-0.35788797479177));
#76956=CARTESIAN_POINT('Ctrl Pts',(-0.234959734190297,0.25699124857999,
-0.342004044717782));
#76957=CARTESIAN_POINT('Ctrl Pts',(-0.343316011856417,-0.0581780675448442,
-0.326120114643794));
#76958=CARTESIAN_POINT('Ctrl Pts',(-0.137174305814673,-0.320052794782354,
-0.310236184569806));
#76959=CARTESIAN_POINT('Ctrl Pts',(0.194627323824718,-0.288740006056718,
-0.294352254495817));
#76960=CARTESIAN_POINT('Ctrl Pts',(0.348138580916076,0.00707589771753539,
-0.27846832442183));
#76961=CARTESIAN_POINT('Ctrl Pts',(0.182734252248176,0.296409871720789,
-0.262584394347841));
#76962=CARTESIAN_POINT('Ctrl Pts',(-0.150065942415735,0.31421463595112,
-0.246700464273853));
#76963=CARTESIAN_POINT('Ctrl Pts',(-0.34539607339384,0.0441800496300475,
-0.230816534199865));
#76964=CARTESIAN_POINT('Ctrl Pts',(-0.224324033250605,-0.26632621700842,
-0.214932604125877));
#76965=CARTESIAN_POINT('Ctrl Pts',(0.102244728201643,-0.332861519865864,
-0.199048674051889));
#76966=CARTESIAN_POINT('Ctrl Pts',(0.335146456388876,-0.0944761581462219,
-0.183164743977901));
#76967=CARTESIAN_POINT('Ctrl Pts',(0.261043037650893,0.23045579262935,-0.167280813903913));
#76968=CARTESIAN_POINT('Ctrl Pts',(-0.0522087338317124,0.344274967070772,
-0.151396883829924));
#76969=CARTESIAN_POINT('Ctrl Pts',(-0.317601115841721,0.142720497810793,
-0.135512953755936));
#76970=CARTESIAN_POINT('Ctrl Pts',(-0.292115037072835,-0.189579887209652,
-0.119629023681948));
#76971=CARTESIAN_POINT('Ctrl Pts',(0.00108660914303244,-0.348203443840996,
-0.103745093607961));
#76972=CARTESIAN_POINT('Ctrl Pts',(0.293061778238414,-0.187871440927789,
-0.0878611635339722));
#76973=CARTESIAN_POINT('Ctrl Pts',(0.31702060395061,0.144599030699003,-0.0719772334599843));
#76974=CARTESIAN_POINT('Ctrl Pts',(0.04967936712779,0.344541914343505,-0.056093303385996));
#76975=CARTESIAN_POINT('Ctrl Pts',(-0.157537689676105,0.267491347263654,
-0.045504016670004));
#76976=CARTESIAN_POINT('Ctrl Pts',(-0.221960127786206,0.193651371357618,
-0.0402093733120079));
#76977=CARTESIAN_POINT('Ctrl Pts',(0.159723474619028,-0.224219139087579,
-1.98281477796869));
#76978=CARTESIAN_POINT('Ctrl Pts',(0.234354202431277,-0.171059949578467,
-1.97751753969362));
#76979=CARTESIAN_POINT('Ctrl Pts',(0.325024989412419,0.0146796255222407,
-1.96692565806054));
#76980=CARTESIAN_POINT('Ctrl Pts',(0.163460568766758,0.281648170320817,
-1.95103913306949));
#76981=CARTESIAN_POINT('Ctrl Pts',(-0.147960065074204,0.289744587841742,
-1.9351552029955));
#76982=CARTESIAN_POINT('Ctrl Pts',(-0.323765289291095,0.0328288676465,-1.91927127292151));
#76983=CARTESIAN_POINT('Ctrl Pts',(-0.203021509206835,-0.254373192032829,
-1.90338734284752));
#76984=CARTESIAN_POINT('Ctrl Pts',(0.103722739471405,-0.308442852319218,
-1.88750341277353));
#76985=CARTESIAN_POINT('Ctrl Pts',(0.315439958011422,-0.0800186606160754,
-1.87161948269955));
#76986=CARTESIAN_POINT('Ctrl Pts',(0.238200950425248,0.22173790806543,-1.85573555262556));
#76987=CARTESIAN_POINT('Ctrl Pts',(-0.0572473397758462,0.320353319846208,
-1.83985162255157));
#76988=CARTESIAN_POINT('Ctrl Pts',(-0.300252092377886,0.125514278762123,
-1.82396769247758));
#76989=CARTESIAN_POINT('Ctrl Pts',(-0.268208772437333,-0.184307727654305,
-1.8080837624036));
#76990=CARTESIAN_POINT('Ctrl Pts',(0.00953025680760637,-0.325290536218316,
-1.7921998323296));
#76991=CARTESIAN_POINT('Ctrl Pts',(0.278538778324083,-0.168288947764529,
-1.77631590225562));
#76992=CARTESIAN_POINT('Ctrl Pts',(0.292389227805628,0.142876014820982,
-1.76043197218163));
#76993=CARTESIAN_POINT('Ctrl Pts',(0.0383935874989864,0.323157669654262,
-1.74454804210764));
#76994=CARTESIAN_POINT('Ctrl Pts',(-0.250772844499381,0.20740773377436,
-1.72866411203365));
#76995=CARTESIAN_POINT('Ctrl Pts',(-0.310216361684961,-0.098340187342182,
-1.71278018195966));
#76996=CARTESIAN_POINT('Ctrl Pts',(-0.0854831198584704,-0.314002565141601,
-1.69689625188568));
#76997=CARTESIAN_POINT('Ctrl Pts',(0.217557770389958,-0.242019828424955,
-1.68101232181169));
#76998=CARTESIAN_POINT('Ctrl Pts',(0.321302726963141,0.0516675662251906,
-1.6651283917377));
#76999=CARTESIAN_POINT('Ctrl Pts',(0.130715158019189,0.29802437172297,-1.64924446166371));
#77000=CARTESIAN_POINT('Ctrl Pts',(-0.179615316850372,0.271373022847792,
-1.63336053158972));
#77001=CARTESIAN_POINT('Ctrl Pts',(-0.325407413866073,-0.00387225544248687,
-1.61747660151573));
#77002=CARTESIAN_POINT('Ctrl Pts',(-0.173106847615926,-0.275570315065653,
-1.60159267144175));
#77003=CARTESIAN_POINT('Ctrl Pts',(0.137769949459867,-0.294829476803729,
-1.58570874136776));
#77004=CARTESIAN_POINT('Ctrl Pts',(0.322441228893183,-0.0440071952855393,
-1.56982481129377));
#77005=CARTESIAN_POINT('Ctrl Pts',(0.211737048142804,0.247128310312073,
-1.55394088121978));
#77006=CARTESIAN_POINT('Ctrl Pts',(-0.0929309387808109,0.311879495878635,
-1.53805695114579));
#77007=CARTESIAN_POINT('Ctrl Pts',(-0.312468624913705,0.0909304006917473,
-1.52217302107181));
#77008=CARTESIAN_POINT('Ctrl Pts',(-0.245766352878728,-0.213316382673595,
-1.50628909099782));
#77009=CARTESIAN_POINT('Ctrl Pts',(0.0460726047514509,-0.322152594926988,
-1.49040516092383));
#77010=CARTESIAN_POINT('Ctrl Pts',(0.295706299501574,-0.135877753001558,
-1.47452123084984));
#77011=CARTESIAN_POINT('Ctrl Pts',(0.274455329201714,0.174869241430234,
-1.45863730077585));
#77012=CARTESIAN_POINT('Ctrl Pts',(0.0017868542796178,0.325425546750295,
-1.44275337070187));
#77013=CARTESIAN_POINT('Ctrl Pts',(-0.272518486085944,0.177872578176609,
-1.42686944062788));
#77014=CARTESIAN_POINT('Ctrl Pts',(-0.297180586021304,-0.1326223156856,
-1.41098551055389));
#77015=CARTESIAN_POINT('Ctrl Pts',(-0.0496074862356628,-0.321627232421633,
-1.3951015804799));
#77016=CARTESIAN_POINT('Ctrl Pts',(0.243409039393625,-0.216002358476167,
-1.37921765040591));
#77017=CARTESIAN_POINT('Ctrl Pts',(0.313448319636893,0.0874936011523395,
-1.36333372033192));
#77018=CARTESIAN_POINT('Ctrl Pts',(0.0963501827258152,0.310840186614447,
-1.34744979025794));
#77019=CARTESIAN_POINT('Ctrl Pts',(-0.20901048704009,0.249438560838261,
-1.33156586018395));
#77020=CARTESIAN_POINT('Ctrl Pts',(-0.322905043743439,-0.0404637127664561,
-1.31568193010996));
#77021=CARTESIAN_POINT('Ctrl Pts',(-0.140999258131951,-0.293298804177649,
-1.29979800003597));
#77022=CARTESIAN_POINT('Ctrl Pts',(0.170070285152855,-0.277454640317703,
-1.28391406996198));
#77023=CARTESIAN_POINT('Ctrl Pts',(0.325345270438228,-0.0074454233778606,
-1.268030139888));
#77024=CARTESIAN_POINT('Ctrl Pts',(0.18258451973613,0.269384246901198,-1.25214620981401));
#77025=CARTESIAN_POINT('Ctrl Pts',(-0.127434576680288,0.299441827392426,
-1.23626227974002));
#77026=CARTESIAN_POINT('Ctrl Pts',(-0.320715975327185,0.0551927757567259,
-1.22037834966603));
#77027=CARTESIAN_POINT('Ctrl Pts',(-0.220202349319727,-0.239616161140838,
-1.20449441959204));
#77028=CARTESIAN_POINT('Ctrl Pts',(0.082029805305883,-0.314922356093178,
-1.18861048951806));
#77029=CARTESIAN_POINT('Ctrl Pts',(0.309117749707331,-0.101740828292656,
-1.17272655944407));
#77030=CARTESIAN_POINT('Ctrl Pts',(0.253035338145952,0.204641386271602,
-1.15684262937008));
#77031=CARTESIAN_POINT('Ctrl Pts',(-0.0348425844845974,0.323559845518928,
-1.14095869929609));
#77032=CARTESIAN_POINT('Ctrl Pts',(-0.290802614789294,0.146078124842525,
-1.1250747692221));
#77033=CARTESIAN_POINT('Ctrl Pts',(-0.28037004867153,-0.1652198993273,-1.10919083914812));
#77034=CARTESIAN_POINT('Ctrl Pts',(-0.0131017409672661,-0.3251666091551,
-1.09330690907413));
#77035=CARTESIAN_POINT('Ctrl Pts',(0.266168545455288,-0.18724124742165,
-1.07742297900014));
#77036=CARTESIAN_POINT('Ctrl Pts',(0.301612517038136,0.12220830123899,-1.06153904892615));
#77037=CARTESIAN_POINT('Ctrl Pts',(0.0607613748871524,0.319707733168315,
-1.04565511885216));
#77038=CARTESIAN_POINT('Ctrl Pts',(-0.235750822547378,0.224335750592797,
-1.02977118877818));
#77039=CARTESIAN_POINT('Ctrl Pts',(-0.316301159485464,-0.0765412035047192,
-1.01388725870419));
#77040=CARTESIAN_POINT('Ctrl Pts',(-0.107100707257433,-0.307301835059209,
-0.998003328630197));
#77041=CARTESIAN_POINT('Ctrl Pts',(0.200210401594721,-0.256555597130681,
-0.982119398556207));
#77042=CARTESIAN_POINT('Ctrl Pts',(0.324116802238711,0.029210919745057,
-0.96623546848222));
#77043=CARTESIAN_POINT('Ctrl Pts',(0.151112817276033,0.288218486188343,
-0.950351538408232));
#77044=CARTESIAN_POINT('Ctrl Pts',(-0.160319550719043,0.283200672638755,
-0.934467608334243));
#77045=CARTESIAN_POINT('Ctrl Pts',(-0.32488961692817,0.0187540965675897,
-0.918583678260256));
#77046=CARTESIAN_POINT('Ctrl Pts',(-0.191841353030792,-0.262872354181862,
-0.902699748186266));
#77047=CARTESIAN_POINT('Ctrl Pts',(0.116945069796483,-0.303691998538148,
-0.88681581811228));
#77048=CARTESIAN_POINT('Ctrl Pts',(0.318602810839161,-0.0663115996729461,
-0.870931888038291));
#77049=CARTESIAN_POINT('Ctrl Pts',(0.228401312347713,0.231814192498305,
-0.855047957964302));
#77050=CARTESIAN_POINT('Ctrl Pts',(-0.0710294555115186,0.317584312861226,
-0.839164027890315));
#77051=CARTESIAN_POINT('Ctrl Pts',(-0.305392991805803,0.11242819878349,
-0.823280097816326));
#77052=CARTESIAN_POINT('Ctrl Pts',(-0.259998273260052,-0.195718872946862,
-0.807396167742339));
#77053=CARTESIAN_POINT('Ctrl Pts',(0.0235704215729706,-0.324575745478112,
-0.79151223766835));
#77054=CARTESIAN_POINT('Ctrl Pts',(0.285547199819738,-0.156101812932796,
-0.775628307594363));
#77055=CARTESIAN_POINT('Ctrl Pts',(0.285945656233808,0.155370721201957,
-0.759744377520373));
#77056=CARTESIAN_POINT('Ctrl Pts',(0.0244007808967447,0.324514377520363,
-0.743860447446387));
#77057=CARTESIAN_POINT('Ctrl Pts',(-0.259496669854845,0.196383445483687,
-0.727976517372397));
#77058=CARTESIAN_POINT('Ctrl Pts',(-0.305679643053672,-0.111646473963038,
-0.71209258729841));
#77059=CARTESIAN_POINT('Ctrl Pts',(-0.0718417717165509,-0.317401542470144,
-0.696208657224421));
#77060=CARTESIAN_POINT('Ctrl Pts',(0.227807461437338,-0.232397805151584,
-0.680324727150434));
#77061=CARTESIAN_POINT('Ctrl Pts',(0.318771428192673,0.0654962280883837,
-0.664440797076445));
#77062=CARTESIAN_POINT('Ctrl Pts',(0.117721691828191,0.303391797184606,
-0.648556867002457));
#77063=CARTESIAN_POINT('Ctrl Pts',(-0.191168158574021,0.263362325462871,
-0.632672936928469));
#77064=CARTESIAN_POINT('Ctrl Pts',(-0.324936536451937,-0.0179227956647243,
-0.616789006854481));
#77065=CARTESIAN_POINT('Ctrl Pts',(-0.161043603131856,-0.282789563485085,
-0.600905076780493));
#77066=CARTESIAN_POINT('Ctrl Pts',(0.150374907310509,-0.288604169368921,
-0.585021146706504));
#77067=CARTESIAN_POINT('Ctrl Pts',(0.32404100440495,-0.030040086387625,
-0.569137216632518));
#77068=CARTESIAN_POINT('Ctrl Pts',(0.200866151243303,0.256042513286972,
-0.553253286558528));
#77069=CARTESIAN_POINT('Ctrl Pts',(-0.106314116042351,0.307574849517642,
-0.537369356484541));
#77070=CARTESIAN_POINT('Ctrl Pts',(-0.316104291328467,0.0773502186842683,
-0.521485426410552));
#77071=CARTESIAN_POINT('Ctrl Pts',(-0.236324020455074,-0.223731841006614,
-0.505601496336565));
#77072=CARTESIAN_POINT('Ctrl Pts',(0.059943194487078,-0.319862146494561,
-0.489717566262575));
#77073=CARTESIAN_POINT('Ctrl Pts',(0.301298856371324,-0.122979585629188,
-0.473833636188588));
#77074=CARTESIAN_POINT('Ctrl Pts',(0.266646736422932,0.186559634618336,
-0.4579497061146));
#77075=CARTESIAN_POINT('Ctrl Pts',(-0.0122697498320095,0.325199066059707,
-0.442065776040612));
#77076=CARTESIAN_POINT('Ctrl Pts',(-0.279946411175029,0.165936693460959,
-0.426181845966624));
#77077=CARTESIAN_POINT('Ctrl Pts',(-0.291175407958708,-0.145333619775284,
-0.410297915892635));
#77078=CARTESIAN_POINT('Ctrl Pts',(-0.035670307984215,-0.323469640754012,
-0.394413985818648));
#77079=CARTESIAN_POINT('Ctrl Pts',(0.252510929555415,-0.205288114687303,
-0.378530055744659));
#77080=CARTESIAN_POINT('Ctrl Pts',(0.309377043795816,0.100949608463896,
-0.362646125670671));
#77081=CARTESIAN_POINT('Ctrl Pts',(0.0828352767616206,0.314711449867035,
-0.346762195596683));
#77082=CARTESIAN_POINT('Ctrl Pts',(-0.219588567404444,0.240178770654608,
-0.330878265522695));
#77083=CARTESIAN_POINT('Ctrl Pts',(-0.320856130818992,-0.0543720333637462,
-0.314994335448707));
#77084=CARTESIAN_POINT('Ctrl Pts',(-0.128200303776929,-0.299114803403398,
-0.299110405374719));
#77085=CARTESIAN_POINT('Ctrl Pts',(0.181894720658038,-0.26985051077302,
-0.283226475300731));
#77086=CARTESIAN_POINT('Ctrl Pts',(0.325363205338246,0.00661298944795382,
-0.267342545226742));
#77087=CARTESIAN_POINT('Ctrl Pts',(0.170779698935137,0.277018610529187,
-0.251458615152755));
#77088=CARTESIAN_POINT('Ctrl Pts',(-0.140248563971308,0.293658579431881,
-0.235574685078766));
#77089=CARTESIAN_POINT('Ctrl Pts',(-0.322800113836719,0.0412897717966501,
-0.219690755004778));
#77090=CARTESIAN_POINT('Ctrl Pts',(-0.209648658590971,-0.248903041436704,
-0.20380682493079));
#77091=CARTESIAN_POINT('Ctrl Pts',(0.0955558341425081,-0.31108557618733,
-0.187922894856802));
#77092=CARTESIAN_POINT('Ctrl Pts',(0.313221031181045,-0.0882954872786916,
-0.172038964782814));
#77093=CARTESIAN_POINT('Ctrl Pts',(0.243965489943215,0.215379275636006,
-0.156155034708826));
#77094=CARTESIAN_POINT('Ctrl Pts',(-0.0487932160274783,0.321752350771107,
-0.140271104634837));
#77095=CARTESIAN_POINT('Ctrl Pts',(-0.296823514352684,0.13338366150916,
-0.124387174560849));
#77096=CARTESIAN_POINT('Ctrl Pts',(-0.273004745809628,-0.17717748951549,
-0.108503244486861));
#77097=CARTESIAN_POINT('Ctrl Pts',(0.00101552270592162,-0.325423824902742,
-0.0926193144128733));
#77098=CARTESIAN_POINT('Ctrl Pts',(0.273889550761288,-0.175580810523597,
-0.0767353843388852));
#77099=CARTESIAN_POINT('Ctrl Pts',(0.296280979798966,0.135139299968517,
-0.0608514542648971));
#77100=CARTESIAN_POINT('Ctrl Pts',(0.0464293215803309,0.322001834238538,
-0.044967524190909));
#77101=CARTESIAN_POINT('Ctrl Pts',(-0.147231506314883,0.249991948369916,
-0.0343782374749169));
#77102=CARTESIAN_POINT('Ctrl Pts',(-0.207439400837955,0.180982615420753,
-0.0290835941169209));
#77103=CARTESIAN_POINT('Ctrl Pts',(0.14854285534998,-0.208523832978368,
-1.9716889987736));
#77104=CARTESIAN_POINT('Ctrl Pts',(0.217949443407999,-0.159085778762425,
-1.96639176049853));
#77105=CARTESIAN_POINT('Ctrl Pts',(0.302273288898672,0.0136520539372401,
-1.95579987886546));
#77106=CARTESIAN_POINT('Ctrl Pts',(0.15201835346783,0.261932840638111,-1.9399133538744));
#77107=CARTESIAN_POINT('Ctrl Pts',(-0.137602882709094,0.269462510146818,
-1.92402942380041));
#77108=CARTESIAN_POINT('Ctrl Pts',(-0.301101767596918,0.0305308518347021,
-1.90814549372642));
#77109=CARTESIAN_POINT('Ctrl Pts',(-0.188810034010194,-0.23656710673976,
-1.89226156365243));
#77110=CARTESIAN_POINT('Ctrl Pts',(0.0964621632640678,-0.286851898915114,
-1.87637763357845));
#77111=CARTESIAN_POINT('Ctrl Pts',(0.293359208258245,-0.0744173663736239,
-1.86049370350446));
#77112=CARTESIAN_POINT('Ctrl Pts',(0.2215269196193,0.206216287755652,-1.84460977343047));
#77113=CARTESIAN_POINT('Ctrl Pts',(-0.0532400345771204,0.29792863550147,
-1.82872584335648));
#77114=CARTESIAN_POINT('Ctrl Pts',(-0.27923449094128,0.116728298072583,
-1.81284191328249));
#77115=CARTESIAN_POINT('Ctrl Pts',(-0.249434198590917,-0.171406214359773,
-1.79695798320851));
#77116=CARTESIAN_POINT('Ctrl Pts',(0.00886314026036145,-0.302520247467981,
-1.78107405313452));
#77117=CARTESIAN_POINT('Ctrl Pts',(0.259041105614823,-0.156508746659887,
-1.76519012306053));
#77118=CARTESIAN_POINT('Ctrl Pts',(0.271922025709858,0.132874715211126,
-1.74930619298654));
#77119=CARTESIAN_POINT('Ctrl Pts',(0.0357060421320745,0.300536681243538,
-1.73342226291256));
#77120=CARTESIAN_POINT('Ctrl Pts',(-0.233218782993697,0.192889223515808,
-1.71753833283856));
#77121=CARTESIAN_POINT('Ctrl Pts',(-0.288501262891236,-0.0914563889766494,
-1.70165440276458));
#77122=CARTESIAN_POINT('Ctrl Pts',(-0.0794993142885749,-0.29202243267374,
-1.68577047269059));
#77123=CARTESIAN_POINT('Ctrl Pts',(0.202328759090555,-0.225078476731758,
-1.6698865426166));
#77124=CARTESIAN_POINT('Ctrl Pts',(0.298811584262604,0.0480508443381929,
-1.65400261254261));
#77125=CARTESIAN_POINT('Ctrl Pts',(0.121565116561649,0.277162710398109,
-1.63811868246863));
#77126=CARTESIAN_POINT('Ctrl Pts',(-0.167042271608378,0.252376951947197,
-1.62223475239464));
#77127=CARTESIAN_POINT('Ctrl Pts',(-0.302628943697925,-0.00360119814225005,
-1.60635082232065));
#77128=CARTESIAN_POINT('Ctrl Pts',(-0.160989394244243,-0.256280434339293,
-1.59046689224666));
#77129=CARTESIAN_POINT('Ctrl Pts',(0.128126073659514,-0.274191457644064,
-1.57458296217267));
#77130=CARTESIAN_POINT('Ctrl Pts',(0.299870391228289,-0.040926698215461,
-1.55869903209869));
#77131=CARTESIAN_POINT('Ctrl Pts',(0.196915486527744,0.229829365652916,
-1.5428151020247));
#77132=CARTESIAN_POINT('Ctrl Pts',(-0.0864257870033305,0.290047977940778,
-1.52693117195071));
#77133=CARTESIAN_POINT('Ctrl Pts',(-0.290595868031748,0.0845652862804702,
-1.51104724187672));
#77134=CARTESIAN_POINT('Ctrl Pts',(-0.228562745035647,-0.198384267878241,
-1.49516331180273));
#77135=CARTESIAN_POINT('Ctrl Pts',(0.042847529328519,-0.299601961596439,
-1.47927938172874));
#77136=CARTESIAN_POINT('Ctrl Pts',(0.275006902884562,-0.126366330669504,
-1.46339545165476));
#77137=CARTESIAN_POINT('Ctrl Pts',(0.255243497318609,0.162628420755865,
-1.44751152158077));
#77138=CARTESIAN_POINT('Ctrl Pts',(0.00166177474802338,0.302645807282969,
-1.43162759150678));
#77139=CARTESIAN_POINT('Ctrl Pts',(-0.25344223293047,0.165421524380412,
-1.41574366143279));
#77140=CARTESIAN_POINT('Ctrl Pts',(-0.276377989569012,-0.123338773477437,
-1.3998597313588));
#77141=CARTESIAN_POINT('Ctrl Pts',(-0.046134969638971,-0.299113374387668,
-1.38397580128481));
#77142=CARTESIAN_POINT('Ctrl Pts',(0.226370443140969,-0.200882225777455,
-1.36809187121083));
#77143=CARTESIAN_POINT('Ctrl Pts',(0.291506984271239,0.0813690621933957,
-1.35220794113684));
#77144=CARTESIAN_POINT('Ctrl Pts',(0.0896056843849767,0.289081420169215,
-1.33632401106285));
#77145=CARTESIAN_POINT('Ctrl Pts',(-0.194379784293312,0.231977898988746,
-1.32044008098886));
#77146=CARTESIAN_POINT('Ctrl Pts',(-0.300301739108585,-0.037631258941289,
-1.30455615091488));
#77147=CARTESIAN_POINT('Ctrl Pts',(-0.13112933120886,-0.272767931872252,
-1.28867222084089));
#77148=CARTESIAN_POINT('Ctrl Pts',(0.158165390698187,-0.258032857106295,
-1.2727882907669));
#77149=CARTESIAN_POINT('Ctrl Pts',(0.302571150300708,-0.0069242448580246,
-1.25690436069291));
#77150=CARTESIAN_POINT('Ctrl Pts',(0.169803630737432,0.250527390018603,
-1.24102043061892));
#77151=CARTESIAN_POINT('Ctrl Pts',(-0.118514175424474,0.278480944383283,
-1.22513650054494));
#77152=CARTESIAN_POINT('Ctrl Pts',(-0.298265905153167,0.051329289731205,
-1.20925257047095));
#77153=CARTESIAN_POINT('Ctrl Pts',(-0.204788217891854,-0.222843065797045,
-1.19336864039696));
#77154=CARTESIAN_POINT('Ctrl Pts',(0.0762877312367668,-0.292877838396651,
-1.17748471032297));
#77155=CARTESIAN_POINT('Ctrl Pts',(0.287479553587276,-0.0946189855705929,
-1.16160078024898));
#77156=CARTESIAN_POINT('Ctrl Pts',(0.23532290242432,0.190316519923368,-1.14571685017499));
#77157=CARTESIAN_POINT('Ctrl Pts',(-0.0324036087961405,0.300910704857994,
-1.12983292010101));
#77158=CARTESIAN_POINT('Ctrl Pts',(-0.270446475366719,0.135852678011388,
-1.11394899002702));
#77159=CARTESIAN_POINT('Ctrl Pts',(-0.260744187312589,-0.153654531152992,
-1.09806505995303));
#77160=CARTESIAN_POINT('Ctrl Pts',(-0.0121846210644688,-0.302404995280605,
-1.08218112987904));
#77161=CARTESIAN_POINT('Ctrl Pts',(0.247536787191636,-0.174134388183351,
-1.06629719980505));
#77162=CARTESIAN_POINT('Ctrl Pts',(0.280499686079339,0.113653738480264,
-1.05041326973106));
#77163=CARTESIAN_POINT('Ctrl Pts',(0.0565080877576434,0.297328239794208,
-1.03452933965708));
#77164=CARTESIAN_POINT('Ctrl Pts',(-0.219248300325429,0.208632281695709,
-1.01864540958309));
#77165=CARTESIAN_POINT('Ctrl Pts',(-0.29416012575826,-0.0711833307385401,
-1.0027614795091));
#77166=CARTESIAN_POINT('Ctrl Pts',(-0.0996036738116745,-0.285790752692184,
-0.986877549435108));
#77167=CARTESIAN_POINT('Ctrl Pts',(0.186195703509339,-0.238596743808063,
-0.970993619361121));
#77168=CARTESIAN_POINT('Ctrl Pts',(0.30142867469092,0.0271661597437678,
-0.955109689287132));
#77169=CARTESIAN_POINT('Ctrl Pts',(0.140534942729621,0.268043235380283,
-0.939225759213145));
#77170=CARTESIAN_POINT('Ctrl Pts',(-0.14909720621239,0.263376668026626,
-0.923341829139156));
#77171=CARTESIAN_POINT('Ctrl Pts',(-0.302147392468019,0.0174413126204732,
-0.907457899065168));
#77172=CARTESIAN_POINT('Ctrl Pts',(-0.178412487089747,-0.244471328813009,
-0.891573968991181));
#77173=CARTESIAN_POINT('Ctrl Pts',(0.108758932449388,-0.282433604186218,
-0.875690038917191));
#77174=CARTESIAN_POINT('Ctrl Pts',(0.296300661862387,-0.061669797640818,
-0.859806108843205));
#77175=CARTESIAN_POINT('Ctrl Pts',(0.212413254737507,0.215587233789401,
-0.843922178769215));
#77176=CARTESIAN_POINT('Ctrl Pts',(-0.0660574042782473,0.295353458590158,
-0.828038248695228));
#77177=CARTESIAN_POINT('Ctrl Pts',(-0.284015528180242,0.10455824172989,
-0.812154318621239));
#77178=CARTESIAN_POINT('Ctrl Pts',(-0.241798433124689,-0.18201858119322,
-0.796270388547252));
#77179=CARTESIAN_POINT('Ctrl Pts',(0.0219204955978022,-0.301855491972392,
-0.780386458473262));
#77180=CARTESIAN_POINT('Ctrl Pts',(0.265558938656859,-0.145174709438629,
-0.764502528399276));
#77181=CARTESIAN_POINT('Ctrl Pts',(0.2659295031817,0.144494794019306,-0.748618598325286));
#77182=CARTESIAN_POINT('Ctrl Pts',(0.0226927298934404,0.301798419762482,
-0.7327346682513));
#77183=CARTESIAN_POINT('Ctrl Pts',(-0.241331941882621,0.182636633752132,
-0.71685073817731));
#77184=CARTESIAN_POINT('Ctrl Pts',(-0.284282113883749,-0.103831237529635,
-0.700966808103323));
#77185=CARTESIAN_POINT('Ctrl Pts',(-0.0668128584707501,-0.295183482099042,
-0.685082878029334));
#77186=CARTESIAN_POINT('Ctrl Pts',(0.2118609733018,-0.216129993644475,-0.669198947955347));
#77187=CARTESIAN_POINT('Ctrl Pts',(0.29645747602644,0.0609115019448947,
-0.653315017881357));
#77188=CARTESIAN_POINT('Ctrl Pts',(0.109481191055346,0.282154416882402,
-0.637431087807371));
#77189=CARTESIAN_POINT('Ctrl Pts',(-0.177786416143992,0.244927002177829,
-0.621547157733382));
#77190=CARTESIAN_POINT('Ctrl Pts',(-0.302191027632159,-0.0166682026561393,
-0.605663227659394));
#77191=CARTESIAN_POINT('Ctrl Pts',(-0.149770575064891,-0.262994336452061,
-0.589779297585406));
#77192=CARTESIAN_POINT('Ctrl Pts',(0.139848686351021,-0.268401920796062,
-0.573895367511417));
#77193=CARTESIAN_POINT('Ctrl Pts',(0.301358182694155,-0.0279372848457049,
-0.558011437437431));
#77194=CARTESIAN_POINT('Ctrl Pts',(0.186805550780861,0.238119575756467,
-0.542127507363441));
#77195=CARTESIAN_POINT('Ctrl Pts',(-0.0988721438636844,0.286044656179471,
-0.526243577289453));
#77196=CARTESIAN_POINT('Ctrl Pts',(-0.29397703834273,0.0719357149768477,
-0.510359647215465));
#77197=CARTESIAN_POINT('Ctrl Pts',(-0.21978137446555,-0.208070645689991,
-0.494475717141477));
#77198=CARTESIAN_POINT('Ctrl Pts',(0.0557471798628727,-0.297471844210775,
-0.478591787067489));
#77199=CARTESIAN_POINT('Ctrl Pts',(0.280207981612165,-0.114371033078817,
-0.462707856993501));
#77200=CARTESIAN_POINT('Ctrl Pts',(0.247981504863259,0.173500488174049,
-0.446823926919513));
#77201=CARTESIAN_POINT('Ctrl Pts',(-0.0114108691839076,0.302435180206757,
-0.430939996845525));
#77202=CARTESIAN_POINT('Ctrl Pts',(-0.26035020437731,0.154321149804791,
-0.415056066771537));
#77203=CARTESIAN_POINT('Ctrl Pts',(-0.270793173070181,-0.135160288187202,
-0.399172136697548));
#77204=CARTESIAN_POINT('Ctrl Pts',(-0.0331733917749176,-0.300826814413094,
-0.383288206623561));
#77205=CARTESIAN_POINT('Ctrl Pts',(0.234835202356476,-0.19091797744696,
-0.367404276549572));
#77206=CARTESIAN_POINT('Ctrl Pts',(0.287720697128454,0.0938831510111875,
-0.351520346475584));
#77207=CARTESIAN_POINT('Ctrl Pts',(0.0770368198113984,0.292681695574709,
-0.335636416401596));
#77208=CARTESIAN_POINT('Ctrl Pts',(-0.204217400618593,0.223366292729226,
-0.319752486327608));
#77209=CARTESIAN_POINT('Ctrl Pts',(-0.298396249781567,-0.0505659991826476,
-0.30386855625362));
#77210=CARTESIAN_POINT('Ctrl Pts',(-0.119226301739186,-0.278176812024444,
-0.287984626179632));
#77211=CARTESIAN_POINT('Ctrl Pts',(0.169162117491358,-0.250961015489323,
-0.272100696105643));
#77212=CARTESIAN_POINT('Ctrl Pts',(0.302587829760414,0.00615008117837171,
-0.256216766031655));
#77213=CARTESIAN_POINT('Ctrl Pts',(0.158825145622099,0.257627349337584,
-0.240332835957668));
#77214=CARTESIAN_POINT('Ctrl Pts',(-0.13043118552688,0.273102522912643,
-0.224448905883679));
#77215=CARTESIAN_POINT('Ctrl Pts',(-0.3002041542796,0.0383994939632529,
-0.208564975809691));
#77216=CARTESIAN_POINT('Ctrl Pts',(-0.194973283931337,-0.231479865864986,
-0.192681045735703));
#77217=CARTESIAN_POINT('Ctrl Pts',(0.0888669400833733,-0.289309632508797,
-0.176797115661715));
#77218=CARTESIAN_POINT('Ctrl Pts',(0.291295605973215,-0.0821148164111612,
-0.160913185587726));
#77219=CARTESIAN_POINT('Ctrl Pts',(0.226887942235539,0.200302758642664,
-0.145029255513739));
#77220=CARTESIAN_POINT('Ctrl Pts',(-0.0453776982232441,0.299229734471443,
-0.12914532543975));
#77221=CARTESIAN_POINT('Ctrl Pts',(-0.276045912863647,0.124046825207526,
-0.113261395365762));
#77222=CARTESIAN_POINT('Ctrl Pts',(-0.253894454546419,-0.164775091821329,
-0.0973774652917741));
#77223=CARTESIAN_POINT('Ctrl Pts',(0.000944436268810345,-0.302644205964487,
-0.0814935352177862));
#77224=CARTESIAN_POINT('Ctrl Pts',(0.254717323284163,-0.163290180119405,
-0.0656096051437982));
#77225=CARTESIAN_POINT('Ctrl Pts',(0.275541355647321,0.125679569238032,
-0.0497256750698101));
#77226=CARTESIAN_POINT('Ctrl Pts',(0.0431792760328719,0.29946175413357,
-0.0338417449958219));
#77227=CARTESIAN_POINT('Ctrl Pts',(-0.136925322953661,0.23249254947618,
-0.0232524582798299));
#77228=CARTESIAN_POINT('Ctrl Pts',(-0.192918673889705,0.168313859483889,
-0.0179578149218338));
#77229=CARTESIAN_POINT('Ctrl Pts',(0.137362236080932,-0.192828526869157,
-1.96056321957851));
#77230=CARTESIAN_POINT('Ctrl Pts',(0.201544684384722,-0.147111607946385,
-1.95526598130344));
#77231=CARTESIAN_POINT('Ctrl Pts',(0.279521588384925,0.0126244823522396,
-1.94467409967037));
#77232=CARTESIAN_POINT('Ctrl Pts',(0.140576138168903,0.242217510955405,
-1.9287875746793));
#77233=CARTESIAN_POINT('Ctrl Pts',(-0.127245700343985,0.249180432451894,
-1.91290364460532));
#77234=CARTESIAN_POINT('Ctrl Pts',(-0.278438245902744,0.0282328360229038,
-1.89701971453133));
#77235=CARTESIAN_POINT('Ctrl Pts',(-0.174598558813552,-0.218761021446692,
-1.88113578445734));
#77236=CARTESIAN_POINT('Ctrl Pts',(0.0892015870567291,-0.265260945511011,
-1.86525185438335));
#77237=CARTESIAN_POINT('Ctrl Pts',(0.271278458505069,-0.0688160721311721,
-1.84936792430937));
#77238=CARTESIAN_POINT('Ctrl Pts',(0.204852888813353,0.190694667445875,
-1.83348399423537));
#77239=CARTESIAN_POINT('Ctrl Pts',(-0.0492327293783949,0.275503951156731,
-1.81760006416139));
#77240=CARTESIAN_POINT('Ctrl Pts',(-0.258216889504675,0.107942317383044,
-1.8017161340874));
#77241=CARTESIAN_POINT('Ctrl Pts',(-0.2306596247445,-0.158504701065241,
-1.78583220401341));
#77242=CARTESIAN_POINT('Ctrl Pts',(0.00819602371311662,-0.279749958717647,
-1.76994827393942));
#77243=CARTESIAN_POINT('Ctrl Pts',(0.239543432905563,-0.144728545555244,
-1.75406434386544));
#77244=CARTESIAN_POINT('Ctrl Pts',(0.251454823614088,0.122873415601269,
-1.73818041379144));
#77245=CARTESIAN_POINT('Ctrl Pts',(0.0330184967651629,0.277915692832815,
-1.72229648371746));
#77246=CARTESIAN_POINT('Ctrl Pts',(-0.215664721488012,0.178370713257257,
-1.70641255364347));
#77247=CARTESIAN_POINT('Ctrl Pts',(-0.266786164097509,-0.0845725906111169,
-1.69052862356948));
#77248=CARTESIAN_POINT('Ctrl Pts',(-0.0735155087186798,-0.270042300205881,
-1.67464469349549));
#77249=CARTESIAN_POINT('Ctrl Pts',(0.187099747791151,-0.208137125038562,
-1.65876076342151));
#77250=CARTESIAN_POINT('Ctrl Pts',(0.276320441562065,0.0444341224511951,
-1.64287683334751));
#77251=CARTESIAN_POINT('Ctrl Pts',(0.112415075104108,0.256301049073249,
-1.62699290327353));
#77252=CARTESIAN_POINT('Ctrl Pts',(-0.154469226366385,0.233380881046602,
-1.61110897319954));
#77253=CARTESIAN_POINT('Ctrl Pts',(-0.279850473529776,-0.00333014084201356,
-1.59522504312556));
#77254=CARTESIAN_POINT('Ctrl Pts',(-0.14887194087256,-0.236990553612932,
-1.57934111305156));
#77255=CARTESIAN_POINT('Ctrl Pts',(0.118482197859161,-0.2535534384844,-1.56345718297758));
#77256=CARTESIAN_POINT('Ctrl Pts',(0.277299553563392,-0.0378462011453827,
-1.54757325290359));
#77257=CARTESIAN_POINT('Ctrl Pts',(0.182093924912684,0.212530420993761,
-1.5316893228296));
#77258=CARTESIAN_POINT('Ctrl Pts',(-0.0799206352258501,0.268216460002921,
-1.51580539275561));
#77259=CARTESIAN_POINT('Ctrl Pts',(-0.26872311114979,0.0782001718691929,
-1.49992146268163));
#77260=CARTESIAN_POINT('Ctrl Pts',(-0.211359137192565,-0.183452153082888,
-1.48403753260764));
#77261=CARTESIAN_POINT('Ctrl Pts',(0.0396224539055875,-0.27705132826589,
-1.46815360253365));
#77262=CARTESIAN_POINT('Ctrl Pts',(0.25430750626755,-0.116854908337451,
-1.45226967245966));
#77263=CARTESIAN_POINT('Ctrl Pts',(0.236031665435503,0.150387600081495,
-1.43638574238567));
#77264=CARTESIAN_POINT('Ctrl Pts',(0.00153669521642899,0.279866067815646,
-1.42050181231168));
#77265=CARTESIAN_POINT('Ctrl Pts',(-0.234365979774995,0.152970470584214,
-1.4046178822377));
#77266=CARTESIAN_POINT('Ctrl Pts',(-0.255575393116723,-0.114055231269275,
-1.38873395216371));
#77267=CARTESIAN_POINT('Ctrl Pts',(-0.0426624530422791,-0.276599516353704,
-1.37285002208972));
#77268=CARTESIAN_POINT('Ctrl Pts',(0.209331846888312,-0.185762093078744,
-1.35696609201573));
#77269=CARTESIAN_POINT('Ctrl Pts',(0.269565648905586,0.0752445232344523,
-1.34108216194174));
#77270=CARTESIAN_POINT('Ctrl Pts',(0.0828611860441382,0.267322653723983,
-1.32519823186776));
#77271=CARTESIAN_POINT('Ctrl Pts',(-0.179749081546533,0.214517237139231,
-1.30931430179377));
#77272=CARTESIAN_POINT('Ctrl Pts',(-0.277698434473732,-0.0347988051161221,
-1.29343037171978));
#77273=CARTESIAN_POINT('Ctrl Pts',(-0.121259404285768,-0.252237059566854,
-1.27754644164579));
#77274=CARTESIAN_POINT('Ctrl Pts',(0.146260496243518,-0.238611073894888,
-1.2616625115718));
#77275=CARTESIAN_POINT('Ctrl Pts',(0.279797030163189,-0.00640306633818836,
-1.24577858149781));
#77276=CARTESIAN_POINT('Ctrl Pts',(0.157022741738734,0.231670533136009,
-1.22989465142383));
#77277=CARTESIAN_POINT('Ctrl Pts',(-0.10959377416866,0.25752006137414,-1.21401072134984));
#77278=CARTESIAN_POINT('Ctrl Pts',(-0.27581583497915,0.0474658037056839,
-1.19812679127585));
#77279=CARTESIAN_POINT('Ctrl Pts',(-0.189374086463979,-0.206069970453253,
-1.18224286120186));
#77280=CARTESIAN_POINT('Ctrl Pts',(0.0705456571676509,-0.270833320700124,
-1.16635893112788));
#77281=CARTESIAN_POINT('Ctrl Pts',(0.265841357467223,-0.0874971428485293,
-1.15047500105388));
#77282=CARTESIAN_POINT('Ctrl Pts',(0.217610466702688,0.175991653575135,
-1.1345910709799));
#77283=CARTESIAN_POINT('Ctrl Pts',(-0.0299646331076837,0.278261564197058,
-1.11870714090591));
#77284=CARTESIAN_POINT('Ctrl Pts',(-0.250090335944144,0.125627231180252,
-1.10282321083192));
#77285=CARTESIAN_POINT('Ctrl Pts',(-0.241118325953647,-0.142089162978682,
-1.08693928075793));
#77286=CARTESIAN_POINT('Ctrl Pts',(-0.0112675011616718,-0.279643381406111,
-1.07105535068396));
#77287=CARTESIAN_POINT('Ctrl Pts',(0.228905028927986,-0.161027528945051,
-1.05517142060996));
#77288=CARTESIAN_POINT('Ctrl Pts',(0.259386855120543,0.105099175721539,
-1.03928749053597));
#77289=CARTESIAN_POINT('Ctrl Pts',(0.0522548006281345,0.274948746420102,
-1.02340356046198));
#77290=CARTESIAN_POINT('Ctrl Pts',(-0.202745778103481,0.192928812798621,
-1.00751963038799));
#77291=CARTESIAN_POINT('Ctrl Pts',(-0.272019092031057,-0.0658254579723609,
-0.991635700314011));
#77292=CARTESIAN_POINT('Ctrl Pts',(-0.0921066403659162,-0.26427967032516,
-0.975751770240021));
#77293=CARTESIAN_POINT('Ctrl Pts',(0.172181005423957,-0.220637890485445,
-0.959867840166033));
#77294=CARTESIAN_POINT('Ctrl Pts',(0.278740547143128,0.0251213997424785,
-0.943983910092046));
#77295=CARTESIAN_POINT('Ctrl Pts',(0.12995706818321,0.247867984572224,-0.928099980018057));
#77296=CARTESIAN_POINT('Ctrl Pts',(-0.137874861705736,0.243552663414497,
-0.912216049944069));
#77297=CARTESIAN_POINT('Ctrl Pts',(-0.279405168007867,0.0161285286733566,
-0.896332119870082));
#77298=CARTESIAN_POINT('Ctrl Pts',(-0.164983621148702,-0.226070303444157,
-0.880448189796093));
#77299=CARTESIAN_POINT('Ctrl Pts',(0.100572795102292,-0.261175209834287,
-0.864564259722106));
#77300=CARTESIAN_POINT('Ctrl Pts',(0.273998512885612,-0.05702799560869,
-0.848680329648117));
#77301=CARTESIAN_POINT('Ctrl Pts',(0.196425197127302,0.199360275080499,
-0.832796399574128));
#77302=CARTESIAN_POINT('Ctrl Pts',(-0.0610853530449764,0.273122604319091,
-0.816912469500142));
#77303=CARTESIAN_POINT('Ctrl Pts',(-0.26263806455468,0.0966882846762901,
-0.801028539426152));
#77304=CARTESIAN_POINT('Ctrl Pts',(-0.223598592989326,-0.168318289439578,
-0.785144609352165));
#77305=CARTESIAN_POINT('Ctrl Pts',(0.0202705696226342,-0.279135238466673,
-0.769260679278176));
#77306=CARTESIAN_POINT('Ctrl Pts',(0.245570677493981,-0.13424760594446,
-0.753376749204189));
#77307=CARTESIAN_POINT('Ctrl Pts',(0.245913350129593,0.133618866836656,
-0.737492819130199));
#77308=CARTESIAN_POINT('Ctrl Pts',(0.0209846788901358,0.279082462004602,
-0.721608889056213));
#77309=CARTESIAN_POINT('Ctrl Pts',(-0.223167213910397,0.168889822020577,
-0.705724958982223));
#77310=CARTESIAN_POINT('Ctrl Pts',(-0.262884584713825,-0.0960160010962316,
-0.689841028908236));
#77311=CARTESIAN_POINT('Ctrl Pts',(-0.0617839452249487,-0.272965421727941,
-0.673957098834247));
#77312=CARTESIAN_POINT('Ctrl Pts',(0.195914485166261,-0.199862182137365,
-0.65807316876026));
#77313=CARTESIAN_POINT('Ctrl Pts',(0.274143523860207,0.0563267758014057,
-0.642189238686271));
#77314=CARTESIAN_POINT('Ctrl Pts',(0.1012406902825,0.260917036580199,-0.626305308612284));
#77315=CARTESIAN_POINT('Ctrl Pts',(-0.164404673713962,0.226491678892785,
-0.610421378538294));
#77316=CARTESIAN_POINT('Ctrl Pts',(-0.27944551881238,-0.015413609647554,
-0.594537448464308));
#77317=CARTESIAN_POINT('Ctrl Pts',(-0.138497546997926,-0.243199109419036,
-0.578653518390318));
#77318=CARTESIAN_POINT('Ctrl Pts',(0.129322465391532,-0.248199672223202,
-0.562769588316331));
#77319=CARTESIAN_POINT('Ctrl Pts',(0.27867536098336,-0.0258344833037851,
-0.546885658242343));
#77320=CARTESIAN_POINT('Ctrl Pts',(0.172744950318421,0.220196638225962,
-0.531001728168355));
#77321=CARTESIAN_POINT('Ctrl Pts',(-0.0914301716850177,0.264514462841301,
-0.515117798094366));
#77322=CARTESIAN_POINT('Ctrl Pts',(-0.271849785356991,0.0665212112694271,
-0.499233868020378));
#77323=CARTESIAN_POINT('Ctrl Pts',(-0.203238728476024,-0.192409450373368,
-0.483349937946391));
#77324=CARTESIAN_POINT('Ctrl Pts',(0.0515511652386677,-0.275081541926988,
-0.467466007872402));
#77325=CARTESIAN_POINT('Ctrl Pts',(0.259117106853005,-0.105762480528446,
-0.451582077798414));
#77326=CARTESIAN_POINT('Ctrl Pts',(0.229316273303587,0.160441341729761,
-0.435698147724425));
#77327=CARTESIAN_POINT('Ctrl Pts',(-0.0105519885358059,0.279671294353807,
-0.419814217650438));
#77328=CARTESIAN_POINT('Ctrl Pts',(-0.240753997579591,0.142705606148622,
-0.403930287576449));
#77329=CARTESIAN_POINT('Ctrl Pts',(-0.250410938181655,-0.12498695659912,
-0.388046357502461));
#77330=CARTESIAN_POINT('Ctrl Pts',(-0.03067647556562,-0.278183988072175,
-0.372162427428474));
#77331=CARTESIAN_POINT('Ctrl Pts',(0.217159475157536,-0.176547840206616,
-0.356278497354485));
#77332=CARTESIAN_POINT('Ctrl Pts',(0.266064350461092,0.086816693558479,
-0.340394567280497));
#77333=CARTESIAN_POINT('Ctrl Pts',(0.0712383628611763,0.270651941282383,
-0.324510637206509));
#77334=CARTESIAN_POINT('Ctrl Pts',(-0.18884623383274,0.206553814803844,
-0.308626707132521));
#77335=CARTESIAN_POINT('Ctrl Pts',(-0.275936368744142,-0.0467599650015497,
-0.292742777058533));
#77336=CARTESIAN_POINT('Ctrl Pts',(-0.110252299701442,-0.257238820645489,
-0.276858846984545));
#77337=CARTESIAN_POINT('Ctrl Pts',(0.156429514324678,-0.232071520205626,
-0.260974916910556));
#77338=CARTESIAN_POINT('Ctrl Pts',(0.279812454182582,0.00568717290878994,
-0.245090986836568));
#77339=CARTESIAN_POINT('Ctrl Pts',(0.14687059230906,0.238236088145982,-0.229207056762581));
#77340=CARTESIAN_POINT('Ctrl Pts',(-0.120613807082454,0.252546466393404,
-0.213323126688592));
#77341=CARTESIAN_POINT('Ctrl Pts',(-0.277608194722481,0.0355092161298553,
-0.197439196614604));
#77342=CARTESIAN_POINT('Ctrl Pts',(-0.180297909271702,-0.214056690293268,
-0.181555266540616));
#77343=CARTESIAN_POINT('Ctrl Pts',(0.0821780460242392,-0.267533688830265,
-0.165671336466628));
#77344=CARTESIAN_POINT('Ctrl Pts',(0.269370180765385,-0.0759341455436309,
-0.14978740639264));
#77345=CARTESIAN_POINT('Ctrl Pts',(0.209810394527861,0.18522624164932,-0.133903476318652));
#77346=CARTESIAN_POINT('Ctrl Pts',(-0.0419621804190102,0.27670711817178,
-0.118019546244663));
#77347=CARTESIAN_POINT('Ctrl Pts',(-0.255268311374609,0.114709988905893,
-0.102135616170675));
#77348=CARTESIAN_POINT('Ctrl Pts',(-0.234784163283211,-0.152372694127167,
-0.0862516860966871));
#77349=CARTESIAN_POINT('Ctrl Pts',(0.000873349831699318,-0.279864587026233,
-0.0703677560226992));
#77350=CARTESIAN_POINT('Ctrl Pts',(0.235545095807039,-0.150999549715214,
-0.0544838259487111));
#77351=CARTESIAN_POINT('Ctrl Pts',(0.254801731495678,0.116219838507545,
-0.038599895874723));
#77352=CARTESIAN_POINT('Ctrl Pts',(0.0399292304854129,0.276921674028602,
-0.0227159658007349));
#77353=CARTESIAN_POINT('Ctrl Pts',(-0.126619139592439,0.214993150582441,
-0.0121266790847428));
#77354=CARTESIAN_POINT('Ctrl Pts',(-0.178397946941454,0.155645103547024,
-0.00683203572674675));
#77355=CARTESIAN_POINT('Ctrl Pts',(0.133821547094406,0.262002735736212,
-1.9608));
#77356=CARTESIAN_POINT('Ctrl Pts',(0.132194727536144,0.262814729912177,
-1.9608));
#77357=CARTESIAN_POINT('Ctrl Pts',(0.130567907977882,0.263626724088142,
-1.9608));
#77358=CARTESIAN_POINT('Ctrl Pts',(0.12894108841962,0.264438718264107,-1.9608));
#77359=CARTESIAN_POINT('Origin',(0.,0.,-0.04));
#77360=CARTESIAN_POINT('',(-0.3342,4.09276960275046E-17,0.));
#77361=CARTESIAN_POINT('Origin',(0.,0.,0.));
#77362=CARTESIAN_POINT('Origin',(-0.3342,-4.09276960275045E-17,-0.04));
#77363=CARTESIAN_POINT('Origin',(0.48,0.,0.));
#77364=CARTESIAN_POINT('',(-0.48,-5.8783046359073E-17,3.46944695195361E-18));
#77365=CARTESIAN_POINT('Origin',(0.,0.,0.));
#77366=CARTESIAN_POINT('Origin',(0.,0.,0.6066185719505));
#77367=CARTESIAN_POINT('',(-0.25,0.144337567297406,0.588452994616207));
#77368=CARTESIAN_POINT('',(-0.25,-5.3231743852413E-17,0.566123895246948));
#77369=CARTESIAN_POINT('Ctrl Pts',(-0.25,0.144337567297406,0.588452994616208));
#77370=CARTESIAN_POINT('Ctrl Pts',(-0.25,0.0669872981077805,0.566123895246948));
#77371=CARTESIAN_POINT('Ctrl Pts',(-0.25,-7.58473177261421E-17,0.566123895246948));
#77372=CARTESIAN_POINT('',(1.76762539787485E-17,0.288675134594813,0.588452994616207));
#77373=CARTESIAN_POINT('Ctrl Pts',(1.76762539787485E-17,0.288675134594813,
0.588452994616207));
#77374=CARTESIAN_POINT('Ctrl Pts',(-0.125,0.21650635094611,0.546786327949541));
#77375=CARTESIAN_POINT('Ctrl Pts',(-0.25,0.144337567297406,0.588452994616207));
#77376=CARTESIAN_POINT('',(0.25,0.144337567297406,0.588452994616207));
#77377=CARTESIAN_POINT('Ctrl Pts',(0.25,0.144337567297406,0.588452994616207));
#77378=CARTESIAN_POINT('Ctrl Pts',(0.125,0.21650635094611,0.546786327949541));
#77379=CARTESIAN_POINT('Ctrl Pts',(1.76762539787485E-17,0.288675134594813,
0.588452994616207));
#77380=CARTESIAN_POINT('',(0.25,-0.144337567297407,0.588452994616207));
#77381=CARTESIAN_POINT('Ctrl Pts',(0.25,-0.144337567297407,0.588452994616207));
#77382=CARTESIAN_POINT('Ctrl Pts',(0.25,-2.77555756156289E-17,0.546786327949541));
#77383=CARTESIAN_POINT('Ctrl Pts',(0.25,0.144337567297406,0.588452994616207));
#77384=CARTESIAN_POINT('',(-5.30287619362454E-17,-0.288675134594813,0.588452994616207));
#77385=CARTESIAN_POINT('Ctrl Pts',(-5.30287619362454E-17,-0.288675134594813,
0.588452994616207));
#77386=CARTESIAN_POINT('Ctrl Pts',(0.125,-0.21650635094611,0.546786327949541));
#77387=CARTESIAN_POINT('Ctrl Pts',(0.25,-0.144337567297407,0.588452994616207));
#77388=CARTESIAN_POINT('',(-0.25,-0.144337567297406,0.588452994616207));
#77389=CARTESIAN_POINT('Ctrl Pts',(-0.25,-0.144337567297406,0.588452994616207));
#77390=CARTESIAN_POINT('Ctrl Pts',(-0.125,-0.21650635094611,0.546786327949541));
#77391=CARTESIAN_POINT('Ctrl Pts',(-5.30287619362454E-17,-0.288675134594813,
0.588452994616207));
#77392=CARTESIAN_POINT('Ctrl Pts',(-0.25,-7.58473177261421E-17,0.566123895246948));
#77393=CARTESIAN_POINT('Ctrl Pts',(-0.25,-0.0669872981077807,0.566123895246948));
#77394=CARTESIAN_POINT('Ctrl Pts',(-0.25,-0.144337567297406,0.588452994616208));
#77395=CARTESIAN_POINT('',(-0.308675134594813,3.78018015557916E-17,0.6));
#77396=CARTESIAN_POINT('',(-0.320138837486628,-3.92057002610754E-17,0.6066185719505));
#77397=CARTESIAN_POINT('Origin',(0.,0.,0.6));
#77398=CARTESIAN_POINT('Origin',(-5.55111512312578E-17,-0.288675134594813,
0.6));
#77399=CARTESIAN_POINT('',(-5.55111512312578E-17,-0.288675134594813,0.25));
#77400=CARTESIAN_POINT('',(-5.30287619362453E-17,-0.288675134594813,0.6));
#77401=CARTESIAN_POINT('',(-0.25,-0.144337567297406,0.25));
#77402=CARTESIAN_POINT('',(-0.25,-0.144337567297406,0.25));
#77403=CARTESIAN_POINT('',(-0.25,-0.144337567297406,0.6));
#77404=CARTESIAN_POINT('Origin',(0.25,-0.144337567297407,0.6));
#77405=CARTESIAN_POINT('',(0.25,-0.144337567297407,0.25));
#77406=CARTESIAN_POINT('',(0.25,-0.144337567297407,0.6));
#77407=CARTESIAN_POINT('',(-5.30287619362453E-17,-0.288675134594813,0.25));
#77408=CARTESIAN_POINT('Origin',(0.25,0.144337567297406,0.6));
#77409=CARTESIAN_POINT('',(0.25,0.144337567297406,0.25));
#77410=CARTESIAN_POINT('',(0.25,0.144337567297406,0.6));
#77411=CARTESIAN_POINT('',(0.25,-0.144337567297407,0.25));
#77412=CARTESIAN_POINT('Origin',(0.,0.,0.176894574169124));
#77413=CARTESIAN_POINT('',(0.,0.,0.102789148338248));
#77414=CARTESIAN_POINT('',(-0.243346949651439,2.98014062972907E-17,0.25));
#77415=CARTESIAN_POINT('',(-0.1225,-1.50019232895551E-17,0.176894574169124));
#77416=CARTESIAN_POINT('Origin',(0.,0.,0.25));
#77417=CARTESIAN_POINT('Origin',(0.,0.288675134594813,0.6));
#77418=CARTESIAN_POINT('',(2.77555756156289E-17,0.288675134594813,0.25));
#77419=CARTESIAN_POINT('',(1.76762539787485E-17,0.288675134594813,0.6));
#77420=CARTESIAN_POINT('',(0.25,0.144337567297406,0.25));
#77421=CARTESIAN_POINT('Origin',(-0.25,0.144337567297406,0.6));
#77422=CARTESIAN_POINT('',(-0.25,0.144337567297406,0.25));
#77423=CARTESIAN_POINT('',(-0.25,0.144337567297406,0.6));
#77424=CARTESIAN_POINT('',(1.76762539787485E-17,0.288675134594813,0.25));
#77425=CARTESIAN_POINT('Origin',(-0.25,-0.144337567297406,0.6));
#77426=CARTESIAN_POINT('',(-0.25,0.144337567297406,0.25));
#77427=CARTESIAN_POINT('Origin',(0.,0.,0.25));
#77428=CARTESIAN_POINT('Origin',(0.,0.,0.54));
#77429=CARTESIAN_POINT('',(-0.44,-5.38844591624835E-17,0.6));
#77430=CARTESIAN_POINT('Origin',(0.,0.,0.6));
#77431=CARTESIAN_POINT('',(-0.5,-6.12323399573677E-17,0.54));
#77432=CARTESIAN_POINT('Origin',(-0.44,-5.38844591624835E-17,0.54));
#77433=CARTESIAN_POINT('Origin',(0.,0.,0.54));
#77434=CARTESIAN_POINT('Origin',(0.,0.,0.31));
#77435=CARTESIAN_POINT('',(-0.5,-6.12323399573677E-17,0.02));
#77436=CARTESIAN_POINT('',(-0.5,-6.12323399573677E-17,0.31));
#77437=CARTESIAN_POINT('Origin',(0.,0.,0.02));
#77438=CARTESIAN_POINT('Origin',(0.,0.,0.6));
#77439=CARTESIAN_POINT('Origin',(0.255,0.,-2.));
#77440=CARTESIAN_POINT('',(-0.255,-3.12284933782575E-17,-2.));
#77441=CARTESIAN_POINT('Origin',(0.,0.,-2.));
#77442=CARTESIAN_POINT('Origin',(0.,0.,-1.9775));
#77443=CARTESIAN_POINT('',(-0.2775,-3.39839486763391E-17,-1.9775));
#77444=CARTESIAN_POINT('Origin',(0.,0.,0.01));
#77445=CARTESIAN_POINT('',(-0.49,-6.00076931582203E-17,0.01));
#77446=CARTESIAN_POINT('',(0.,0.,0.));
#77447=CARTESIAN_POINT('Origin',(0.,0.,-1.7456589891905));
#77448=CARTESIAN_POINT('',(-0.0419358257166342,0.233438144154858,-1.49810946104348));
#77449=CARTESIAN_POINT('',(-0.0419358257166344,0.233438144154858,-1.51783893213918));
#77450=CARTESIAN_POINT('',(-0.0419358257166344,0.233438144154858,-1.7456589891905));
#77451=CARTESIAN_POINT('',(-0.137697638232154,-0.193109660686064,-1.56079343935569));
#77452=CARTESIAN_POINT('Ctrl Pts',(-0.137697638232154,-0.193109660686064,
-1.56079343935569));
#77453=CARTESIAN_POINT('Ctrl Pts',(-0.126370765437366,-0.201186333944446,
-1.55985488745099));
#77454=CARTESIAN_POINT('Ctrl Pts',(-0.114290892516889,-0.208291353281666,
-1.5589163355463));
#77455=CARTESIAN_POINT('Ctrl Pts',(-0.101651101434149,-0.214287270275731,
-1.5579777836416));
#77456=CARTESIAN_POINT('Ctrl Pts',(-0.0883887572017104,-0.220578506787781,
-1.5569930048301));
#77457=CARTESIAN_POINT('Ctrl Pts',(-0.0745105783197592,-0.225647730152209,
-1.5560082260186));
#77458=CARTESIAN_POINT('Ctrl Pts',(-0.0602716607461343,-0.229388987390203,
-1.5550234472071));
#77459=CARTESIAN_POINT('Ctrl Pts',(-0.0467279065913889,-0.232947591335977,
-1.55408674664325));
#77460=CARTESIAN_POINT('Ctrl Pts',(-0.0328587864043571,-0.235304889593483,
-1.5531500460794));
#77461=CARTESIAN_POINT('Ctrl Pts',(-0.0188993798127954,-0.236420798720611,
-1.55221334551556));
#77462=CARTESIAN_POINT('Ctrl Pts',(-0.00493879338562826,-0.237536802163304,
-1.55127656578268));
#77463=CARTESIAN_POINT('Ctrl Pts',(0.00911124316326098,-0.23741117478722,
-1.5503397860498));
#77464=CARTESIAN_POINT('Ctrl Pts',(0.0230131566390361,-0.236055873145548,
-1.54940300631693));
#77465=CARTESIAN_POINT('Ctrl Pts',(0.0369446089546456,-0.234697691753676,
-1.54846423611083));
#77466=CARTESIAN_POINT('Ctrl Pts',(0.0507264729274663,-0.232104781046902,
-1.54752546590473));
#77467=CARTESIAN_POINT('Ctrl Pts',(0.064129947202506,-0.228340382974199,
-1.54658669569864));
#77468=CARTESIAN_POINT('Ctrl Pts',(0.0661586067379395,-0.227770629051548,
-1.54644460976695));
#77469=CARTESIAN_POINT('Ctrl Pts',(0.0681786309103138,-0.227174130570319,
-1.54630252383527));
#77470=CARTESIAN_POINT('Ctrl Pts',(0.0701892650732185,-0.226551203248805,
-1.54616043790358));
#77471=CARTESIAN_POINT('Ctrl Pts',(0.0836284579295186,-0.22238752167822,
-1.54521072747226));
#77472=CARTESIAN_POINT('Ctrl Pts',(0.0967391885512409,-0.217010454215219,
-1.54426101704094));
#77473=CARTESIAN_POINT('Ctrl Pts',(0.10929121432994,-0.21049325665039,-1.54331130660963));
#77474=CARTESIAN_POINT('Ctrl Pts',(0.121818655152384,-0.203988823958728,
-1.54236345632342));
#77475=CARTESIAN_POINT('Ctrl Pts',(0.133788802529112,-0.196349013696355,
-1.54141560603721));
#77476=CARTESIAN_POINT('Ctrl Pts',(0.144991705523557,-0.187694927886638,
-1.54046775575101));
#77477=CARTESIAN_POINT('Ctrl Pts',(0.156193459843084,-0.179041729412223,
-1.53952000265138));
#77478=CARTESIAN_POINT('Ctrl Pts',(0.166627440775333,-0.169374931443179,
-1.53857224955176));
#77479=CARTESIAN_POINT('Ctrl Pts',(0.176113728514314,-0.158858223752459,
-1.53762449645214));
#77480=CARTESIAN_POINT('Ctrl Pts',(0.185598801175167,-0.148342863124136,
-1.53667686474816));
#77481=CARTESIAN_POINT('Ctrl Pts',(0.194135879692125,-0.136978439371701,
-1.53572923304419));
#77482=CARTESIAN_POINT('Ctrl Pts',(0.201584340829336,-0.124962931133204,
-1.53478160134021));
#77483=CARTESIAN_POINT('Ctrl Pts',(0.209050214271248,-0.112919334181251,
-1.53383175435288));
#77484=CARTESIAN_POINT('Ctrl Pts',(0.215421989731213,-0.100222345577201,
-1.53288190736556));
#77485=CARTESIAN_POINT('Ctrl Pts',(0.220604506107634,-0.0870955366824668,
-1.53193206037823));
#77486=CARTESIAN_POINT('Ctrl Pts',(0.223561640495988,-0.0796054034783375,
-1.53139007942035));
#77487=CARTESIAN_POINT('Ctrl Pts',(0.226132462018965,-0.0719757125191499,
-1.53084809846247));
#77488=CARTESIAN_POINT('Ctrl Pts',(0.22830661995882,-0.0642500420854265,
-1.5303061175046));
#77489=CARTESIAN_POINT('Ctrl Pts',(0.2321046350015,-0.0507541446696043,
-1.52935933631951));
#77490=CARTESIAN_POINT('Ctrl Pts',(0.23471489071116,-0.0368738355829154,
-1.52841255513442));
#77491=CARTESIAN_POINT('Ctrl Pts',(0.236072645345789,-0.0228404628771269,
-1.52746577394934));
#77492=CARTESIAN_POINT('Ctrl Pts',(0.237427618165454,-0.00883584223389452,
-1.5265209325625));
#77493=CARTESIAN_POINT('Ctrl Pts',(0.237535031407606,0.00532040275172917,
-1.52557609117567));
#77494=CARTESIAN_POINT('Ctrl Pts',(0.236381263236701,0.0193875995322088,
-1.52463124978883));
#77495=CARTESIAN_POINT('Ctrl Pts',(0.235227703772985,0.0334522516722969,
-1.52368657931605));
#77496=CARTESIAN_POINT('Ctrl Pts',(0.232813433502387,0.047427051266188,
-1.52274190884326));
#77497=CARTESIAN_POINT('Ctrl Pts',(0.229176908063932,0.0610731154867347,
-1.52179723837048));
#77498=CARTESIAN_POINT('Ctrl Pts',(0.225541026574461,0.074716763288276,
-1.52085273517814));
#77499=CARTESIAN_POINT('Ctrl Pts',(0.220683552684347,0.0880309870194809,
-1.51990823198579));
#77500=CARTESIAN_POINT('Ctrl Pts',(0.214693137571915,0.100791057661516,
-1.51896372879345));
#77501=CARTESIAN_POINT('Ctrl Pts',(0.208688739205051,0.113580913771001,
-1.51801702087436));
#77502=CARTESIAN_POINT('Ctrl Pts',(0.201546517088136,0.125813294406853,
-1.51707031295527));
#77503=CARTESIAN_POINT('Ctrl Pts',(0.193401382393456,0.137287602911918,
-1.51612360503618));
#77504=CARTESIAN_POINT('Ctrl Pts',(0.188606837527871,0.144041829697759,
-1.51556633572599));
#77505=CARTESIAN_POINT('Ctrl Pts',(0.18346562526578,0.150533934177916,-1.5150090664158));
#77506=CARTESIAN_POINT('Ctrl Pts',(0.178011591305242,0.156728599770353,
-1.51445179710561));
#77507=CARTESIAN_POINT('Ctrl Pts',(0.168730151462301,0.167270414592069,
-1.51350346022024));
#77508=CARTESIAN_POINT('Ctrl Pts',(0.158478018770147,0.177020135394206,
-1.51255512333488));
#77509=CARTESIAN_POINT('Ctrl Pts',(0.147415180258664,0.185797592164984,
-1.51160678644951));
#77510=CARTESIAN_POINT('Ctrl Pts',(0.136374636156082,0.194557360147287,
-1.51066036070207));
#77511=CARTESIAN_POINT('Ctrl Pts',(0.12452723184534,0.202348185692752,-1.50971393495463));
#77512=CARTESIAN_POINT('Ctrl Pts',(0.112068452964966,0.209027850955415,
-1.5087675092072));
#77513=CARTESIAN_POINT('Ctrl Pts',(0.0996116721553255,0.215706444969941,
-1.50782123524234));
#77514=CARTESIAN_POINT('Ctrl Pts',(0.0865444213950397,0.221273796036656,
-1.50687496127748));
#77515=CARTESIAN_POINT('Ctrl Pts',(0.0730888892767603,0.225632433150222,
-1.50592868731262));
#77516=CARTESIAN_POINT('Ctrl Pts',(0.0596355491877476,0.229990360201932,
-1.50498256750445));
#77517=CARTESIAN_POINT('Ctrl Pts',(0.0457948524215321,0.233139724829233,
-1.50403644769627));
#77518=CARTESIAN_POINT('Ctrl Pts',(0.0318043181461604,0.23503290402039,
-1.5030903278881));
#77519=CARTESIAN_POINT('Ctrl Pts',(0.0177813457353162,0.236930472693883,
-1.502142014428));
#77520=CARTESIAN_POINT('Ctrl Pts',(0.00360867606594497,0.237565973563984,
-1.5011937009679));
#77521=CARTESIAN_POINT('Ctrl Pts',(-0.0104713284861235,0.23694373151602,
-1.50024538750779));
#77522=CARTESIAN_POINT('Ctrl Pts',(-0.0186270676159718,0.236583302384051,
-1.4996960839074));
#77523=CARTESIAN_POINT('Ctrl Pts',(-0.0267517235308848,0.235801856681092,
-1.49914678030702));
#77524=CARTESIAN_POINT('Ctrl Pts',(-0.0347993793595566,0.234608149519981,
-1.49859747670663));
#77525=CARTESIAN_POINT('Ctrl Pts',(-0.0371826285580409,0.234254642648476,
-1.49843480481891));
#77526=CARTESIAN_POINT('Ctrl Pts',(-0.0395618469931956,0.233864615836945,
-1.49827213293119));
#77527=CARTESIAN_POINT('Ctrl Pts',(-0.0419358257166342,0.233438144154858,
-1.49810946104348));
#77528=CARTESIAN_POINT('',(0.137702479013102,-0.193106208855765,-1.5608));
#77529=CARTESIAN_POINT('Origin',(0.,0.,-1.5608));
#77530=CARTESIAN_POINT('Ctrl Pts',(0.137702479013101,-0.193106208855765,
-1.5608));
#77531=CARTESIAN_POINT('Ctrl Pts',(0.149478942681546,-0.184708507659302,
-1.55982940334437));
#77532=CARTESIAN_POINT('Ctrl Pts',(0.160499517164105,-0.175219427018632,
-1.55885880668873));
#77533=CARTESIAN_POINT('Ctrl Pts',(0.17056779482257,-0.164798689298082,
-1.5578882100331));
#77534=CARTESIAN_POINT('Ctrl Pts',(0.180628695633146,-0.154385586666636,
-1.55691832451636));
#77535=CARTESIAN_POINT('Ctrl Pts',(0.189738136346402,-0.14304273078033,
-1.55594843899963));
#77536=CARTESIAN_POINT('Ctrl Pts',(0.197736432649809,-0.130966727942357,
-1.55497855348289));
#77537=CARTESIAN_POINT('Ctrl Pts',(0.205744047618538,-0.118876655579501,
-1.5540075379707));
#77538=CARTESIAN_POINT('Ctrl Pts',(0.212637498410565,-0.10605237729402,
-1.5530365224585));
#77539=CARTESIAN_POINT('Ctrl Pts',(0.218300389818104,-0.0927195795410208,
-1.5520655069463));
#77540=CARTESIAN_POINT('Ctrl Pts',(0.223966545314624,-0.079379096767229,
-1.55109393174105));
#77541=CARTESIAN_POINT('Ctrl Pts',(0.228400465487478,-0.0655302442710616,
-1.55012235653579));
#77542=CARTESIAN_POINT('Ctrl Pts',(0.231534592040504,-0.0514170527513709,
-1.54915078133053));
#77543=CARTESIAN_POINT('Ctrl Pts',(0.234677425683833,-0.0372646525938184,
-1.54817650693846));
#77544=CARTESIAN_POINT('Ctrl Pts',(0.236513140568815,-0.0228472191527624,
-1.54720223254639));
#77545=CARTESIAN_POINT('Ctrl Pts',(0.237025582884283,-0.00841746300057407,
-1.54622795815432));
#77546=CARTESIAN_POINT('Ctrl Pts',(0.2372503976443,-0.00208695111944139,
-1.54580053196989));
#77547=CARTESIAN_POINT('Ctrl Pts',(0.237221203791196,0.00424591693677301,
-1.54537310578545));
#77548=CARTESIAN_POINT('Ctrl Pts',(0.236939796631132,0.0105599904070905,
-1.54494567960102));
#77549=CARTESIAN_POINT('Ctrl Pts',(0.236321990332825,0.0244220199199111,
-1.54400730053225));
#77550=CARTESIAN_POINT('Ctrl Pts',(0.234480871056891,0.0382861540118555,
-1.54306892146348));
#77551=CARTESIAN_POINT('Ctrl Pts',(0.231423179372956,0.0519162082004513,
-1.54213054239472));
#77552=CARTESIAN_POINT('Ctrl Pts',(0.228372420405316,0.0655153589139597,
-1.54119429091648));
#77553=CARTESIAN_POINT('Ctrl Pts',(0.224110660071987,0.0788806421642751,
-1.54025803943824));
#77554=CARTESIAN_POINT('Ctrl Pts',(0.218696210916371,0.0917820677247033,
-1.53932178796));
#77555=CARTESIAN_POINT('Ctrl Pts',(0.213283688291701,0.104678902791277,
-1.53838586961213));
#77556=CARTESIAN_POINT('Ctrl Pts',(0.206719564054125,0.117111399699901,
-1.53744995126426));
#77557=CARTESIAN_POINT('Ctrl Pts',(0.199111287314113,0.128866892137262,
-1.53651403291638));
#77558=CARTESIAN_POINT('Ctrl Pts',(0.191505257362885,0.140618913077796,
-1.53557839095316));
#77559=CARTESIAN_POINT('Ctrl Pts',(0.182856162507269,0.151693616802622,
-1.53464274898993));
#77560=CARTESIAN_POINT('Ctrl Pts',(0.173314975293426,0.161907072001316,
-1.5337071070267));
#77561=CARTESIAN_POINT('Ctrl Pts',(0.163751335877573,0.172144561374605,
-1.53276926332255));
#77562=CARTESIAN_POINT('Ctrl Pts',(0.153292029975829,0.181516161201482,
-1.53183141961839));
#77563=CARTESIAN_POINT('Ctrl Pts',(0.142124653048296,0.189875126388112,
-1.53089357591424));
#77564=CARTESIAN_POINT('Ctrl Pts',(0.134971352613422,0.195229489341259,
-1.53029283701017));
#77565=CARTESIAN_POINT('Ctrl Pts',(0.127528224370449,0.200169177942891,
-1.5296920981061));
#77566=CARTESIAN_POINT('Ctrl Pts',(0.119850226191402,0.204665346130872,
-1.52909135920203));
#77567=CARTESIAN_POINT('Ctrl Pts',(0.107714278591147,0.211772050281987,
-1.52814182317829));
#77568=CARTESIAN_POINT('Ctrl Pts',(0.0949040243045732,0.217819023637601,
-1.52719228715455));
#77569=CARTESIAN_POINT('Ctrl Pts',(0.0816285163303515,0.222685351890746,
-1.52624275113081));
#77570=CARTESIAN_POINT('Ctrl Pts',(0.0683792569347776,0.227542058350124,
-1.52529509254717));
#77571=CARTESIAN_POINT('Ctrl Pts',(0.0546673184985617,0.23122240437951,
-1.52434743396353));
#77572=CARTESIAN_POINT('Ctrl Pts',(0.0407235335477553,0.233652679078124,
-1.52339977537989));
#77573=CARTESIAN_POINT('Ctrl Pts',(0.0267801846357797,0.236082877779142,
-1.52245214643066));
#77574=CARTESIAN_POINT('Ctrl Pts',(0.0126058125709699,0.237262888211552,
-1.52150451748144));
#77575=CARTESIAN_POINT('Ctrl Pts',(-0.00155735652436486,0.237169886928455,
-1.52055688853221));
#77576=CARTESIAN_POINT('Ctrl Pts',(-0.0150981261894554,0.237080972579943,
-1.51965090306787));
#77577=CARTESIAN_POINT('Ctrl Pts',(-0.0286279485024635,0.23582882808328,
-1.51874491760353));
#77578=CARTESIAN_POINT('Ctrl Pts',(-0.0419358257166344,0.233438144154858,
-1.51783893213918));
#77579=CARTESIAN_POINT('Origin',(0.,0.,-1.7456589891905));
#77580=CARTESIAN_POINT('',(-0.0419358227397264,0.233438144689642,-1.39796759050954));
#77581=CARTESIAN_POINT('',(-0.0420041065163025,0.233814670441123,-1.41782827198422));
#77582=CARTESIAN_POINT('',(-0.0419358257166344,0.233438144154858,-1.7456589891905));
#77583=CARTESIAN_POINT('',(-0.237174982656716,9.07016348682755E-5,-1.47594101081397));
#77584=CARTESIAN_POINT('Ctrl Pts',(-0.0419358227397264,0.233438144689642,
-1.39796759050954));
#77585=CARTESIAN_POINT('Ctrl Pts',(-0.0385115227848158,0.234053300520784,
-1.3982158823771));
#77586=CARTESIAN_POINT('Ctrl Pts',(-0.0350737264621262,0.234593103052235,
-1.39846590841708));
#77587=CARTESIAN_POINT('Ctrl Pts',(-0.0228340253071061,0.236239849252627,
-1.39935797186273));
#77588=CARTESIAN_POINT('Ctrl Pts',(-0.0139839628830158,0.236928465946922,
-1.40000675194027));
#77589=CARTESIAN_POINT('Ctrl Pts',(0.0062048354393095,0.237364093489822,
-1.40147949715167));
#77590=CARTESIAN_POINT('Ctrl Pts',(0.0175304436519194,0.236797283269903,
-1.40230066413439));
#77591=CARTESIAN_POINT('Ctrl Pts',(0.0304816933296712,0.235214390114697,
-1.40320649359698));
#77592=CARTESIAN_POINT('Ctrl Pts',(0.0321878590607497,0.234986989220831,
-1.40332513900844));
#77593=CARTESIAN_POINT('Ctrl Pts',(0.0348481363742243,0.234602903491431,
-1.40350890508603));
#77594=CARTESIAN_POINT('Ctrl Pts',(0.0358039822502094,0.23445893003607,
-1.40357468449152));
#77595=CARTESIAN_POINT('Ctrl Pts',(0.0375012861816143,0.234192653166615,
-1.40369101608473));
#77596=CARTESIAN_POINT('Ctrl Pts',(0.03824305479765,0.234072668300515,-1.4037416921443));
#77597=CARTESIAN_POINT('Ctrl Pts',(0.040041031267924,0.233773061292673,
-1.40386414144227));
#77598=CARTESIAN_POINT('Ctrl Pts',(0.0410966092933508,0.233589805398562,
-1.40393571119502));
#77599=CARTESIAN_POINT('Ctrl Pts',(0.0444106392871122,0.232991305735389,
-1.40415950614305));
#77600=CARTESIAN_POINT('Ctrl Pts',(0.0466644010411356,0.23255039896938,
-1.40431038321784));
#77601=CARTESIAN_POINT('Ctrl Pts',(0.058794893214838,0.229993828917358,
-1.40511706439754));
#77602=CARTESIAN_POINT('Ctrl Pts',(0.0685363003703231,0.227281372891614,
-1.40574574024272));
#77603=CARTESIAN_POINT('Ctrl Pts',(0.0957465208308804,0.217795275175144,
-1.40752101448389));
#77604=CARTESIAN_POINT('Ctrl Pts',(0.112624314419017,0.209565956220392,
-1.40865116116187));
#77605=CARTESIAN_POINT('Ctrl Pts',(0.131626835676394,0.197335897561624,
-1.4101021456057));
#77606=CARTESIAN_POINT('Ctrl Pts',(0.134842071643729,0.195152999699572,
-1.41035421447998));
#77607=CARTESIAN_POINT('Ctrl Pts',(0.139525226924441,0.191802500136539,
-1.41073212287856));
#77608=CARTESIAN_POINT('Ctrl Pts',(0.141035360131173,0.190694821285337,
-1.41085569667013));
#77609=CARTESIAN_POINT('Ctrl Pts',(0.143714122362353,0.188680731328749,
-1.41107808339702));
#77610=CARTESIAN_POINT('Ctrl Pts',(0.14488770220306,0.187781045162446,-1.41117663131866));
#77611=CARTESIAN_POINT('Ctrl Pts',(0.147367584262801,0.185842838114168,
-1.41138731591022));
#77612=CARTESIAN_POINT('Ctrl Pts',(0.148671486572401,0.184801391238574,
-1.41149956519719));
#77613=CARTESIAN_POINT('Ctrl Pts',(0.152183327575941,0.181935207476623,
-1.41180599082377));
#77614=CARTESIAN_POINT('Ctrl Pts',(0.154369314046198,0.180084142960229,
-1.41200121847907));
#77615=CARTESIAN_POINT('Ctrl Pts',(0.15915197844672,0.175883170235995,-1.41243866022511));
#77616=CARTESIAN_POINT('Ctrl Pts',(0.161731172222493,0.173514459201455,
-1.4126816093225));
#77617=CARTESIAN_POINT('Ctrl Pts',(0.169798748114308,0.165769075430633,
-1.41346461481212));
#77618=CARTESIAN_POINT('Ctrl Pts',(0.175078348686338,0.160182876665333,
-1.41401272850317));
#77619=CARTESIAN_POINT('Ctrl Pts',(0.185812558339347,0.147659544691448,
-1.4152040761576));
#77620=CARTESIAN_POINT('Ctrl Pts',(0.191170327439097,0.140653986999804,
-1.4158486058659));
#77621=CARTESIAN_POINT('Ctrl Pts',(0.202534132182428,0.123942686382771,
-1.41732258603659));
#77622=CARTESIAN_POINT('Ctrl Pts',(0.208255764826146,0.114067779206743,
-1.41814923792898));
#77623=CARTESIAN_POINT('Ctrl Pts',(0.213999403889504,0.102270239278141,
-1.41906020408607));
#77624=CARTESIAN_POINT('Ctrl Pts',(0.2147364161444,0.100713547837493,-1.41917892625864));
#77625=CARTESIAN_POINT('Ctrl Pts',(0.215860613511241,0.0982706006451665,
-1.41936278546606));
#77626=CARTESIAN_POINT('Ctrl Pts',(0.216259429639905,0.097389807432605,
-1.41942858225961));
#77627=CARTESIAN_POINT('Ctrl Pts',(0.216958546654219,0.0958203217273344,
-1.41954492055797));
#77628=CARTESIAN_POINT('Ctrl Pts',(0.217260966693063,0.0951326305599371,
-1.41959558619686));
#77629=CARTESIAN_POINT('Ctrl Pts',(0.217986477397933,0.0934613431893207,
-1.41971798250195));
#77630=CARTESIAN_POINT('Ctrl Pts',(0.218406182192277,0.0924763033946822,
-1.41978951003484));
#77631=CARTESIAN_POINT('Ctrl Pts',(0.219703950920165,0.0893723401339488,
-1.42001308787452));
#77632=CARTESIAN_POINT('Ctrl Pts',(0.220557988058772,0.0872434300490766,
-1.42016379314305));
#77633=CARTESIAN_POINT('Ctrl Pts',(0.224996491361345,0.0756973298365073,
-1.42096872802044));
#77634=CARTESIAN_POINT('Ctrl Pts',(0.228009349873586,0.066070334627584,
-1.42159594882526));
#77635=CARTESIAN_POINT('Ctrl Pts',(0.234822507878949,0.0381783565535167,
-1.42336486101796));
#77636=CARTESIAN_POINT('Ctrl Pts',(0.237095305635452,0.0196204699282895,
-1.42449008134364));
#77637=CARTESIAN_POINT('Ctrl Pts',(0.237189437135739,-0.00297073851907267,
-1.42593975158081));
#77638=CARTESIAN_POINT('Ctrl Pts',(0.237106803290778,-0.00692930719472698,
-1.4261964496161));
#77639=CARTESIAN_POINT('Ctrl Pts',(0.236838594622866,-0.0127678475325734,
-1.42657993949217));
#77640=CARTESIAN_POINT('Ctrl Pts',(0.236729576540385,-0.0146507707299379,
-1.42670436332119));
#77641=CARTESIAN_POINT('Ctrl Pts',(0.236494965440406,-0.0180083828251615,
-1.42692766604776));
#77642=CARTESIAN_POINT('Ctrl Pts',(0.236378002591804,-0.0194835892956288,
-1.42702627070875));
#77643=CARTESIAN_POINT('Ctrl Pts',(0.23610054808405,-0.022611234457552,
-1.42723642030768));
#77644=CARTESIAN_POINT('Ctrl Pts',(0.23593649625322,-0.0242632689964275,
-1.42734807164072));
#77645=CARTESIAN_POINT('Ctrl Pts',(0.235446490425838,-0.0287212459295221,
-1.42765118190855));
#77646=CARTESIAN_POINT('Ctrl Pts',(0.235087737544856,-0.0315232339904567,
-1.42784365431889));
#77647=CARTESIAN_POINT('Ctrl Pts',(0.232319170964273,-0.0504556805905314,
-1.42915797094521));
#77648=CARTESIAN_POINT('Ctrl Pts',(0.22830150962364,-0.0663039106971981,
-1.43033089979363));
#77649=CARTESIAN_POINT('Ctrl Pts',(0.217737196604775,-0.0951303715589203,
-1.43257014431758));
#77650=CARTESIAN_POINT('Ctrl Pts',(0.211561906303192,-0.108170705424929,
-1.43362711178));
#77651=CARTESIAN_POINT('Ctrl Pts',(0.203112941795011,-0.122482820693217,
-1.43478809538256));
#77652=CARTESIAN_POINT('Ctrl Pts',(0.20195760122813,-0.124378602178046,
-1.43494185233243));
#77653=CARTESIAN_POINT('Ctrl Pts',(0.200213137941164,-0.127152652478288,
-1.43516649137864));
#77654=CARTESIAN_POINT('Ctrl Pts',(0.199644525764759,-0.128043590530309,
-1.43523858411618));
#77655=CARTESIAN_POINT('Ctrl Pts',(0.198618812406788,-0.129627299380353,
-1.43536659551601));
#77656=CARTESIAN_POINT('Ctrl Pts',(0.198164010562332,-0.13032150385923,
-1.43542265703305));
#77657=CARTESIAN_POINT('Ctrl Pts',(0.197145964434181,-0.131857785336601,
-1.43554660767136));
#77658=CARTESIAN_POINT('Ctrl Pts',(0.196580960679258,-0.13269865424826,
-1.43561437949057));
#77659=CARTESIAN_POINT('Ctrl Pts',(0.194887550087053,-0.135184325819797,
-1.43581458801289));
#77660=CARTESIAN_POINT('Ctrl Pts',(0.193743731047786,-0.136818589556655,
-1.43594604936458));
#77661=CARTESIAN_POINT('Ctrl Pts',(0.191037537522976,-0.140583133819324,
-1.4362489661089));
#77662=CARTESIAN_POINT('Ctrl Pts',(0.189459897267262,-0.142702161204216,
-1.43641954723445));
#77663=CARTESIAN_POINT('Ctrl Pts',(0.183754910419155,-0.15010344700502,
-1.43701733590484));
#77664=CARTESIAN_POINT('Ctrl Pts',(0.179439185425535,-0.155236925469464,
-1.43743566835982));
#77665=CARTESIAN_POINT('Ctrl Pts',(0.164359446309655,-0.171703422856967,
-1.43881571772802));
#77666=CARTESIAN_POINT('Ctrl Pts',(0.152695044690636,-0.182154633961043,
-1.43975884068888));
#77667=CARTESIAN_POINT('Ctrl Pts',(0.134475040986205,-0.195491237786616,
-1.44117824261699));
#77668=CARTESIAN_POINT('Ctrl Pts',(0.128684851892426,-0.199350334193594,
-1.44162202884404));
#77669=CARTESIAN_POINT('Ctrl Pts',(0.120693385116736,-0.204183186490165,
-1.44223054843731));
#77670=CARTESIAN_POINT('Ctrl Pts',(0.118634482409945,-0.205386284264406,
-1.44238697158936));
#77671=CARTESIAN_POINT('Ctrl Pts',(0.115193077608888,-0.207328220908325,
-1.44264804090642));
#77672=CARTESIAN_POINT('Ctrl Pts',(0.11382073544532,-0.20808478151291,-1.44275204771688));
#77673=CARTESIAN_POINT('Ctrl Pts',(0.111108015260505,-0.209545416652104,
-1.44295749532978));
#77674=CARTESIAN_POINT('Ctrl Pts',(0.109768191839825,-0.210250366401893,
-1.44305889893902));
#77675=CARTESIAN_POINT('Ctrl Pts',(0.106541729213029,-0.211908727354906,
-1.44330297863427));
#77676=CARTESIAN_POINT('Ctrl Pts',(0.104648941718163,-0.212849823320916,
-1.44344607596967));
#77677=CARTESIAN_POINT('Ctrl Pts',(0.0979208303261277,-0.216083611620292,
-1.44395455925712));
#77678=CARTESIAN_POINT('Ctrl Pts',(0.0930210722525494,-0.218237687910149,
-1.44432460087382));
#77679=CARTESIAN_POINT('Ctrl Pts',(0.0804665399451123,-0.223257411443849,
-1.44527264343318));
#77680=CARTESIAN_POINT('Ctrl Pts',(0.0727291138993964,-0.225896413281411,
-1.44585699716101));
#77681=CARTESIAN_POINT('Ctrl Pts',(0.0484925840948999,-0.232788348119927,
-1.44768090076866));
#77682=CARTESIAN_POINT('Ctrl Pts',(0.0316597436471689,-0.235668460739882,
-1.44894206829237));
#77683=CARTESIAN_POINT('Ctrl Pts',(0.0113577316712747,-0.236926048203879,
-1.45037926527418));
#77684=CARTESIAN_POINT('Ctrl Pts',(0.008047870637609,-0.237061563419197,
-1.45061078116697));
#77685=CARTESIAN_POINT('Ctrl Pts',(0.0034640937090203,-0.237153113473312,
-1.45092659849045));
#77686=CARTESIAN_POINT('Ctrl Pts',(0.00219190498361422,-0.237168283945298,
-1.4510137385851));
#77687=CARTESIAN_POINT('Ctrl Pts',(6.82070392426777E-5,-0.23717651841754,
-1.45115828139573));
#77688=CARTESIAN_POINT('Ctrl Pts',(-0.000783241418594574,-0.237175235129772,
-1.45121598484313));
#77689=CARTESIAN_POINT('Ctrl Pts',(-0.00253457421257168,-0.237163164059402,
-1.45133414100589));
#77690=CARTESIAN_POINT('Ctrl Pts',(-0.00343443356706208,-0.237151839940067,
-1.45139456418305));
#77691=CARTESIAN_POINT('Ctrl Pts',(-0.00579312183182301,-0.237108729181641,
-1.45155224232815));
#77692=CARTESIAN_POINT('Ctrl Pts',(-0.00725178649765415,-0.237068600983041,
-1.4516490503791));
#77693=CARTESIAN_POINT('Ctrl Pts',(-0.0140361093464927,-0.236819284811098,
-1.45209642249942));
#77694=CARTESIAN_POINT('Ctrl Pts',(-0.0193545418351217,-0.236444068392913,
-1.45243886043213));
#77695=CARTESIAN_POINT('Ctrl Pts',(-0.0360037235606818,-0.234703823142002,
-1.45349739019527));
#77696=CARTESIAN_POINT('Ctrl Pts',(-0.047251593670237,-0.232700396680081,
-1.45419335349711));
#77697=CARTESIAN_POINT('Ctrl Pts',(-0.0719890195642776,-0.226425821165901,
-1.45575911049224));
#77698=CARTESIAN_POINT('Ctrl Pts',(-0.0853274533528092,-0.221743623405162,
-1.45662900645784));
#77699=CARTESIAN_POINT('Ctrl Pts',(-0.101021615892802,-0.214607611641924,
-1.45773989316845));
#77700=CARTESIAN_POINT('Ctrl Pts',(-0.103847197587359,-0.213254664530967,
-1.45794345037883));
#77701=CARTESIAN_POINT('Ctrl Pts',(-0.108351474897206,-0.210987175704623,
-1.45827420285073));
#77702=CARTESIAN_POINT('Ctrl Pts',(-0.110047411805366,-0.210107584881623,
-1.45840019625464));
#77703=CARTESIAN_POINT('Ctrl Pts',(-0.113040872083618,-0.208508853497178,
-1.45862529097428));
#77704=CARTESIAN_POINT('Ctrl Pts',(-0.114342636695129,-0.207797839284336,
-1.45872410203686));
#77705=CARTESIAN_POINT('Ctrl Pts',(-0.117076446692352,-0.206271185741886,
-1.45893361942195));
#77706=CARTESIAN_POINT('Ctrl Pts',(-0.118506825851804,-0.205452740129825,
-1.45904442214966));
#77707=CARTESIAN_POINT('Ctrl Pts',(-0.122313682920159,-0.203221521548993,
-1.45934255654036));
#77708=CARTESIAN_POINT('Ctrl Pts',(-0.124674119595853,-0.201782027524024,
-1.45953084382207));
#77709=CARTESIAN_POINT('Ctrl Pts',(-0.138785438436959,-0.192834216910929,
-1.46067787415787));
#77710=CARTESIAN_POINT('Ctrl Pts',(-0.149878585889672,-0.184344031316412,
-1.46167306143995));
#77711=CARTESIAN_POINT('Ctrl Pts',(-0.170603941412359,-0.165368594017367,
-1.46371534232905));
#77712=CARTESIAN_POINT('Ctrl Pts',(-0.180170453569703,-0.154890629509906,
-1.46475874418413));
#77713=CARTESIAN_POINT('Ctrl Pts',(-0.19126534308864,-0.140309897044045,
-1.46606185369443));
#77714=CARTESIAN_POINT('Ctrl Pts',(-0.193697931935111,-0.136932154204561,
-1.46635432140335));
#77715=CARTESIAN_POINT('Ctrl Pts',(-0.196820056118584,-0.132347135583678,
-1.46673724577035));
#77716=CARTESIAN_POINT('Ctrl Pts',(-0.197589560264613,-0.131195520859702,
-1.46683227518843));
#77717=CARTESIAN_POINT('Ctrl Pts',(-0.198785307029542,-0.129371618726384,
-1.46698089979822));
#77718=CARTESIAN_POINT('Ctrl Pts',(-0.199218314282917,-0.128703835701187,
-1.46703492340966));
#77719=CARTESIAN_POINT('Ctrl Pts',(-0.200109503315686,-0.12731417164089,
-1.46714651567243));
#77720=CARTESIAN_POINT('Ctrl Pts',(-0.20056715391065,-0.126591976111283,
-1.46720404508168));
#77721=CARTESIAN_POINT('Ctrl Pts',(-0.20168420389995,-0.124807951455004,
-1.46734505789291));
#77722=CARTESIAN_POINT('Ctrl Pts',(-0.202339146342763,-0.123743334678699,
-1.46742825589117));
#77723=CARTESIAN_POINT('Ctrl Pts',(-0.204755126852568,-0.119745656667404,
-1.46773732509588));
#77724=CARTESIAN_POINT('Ctrl Pts',(-0.206461149029418,-0.11677962629092,
-1.4679599684805));
#77725=CARTESIAN_POINT('Ctrl Pts',(-0.210756962966191,-0.108922455065835,
-1.46853532621668));
#77726=CARTESIAN_POINT('Ctrl Pts',(-0.213240883127421,-0.103975633730006,
-1.46888333159881));
#77727=CARTESIAN_POINT('Ctrl Pts',(-0.222858481493534,-0.0830241386476146,
-1.47031717910625));
#77728=CARTESIAN_POINT('Ctrl Pts',(-0.228380644288481,-0.0663416267354367,
-1.47136820539355));
#77729=CARTESIAN_POINT('Ctrl Pts',(-0.233441074249819,-0.0424792295932923,
-1.47290221919543));
#77730=CARTESIAN_POINT('Ctrl Pts',(-0.234573873129283,-0.0356974047384165,
-1.47334089467773));
#77731=CARTESIAN_POINT('Ctrl Pts',(-0.235699166942779,-0.0265236168339529,
-1.47394318760822));
#77732=CARTESIAN_POINT('Ctrl Pts',(-0.235952472644799,-0.0241667030348894,
-1.47409869549489));
#77733=CARTESIAN_POINT('Ctrl Pts',(-0.236314112713833,-0.0202500336210339,
-1.47435857727544));
#77734=CARTESIAN_POINT('Ctrl Pts',(-0.236442430454597,-0.0186922607503921,
-1.47446232187662));
#77735=CARTESIAN_POINT('Ctrl Pts',(-0.236656367354034,-0.0157384966995887,
-1.47465981115459));
#77736=CARTESIAN_POINT('Ctrl Pts',(-0.236745054315237,-0.0143427891428809,
-1.47475345538074));
#77737=CARTESIAN_POINT('Ctrl Pts',(-0.236902105175347,-0.0114699448769709,
-1.47494691258588));
#77738=CARTESIAN_POINT('Ctrl Pts',(-0.236969008503276,-0.00999279284550699,
-1.47504676705725));
#77739=CARTESIAN_POINT('Ctrl Pts',(-0.237125281952006,-0.0056428633784824,
-1.47534199169133));
#77740=CARTESIAN_POINT('Ctrl Pts',(-0.237176246592844,-0.00276908247686686,
-1.47553853944128));
#77741=CARTESIAN_POINT('Ctrl Pts',(-0.23717497685085,0.000104789305429084,
-1.4757366710682));
#77742=CARTESIAN_POINT('Ctrl Pts',(-0.0419358257166342,0.233438144154858,
-1.49810946104348));
#77743=CARTESIAN_POINT('Ctrl Pts',(-0.0557685687745926,0.230953171083461,
-1.49716160148462));
#77744=CARTESIAN_POINT('Ctrl Pts',(-0.069422922806279,0.227226644879475,
-1.49621374192575));
#77745=CARTESIAN_POINT('Ctrl Pts',(-0.0826620679931504,0.222303763216226,
-1.49526588236689));
#77746=CARTESIAN_POINT('Ctrl Pts',(-0.0958768314395088,0.217389947729199,
-1.49431976842419));
#77747=CARTESIAN_POINT('Ctrl Pts',(-0.108677107711918,0.211284379769945,
-1.49337365448149));
#77748=CARTESIAN_POINT('Ctrl Pts',(-0.120840594102836,0.204082168358418,
-1.49242754053879));
#77749=CARTESIAN_POINT('Ctrl Pts',(-0.133004145272652,0.19687991859018,
-1.49148142155739));
#77750=CARTESIAN_POINT('Ctrl Pts',(-0.144530162094799,0.188581402075368,
-1.49053530257598));
#77751=CARTESIAN_POINT('Ctrl Pts',(-0.155221192718087,0.179327527045277,
-1.48958918359458));
#77752=CARTESIAN_POINT('Ctrl Pts',(-0.165912151595259,0.170073714116737,
-1.48864307096246));
#77753=CARTESIAN_POINT('Ctrl Pts',(-0.175767522195974,0.159865120916746,
-1.48769695833033));
#77754=CARTESIAN_POINT('Ctrl Pts',(-0.184624890693679,0.14888126262679,
-1.48675084569821));
#77755=CARTESIAN_POINT('Ctrl Pts',(-0.1935024630955,0.137872349850303,-1.48580257495683));
#77756=CARTESIAN_POINT('Ctrl Pts',(-0.201377010051896,0.126085326568405,
-1.48485430421546));
#77757=CARTESIAN_POINT('Ctrl Pts',(-0.208128362015914,0.113730231467155,
-1.48390603347408));
#77758=CARTESIAN_POINT('Ctrl Pts',(-0.210888119927161,0.108679825025362,
-1.48351840775194));
#77759=CARTESIAN_POINT('Ctrl Pts',(-0.213460739258607,0.103534776502822,
-1.48313078202979));
#77760=CARTESIAN_POINT('Ctrl Pts',(-0.215840324500079,0.0983104009995918,
-1.48274315630764));
#77761=CARTESIAN_POINT('Ctrl Pts',(-0.222182201605667,0.0843868201933717,
-1.48171008775016));
#77762=CARTESIAN_POINT('Ctrl Pts',(-0.227186699712206,0.0698174069716404,
-1.48067701919268));
#77763=CARTESIAN_POINT('Ctrl Pts',(-0.230742419362563,0.0548627062011248,
-1.47964395063519));
#77764=CARTESIAN_POINT('Ctrl Pts',(-0.234275250085543,0.040004272035841,
-1.47861753216082));
#77765=CARTESIAN_POINT('Ctrl Pts',(-0.236377637504013,0.0247660283467118,
-1.47759111368645));
#77766=CARTESIAN_POINT('Ctrl Pts',(-0.236987714546397,0.0094235757054001,
-1.47656469521208));
#77767=CARTESIAN_POINT('Ctrl Pts',(-0.237111281928992,0.0063160555337377,
-1.47635680041271));
#77768=CARTESIAN_POINT('Ctrl Pts',(-0.237173791934776,0.00320431095113047,
-1.47614890561334));
#77769=CARTESIAN_POINT('Ctrl Pts',(-0.237174982656716,9.07016348682755E-5,
-1.47594101081397));
#77770=CARTESIAN_POINT('',(-0.237174946895483,0.000158713971423185,-1.4956589891905));
#77771=CARTESIAN_POINT('Ctrl Pts',(-0.0419358257166344,0.233438144154858,
-1.51783893213918));
#77772=CARTESIAN_POINT('Ctrl Pts',(-0.0558810547429703,0.23093296362344,
-1.51688955647307));
#77773=CARTESIAN_POINT('Ctrl Pts',(-0.0695817208837182,0.227177409959992,
-1.51594018080695));
#77774=CARTESIAN_POINT('Ctrl Pts',(-0.0828077196110171,0.222249549375973,
-1.51499080514083));
#77775=CARTESIAN_POINT('Ctrl Pts',(-0.0909517775708719,0.219215163614881,
-1.51440621636157));
#77776=CARTESIAN_POINT('Ctrl Pts',(-0.0989161661920512,0.21573728046195,
-1.51382162758231));
#77777=CARTESIAN_POINT('Ctrl Pts',(-0.10665151759329,0.211842947534366,
-1.51323703880304));
#77778=CARTESIAN_POINT('Ctrl Pts',(-0.119218195906053,0.20551630164522,
-1.51228732898985));
#77779=CARTESIAN_POINT('Ctrl Pts',(-0.131260473127216,0.198047205927597,
-1.51133761917666));
#77780=CARTESIAN_POINT('Ctrl Pts',(-0.142563372296947,0.189545945628816,
-1.51038790936346));
#77781=CARTESIAN_POINT('Ctrl Pts',(-0.153844132760301,0.181061336536311,
-1.50944005972317));
#77782=CARTESIAN_POINT('Ctrl Pts',(-0.164387692340001,0.171549016985991,
-1.50849221008287));
#77783=CARTESIAN_POINT('Ctrl Pts',(-0.174006991136474,0.161163108869962,
-1.50754436044258));
#77784=CARTESIAN_POINT('Ctrl Pts',(-0.183625303303705,0.15077826601252,
-1.50659660802103));
#77785=CARTESIAN_POINT('Ctrl Pts',(-0.19231894469696,0.139520588804458,
-1.50564885559948));
#77786=CARTESIAN_POINT('Ctrl Pts',(-0.199937509431487,0.127581240577657,
-1.50470110317793));
#77787=CARTESIAN_POINT('Ctrl Pts',(-0.207555098166764,0.115643421877128,
-1.50375347217107));
#77788=CARTESIAN_POINT('Ctrl Pts',(-0.214097453328319,0.103024816868292,
-1.50280584116421));
#77789=CARTESIAN_POINT('Ctrl Pts',(-0.219458590204809,0.0899439148042685,
-1.50185821015735));
#77790=CARTESIAN_POINT('Ctrl Pts',(-0.224832259753346,0.0768324336561026,
-1.50090836388367));
#77791=CARTESIAN_POINT('Ctrl Pts',(-0.229018924614474,0.0632572854076371,
-1.49995851760998));
#77792=CARTESIAN_POINT('Ctrl Pts',(-0.231961665499544,0.0494546900068923,
-1.4990086713363));
#77793=CARTESIAN_POINT('Ctrl Pts',(-0.233640799728419,0.0415788996162779,
-1.49846668702556));
#77794=CARTESIAN_POINT('Ctrl Pts',(-0.234915868802463,0.0336292874429718,
-1.49792470271481));
#77795=CARTESIAN_POINT('Ctrl Pts',(-0.235783863370645,0.0256505438346448,
-1.49738271840406));
#77796=CARTESIAN_POINT('Ctrl Pts',(-0.236704054579574,0.0171920004337824,
-1.49680814199954));
#77797=CARTESIAN_POINT('Ctrl Pts',(-0.237169242852117,0.00868257718441503,
-1.49623356559502));
#77798=CARTESIAN_POINT('Ctrl Pts',(-0.237174946895483,0.000158713971423185,
-1.4956589891905));
#77799=CARTESIAN_POINT('Ctrl Pts',(-0.237447721697233,0.000156842808466644,
-1.49565885091385));
#77800=CARTESIAN_POINT('Ctrl Pts',(-0.236948243252312,-0.0697991706694208,
-1.49094869994426));
#77801=CARTESIAN_POINT('Ctrl Pts',(-0.167292428838403,-0.21916121968206,
-1.48095377550834));
#77802=CARTESIAN_POINT('Ctrl Pts',(0.0863349738534437,-0.266549188346143,
-1.46567407760609));
#77803=CARTESIAN_POINT('Ctrl Pts',(0.270673100350359,-0.0724268647347502,
-1.44981975720711));
#77804=CARTESIAN_POINT('Ctrl Pts',(0.207909186801171,0.187842407039071,
-1.43396543680812));
#77805=CARTESIAN_POINT('Ctrl Pts',(0.0380245598870128,0.247548846411421,
-1.42330160840049));
#77806=CARTESIAN_POINT('Ctrl Pts',(-0.0406278707645089,0.234064275081112,
-1.41792255345919));
#77807=CARTESIAN_POINT('Ctrl Pts',(-0.0420041065163025,0.233814670441123,
-1.41782827198422));
#77808=CARTESIAN_POINT('Origin',(0.,0.,-1.7456589891905));
#77809=CARTESIAN_POINT('',(-0.0419357855265134,0.233438151374779,-1.29797390460371));
#77810=CARTESIAN_POINT('',(-0.0419358330286197,0.233438142841301,-1.31793598285019));
#77811=CARTESIAN_POINT('',(-0.0419358257166344,0.233438144154858,-1.7456589891905));
#77812=CARTESIAN_POINT('Ctrl Pts',(-0.0419357855265143,0.233438151374779,
-1.29797390460371));
#77813=CARTESIAN_POINT('Ctrl Pts',(-0.0356815834665369,0.23456168184605,
-1.29837265202323));
#77814=CARTESIAN_POINT('Ctrl Pts',(-0.0293811282187784,0.235434073806115,
-1.29877694890039));
#77815=CARTESIAN_POINT('Ctrl Pts',(-0.0201633428806279,0.236334146715947,
-1.29937698695918));
#77816=CARTESIAN_POINT('Ctrl Pts',(-0.0172724797192631,0.236562992781477,
-1.29956636593925));
#77817=CARTESIAN_POINT('Ctrl Pts',(-0.0127051448028816,0.23684038826945,
-1.29986780838322));
#77818=CARTESIAN_POINT('Ctrl Pts',(-0.0110310500785527,0.236924261973956,
-1.29997877052277));
#77819=CARTESIAN_POINT('Ctrl Pts',(-0.00787985660688119,0.237048669258367,
-1.30018859169584));
#77820=CARTESIAN_POINT('Ctrl Pts',(-0.00640298786574809,0.237093157459478,
-1.30028732233165));
#77821=CARTESIAN_POINT('Ctrl Pts',(-0.00306545500570211,0.237162488796146,
-1.30051137526909));
#77822=CARTESIAN_POINT('Ctrl Pts',(-0.00120473916601999,0.237179238904851,
-1.3006369437093));
#77823=CARTESIAN_POINT('Ctrl Pts',(0.00361807646716839,0.237165900774792,
-1.30096418744831));
#77824=CARTESIAN_POINT('Ctrl Pts',(0.00657968127167582,0.237102217173144,
-1.30116688669007));
#77825=CARTESIAN_POINT('Ctrl Pts',(0.027774878239727,0.236249053690374,
-1.30263057284041));
#77826=CARTESIAN_POINT('Ctrl Pts',(0.0458617641182701,0.233412763704121,
-1.30395581274328));
#77827=CARTESIAN_POINT('Ctrl Pts',(0.0749562716701144,0.225336107315267,
-1.30615962450828));
#77828=CARTESIAN_POINT('Ctrl Pts',(0.0862147971548094,0.2212732937283,-1.30702959026431));
#77829=CARTESIAN_POINT('Ctrl Pts',(0.098966661662484,0.215549710688493,
-1.30800366101553));
#77830=CARTESIAN_POINT('Ctrl Pts',(0.100802737872338,0.214697197505889,
-1.30814360145063));
#77831=CARTESIAN_POINT('Ctrl Pts',(0.103546399557912,0.213380322656402,
-1.30835200494468));
#77832=CARTESIAN_POINT('Ctrl Pts',(0.104462220559208,0.212933472077213,
-1.30842144845986));
#77833=CARTESIAN_POINT('Ctrl Pts',(0.106118555756728,0.212112048962696,
-1.30854678531595));
#77834=CARTESIAN_POINT('Ctrl Pts',(0.106860005420303,0.211739482574178,
-1.30860279380196));
#77835=CARTESIAN_POINT('Ctrl Pts',(0.108535631801202,0.210886463897045,
-1.30872915460454));
#77836=CARTESIAN_POINT('Ctrl Pts',(0.109468587258053,0.210403689448779,
-1.30879936253886));
#77837=CARTESIAN_POINT('Ctrl Pts',(0.112332563545517,0.208897467363209,
-1.30901452664639));
#77838=CARTESIAN_POINT('Ctrl Pts',(0.114252732678571,0.207853483516654,
-1.30915827798821));
#77839=CARTESIAN_POINT('Ctrl Pts',(0.129007174107794,0.199565326307494,
-1.31026106335337));
#77840=CARTESIAN_POINT('Ctrl Pts',(0.141157186330558,0.191164686746783,
-1.31115991449037));
#77841=CARTESIAN_POINT('Ctrl Pts',(0.164616073204325,0.171481058161546,
-1.31303788325358));
#77842=CARTESIAN_POINT('Ctrl Pts',(0.175724626897241,0.160078031720973,
-1.31401453224822));
#77843=CARTESIAN_POINT('Ctrl Pts',(0.18741540607085,0.145381763767024,-1.31523117935613));
#77844=CARTESIAN_POINT('Ctrl Pts',(0.189179040879372,0.143079282111341,
-1.31542058442191));
#77845=CARTESIAN_POINT('Ctrl Pts',(0.191894691798205,0.13939590300908,-1.31572205901251));
#77846=CARTESIAN_POINT('Ctrl Pts',(0.192875077085216,0.138036208702767,
-1.31583302681193));
#77847=CARTESIAN_POINT('Ctrl Pts',(0.194692335142278,0.135458696095318,
-1.31604285297072));
#77848=CARTESIAN_POINT('Ctrl Pts',(0.1955324040131,0.134243221513283,-1.31614158286913));
#77849=CARTESIAN_POINT('Ctrl Pts',(0.197404592492912,0.131479540217701,
-1.3163656263443));
#77850=CARTESIAN_POINT('Ctrl Pts',(0.198429949392734,0.129926892808175,
-1.31649118597169));
#77851=CARTESIAN_POINT('Ctrl Pts',(0.201039825656098,0.125871922403272,
-1.31681839037012));
#77852=CARTESIAN_POINT('Ctrl Pts',(0.202595888025147,0.123351761769579,
-1.31702105867031));
#77853=CARTESIAN_POINT('Ctrl Pts',(0.213402310709098,0.10509366182779,-1.31848501906883));
#77854=CARTESIAN_POINT('Ctrl Pts',(0.22085394003321,0.0883658384830213,
-1.31981060071742));
#77855=CARTESIAN_POINT('Ctrl Pts',(0.229887277007946,0.0595529943387015,
-1.32201447970667));
#77856=CARTESIAN_POINT('Ctrl Pts',(0.232595298218134,0.04789785306129,-1.32288417717998));
#77857=CARTESIAN_POINT('Ctrl Pts',(0.234721481644093,0.0340867079382427,
-1.32385799502002));
#77858=CARTESIAN_POINT('Ctrl Pts',(0.235003848364171,0.0320822308787528,
-1.32399793030747));
#77859=CARTESIAN_POINT('Ctrl Pts',(0.235389737772768,0.0290635558902885,
-1.32420632775149));
#77860=CARTESIAN_POINT('Ctrl Pts',(0.235512433664742,0.0280519627778268,
-1.3242757702817));
#77861=CARTESIAN_POINT('Ctrl Pts',(0.235723211632927,0.0262151995384508,
-1.32440110607555));
#77862=CARTESIAN_POINT('Ctrl Pts',(0.235813485932486,0.0253903345766434,
-1.32445711447523));
#77863=CARTESIAN_POINT('Ctrl Pts',(0.23600823123509,0.0235201794212471,
-1.32458347597471));
#77864=CARTESIAN_POINT('Ctrl Pts',(0.236110089081015,0.0224746521514455,
-1.32465368468257));
#77865=CARTESIAN_POINT('Ctrl Pts',(0.23640245663755,0.0192518967614226,
-1.32486885449985));
#77866=CARTESIAN_POINT('Ctrl Pts',(0.236569828329751,0.0170726151586642,
-1.32501261067615));
#77867=CARTESIAN_POINT('Ctrl Pts',(0.237864193052071,-0.00350225378583714,
-1.3263560205701));
#77868=CARTESIAN_POINT('Ctrl Pts',(0.236873663798885,-0.0219706016214408,
-1.32746154678167));
#77869=CARTESIAN_POINT('Ctrl Pts',(0.232010587234733,-0.0502905722377621,
-1.32923121290721));
#77870=CARTESIAN_POINT('Ctrl Pts',(0.229608381542239,-0.0603159563745694,
-1.3298720899765));
#77871=CARTESIAN_POINT('Ctrl Pts',(0.22536368248678,-0.0740244365331746,
-1.33079226410555));
#77872=CARTESIAN_POINT('Ctrl Pts',(0.22406591743754,-0.0778644213959656,
-1.3310549027869));
#77873=CARTESIAN_POINT('Ctrl Pts',(0.222015098974196,-0.08345596963305,
-1.33144557234544));
#77874=CARTESIAN_POINT('Ctrl Pts',(0.221338258356063,-0.0852348407468056,
-1.33157110218501));
#77875=CARTESIAN_POINT('Ctrl Pts',(0.220096481854711,-0.088383908571288,
-1.33179564201375));
#77876=CARTESIAN_POINT('Ctrl Pts',(0.219539968033937,-0.0897573333198564,
-1.33189436618155));
#77877=CARTESIAN_POINT('Ctrl Pts',(0.218336419208842,-0.0926494113637381,
-1.33210398376296));
#77878=CARTESIAN_POINT('Ctrl Pts',(0.217686329143207,-0.0941666992343994,
-1.33221497620264));
#77879=CARTESIAN_POINT('Ctrl Pts',(0.215899189980714,-0.0982203965159218,
-1.33251432423628));
#77880=CARTESIAN_POINT('Ctrl Pts',(0.214733332043485,-0.100743741718888,
-1.33270365015046));
#77881=CARTESIAN_POINT('Ctrl Pts',(0.207736208029548,-0.115214530628078,
-1.33380724406798));
#77882=CARTESIAN_POINT('Ctrl Pts',(0.200953900236698,-0.126673377471663,
-1.33475435316393));
#77883=CARTESIAN_POINT('Ctrl Pts',(0.185694362214561,-0.14811947391486,
-1.33666491128915));
#77884=CARTESIAN_POINT('Ctrl Pts',(0.177277843696724,-0.158096004707518,
-1.33762422415913));
#77885=CARTESIAN_POINT('Ctrl Pts',(0.164064856101045,-0.171368502915784,
-1.33896807698471));
#77886=CARTESIAN_POINT('Ctrl Pts',(0.159900698971384,-0.175260431693226,
-1.33937159561583));
#77887=CARTESIAN_POINT('Ctrl Pts',(0.154476371922974,-0.179975686919883,
-1.33986863855301));
#77888=CARTESIAN_POINT('Ctrl Pts',(0.15334349266036,-0.180941899260514,
-1.33997094605253));
#77889=CARTESIAN_POINT('Ctrl Pts',(0.151506698747924,-0.18247882542219,
-1.34013432430975));
#77890=CARTESIAN_POINT('Ctrl Pts',(0.1508085030203,-0.183056267249122,-1.34019585659972));
#77891=CARTESIAN_POINT('Ctrl Pts',(0.14945111682113,-0.184165854448735,
-1.34031435641435));
#77892=CARTESIAN_POINT('Ctrl Pts',(0.148792360823586,-0.184698488493589,
-1.34037135636453));
#77893=CARTESIAN_POINT('Ctrl Pts',(0.147310739668852,-0.185883374963248,
-1.34049845419781));
#77894=CARTESIAN_POINT('Ctrl Pts',(0.146486357613181,-0.186533724148596,
-1.34056842003342));
#77895=CARTESIAN_POINT('Ctrl Pts',(0.143554273847945,-0.188815397866359,
-1.34081473039456));
#77896=CARTESIAN_POINT('Ctrl Pts',(0.14142333486013,-0.190416716207678,
-1.34098914443833));
#77897=CARTESIAN_POINT('Ctrl Pts',(0.124879274300976,-0.202417959823925,
-1.34231233260961));
#77898=CARTESIAN_POINT('Ctrl Pts',(0.109363508111551,-0.211205235718552,
-1.34337951637296));
#77899=CARTESIAN_POINT('Ctrl Pts',(0.0854046120766593,-0.221419021527631,
-1.34498397526705));
#77900=CARTESIAN_POINT('Ctrl Pts',(0.0776355624248473,-0.224261087058582,
-1.34549757559088));
#77901=CARTESIAN_POINT('Ctrl Pts',(0.066228833926949,-0.227770003344585,
-1.34625536969454));
#77902=CARTESIAN_POINT('Ctrl Pts',(0.0626988273682074,-0.228766885251032,
-1.34649033735879));
#77903=CARTESIAN_POINT('Ctrl Pts',(0.0562717487439546,-0.230421977725582,
-1.34692001570409));
#77904=CARTESIAN_POINT('Ctrl Pts',(0.0533826951552514,-0.23110838173588,
-1.34711383349519));
#77905=CARTESIAN_POINT('Ctrl Pts',(0.0488295217204145,-0.232100231310048,
-1.34742072270118));
#77906=CARTESIAN_POINT('Ctrl Pts',(0.0471736614122442,-0.232442433703559,
-1.34753262292408));
#77907=CARTESIAN_POINT('Ctrl Pts',(0.0440660050542402,-0.233050092550856,
-1.34774324859984));
#77908=CARTESIAN_POINT('Ctrl Pts',(0.0426151082761807,-0.233319760880015,
-1.34784183488974));
#77909=CARTESIAN_POINT('Ctrl Pts',(0.0393505874012215,-0.233895049812903,
-1.34806425908346));
#77910=CARTESIAN_POINT('Ctrl Pts',(0.0375357521951193,-0.234193146851851,
-1.34818832849976));
#77911=CARTESIAN_POINT('Ctrl Pts',(0.032172644630773,-0.23501012839468,
-1.34855629164672));
#77912=CARTESIAN_POINT('Ctrl Pts',(0.0286159991199586,-0.235469661897079,
-1.34880201926783));
#77913=CARTESIAN_POINT('Ctrl Pts',(0.00614476469676354,-0.237856427884637,
-1.35036605240399));
#77914=CARTESIAN_POINT('Ctrl Pts',(-0.0129308310718226,-0.237583616622203,
-1.35175308476257));
#77915=CARTESIAN_POINT('Ctrl Pts',(-0.0418664844139423,-0.233673028299149,
-1.35388211840228));
#77916=CARTESIAN_POINT('Ctrl Pts',(-0.0518705825065041,-0.231657871601777,
-1.35462109642587));
#77917=CARTESIAN_POINT('Ctrl Pts',(-0.0639408871745872,-0.228405032857378,
-1.35549520514729));
#77918=CARTESIAN_POINT('Ctrl Pts',(-0.066158235293999,-0.227772660724465,
-1.35565501665582));
#77919=CARTESIAN_POINT('Ctrl Pts',(-0.0693935479898279,-0.226798737678322,
-1.35588672705042));
#77920=CARTESIAN_POINT('Ctrl Pts',(-0.0704189012452659,-0.226482472554529,
-1.35595994380997));
#77921=CARTESIAN_POINT('Ctrl Pts',(-0.0721587491312422,-0.225932866995077,
-1.35608376691195));
#77922=CARTESIAN_POINT('Ctrl Pts',(-0.0728743261634547,-0.225703075099686,
-1.35613457271426));
#77923=CARTESIAN_POINT('Ctrl Pts',(-0.0745065750487541,-0.225170341908694,
-1.35625017869265));
#77924=CARTESIAN_POINT('Ctrl Pts',(-0.0754225027486349,-0.224865201314728,
-1.35631485027713));
#77925=CARTESIAN_POINT('Ctrl Pts',(-0.077961009318451,-0.224002244260091,
-1.35649359863398));
#77926=CARTESIAN_POINT('Ctrl Pts',(-0.0795794744509733,-0.22343238814436,
-1.35660700428359));
#77927=CARTESIAN_POINT('Ctrl Pts',(-0.0909210014600033,-0.219300199747203,
-1.35739871354855));
#77928=CARTESIAN_POINT('Ctrl Pts',(-0.100409034682874,-0.215121561267084,
-1.35804573589368));
#77929=CARTESIAN_POINT('Ctrl Pts',(-0.111254590787385,-0.209470524493601,
-1.35880037274307));
#77930=CARTESIAN_POINT('Ctrl Pts',(-0.112904367507583,-0.208585925957488,
-1.35891558519284));
#77931=CARTESIAN_POINT('Ctrl Pts',(-0.121632093978949,-0.20377229263534,
-1.35952815769962));
#77932=CARTESIAN_POINT('Ctrl Pts',(-0.128515798566275,-0.199502385177493,
-1.36002235270214));
#77933=CARTESIAN_POINT('Ctrl Pts',(-0.141427876311033,-0.190547050241054,
-1.36099272085092));
#77934=CARTESIAN_POINT('Ctrl Pts',(-0.147474841390952,-0.185906376444795,
-1.36146765496924));
#77935=CARTESIAN_POINT('Ctrl Pts',(-0.157181338721424,-0.177685235778625,
-1.36227695095893));
#77936=CARTESIAN_POINT('Ctrl Pts',(-0.160967273026642,-0.174262868422231,
-1.36260568339115));
#77937=CARTESIAN_POINT('Ctrl Pts',(-0.166134703692136,-0.169279515983874,
-1.36307533320037));
#77938=CARTESIAN_POINT('Ctrl Pts',(-0.167610665108986,-0.167818231405802,
-1.36321201742534));
#77939=CARTESIAN_POINT('Ctrl Pts',(-0.170124435174203,-0.165263213163865,
-1.36344937490728));
#77940=CARTESIAN_POINT('Ctrl Pts',(-0.171171372744094,-0.164178604096371,
-1.36354964165154));
#77941=CARTESIAN_POINT('Ctrl Pts',(-0.173163692109138,-0.16207482406146,
-1.36374323387447));
#77942=CARTESIAN_POINT('Ctrl Pts',(-0.174110595073983,-0.161057174321265,
-1.36383648813062));
#77943=CARTESIAN_POINT('Ctrl Pts',(-0.176582349273387,-0.158353472756012,
-1.36408326493934));
#77944=CARTESIAN_POINT('Ctrl Pts',(-0.178091968086203,-0.156653754142891,
-1.36423741703766));
#77945=CARTESIAN_POINT('Ctrl Pts',(-0.183521678072306,-0.150360372009771,
-1.36480479692139));
#77946=CARTESIAN_POINT('Ctrl Pts',(-0.187290082216158,-0.145639492109189,
-1.36522403431857));
#77947=CARTESIAN_POINT('Ctrl Pts',(-0.200632579960041,-0.127549351721758,
-1.3668082445995));
#77948=CARTESIAN_POINT('Ctrl Pts',(-0.208988026649325,-0.113340841070711,
-1.36801339816816));
#77949=CARTESIAN_POINT('Ctrl Pts',(-0.218682357394607,-0.0920764815813074,
-1.36971514978385));
#77950=CARTESIAN_POINT('Ctrl Pts',(-0.221280623977151,-0.085644318545201,
-1.37021710475253));
#77951=CARTESIAN_POINT('Ctrl Pts',(-0.224919421688914,-0.0753593957652675,
-1.37099160631891));
#77952=CARTESIAN_POINT('Ctrl Pts',(-0.226151046528502,-0.0715785820053708,
-1.37127051310378));
#77953=CARTESIAN_POINT('Ctrl Pts',(-0.227664673022354,-0.0665020548682916,
-1.3716357744557));
#77954=CARTESIAN_POINT('Ctrl Pts',(-0.228031652133885,-0.0652326028274289,
-1.37172635288591));
#77955=CARTESIAN_POINT('Ctrl Pts',(-0.228622564107025,-0.0631225813856818,
-1.37187557599183));
#77956=CARTESIAN_POINT('Ctrl Pts',(-0.228852512332779,-0.0622837440740553,
-1.37193455229684));
#77957=CARTESIAN_POINT('Ctrl Pts',(-0.229307913214832,-0.0605858912948844,
-1.37205319678235));
#77958=CARTESIAN_POINT('Ctrl Pts',(-0.229533165143973,-0.0597268402924974,
-1.37211285343147));
#77959=CARTESIAN_POINT('Ctrl Pts',(-0.230102745793748,-0.0575037908385168,
-1.37226631851309));
#77960=CARTESIAN_POINT('Ctrl Pts',(-0.230439779837097,-0.0561379345016123,
-1.37235972209924));
#77961=CARTESIAN_POINT('Ctrl Pts',(-0.231768403757476,-0.0505398997054712,
-1.3727392295504));
#77962=CARTESIAN_POINT('Ctrl Pts',(-0.232655778509416,-0.0462835688121242,
-1.3730200682004));
#77963=CARTESIAN_POINT('Ctrl Pts',(-0.235907615415331,-0.0282127848867452,
-1.37418923518371));
#77964=CARTESIAN_POINT('Ctrl Pts',(-0.2371624653087,-0.0142266276722643,
-1.37503872842268));
#77965=CARTESIAN_POINT('Ctrl Pts',(-0.23718716775891,0.0136027218036718,
-1.37674851656479));
#77966=CARTESIAN_POINT('Ctrl Pts',(-0.235992727765574,0.0273888476668221,
-1.37760563568916));
#77967=CARTESIAN_POINT('Ctrl Pts',(-0.233124288714224,0.0437356559762051,
-1.37868215379816));
#77968=CARTESIAN_POINT('Ctrl Pts',(-0.232594510634388,0.0464707881844598,
-1.37886425701086));
#77969=CARTESIAN_POINT('Ctrl Pts',(-0.231674030153142,0.0508119425741966,
-1.37915676692936));
#77970=CARTESIAN_POINT('Ctrl Pts',(-0.231314495548988,0.0524243614375532,
-1.37926618278226));
#77971=CARTESIAN_POINT('Ctrl Pts',(-0.23060061972385,0.0554754893528476,
-1.37947475347017));
#77972=CARTESIAN_POINT('Ctrl Pts',(-0.23024958230856,0.0569148962185885,
-1.37957379812391));
#77973=CARTESIAN_POINT('Ctrl Pts',(-0.229417443049485,0.060193276384009,
-1.37980091132009));
#77974=CARTESIAN_POINT('Ctrl Pts',(-0.228927678215585,0.062029924060232,
-1.37992925311125));
#77975=CARTESIAN_POINT('Ctrl Pts',(-0.2273282766491,0.0677506604950433,
-1.38033257786884));
#77976=CARTESIAN_POINT('Ctrl Pts',(-0.2261415070581,0.0716122383843702,
-1.38061001753718));
#77977=CARTESIAN_POINT('Ctrl Pts',(-0.221732005447868,0.0847549672293667,
-1.38157275132017));
#77978=CARTESIAN_POINT('Ctrl Pts',(-0.218031984731433,0.0938642587194592,
-1.38227265924416));
#77979=CARTESIAN_POINT('Ctrl Pts',(-0.211315873395721,0.107842070651639,
-1.38339454517707));
#77980=CARTESIAN_POINT('Ctrl Pts',(-0.208669935687468,0.11287677027982,
-1.38380896285301));
#77981=CARTESIAN_POINT('Ctrl Pts',(-0.199345160363129,0.129169465143316,
-1.38517916920891));
#77982=CARTESIAN_POINT('Ctrl Pts',(-0.191915117017114,0.139971040875455,
-1.3861363832532));
#77983=CARTESIAN_POINT('Ctrl Pts',(-0.182189411815351,0.151868985162163,
-1.3872105756967));
#77984=CARTESIAN_POINT('Ctrl Pts',(-0.180722215689246,0.153612018211657,
-1.3873684485579));
#77985=CARTESIAN_POINT('Ctrl Pts',(-0.178530673670137,0.156140704372718,
-1.38759789906506));
#77986=CARTESIAN_POINT('Ctrl Pts',(-0.177825821422167,0.156942978017678,
-1.38767075978209));
#77987=CARTESIAN_POINT('Ctrl Pts',(-0.176563199469565,0.15836068631454,
-1.38779958333208));
#77988=CARTESIAN_POINT('Ctrl Pts',(-0.176007588422428,0.158977983578156,
-1.38785569687315));
#77989=CARTESIAN_POINT('Ctrl Pts',(-0.174773130939952,0.160335090865518,
-1.38797910570813));
#77990=CARTESIAN_POINT('Ctrl Pts',(-0.174092819169678,0.161073520688348,
-1.38804629044477));
#77991=CARTESIAN_POINT('Ctrl Pts',(-0.172077662852082,0.163233146174379,
-1.38824296496984));
#77992=CARTESIAN_POINT('Ctrl Pts',(-0.170729922179254,0.164642267773295,
-1.38837153032768));
#77993=CARTESIAN_POINT('Ctrl Pts',(-0.160675323670463,0.174898536419804,
-1.38931052972371));
#77994=CARTESIAN_POINT('Ctrl Pts',(-0.151302082296147,0.183067800070646,
-1.39007706394631));
#77995=CARTESIAN_POINT('Ctrl Pts',(-0.12700778539669,0.201094815634018,
-1.39193486728141));
#77996=CARTESIAN_POINT('Ctrl Pts',(-0.111532908806243,0.210072455227272,
-1.39301956879735));
#77997=CARTESIAN_POINT('Ctrl Pts',(-0.0924504341320403,0.218435120028361,
-1.39436378176224));
#77998=CARTESIAN_POINT('Ctrl Pts',(-0.0896796213965928,0.219587223322597,
-1.3945589588842));
#77999=CARTESIAN_POINT('Ctrl Pts',(-0.0851459530671215,0.221372201549348,
-1.39487873152857));
#78000=CARTESIAN_POINT('Ctrl Pts',(-0.0833960972814792,0.22203732921867,
-1.39500225239986));
#78001=CARTESIAN_POINT('Ctrl Pts',(-0.0802503654460852,0.223190603902801,
-1.39522457474318));
#78002=CARTESIAN_POINT('Ctrl Pts',(-0.0788574372384819,0.223686546863685,
-1.39532311168139));
#78003=CARTESIAN_POINT('Ctrl Pts',(-0.075882460446758,0.224714526803235,
-1.39553380579502));
#78004=CARTESIAN_POINT('Ctrl Pts',(-0.0742992573673935,0.225242949873987,
-1.39564607589331));
#78005=CARTESIAN_POINT('Ctrl Pts',(-0.0699825768934366,0.226633258658918,
-1.39595264325985));
#78006=CARTESIAN_POINT('Ctrl Pts',(-0.067238917008975,0.227462352465796,
-1.39614799367707));
#78007=CARTESIAN_POINT('Ctrl Pts',(-0.0611085656142311,0.229194251556927,
-1.39658576016739));
#78008=CARTESIAN_POINT('Ctrl Pts',(-0.057715581113362,0.23007210007809,
-1.39682891304125));
#78009=CARTESIAN_POINT('Ctrl Pts',(-0.0502043344891319,0.23183883889443,
-1.39736916411075));
#78010=CARTESIAN_POINT('Ctrl Pts',(-0.0460799619130002,0.232693673874856,
-1.39766710396681));
#78011=CARTESIAN_POINT('Ctrl Pts',(-0.0419358227397264,0.233438144689642,
-1.39796759050954));
#78012=CARTESIAN_POINT('',(-0.236838115873986,0.000105245926622949,-1.39566205967354));
#78013=CARTESIAN_POINT('Ctrl Pts',(-0.0420041065163025,0.233814670441123,
-1.41782827198422));
#78014=CARTESIAN_POINT('Ctrl Pts',(-0.117770216984918,0.220073149264774,
-1.41263777999286));
#78015=CARTESIAN_POINT('Ctrl Pts',(-0.215515586929785,0.143319562669835,
-1.40524805039436));
#78016=CARTESIAN_POINT('Ctrl Pts',(-0.23696289445876,0.0329890296572519,
-1.39785832079586));
#78017=CARTESIAN_POINT('Ctrl Pts',(-0.236832944309853,0.000105455023683012,
-1.39565908318872));
#78018=CARTESIAN_POINT('Ctrl Pts',(-0.237174982301523,9.16257185350831E-5,
-1.39585594256495));
#78019=CARTESIAN_POINT('Ctrl Pts',(-0.237175795591863,-0.00201359239129307,
-1.39572069814429));
#78020=CARTESIAN_POINT('Ctrl Pts',(-0.237148579287857,-0.00411868598000703,
-1.39558469481686));
#78021=CARTESIAN_POINT('Ctrl Pts',(-0.237045465987812,-0.00804719088092806,
-1.39532926879552));
#78022=CARTESIAN_POINT('Ctrl Pts',(-0.236976540307452,-0.00987062676514676,
-1.39521006031992));
#78023=CARTESIAN_POINT('Ctrl Pts',(-0.236813981095099,-0.0131638744504354,
-1.39499348396549));
#78024=CARTESIAN_POINT('Ctrl Pts',(-0.236727683409255,-0.0146339665759775,
-1.39489634447685));
#78025=CARTESIAN_POINT('Ctrl Pts',(-0.236532434782362,-0.0175030501932012,
-1.39470581431299));
#78026=CARTESIAN_POINT('Ctrl Pts',(-0.236424747294716,-0.0189020684782139,
-1.39461246665617));
#78027=CARTESIAN_POINT('Ctrl Pts',(-0.236170031794636,-0.0218671122183269,
-1.39441365117725));
#78028=CARTESIAN_POINT('Ctrl Pts',(-0.23601982691454,-0.0234327892487353,
-1.39430808836039));
#78029=CARTESIAN_POINT('Ctrl Pts',(-0.235599560070182,-0.0273981586514169,
-1.39403920592918));
#78030=CARTESIAN_POINT('Ctrl Pts',(-0.235308406271673,-0.0297953854104867,
-1.39387523499128));
#78031=CARTESIAN_POINT('Ctrl Pts',(-0.233995106208499,-0.0393829120711009,
-1.39321351841015));
#78032=CARTESIAN_POINT('Ctrl Pts',(-0.232679643410945,-0.0465283554801728,
-1.39270677819602));
#78033=CARTESIAN_POINT('Ctrl Pts',(-0.226771417425548,-0.0719945443090971,
-1.39085145013459));
#78034=CARTESIAN_POINT('Ctrl Pts',(-0.220323080727087,-0.0898114322158612,
-1.38945327950828));
#78035=CARTESIAN_POINT('Ctrl Pts',(-0.209863928409587,-0.11058151213702,
-1.38777817708755));
#78036=CARTESIAN_POINT('Ctrl Pts',(-0.207787332795316,-0.114435868906816,
-1.38746562333672));
#78037=CARTESIAN_POINT('Ctrl Pts',(-0.204158098086563,-0.120747164986921,
-1.38695338834692));
#78038=CARTESIAN_POINT('Ctrl Pts',(-0.202664906651683,-0.123236943953029,
-1.3867511984491));
#78039=CARTESIAN_POINT('Ctrl Pts',(-0.200503856833246,-0.126694764578667,
-1.38647088306876));
#78040=CARTESIAN_POINT('Ctrl Pts',(-0.199874007993179,-0.127686103590465,
-1.38639057583588));
#78041=CARTESIAN_POINT('Ctrl Pts',(-0.198779900430429,-0.129380219067176,
-1.38625349162518));
#78042=CARTESIAN_POINT('Ctrl Pts',(-0.198319220977252,-0.130085266592673,
-1.38619648823444));
#78043=CARTESIAN_POINT('Ctrl Pts',(-0.197337523094531,-0.131570370726676,
-1.3860765347672));
#78044=CARTESIAN_POINT('Ctrl Pts',(-0.196815621810583,-0.132349807561635,
-1.38601364345898));
#78045=CARTESIAN_POINT('Ctrl Pts',(-0.195370665223989,-0.134480337425429,
-1.38584185237002));
#78046=CARTESIAN_POINT('Ctrl Pts',(-0.194438210913681,-0.135825036305808,
-1.38573355588428));
#78047=CARTESIAN_POINT('Ctrl Pts',(-0.189359997957431,-0.142988880159454,
-1.38515668575407));
#78048=CARTESIAN_POINT('Ctrl Pts',(-0.184966395026557,-0.148628672811585,
-1.38470277128628));
#78049=CARTESIAN_POINT('Ctrl Pts',(-0.171025782779141,-0.164945692672423,
-1.3833615865507));
#78050=CARTESIAN_POINT('Ctrl Pts',(-0.160760697703925,-0.174965508282461,
-1.38249770756623));
#78051=CARTESIAN_POINT('Ctrl Pts',(-0.144191356434958,-0.188442089055549,
-1.38117532017615));
#78052=CARTESIAN_POINT('Ctrl Pts',(-0.138533517504667,-0.192639616371909,
-1.38073489731501));
#78053=CARTESIAN_POINT('Ctrl Pts',(-0.128693970697739,-0.199281649724844,
-1.37997814834188));
#78054=CARTESIAN_POINT('Ctrl Pts',(-0.124608921676507,-0.201861154109281,
-1.3796664932836));
#78055=CARTESIAN_POINT('Ctrl Pts',(-0.118695529821715,-0.205347245374128,
-1.37921713526175));
#78056=CARTESIAN_POINT('Ctrl Pts',(-0.116929702195988,-0.206357854953375,
-1.37908317397037));
#78057=CARTESIAN_POINT('Ctrl Pts',(-0.113839706381855,-0.20807391034005,
-1.37884902382019));
#78058=CARTESIAN_POINT('Ctrl Pts',(-0.112521422928308,-0.208789750992499,
-1.37874921160514));
#78059=CARTESIAN_POINT('Ctrl Pts',(-0.109960056442997,-0.210149294559195,
-1.37855539675321));
#78060=CARTESIAN_POINT('Ctrl Pts',(-0.108717887783892,-0.21079459373373,
-1.37846145563664));
#78061=CARTESIAN_POINT('Ctrl Pts',(-0.105394781135523,-0.212483741716781,
-1.37821023691871));
#78062=CARTESIAN_POINT('Ctrl Pts',(-0.103304107563149,-0.213507988314395,
-1.37805228603065));
#78063=CARTESIAN_POINT('Ctrl Pts',(-0.0953664499642538,-0.217252866477978,
-1.3774527689252));
#78064=CARTESIAN_POINT('Ctrl Pts',(-0.0894248714691551,-0.219765207759282,
-1.37700426445785));
#78065=CARTESIAN_POINT('Ctrl Pts',(-0.0683516447625824,-0.227679694220197,
-1.37541386197654));
#78066=CARTESIAN_POINT('Ctrl Pts',(-0.0527810137464234,-0.23178447326964,
-1.37423581249133));
#78067=CARTESIAN_POINT('Ctrl Pts',(-0.0301738899954698,-0.235346815644265,
-1.37256974293882));
#78068=CARTESIAN_POINT('Ctrl Pts',(-0.0233870183136434,-0.236117865204951,
-1.37207572631368));
#78069=CARTESIAN_POINT('Ctrl Pts',(-0.0139107578500921,-0.236781776307064,
-1.37140153904671));
#78070=CARTESIAN_POINT('Ctrl Pts',(-0.0112424714038401,-0.236923462113636,
-1.37121342717392));
#78071=CARTESIAN_POINT('Ctrl Pts',(-0.00656159139933815,-0.237092754332976,
-1.37088706128202));
#78072=CARTESIAN_POINT('Ctrl Pts',(-0.00455001009005155,-0.237139888496981,
-1.37074798185936));
#78073=CARTESIAN_POINT('Ctrl Pts',(-0.00152161308756375,-0.237172296994421,
-1.37054060383575));
#78074=CARTESIAN_POINT('Ctrl Pts',(-0.000505151697553854,-0.237176640261484,
-1.37047133843824));
#78075=CARTESIAN_POINT('Ctrl Pts',(0.00134100771431228,-0.237172660086146,
-1.37034618890469));
#78076=CARTESIAN_POINT('Ctrl Pts',(0.00217065689784853,-0.237166518062558,
-1.37029019138569));
#78077=CARTESIAN_POINT('Ctrl Pts',(0.00405295482133211,-0.237142704808126,
-1.37016368956015));
#78078=CARTESIAN_POINT('Ctrl Pts',(0.00510553519943075,-0.23712237874548,
-1.37009333139362));
#78079=CARTESIAN_POINT('Ctrl Pts',(0.00835567896387067,-0.23703796412398,
-1.36987716249979));
#78080=CARTESIAN_POINT('Ctrl Pts',(0.0105525843125146,-0.236950327318595,
-1.36973257317255));
#78081=CARTESIAN_POINT('Ctrl Pts',(0.0273038899655948,-0.236048648851461,
-1.36863958271983));
#78082=CARTESIAN_POINT('Ctrl Pts',(0.0417585545839553,-0.233924785151911,
-1.36774993578599));
#78083=CARTESIAN_POINT('Ctrl Pts',(0.0715141225821607,-0.226704509336095,
-1.36587224954963));
#78084=CARTESIAN_POINT('Ctrl Pts',(0.086674210281199,-0.221351982902229,
-1.36488651062116));
#78085=CARTESIAN_POINT('Ctrl Pts',(0.103792165335796,-0.213278045697669,
-1.36366019814956));
#78086=CARTESIAN_POINT('Ctrl Pts',(0.106384023197842,-0.211997115050351,
-1.36347138073069));
#78087=CARTESIAN_POINT('Ctrl Pts',(0.110438665317319,-0.209900176644186,
-1.36317064796775));
#78088=CARTESIAN_POINT('Ctrl Pts',(0.111917382467928,-0.20911547578414,
-1.36305982543613));
#78089=CARTESIAN_POINT('Ctrl Pts',(0.114685203164893,-0.207608928758897,
-1.36285015616172));
#78090=CARTESIAN_POINT('Ctrl Pts',(0.115976115328242,-0.206890559545931,
-1.36275143650084));
#78091=CARTESIAN_POINT('Ctrl Pts',(0.118879401727701,-0.205239222476864,
-1.3625272560819));
#78092=CARTESIAN_POINT('Ctrl Pts',(0.120487648312623,-0.20429923362212,
-1.36240154759485));
#78093=CARTESIAN_POINT('Ctrl Pts',(0.125371833381066,-0.201366792257235,
-1.36201498170954));
#78094=CARTESIAN_POINT('Ctrl Pts',(0.128610530848772,-0.199313848033501,
-1.36175195100742));
#78095=CARTESIAN_POINT('Ctrl Pts',(0.147408743599202,-0.186749074880236,
-1.36018431420591));
#78096=CARTESIAN_POINT('Ctrl Pts',(0.161722856494158,-0.174499367397765,
-1.35881371746332));
#78097=CARTESIAN_POINT('Ctrl Pts',(0.181297658453648,-0.153250026796478,
-1.35670728516821));
#78098=CARTESIAN_POINT('Ctrl Pts',(0.187672041552431,-0.145374193498671,
-1.35597377334996));
#78099=CARTESIAN_POINT('Ctrl Pts',(0.194852651797957,-0.135239436809794,
-1.35510534651962));
#78100=CARTESIAN_POINT('Ctrl Pts',(0.196153871236581,-0.133345119725638,
-1.35494607119793));
#78101=CARTESIAN_POINT('Ctrl Pts',(0.198021123735284,-0.130540273619924,
-1.35471499893364));
#78102=CARTESIAN_POINT('Ctrl Pts',(0.198608801361587,-0.129644408345657,
-1.35464189361358));
#78103=CARTESIAN_POINT('Ctrl Pts',(0.199598156337058,-0.128113702891585,
-1.35451820835669));
#78104=CARTESIAN_POINT('Ctrl Pts',(0.200002914161758,-0.127480897653863,
-1.35446742993155));
#78105=CARTESIAN_POINT('Ctrl Pts',(0.200921251712227,-0.126030012967184,
-1.35435181902011));
#78106=CARTESIAN_POINT('Ctrl Pts',(0.201432848084865,-0.125210707821098,
-1.35428711566809));
#78107=CARTESIAN_POINT('Ctrl Pts',(0.202840876952476,-0.122924828870483,
-1.35410813463067));
#78108=CARTESIAN_POINT('Ctrl Pts',(0.203726414729484,-0.12145156762085,
-1.35399453117514));
#78109=CARTESIAN_POINT('Ctrl Pts',(0.210226453817895,-0.110366337578196,
-1.35315173395839));
#78110=CARTESIAN_POINT('Ctrl Pts',(0.215174792269841,-0.100378106010538,
-1.35245881617375));
#78111=CARTESIAN_POINT('Ctrl Pts',(0.222782022996827,-0.0818491244441361,
-1.35122523740475));
#78112=CARTESIAN_POINT('Ctrl Pts',(0.225694831281892,-0.0734367244527316,
-1.3506829883356));
#78113=CARTESIAN_POINT('Ctrl Pts',(0.230261477039953,-0.0573798313792536,
-1.34965285573392));
#78114=CARTESIAN_POINT('Ctrl Pts',(0.232023358021294,-0.0497789178323422,
-1.34916719705328));
#78115=CARTESIAN_POINT('Ctrl Pts',(0.234035136962451,-0.038626802490816,
-1.34844661960073));
#78116=CARTESIAN_POINT('Ctrl Pts',(0.234584790326267,-0.0351347325073054,
-1.34821989688206));
#78117=CARTESIAN_POINT('Ctrl Pts',(0.235440978611729,-0.02877239247986,
-1.34780391957597));
#78118=CARTESIAN_POINT('Ctrl Pts',(0.235773551713395,-0.0259062949418869,
-1.34761547137768));
#78119=CARTESIAN_POINT('Ctrl Pts',(0.236216212096634,-0.0213700714723223,
-1.34731519281886));
#78120=CARTESIAN_POINT('Ctrl Pts',(0.236361054432868,-0.0197035661360794,
-1.34720444959608));
#78121=CARTESIAN_POINT('Ctrl Pts',(0.236600606918957,-0.0165624993218356,
-1.34699484829193));
#78122=CARTESIAN_POINT('Ctrl Pts',(0.236699189686879,-0.0150883070682883,
-1.34689611638911));
#78123=CARTESIAN_POINT('Ctrl Pts',(0.23689101747421,-0.0117517399937514,
-1.3466717958064));
#78124=CARTESIAN_POINT('Ctrl Pts',(0.236976084545565,-0.00988901217047821,
-1.34654595812243));
#78125=CARTESIAN_POINT('Ctrl Pts',(0.237169259861288,-0.00418344827775827,
-1.34615856922182));
#78126=CARTESIAN_POINT('Ctrl Pts',(0.237205904563023,-0.000338989302938372,
-1.34589483111555));
#78127=CARTESIAN_POINT('Ctrl Pts',(0.236871841173798,0.0222671988442763,
-1.34432720994275));
#78128=CARTESIAN_POINT('Ctrl Pts',(0.234368863128452,0.040927873908069,
-1.34295747228143));
#78129=CARTESIAN_POINT('Ctrl Pts',(0.227174308725929,0.0688924206830977,
-1.34085223027819));
#78130=CARTESIAN_POINT('Ctrl Pts',(0.224029002892859,0.0785199187998523,
-1.34011901554371));
#78131=CARTESIAN_POINT('Ctrl Pts',(0.219426395991204,0.0900517411378575,
-1.3392508963785));
#78132=CARTESIAN_POINT('Ctrl Pts',(0.218543722445539,0.092173215703996,
-1.33909164955469));
#78133=CARTESIAN_POINT('Ctrl Pts',(0.217204453602668,0.0952646506539745,
-1.33886061031242));
#78134=CARTESIAN_POINT('Ctrl Pts',(0.216771921517342,0.0962448049618629,
-1.3387875100461));
#78135=CARTESIAN_POINT('Ctrl Pts',(0.216024834939209,0.0979071783471902,
-1.33866382986567));
#78136=CARTESIAN_POINT('Ctrl Pts',(0.215713662010635,0.0985908766693289,
-1.33861305152136));
#78137=CARTESIAN_POINT('Ctrl Pts',(0.214994913400916,0.10015039153322,-1.33849743543056));
#78138=CARTESIAN_POINT('Ctrl Pts',(0.21458522999125,0.101025209055305,-1.3384327268686));
#78139=CARTESIAN_POINT('Ctrl Pts',(0.213431628067686,0.103449872220064,
-1.33825372142323));
#78140=CARTESIAN_POINT('Ctrl Pts',(0.212676169725761,0.104994205427463,
-1.33814009902433));
#78141=CARTESIAN_POINT('Ctrl Pts',(0.206890292448835,0.116503146728735,
-1.3372952683115));
#78142=CARTESIAN_POINT('Ctrl Pts',(0.20117814328167,0.126111048115842,-1.33660053908841));
#78143=CARTESIAN_POINT('Ctrl Pts',(0.189763808172186,0.142548011093985,
-1.3353681695696));
#78144=CARTESIAN_POINT('Ctrl Pts',(0.184315403321145,0.14952615434846,-1.33482887280208));
#78145=CARTESIAN_POINT('Ctrl Pts',(0.173347475914995,0.16206053202378,-1.3338011356029));
#78146=CARTESIAN_POINT('Ctrl Pts',(0.167918253949125,0.167679485535629,
-1.33331482406106));
#78147=CARTESIAN_POINT('Ctrl Pts',(0.159641141388833,0.175440028456389,
-1.33259337360236));
#78148=CARTESIAN_POINT('Ctrl Pts',(0.157006486954748,0.177801739966896,
-1.33236645395149));
#78149=CARTESIAN_POINT('Ctrl Pts',(0.15212762339867,0.181982149874415,-1.33195014815748));
#78150=CARTESIAN_POINT('Ctrl Pts',(0.149901115409691,0.183820486064305,
-1.33176157038228));
#78151=CARTESIAN_POINT('Ctrl Pts',(0.146332174026146,0.186659248869644,
-1.33146113083248));
#78152=CARTESIAN_POINT('Ctrl Pts',(0.145011711086444,0.187686930153582,
-1.3313503581488));
#78153=CARTESIAN_POINT('Ctrl Pts',(0.142505016609965,0.189595579503373,
-1.3311407288982));
#78154=CARTESIAN_POINT('Ctrl Pts',(0.141321206011921,0.190479605438435,
-1.3310419988192));
#78155=CARTESIAN_POINT('Ctrl Pts',(0.138625310871336,0.192453834847101,
-1.33081772036805));
#78156=CARTESIAN_POINT('Ctrl Pts',(0.137108492871284,0.193537376751465,
-1.33069192341743));
#78157=CARTESIAN_POINT('Ctrl Pts',(0.133138619880586,0.196303172093216,
-1.33036360778821));
#78158=CARTESIAN_POINT('Ctrl Pts',(0.130666475369076,0.197957314342616,
-1.33016005360139));
#78159=CARTESIAN_POINT('Ctrl Pts',(0.110219399975613,0.211088802328886,
-1.32848306639413));
#78160=CARTESIAN_POINT('Ctrl Pts',(0.0908051149535009,0.220138292566319,
-1.32691880170839));
#78161=CARTESIAN_POINT('Ctrl Pts',(0.064329074535868,0.228374325356081,
-1.3249025942938));
#78162=CARTESIAN_POINT('Ctrl Pts',(0.0581337950144433,0.230029420994305,
-1.32443965199956));
#78163=CARTESIAN_POINT('Ctrl Pts',(0.0493729297070068,0.231993295038763,
-1.32380321942766));
#78164=CARTESIAN_POINT('Ctrl Pts',(0.0468580686445437,0.232514295676086,
-1.32362260612725));
#78165=CARTESIAN_POINT('Ctrl Pts',(0.0424176602872986,0.233359234992425,
-1.32330789890318));
#78166=CARTESIAN_POINT('Ctrl Pts',(0.0404956762459849,0.233700430637499,
-1.32317305426759));
#78167=CARTESIAN_POINT('Ctrl Pts',(0.0375786990151602,0.234181191834915,
-1.32297069405255));
#78168=CARTESIAN_POINT('Ctrl Pts',(0.0365867245435667,0.234338219052782,
-1.32290227740962));
#78169=CARTESIAN_POINT('Ctrl Pts',(0.034772901804239,0.234613544490767,
-1.32277794397236));
#78170=CARTESIAN_POINT('Ctrl Pts',(0.0339514116270074,0.234733831496263,
-1.32272192279748));
#78171=CARTESIAN_POINT('Ctrl Pts',(0.0320728370872758,0.2349988340294,-1.32259446548958));
#78172=CARTESIAN_POINT('Ctrl Pts',(0.0310153901569653,0.235140733511951,
-1.32252318561633));
#78173=CARTESIAN_POINT('Ctrl Pts',(0.027701533066287,0.235562678027431,
-1.32230116156725));
#78174=CARTESIAN_POINT('Ctrl Pts',(0.0254419549091784,0.235817425295826,
-1.32215173598909));
#78175=CARTESIAN_POINT('Ctrl Pts',(0.0100281099386102,0.237331056319137,
-1.32114362932619));
#78176=CARTESIAN_POINT('Ctrl Pts',(-0.0032094353065917,0.23752133059925,
-1.32033253787148));
#78177=CARTESIAN_POINT('Ctrl Pts',(-0.0249624680853009,0.236013991717859,
-1.31899503856155));
#78178=CARTESIAN_POINT('Ctrl Pts',(-0.0334885117149788,0.234955656011327,
-1.31846975277959));
#78179=CARTESIAN_POINT('Ctrl Pts',(-0.0419358330286197,0.233438142841301,
-1.31793598285019));
#78180=CARTESIAN_POINT('Origin',(0.,0.,-1.7456589891905));
#78181=CARTESIAN_POINT('',(-0.0419358257152316,0.23343814415511,-1.19832585242651));
#78182=CARTESIAN_POINT('',(-0.0419358439263085,0.233438140883593,-1.21800162451869));
#78183=CARTESIAN_POINT('',(-0.0419358257166344,0.233438144154858,-1.7456589891905));
#78184=CARTESIAN_POINT('',(-0.237174995128926,4.80686365711195E-5,-1.27615111301349));
#78185=CARTESIAN_POINT('Ctrl Pts',(-0.0419358257152316,0.23343814415511,
-1.19832585242651));
#78186=CARTESIAN_POINT('Ctrl Pts',(-0.0396781609992177,0.233843720691884,
-1.19847529274218));
#78187=CARTESIAN_POINT('Ctrl Pts',(-0.0374146269178974,0.234216542598402,
-1.19862326078251));
#78188=CARTESIAN_POINT('Ctrl Pts',(-0.0285556537828558,0.235543970926263,
-1.19919637462169));
#78189=CARTESIAN_POINT('Ctrl Pts',(-0.0219262080047059,0.236253341205789,
-1.19961236340081));
#78190=CARTESIAN_POINT('Ctrl Pts',(0.000180787645325519,0.237680105942458,
-1.2009818499977));
#78191=CARTESIAN_POINT('Ctrl Pts',(0.0156969032840805,0.237161270717864,
-1.20191685478394));
#78192=CARTESIAN_POINT('Ctrl Pts',(0.0380990898538144,0.234202844417619,
-1.20333619123462));
#78193=CARTESIAN_POINT('Ctrl Pts',(0.0451005198850373,0.232955878672664,
-1.20378943582846));
#78194=CARTESIAN_POINT('Ctrl Pts',(0.0543769107165645,0.230869864715835,
-1.20440883861378));
#78195=CARTESIAN_POINT('Ctrl Pts',(0.0567106868691924,0.230307707554651,
-1.20456627927336));
#78196=CARTESIAN_POINT('Ctrl Pts',(0.0605563704476955,0.229319368069006,
-1.20482858574294));
#78197=CARTESIAN_POINT('Ctrl Pts',(0.062073328870888,0.228913407679896,
-1.20493279935709));
#78198=CARTESIAN_POINT('Ctrl Pts',(0.0650426259917649,0.228087095526861,
-1.20513830687406));
#78199=CARTESIAN_POINT('Ctrl Pts',(0.0664951993510447,0.227667860320054,
-1.20523956031059));
#78200=CARTESIAN_POINT('Ctrl Pts',(0.0699577076530744,0.22663256364463,
-1.20548269202567));
#78201=CARTESIAN_POINT('Ctrl Pts',(0.0719636244782297,0.226003619488697,
-1.20562498324758));
#78202=CARTESIAN_POINT('Ctrl Pts',(0.0789697688816637,0.223704152810454,
-1.20612718131918));
#78203=CARTESIAN_POINT('Ctrl Pts',(0.0839221005964498,0.221893771513249,
-1.20649159192433));
#78204=CARTESIAN_POINT('Ctrl Pts',(0.096219655637753,0.216927684324084,
-1.20742101708266));
#78205=CARTESIAN_POINT('Ctrl Pts',(0.103472982827372,0.213563019050453,
-1.20799206242827));
#78206=CARTESIAN_POINT('Ctrl Pts',(0.124003784272244,0.202747499575129,
-1.20967050781545));
#78207=CARTESIAN_POINT('Ctrl Pts',(0.136751505430185,0.194377234375328,
-1.21079432348841));
#78208=CARTESIAN_POINT('Ctrl Pts',(0.152498099546546,0.181717375441858,
-1.21223908776855));
#78209=CARTESIAN_POINT('Ctrl Pts',(0.156287340208863,0.17846890581939,-1.21259138963));
#78210=CARTESIAN_POINT('Ctrl Pts',(0.161061041561957,0.174107722894649,
-1.21303844816714));
#78211=CARTESIAN_POINT('Ctrl Pts',(0.162141243888337,0.173102211390518,
-1.21313983170415));
#78212=CARTESIAN_POINT('Ctrl Pts',(0.163867309392779,0.171465160271841,
-1.2133020940107));
#78213=CARTESIAN_POINT('Ctrl Pts',(0.164519052923484,0.170839917960272,
-1.21336342353618));
#78214=CARTESIAN_POINT('Ctrl Pts',(0.165783615616239,0.169612827095649,
-1.21348251108903));
#78215=CARTESIAN_POINT('Ctrl Pts',(0.166396759807231,0.169011350738139,
-1.21354029273356));
#78216=CARTESIAN_POINT('Ctrl Pts',(0.16790662167669,0.167514039943685,-1.21368271905115));
#78217=CARTESIAN_POINT('Ctrl Pts',(0.168799468252138,0.166614305738228,
-1.21376706593619));
#78218=CARTESIAN_POINT('Ctrl Pts',(0.172162588837373,0.163170456603198,
-1.21408546098894));
#78219=CARTESIAN_POINT('Ctrl Pts',(0.174583046748999,0.16057807416605,-1.21431603071219));
#78220=CARTESIAN_POINT('Ctrl Pts',(0.180827942886438,0.153581397585631,
-1.21491789466115));
#78221=CARTESIAN_POINT('Ctrl Pts',(0.184549753430381,0.149088524521435,
-1.21528393254017));
#78222=CARTESIAN_POINT('Ctrl Pts',(0.198842250592816,0.130478517010214,
-1.21674085061775));
#78223=CARTESIAN_POINT('Ctrl Pts',(0.207988984039867,0.115340697901134,
-1.21779952652288));
#78224=CARTESIAN_POINT('Ctrl Pts',(0.218050138073271,0.0935252025029785,
-1.21931445631422));
#78225=CARTESIAN_POINT('Ctrl Pts',(0.220490833630498,0.0876162512605708,
-1.21972326080672));
#78226=CARTESIAN_POINT('Ctrl Pts',(0.223488593765181,0.0794368752657272,
-1.22029131915498));
#78227=CARTESIAN_POINT('Ctrl Pts',(0.224255306812717,0.0772458765030693,
-1.22044367973588));
#78228=CARTESIAN_POINT('Ctrl Pts',(0.225432292397446,0.0737171531548524,
-1.22068954780572));
#78229=CARTESIAN_POINT('Ctrl Pts',(0.225863112793076,0.0723864024691382,
-1.22078237794979));
#78230=CARTESIAN_POINT('Ctrl Pts',(0.226731882117881,0.0696195960241475,
-1.2209756485522));
#78231=CARTESIAN_POINT('Ctrl Pts',(0.227168015633163,0.0681830405171525,
-1.22107614331163));
#78232=CARTESIAN_POINT('Ctrl Pts',(0.228164627734883,0.0647846133648534,
-1.22131427371725));
#78233=CARTESIAN_POINT('Ctrl Pts',(0.228713478585986,0.0628194853493693,
-1.22145227851539));
#78234=CARTESIAN_POINT('Ctrl Pts',(0.230485094021345,0.0561451087257307,
-1.22192216362513));
#78235=CARTESIAN_POINT('Ctrl Pts',(0.231588217714727,0.0514056731071655,
-1.22225780712472));
#78236=CARTESIAN_POINT('Ctrl Pts',(0.233943604620991,0.0396608104487631,
-1.22309490510922));
#78237=CARTESIAN_POINT('Ctrl Pts',(0.235027791857391,0.0326268514051426,
-1.22360093432746));
#78238=CARTESIAN_POINT('Ctrl Pts',(0.237333114580107,0.0113560769014225,
-1.22514186521636));
#78239=CARTESIAN_POINT('Ctrl Pts',(0.237586244616119,-0.00295234577984794,
-1.22619448580137));
#78240=CARTESIAN_POINT('Ctrl Pts',(0.236038644205291,-0.0242411332845506,
-1.22773612715121));
#78241=CARTESIAN_POINT('Ctrl Pts',(0.235211990319785,-0.0312604157511371,
-1.228239924464));
#78242=CARTESIAN_POINT('Ctrl Pts',(0.233809942409609,-0.0398441548554468,
-1.22884277936169));
#78243=CARTESIAN_POINT('Ctrl Pts',(0.233530135095655,-0.0414526503106507,
-1.22895516511401));
#78244=CARTESIAN_POINT('Ctrl Pts',(0.233063559042569,-0.0439799579232817,
-1.22913069694454));
#78245=CARTESIAN_POINT('Ctrl Pts',(0.232887919902086,-0.0449007359914931,
-1.22919442812406));
#78246=CARTESIAN_POINT('Ctrl Pts',(0.232543988369845,-0.0466474491284448,
-1.22931487556662));
#78247=CARTESIAN_POINT('Ctrl Pts',(0.232376751692154,-0.0474735329551559,
-1.22937164375206));
#78248=CARTESIAN_POINT('Ctrl Pts',(0.231965421994281,-0.0494510762804358,
-1.22950709969876));
#78249=CARTESIAN_POINT('Ctrl Pts',(0.231717155560191,-0.0506016393946176,
-1.22958555358991));
#78250=CARTESIAN_POINT('Ctrl Pts',(0.230823825842356,-0.0545971764997261,
-1.2298569094147));
#78251=CARTESIAN_POINT('Ctrl Pts',(0.230134820968382,-0.0574321887449935,
-1.23004752217888));
#78252=CARTESIAN_POINT('Ctrl Pts',(0.22827411595513,-0.0645161081842341,
-1.23052061758942));
#78253=CARTESIAN_POINT('Ctrl Pts',(0.227035944427103,-0.0687465254732881,
-1.23080023310318));
#78254=CARTESIAN_POINT('Ctrl Pts',(0.222273633360089,-0.0834813442281059,
-1.23177167822095));
#78255=CARTESIAN_POINT('Ctrl Pts',(0.218132219259187,-0.0937713298240962,
-1.23244611814119));
#78256=CARTESIAN_POINT('Ctrl Pts',(0.207037229656744,-0.116583512461436,
-1.23400373231551));
#78257=CARTESIAN_POINT('Ctrl Pts',(0.19964055612945,-0.12883983746124,-1.2348887813357));
#78258=CARTESIAN_POINT('Ctrl Pts',(0.189542776674368,-0.142594647040605,
-1.23599567394002));
#78259=CARTESIAN_POINT('Ctrl Pts',(0.187859694490644,-0.144804805473468,
-1.23617727155203));
#78260=CARTESIAN_POINT('Ctrl Pts',(0.185115468171708,-0.148280031353603,
-1.23646916200283));
#78261=CARTESIAN_POINT('Ctrl Pts',(0.184079230590837,-0.149564504104685,
-1.23657847151481));
#78262=CARTESIAN_POINT('Ctrl Pts',(0.182087198706978,-0.151981672928404,
-1.23678696265033));
#78263=CARTESIAN_POINT('Ctrl Pts',(0.18113402392114,-0.153116432971608,
-1.23688603539549));
#78264=CARTESIAN_POINT('Ctrl Pts',(0.178932137356722,-0.155688457006322,
-1.23711338811316));
#78265=CARTESIAN_POINT('Ctrl Pts',(0.177676641527493,-0.157119750867539,
-1.23724194340613));
#78266=CARTESIAN_POINT('Ctrl Pts',(0.173692669004136,-0.16155275138188,
-1.23764665003713));
#78267=CARTESIAN_POINT('Ctrl Pts',(0.170904458612851,-0.164499535765807,
-1.23792528219711));
#78268=CARTESIAN_POINT('Ctrl Pts',(0.160691626878338,-0.174753187207367,
-1.23893046668008));
#78269=CARTESIAN_POINT('Ctrl Pts',(0.152863790928762,-0.181639996328916,
-1.23967383213728));
#78270=CARTESIAN_POINT('Ctrl Pts',(0.130141413392986,-0.199119037405477,
-1.24175106382711));
#78271=CARTESIAN_POINT('Ctrl Pts',(0.114436554812705,-0.208541362291877,
-1.24310518124741));
#78272=CARTESIAN_POINT('Ctrl Pts',(0.095781807183824,-0.216985628947662,
-1.24453562220305));
#78273=CARTESIAN_POINT('Ctrl Pts',(0.0937447002829357,-0.217873472025179,
-1.24468952566214));
#78274=CARTESIAN_POINT('Ctrl Pts',(0.0907201799775787,-0.219141387224933,
-1.24491434186391));
#78275=CARTESIAN_POINT('Ctrl Pts',(0.0897422860112767,-0.219543665039204,
-1.24498646761317));
#78276=CARTESIAN_POINT('Ctrl Pts',(0.0879920002586462,-0.220250033971538,
-1.24511451955892));
#78277=CARTESIAN_POINT('Ctrl Pts',(0.0872206674940196,-0.220556624928486,
-1.24517058888646));
#78278=CARTESIAN_POINT('Ctrl Pts',(0.0855045201920958,-0.221228351560247,
-1.24529453618946));
#78279=CARTESIAN_POINT('Ctrl Pts',(0.0845589617588538,-0.221591490332732,
-1.24536229706069));
#78280=CARTESIAN_POINT('Ctrl Pts',(0.0817455482092795,-0.222651341986079,
-1.24556242219509));
#78281=CARTESIAN_POINT('Ctrl Pts',(0.0798711502316693,-0.223330595177069,
-1.24569381248973));
#78282=CARTESIAN_POINT('Ctrl Pts',(0.0670709882815222,-0.227787403244509,
-1.24657938012724));
#78283=CARTESIAN_POINT('Ctrl Pts',(0.0558888660593665,-0.230785877723939,
-1.24729587153018));
#78284=CARTESIAN_POINT('Ctrl Pts',(0.0260674725651557,-0.23648644925664,
-1.2491625809012));
#78285=CARTESIAN_POINT('Ctrl Pts',(0.00725152689139191,-0.237808103174622,
-1.25030200564773));
#78286=CARTESIAN_POINT('Ctrl Pts',(-0.0144231909681409,-0.236753851291595,
-1.25170347451265));
#78287=CARTESIAN_POINT('Ctrl Pts',(-0.0173209390168144,-0.236559502945541,
-1.25189251951777));
#78288=CARTESIAN_POINT('Ctrl Pts',(-0.0220513610137182,-0.236154859415893,
-1.252204259333));
#78289=CARTESIAN_POINT('Ctrl Pts',(-0.0238864921757022,-0.23597630245453,
-1.25232596920424));
#78290=CARTESIAN_POINT('Ctrl Pts',(-0.0271867094215329,-0.235616303193861,
-1.25254632757373));
#78291=CARTESIAN_POINT('Ctrl Pts',(-0.0286525506330593,-0.235442542191863,
-1.25264473070611));
#78292=CARTESIAN_POINT('Ctrl Pts',(-0.0317905796184613,-0.235040821231997,
-1.2528565659177));
#78293=CARTESIAN_POINT('Ctrl Pts',(-0.0334621392098675,-0.234808674419038,
-1.25297012457245));
#78294=CARTESIAN_POINT('Ctrl Pts',(-0.0380523415256968,-0.23412117665255,
-1.25328401176368));
#78295=CARTESIAN_POINT('Ctrl Pts',(-0.0409650912407725,-0.233629120585648,
-1.2534854803568));
#78296=CARTESIAN_POINT('Ctrl Pts',(-0.0474481025143045,-0.232408973478222,
-1.25393921657003));
#78297=CARTESIAN_POINT('Ctrl Pts',(-0.0510122458592781,-0.231652761038222,
-1.25419230639155));
#78298=CARTESIAN_POINT('Ctrl Pts',(-0.0625175587552499,-0.228933264878961,
-1.25502127776127));
#78299=CARTESIAN_POINT('Ctrl Pts',(-0.070374328844154,-0.226641382848858,
-1.2556063129692));
#78300=CARTESIAN_POINT('Ctrl Pts',(-0.0942317461438074,-0.218321709650529,
-1.25743530348131));
#78301=CARTESIAN_POINT('Ctrl Pts',(-0.109711641892026,-0.210967685950249,
-1.25870104585965));
#78302=CARTESIAN_POINT('Ctrl Pts',(-0.127042903920494,-0.200306520281306,
-1.26013808603997));
#78303=CARTESIAN_POINT('Ctrl Pts',(-0.129783417054643,-0.198541856370272,
-1.26036580907024));
#78304=CARTESIAN_POINT('Ctrl Pts',(-0.133535341495015,-0.196015027913566,
-1.26067736169793));
#78305=CARTESIAN_POINT('Ctrl Pts',(-0.134578204515581,-0.195300500879943,
-1.26076393511293));
#78306=CARTESIAN_POINT('Ctrl Pts',(-0.136292950973946,-0.194105369206056,
-1.26090617988225));
#78307=CARTESIAN_POINT('Ctrl Pts',(-0.136968114323581,-0.193629539513505,
-1.26096215981674));
#78308=CARTESIAN_POINT('Ctrl Pts',(-0.138350642785387,-0.192644335562723,
-1.26107671087382));
#78309=CARTESIAN_POINT('Ctrl Pts',(-0.139057709045866,-0.192134572631307,
-1.26113525470778));
#78310=CARTESIAN_POINT('Ctrl Pts',(-0.14081623410786,-0.190851962547866,
-1.26128079903513));
#78311=CARTESIAN_POINT('Ctrl Pts',(-0.141864170670573,-0.190074303018333,
-1.26136747885913));
#78312=CARTESIAN_POINT('Ctrl Pts',(-0.144193762320322,-0.188315544821261,
-1.26156018525671));
#78313=CARTESIAN_POINT('Ctrl Pts',(-0.145471939960449,-0.187329924251805,
-1.26166592772791));
#78314=CARTESIAN_POINT('Ctrl Pts',(-0.154678679801214,-0.180079414286266,
-1.26242848356474));
#78315=CARTESIAN_POINT('Ctrl Pts',(-0.162210645187375,-0.17332582669859,
-1.26305741221355));
#78316=CARTESIAN_POINT('Ctrl Pts',(-0.182404828362225,-0.152745308568872,
-1.26483369041657));
#78317=CARTESIAN_POINT('Ctrl Pts',(-0.193889975237656,-0.137874131113492,
-1.26596458683913));
#78318=CARTESIAN_POINT('Ctrl Pts',(-0.205497308366332,-0.118481483010034,
-1.26741587165789));
#78319=CARTESIAN_POINT('Ctrl Pts',(-0.207406101536215,-0.115107392756048,
-1.26766732969837));
#78320=CARTESIAN_POINT('Ctrl Pts',(-0.210112323634053,-0.110037686700223,
-1.26804449435754));
#78321=CARTESIAN_POINT('Ctrl Pts',(-0.210973785933376,-0.10837685339845,
-1.26816794820959));
#78322=CARTESIAN_POINT('Ctrl Pts',(-0.212480665314051,-0.105385641370273,
-1.26839019750658));
#78323=CARTESIAN_POINT('Ctrl Pts',(-0.213133467195466,-0.10405907712203,
-1.26848872913115));
#78324=CARTESIAN_POINT('Ctrl Pts',(-0.214497006196713,-0.101221553519554,
-1.26869946330318));
#78325=CARTESIAN_POINT('Ctrl Pts',(-0.215204271930364,-0.0997090249692457,
-1.26881177926179));
#78326=CARTESIAN_POINT('Ctrl Pts',(-0.21708331623625,-0.095577437704139,
-1.26911860543523));
#78327=CARTESIAN_POINT('Ctrl Pts',(-0.218223601247948,-0.0929444532576411,
-1.26931417181783));
#78328=CARTESIAN_POINT('Ctrl Pts',(-0.225403679924603,-0.0755042268541385,
-1.27061029899731));
#78329=CARTESIAN_POINT('Ctrl Pts',(-0.229979335268381,-0.0601418153635036,
-1.27175967532887));
#78330=CARTESIAN_POINT('Ctrl Pts',(-0.234163398642582,-0.0382065364502483,
-1.27338802391003));
#78331=CARTESIAN_POINT('Ctrl Pts',(-0.235101642518382,-0.0319289118803864,
-1.27385205053657));
#78332=CARTESIAN_POINT('Ctrl Pts',(-0.236713328902362,-0.0170968632199078,
-1.27493628835472));
#78333=CARTESIAN_POINT('Ctrl Pts',(-0.237176733220839,-0.00852783387215598,
-1.27555340593406));
#78334=CARTESIAN_POINT('Ctrl Pts',(-0.237174995128926,4.80686365711195E-5,
-1.27615111301349));
#78335=CARTESIAN_POINT('Ctrl Pts',(-0.23717499508403,4.82896501978278E-5,
-1.27615112841727));
#78336=CARTESIAN_POINT('Ctrl Pts',(-0.237174613853761,0.00192070510180656,
-1.27628162842272));
#78337=CARTESIAN_POINT('Ctrl Pts',(-0.23715205948629,0.00379313235517636,
-1.27641117093985));
#78338=CARTESIAN_POINT('Ctrl Pts',(-0.237086814510887,0.00652386181438924,
-1.27659851217209));
#78339=CARTESIAN_POINT('Ctrl Pts',(-0.237061633173535,0.00738244688167251,
-1.27665718692539));
#78340=CARTESIAN_POINT('Ctrl Pts',(-0.237004606977172,0.00902268439812538,
-1.27676881879035));
#78341=CARTESIAN_POINT('Ctrl Pts',(-0.236973558060478,0.00980435659168084,
-1.27682181816431));
#78342=CARTESIAN_POINT('Ctrl Pts',(-0.236898555557878,0.0114831008895777,
-1.27693519244308));
#78343=CARTESIAN_POINT('Ctrl Pts',(-0.23685337313074,0.0123801024020447,
-1.27699549835875));
#78344=CARTESIAN_POINT('Ctrl Pts',(-0.236721772223277,0.0147273094283117,
-1.27715263780297));
#78345=CARTESIAN_POINT('Ctrl Pts',(-0.236627121583874,0.0161770417608945,
-1.27724902916325));
#78346=CARTESIAN_POINT('Ctrl Pts',(-0.236164586880043,0.022383736471244,
-1.27765921014127));
#78347=CARTESIAN_POINT('Ctrl Pts',(-0.2356665066264,0.0271302153687484,
-1.2779666075352));
#78348=CARTESIAN_POINT('Ctrl Pts',(-0.232710181682495,0.0489393220743692,
-1.27936324243328));
#78349=CARTESIAN_POINT('Ctrl Pts',(-0.228539638905983,0.065717688799441,
-1.28039621453562));
#78350=CARTESIAN_POINT('Ctrl Pts',(-0.220195779911241,0.0883954056428438,
-1.28189321490591));
#78351=CARTESIAN_POINT('Ctrl Pts',(-0.217521450463328,0.0947857440973023,
-1.28232659352862));
#78352=CARTESIAN_POINT('Ctrl Pts',(-0.212537664449414,0.105368452629825,
-1.28307255017715));
#78353=CARTESIAN_POINT('Ctrl Pts',(-0.210373963686022,0.10962463262242,
-1.28338064108519));
#78354=CARTESIAN_POINT('Ctrl Pts',(-0.207111324327873,0.11558972175671,
-1.28382577423364));
#78355=CARTESIAN_POINT('Ctrl Pts',(-0.206116510994967,0.117354454177868,
-1.28395917348986));
#78356=CARTESIAN_POINT('Ctrl Pts',(-0.204346486089286,0.120402413174954,
-1.28419268691012));
#78357=CARTESIAN_POINT('Ctrl Pts',(-0.203581476875947,0.121691452340644,
-1.28429243070438));
#78358=CARTESIAN_POINT('Ctrl Pts',(-0.202077128150336,0.124172387941331,
-1.2844863656046));
#78359=CARTESIAN_POINT('Ctrl Pts',(-0.201339331815747,0.125365150526535,
-1.28458049735977));
#78360=CARTESIAN_POINT('Ctrl Pts',(-0.19934155947504,0.128531733957456,
-1.28483284030694));
#78361=CARTESIAN_POINT('Ctrl Pts',(-0.198062884566006,0.130493513411497,
-1.28499173572442));
#78362=CARTESIAN_POINT('Ctrl Pts',(-0.193092080790156,0.137878459303881,
-1.28559991623431));
#78363=CARTESIAN_POINT('Ctrl Pts',(-0.189204848899054,0.143166099579953,
-1.28605640561929));
#78364=CARTESIAN_POINT('Ctrl Pts',(-0.17512245504322,0.160745064466465,
-1.28764880793862));
#78365=CARTESIAN_POINT('Ctrl Pts',(-0.163909452640218,0.17216396820272,
-1.28881982984788));
#78366=CARTESIAN_POINT('Ctrl Pts',(-0.14640858397937,0.186715653042787,
-1.29047664895832));
#78367=CARTESIAN_POINT('Ctrl Pts',(-0.140995762192899,0.190836094953807,
-1.29096859992884));
#78368=CARTESIAN_POINT('Ctrl Pts',(-0.133225045603013,0.196240083922836,
-1.29164029682386));
#78369=CARTESIAN_POINT('Ctrl Pts',(-0.131011441475805,0.197724775372766,
-1.2918279293152));
#78370=CARTESIAN_POINT('Ctrl Pts',(-0.127086746646118,0.200262259059966,
-1.29215355699167));
#78371=CARTESIAN_POINT('Ctrl Pts',(-0.12538645638855,0.2013311967805,-1.29229237270104));
#78372=CARTESIAN_POINT('Ctrl Pts',(-0.122805952756376,0.20290813302879,
-1.29249944676409));
#78373=CARTESIAN_POINT('Ctrl Pts',(-0.121935766244549,0.203432252820918,
-1.29256866778261));
#78374=CARTESIAN_POINT('Ctrl Pts',(-0.120348565082024,0.20437439237667,
-1.29269378803014));
#78375=CARTESIAN_POINT('Ctrl Pts',(-0.119632704711833,0.20479425135185,
-1.29274980005055));
#78376=CARTESIAN_POINT('Ctrl Pts',(-0.118002674916204,0.205738815585851,
-1.2928763991299));
#78377=CARTESIAN_POINT('Ctrl Pts',(-0.117087197006904,0.206261193462472,
-1.29294683925375));
#78378=CARTESIAN_POINT('Ctrl Pts',(-0.114246584818606,0.20785705854695,
-1.29316346424137));
#78379=CARTESIAN_POINT('Ctrl Pts',(-0.112309883359026,0.208909860661662,
-1.2933084205414));
#78380=CARTESIAN_POINT('Ctrl Pts',(-0.0974643434743828,0.216713848486018,
-1.29440108104783));
#78381=CARTESIAN_POINT('Ctrl Pts',(-0.0839711009534717,0.222290708842954,
-1.29529015439558));
#78382=CARTESIAN_POINT('Ctrl Pts',(-0.060820204530989,0.229447618452871,
-1.29677615038389));
#78383=CARTESIAN_POINT('Ctrl Pts',(-0.0514312966570702,0.231732338867738,
-1.29736850194418));
#78384=CARTESIAN_POINT('Ctrl Pts',(-0.0419357855265143,0.233438151374779,
-1.29797390460371));
#78385=CARTESIAN_POINT('Ctrl Pts',(-0.0419358330286197,0.233438142841301,
-1.31793598285019));
#78386=CARTESIAN_POINT('Ctrl Pts',(-0.0450441429985747,0.232879752655727,
-1.31773957474262));
#78387=CARTESIAN_POINT('Ctrl Pts',(-0.04814179629025,0.232259191105194,
-1.31754205121923));
#78388=CARTESIAN_POINT('Ctrl Pts',(-0.0577876136853906,0.230125446609451,
-1.31691982461284));
#78389=CARTESIAN_POINT('Ctrl Pts',(-0.0642831373476861,0.228396136166716,
-1.3164903219229));
#78390=CARTESIAN_POINT('Ctrl Pts',(-0.0728828678656407,0.225710692145085,
-1.31590261812276));
#78391=CARTESIAN_POINT('Ctrl Pts',(-0.0750595815023466,0.224996194635055,
-1.31575220065891));
#78392=CARTESIAN_POINT('Ctrl Pts',(-0.0786887843991768,0.223746398463105,
-1.31549844435571));
#78393=CARTESIAN_POINT('Ctrl Pts',(-0.0801470286781594,0.223228199869836,
-1.31539567109858));
#78394=CARTESIAN_POINT('Ctrl Pts',(-0.0830175950225842,0.222176368475757,
-1.31519170064363));
#78395=CARTESIAN_POINT('Ctrl Pts',(-0.0844301008704209,0.221643447179722,
-1.31509053112946));
#78396=CARTESIAN_POINT('Ctrl Pts',(-0.0875440662685072,0.220434500101537,
-1.31486566957707));
#78397=CARTESIAN_POINT('Ctrl Pts',(-0.0892429653781162,0.219752190382436,
-1.31474177220115));
#78398=CARTESIAN_POINT('Ctrl Pts',(-0.095123864715261,0.217310868621154,
-1.31430853688414));
#78399=CARTESIAN_POINT('Ctrl Pts',(-0.099262935789353,0.215451683609025,
-1.31399587239903));
#78400=CARTESIAN_POINT('Ctrl Pts',(-0.107841142029432,0.211298867914212,
-1.3133310339242));
#78401=CARTESIAN_POINT('Ctrl Pts',(-0.112266229694683,0.208981366202108,
-1.31297821762308));
#78402=CARTESIAN_POINT('Ctrl Pts',(-0.135252818582009,0.196002023127546,
-1.31109382928894));
#78403=CARTESIAN_POINT('Ctrl Pts',(-0.152378581360006,0.183004848574158,
-1.30949568664175));
#78404=CARTESIAN_POINT('Ctrl Pts',(-0.169827168311404,0.165593669404444,
-1.30775593115861));
#78405=CARTESIAN_POINT('Ctrl Pts',(-0.17207912029863,0.163252287469712,
-1.30752913127844));
#78406=CARTESIAN_POINT('Ctrl Pts',(-0.175114118411427,0.159964151903194,
-1.30722117380077));
#78407=CARTESIAN_POINT('Ctrl Pts',(-0.175938864106136,0.159056595656399,
-1.30713724564809));
#78408=CARTESIAN_POINT('Ctrl Pts',(-0.177323949862539,0.15750848087697,
-1.30699594322574));
#78409=CARTESIAN_POINT('Ctrl Pts',(-0.17788794223114,0.156871236513331,
-1.3069383058608));
#78410=CARTESIAN_POINT('Ctrl Pts',(-0.179052322504935,0.155541269988359,
-1.30681912308066));
#78411=CARTESIAN_POINT('Ctrl Pts',(-0.179652140987566,0.154848084179086,
-1.30675761760112));
#78412=CARTESIAN_POINT('Ctrl Pts',(-0.181247697066692,0.152982414132579,
-1.30659365795654));
#78413=CARTESIAN_POINT('Ctrl Pts',(-0.182236092275154,0.151803668288471,
-1.30649171863803));
#78414=CARTESIAN_POINT('Ctrl Pts',(-0.186798973782789,0.146253243879088,
-1.3060189085307));
#78415=CARTESIAN_POINT('Ctrl Pts',(-0.190228361183153,0.141764063963232,
-1.30565708234828));
#78416=CARTESIAN_POINT('Ctrl Pts',(-0.201045234314995,0.126504068229178,
-1.30447768072002));
#78417=CARTESIAN_POINT('Ctrl Pts',(-0.207703892625618,0.115245828996515,
-1.30368602951979));
#78418=CARTESIAN_POINT('Ctrl Pts',(-0.218233931378992,0.0935335708904622,
-1.30220210262495));
#78419=CARTESIAN_POINT('Ctrl Pts',(-0.222361564696137,0.0832458788099616,
-1.30151496832772));
#78420=CARTESIAN_POINT('Ctrl Pts',(-0.22700510615083,0.0688279064878478,
-1.30054389320636));
#78421=CARTESIAN_POINT('Ctrl Pts',(-0.228154499275156,0.0649162554910571,
-1.30027975831467));
#78422=CARTESIAN_POINT('Ctrl Pts',(-0.2296928062652,0.0591340236838122,
-1.29988730638604));
#78423=CARTESIAN_POINT('Ctrl Pts',(-0.230160879397401,0.0572851398640504,
-1.29976152481689));
#78424=CARTESIAN_POINT('Ctrl Pts',(-0.230952948371306,0.053989929567063,
-1.29953672963019));
#78425=CARTESIAN_POINT('Ctrl Pts',(-0.231285783794987,0.0525458171528234,
-1.29943800472394));
#78426=CARTESIAN_POINT('Ctrl Pts',(-0.231960053659516,0.0494896868279002,
-1.29922858992634));
#78427=CARTESIAN_POINT('Ctrl Pts',(-0.232298264732778,0.0478770462857149,
-1.29911780297253));
#78428=CARTESIAN_POINT('Ctrl Pts',(-0.233159353221392,0.0435471379775066,
-1.29881951843526));
#78429=CARTESIAN_POINT('Ctrl Pts',(-0.233651512436548,0.0408240962170101,
-1.298631062065));
#78430=CARTESIAN_POINT('Ctrl Pts',(-0.236157087266594,0.0254264570466844,
-1.29756011921402));
#78431=CARTESIAN_POINT('Ctrl Pts',(-0.237186487745343,0.0126154199031188,
-1.29664718680896));
#78432=CARTESIAN_POINT('Ctrl Pts',(-0.237163727982746,-0.0125906655638286,
-1.29481955572637));
#78433=CARTESIAN_POINT('Ctrl Pts',(-0.236183822465995,-0.0249471197383958,
-1.29390906147413));
#78434=CARTESIAN_POINT('Ctrl Pts',(-0.233208241266744,-0.0436988271985021,
-1.29254025055463));
#78435=CARTESIAN_POINT('Ctrl Pts',(-0.231899765624004,-0.0501815388615261,
-1.2920697584571));
#78436=CARTESIAN_POINT('Ctrl Pts',(-0.229938258470567,-0.0581632503069999,
-1.2915002685275));
#78437=CARTESIAN_POINT('Ctrl Pts',(-0.22953861792341,-0.0597209312621274,
-1.29138960360416));
#78438=CARTESIAN_POINT('Ctrl Pts',(-0.228882403554558,-0.062174708199118,
-1.29121615496909));
#78439=CARTESIAN_POINT('Ctrl Pts',(-0.228636346429202,-0.0630735298139263,
-1.29115280794653));
#78440=CARTESIAN_POINT('Ctrl Pts',(-0.22815722786432,-0.0647840496747016,
-1.29103264254622));
#78441=CARTESIAN_POINT('Ctrl Pts',(-0.227925122152485,-0.0655959787771291,
-1.2909757751496));
#78442=CARTESIAN_POINT('Ctrl Pts',(-0.227355984668928,-0.0675473817708406,
-1.29083948101293));
#78443=CARTESIAN_POINT('Ctrl Pts',(-0.227014711547396,-0.0686856130343581,
-1.29076029479745));
#78444=CARTESIAN_POINT('Ctrl Pts',(-0.225784335532602,-0.0726798554655385,
-1.29048336104323));
#78445=CARTESIAN_POINT('Ctrl Pts',(-0.224849733719117,-0.0755216976234497,
-1.29028803050334));
#78446=CARTESIAN_POINT('Ctrl Pts',(-0.22235377324437,-0.0826535862708674,
-1.28980035416054));
#78447=CARTESIAN_POINT('Ctrl Pts',(-0.220721824881644,-0.0869177590281617,
-1.28951110732223));
#78448=CARTESIAN_POINT('Ctrl Pts',(-0.211216182583872,-0.109757369678011,
-1.28796124740441));
#78449=CARTESIAN_POINT('Ctrl Pts',(-0.201120220918594,-0.127317224426492,
-1.28676008226972));
#78450=CARTESIAN_POINT('Ctrl Pts',(-0.185304495136652,-0.148155487006802,
-1.28510636895507));
#78451=CARTESIAN_POINT('Ctrl Pts',(-0.181507086894655,-0.152784071292551,
-1.28472277003582));
#78452=CARTESIAN_POINT('Ctrl Pts',(-0.176036867941301,-0.158959533811389,
-1.28418443151328));
#78453=CARTESIAN_POINT('Ctrl Pts',(-0.174510632909879,-0.160633591392015,
-1.28403565717631));
#78454=CARTESIAN_POINT('Ctrl Pts',(-0.172010745431868,-0.163297922573376,
-1.28379407810843));
#78455=CARTESIAN_POINT('Ctrl Pts',(-0.171051941766071,-0.164301981546365,
-1.28370190632642));
#78456=CARTESIAN_POINT('Ctrl Pts',(-0.169033394393446,-0.166378983989582,
-1.28350881842571));
#78457=CARTESIAN_POINT('Ctrl Pts',(-0.167972124823112,-0.167450350358176,
-1.2834078382839));
#78458=CARTESIAN_POINT('Ctrl Pts',(-0.165421373517851,-0.169976719491634,
-1.28316635265509));
#78459=CARTESIAN_POINT('Ctrl Pts',(-0.163922827664636,-0.171422349989504,
-1.28302544829807));
#78460=CARTESIAN_POINT('Ctrl Pts',(-0.15865988695442,-0.176367332347506,
-1.28253375689749));
#78461=CARTESIAN_POINT('Ctrl Pts',(-0.154801157888161,-0.179763706378,-1.28217871379119));
#78462=CARTESIAN_POINT('Ctrl Pts',(-0.144893338313225,-0.187928678431054,
-1.28127979746314));
#78463=CARTESIAN_POINT('Ctrl Pts',(-0.138716863633347,-0.192532802977061,
-1.28073039985551));
#78464=CARTESIAN_POINT('Ctrl Pts',(-0.124935431366625,-0.201798088856931,
-1.27953084557776));
#78465=CARTESIAN_POINT('Ctrl Pts',(-0.117269002870168,-0.206347526527299,
-1.27887925605728));
#78466=CARTESIAN_POINT('Ctrl Pts',(-0.0993585797783119,-0.215654877290188,
-1.27740724124203));
#78467=CARTESIAN_POINT('Ctrl Pts',(-0.0889926650755201,-0.220135221091236,
-1.27658961037133));
#78468=CARTESIAN_POINT('Ctrl Pts',(-0.0767226060801704,-0.22442945758325,
-1.27568711172987));
#78469=CARTESIAN_POINT('Ctrl Pts',(-0.0750927753327918,-0.224980032971189,
-1.27556853213438));
#78470=CARTESIAN_POINT('Ctrl Pts',(-0.0725383412970844,-0.225812097165995,
-1.27538485780239));
#78471=CARTESIAN_POINT('Ctrl Pts',(-0.0716178012997184,-0.226105738106755,
-1.27531910508714));
#78472=CARTESIAN_POINT('Ctrl Pts',(-0.0699784652905857,-0.226617649908129,
-1.27520281843302));
#78473=CARTESIAN_POINT('Ctrl Pts',(-0.0692604158059864,-0.226838135417788,
-1.27515216073012));
#78474=CARTESIAN_POINT('Ctrl Pts',(-0.0675160309834869,-0.227364713949789,
-1.27502975417674));
#78475=CARTESIAN_POINT('Ctrl Pts',(-0.0664886535288321,-0.227667271805715,
-1.2749582086996));
#78476=CARTESIAN_POINT('Ctrl Pts',(-0.0632527759030804,-0.228596449806423,
-1.27473447949377));
#78477=CARTESIAN_POINT('Ctrl Pts',(-0.0610371317592492,-0.229197993064283,
-1.27458364336766));
#78478=CARTESIAN_POINT('Ctrl Pts',(-0.0490308158085041,-0.232271221989006,
-1.27377719053391));
#78479=CARTESIAN_POINT('Ctrl Pts',(-0.039097545118008,-0.234148178577223,
-1.27314869165308));
#78480=CARTESIAN_POINT('Ctrl Pts',(-0.0105130346913182,-0.237678810716966,
-1.27137432567611));
#78481=CARTESIAN_POINT('Ctrl Pts',(0.00825210940212877,-0.237767937218976,
-1.27024491584511));
#78482=CARTESIAN_POINT('Ctrl Pts',(0.0307053456039303,-0.235211299498663,
-1.26879406032633));
#78483=CARTESIAN_POINT('Ctrl Pts',(0.0345664947360843,-0.234674941819115,
-1.26854123294892));
#78484=CARTESIAN_POINT('Ctrl Pts',(0.0402623746793533,-0.233740103541622,
-1.26816243328623));
#78485=CARTESIAN_POINT('Ctrl Pts',(0.0421085330731738,-0.233414579504707,
-1.26803874372369));
#78486=CARTESIAN_POINT('Ctrl Pts',(0.0454034487304112,-0.23279324154899,
-1.26781626218158));
#78487=CARTESIAN_POINT('Ctrl Pts',(0.0468536794602432,-0.232505696746309,
-1.26771773674122));
#78488=CARTESIAN_POINT('Ctrl Pts',(0.0499327580407142,-0.231865214733297,
-1.26750722331897));
#78489=CARTESIAN_POINT('Ctrl Pts',(0.0515607567142857,-0.231508631049575,
-1.26739512395608));
#78490=CARTESIAN_POINT('Ctrl Pts',(0.0559679587577904,-0.230494520891279,
-1.26708942877798));
#78491=CARTESIAN_POINT('Ctrl Pts',(0.0587391857584915,-0.229803923789111,
-1.26689478953184));
#78492=CARTESIAN_POINT('Ctrl Pts',(0.0648664927568811,-0.22815891249998,
-1.26645885599361));
#78493=CARTESIAN_POINT('Ctrl Pts',(0.0682152918508011,-0.227180155430401,
-1.26621683415158));
#78494=CARTESIAN_POINT('Ctrl Pts',(0.0788243320530306,-0.223823724309985,
-1.26543789013055));
#78495=CARTESIAN_POINT('Ctrl Pts',(0.0859913049501179,-0.221169192154312,
-1.26489300246711));
#78496=CARTESIAN_POINT('Ctrl Pts',(0.10074000545528,-0.214881165343914,
-1.26373518793276));
#78497=CARTESIAN_POINT('Ctrl Pts',(0.10828233387994,-0.211180943681267,
-1.26312162378104));
#78498=CARTESIAN_POINT('Ctrl Pts',(0.125204840653095,-0.201733546780958,
-1.26170747701845));
#78499=CARTESIAN_POINT('Ctrl Pts',(0.134414642907821,-0.195717720522456,
-1.26090902967387));
#78500=CARTESIAN_POINT('Ctrl Pts',(0.144830034500502,-0.187831179552273,
-1.25999558077016));
#78501=CARTESIAN_POINT('Ctrl Pts',(0.146468735455883,-0.186556160851772,
-1.25985155522803));
#78502=CARTESIAN_POINT('Ctrl Pts',(0.148905496880018,-0.184608293808231,
-1.25963717685695));
#78503=CARTESIAN_POINT('Ctrl Pts',(0.149716156998933,-0.183951465279907,
-1.25956582184369));
#78504=CARTESIAN_POINT('Ctrl Pts',(0.151175701040167,-0.182752845452011,
-1.25943732671426));
#78505=CARTESIAN_POINT('Ctrl Pts',(0.151826072585513,-0.182212894378135,
-1.25938006077436));
#78506=CARTESIAN_POINT('Ctrl Pts',(0.153169550020457,-0.181085325682063,
-1.25926177034901));
#78507=CARTESIAN_POINT('Ctrl Pts',(0.153862186401006,-0.180497185286605,
-1.25920078435919));
#78508=CARTESIAN_POINT('Ctrl Pts',(0.155690424684337,-0.17892659661308,
-1.25903975424156));
#78509=CARTESIAN_POINT('Ctrl Pts',(0.15682012772571,-0.177937301152442,
-1.25894019332116));
#78510=CARTESIAN_POINT('Ctrl Pts',(0.162315523802163,-0.173031919605993,
-1.25845515414894));
#78511=CARTESIAN_POINT('Ctrl Pts',(0.166544705055028,-0.168965228024774,
-1.25807957309652));
#78512=CARTESIAN_POINT('Ctrl Pts',(0.180245619459974,-0.154775844527607,
-1.25683694899645));
#78513=CARTESIAN_POINT('Ctrl Pts',(0.18898030055248,-0.143981032986993,
-1.25599881848316));
#78514=CARTESIAN_POINT('Ctrl Pts',(0.203600700860742,-0.1222716175674,-1.25438640198874));
#78515=CARTESIAN_POINT('Ctrl Pts',(0.20967216701723,-0.11153976975976,-1.25361792586346));
#78516=CARTESIAN_POINT('Ctrl Pts',(0.216050106899534,-0.0978873724638894,
-1.25264022120727));
#78517=CARTESIAN_POINT('Ctrl Pts',(0.217173676647155,-0.0953686506188229,
-1.25245990714688));
#78518=CARTESIAN_POINT('Ctrl Pts',(0.218897190885251,-0.0913165317726143,
-1.25216961265539));
#78519=CARTESIAN_POINT('Ctrl Pts',(0.219525551547244,-0.0897954405329999,
-1.252060596824));
#78520=CARTESIAN_POINT('Ctrl Pts',(0.220689712085365,-0.0868920542996715,
-1.25185236603007));
#78521=CARTESIAN_POINT('Ctrl Pts',(0.221228483257865,-0.0855110293747747,
-1.25175325671305));
#78522=CARTESIAN_POINT('Ctrl Pts',(0.222432020934401,-0.08233849582987,
-1.25152539224879));
#78523=CARTESIAN_POINT('Ctrl Pts',(0.223088146145137,-0.080543842167447,
-1.2513963568648));
#78524=CARTESIAN_POINT('Ctrl Pts',(0.225082609794726,-0.0748771176937524,
-1.25098839037956));
#78525=CARTESIAN_POINT('Ctrl Pts',(0.226342289373083,-0.0709783658551482,
-1.25070692020863));
#78526=CARTESIAN_POINT('Ctrl Pts',(0.230791318739979,-0.0558826402858122,
-1.2496134749995));
#78527=CARTESIAN_POINT('Ctrl Pts',(0.233255297860058,-0.0444904764475818,
-1.24877970102691));
#78528=CARTESIAN_POINT('Ctrl Pts',(0.236820128736334,-0.0190912640524416,
-1.24691593649711));
#78529=CARTESIAN_POINT('Ctrl Pts',(0.237534297317153,-0.00507220455330229,
-1.24588367890338));
#78530=CARTESIAN_POINT('Ctrl Pts',(0.236843006920982,0.0132787376186449,
-1.24457583536122));
#78531=CARTESIAN_POINT('Ctrl Pts',(0.236559347471268,0.0176242897715005,
-1.24426951620173));
#78532=CARTESIAN_POINT('Ctrl Pts',(0.236025883066952,0.0233611583744994,
-1.24387162037408));
#78533=CARTESIAN_POINT('Ctrl Pts',(0.235883105807222,0.0247612971223859,
-1.24377502529658));
#78534=CARTESIAN_POINT('Ctrl Pts',(0.235629920835171,0.0270427371355732,
-1.24361855944217));
#78535=CARTESIAN_POINT('Ctrl Pts',(0.235527013724967,0.027924811477552,
-1.24355829219037));
#78536=CARTESIAN_POINT('Ctrl Pts',(0.235313569349336,0.0296691828447669,
-1.24343958639284));
#78537=CARTESIAN_POINT('Ctrl Pts',(0.235203241316504,0.0305314862230657,
-1.24338113855616));
#78538=CARTESIAN_POINT('Ctrl Pts',(0.234913447447265,0.0327016109983514,
-1.2432345874128));
#78539=CARTESIAN_POINT('Ctrl Pts',(0.234727796429805,0.0340086009129097,
-1.24314682143507));
#78540=CARTESIAN_POINT('Ctrl Pts',(0.233940673480156,0.0392361273351585,
-1.24279753089698));
#78541=CARTESIAN_POINT('Ctrl Pts',(0.233251775092791,0.0431430896531191,
-1.24254041167414));
#78542=CARTESIAN_POINT('Ctrl Pts',(0.231095065483561,0.0538032444869224,
-1.24184514534651));
#78543=CARTESIAN_POINT('Ctrl Pts',(0.229429613166123,0.0605126784784325,
-1.24141448516452));
#78544=CARTESIAN_POINT('Ctrl Pts',(0.22284436955349,0.0828237140128339,
-1.23997794857061));
#78545=CARTESIAN_POINT('Ctrl Pts',(0.216606019691338,0.0979857082961548,
-1.23899106481429));
#78546=CARTESIAN_POINT('Ctrl Pts',(0.205951842108191,0.117785504292723,
-1.23757102034217));
#78547=CARTESIAN_POINT('Ctrl Pts',(0.202837902719818,0.123070555631066,
-1.23717827743808));
#78548=CARTESIAN_POINT('Ctrl Pts',(0.198286980784147,0.130151755539494,
-1.23662914227295));
#78549=CARTESIAN_POINT('Ctrl Pts',(0.197023377613028,0.132056784357728,
-1.23647904374724));
#78550=CARTESIAN_POINT('Ctrl Pts',(0.194946324922046,0.135092001240454,
-1.23623589007464));
#78551=CARTESIAN_POINT('Ctrl Pts',(0.194150094447349,0.136233839724119,
-1.23614348420485));
#78552=CARTESIAN_POINT('Ctrl Pts',(0.1924720882906,0.138595603983667,-1.23595036146244));
#78553=CARTESIAN_POINT('Ctrl Pts',(0.19158866078083,0.139814273573524,-1.23584958428538));
#78554=CARTESIAN_POINT('Ctrl Pts',(0.189465453198506,0.142685282077827,
-1.23560943094656));
#78555=CARTESIAN_POINT('Ctrl Pts',(0.18821558527278,0.144329971485164,-1.23546966757829));
#78556=CARTESIAN_POINT('Ctrl Pts',(0.183848325930768,0.149923596657927,
-1.23498660062116));
#78557=CARTESIAN_POINT('Ctrl Pts',(0.180627052215816,0.153789314269525,
-1.23463923941294));
#78558=CARTESIAN_POINT('Ctrl Pts',(0.172326718473209,0.163129422210018,
-1.23376502065946));
#78559=CARTESIAN_POINT('Ctrl Pts',(0.167107689350186,0.168471685231689,
-1.23323303037805));
#78560=CARTESIAN_POINT('Ctrl Pts',(0.155082334784136,0.179671643960712,
-1.23204733898518));
#78561=CARTESIAN_POINT('Ctrl Pts',(0.148177503900019,0.185407244343262,
-1.23139154838752));
#78562=CARTESIAN_POINT('Ctrl Pts',(0.13164387099311,0.197626426020707,-1.22989178108285));
#78563=CARTESIAN_POINT('Ctrl Pts',(0.1218294744188,0.203823334251217,-1.22905050540981));
#78564=CARTESIAN_POINT('Ctrl Pts',(0.110077478450933,0.210090237085562,
-1.22812580363861));
#78565=CARTESIAN_POINT('Ctrl Pts',(0.108545802984555,0.210885675348611,
-1.2280068309674));
#78566=CARTESIAN_POINT('Ctrl Pts',(0.106142131123382,0.212100835915446,
-1.22782268155167));
#78567=CARTESIAN_POINT('Ctrl Pts',(0.105276053468683,0.212532042866423,
-1.22775684157335));
#78568=CARTESIAN_POINT('Ctrl Pts',(0.103733073253316,0.213288523032304,
-1.2276404808205));
#78569=CARTESIAN_POINT('Ctrl Pts',(0.103057253835324,0.213615886579926,
-1.22758983533707));
#78570=CARTESIAN_POINT('Ctrl Pts',(0.101415461003773,0.214401557718059,
-1.22746756117304));
#78571=CARTESIAN_POINT('Ctrl Pts',(0.10044792823023,0.214856550997556,-1.22739613463144));
#78572=CARTESIAN_POINT('Ctrl Pts',(0.0974023185357063,0.216263713491801,
-1.22717316978657));
#78573=CARTESIAN_POINT('Ctrl Pts',(0.0953134632994689,0.217192426401864,
-1.22702296604742));
#78574=CARTESIAN_POINT('Ctrl Pts',(0.0840155051846943,0.222021142179964,
-1.22622336193045));
#78575=CARTESIAN_POINT('Ctrl Pts',(0.0745791271001816,0.225366349657924,
-1.22560057551634));
#78576=CARTESIAN_POINT('Ctrl Pts',(0.0472643139616395,0.233144910556682,
-1.22385045008607));
#78577=CARTESIAN_POINT('Ctrl Pts',(0.0290451990073976,0.236107592732624,
-1.22273960580836));
#78578=CARTESIAN_POINT('Ctrl Pts',(0.00649936194552893,0.237122635682033,
-1.22129384957588));
#78579=CARTESIAN_POINT('Ctrl Pts',(0.00232759538006935,0.23720026344767,
-1.22102368410162));
#78580=CARTESIAN_POINT('Ctrl Pts',(-0.003747372722769,0.237153033754965,
-1.22062532152382));
#78581=CARTESIAN_POINT('Ctrl Pts',(-0.00565059503424683,0.237115319300166,
-1.2204998148991));
#78582=CARTESIAN_POINT('Ctrl Pts',(-0.00903786662288286,0.237007392976922,
-1.22027509270159));
#78583=CARTESIAN_POINT('Ctrl Pts',(-0.0105221142464977,0.236946137970936,
-1.22017616094276));
#78584=CARTESIAN_POINT('Ctrl Pts',(-0.0136363831216303,0.236788293141701,
-1.21996756505058));
#78585=CARTESIAN_POINT('Ctrl Pts',(-0.0152661726847158,0.23668880508901,
-1.21985781552019));
#78586=CARTESIAN_POINT('Ctrl Pts',(-0.0195850273237711,0.236380375080471,
-1.21956537070213));
#78587=CARTESIAN_POINT('Ctrl Pts',(-0.0222717101378768,0.236142382693003,
-1.2193817812597));
#78588=CARTESIAN_POINT('Ctrl Pts',(-0.0306441885390416,0.235256581103655,
-1.21880423717975));
#78589=CARTESIAN_POINT('Ctrl Pts',(-0.0363085877279333,0.234449045685933,
-1.21840560443526));
#78590=CARTESIAN_POINT('Ctrl Pts',(-0.0419358439263085,0.233438140883593,
-1.21800162451869));
#78591=CARTESIAN_POINT('Origin',(0.,0.,-1.7456589891905));
#78592=CARTESIAN_POINT('',(-0.0419358102824307,0.233438146927523,-1.09805944304797));
#78593=CARTESIAN_POINT('',(-0.0419358257386354,0.233438144150905,-1.11763442355469));
#78594=CARTESIAN_POINT('',(-0.0419358257166344,0.233438144154858,-1.7456589891905));
#78595=CARTESIAN_POINT('Ctrl Pts',(-0.0419358102824291,0.233438146927524,
-1.09805944304797));
#78596=CARTESIAN_POINT('Ctrl Pts',(-0.0379568861939225,0.234152937581493,
-1.09835331162497));
#78597=CARTESIAN_POINT('Ctrl Pts',(-0.0339584290944791,0.23476622439805,
-1.09864841709242));
#78598=CARTESIAN_POINT('Ctrl Pts',(-0.0166710106798612,0.236966435425049,
-1.09992053886217));
#78599=CARTESIAN_POINT('Ctrl Pts',(-0.00327721598154022,0.237529675797298,
-1.10089800105867));
#78600=CARTESIAN_POINT('Ctrl Pts',(0.0119081045847333,0.236882831003429,
-1.10195430417511));
#78601=CARTESIAN_POINT('Ctrl Pts',(0.013721608450018,0.236784705040578,
-1.1020795840633));
#78602=CARTESIAN_POINT('Ctrl Pts',(0.0165082372712046,0.236601800926374,
-1.1022705740362));
#78603=CARTESIAN_POINT('Ctrl Pts',(0.0174822186028563,0.236531829185448,
-1.10233704370119));
#78604=CARTESIAN_POINT('Ctrl Pts',(0.0192867741586138,0.236390980700097,
-1.10245963342723));
#78605=CARTESIAN_POINT('Ctrl Pts',(0.0201174167927684,0.236321740400687,
-1.1025158365596));
#78606=CARTESIAN_POINT('Ctrl Pts',(0.0220304384324753,0.236152116036669,
-1.10264477469416));
#78607=CARTESIAN_POINT('Ctrl Pts',(0.0231125128605143,0.236048668689644,
-1.10271734038701));
#78608=CARTESIAN_POINT('Ctrl Pts',(0.026628246868269,0.235688153348297,
-1.10295203116607));
#78609=CARTESIAN_POINT('Ctrl Pts',(0.0290587371354134,0.235400849825394,
-1.10311259246941));
#78610=CARTESIAN_POINT('Ctrl Pts',(0.0494228640885475,0.232673418617775,
-1.10444699357168));
#78611=CARTESIAN_POINT('Ctrl Pts',(0.0670297559238366,0.228225179715533,
-1.10553318500805));
#78612=CARTESIAN_POINT('Ctrl Pts',(0.0917299520849377,0.218875764162056,
-1.10715993523477));
#78613=CARTESIAN_POINT('Ctrl Pts',(0.0993385556377833,0.215529163551474,
-1.1076758790892));
#78614=CARTESIAN_POINT('Ctrl Pts',(0.110040452574452,0.210134747229016,
-1.10843678363915));
#78615=CARTESIAN_POINT('Ctrl Pts',(0.113286288201231,0.208402802183751,
-1.10867242878256));
#78616=CARTESIAN_POINT('Ctrl Pts',(0.119082883116074,0.2051343591205,-1.10910322992232));
#78617=CARTESIAN_POINT('Ctrl Pts',(0.121647512319049,0.203623966678832,
-1.10929748570112));
#78618=CARTESIAN_POINT('Ctrl Pts',(0.125624725325469,0.201179702841588,
-1.10960491230329));
#78619=CARTESIAN_POINT('Ctrl Pts',(0.127056941588665,0.200278250924797,
-1.10971690494336));
#78620=CARTESIAN_POINT('Ctrl Pts',(0.129719692893389,0.198562230229268,
-1.10992761174361));
#78621=CARTESIAN_POINT('Ctrl Pts',(0.130952516365157,0.197751349645869,
-1.1100261856922));
#78622=CARTESIAN_POINT('Ctrl Pts',(0.133703042986597,0.195905211509962,
-1.11024845839622));
#78623=CARTESIAN_POINT('Ctrl Pts',(0.135216430907903,0.194863726957308,
-1.11037238729124));
#78624=CARTESIAN_POINT('Ctrl Pts',(0.13973810751901,0.19167395823162,-1.11074770132054));
#78625=CARTESIAN_POINT('Ctrl Pts',(0.142708298660339,0.189472910435648,
-1.11100107836532));
#78626=CARTESIAN_POINT('Ctrl Pts',(0.160571045103683,0.17557746715302,-1.11256830325633));
#78627=CARTESIAN_POINT('Ctrl Pts',(0.174068028101914,0.162205353187178,
-1.1139499374506));
#78628=CARTESIAN_POINT('Ctrl Pts',(0.192148652817416,0.13940694373149,-1.11607154335916));
#78629=CARTESIAN_POINT('Ctrl Pts',(0.197949400544702,0.131039976854892,
-1.11680872452397));
#78630=CARTESIAN_POINT('Ctrl Pts',(0.204383349933768,0.120352529290333,
-1.11768097305564));
#78631=CARTESIAN_POINT('Ctrl Pts',(0.205542467371631,0.118362072151934,
-1.11784061497889));
#78632=CARTESIAN_POINT('Ctrl Pts',(0.207198630536244,0.1154203555069,-1.11807212780044));
#78633=CARTESIAN_POINT('Ctrl Pts',(0.207718470588126,0.114482173501986,
-1.11814531351209));
#78634=CARTESIAN_POINT('Ctrl Pts',(0.208591700254312,0.112880680214559,
-1.11826910167038));
#78635=CARTESIAN_POINT('Ctrl Pts',(0.208948324474874,0.112219174556597,
-1.11831990327893));
#78636=CARTESIAN_POINT('Ctrl Pts',(0.209756020322366,0.110703771771564,
-1.11843552361632));
#78637=CARTESIAN_POINT('Ctrl Pts',(0.21020502784578,0.109848802891782,-1.11850021353258));
#78638=CARTESIAN_POINT('Ctrl Pts',(0.21143786020895,0.107466088345999,-1.11867906563629));
#78639=CARTESIAN_POINT('Ctrl Pts',(0.212210353842035,0.105932502167883,
-1.11879255542525));
#78640=CARTESIAN_POINT('Ctrl Pts',(0.217691925524666,0.0947496069830524,
-1.11960938515718));
#78641=CARTESIAN_POINT('Ctrl Pts',(0.221758207810503,0.0847975186055965,
-1.12027903004796));
#78642=CARTESIAN_POINT('Ctrl Pts',(0.225699193913305,0.0729044320733339,
-1.12105138176533));
#78643=CARTESIAN_POINT('Ctrl Pts',(0.226242790643945,0.071199593504161,
-1.1211614387327));
#78644=CARTESIAN_POINT('Ctrl Pts',(0.229057632932387,0.0620137408996998,
-1.12175163552292));
#78645=CARTESIAN_POINT('Ctrl Pts',(0.230977205426684,0.0544300674448357,
-1.12222913516895));
#78646=CARTESIAN_POINT('Ctrl Pts',(0.234018036185483,0.0393110316288712,
-1.12318153568289));
#78647=CARTESIAN_POINT('Ctrl Pts',(0.235157886907406,0.0317892094317245,
-1.12365559003462));
#78648=CARTESIAN_POINT('Ctrl Pts',(0.236289806934538,0.0207655661354777,
-1.12436066678052));
#78649=CARTESIAN_POINT('Ctrl Pts',(0.236568941063478,0.0172978577153588,
-1.12458390541195));
#78650=CARTESIAN_POINT('Ctrl Pts',(0.236937814318573,0.0109805865294207,
-1.12499409383492));
#78651=CARTESIAN_POINT('Ctrl Pts',(0.237052636155568,0.00813312326850457,
-1.12518027265812));
#78652=CARTESIAN_POINT('Ctrl Pts',(0.237153233259539,0.00361921584620531,
-1.12547778705443));
#78653=CARTESIAN_POINT('Ctrl Pts',(0.237172800738508,0.00195374530733741,
-1.12558807051801));
#78654=CARTESIAN_POINT('Ctrl Pts',(0.237176622468758,-0.00119089941568732,
-1.12579733092218));
#78655=CARTESIAN_POINT('Ctrl Pts',(0.2371645830232,-0.00266999556853016,
-1.12589618738561));
#78656=CARTESIAN_POINT('Ctrl Pts',(0.237105864454018,-0.0060262104382984,
-1.1261215234105));
#78657=CARTESIAN_POINT('Ctrl Pts',(0.237050727542241,-0.00790306210016809,
-1.12624826051714));
#78658=CARTESIAN_POINT('Ctrl Pts',(0.236848789925979,-0.0127965839830782,
-1.12658067828505));
#78659=CARTESIAN_POINT('Ctrl Pts',(0.236666645128691,-0.0158113718454506,
-1.12678743737864));
#78660=CARTESIAN_POINT('Ctrl Pts',(0.235030222425289,-0.0363670922790522,
-1.12821113877261));
#78661=CARTESIAN_POINT('Ctrl Pts',(0.231684966740276,-0.0536994512001545,
-1.12948720458719));
#78662=CARTESIAN_POINT('Ctrl Pts',(0.222744317114931,-0.0824184046399465,
-1.1316828527758));
#78663=CARTESIAN_POINT('Ctrl Pts',(0.218097936040237,-0.0940275297809924,
-1.13259319541156));
#78664=CARTESIAN_POINT('Ctrl Pts',(0.211658486553904,-0.107036364051021,
-1.13360481667437));
#78665=CARTESIAN_POINT('Ctrl Pts',(0.210734947422177,-0.108843377291534,
-1.13374510960598));
#78666=CARTESIAN_POINT('Ctrl Pts',(0.209312487455712,-0.111540591630558,
-1.13395392951042));
#78667=CARTESIAN_POINT('Ctrl Pts',(0.208830856307402,-0.112439737357566,
-1.13402344254483));
#78668=CARTESIAN_POINT('Ctrl Pts',(0.207946918314087,-0.114064667193416,
-1.13414884728472));
#78669=CARTESIAN_POINT('Ctrl Pts',(0.207546592278577,-0.114791468412994,
-1.13420485487078));
#78670=CARTESIAN_POINT('Ctrl Pts',(0.206631364403101,-0.116432645581979,
-1.13433114221386));
#78671=CARTESIAN_POINT('Ctrl Pts',(0.206114200753142,-0.117345720264258,
-1.13440127837755));
#78672=CARTESIAN_POINT('Ctrl Pts',(0.204504203039306,-0.120144756415573,
-1.134615992799));
#78673=CARTESIAN_POINT('Ctrl Pts',(0.203391382666009,-0.122019169957057,
-1.13475937347675));
#78674=CARTESIAN_POINT('Ctrl Pts',(0.194500326445898,-0.136535391462297,
-1.13586874097261));
#78675=CARTESIAN_POINT('Ctrl Pts',(0.185575657542781,-0.148438828680248,
-1.13677362065547));
#78676=CARTESIAN_POINT('Ctrl Pts',(0.16497822847736,-0.171124613563893,
-1.13865276890389));
#78677=CARTESIAN_POINT('Ctrl Pts',(0.153220901253196,-0.181727050625171,
-1.13962444560233));
#78678=CARTESIAN_POINT('Ctrl Pts',(0.138165686929101,-0.192796795172578,
-1.1408351812615));
#78679=CARTESIAN_POINT('Ctrl Pts',(0.135802244660728,-0.194468790384343,
-1.14102425148977));
#78680=CARTESIAN_POINT('Ctrl Pts',(0.13202384234333,-0.197039315489351,
-1.14132531500762));
#78681=CARTESIAN_POINT('Ctrl Pts',(0.130628899190503,-0.197966858968787,
-1.14143621176386));
#78682=CARTESIAN_POINT('Ctrl Pts',(0.127985191374101,-0.199684638743322,
-1.14164597813001));
#78683=CARTESIAN_POINT('Ctrl Pts',(0.12673863326206,-0.200478135541841,
-1.14174472010043));
#78684=CARTESIAN_POINT('Ctrl Pts',(0.123904425166016,-0.202245253126783,
-1.14196889275028));
#78685=CARTESIAN_POINT('Ctrl Pts',(0.122312574370884,-0.203211915978114,
-1.14209457063592));
#78686=CARTESIAN_POINT('Ctrl Pts',(0.118155070821138,-0.205670042304123,
-1.14242229765477));
#78687=CARTESIAN_POINT('Ctrl Pts',(0.115572582593216,-0.207132237553247,
-1.14262537576459));
#78688=CARTESIAN_POINT('Ctrl Pts',(0.0969645123772812,-0.217211722339492,
-1.14408571004271));
#78689=CARTESIAN_POINT('Ctrl Pts',(0.0800242044932442,-0.224006558375495,
-1.14540677223974));
#78690=CARTESIAN_POINT('Ctrl Pts',(0.0506573710478196,-0.232025762864838,
-1.14762867352109));
#78691=CARTESIAN_POINT('Ctrl Pts',(0.0386032106173287,-0.234333051683242,
-1.14852075039402));
#78692=CARTESIAN_POINT('Ctrl Pts',(0.0245681651621397,-0.235906489815959,
-1.14950294916515));
#78693=CARTESIAN_POINT('Ctrl Pts',(0.0227102269446111,-0.236092593722149,
-1.14963182293467));
#78694=CARTESIAN_POINT('Ctrl Pts',(0.0198669459657504,-0.236343519964401,
-1.14982709846271));
#78695=CARTESIAN_POINT('Ctrl Pts',(0.0188831233099919,-0.236424158481266,
-1.14989431173221));
#78696=CARTESIAN_POINT('Ctrl Pts',(0.0170690739544669,-0.236561450228668,
-1.15001755530464));
#78697=CARTESIAN_POINT('Ctrl Pts',(0.016239039773748,-0.236619877951739,
-1.15007367683561));
#78698=CARTESIAN_POINT('Ctrl Pts',(0.0143389670226909,-0.236743582327482,
-1.15020154602753));
#78699=CARTESIAN_POINT('Ctrl Pts',(0.0132687743564023,-0.236805974345982,
-1.15027313475458));
#78700=CARTESIAN_POINT('Ctrl Pts',(0.009838664754885,-0.2369826224232,-1.15050130823869));
#78701=CARTESIAN_POINT('Ctrl Pts',(0.00747736579035017,-0.23706887752416,
-1.15065644722717));
#78702=CARTESIAN_POINT('Ctrl Pts',(-0.0106753686953257,-0.237460461826431,
-1.15183693279482));
#78703=CARTESIAN_POINT('Ctrl Pts',(-0.0264625184678278,-0.236222996466737,
-1.1527947487485));
#78704=CARTESIAN_POINT('Ctrl Pts',(-0.0565479942935877,-0.230808302056091,
-1.15467080818325));
#78705=CARTESIAN_POINT('Ctrl Pts',(-0.0708068286774048,-0.226840169367799,
-1.15558399992836));
#78706=CARTESIAN_POINT('Ctrl Pts',(-0.087203329217904,-0.220579479207914,
-1.15672246529454));
#78707=CARTESIAN_POINT('Ctrl Pts',(-0.0897857384746955,-0.219540992489487,
-1.1569044043934));
#78708=CARTESIAN_POINT('Ctrl Pts',(-0.0938703353750423,-0.217814297385418,
-1.15719671405723));
#78709=CARTESIAN_POINT('Ctrl Pts',(-0.0953846900475314,-0.217155402146338,
-1.15730609623577));
#78710=CARTESIAN_POINT('Ctrl Pts',(-0.0982444529388262,-0.215875435413101,
-1.15751464320215));
#78711=CARTESIAN_POINT('Ctrl Pts',(-0.0995911679125088,-0.215257462706168,
-1.15761369823569));
#78712=CARTESIAN_POINT('Ctrl Pts',(-0.102653013448634,-0.213817577523939,
-1.15784089273573));
#78713=CARTESIAN_POINT('Ctrl Pts',(-0.104364206441023,-0.212987581038248,
-1.15796930613361));
#78714=CARTESIAN_POINT('Ctrl Pts',(-0.108841534430782,-0.210748988116981,
-1.15830919648846));
#78715=CARTESIAN_POINT('Ctrl Pts',(-0.111590240162673,-0.209306551096509,
-1.15852183289576));
#78716=CARTESIAN_POINT('Ctrl Pts',(-0.128245359726734,-0.200145122610809,
-1.15983532261843));
#78717=CARTESIAN_POINT('Ctrl Pts',(-0.141372263207861,-0.191098567686547,
-1.16098325038798));
#78718=CARTESIAN_POINT('Ctrl Pts',(-0.16416545409768,-0.171748834749719,
-1.16316502698073));
#78719=CARTESIAN_POINT('Ctrl Pts',(-0.174015518247122,-0.161761023090044,
-1.16419080476079));
#78720=CARTESIAN_POINT('Ctrl Pts',(-0.184229120115131,-0.149384714942885,
-1.16530935446074));
#78721=CARTESIAN_POINT('Ctrl Pts',(-0.18551022869534,-0.147790789655864,
-1.16545074836913));
#78722=CARTESIAN_POINT('Ctrl Pts',(-0.18740117947556,-0.14537477514018,
-1.16566086820921));
#78723=CARTESIAN_POINT('Ctrl Pts',(-0.188026539320907,-0.144565030089082,
-1.16573059779801));
#78724=CARTESIAN_POINT('Ctrl Pts',(-0.189149524688123,-0.143091321584795,
-1.16585621514323));
#78725=CARTESIAN_POINT('Ctrl Pts',(-0.189648921470875,-0.142428773909899,
-1.16591222106481));
#78726=CARTESIAN_POINT('Ctrl Pts',(-0.190770039981206,-0.140925038532919,
-1.16603828443429));
#78727=CARTESIAN_POINT('Ctrl Pts',(-0.191389684195424,-0.140082345521155,
-1.16610820071153));
#78728=CARTESIAN_POINT('Ctrl Pts',(-0.193272994339512,-0.137485289113059,
-1.16632153956532));
#78729=CARTESIAN_POINT('Ctrl Pts',(-0.194518303713542,-0.135717667936478,
-1.16646378662279));
#78730=CARTESIAN_POINT('Ctrl Pts',(-0.2043231189953,-0.121388225878524,
-1.16759558719514));
#78731=CARTESIAN_POINT('Ctrl Pts',(-0.211682254887129,-0.108045310553759,
-1.16852086338635));
#78732=CARTESIAN_POINT('Ctrl Pts',(-0.219536415776316,-0.0898712726390406,
-1.16973519403368));
#78733=CARTESIAN_POINT('Ctrl Pts',(-0.221235864916009,-0.0856024209953103,
-1.17001719864522));
#78734=CARTESIAN_POINT('Ctrl Pts',(-0.22538682782221,-0.0742244959781561,
-1.17076543685948));
#78735=CARTESIAN_POINT('Ctrl Pts',(-0.227625990001952,-0.0670439712040082,
-1.17123435290941));
#78736=CARTESIAN_POINT('Ctrl Pts',(-0.230794433838549,-0.0548768814839222,
-1.17203453332438));
#78737=CARTESIAN_POINT('Ctrl Pts',(-0.231911701121949,-0.049944968578224,
-1.17236034231648));
#78738=CARTESIAN_POINT('Ctrl Pts',(-0.233263025845686,-0.042949105542025,
-1.17282652693108));
#78739=CARTESIAN_POINT('Ctrl Pts',(-0.233628951144174,-0.040911827545721,
-1.17296275568478));
#78740=CARTESIAN_POINT('Ctrl Pts',(-0.234215009495198,-0.0373842038365646,
-1.17319957684469));
#78741=CARTESIAN_POINT('Ctrl Pts',(-0.234447697850059,-0.035896046635954,
-1.17329976777564));
#78742=CARTESIAN_POINT('Ctrl Pts',(-0.234895422259891,-0.032842323901222,
-1.17350599373551));
#78743=CARTESIAN_POINT('Ctrl Pts',(-0.235109017354494,-0.0312766268589381,
-1.17361206872707));
#78744=CARTESIAN_POINT('Ctrl Pts',(-0.235613546912353,-0.0272805471644105,
-1.17388372019997));
#78745=CARTESIAN_POINT('Ctrl Pts',(-0.235882526191231,-0.0248476316797227,
-1.17404997451111));
#78746=CARTESIAN_POINT('Ctrl Pts',(-0.236826541015641,-0.0149018788751919,
-1.1747333856812));
#78747=CARTESIAN_POINT('Ctrl Pts',(-0.237180585799741,-0.00736375334486454,
-1.17526029872133));
#78748=CARTESIAN_POINT('Ctrl Pts',(-0.237164963147181,0.0134802090323218,
-1.17674180571664));
#78749=CARTESIAN_POINT('Ctrl Pts',(-0.23603586025259,0.0267572040969771,
-1.17771438393518));
#78750=CARTESIAN_POINT('Ctrl Pts',(-0.231890173455107,0.05106891107705,
-1.17951314255089));
#78751=CARTESIAN_POINT('Ctrl Pts',(-0.229177530975958,0.0621192629928734,
-1.18033721590058));
#78752=CARTESIAN_POINT('Ctrl Pts',(-0.225153259850731,0.0745718067036157,
-1.18124576340917));
#78753=CARTESIAN_POINT('Ctrl Pts',(-0.22460598772417,0.0762043009547344,
-1.1813644463234));
#78754=CARTESIAN_POINT('Ctrl Pts',(-0.223723736382412,0.0787439198990912,
-1.1815482569367));
#78755=CARTESIAN_POINT('Ctrl Pts',(-0.223400918027898,0.0796551633578571,
-1.18161404389417));
#78756=CARTESIAN_POINT('Ctrl Pts',(-0.222817310851792,0.0812710965069608,
-1.18173037775845));
#78757=CARTESIAN_POINT('Ctrl Pts',(-0.222558741407624,0.0819765319401293,
-1.18178104865724));
#78758=CARTESIAN_POINT('Ctrl Pts',(-0.221923449729732,0.0836845873412313,
-1.18190347199583));
#78759=CARTESIAN_POINT('Ctrl Pts',(-0.221543282633284,0.084685900413273,
-1.18197502112334));
#78760=CARTESIAN_POINT('Ctrl Pts',(-0.220327251874794,0.0878245369980222,
-1.18219870654821));
#78761=CARTESIAN_POINT('Ctrl Pts',(-0.21946711455013,0.0899523974241675,
-1.18234949633113));
#78762=CARTESIAN_POINT('Ctrl Pts',(-0.214660259358054,0.101364282332333,
-1.18315527501331));
#78763=CARTESIAN_POINT('Ctrl Pts',(-0.210154719831366,0.11040282790138,
-1.18378319822383));
#78764=CARTESIAN_POINT('Ctrl Pts',(-0.195708108043289,0.13527366252212,
-1.18555517197028));
#78765=CARTESIAN_POINT('Ctrl Pts',(-0.184456672933163,0.150254158165038,
-1.18668276027806));
#78766=CARTESIAN_POINT('Ctrl Pts',(-0.168855845418044,0.166598567304544,
-1.18813307580829));
#78767=CARTESIAN_POINT('Ctrl Pts',(-0.166076516447608,0.169369321325349,
-1.18838756609604));
#78768=CARTESIAN_POINT('Ctrl Pts',(-0.161866074459566,0.173363456895554,
-1.18876839769736));
#78769=CARTESIAN_POINT('Ctrl Pts',(-0.160486991618448,0.174640887053243,
-1.18889242017034));
#78770=CARTESIAN_POINT('Ctrl Pts',(-0.157995729885839,0.176894088274434,
-1.18911529286234));
#78771=CARTESIAN_POINT('Ctrl Pts',(-0.156889318883804,0.177876110198741,
-1.18921387324091));
#78772=CARTESIAN_POINT('Ctrl Pts',(-0.154518828904213,0.179940773423516,
-1.18942428197248));
#78773=CARTESIAN_POINT('Ctrl Pts',(-0.153252401354669,0.181020583527869,
-1.18953621966753));
#78774=CARTESIAN_POINT('Ctrl Pts',(-0.149791691648096,0.183908986331325,
-1.18984090462305));
#78775=CARTESIAN_POINT('Ctrl Pts',(-0.147576137778808,0.185691541213951,
-1.19003468315785));
#78776=CARTESIAN_POINT('Ctrl Pts',(-0.132429907503383,0.197435363255094,
-1.1913514468248));
#78777=CARTESIAN_POINT('Ctrl Pts',(-0.118535028197694,0.206076842626899,
-1.19252554982149));
#78778=CARTESIAN_POINT('Ctrl Pts',(-0.0909763132200518,0.219501395551439,
-1.19476145484212));
#78779=CARTESIAN_POINT('Ctrl Pts',(-0.077542711279048,0.224599080845148,
-1.19581385467492));
#78780=CARTESIAN_POINT('Ctrl Pts',(-0.0615844206030869,0.229050871030349,
-1.19697127888527));
#78781=CARTESIAN_POINT('Ctrl Pts',(-0.0594304186414556,0.229619181719115,
-1.19712557344875));
#78782=CARTESIAN_POINT('Ctrl Pts',(-0.0562415411308435,0.230412651372072,
-1.19735084695065));
#78783=CARTESIAN_POINT('Ctrl Pts',(-0.0552127230172826,0.230661345235265,
-1.19742304571925));
#78784=CARTESIAN_POINT('Ctrl Pts',(-0.0533741286526486,0.231092777980647,
-1.19755117394801));
#78785=CARTESIAN_POINT('Ctrl Pts',(-0.0525650207246063,0.231278162187507,
-1.19760724729238));
#78786=CARTESIAN_POINT('Ctrl Pts',(-0.0507673437369217,0.231680127535726,
-1.19773113934569));
#78787=CARTESIAN_POINT('Ctrl Pts',(-0.0497783466183655,0.231894633372684,
-1.19779884161479));
#78788=CARTESIAN_POINT('Ctrl Pts',(-0.0468414856311332,0.232511961224511,
-1.1979986139317));
#78789=CARTESIAN_POINT('Ctrl Pts',(-0.0448898384669629,0.232896629276128,
-1.1981297151378));
#78790=CARTESIAN_POINT('Ctrl Pts',(-0.0426010743960498,0.233317901883917,
-1.19828177758529));
#78791=CARTESIAN_POINT('Ctrl Pts',(-0.0422685137818562,0.233378378649217,
-1.19830383099465));
#78792=CARTESIAN_POINT('Ctrl Pts',(-0.0419358257152316,0.23343814415511,
-1.19832585242651));
#78793=CARTESIAN_POINT('',(-0.237175055044089,5.9077571581536E-5,-1.19544314726977));
#78794=CARTESIAN_POINT('Ctrl Pts',(-0.0419358439263085,0.233438140883593,
-1.21800162451869));
#78795=CARTESIAN_POINT('Ctrl Pts',(-0.0481832754706132,0.232315825082111,
-1.21755312230286));
#78796=CARTESIAN_POINT('Ctrl Pts',(-0.0543849249259875,0.230942845640307,
-1.21709801040124));
#78797=CARTESIAN_POINT('Ctrl Pts',(-0.0660051115692908,0.227875887400181,
-1.21622856511696));
#78798=CARTESIAN_POINT('Ctrl Pts',(-0.0714306853965034,0.226233836549135,
-1.21581554198375));
#78799=CARTESIAN_POINT('Ctrl Pts',(-0.0891987386654505,0.220153392967026,
-1.21444481671099));
#78800=CARTESIAN_POINT('Ctrl Pts',(-0.101233010577412,0.214885713774959,
-1.21348563312763));
#78801=CARTESIAN_POINT('Ctrl Pts',(-0.114769745884238,0.207569382010105,
-1.21241010430238));
#78802=CARTESIAN_POINT('Ctrl Pts',(-0.116753015793813,0.206460352526113,
-1.2122526592125));
#78803=CARTESIAN_POINT('Ctrl Pts',(-0.11964347709157,0.204789053961714,
-1.21202371936478));
#78804=CARTESIAN_POINT('Ctrl Pts',(-0.120563234595947,0.204248928532995,
-1.21195094906331));
#78805=CARTESIAN_POINT('Ctrl Pts',(-0.122192397466522,0.203277366927712,
-1.21182223547746));
#78806=CARTESIAN_POINT('Ctrl Pts',(-0.12290321702151,0.20284838973218,-1.21176614228712));
#78807=CARTESIAN_POINT('Ctrl Pts',(-0.124469105945273,0.201892127998671,
-1.21164272055101));
#78808=CARTESIAN_POINT('Ctrl Pts',(-0.125323091549005,0.201363135899676,
-1.21157550308749));
#78809=CARTESIAN_POINT('Ctrl Pts',(-0.127827451402393,0.199789733597376,
-1.2113785784341));
#78810=CARTESIAN_POINT('Ctrl Pts',(-0.129468362186863,0.198730316712671,
-1.21124979946835));
#78811=CARTESIAN_POINT('Ctrl Pts',(-0.142141382055089,0.19032466504217,
-1.2102556299785));
#78812=CARTESIAN_POINT('Ctrl Pts',(-0.152554743999959,0.182084586471879,
-1.20944039810114));
#78813=CARTESIAN_POINT('Ctrl Pts',(-0.174527780677602,0.161481922963948,
-1.20759224170489));
#78814=CARTESIAN_POINT('Ctrl Pts',(-0.185562908911338,0.148669732259347,
-1.20656311849887));
#78815=CARTESIAN_POINT('Ctrl Pts',(-0.196889356537466,0.13227234268149,
-1.20527819735666));
#78816=CARTESIAN_POINT('Ctrl Pts',(-0.198583650983616,0.129714777650927,
-1.20507876298616));
#78817=CARTESIAN_POINT('Ctrl Pts',(-0.201241433686387,0.12552865123598,
-1.20475344088543));
#78818=CARTESIAN_POINT('Ctrl Pts',(-0.202235906231281,0.123920114589567,
-1.20462869233618));
#78819=CARTESIAN_POINT('Ctrl Pts',(-0.203974265404521,0.121031692420664,
-1.20440504446034));
#78820=CARTESIAN_POINT('Ctrl Pts',(-0.204725613153335,0.119756397185868,
-1.20430642288659));
#78821=CARTESIAN_POINT('Ctrl Pts',(-0.206292546161303,0.117038928817861,
-1.20409648953868));
#78822=CARTESIAN_POINT('Ctrl Pts',(-0.207105051777241,0.115595080984363,
-1.20398507378913));
#78823=CARTESIAN_POINT('Ctrl Pts',(-0.209254465579841,0.111680091186355,
-1.20368324331998));
#78824=CARTESIAN_POINT('Ctrl Pts',(-0.210562664326068,0.109193577408518,
-1.20349182968687));
#78825=CARTESIAN_POINT('Ctrl Pts',(-0.21336296895045,0.10363346077934,-1.20306426403028));
#78826=CARTESIAN_POINT('Ctrl Pts',(-0.214833430602607,0.100549717870182,
-1.20282742691546));
#78827=CARTESIAN_POINT('Ctrl Pts',(-0.219273659906438,0.0906955952659816,
-1.2020714177945));
#78828=CARTESIAN_POINT('Ctrl Pts',(-0.221993572046388,0.0838180506411659,
-1.20154479707658));
#78829=CARTESIAN_POINT('Ctrl Pts',(-0.229817428001329,0.0609664895496733,
-1.19980267347884));
#78830=CARTESIAN_POINT('Ctrl Pts',(-0.233550414748087,0.0445774651567908,
-1.19856149451342));
#78831=CARTESIAN_POINT('Ctrl Pts',(-0.236056795047792,0.0234435553854519,
-1.19704415606684));
#78832=CARTESIAN_POINT('Ctrl Pts',(-0.236460734547928,0.0189403817494118,
-1.1967258311806));
#78833=CARTESIAN_POINT('Ctrl Pts',(-0.236822474981413,0.0130049531258889,
-1.19631503900962));
#78834=CARTESIAN_POINT('Ctrl Pts',(-0.236896377527786,0.0115810201544257,
-1.19621715202846));
#78835=CARTESIAN_POINT('Ctrl Pts',(-0.236995636875841,0.00926522985563239,
-1.19605912546995));
#78836=CARTESIAN_POINT('Ctrl Pts',(-0.237028809321001,0.00837376861655289,
-1.19599857498779));
#78837=CARTESIAN_POINT('Ctrl Pts',(-0.23708153664459,0.00670320283296535,
-1.19588565963598));
#78838=CARTESIAN_POINT('Ctrl Pts',(-0.237102282419113,0.00592415785210215,
-1.19583323006463));
#78839=CARTESIAN_POINT('Ctrl Pts',(-0.237138178825484,0.00426979397335219,
-1.19572234715988));
#78840=CARTESIAN_POINT('Ctrl Pts',(-0.237152323864252,0.00339445763363649,
-1.19566394869549));
#78841=CARTESIAN_POINT('Ctrl Pts',(-0.23717033193529,0.0016990446880916,
-1.19555132749142));
#78842=CARTESIAN_POINT('Ctrl Pts',(-0.237174788959285,0.000878991296439202,
-1.19549707534045));
#78843=CARTESIAN_POINT('Ctrl Pts',(-0.237174992681668,5.89190195836492E-5,
-1.19544302870655));
#78844=CARTESIAN_POINT('Ctrl Pts',(-0.237174992640464,5.90846497784872E-5,
-1.19544303962237));
#78845=CARTESIAN_POINT('Ctrl Pts',(-0.23717571343138,-0.00283428242356205,
-1.19525235297691));
#78846=CARTESIAN_POINT('Ctrl Pts',(-0.237123488630181,-0.00572759877968307,
-1.19506424287379));
#78847=CARTESIAN_POINT('Ctrl Pts',(-0.236503771768316,-0.0227687045973912,
-1.19396767567369));
#78848=CARTESIAN_POINT('Ctrl Pts',(-0.234723191033778,-0.0368450523929681,
-1.19310682893217));
#78849=CARTESIAN_POINT('Ctrl Pts',(-0.228534035968796,-0.0651406092883096,
-1.19132962795524));
#78850=CARTESIAN_POINT('Ctrl Pts',(-0.224024566439007,-0.0792718214660879,
-1.19041554110495));
#78851=CARTESIAN_POINT('Ctrl Pts',(-0.217087957597159,-0.0955681589639875,
-1.18926820578326));
#78852=CARTESIAN_POINT('Ctrl Pts',(-0.215898705552173,-0.0982252619154099,
-1.18907811239317));
#78853=CARTESIAN_POINT('Ctrl Pts',(-0.213947213138157,-0.102378645776983,
-1.18877581340901));
#78854=CARTESIAN_POINT('Ctrl Pts',(-0.213217447541096,-0.103889927045731,
-1.18866472045405));
#78855=CARTESIAN_POINT('Ctrl Pts',(-0.211815496879125,-0.106716243866289,
-1.1884548233863));
#78856=CARTESIAN_POINT('Ctrl Pts',(-0.211146944919434,-0.108032999148215,
-1.18835614948209));
#78857=CARTESIAN_POINT('Ctrl Pts',(-0.209610349512394,-0.110990665758213,
-1.18813245925699));
#78858=CARTESIAN_POINT('Ctrl Pts',(-0.208735258496133,-0.112627785331814,
-1.18800719958805));
#78859=CARTESIAN_POINT('Ctrl Pts',(-0.20642100083665,-0.116837668412553,
-1.18768125377528));
#78860=CARTESIAN_POINT('Ctrl Pts',(-0.204952961038353,-0.119394106865174,
-1.18747955674621));
#78861=CARTESIAN_POINT('Ctrl Pts',(-0.192409671674333,-0.140323629130649,
-1.18579613848267));
#78862=CARTESIAN_POINT('Ctrl Pts',(-0.178937578504926,-0.157140627398603,
-1.18422224984896));
#78863=CARTESIAN_POINT('Ctrl Pts',(-0.1587849526264,-0.176294504272544,
-1.182200873858));
#78864=CARTESIAN_POINT('Ctrl Pts',(-0.154001323005728,-0.180488271378968,
-1.18174171122945));
#78865=CARTESIAN_POINT('Ctrl Pts',(-0.14706719896306,-0.18609069837606,
-1.18110989233811));
#78866=CARTESIAN_POINT('Ctrl Pts',(-0.145053844145608,-0.187664307944215,
-1.180930210797));
#78867=CARTESIAN_POINT('Ctrl Pts',(-0.141906397311298,-0.19004338318521,
-1.1806555400361));
#78868=CARTESIAN_POINT('Ctrl Pts',(-0.140790047312149,-0.190871883434588,
-1.1805592970011));
#78869=CARTESIAN_POINT('Ctrl Pts',(-0.138728450155233,-0.192373970829441,
-1.1803838048426));
#78870=CARTESIAN_POINT('Ctrl Pts',(-0.137785425931719,-0.193050522078221,
-1.18030437688981));
#78871=CARTESIAN_POINT('Ctrl Pts',(-0.136825087547286,-0.193728873097802,
-1.18022437462264));
#78872=CARTESIAN_POINT('Ctrl Pts',(-0.136812724756105,-0.193737603987655,
-1.18022334487149));
#78873=CARTESIAN_POINT('Ctrl Pts',(-0.136788035365436,-0.193755036666225,
-1.18022128867867));
#78874=CARTESIAN_POINT('Ctrl Pts',(-0.136775708772323,-0.19376373846129,
-1.18022026223662));
#78875=CARTESIAN_POINT('Ctrl Pts',(-0.136751078476457,-0.193781122370797,
-1.18021821155198));
#78876=CARTESIAN_POINT('Ctrl Pts',(-0.136738774776263,-0.19378980449045,
-1.18021718730901));
#78877=CARTESIAN_POINT('Ctrl Pts',(-0.136714176725909,-0.193807158622976,
-1.18021513989389));
#78878=CARTESIAN_POINT('Ctrl Pts',(-0.13670188237759,-0.193815830637692,
-1.18021411672162));
#78879=CARTESIAN_POINT('Ctrl Pts',(-0.136677289186981,-0.193833174332872,
-1.18021207029527));
#78880=CARTESIAN_POINT('Ctrl Pts',(-0.136664990344591,-0.1938418460126,
-1.18021104704125));
#78881=CARTESIAN_POINT('Ctrl Pts',(-0.136640373948553,-0.193859199057687,
-1.18020899926902));
#78882=CARTESIAN_POINT('Ctrl Pts',(-0.136628056392239,-0.193867880420062,
-1.180207974751));
#78883=CARTESIAN_POINT('Ctrl Pts',(-0.13660338789969,-0.193885263152169,
-1.18020592323225));
#78884=CARTESIAN_POINT('Ctrl Pts',(-0.136591036958593,-0.193893964516269,
-1.18020489623186));
#78885=CARTESIAN_POINT('Ctrl Pts',(-0.13656628649085,-0.193911397934974,
-1.18020283848658));
#78886=CARTESIAN_POINT('Ctrl Pts',(-0.136553886957918,-0.193920129980571,
-1.18020180774228));
#78887=CARTESIAN_POINT('Ctrl Pts',(-0.136529023470478,-0.193937635871761,
-1.18019974119647));
#78888=CARTESIAN_POINT('Ctrl Pts',(-0.136516559507797,-0.193946409705064,
-1.18019870539578));
#78889=CARTESIAN_POINT('Ctrl Pts',(-0.136491550590124,-0.193964010779834,
-1.18019662736496));
#78890=CARTESIAN_POINT('Ctrl Pts',(-0.136479005624352,-0.193972838005955,
-1.18019558513585));
#78891=CARTESIAN_POINT('Ctrl Pts',(-0.13645381727651,-0.193990558055298,
-1.18019349280672));
#78892=CARTESIAN_POINT('Ctrl Pts',(-0.136441173881835,-0.193999450859234,
-1.180192442708));
#78893=CARTESIAN_POINT('Ctrl Pts',(-0.136415770267691,-0.194017314924671,
-1.18019033311819));
#78894=CARTESIAN_POINT('Ctrl Pts',(-0.136403010031694,-0.194026286164016,
-1.18018927362854));
#78895=CARTESIAN_POINT('Ctrl Pts',(-0.136377353189231,-0.194044320737727,
-1.18018714364286));
#78896=CARTESIAN_POINT('Ctrl Pts',(-0.136364456564841,-0.194053384044809,
-1.18018607314867));
#78897=CARTESIAN_POINT('Ctrl Pts',(-0.136338506092843,-0.194071617285636,
-1.18018391943345));
#78898=CARTESIAN_POINT('Ctrl Pts',(-0.136325452223259,-0.19408078718826,
-1.18018283621449));
#78899=CARTESIAN_POINT('Ctrl Pts',(-0.136299164903168,-0.194099249182386,
-1.18018065520663));
#78900=CARTESIAN_POINT('Ctrl Pts',(-0.136285931427581,-0.194108541237587,
-1.18017955742017));
#78901=CARTESIAN_POINT('Ctrl Pts',(-0.13625926080581,-0.194127264285969,
-1.180177345293));
#78902=CARTESIAN_POINT('Ctrl Pts',(-0.136245823629571,-0.194136695238176,
-1.180176230955));
#78903=CARTESIAN_POINT('Ctrl Pts',(-0.136218719519434,-0.194155714199198,
-1.18017398357752));
#78904=CARTESIAN_POINT('Ctrl Pts',(-0.136205052551574,-0.194165302160654,
-1.1801728505412));
#78905=CARTESIAN_POINT('Ctrl Pts',(-0.136177460464758,-0.194184654840767,
-1.1801705634317));
#78906=CARTESIAN_POINT('Ctrl Pts',(-0.136163535307626,-0.194194419504753,
-1.18016940936219));
#78907=CARTESIAN_POINT('Ctrl Pts',(-0.136135395780618,-0.194214147121066,
-1.1801670776332));
#78908=CARTESIAN_POINT('Ctrl Pts',(-0.136121181366843,-0.1942241100111,
-1.18016589997789));
#78909=CARTESIAN_POINT('Ctrl Pts',(-0.136092429166997,-0.194244257736242,
-1.1801635182714));
#78910=CARTESIAN_POINT('Ctrl Pts',(-0.136077891330581,-0.194254442500297,
-1.18016231422499));
#78911=CARTESIAN_POINT('Ctrl Pts',(-0.136048454515408,-0.194275060107551,
-1.18015987663575));
#78912=CARTESIAN_POINT('Ctrl Pts',(-0.13603355548025,-0.19428549286868,
-1.18015864309847));
#78913=CARTESIAN_POINT('Ctrl Pts',(-0.136003354276113,-0.194306635500447,
-1.18015614308253));
#78914=CARTESIAN_POINT('Ctrl Pts',(-0.135988052040609,-0.194317345278435,
-1.18015487661007));
#78915=CARTESIAN_POINT('Ctrl Pts',(-0.135956997479325,-0.194339074380238,
-1.18015230687368));
#78916=CARTESIAN_POINT('Ctrl Pts',(-0.135941245078386,-0.194350093596838,
-1.18015100361697));
#78917=CARTESIAN_POINT('Ctrl Pts',(-0.135916103532947,-0.19436767621355,
-1.18014892394344));
#78918=CARTESIAN_POINT('Ctrl Pts',(-0.135906715257174,-0.194374240845436,
-1.18014814744364));
#78919=CARTESIAN_POINT('Ctrl Pts',(-0.135239915317502,-0.194840420256555,
-1.18009300279612));
#78920=CARTESIAN_POINT('Ctrl Pts',(-0.134580187697683,-0.195296690146628,
-1.18003886439368));
#78921=CARTESIAN_POINT('Ctrl Pts',(-0.133054832223663,-0.196340231067417,
-1.17991465064266));
#78922=CARTESIAN_POINT('Ctrl Pts',(-0.132187621147164,-0.19692513204853,
-1.17984473241733));
#78923=CARTESIAN_POINT('Ctrl Pts',(-0.129515197985657,-0.198701971352152,
-1.1796313176645));
#78924=CARTESIAN_POINT('Ctrl Pts',(-0.127697468455801,-0.199875004154864,
-1.17948899818403));
#78925=CARTESIAN_POINT('Ctrl Pts',(-0.113099343294529,-0.209015132386064,
-1.17836629878244));
#78926=CARTESIAN_POINT('Ctrl Pts',(-0.0996007901584415,-0.215774406846182,
-1.17744899296487));
#78927=CARTESIAN_POINT('Ctrl Pts',(-0.0709712821265411,-0.226846664402345,
-1.17556638437772));
#78928=CARTESIAN_POINT('Ctrl Pts',(-0.0558721049781062,-0.231029342004321,
-1.17460397910813));
#78929=CARTESIAN_POINT('Ctrl Pts',(-0.0376354152584684,-0.234187628086533,
-1.17340462834023));
#78930=CARTESIAN_POINT('Ctrl Pts',(-0.0347899742566997,-0.234627206767253,
-1.17321657150095));
#78931=CARTESIAN_POINT('Ctrl Pts',(-0.0302810581251585,-0.235239945699456,
-1.17291677210019));
#78932=CARTESIAN_POINT('Ctrl Pts',(-0.0286224864007411,-0.235447504904431,
-1.17280611060909));
#78933=CARTESIAN_POINT('Ctrl Pts',(-0.0254937732926261,-0.235805495581379,
-1.17259657511645));
#78934=CARTESIAN_POINT('Ctrl Pts',(-0.0240241436796043,-0.235959752021114,
-1.17249782632186));
#78935=CARTESIAN_POINT('Ctrl Pts',(-0.0206949118531588,-0.236277772929812,
-1.17227334534506));
#78936=CARTESIAN_POINT('Ctrl Pts',(-0.0188346438174366,-0.236433333529347,
-1.17214736276259));
#78937=CARTESIAN_POINT('Ctrl Pts',(-0.0131272684522955,-0.23684281605482,
-1.17175906349662));
#78938=CARTESIAN_POINT('Ctrl Pts',(-0.00927581123095014,-0.23702489532715,
-1.17149454497683));
#78939=CARTESIAN_POINT('Ctrl Pts',(0.0133253485765188,-0.237541692357222,
-1.16992688982243));
#78940=CARTESIAN_POINT('Ctrl Pts',(0.0320543621561828,-0.235745406568818,
-1.16855804385412));
#78941=CARTESIAN_POINT('Ctrl Pts',(0.0602544759826042,-0.229616307893173,
-1.16645403396751));
#78942=CARTESIAN_POINT('Ctrl Pts',(0.0699901438947053,-0.226838422821999,
-1.16572112293165));
#78943=CARTESIAN_POINT('Ctrl Pts',(0.0816837076881318,-0.22267696206279,
-1.16485331695987));
#78944=CARTESIAN_POINT('Ctrl Pts',(0.0838366973694974,-0.221875340411693,
-1.16469409794925));
#78945=CARTESIAN_POINT('Ctrl Pts',(0.0869761781877329,-0.220654192397584,
-1.16446309039073));
#78946=CARTESIAN_POINT('Ctrl Pts',(0.0879719415245645,-0.220259087918213,
-1.16438999452244));
#78947=CARTESIAN_POINT('Ctrl Pts',(0.089661337720843,-0.219575475398744,
-1.16426631893732));
#78948=CARTESIAN_POINT('Ctrl Pts',(0.0903563204855477,-0.219290401716164,
-1.16421554083563));
#78949=CARTESIAN_POINT('Ctrl Pts',(0.0919419634242805,-0.218631171543051,
-1.16409992172058));
#78950=CARTESIAN_POINT('Ctrl Pts',(0.0928317048229706,-0.218254870440072,
-1.16403520992679));
#78951=CARTESIAN_POINT('Ctrl Pts',(0.0952985530389372,-0.217193744214037,
-1.16385618567953));
#78952=CARTESIAN_POINT('Ctrl Pts',(0.0968705862958924,-0.216497174735559,
-1.16374254794702));
#78953=CARTESIAN_POINT('Ctrl Pts',(0.108613919945221,-0.211140164870983,
-1.16289601318515));
#78954=CARTESIAN_POINT('Ctrl Pts',(0.118452973115967,-0.205781709215421,
-1.16219976709747));
#78955=CARTESIAN_POINT('Ctrl Pts',(0.135296045942244,-0.19499882471013,
-1.16096824065607));
#78956=CARTESIAN_POINT('Ctrl Pts',(0.142443785311366,-0.18984027509809,
-1.16043125136447));
#78957=CARTESIAN_POINT('Ctrl Pts',(0.155361903658598,-0.179376026077553,
-1.15940545020663));
#78958=CARTESIAN_POINT('Ctrl Pts',(0.16118842765626,-0.174158999298415,
-1.15891869467996));
#78959=CARTESIAN_POINT('Ctrl Pts',(0.169263964329329,-0.166175278172396,
-1.15819665200071));
#78960=CARTESIAN_POINT('Ctrl Pts',(0.171725297880547,-0.163630476480484,
-1.15796960016637));
#78961=CARTESIAN_POINT('Ctrl Pts',(0.17608987934439,-0.158910914797117,
-1.15755307494382));
#78962=CARTESIAN_POINT('Ctrl Pts',(0.178012113622753,-0.156754619310853,
-1.15736441129175));
#78963=CARTESIAN_POINT('Ctrl Pts',(0.180985026645301,-0.153294492364698,
-1.15706386707515));
#78964=CARTESIAN_POINT('Ctrl Pts',(0.182062141361734,-0.152013676031831,
-1.15695307694633));
#78965=CARTESIAN_POINT('Ctrl Pts',(0.184064461264845,-0.149580872621275,
-1.15674343442754));
#78966=CARTESIAN_POINT('Ctrl Pts',(0.184992635775463,-0.148431424887543,
-1.15664470874059));
#78967=CARTESIAN_POINT('Ctrl Pts',(0.187067185084337,-0.145812625829884,
-1.15642046733574));
#78968=CARTESIAN_POINT('Ctrl Pts',(0.188207090294475,-0.144338298471596,
-1.15629470335024));
#78969=CARTESIAN_POINT('Ctrl Pts',(0.19164138993426,-0.139786594999662,
-1.15590778747334));
#78970=CARTESIAN_POINT('Ctrl Pts',(0.193878453539476,-0.136666955606424,
-1.15564445654857));
#78971=CARTESIAN_POINT('Ctrl Pts',(0.206604223226656,-0.117978975412042,
-1.1540768581113));
#78972=CARTESIAN_POINT('Ctrl Pts',(0.215288743854662,-0.101266271111253,
-1.15270666238492));
#78973=CARTESIAN_POINT('Ctrl Pts',(0.225483045351733,-0.0742412920769977,
-1.15060079122418));
#78974=CARTESIAN_POINT('Ctrl Pts',(0.228445234185086,-0.0645537589485454,
-1.14986742452374));
#78975=CARTESIAN_POINT('Ctrl Pts',(0.23130966592657,-0.0524699799103707,
-1.14899914651404));
#78976=CARTESIAN_POINT('Ctrl Pts',(0.231807164342592,-0.0502264858064748,
-1.14883988428649));
#78977=CARTESIAN_POINT('Ctrl Pts',(0.232488717182714,-0.0469268027877572,
-1.14860882638611));
#78978=CARTESIAN_POINT('Ctrl Pts',(0.232698326629021,-0.0458761085165478,
-1.14853572261445));
#78979=CARTESIAN_POINT('Ctrl Pts',(0.233042780784099,-0.0440863609553087,
-1.14841203822367));
#78980=CARTESIAN_POINT('Ctrl Pts',(0.233181243354767,-0.0433480415182524,
-1.1483612591427));
#78981=CARTESIAN_POINT('Ctrl Pts',(0.233489734654157,-0.0416588222514061,
-1.1482456441009));
#78982=CARTESIAN_POINT('Ctrl Pts',(0.233657464882031,-0.04070752814505,
-1.14818093730115));
#78983=CARTESIAN_POINT('Ctrl Pts',(0.234107519078384,-0.0380605447374178,
-1.14800194062593));
#78984=CARTESIAN_POINT('Ctrl Pts',(0.23437723378552,-0.03636273172241,-1.14788832513783));
#78985=CARTESIAN_POINT('Ctrl Pts',(0.236258131354591,-0.0236308883771642,
-1.14704424307061));
#78986=CARTESIAN_POINT('Ctrl Pts',(0.237108022606951,-0.0124969777036749,
-1.14635018056881));
#78987=CARTESIAN_POINT('Ctrl Pts',(0.237222106362764,0.00764528731840521,
-1.14510970813887));
#78988=CARTESIAN_POINT('Ctrl Pts',(0.236761988005263,0.0166294764994894,
-1.14456182047828));
#78989=CARTESIAN_POINT('Ctrl Pts',(0.234785677560178,0.0348569184840514,
-1.14343013261823));
#78990=CARTESIAN_POINT('Ctrl Pts',(0.233230126660741,0.0440795023206173,
-1.1428467093291));
#78991=CARTESIAN_POINT('Ctrl Pts',(0.230231859226091,0.0571093858675861,
-1.14198920209376));
#78992=CARTESIAN_POINT('Ctrl Pts',(0.229229278212034,0.0610092281020387,
-1.14172825093923));
#78993=CARTESIAN_POINT('Ctrl Pts',(0.227608727782022,0.066707199742506,
-1.14133963830574));
#78994=CARTESIAN_POINT('Ctrl Pts',(0.227067595627987,0.0685265651250507,
-1.14121443980705));
#78995=CARTESIAN_POINT('Ctrl Pts',(0.226065495052678,0.0717535068402572,
-1.1409902932548));
#78996=CARTESIAN_POINT('Ctrl Pts',(0.225613064297506,0.073163644289787,
-1.14089162772368));
#78997=CARTESIAN_POINT('Ctrl Pts',(0.2246278283599,0.0761383671523528,-1.14068192555849));
#78998=CARTESIAN_POINT('Ctrl Pts',(0.22409181696016,0.0777017989396298,
-1.14057078799549));
#78999=CARTESIAN_POINT('Ctrl Pts',(0.222606912065868,0.0818897519950092,
-1.14027052747034));
#79000=CARTESIAN_POINT('Ctrl Pts',(0.221627988211237,0.0845032689838849,
-1.14008042344662));
#79001=CARTESIAN_POINT('Ctrl Pts',(0.215219142871203,0.100735544230943,
-1.13888207996312));
#79002=CARTESIAN_POINT('Ctrl Pts',(0.208583204862185,0.113841282203137,
-1.13783325996404));
#79003=CARTESIAN_POINT('Ctrl Pts',(0.194432690161524,0.136345766527621,
-1.13589853544609));
#79004=CARTESIAN_POINT('Ctrl Pts',(0.187331109504395,0.14594967601894,-1.13502216821175));
#79005=CARTESIAN_POINT('Ctrl Pts',(0.175973922020966,0.159106548687766,
-1.13377662396129));
#79006=CARTESIAN_POINT('Ctrl Pts',(0.172269160985255,0.163110580995786,
-1.13339089834269));
#79007=CARTESIAN_POINT('Ctrl Pts',(0.167395270323038,0.168026668420938,
-1.13291231818626));
#79008=CARTESIAN_POINT('Ctrl Pts',(0.166351499667832,0.169060097773275,
-1.13281142126191));
#79009=CARTESIAN_POINT('Ctrl Pts',(0.164651716452049,0.17071205433796,-1.1326497582156));
#79010=CARTESIAN_POINT('Ctrl Pts',(0.16400167919979,0.171336635063889,-1.13258854688121));
#79011=CARTESIAN_POINT('Ctrl Pts',(0.162732234401276,0.172542522364348,
-1.13247021972754));
#79012=CARTESIAN_POINT('Ctrl Pts',(0.162113242334103,0.17312422946334,-1.1324130753917));
#79013=CARTESIAN_POINT('Ctrl Pts',(0.160565818415407,0.174562867857997,
-1.13227154946347));
#79014=CARTESIAN_POINT('Ctrl Pts',(0.159633621480794,0.175415746007112,
-1.13218746777091));
#79015=CARTESIAN_POINT('Ctrl Pts',(0.15627488324745,0.178439745861253,-1.13188850171064));
#79016=CARTESIAN_POINT('Ctrl Pts',(0.153810387821108,0.18056840574687,-1.13167647401497));
#79017=CARTESIAN_POINT('Ctrl Pts',(0.138141201076488,0.193548669630834,
-1.13036770839144));
#79018=CARTESIAN_POINT('Ctrl Pts',(0.123838347104174,0.202998216631934,
-1.12934041704827));
#79019=CARTESIAN_POINT('Ctrl Pts',(0.101371473007988,0.214575655586314,
-1.12778297015812));
#79020=CARTESIAN_POINT('Ctrl Pts',(0.0939119077846063,0.217943630893141,
-1.12727458701274));
#79021=CARTESIAN_POINT('Ctrl Pts',(0.0813055343578469,0.222867828632727,
-1.12641498976776));
#79022=CARTESIAN_POINT('Ctrl Pts',(0.0762531265663769,0.224646639916416,
-1.12607042489111));
#79023=CARTESIAN_POINT('Ctrl Pts',(0.069128485665901,0.226886980855791,
-1.12558207963748));
#79024=CARTESIAN_POINT('Ctrl Pts',(0.0671035072269477,0.22749410641624,
-1.12544301642279));
#79025=CARTESIAN_POINT('Ctrl Pts',(0.0636151842462336,0.228489343394919,
-1.12520287314986));
#79026=CARTESIAN_POINT('Ctrl Pts',(0.0621557195680453,0.228890668346634,
-1.12510222639941));
#79027=CARTESIAN_POINT('Ctrl Pts',(0.059178380292214,0.229678804571674,
-1.12489650311316));
#79028=CARTESIAN_POINT('Ctrl Pts',(0.0576603177507672,0.23006460292077,
-1.12479139959907));
#79029=CARTESIAN_POINT('Ctrl Pts',(0.0538236818327608,0.230999282853407,
-1.12452518422509));
#79030=CARTESIAN_POINT('Ctrl Pts',(0.0515004974405383,0.231528303774867,
-1.12436344715271));
#79031=CARTESIAN_POINT('Ctrl Pts',(0.0423794431009992,0.233461224261411,
-1.12372614550876));
#79032=CARTESIAN_POINT('Ctrl Pts',(0.0355298387196741,0.23460130896958,
-1.12324243105599));
#79033=CARTESIAN_POINT('Ctrl Pts',(0.0131211319716126,0.23732727781197,
-1.12164312504461));
#79034=CARTESIAN_POINT('Ctrl Pts',(-0.00254581916659853,0.237675876068617,
-1.12049590675736));
#79035=CARTESIAN_POINT('Ctrl Pts',(-0.0248166681487722,0.235968378843026,
-1.11887035590126));
#79036=CARTESIAN_POINT('Ctrl Pts',(-0.0314781245514314,0.235172451103579,
-1.11838538808268));
#79037=CARTESIAN_POINT('Ctrl Pts',(-0.0393785578008861,0.233886714018427,
-1.11781750139299));
#79038=CARTESIAN_POINT('Ctrl Pts',(-0.0406581203423751,0.233667676608155,
-1.11772575923853));
#79039=CARTESIAN_POINT('Ctrl Pts',(-0.041935825738619,0.233438144150908,
-1.1176344235547));
#79040=CARTESIAN_POINT('Origin',(0.,0.,-1.7456589891905));
#79041=CARTESIAN_POINT('',(-0.0419358256939468,0.233438144158933,-0.997911004226539));
#79042=CARTESIAN_POINT('',(-0.0419358384531382,0.233438141866817,-1.01783655831731));
#79043=CARTESIAN_POINT('',(-0.0419358257166344,0.233438144154858,-1.7456589891905));
#79044=CARTESIAN_POINT('',(-0.237174940775019,-0.000167610758756324,-1.07580646542871));
#79045=CARTESIAN_POINT('Ctrl Pts',(-0.0419358256939468,0.233438144158933,
-0.997911004226539));
#79046=CARTESIAN_POINT('Ctrl Pts',(-0.0395037055194274,0.233875060619492,
-0.998070885658115));
#79047=CARTESIAN_POINT('Ctrl Pts',(-0.0370649471817316,0.234273933759101,
-0.998231859080892));
#79048=CARTESIAN_POINT('Ctrl Pts',(-0.0327621878678806,0.234908807711934,
-0.998517273008057));
#79049=CARTESIAN_POINT('Ctrl Pts',(-0.0309007925650829,0.235160901460861,
-0.998641204004634));
#79050=CARTESIAN_POINT('Ctrl Pts',(-0.0275685550342167,0.235571949680004,
-0.998863976190943));
#79051=CARTESIAN_POINT('Ctrl Pts',(-0.0260988342980983,0.235739303854267,
-0.998962548508873));
#79052=CARTESIAN_POINT('Ctrl Pts',(-0.0229715385961057,0.236065799542703,
-0.999173008536609));
#79053=CARTESIAN_POINT('Ctrl Pts',(-0.0213136677327853,0.236221253536087,
-0.999285006236125));
#79054=CARTESIAN_POINT('Ctrl Pts',(-0.0168165544126772,0.23659520873371,
-0.999590030645525));
#79055=CARTESIAN_POINT('Ctrl Pts',(-0.0139748686674424,0.236780047973819,
-0.999784092559481));
#79056=CARTESIAN_POINT('Ctrl Pts',(-0.00765908000192806,0.237076775547993,
-1.00021850949973));
#79057=CARTESIAN_POINT('Ctrl Pts',(-0.00418451024441479,0.237163544281956,
-1.00045958404844));
#79058=CARTESIAN_POINT('Ctrl Pts',(0.00688332156365574,0.237196650520249,
-1.00123425551244));
#79059=CARTESIAN_POINT('Ctrl Pts',(0.0144721234967209,0.236854745070778,
-1.00177571935123));
#79060=CARTESIAN_POINT('Ctrl Pts',(0.0295711457241576,0.235446126494015,
-1.00287056801049));
#79061=CARTESIAN_POINT('Ctrl Pts',(0.0370731570972976,0.234381963261688,
-1.00342330109824));
#79062=CARTESIAN_POINT('Ctrl Pts',(0.0561602198867919,0.230735055215907,
-1.00484176435888));
#79063=CARTESIAN_POINT('Ctrl Pts',(0.0676270761274038,0.227638456918103,
-1.00570614079791));
#79064=CARTESIAN_POINT('Ctrl Pts',(0.0809992281168247,0.222927048008454,
-1.00669762269112));
#79065=CARTESIAN_POINT('Ctrl Pts',(0.083172165866514,0.222125494957821,
-1.0068581628455));
#79066=CARTESIAN_POINT('Ctrl Pts',(0.0863360119806713,0.220905475324993,
-1.00709072135076));
#79067=CARTESIAN_POINT('Ctrl Pts',(0.0873362954927727,0.220511921662653,
-1.00716407077778));
#79068=CARTESIAN_POINT('Ctrl Pts',(0.0891050594726022,0.219802091612276,
-1.00729341487535));
#79069=CARTESIAN_POINT('Ctrl Pts',(0.0898745948312143,0.219488560920778,
-1.00734956525357));
#79070=CARTESIAN_POINT('Ctrl Pts',(0.0915652039246766,0.218789375992474,
-1.00747264774058));
#79071=CARTESIAN_POINT('Ctrl Pts',(0.0924855047009454,0.218401943965069,
-1.00753947342932));
#79072=CARTESIAN_POINT('Ctrl Pts',(0.0951705600999876,0.217251562481697,
-1.00773400616461));
#79073=CARTESIAN_POINT('Ctrl Pts',(0.0969285659546191,0.216472932698964,
-1.00786081896333));
#79074=CARTESIAN_POINT('Ctrl Pts',(0.100966386160027,0.214625506608964,
-1.00815123568739));
#79075=CARTESIAN_POINT('Ctrl Pts',(0.103239069689121,0.213541599673102,
-1.00831406286444));
#79076=CARTESIAN_POINT('Ctrl Pts',(0.111057652169243,0.209658687004037,
-1.00887348328622));
#79077=CARTESIAN_POINT('Ctrl Pts',(0.116510842144015,0.206678013438127,
-1.0092623755141));
#79078=CARTESIAN_POINT('Ctrl Pts',(0.139758560259365,0.192758040598492,
-1.01094119849615));
#79079=CARTESIAN_POINT('Ctrl Pts',(0.156179431548195,0.179711110205591,
-1.01219158069486));
#79080=CARTESIAN_POINT('Ctrl Pts',(0.173287549748883,0.161979968531225,
-1.01377532910191));
#79081=CARTESIAN_POINT('Ctrl Pts',(0.175830562782717,0.159215877948241,
-1.01401914618759));
#79082=CARTESIAN_POINT('Ctrl Pts',(0.179525563313952,0.155003126083689,
-1.01438705624024));
#79083=CARTESIAN_POINT('Ctrl Pts',(0.180728038580167,0.153599390388899,
-1.01450905880859));
#79084=CARTESIAN_POINT('Ctrl Pts',(0.182861322127711,0.151049321250023,
-1.01472973217788));
#79085=CARTESIAN_POINT('Ctrl Pts',(0.183798073446195,0.14990806719247,-1.01482815451542));
#79086=CARTESIAN_POINT('Ctrl Pts',(0.18578059734147,0.147446219615703,-1.01503979342924));
#79087=CARTESIAN_POINT('Ctrl Pts',(0.186823073535118,0.146123088418209,
-1.01515313429471));
#79088=CARTESIAN_POINT('Ctrl Pts',(0.189645521350974,0.142461203614739,
-1.01546578083391));
#79089=CARTESIAN_POINT('Ctrl Pts',(0.191396201537394,0.140100360436919,
-1.01566621162363));
#79090=CARTESIAN_POINT('Ctrl Pts',(0.202109076250495,0.125078084565119,
-1.01693509022905));
#79091=CARTESIAN_POINT('Ctrl Pts',(0.209853328757292,0.111597610748854,
-1.01804904138494));
#79092=CARTESIAN_POINT('Ctrl Pts',(0.22241519543432,0.0837278678197506,
-1.02027734978069));
#79093=CARTESIAN_POINT('Ctrl Pts',(0.227283070624532,0.0694359463824354,
-1.02138508368915));
#79094=CARTESIAN_POINT('Ctrl Pts',(0.231263654141999,0.0526669738965393,
-1.02258830719844));
#79095=CARTESIAN_POINT('Ctrl Pts',(0.231735782018901,0.0505491446729149,
-1.02273851225793));
#79096=CARTESIAN_POINT('Ctrl Pts',(0.232392654371467,0.0473997033287799,
-1.02295899762309));
#79097=CARTESIAN_POINT('Ctrl Pts',(0.232599718162231,0.04637293280376,-1.02303042724171));
#79098=CARTESIAN_POINT('Ctrl Pts',(0.232958608523065,0.044530391475474,
-1.02315775770819));
#79099=CARTESIAN_POINT('Ctrl Pts',(0.233112963382452,0.0437151622787919,
-1.02321379448628));
#79100=CARTESIAN_POINT('Ctrl Pts',(0.233447851712856,0.0418942132404122,
-1.02333829396824));
#79101=CARTESIAN_POINT('Ctrl Pts',(0.23362616763129,0.0408881213423924,
-1.02340663304528));
#79102=CARTESIAN_POINT('Ctrl Pts',(0.234140671618654,0.037871889577955,
-1.02361025670466));
#79103=CARTESIAN_POINT('Ctrl Pts',(0.234457468222649,0.0358584774264697,
-1.0237445157702));
#79104=CARTESIAN_POINT('Ctrl Pts',(0.236651664567177,0.020637841411547,
-1.02474863622168));
#79105=CARTESIAN_POINT('Ctrl Pts',(0.237437993336628,0.00729561798802651,
-1.02556829761763));
#79106=CARTESIAN_POINT('Ctrl Pts',(0.236674537128162,-0.0226565124179727,
-1.02740638068047));
#79107=CARTESIAN_POINT('Ctrl Pts',(0.2345063536851,-0.0391771551577578,
-1.02842145672832));
#79108=CARTESIAN_POINT('Ctrl Pts',(0.229911195095774,-0.0583292898643307,
-1.02969118834136));
#79109=CARTESIAN_POINT('Ctrl Pts',(0.229134509341683,-0.0613093705956127,
-1.02989136937367));
#79110=CARTESIAN_POINT('Ctrl Pts',(0.227786573459721,-0.0660972599727433,
-1.03021768593589));
#79111=CARTESIAN_POINT('Ctrl Pts',(0.227251270761086,-0.0679148762477218,
-1.03034267102888));
#79112=CARTESIAN_POINT('Ctrl Pts',(0.22625888593375,-0.0711413406657514,
-1.03056660613414));
#79113=CARTESIAN_POINT('Ctrl Pts',(0.225810271827769,-0.0725527034847115,
-1.03066527610617));
#79114=CARTESIAN_POINT('Ctrl Pts',(0.224832244951795,-0.0755326605728396,
-1.03087516842429));
#79115=CARTESIAN_POINT('Ctrl Pts',(0.224299569249094,-0.0771000919416258,
-1.03098649345032));
#79116=CARTESIAN_POINT('Ctrl Pts',(0.222821219024635,-0.0813052045236052,
-1.03128771683671));
#79117=CARTESIAN_POINT('Ctrl Pts',(0.221845162712163,-0.0839318446342196,
-1.03147860675645));
#79118=CARTESIAN_POINT('Ctrl Pts',(0.214978749279347,-0.101452672615652,
-1.03277094216049));
#79119=CARTESIAN_POINT('Ctrl Pts',(0.207640258122412,-0.115731820248825,
-1.03392154336467));
#79120=CARTESIAN_POINT('Ctrl Pts',(0.190866620668025,-0.141565051613736,
-1.0361673230617));
#79121=CARTESIAN_POINT('Ctrl Pts',(0.181668931873745,-0.153190075005969,
-1.03725418555946));
#79122=CARTESIAN_POINT('Ctrl Pts',(0.16993967111422,-0.165460723834768,
-1.03843942680745));
#79123=CARTESIAN_POINT('Ctrl Pts',(0.168409994050772,-0.167017417344487,
-1.03859052592468));
#79124=CARTESIAN_POINT('Ctrl Pts',(0.166112903541157,-0.16929142340211,
-1.03881205931299));
#79125=CARTESIAN_POINT('Ctrl Pts',(0.165361911283401,-0.17002506039485,
-1.03888365815618));
#79126=CARTESIAN_POINT('Ctrl Pts',(0.164008659216534,-0.171329591298828,
-1.03901116303144));
#79127=CARTESIAN_POINT('Ctrl Pts',(0.163408249876109,-0.171902335894749,
-1.03906720674767));
#79128=CARTESIAN_POINT('Ctrl Pts',(0.162063422706916,-0.173171784893965,
-1.03919156767787));
#79129=CARTESIAN_POINT('Ctrl Pts',(0.161317507197171,-0.173866851442591,
-1.03925976288274));
#79130=CARTESIAN_POINT('Ctrl Pts',(0.159075352176605,-0.175929307564545,
-1.03946251298447));
#79131=CARTESIAN_POINT('Ctrl Pts',(0.157565998515745,-0.177282389745873,
-1.03959605535742));
#79132=CARTESIAN_POINT('Ctrl Pts',(0.14680435203695,-0.18668379279955,-1.04052926957786));
#79133=CARTESIAN_POINT('Ctrl Pts',(0.13695621997452,-0.194024298481766,
-1.04128660916368));
#79134=CARTESIAN_POINT('Ctrl Pts',(0.111475754418332,-0.210105411199603,
-1.04313702348199));
#79135=CARTESIAN_POINT('Ctrl Pts',(0.0953411112426121,-0.217901638173178,
-1.04422336469095));
#79136=CARTESIAN_POINT('Ctrl Pts',(0.0756558190753961,-0.224804728092625,
-1.04556929784692));
#79137=CARTESIAN_POINT('Ctrl Pts',(0.0728082600008156,-0.22574305021203,
-1.04576430875033));
#79138=CARTESIAN_POINT('Ctrl Pts',(0.0681557743682794,-0.227178943837498,
-1.04608386395093));
#79139=CARTESIAN_POINT('Ctrl Pts',(0.0663613458199406,-0.227709581594742,
-1.04620733608837));
#79140=CARTESIAN_POINT('Ctrl Pts',(0.0631381880482992,-0.228621380954511,
-1.04642960536175));
#79141=CARTESIAN_POINT('Ctrl Pts',(0.0617118039432741,-0.229010523130603,
-1.04652813848353));
#79142=CARTESIAN_POINT('Ctrl Pts',(0.0586671946068927,-0.229810635622641,
-1.04673886187873));
#79143=CARTESIAN_POINT('Ctrl Pts',(0.0570480886870439,-0.230217903949045,
-1.04685116543061));
#79144=CARTESIAN_POINT('Ctrl Pts',(0.0526359396573457,-0.231278329753846,
-1.04715792139466));
#79145=CARTESIAN_POINT('Ctrl Pts',(0.0498352077782843,-0.231897949044186,
-1.04735342915494));
#79146=CARTESIAN_POINT('Ctrl Pts',(0.0435856875377352,-0.233162120464749,
-1.04779160436029));
#79147=CARTESIAN_POINT('Ctrl Pts',(0.0401324999153883,-0.233781237102707,
-1.0480350107266));
#79148=CARTESIAN_POINT('Ctrl Pts',(0.0290548992958242,-0.235514662775766,
-1.04882007640004));
#79149=CARTESIAN_POINT('Ctrl Pts',(0.0213899516262793,-0.236334073523972,
-1.04936984116713));
#79150=CARTESIAN_POINT('Ctrl Pts',(0.00478799391328773,-0.237294613084045,
-1.05057110856909));
#79151=CARTESIAN_POINT('Ctrl Pts',(-0.00414509168481391,-0.237306693014067,
-1.05122406692639));
#79152=CARTESIAN_POINT('Ctrl Pts',(-0.0242902853884312,-0.236195952007191,
-1.05269541458123));
#79153=CARTESIAN_POINT('Ctrl Pts',(-0.035466344310009,-0.234778066270788,
-1.05351101266602));
#79154=CARTESIAN_POINT('Ctrl Pts',(-0.0481873793934987,-0.232234614500244,
-1.05441163721122));
#79155=CARTESIAN_POINT('Ctrl Pts',(-0.0498705338404079,-0.231878998590682,
-1.05453021653198));
#79156=CARTESIAN_POINT('Ctrl Pts',(-0.0524930028081179,-0.231295047854816,
-1.05471390190666));
#79157=CARTESIAN_POINT('Ctrl Pts',(-0.0534350043918111,-0.231079239428459,
-1.05477966583622));
#79158=CARTESIAN_POINT('Ctrl Pts',(-0.0551070662549488,-0.230685405854194,
-1.05489598017823));
#79159=CARTESIAN_POINT('Ctrl Pts',(-0.0558376110229498,-0.230509666703362,
-1.05494665433323));
#79160=CARTESIAN_POINT('Ctrl Pts',(-0.0576079170433217,-0.230074893519484,
-1.05506911274893));
#79161=CARTESIAN_POINT('Ctrl Pts',(-0.058646774827929,-0.229812281322856,
-1.05514069337026));
#79162=CARTESIAN_POINT('Ctrl Pts',(-0.061907423111873,-0.228964473593114,
-1.05536458143485));
#79163=CARTESIAN_POINT('Ctrl Pts',(-0.0641225870506104,-0.228354010235895,
-1.05551553889758));
#79164=CARTESIAN_POINT('Ctrl Pts',(-0.0760387201802356,-0.224883034764211,
-1.05632314052172));
#79165=CARTESIAN_POINT('Ctrl Pts',(-0.0855591086550003,-0.221436111529642,
-1.05695258421108));
#79166=CARTESIAN_POINT('Ctrl Pts',(-0.112001080645514,-0.209901502775712,
-1.05872974198964));
#79167=CARTESIAN_POINT('Ctrl Pts',(-0.128221636485734,-0.2004046965426,
-1.0598610489778));
#79168=CARTESIAN_POINT('Ctrl Pts',(-0.146237878195228,-0.186765647193521,
-1.06131218136869));
#79169=CARTESIAN_POINT('Ctrl Pts',(-0.149262305835884,-0.184357493278386,
-1.06156297218875));
#79170=CARTESIAN_POINT('Ctrl Pts',(-0.153659624721604,-0.180677041837979,
-1.06193932951711));
#79171=CARTESIAN_POINT('Ctrl Pts',(-0.155078580404469,-0.179460600924075,
-1.06206265767154));
#79172=CARTESIAN_POINT('Ctrl Pts',(-0.157593859110736,-0.177252197603157,
-1.06228476957315));
#79173=CARTESIAN_POINT('Ctrl Pts',(-0.158695574409021,-0.176266504130917,
-1.06238329083007));
#79174=CARTESIAN_POINT('Ctrl Pts',(-0.160960147694014,-0.174201973018063,
-1.06258842426603));
#79175=CARTESIAN_POINT('Ctrl Pts',(-0.162121538277117,-0.173121642679709,
-1.06269509673446));
#79176=CARTESIAN_POINT('Ctrl Pts',(-0.165218586701251,-0.170182260488473,
-1.0629836062656));
#79177=CARTESIAN_POINT('Ctrl Pts',(-0.167133620764754,-0.168301916091612,
-1.06316635310828));
#79178=CARTESIAN_POINT('Ctrl Pts',(-0.171322343294662,-0.16404706792143,
-1.06357606163662));
#79179=CARTESIAN_POINT('Ctrl Pts',(-0.173579366219792,-0.161657006033895,
-1.06380368119495));
#79180=CARTESIAN_POINT('Ctrl Pts',(-0.180460826024781,-0.154059614458277,
-1.06451964334591));
#79181=CARTESIAN_POINT('Ctrl Pts',(-0.184905782807541,-0.148695363808847,
-1.06501457395697));
#79182=CARTESIAN_POINT('Ctrl Pts',(-0.194794536377068,-0.135631276239693,
-1.06619366010916));
#79183=CARTESIAN_POINT('Ctrl Pts',(-0.200028103684586,-0.127786919545031,
-1.06688210049181));
#79184=CARTESIAN_POINT('Ctrl Pts',(-0.210368095907426,-0.110090393717345,
-1.06837768425044));
#79185=CARTESIAN_POINT('Ctrl Pts',(-0.215279144308696,-0.100147728734526,
-1.06918280575839));
#79186=CARTESIAN_POINT('Ctrl Pts',(-0.220350216298021,-0.087767091446773,
-1.07011827124123));
#79187=CARTESIAN_POINT('Ctrl Pts',(-0.221191759099009,-0.0856241020359536,
-1.07027783831571));
#79188=CARTESIAN_POINT('Ctrl Pts',(-0.222379393101687,-0.0824653628230672,
-1.0705092639707));
#79189=CARTESIAN_POINT('Ctrl Pts',(-0.22274998036216,-0.0814590504621102,
-1.07058243601345));
#79190=CARTESIAN_POINT('Ctrl Pts',(-0.223395543726707,-0.0796687007431247,
-1.07071159105221));
#79191=CARTESIAN_POINT('Ctrl Pts',(-0.22367324072467,-0.0788856912771928,
-1.0707677279384));
#79192=CARTESIAN_POINT('Ctrl Pts',(-0.224276289152258,-0.0771565144426505,
-1.07089092803574));
#79193=CARTESIAN_POINT('Ctrl Pts',(-0.224599773585302,-0.0762097329305833,
-1.07095788333495));
#79194=CARTESIAN_POINT('Ctrl Pts',(-0.225530436687023,-0.0734284458676882,
-1.07115318645172));
#79195=CARTESIAN_POINT('Ctrl Pts',(-0.226121215753691,-0.0715884830683424,
-1.07128062923413));
#79196=CARTESIAN_POINT('Ctrl Pts',(-0.227434682839628,-0.0673191537280007,
-1.07157273294577));
#79197=CARTESIAN_POINT('Ctrl Pts',(-0.228141061333201,-0.0648849801559172,
-1.07173660435289));
#79198=CARTESIAN_POINT('Ctrl Pts',(-0.234346240336132,-0.0421463515096981,
-1.07324667502831));
#79199=CARTESIAN_POINT('Ctrl Pts',(-0.23716007325367,-0.0212056605925111,
-1.0744921961247));
#79200=CARTESIAN_POINT('Ctrl Pts',(-0.237174940775019,-0.000167610758756324,
-1.07580646542871));
#79201=CARTESIAN_POINT('Ctrl Pts',(-0.237174940975967,-0.000167326167951933,
-1.0758064832074));
#79202=CARTESIAN_POINT('Ctrl Pts',(-0.237178862066123,0.0053905870843023,
-1.07615369207584));
#79203=CARTESIAN_POINT('Ctrl Pts',(-0.236987418744219,0.0109466937660265,
-1.07650459862563));
#79204=CARTESIAN_POINT('Ctrl Pts',(-0.236357235544948,0.0199882338165463,
-1.07708571951255));
#79205=CARTESIAN_POINT('Ctrl Pts',(-0.236035958238224,0.0234797083819207,
-1.07731257753821));
#79206=CARTESIAN_POINT('Ctrl Pts',(-0.235451748788358,0.028585350679067,
-1.07764857627253));
#79207=CARTESIAN_POINT('Ctrl Pts',(-0.235249318460083,0.0302060627445365,
-1.07775586497137));
#79208=CARTESIAN_POINT('Ctrl Pts',(-0.234844445694626,0.0331961253736699,
-1.07795503732914));
#79209=CARTESIAN_POINT('Ctrl Pts',(-0.23464672248286,0.0345660513302701,
-1.07804677063649));
#79210=CARTESIAN_POINT('Ctrl Pts',(-0.234212791364183,0.0373970501584988,
-1.07823737613234));
#79211=CARTESIAN_POINT('Ctrl Pts',(-0.233974875812903,0.0388577960900436,
-1.07833629820839));
#79212=CARTESIAN_POINT('Ctrl Pts',(-0.233402731425097,0.0421746639260142,
-1.07856226748829));
#79213=CARTESIAN_POINT('Ctrl Pts',(-0.233060006585016,0.044029198130332,
-1.07868957783672));
#79214=CARTESIAN_POINT('Ctrl Pts',(-0.232105461240899,0.0488705456121785,
-1.07902454410932));
#79215=CARTESIAN_POINT('Ctrl Pts',(-0.231458118140091,0.0518499124122168,
-1.07923330578739));
#79216=CARTESIAN_POINT('Ctrl Pts',(-0.228201385953775,0.0655594948387103,
-1.08020646466981));
#79217=CARTESIAN_POINT('Ctrl Pts',(-0.224902383434084,0.0761102998773847,
-1.08099207286858));
#79218=CARTESIAN_POINT('Ctrl Pts',(-0.214898809544695,0.101686817098394,
-1.08297985397713));
#79219=CARTESIAN_POINT('Ctrl Pts',(-0.207344183031431,0.116318988124808,
-1.08419510814419));
#79220=CARTESIAN_POINT('Ctrl Pts',(-0.1968971818537,0.132251231487878,-1.08554657566402));
#79221=CARTESIAN_POINT('Ctrl Pts',(-0.19541948445007,0.134425127051742,
-1.08573154644371));
#79222=CARTESIAN_POINT('Ctrl Pts',(-0.192761715652386,0.138198587886219,
-1.08605304185617));
#79223=CARTESIAN_POINT('Ctrl Pts',(-0.191597122826209,0.139808697461259,
-1.08619036016341));
#79224=CARTESIAN_POINT('Ctrl Pts',(-0.189809300981019,0.142216149260442,
-1.08639566263785));
#79225=CARTESIAN_POINT('Ctrl Pts',(-0.189201012937958,0.143024405775023,
-1.08646458600006));
#79226=CARTESIAN_POINT('Ctrl Pts',(-0.188084165482272,0.144488810588983,
-1.08658941907345));
#79227=CARTESIAN_POINT('Ctrl Pts',(-0.187577320183138,0.145146197636944,
-1.08664543841547));
#79228=CARTESIAN_POINT('Ctrl Pts',(-0.186416063762288,0.146636124650379,
-1.08677236760309));
#79229=CARTESIAN_POINT('Ctrl Pts',(-0.185759518108305,0.147466957045006,
-1.08684312701278));
#79230=CARTESIAN_POINT('Ctrl Pts',(-0.183703075522032,0.150033775571511,
-1.08706176988591));
#79231=CARTESIAN_POINT('Ctrl Pts',(-0.182284197757902,0.151754492177387,
-1.0872083916332));
#79232=CARTESIAN_POINT('Ctrl Pts',(-0.171580297743114,0.164368652182197,
-1.08828581918711));
#79233=CARTESIAN_POINT('Ctrl Pts',(-0.161349171137063,0.174423068417167,
-1.08916025726684));
#79234=CARTESIAN_POINT('Ctrl Pts',(-0.137584934772982,0.193884761787855,
-1.09104387152952));
#79235=CARTESIAN_POINT('Ctrl Pts',(-0.123855728318893,0.202929999385158,
-1.09205099101611));
#79236=CARTESIAN_POINT('Ctrl Pts',(-0.106808676220347,0.211782423124832,
-1.09329659049535));
#79237=CARTESIAN_POINT('Ctrl Pts',(-0.104290327266397,0.213033834424817,
-1.09348036552311));
#79238=CARTESIAN_POINT('Ctrl Pts',(-0.100253109059542,0.214951255750261,
-1.09377492901638));
#79239=CARTESIAN_POINT('Ctrl Pts',(-0.0987484288401349,0.2156466456769,
-1.09388470170737));
#79240=CARTESIAN_POINT('Ctrl Pts',(-0.0958862203241227,0.216933181829503,
-1.09409355313709));
#79241=CARTESIAN_POINT('Ctrl Pts',(-0.0945301989032289,0.217527501597632,
-1.09419251744437));
#79242=CARTESIAN_POINT('Ctrl Pts',(-0.0914296588243891,0.218851946143835,
-1.09441888364329));
#79243=CARTESIAN_POINT('Ctrl Pts',(-0.0896818122788387,0.219573971660029,
-1.09454655218031));
#79244=CARTESIAN_POINT('Ctrl Pts',(-0.0850774328848414,0.2214118681141,
-1.09488311449045));
#79245=CARTESIAN_POINT('Ctrl Pts',(-0.0822076444581387,0.222493340570655,
-1.09509313129082));
#79246=CARTESIAN_POINT('Ctrl Pts',(-0.067140052852537,0.227840220495628,
-1.09619750318521));
#79247=CARTESIAN_POINT('Ctrl Pts',(-0.0546373980029665,0.231156380301354,
-1.09712135088387));
#79248=CARTESIAN_POINT('Ctrl Pts',(-0.0419358102824288,0.233438146927524,
-1.09805944304797));
#79249=CARTESIAN_POINT('Ctrl Pts',(-0.041935825738619,0.233438144150908,
-1.1176344235547));
#79250=CARTESIAN_POINT('Ctrl Pts',(-0.0432584147431629,0.23320054861047,
-1.11753987940428));
#79251=CARTESIAN_POINT('Ctrl Pts',(-0.0445790138342224,0.232951707726502,
-1.11744577078433));
#79252=CARTESIAN_POINT('Ctrl Pts',(-0.0478545145984987,0.232305628549752,
-1.11721319422148));
#79253=CARTESIAN_POINT('Ctrl Pts',(-0.0498066840877963,0.231894921239782,
-1.11707532872025));
#79254=CARTESIAN_POINT('Ctrl Pts',(-0.0527420365903041,0.23123858723122,
-1.11686939068683));
#79255=CARTESIAN_POINT('Ctrl Pts',(-0.0537291523560751,0.231011222520726,
-1.11680037029715));
#79256=CARTESIAN_POINT('Ctrl Pts',(-0.0555221924243775,0.230586112531759,
-1.11667546141249));
#79257=CARTESIAN_POINT('Ctrl Pts',(-0.0563285566144401,0.230390457483617,
-1.11661946209737));
#79258=CARTESIAN_POINT('Ctrl Pts',(-0.0581593880948962,0.229936040176821,
-1.11649270523686));
#79259=CARTESIAN_POINT('Ctrl Pts',(-0.0591831699277879,0.229674660115662,
-1.11642209661691));
#79260=CARTESIAN_POINT('Ctrl Pts',(-0.0623513108756212,0.228843216399275,
-1.11620434306506));
#79261=CARTESIAN_POINT('Ctrl Pts',(-0.0644895124102746,0.228249879115558,
-1.11605844550895));
#79262=CARTESIAN_POINT('Ctrl Pts',(-0.0804411449225277,0.223581336608984,
-1.11497583139735));
#79263=CARTESIAN_POINT('Ctrl Pts',(-0.0938678722178763,0.218284964487372,
-1.11409628320732));
#79264=CARTESIAN_POINT('Ctrl Pts',(-0.121225158260334,0.204498946064232,
-1.11221768093849));
#79265=CARTESIAN_POINT('Ctrl Pts',(-0.134928190839646,0.195728522223323,
-1.111220778427));
#79266=CARTESIAN_POINT('Ctrl Pts',(-0.149870746536511,0.183844912791191,
-1.10998343070978));
#79267=CARTESIAN_POINT('Ctrl Pts',(-0.152081003720497,0.18202076745062,
-1.10979622974101));
#79268=CARTESIAN_POINT('Ctrl Pts',(-0.155525100972375,0.179071795722006,
-1.10949748089988));
#79269=CARTESIAN_POINT('Ctrl Pts',(-0.156781091943716,0.177973183444333,
-1.10938700094757));
#79270=CARTESIAN_POINT('Ctrl Pts',(-0.159127602488053,0.175876580659945,
-1.10917761533894));
#79271=CARTESIAN_POINT('Ctrl Pts',(-0.160220592650936,0.174881465624513,
-1.10907883277091));
#79272=CARTESIAN_POINT('Ctrl Pts',(-0.162676037205598,0.172603560706968,
-1.10885400800687));
#79273=CARTESIAN_POINT('Ctrl Pts',(-0.164032740614149,0.171314745156312,
-1.10872771235579));
#79274=CARTESIAN_POINT('Ctrl Pts',(-0.167523835053847,0.167918849777242,
-1.10839718727363));
#79275=CARTESIAN_POINT('Ctrl Pts',(-0.169633702827952,0.165787155296867,
-1.10819189907962));
#79276=CARTESIAN_POINT('Ctrl Pts',(-0.18633269399496,0.14826285050924,-1.10652098070454));
#79277=CARTESIAN_POINT('Ctrl Pts',(-0.198835186131925,0.131018926427349,
-1.10496576128198));
#79278=CARTESIAN_POINT('Ctrl Pts',(-0.211936469554454,0.106661251859097,
-1.10295434041515));
#79279=CARTESIAN_POINT('Ctrl Pts',(-0.21476233504746,0.100850581086543,
-1.10248776970752));
#79280=CARTESIAN_POINT('Ctrl Pts',(-0.218866844715034,0.0914532183775448,
-1.10176075598685));
#79281=CARTESIAN_POINT('Ctrl Pts',(-0.220302443603446,0.0879387522343233,
-1.10149476703641));
#79282=CARTESIAN_POINT('Ctrl Pts',(-0.222115461967171,0.0831768616275617,
-1.1011435827967));
#79283=CARTESIAN_POINT('Ctrl Pts',(-0.222567797019122,0.0819587986620246,
-1.10105454939646));
#79284=CARTESIAN_POINT('Ctrl Pts',(-0.223304577744365,0.079923678961788,
-1.10090718962121));
#79285=CARTESIAN_POINT('Ctrl Pts',(-0.223594599298818,0.079108685664839,
-1.10084854765242));
#79286=CARTESIAN_POINT('Ctrl Pts',(-0.224175104256493,0.0774487028060394,
-1.10072988227105));
#79287=CARTESIAN_POINT('Ctrl Pts',(-0.22446528291949,0.0766036276237135,
-1.10066987634708));
#79288=CARTESIAN_POINT('Ctrl Pts',(-0.22520818891043,0.074399622486152,
-1.10051438000326));
#79289=CARTESIAN_POINT('Ctrl Pts',(-0.22565340218859,0.0730381715987563,
-1.10041931512584));
#79290=CARTESIAN_POINT('Ctrl Pts',(-0.227469110746063,0.0673106546749251,
-1.10002318580741));
#79291=CARTESIAN_POINT('Ctrl Pts',(-0.228725529703862,0.0629091332568091,
-1.09972798206613));
#79292=CARTESIAN_POINT('Ctrl Pts',(-0.234701318000397,0.0394189412878362,
-1.09818747149911));
#79293=CARTESIAN_POINT('Ctrl Pts',(-0.237160909058553,0.0198342418859032,
-1.09701798258436));
#79294=CARTESIAN_POINT('Ctrl Pts',(-0.237180895959023,-0.00817906410562867,
-1.09526945720993));
#79295=CARTESIAN_POINT('Ctrl Pts',(-0.23674608175383,-0.0165210456300815,
-1.09474017428215));
#79296=CARTESIAN_POINT('Ctrl Pts',(-0.235605684004054,-0.0273576742908374,
-1.09403156010411));
#79297=CARTESIAN_POINT('Ctrl Pts',(-0.235298000269286,-0.0298886421000947,
-1.09386457201332));
#79298=CARTESIAN_POINT('Ctrl Pts',(-0.234730728404759,-0.0340004443507289,
-1.09359062134863));
#79299=CARTESIAN_POINT('Ctrl Pts',(-0.234495814488319,-0.0355845169790469,
-1.09348443583019));
#79300=CARTESIAN_POINT('Ctrl Pts',(-0.234010490452502,-0.0386433475482477,
-1.09327808426633));
#79301=CARTESIAN_POINT('Ctrl Pts',(-0.233762133698072,-0.0401183576945601,
-1.09317798762596));
#79302=CARTESIAN_POINT('Ctrl Pts',(-0.233147763302373,-0.0435675598671642,
-1.09294248566356));
#79303=CARTESIAN_POINT('Ctrl Pts',(-0.232770604039708,-0.0455396230792217,
-1.09280673365433));
#79304=CARTESIAN_POINT('Ctrl Pts',(-0.231434182177033,-0.052076446103443,
-1.09235295129829));
#79305=CARTESIAN_POINT('Ctrl Pts',(-0.230365358728379,-0.0566174277673322,
-1.09203149976684));
#79306=CARTESIAN_POINT('Ctrl Pts',(-0.227436181018103,-0.0675994291027317,
-1.09123837718875));
#79307=CARTESIAN_POINT('Ctrl Pts',(-0.225435366848108,-0.0739985218730699,
-1.09076274281024));
#79308=CARTESIAN_POINT('Ctrl Pts',(-0.219886246610391,-0.0894196673008559,
-1.08958509792107));
#79309=CARTESIAN_POINT('Ctrl Pts',(-0.216050722666752,-0.0983255080361264,
-1.08887747868718));
#79310=CARTESIAN_POINT('Ctrl Pts',(-0.211077489394449,-0.108166853959196,
-1.08807278828868));
#79311=CARTESIAN_POINT('Ctrl Pts',(-0.210463235784185,-0.109357218463305,
-1.08797507328014));
#79312=CARTESIAN_POINT('Ctrl Pts',(-0.204794420627367,-0.120118147979523,
-1.08708851419382));
#79313=CARTESIAN_POINT('Ctrl Pts',(-0.199099755496709,-0.129338562640794,
-1.08630504860256));
#79314=CARTESIAN_POINT('Ctrl Pts',(-0.191794456136614,-0.13953428040076,
-1.08543432176941));
#79315=CARTESIAN_POINT('Ctrl Pts',(-0.190779238413752,-0.140919166289695,
-1.08531596517228));
#79316=CARTESIAN_POINT('Ctrl Pts',(-0.189169783698143,-0.143065389767239,
-1.08513256053827));
#79317=CARTESIAN_POINT('Ctrl Pts',(-0.188585808980038,-0.143834298927607,
-1.08506685749316));
#79318=CARTESIAN_POINT('Ctrl Pts',(-0.187539111361058,-0.145195133329188,
-1.08495061294781));
#79319=CARTESIAN_POINT('Ctrl Pts',(-0.18707826474446,-0.145788435466187,
-1.08489994822086));
#79320=CARTESIAN_POINT('Ctrl Pts',(-0.185952965723256,-0.147223042905706,
-1.08477746600266));
#79321=CARTESIAN_POINT('Ctrl Pts',(-0.185285618023984,-0.148062046749886,
-1.08470585259045));
#79322=CARTESIAN_POINT('Ctrl Pts',(-0.183167875745051,-0.150687775624103,
-1.08448168594729));
#79323=CARTESIAN_POINT('Ctrl Pts',(-0.181697103286738,-0.15245799436519,
-1.08433048781053));
#79324=CARTESIAN_POINT('Ctrl Pts',(-0.173599167340606,-0.16192097419043,
-1.08352009172825));
#79325=CARTESIAN_POINT('Ctrl Pts',(-0.166508250020531,-0.169204379850674,
-1.0828883038835));
#79326=CARTESIAN_POINT('Ctrl Pts',(-0.14496027030146,-0.188666264735665,
-1.08109977920796));
#79327=CARTESIAN_POINT('Ctrl Pts',(-0.129489536818853,-0.199601713344846,
-1.07995946483688));
#79328=CARTESIAN_POINT('Ctrl Pts',(-0.109595528023059,-0.210368255174794,
-1.07850528921785));
#79329=CARTESIAN_POINT('Ctrl Pts',(-0.106263112035296,-0.212071051985996,
-1.07826233900726));
#79330=CARTESIAN_POINT('Ctrl Pts',(-0.101229227633994,-0.214494824395458,
-1.07789550127565));
#79331=CARTESIAN_POINT('Ctrl Pts',(-0.0995572560229314,-0.215275959346244,
-1.07777368633027));
#79332=CARTESIAN_POINT('Ctrl Pts',(-0.0965320681297575,-0.216646529050584,
-1.07755324147311));
#79333=CARTESIAN_POINT('Ctrl Pts',(-0.0951821297104626,-0.21724299929477,
-1.07745485826849));
#79334=CARTESIAN_POINT('Ctrl Pts',(-0.0922786719891962,-0.218493634851812,
-1.07724318150654));
#79335=CARTESIAN_POINT('Ctrl Pts',(-0.0907235770867759,-0.21914391180543,
-1.07712976255671));
#79336=CARTESIAN_POINT('Ctrl Pts',(-0.0864320615048512,-0.220884939992683,
-1.07681657502509));
#79337=CARTESIAN_POINT('Ctrl Pts',(-0.0836821241165773,-0.221941340717135,
-1.07661567436842));
#79338=CARTESIAN_POINT('Ctrl Pts',(-0.0661468319828223,-0.228305381865129,
-1.07533270991089));
#79339=CARTESIAN_POINT('Ctrl Pts',(-0.0508870687365766,-0.232183315238453,
-1.07420388970789));
#79340=CARTESIAN_POINT('Ctrl Pts',(-0.0206860742155622,-0.236736673614914,
-1.07197708491382));
#79341=CARTESIAN_POINT('Ctrl Pts',(-0.00583693106709541,-0.237567181760435,
-1.07088651934837));
#79342=CARTESIAN_POINT('Ctrl Pts',(0.0111713767472046,-0.236921783383169,
-1.06969812353675));
#79343=CARTESIAN_POINT('Ctrl Pts',(0.0133482226765466,-0.236809114880699,
-1.06954721637732));
#79344=CARTESIAN_POINT('Ctrl Pts',(0.0165701763129834,-0.236597782211589,
-1.06932592038241));
#79345=CARTESIAN_POINT('Ctrl Pts',(0.0176166108213919,-0.236522168979225,
-1.06925437013267));
#79346=CARTESIAN_POINT('Ctrl Pts',(0.0194894788098894,-0.236374340695349,
-1.06912693138538));
#79347=CARTESIAN_POINT('Ctrl Pts',(0.0203160699731221,-0.236304731406512,
-1.06907090556273));
#79348=CARTESIAN_POINT('Ctrl Pts',(0.022157803791001,-0.236139898833785,
-1.06894656186513));
#79349=CARTESIAN_POINT('Ctrl Pts',(0.0231727133625775,-0.236042465547013,
-1.06887836616163));
#79350=CARTESIAN_POINT('Ctrl Pts',(0.0262042667836905,-0.235731689030862,
-1.06867555262856));
#79351=CARTESIAN_POINT('Ctrl Pts',(0.0282188947616265,-0.235499017964752,
-1.06854194855638));
#79352=CARTESIAN_POINT('Ctrl Pts',(0.0425162286639773,-0.233661691164076,
-1.06760057908901));
#79353=CARTESIAN_POINT('Ctrl Pts',(0.0546612103196223,-0.231122582108777,
-1.066836022966));
#79354=CARTESIAN_POINT('Ctrl Pts',(0.0835576052644631,-0.222674558692563,
-1.06498741405034));
#79355=CARTESIAN_POINT('Ctrl Pts',(0.0999492663670512,-0.215814504679519,
-1.06390955869622));
#79356=CARTESIAN_POINT('Ctrl Pts',(0.118053699579086,-0.205728868638331,
-1.06257259555048));
#79357=CARTESIAN_POINT('Ctrl Pts',(0.120655360564963,-0.204213922242535,
-1.06237679568973));
#79358=CARTESIAN_POINT('Ctrl Pts',(0.124829066146606,-0.201675974774374,
-1.06205622661396));
#79359=CARTESIAN_POINT('Ctrl Pts',(0.126419097810772,-0.200683098265499,
-1.0619325415429));
#79360=CARTESIAN_POINT('Ctrl Pts',(0.129241827575505,-0.198873619299367,
-1.0617100648972));
#79361=CARTESIAN_POINT('Ctrl Pts',(0.130478986493682,-0.19806413194422,
-1.06161153981394));
#79362=CARTESIAN_POINT('Ctrl Pts',(0.133094500257903,-0.196317631088904,
-1.06140102372933));
#79363=CARTESIAN_POINT('Ctrl Pts',(0.134470702127523,-0.195377553211979,
-1.06128892131451));
#79364=CARTESIAN_POINT('Ctrl Pts',(0.138178099611331,-0.192787319425447,
-1.06098320895841));
#79365=CARTESIAN_POINT('Ctrl Pts',(0.140489515939453,-0.191109477573222,
-1.06078855538736));
#79366=CARTESIAN_POINT('Ctrl Pts',(0.145556013586486,-0.187290150293546,
-1.06035258462282));
#79367=CARTESIAN_POINT('Ctrl Pts',(0.148295226981576,-0.185128811831091,
-1.06011053968791));
#79368=CARTESIAN_POINT('Ctrl Pts',(0.156877657019354,-0.178044243243746,
-1.05933149275798));
#79369=CARTESIAN_POINT('Ctrl Pts',(0.162530690091508,-0.17289912606251,
-1.05878652292557));
#79370=CARTESIAN_POINT('Ctrl Pts',(0.173864174519878,-0.161536236966017,
-1.05762757763605));
#79371=CARTESIAN_POINT('Ctrl Pts',(0.179482076943847,-0.155270351159474,
-1.05701294170188));
#79372=CARTESIAN_POINT('Ctrl Pts',(0.191634048293048,-0.140173895407708,
-1.05559890707435));
#79373=CARTESIAN_POINT('Ctrl Pts',(0.197912449813362,-0.131160351655729,
-1.05480164848869));
#79374=CARTESIAN_POINT('Ctrl Pts',(0.204725113886799,-0.119770182574942,
-1.05387368016769));
#79375=CARTESIAN_POINT('Ctrl Pts',(0.205876817717127,-0.117779479506916,
-1.05371428644884));
#79376=CARTESIAN_POINT('Ctrl Pts',(0.207522567309833,-0.114836898388701,
-1.05348307539116));
#79377=CARTESIAN_POINT('Ctrl Pts',(0.20803936526954,-0.113897988499236,
-1.05340994758363));
#79378=CARTESIAN_POINT('Ctrl Pts',(0.208945332949383,-0.112225301201956,
-1.05328085484548));
#79379=CARTESIAN_POINT('Ctrl Pts',(0.209337033802809,-0.111492944795534,
-1.05322473634107));
#79380=CARTESIAN_POINT('Ctrl Pts',(0.210192080126655,-0.109873886307508,
-1.0531015600062));
#79381=CARTESIAN_POINT('Ctrl Pts',(0.210653670030632,-0.108986296542092,
-1.05303461019088));
#79382=CARTESIAN_POINT('Ctrl Pts',(0.21199054352247,-0.106375400452049,
-1.05283928139431));
#79383=CARTESIAN_POINT('Ctrl Pts',(0.212850418549568,-0.104644236702914,
-1.05271180808617));
#79384=CARTESIAN_POINT('Ctrl Pts',(0.214789057711334,-0.100618433236373,
-1.05241961094872));
#79385=CARTESIAN_POINT('Ctrl Pts',(0.215852397946036,-0.0983165897528305,
-1.05225567752442));
#79386=CARTESIAN_POINT('Ctrl Pts',(0.2194210200343,-0.0902543627498628,
-1.05169082208325));
#79387=CARTESIAN_POINT('Ctrl Pts',(0.221734378838158,-0.0844115511749129,
-1.05129776320076));
#79388=CARTESIAN_POINT('Ctrl Pts',(0.230975722706703,-0.058057775409552,
-1.04956810329019));
#79389=CARTESIAN_POINT('Ctrl Pts',(0.235308154437333,-0.0367496063000072,
-1.04827267502526));
#79390=CARTESIAN_POINT('Ctrl Pts',(0.236876294148964,-0.01224935120234,
-1.04668717273614));
#79391=CARTESIAN_POINT('Ctrl Pts',(0.237008590165596,-0.0093462475537947,
-1.04649800961096));
#79392=CARTESIAN_POINT('Ctrl Pts',(0.237137592671283,-0.00459818055543863,
-1.04618613342297));
#79393=CARTESIAN_POINT('Ctrl Pts',(0.237166174676999,-0.0027543404976851,
-1.0460644071904));
#79394=CARTESIAN_POINT('Ctrl Pts',(0.237178917304436,0.000565321360051544,
-1.04584405775318));
#79395=CARTESIAN_POINT('Ctrl Pts',(0.237170808543679,0.00204103122160897,
-1.04574568031712));
#79396=CARTESIAN_POINT('Ctrl Pts',(0.237123923356802,0.00520288001015451,
-1.04553394380727));
#79397=CARTESIAN_POINT('Ctrl Pts',(0.237080931901491,0.00688886512915874,
-1.04542045864654));
#79398=CARTESIAN_POINT('Ctrl Pts',(0.236913308281436,0.0115225442702795,
-1.04510689388477));
#79399=CARTESIAN_POINT('Ctrl Pts',(0.236751653754406,0.0144685089101486,
-1.04490567766309));
#79400=CARTESIAN_POINT('Ctrl Pts',(0.235372694165352,0.0332026542227912,
-1.04361368612197));
#79401=CARTESIAN_POINT('Ctrl Pts',(0.232631933987971,0.0488358064434803,
-1.04247534349324));
#79402=CARTESIAN_POINT('Ctrl Pts',(0.2243863945295,0.078221135425702,-1.04024984078445));
#79403=CARTESIAN_POINT('Ctrl Pts',(0.21911155581906,0.0919673583819196,
-1.03917057086671));
#79404=CARTESIAN_POINT('Ctrl Pts',(0.211628035709293,0.107099695578416,
-1.03799174648102));
#79405=CARTESIAN_POINT('Ctrl Pts',(0.210630725807367,0.109048010005371,
-1.03784020551841));
#79406=CARTESIAN_POINT('Ctrl Pts',(0.209114822937106,0.111911016950864,
-1.03761816690457));
#79407=CARTESIAN_POINT('Ctrl Pts',(0.208616920979453,0.112836453655353,
-1.03754649698122));
#79408=CARTESIAN_POINT('Ctrl Pts',(0.207714980146303,0.11448648752969,-1.0374189345759));
#79409=CARTESIAN_POINT('Ctrl Pts',(0.207313273852756,0.115212305549409,
-1.03736290352999));
#79410=CARTESIAN_POINT('Ctrl Pts',(0.206410129580288,0.116824121426516,
-1.03723865641094));
#79411=CARTESIAN_POINT('Ctrl Pts',(0.205906788185745,0.117709012463264,
-1.03717056137602));
#79412=CARTESIAN_POINT('Ctrl Pts',(0.204387682084271,0.120340088063792,
-1.03696835805898));
#79413=CARTESIAN_POINT('Ctrl Pts',(0.203355260157899,0.122076616166908,
-1.03683525450085));
#79414=CARTESIAN_POINT('Ctrl Pts',(0.19622874852658,0.133722017962486,-1.0359435488359));
#79415=CARTESIAN_POINT('Ctrl Pts',(0.189434191489689,0.143185389677278,
-1.03522296781266));
#79416=CARTESIAN_POINT('Ctrl Pts',(0.170008526071012,0.166424199934096,
-1.03336109604057));
#79417=CARTESIAN_POINT('Ctrl Pts',(0.156400355804899,0.179272882566176,
-1.03222990967809));
#79418=CARTESIAN_POINT('Ctrl Pts',(0.139084193357974,0.192135612061835,
-1.03083703494809));
#79419=CARTESIAN_POINT('Ctrl Pts',(0.136708374297954,0.193833241385375,
-1.03064698887796));
#79420=CARTESIAN_POINT('Ctrl Pts',(0.132778626281439,0.196533031779483,
-1.03033395521202));
#79421=CARTESIAN_POINT('Ctrl Pts',(0.131243208204679,0.197561676840038,
-1.03021196715654));
#79422=CARTESIAN_POINT('Ctrl Pts',(0.128460147090678,0.1993794121323,-1.02999133583768));
#79423=CARTESIAN_POINT('Ctrl Pts',(0.127216849449188,0.200175004485255,
-1.02989294111283));
#79424=CARTESIAN_POINT('Ctrl Pts',(0.124539605077382,0.201853170216394,
-1.02968137965615));
#79425=CARTESIAN_POINT('Ctrl Pts',(0.123103530718277,0.202732178084126,
-1.0295680888783));
#79426=CARTESIAN_POINT('Ctrl Pts',(0.11913709296571,0.205102314762505,-1.02925563121948));
#79427=CARTESIAN_POINT('Ctrl Pts',(0.11658827321648,0.206561805874336,-1.02905534103617));
#79428=CARTESIAN_POINT('Ctrl Pts',(0.100446991949007,0.215410612474166,
-1.0277894580985));
#79429=CARTESIAN_POINT('Ctrl Pts',(0.0861881651912132,0.221501177972588,
-1.02667862028116));
#79430=CARTESIAN_POINT('Ctrl Pts',(0.0570305285888865,0.230711662890633,
-1.02444985760861));
#79431=CARTESIAN_POINT('Ctrl Pts',(0.042217314780757,0.233876293929315,
-1.02333837641646));
#79432=CARTESIAN_POINT('Ctrl Pts',(0.0250501503004153,0.23585836026058,
-1.0221319627321));
#79433=CARTESIAN_POINT('Ctrl Pts',(0.0228941366896339,0.236077392957802,
-1.02198194878531));
#79434=CARTESIAN_POINT('Ctrl Pts',(0.0196926342274622,0.236358364298436,
-1.02176169994375));
#79435=CARTESIAN_POINT('Ctrl Pts',(0.018649317604025,0.236442972561779,
-1.02169031886137));
#79436=CARTESIAN_POINT('Ctrl Pts',(0.0167782821581367,0.236582243355564,
-1.02156305436527));
#79437=CARTESIAN_POINT('Ctrl Pts',(0.0159508028836025,0.236639473821558,
-1.02150703537961));
#79438=CARTESIAN_POINT('Ctrl Pts',(0.0141033221573189,0.23675751500798,
-1.0213825527393));
#79439=CARTESIAN_POINT('Ctrl Pts',(0.0130832122459482,0.236816076866771,
-1.02131421287601));
#79440=CARTESIAN_POINT('Ctrl Pts',(0.0100263736711766,0.236971749300597,
-1.02111052376976));
#79441=CARTESIAN_POINT('Ctrl Pts',(0.00798867851495863,0.237049192857883,
-1.02097620131491));
#79442=CARTESIAN_POINT('Ctrl Pts',(-0.00751269379989495,0.237438207772837,
-1.01996371900727));
#79443=CARTESIAN_POINT('Ctrl Pts',(-0.0209817699170307,0.236628836981253,
-1.01913673223224));
#79444=CARTESIAN_POINT('Ctrl Pts',(-0.0368600042990974,0.234307400803627,
-1.0181523677623));
#79445=CARTESIAN_POINT('Ctrl Pts',(-0.0394020145324293,0.233893328965883,
-1.01799451955588));
#79446=CARTESIAN_POINT('Ctrl Pts',(-0.0419358384531398,0.233438141866817,
-1.01783655831731));
#79447=CARTESIAN_POINT('Origin',(0.,0.,-1.7456589891905));
#79448=CARTESIAN_POINT('',(-0.0419358085112891,0.233438147245699,-0.898263402204347));
#79449=CARTESIAN_POINT('',(-0.0419358257166344,0.233438144154858,-0.917832673049623));
#79450=CARTESIAN_POINT('',(-0.0419358257166344,0.233438144154858,-1.7456589891905));
#79451=CARTESIAN_POINT('Ctrl Pts',(-0.0419358085112876,0.233438147245699,
-0.898263402204347));
#79452=CARTESIAN_POINT('Ctrl Pts',(-0.0319888766060671,0.235225055840433,
-0.898895225798914));
#79453=CARTESIAN_POINT('Ctrl Pts',(-0.0219318578014211,0.236375459711886,
-0.899511712826814));
#79454=CARTESIAN_POINT('Ctrl Pts',(0.00272931081665239,0.237606640110077,
-0.901027390268067));
#79455=CARTESIAN_POINT('Ctrl Pts',(0.0173186563714538,0.236990193389189,
-0.901929115462318));
#79456=CARTESIAN_POINT('Ctrl Pts',(0.0345123267016579,0.234667005850247,
-0.903054578955355));
#79457=CARTESIAN_POINT('Ctrl Pts',(0.0372596020371669,0.234246505485218,
-0.903236254471884));
#79458=CARTESIAN_POINT('Ctrl Pts',(0.0416257230043633,0.233499473865356,
-0.903528240560429));
#79459=CARTESIAN_POINT('Ctrl Pts',(0.0432496965276298,0.23320413510385,
-0.903637566652367));
#79460=CARTESIAN_POINT('Ctrl Pts',(0.046325568956889,0.232611518075377,
-0.903846070506072));
#79461=CARTESIAN_POINT('Ctrl Pts',(0.0477780279958681,0.232317533884336,
-0.903945139189474));
#79462=CARTESIAN_POINT('Ctrl Pts',(0.0510895793313697,0.231614892706939,
-0.904172455702432));
#79463=CARTESIAN_POINT('Ctrl Pts',(0.0529466776716615,0.231197432072285,
-0.904300978534616));
#79464=CARTESIAN_POINT('Ctrl Pts',(0.057823902761613,0.230039227300763,
-0.904641358884654));
#79465=CARTESIAN_POINT('Ctrl Pts',(0.0608347485656282,0.229261382723428,
-0.904854381261831));
#79466=CARTESIAN_POINT('Ctrl Pts',(0.0823465451792399,0.223250282427531,
-0.906397872384761));
#79467=CARTESIAN_POINT('Ctrl Pts',(0.100162873238279,0.215844320331424,
-0.907799880074513));
#79468=CARTESIAN_POINT('Ctrl Pts',(0.125812924226704,0.201316504406839,
-0.909949487679603));
#79469=CARTESIAN_POINT('Ctrl Pts',(0.134402978183474,0.1956862460259,-0.910693401308479));
#79470=CARTESIAN_POINT('Ctrl Pts',(0.144449562121192,0.18812668697498,-0.911572616295714));
#79471=CARTESIAN_POINT('Ctrl Pts',(0.146276713074969,0.186709535248029,
-0.911732891397154));
#79472=CARTESIAN_POINT('Ctrl Pts',(0.148922018199757,0.184595143502008,
-0.911965141409346));
#79473=CARTESIAN_POINT('Ctrl Pts',(0.149756560701523,0.183918751486441,
-0.912038442588177));
#79474=CARTESIAN_POINT('Ctrl Pts',(0.151167242551874,0.18275943326571,-0.912162359577785));
#79475=CARTESIAN_POINT('Ctrl Pts',(0.151745718614855,0.182279408077655,
-0.912213175675524));
#79476=CARTESIAN_POINT('Ctrl Pts',(0.15306127146946,0.181177145847669,-0.912328737402071));
#79477=CARTESIAN_POINT('Ctrl Pts',(0.153796845382576,0.180553154040393,
-0.912393355066334));
#79478=CARTESIAN_POINT('Ctrl Pts',(0.155827416314408,0.178809194829818,
-0.912571808566162));
#79479=CARTESIAN_POINT('Ctrl Pts',(0.157114154114831,0.177679640993131,
-0.912684976811264));
#79480=CARTESIAN_POINT('Ctrl Pts',(0.165813577980176,0.169874502992107,
-0.913451594860854));
#79481=CARTESIAN_POINT('Ctrl Pts',(0.172811851616639,0.162750123594717,
-0.91407606452951));
#79482=CARTESIAN_POINT('Ctrl Pts',(0.180882076414711,0.153424896482839,
-0.914837880136115));
#79483=CARTESIAN_POINT('Ctrl Pts',(0.182396277977555,0.15162164235704,-0.914982818756633));
#79484=CARTESIAN_POINT('Ctrl Pts',(0.188940325026111,0.143588446716834,
-0.915619517746367));
#79485=CARTESIAN_POINT('Ctrl Pts',(0.19367961999078,0.137128741727366,-0.916108381332049));
#79486=CARTESIAN_POINT('Ctrl Pts',(0.202270450707712,0.124083085174235,
-0.917072996734549));
#79487=CARTESIAN_POINT('Ctrl Pts',(0.206148895609117,0.117526878646687,
-0.917547635043089));
#79488=CARTESIAN_POINT('Ctrl Pts',(0.211331547029984,0.107717587695387,
-0.918253493502797));
#79489=CARTESIAN_POINT('Ctrl Pts',(0.21288988123294,0.104604006103212,-0.918476909430575));
#79490=CARTESIAN_POINT('Ctrl Pts',(0.215598850286897,0.0988799639369577,
-0.918887393180001));
#79491=CARTESIAN_POINT('Ctrl Pts',(0.216772011600246,0.0962808670801677,
-0.919073688260315));
#79492=CARTESIAN_POINT('Ctrl Pts',(0.218555885205595,0.092130782567806,
-0.919371345368958));
#79493=CARTESIAN_POINT('Ctrl Pts',(0.219197620987187,0.0905933704529978,
-0.91948165351673));
#79494=CARTESIAN_POINT('Ctrl Pts',(0.220378426406352,0.0876784892344844,
-0.91969093397954));
#79495=CARTESIAN_POINT('Ctrl Pts',(0.220920912300254,0.086302483382735,
-0.919789785527184));
#79496=CARTESIAN_POINT('Ctrl Pts',(0.222122553961468,0.0831689534384998,
-0.920015073220043));
#79497=CARTESIAN_POINT('Ctrl Pts',(0.222773779863433,0.0814085158215507,
-0.920141766482311));
#79498=CARTESIAN_POINT('Ctrl Pts',(0.224417420068755,0.0767978531035248,
-0.920473989617902));
#79499=CARTESIAN_POINT('Ctrl Pts',(0.225376420084786,0.0739361649639672,
-0.920680595850073));
#79500=CARTESIAN_POINT('Ctrl Pts',(0.232607012340755,0.0509104165485765,
-0.922346846383017));
#79501=CARTESIAN_POINT('Ctrl Pts',(0.236213491604805,0.0300121412479962,
-0.923895134425683));
#79502=CARTESIAN_POINT('Ctrl Pts',(0.237251504713968,0.00242790597118925,
-0.925902865784434));
#79503=CARTESIAN_POINT('Ctrl Pts',(0.23722902780818,-0.0040706487750538,
-0.92637220302656));
#79504=CARTESIAN_POINT('Ctrl Pts',(0.236770127078069,-0.014366785062582,
-0.927102966723891));
#79505=CARTESIAN_POINT('Ctrl Pts',(0.236508769790435,-0.0181687472925312,
-0.927370000774217));
#79506=CARTESIAN_POINT('Ctrl Pts',(0.23603539020919,-0.0232587319903634,
-0.927722341845574));
#79507=CARTESIAN_POINT('Ctrl Pts',(0.235904219791878,-0.0245534788415448,
-0.927811517314698));
#79508=CARTESIAN_POINT('Ctrl Pts',(0.235668061219351,-0.0267075802354654,
-0.927959058867024));
#79509=CARTESIAN_POINT('Ctrl Pts',(0.235569014407845,-0.0275675434954728,
-0.92801774192755));
#79510=CARTESIAN_POINT('Ctrl Pts',(0.235358188720312,-0.0293138472968358,
-0.928136437930932));
#79511=CARTESIAN_POINT('Ctrl Pts',(0.235246106804209,-0.0302001314727833,
-0.928196433825474));
#79512=CARTESIAN_POINT('Ctrl Pts',(0.234941487447494,-0.0325042348595186,
-0.928351819804342));
#79513=CARTESIAN_POINT('Ctrl Pts',(0.234741119756891,-0.0339210075579321,
-0.928446785683628));
#79514=CARTESIAN_POINT('Ctrl Pts',(0.233848577443344,-0.039844897126972,
-0.928841761282919));
#79515=CARTESIAN_POINT('Ctrl Pts',(0.233039273817071,-0.0443336915432166,
-0.929135953584295));
#79516=CARTESIAN_POINT('Ctrl Pts',(0.229251243090949,-0.0623514239198177,
-0.930306285253463));
#79517=CARTESIAN_POINT('Ctrl Pts',(0.225219367307328,-0.0756315542121117,
-0.931145925736226));
#79518=CARTESIAN_POINT('Ctrl Pts',(0.215742212030513,-0.0992001264668327,
-0.932706840439582));
#79519=CARTESIAN_POINT('Ctrl Pts',(0.210656937786624,-0.10958550398997,
-0.93342235517345));
#79520=CARTESIAN_POINT('Ctrl Pts',(0.2027722181171,-0.123094138228909,-0.934424965733036));
#79521=CARTESIAN_POINT('Ctrl Pts',(0.200617503706549,-0.126575484638188,
-0.934690186483372));
#79522=CARTESIAN_POINT('Ctrl Pts',(0.197326646982513,-0.131597209075127,
-0.935083968886161));
#79523=CARTESIAN_POINT('Ctrl Pts',(0.196260169098409,-0.133182494031873,
-0.935209970361829));
#79524=CARTESIAN_POINT('Ctrl Pts',(0.194332237145921,-0.135974853394169,
-0.935435036153001));
#79525=CARTESIAN_POINT('Ctrl Pts',(0.193478387075772,-0.137187071963324,
-0.935533809641351));
#79526=CARTESIAN_POINT('Ctrl Pts',(0.191652412792085,-0.139728468202048,
-0.93574320054388));
#79527=CARTESIAN_POINT('Ctrl Pts',(0.190677703206727,-0.14105568197786,
-0.935853913889724));
#79528=CARTESIAN_POINT('Ctrl Pts',(0.18803206828221,-0.144580577432116,
-0.93615168830083));
#79529=CARTESIAN_POINT('Ctrl Pts',(0.186336502464633,-0.146759356789292,
-0.936339702000014));
#79530=CARTESIAN_POINT('Ctrl Pts',(0.176794996504949,-0.158588099291582,
-0.937382921135005));
#79531=CARTESIAN_POINT('Ctrl Pts',(0.168238597987363,-0.167637532785864,
-0.938266581391823));
#79532=CARTESIAN_POINT('Ctrl Pts',(0.146059497676426,-0.187679074047201,
-0.94043187299895));
#79533=CARTESIAN_POINT('Ctrl Pts',(0.131852452782993,-0.19791859963494,
-0.941725639439422));
#79534=CARTESIAN_POINT('Ctrl Pts',(0.114160820006072,-0.207912146388026,
-0.943154650002809));
#79535=CARTESIAN_POINT('Ctrl Pts',(0.111646318887781,-0.209273158137317,
-0.943353709977922));
#79536=CARTESIAN_POINT('Ctrl Pts',(0.108070786129276,-0.211125672514613,
-0.943630501436753));
#79537=CARTESIAN_POINT('Ctrl Pts',(0.107029901337166,-0.211655249808483,
-0.943710343775937));
#79538=CARTESIAN_POINT('Ctrl Pts',(0.105232379963273,-0.212553134131468,
-0.943846910657466));
#79539=CARTESIAN_POINT('Ctrl Pts',(0.104477627775119,-0.212925137098191,
-0.943903856758308));
#79540=CARTESIAN_POINT('Ctrl Pts',(0.102874038487572,-0.213704935721174,
-0.944023993684628));
#79541=CARTESIAN_POINT('Ctrl Pts',(0.102024734816949,-0.214111701942578,
-0.944087122900321));
#79542=CARTESIAN_POINT('Ctrl Pts',(0.0996784290524052,-0.215218312598164,
-0.944260217331233));
#79543=CARTESIAN_POINT('Ctrl Pts',(0.0981764676106642,-0.215907602646411,
-0.944369564149316));
#79544=CARTESIAN_POINT('Ctrl Pts',(0.0898335827235146,-0.219631309546036,
-0.944969596557978));
#79545=CARTESIAN_POINT('Ctrl Pts',(0.082858509684902,-0.222356640966223,
-0.945444164032441));
#79546=CARTESIAN_POINT('Ctrl Pts',(0.0552310604596983,-0.231670230502304,
-0.947263025850331));
#79547=CARTESIAN_POINT('Ctrl Pts',(0.0338456399187812,-0.235745786048531,
-0.94855226219004));
#79548=CARTESIAN_POINT('Ctrl Pts',(0.00783959537356827,-0.237085672763866,
-0.950217867414755));
#79549=CARTESIAN_POINT('Ctrl Pts',(0.00347047608295848,-0.237189855239467,
-0.950500517005462));
#79550=CARTESIAN_POINT('Ctrl Pts',(-0.00285774619201431,-0.237165873104083,
-0.950915249877816));
#79551=CARTESIAN_POINT('Ctrl Pts',(-0.00481645643009057,-0.237134180253688,
-0.951044355814498));
#79552=CARTESIAN_POINT('Ctrl Pts',(-0.00826284334683571,-0.237035699872771,
-0.951272924836401));
#79553=CARTESIAN_POINT('Ctrl Pts',(-0.00975072168636051,-0.236979156991875,
-0.951372063975333));
#79554=CARTESIAN_POINT('Ctrl Pts',(-0.0128587934093212,-0.236831723239201,
-0.951580168173632));
#79555=CARTESIAN_POINT('Ctrl Pts',(-0.0144787786149538,-0.236738206557033,
-0.951689210127748));
#79556=CARTESIAN_POINT('Ctrl Pts',(-0.0187396364615713,-0.23644834337798,
-0.951977583149281));
#79557=CARTESIAN_POINT('Ctrl Pts',(-0.021378337559641,-0.236224382224938,
-0.952157763953975));
#79558=CARTESIAN_POINT('Ctrl Pts',(-0.0339353077155991,-0.234946492717549,
-0.953023140324025));
#79559=CARTESIAN_POINT('Ctrl Pts',(-0.043783057441229,-0.233311928742815,
-0.953726088025518));
#79560=CARTESIAN_POINT('Ctrl Pts',(-0.0690710093377817,-0.22745704596678,
-0.95559130993288));
#79561=CARTESIAN_POINT('Ctrl Pts',(-0.0842388904726483,-0.222286481649304,
-0.956772467794112));
#79562=CARTESIAN_POINT('Ctrl Pts',(-0.104442294603412,-0.213032158306117,
-0.958371278548418));
#79563=CARTESIAN_POINT('Ctrl Pts',(-0.110009504577016,-0.210211362646114,
-0.95881425889012));
#79564=CARTESIAN_POINT('Ctrl Pts',(-0.116795117537509,-0.206429695407859,
-0.959351832413855));
#79565=CARTESIAN_POINT('Ctrl Pts',(-0.118123570667535,-0.205672411826346,
-0.959456956689106));
#79566=CARTESIAN_POINT('Ctrl Pts',(-0.120234982846617,-0.204441596567279,
-0.959623736123055));
#79567=CARTESIAN_POINT('Ctrl Pts',(-0.121022660571354,-0.203976305503068,
-0.959685886229579));
#79568=CARTESIAN_POINT('Ctrl Pts',(-0.122530572155076,-0.203073753529747,
-0.959804704399139));
#79569=CARTESIAN_POINT('Ctrl Pts',(-0.123251192871967,-0.202637197878695,
-0.959861412627666));
#79570=CARTESIAN_POINT('Ctrl Pts',(-0.124848733371003,-0.201657725100745,
-0.959986995165987));
#79571=CARTESIAN_POINT('Ctrl Pts',(-0.125724479764138,-0.201112902624777,
-0.960055747997172));
#79572=CARTESIAN_POINT('Ctrl Pts',(-0.128310582099416,-0.199480532979008,
-0.960258597617436));
#79573=CARTESIAN_POINT('Ctrl Pts',(-0.130010630686126,-0.198376725143669,
-0.960391712239343));
#79574=CARTESIAN_POINT('Ctrl Pts',(-0.143475385024,-0.18938687182922,-0.961445900195743));
#79575=CARTESIAN_POINT('Ctrl Pts',(-0.154527897562318,-0.18048215593357,
-0.962311666027193));
#79576=CARTESIAN_POINT('Ctrl Pts',(-0.175190280963965,-0.160536895272755,
-0.964072759845347));
#79577=CARTESIAN_POINT('Ctrl Pts',(-0.184706539918831,-0.149489684743957,
-0.964965352191268));
#79578=CARTESIAN_POINT('Ctrl Pts',(-0.195470993990589,-0.134384016733147,
-0.966155228931278));
#79579=CARTESIAN_POINT('Ctrl Pts',(-0.197708951521922,-0.131069221931135,
-0.96641446546335));
#79580=CARTESIAN_POINT('Ctrl Pts',(-0.200881452717741,-0.126103957145347,
-0.966801030348078));
#79581=CARTESIAN_POINT('Ctrl Pts',(-0.201881791469812,-0.12449621673432,
-0.966925934562255));
#79582=CARTESIAN_POINT('Ctrl Pts',(-0.203629931297421,-0.121610133161877,
-0.967149780077638));
#79583=CARTESIAN_POINT('Ctrl Pts',(-0.204385219520994,-0.120336425405647,
-0.967248442196158));
#79584=CARTESIAN_POINT('Ctrl Pts',(-0.205959878806111,-0.117623347575269,
-0.967458376303169));
#79585=CARTESIAN_POINT('Ctrl Pts',(-0.206776195673512,-0.116182306030534,
-0.96756975152088));
#79586=CARTESIAN_POINT('Ctrl Pts',(-0.208934448051046,-0.11227754621146,
-0.96787125820561));
#79587=CARTESIAN_POINT('Ctrl Pts',(-0.210247836318726,-0.109798438590742,
-0.968062384457869));
#79588=CARTESIAN_POINT('Ctrl Pts',(-0.217855327254678,-0.0948015864052863,
-0.969217259501373));
#79589=CARTESIAN_POINT('Ctrl Pts',(-0.223073029847663,-0.0817715463605787,
-0.970217751685048));
#79590=CARTESIAN_POINT('Ctrl Pts',(-0.230143598316615,-0.0582810542876215,
-0.97200118546628));
#79591=CARTESIAN_POINT('Ctrl Pts',(-0.232502932319108,-0.0480119339481906,
-0.97277377070854));
#79592=CARTESIAN_POINT('Ctrl Pts',(-0.234947239019236,-0.0327969245437359,
-0.973887166313279));
#79593=CARTESIAN_POINT('Ctrl Pts',(-0.235572931925849,-0.0279507231698396,
-0.974237128396923));
#79594=CARTESIAN_POINT('Ctrl Pts',(-0.236354030232911,-0.0199650137968235,
-0.974802897139983));
#79595=CARTESIAN_POINT('Ctrl Pts',(-0.236597529332452,-0.0168357009774926,
-0.975021863389482));
#79596=CARTESIAN_POINT('Ctrl Pts',(-0.236848795085307,-0.0124937713187137,
-0.975321082821356));
#79597=CARTESIAN_POINT('Ctrl Pts',(-0.236909480417535,-0.0112846932238761,
-0.97540391192189));
#79598=CARTESIAN_POINT('Ctrl Pts',(-0.236996945547756,-0.00922757519841145,
-0.975543939118901));
#79599=CARTESIAN_POINT('Ctrl Pts',(-0.237028436896408,-0.00837976965484352,
-0.975601389024825));
#79600=CARTESIAN_POINT('Ctrl Pts',(-0.237084692688825,-0.00660917387670398,
-0.975720807168831));
#79601=CARTESIAN_POINT('Ctrl Pts',(-0.237108620234517,-0.00568638460834532,
-0.97578272988657));
#79602=CARTESIAN_POINT('Ctrl Pts',(-0.237158629248897,-0.00319691335545359,
-0.97594899037061));
#79603=CARTESIAN_POINT('Ctrl Pts',(-0.2371745748802,-0.00163004199203212,
-0.976052788121025));
#79604=CARTESIAN_POINT('Ctrl Pts',(-0.237176804291559,0.00675282459052012,
-0.976604136278266));
#79605=CARTESIAN_POINT('Ctrl Pts',(-0.236884803550436,0.0135663447479153,
-0.977038236216962));
#79606=CARTESIAN_POINT('Ctrl Pts',(-0.234531519968222,0.0408807918839849,
-0.978755387496812));
#79607=CARTESIAN_POINT('Ctrl Pts',(-0.230097666489288,0.0610851876736562,
-0.979980872939617));
#79608=CARTESIAN_POINT('Ctrl Pts',(-0.221198374569576,0.0857611609345249,
-0.981642806249572));
#79609=CARTESIAN_POINT('Ctrl Pts',(-0.219099792493792,0.0909888497071163,
-0.982004383795237));
#79610=CARTESIAN_POINT('Ctrl Pts',(-0.215919966670541,0.0981603241674078,
-0.982516638991088));
#79611=CARTESIAN_POINT('Ctrl Pts',(-0.214994387093487,0.10017132434792,
-0.982662104474577));
#79612=CARTESIAN_POINT('Ctrl Pts',(-0.213446575958021,0.103413939031685,
-0.982899780081914));
#79613=CARTESIAN_POINT('Ctrl Pts',(-0.212841494215128,0.104653627640114,
-0.982991397594286));
#79614=CARTESIAN_POINT('Ctrl Pts',(-0.211548598945636,0.107244909669007,
-0.983184525314668));
#79615=CARTESIAN_POINT('Ctrl Pts',(-0.210858569625071,0.108595321249922,
-0.983286109423759));
#79616=CARTESIAN_POINT('Ctrl Pts',(-0.20916926372872,0.111824541026068,
-0.983531340483627));
#79617=CARTESIAN_POINT('Ctrl Pts',(-0.208157573921936,0.113696670007702,
-0.983675418917355));
#79618=CARTESIAN_POINT('Ctrl Pts',(-0.204465647789918,0.120314087666368,
-0.984191681042377));
#79619=CARTESIAN_POINT('Ctrl Pts',(-0.201647396242047,0.124979998622409,
-0.984568713108398));
#79620=CARTESIAN_POINT('Ctrl Pts',(-0.194085521389976,0.136576997967156,
-0.985540091974101));
#79621=CARTESIAN_POINT('Ctrl Pts',(-0.18913014063275,0.143360496846779,
-0.986141210838845));
#79622=CARTESIAN_POINT('Ctrl Pts',(-0.172249803260152,0.164065895495319,
-0.988076706470161));
#79623=CARTESIAN_POINT('Ctrl Pts',(-0.159067255915847,0.17687641688348,
-0.989435959969911));
#79624=CARTESIAN_POINT('Ctrl Pts',(-0.142790248278858,0.189387969247969,
-0.990869878302855));
#79625=CARTESIAN_POINT('Ctrl Pts',(-0.141020501855693,0.190709404138559,
-0.991022827030757));
#79626=CARTESIAN_POINT('Ctrl Pts',(-0.138378553212631,0.192625204109848,
-0.991246526366501));
#79627=CARTESIAN_POINT('Ctrl Pts',(-0.137520486135181,0.193238736404825,
-0.991318473394183));
#79628=CARTESIAN_POINT('Ctrl Pts',(-0.135980017646399,0.194324739071332,
-0.991446339114255));
#79629=CARTESIAN_POINT('Ctrl Pts',(-0.135299199578616,0.194799373896884,
-0.991502399092463));
#79630=CARTESIAN_POINT('Ctrl Pts',(-0.133780130516193,0.195846592271087,
-0.991626483754823));
#79631=CARTESIAN_POINT('Ctrl Pts',(-0.132940682336721,0.196417377285793,
-0.991694389692887));
#79632=CARTESIAN_POINT('Ctrl Pts',(-0.130432651398717,0.198099274696238,
-0.991895389534579));
#79633=CARTESIAN_POINT('Ctrl Pts',(-0.128753570566453,0.199194673382225,
-0.992027496703202));
#79634=CARTESIAN_POINT('Ctrl Pts',(-0.116463658670243,0.206992024070043,
-0.99297830901679));
#79635=CARTESIAN_POINT('Ctrl Pts',(-0.105348180682879,0.212864571647068,
-0.993752479754958));
#79636=CARTESIAN_POINT('Ctrl Pts',(-0.0776842685374338,0.224779332082987,
-0.995601714421009));
#79637=CARTESIAN_POINT('Ctrl Pts',(-0.0608295107684455,0.229913653799764,
-0.996671092514741));
#79638=CARTESIAN_POINT('Ctrl Pts',(-0.0430210306692712,0.233241239222924,
-0.997839698133149));
#79639=CARTESIAN_POINT('Ctrl Pts',(-0.042478593486725,0.233340639033401,
-0.997875324044025));
#79640=CARTESIAN_POINT('Ctrl Pts',(-0.0419358256939468,0.233438144158933,
-0.997911004226539));
#79641=CARTESIAN_POINT('',(-0.237174942067321,-0.00016577202159111,-0.995658989184409));
#79642=CARTESIAN_POINT('Ctrl Pts',(-0.0419358384531397,0.233438141866817,
-1.01783655831731));
#79643=CARTESIAN_POINT('Ctrl Pts',(-0.055592946826114,0.230984719791547,
-1.01698515986923));
#79644=CARTESIAN_POINT('Ctrl Pts',(-0.069012121426973,0.227336927612748,
-1.01612846358432));
#79645=CARTESIAN_POINT('Ctrl Pts',(-0.0849425892911568,0.221464019903327,
-1.01503406101721));
#79646=CARTESIAN_POINT('Ctrl Pts',(-0.0878245833239149,0.220337007194613,
-1.01483293535467));
#79647=CARTESIAN_POINT('Ctrl Pts',(-0.0924381062532635,0.218427980104624,
-1.01450540334796));
#79648=CARTESIAN_POINT('Ctrl Pts',(-0.0941837853024383,0.21768095970503,
-1.01438016221878));
#79649=CARTESIAN_POINT('Ctrl Pts',(-0.0972747531210218,0.216314115171633,
-1.01415596832755));
#79650=CARTESIAN_POINT('Ctrl Pts',(-0.0986235736721244,0.215702490860777,
-1.01405729854005));
#79651=CARTESIAN_POINT('Ctrl Pts',(-0.101464987729986,0.214381825853848,
-1.01384761782651));
#79652=CARTESIAN_POINT('Ctrl Pts',(-0.102956070470368,0.213669741202609,
-1.01373650625723));
#79653=CARTESIAN_POINT('Ctrl Pts',(-0.106943571968904,0.211714032113678,
-1.01343639235263));
#79654=CARTESIAN_POINT('Ctrl Pts',(-0.109425630478381,0.210441890369043,
-1.01324641061616));
#79655=CARTESIAN_POINT('Ctrl Pts',(-0.125199291740754,0.202002830148127,
-1.01201803951623));
#79656=CARTESIAN_POINT('Ctrl Pts',(-0.137800888181475,0.193625336759183,
-1.01093637717332));
#79657=CARTESIAN_POINT('Ctrl Pts',(-0.161823302152502,0.174116199737272,
-1.008682628341));
#79658=CARTESIAN_POINT('Ctrl Pts',(-0.173095748347187,0.162914595846265,
-1.00751457028428));
#79659=CARTESIAN_POINT('Ctrl Pts',(-0.184504154036458,0.149045727716184,
-1.00626183067727));
#79660=CARTESIAN_POINT('Ctrl Pts',(-0.185819788098912,0.147402235121337,
-1.00611618535596));
#79661=CARTESIAN_POINT('Ctrl Pts',(-0.187749257879857,0.144925040901263,
-1.0059010679874));
#79662=CARTESIAN_POINT('Ctrl Pts',(-0.188379760875563,0.144104535348781,
-1.00583052295506));
#79663=CARTESIAN_POINT('Ctrl Pts',(-0.189505883057362,0.142619033322668,
-1.00570410970204));
#79664=CARTESIAN_POINT('Ctrl Pts',(-0.190003402434016,0.141955540567041,
-1.00564811461029));
#79665=CARTESIAN_POINT('Ctrl Pts',(-0.191112958528264,0.140459550157149,
-1.00552290146471));
#79666=CARTESIAN_POINT('Ctrl Pts',(-0.191723045335776,0.139625649988255,
-1.00545381553612));
#79667=CARTESIAN_POINT('Ctrl Pts',(-0.193554890896918,0.13708713667679,
-1.0052455617486));
#79668=CARTESIAN_POINT('Ctrl Pts',(-0.194759545791538,0.135370228984546,
-1.0051074899361));
#79669=CARTESIAN_POINT('Ctrl Pts',(-0.197530986951853,0.131306700051836,
-1.00478658416685));
#79670=CARTESIAN_POINT('Ctrl Pts',(-0.199079014492286,0.128947616244146,
-1.00460477594465));
#79671=CARTESIAN_POINT('Ctrl Pts',(-0.209825244877523,0.111916124700385,
-1.00331965870747));
#79672=CARTESIAN_POINT('Ctrl Pts',(-0.21743493112877,0.096301697396637,
-1.00228138320339));
#79673=CARTESIAN_POINT('Ctrl Pts',(-0.226965413984013,0.0697013506874559,
-1.00053463564309));
#79674=CARTESIAN_POINT('Ctrl Pts',(-0.229937143142169,0.059164555169512,
-0.999848561577447));
#79675=CARTESIAN_POINT('Ctrl Pts',(-0.232728571919164,0.0457911769869978,
-0.998961868290114));
#79676=CARTESIAN_POINT('Ctrl Pts',(-0.233239761376087,0.043111863716989,
-0.998783492065912));
#79677=CARTESIAN_POINT('Ctrl Pts',(-0.23398401988198,0.038809101737257,
-0.998495576213637));
#79678=CARTESIAN_POINT('Ctrl Pts',(-0.234246664096322,0.0371909675907741,
-0.998386972906712));
#79679=CARTESIAN_POINT('Ctrl Pts',(-0.234707754011815,0.0341512909935617,
-0.998182287846869));
#79680=CARTESIAN_POINT('Ctrl Pts',(-0.23491011161308,0.0327304105710576,
-0.99808633438141));
#79681=CARTESIAN_POINT('Ctrl Pts',(-0.235289166899945,0.0298839726597515,
-0.99789352695911));
#79682=CARTESIAN_POINT('Ctrl Pts',(-0.235465834169476,0.0284584726186601,
-0.997796676386154));
#79683=CARTESIAN_POINT('Ctrl Pts',(-0.235840539784608,0.0251922177554452,
-0.99757406024522));
#79684=CARTESIAN_POINT('Ctrl Pts',(-0.236029992892698,0.0233505922664693,
-0.997448032424324));
#79685=CARTESIAN_POINT('Ctrl Pts',(-0.236854354096121,0.0142971437432219,
-0.99682586748679));
#79686=CARTESIAN_POINT('Ctrl Pts',(-0.237180312975127,0.00706187281541956,
-0.996320355240562));
#79687=CARTESIAN_POINT('Ctrl Pts',(-0.237174934520829,-0.000176238589683619,
-0.995806388174485));
#79688=CARTESIAN_POINT('Ctrl Pts',(-0.237174942067321,-0.00016577202159111,
-0.995658989184409));
#79689=CARTESIAN_POINT('Ctrl Pts',(-0.237163585248673,-0.0164143088910714,
-0.99457247635419));
#79690=CARTESIAN_POINT('Ctrl Pts',(-0.23547834423869,-0.0325957541205758,
-0.993485963523971));
#79691=CARTESIAN_POINT('Ctrl Pts',(-0.232184488208474,-0.0483977691672791,
-0.992399450693752));
#79692=CARTESIAN_POINT('Ctrl Pts',(-0.229804709060592,-0.0598145723176513,
-0.99161445567468));
#79693=CARTESIAN_POINT('Ctrl Pts',(-0.226586336671938,-0.071033649634856,
-0.990829460655608));
#79694=CARTESIAN_POINT('Ctrl Pts',(-0.222569518205059,-0.0819438233850974,
-0.990044465636536));
#79695=CARTESIAN_POINT('Ctrl Pts',(-0.217718298757162,-0.0951203329818135,
-0.98909640608781));
#79696=CARTESIAN_POINT('Ctrl Pts',(-0.211676632312198,-0.107908762849582,
-0.988148346539084));
#79697=CARTESIAN_POINT('Ctrl Pts',(-0.204528599500758,-0.120083440204129,
-0.987200286990358));
#79698=CARTESIAN_POINT('Ctrl Pts',(-0.197394987953441,-0.132233554963291,
-0.986254140166086));
#79699=CARTESIAN_POINT('Ctrl Pts',(-0.189159797849578,-0.143771627616582,
-0.985307993341815));
#79700=CARTESIAN_POINT('Ctrl Pts',(-0.179953918574813,-0.154494555938291,
-0.984361846517543));
#79701=CARTESIAN_POINT('Ctrl Pts',(-0.170749497480443,-0.165215785784125,
-0.983415849559754));
#79702=CARTESIAN_POINT('Ctrl Pts',(-0.160575197282862,-0.175121463826213,
-0.982469852601965));
#79703=CARTESIAN_POINT('Ctrl Pts',(-0.149602964644826,-0.184040575945847,
-0.981523855644176));
#79704=CARTESIAN_POINT('Ctrl Pts',(-0.138632511781998,-0.192958241321216,
-0.980578012133911));
#79705=CARTESIAN_POINT('Ctrl Pts',(-0.12686504275345,-0.200889146492325,
-0.979632168623647));
#79706=CARTESIAN_POINT('Ctrl Pts',(-0.114504790606895,-0.207703234334642,
-0.978686325113382));
#79707=CARTESIAN_POINT('Ctrl Pts',(-0.102115785638396,-0.214533173330489,
-0.977738281351074));
#79708=CARTESIAN_POINT('Ctrl Pts',(-0.0891319983572828,-0.220240744143584,
-0.976790237588767));
#79709=CARTESIAN_POINT('Ctrl Pts',(-0.0757809214441986,-0.224742591802418,
-0.975842193826459));
#79710=CARTESIAN_POINT('Ctrl Pts',(-0.0680257844447021,-0.227357545305599,
-0.97529151096349));
#79711=CARTESIAN_POINT('Ctrl Pts',(-0.0601470726480214,-0.229566609646384,
-0.974740828100521));
#79712=CARTESIAN_POINT('Ctrl Pts',(-0.0521911341244206,-0.231361332430047,
-0.974190145237552));
#79713=CARTESIAN_POINT('Ctrl Pts',(-0.0384941335573052,-0.234451139988606,
-0.973242085688825));
#79714=CARTESIAN_POINT('Ctrl Pts',(-0.0244758356660067,-0.236330766586181,
-0.972294026140098));
#79715=CARTESIAN_POINT('Ctrl Pts',(-0.0103713680518171,-0.23694812797263,
-0.971345966591371));
#79716=CARTESIAN_POINT('Ctrl Pts',(0.00370464358600231,-0.23756424382316,
-0.970399819767098));
#79717=CARTESIAN_POINT('Ctrl Pts',(0.0178656583111794,-0.236923042955139,
-0.969453672942825));
#79718=CARTESIAN_POINT('Ctrl Pts',(0.0318700518927368,-0.23502399966249,
-0.968507526118551));
#79719=CARTESIAN_POINT('Ctrl Pts',(0.0458722272253272,-0.233125257171929,
-0.967561529160761));
#79720=CARTESIAN_POINT('Ctrl Pts',(0.0597169990888082,-0.22996913074344,
-0.966615532202972));
#79721=CARTESIAN_POINT('Ctrl Pts',(0.073167361654758,-0.225606998591537,
-0.965669535245182));
#79722=CARTESIAN_POINT('Ctrl Pts',(0.0866155424749664,-0.221245574008906,
-0.964723691734916));
#79723=CARTESIAN_POINT('Ctrl Pts',(0.0996686528945936,-0.215678807214401,
-0.96377784822465));
#79724=CARTESIAN_POINT('Ctrl Pts',(0.112106517191718,-0.20900743869093,
-0.962832004714384));
#79725=CARTESIAN_POINT('Ctrl Pts',(0.124573314854705,-0.202320551012267,
-0.961883960952075));
#79726=CARTESIAN_POINT('Ctrl Pts',(0.136421293702348,-0.194524366434287,
-0.960935917189766));
#79727=CARTESIAN_POINT('Ctrl Pts',(0.14745683687118,-0.18576453344206,-0.959987873427458));
#79728=CARTESIAN_POINT('Ctrl Pts',(0.153866967656463,-0.180676276862538,
-0.959437190564494));
#79729=CARTESIAN_POINT('Ctrl Pts',(0.160003566873437,-0.175263679067963,
-0.95888650770153));
#79730=CARTESIAN_POINT('Ctrl Pts',(0.165834347993985,-0.169561049921289,
-0.958335824838567));
#79731=CARTESIAN_POINT('Ctrl Pts',(0.175872662402621,-0.159743362865875,
-0.957387765289839));
#79732=CARTESIAN_POINT('Ctrl Pts',(0.185069800982204,-0.148998209825383,
-0.956439705741112));
#79733=CARTESIAN_POINT('Ctrl Pts',(0.193254245309879,-0.137494644603742,
-0.955491646192384));
#79734=CARTESIAN_POINT('Ctrl Pts',(0.201422177397549,-0.126014287998623,
-0.954545499368111));
#79735=CARTESIAN_POINT('Ctrl Pts',(0.208580934834249,-0.113779188139508,
-0.953599352543837));
#79736=CARTESIAN_POINT('Ctrl Pts',(0.214598745691559,-0.100991875775281,
-0.952653205719564));
#79737=CARTESIAN_POINT('Ctrl Pts',(0.220615603347815,-0.0882065888784383,
-0.951707208761774));
#79738=CARTESIAN_POINT('Ctrl Pts',(0.225491474053488,-0.074869995353623,
-0.950761211803983));
#79739=CARTESIAN_POINT('Ctrl Pts',(0.229140663662373,-0.0612089607930668,
-0.949815214846193));
#79740=CARTESIAN_POINT('Ctrl Pts',(0.232789261346405,-0.0475501421507673,
-0.948869371335927));
#79741=CARTESIAN_POINT('Ctrl Pts',(0.235211375546206,-0.0335677980348952,
-0.94792352782566));
#79742=CARTESIAN_POINT('Ctrl Pts',(0.236371893925085,-0.0195014970519764,
-0.946977684315394));
#79743=CARTESIAN_POINT('Ctrl Pts',(0.237535111939693,-0.00540247458063008,
-0.946029640553085));
#79744=CARTESIAN_POINT('Ctrl Pts',(0.237430851188402,0.00878005786051047,
-0.945081596790776));
#79745=CARTESIAN_POINT('Ctrl Pts',(0.236076130180546,0.0228044158876671,
-0.944133553028467));
#79746=CARTESIAN_POINT('Ctrl Pts',(0.235289223844806,0.0309506364912213,
-0.943582870165505));
#79747=CARTESIAN_POINT('Ctrl Pts',(0.234081396039,0.0390435480085086,-0.943032187302543));
#79748=CARTESIAN_POINT('Ctrl Pts',(0.232463897269428,0.0470374009837774,
-0.942481504439582));
#79749=CARTESIAN_POINT('Ctrl Pts',(0.229679199838862,0.0607996753417688,
-0.941533444890855));
#79750=CARTESIAN_POINT('Ctrl Pts',(0.225658792039843,0.0743599848162986,
-0.940585385342128));
#79751=CARTESIAN_POINT('Ctrl Pts',(0.220451349750043,0.0874824726352891,
-0.939637325793401));
#79752=CARTESIAN_POINT('Ctrl Pts',(0.215254413553688,0.100578485636974,
-0.938691178969128));
#79753=CARTESIAN_POINT('Ctrl Pts',(0.208875435538092,0.113237637112344,
-0.937745032144855));
#79754=CARTESIAN_POINT('Ctrl Pts',(0.201412795245007,0.125239237208604,
-0.936798885320582));
#79755=CARTESIAN_POINT('Ctrl Pts',(0.193951337009112,0.137238936291666,
-0.935852888362792));
#79756=CARTESIAN_POINT('Ctrl Pts',(0.185406954935095,0.148580557734724,
-0.934906891405002));
#79757=CARTESIAN_POINT('Ctrl Pts',(0.175923499719716,0.159068862042095,
-0.933960894447212));
#79758=CARTESIAN_POINT('Ctrl Pts',(0.166441582789117,0.169555465070921,
-0.933015050936947));
#79759=CARTESIAN_POINT('Ctrl Pts',(0.156021468637956,0.179188419199748,
-0.932069207426681));
#79760=CARTESIAN_POINT('Ctrl Pts',(0.144845163585783,0.187808038195408,
-0.931123363916415));
#79761=CARTESIAN_POINT('Ctrl Pts',(0.133642859848036,0.196447708430093,
-0.930175320154107));
#79762=CARTESIAN_POINT('Ctrl Pts',(0.121681542756846,0.204068862554768,
-0.929227276391798));
#79763=CARTESIAN_POINT('Ctrl Pts',(0.109173329406417,0.210554422350418,
-0.928279232629489));
#79764=CARTESIAN_POINT('Ctrl Pts',(0.101907780059194,0.214321639411681,
-0.927728549766525));
#79765=CARTESIAN_POINT('Ctrl Pts',(0.0944581931614917,0.217706564800712,
-0.927177866903561));
#79766=CARTESIAN_POINT('Ctrl Pts',(0.0868690852762904,0.220693775735204,
-0.926627184040597));
#79767=CARTESIAN_POINT('Ctrl Pts',(0.0738038378845529,0.225836494808489,
-0.925679140087625));
#79768=CARTESIAN_POINT('Ctrl Pts',(0.060236485051065,0.229832236751135,
-0.924731096134653));
#79769=CARTESIAN_POINT('Ctrl Pts',(0.046391447811875,0.232593667572697,
-0.923783052181681));
#79770=CARTESIAN_POINT('Ctrl Pts',(0.0319084307160987,0.235482345234341,
-0.922791322326338));
#79771=CARTESIAN_POINT('Ctrl Pts',(0.0171223396133438,0.237019582137728,
-0.921799592470995));
#79772=CARTESIAN_POINT('Ctrl Pts',(0.00230831192544603,0.237163766880725,
-0.920807862615652));
#79773=CARTESIAN_POINT('Ctrl Pts',(-0.0125057157624517,0.237307951623722,
-0.919816132760309));
#79774=CARTESIAN_POINT('Ctrl Pts',(-0.0273466268406475,0.236059010181803,
-0.918824402904966));
#79775=CARTESIAN_POINT('Ctrl Pts',(-0.0419358257166344,0.233438144154858,
-0.917832673049623));
#79776=CARTESIAN_POINT('Origin',(0.,0.,-1.7456589891905));
#79777=CARTESIAN_POINT('',(-0.0419357988072456,0.233438148988974,-0.798166224572097));
#79778=CARTESIAN_POINT('',(-0.0419725940269791,0.233652521193877,-0.817841625530981));
#79779=CARTESIAN_POINT('',(-0.0419358257166344,0.233438144154858,-1.7456589891905));
#79780=CARTESIAN_POINT('',(-0.237174902566701,0.000214982501742253,-0.87588669733343));
#79781=CARTESIAN_POINT('Ctrl Pts',(-0.0419357988072473,0.233438148988973,
-0.798166224572096));
#79782=CARTESIAN_POINT('Ctrl Pts',(-0.0313505303885184,0.235339730579862,
-0.798950663251301));
#79783=CARTESIAN_POINT('Ctrl Pts',(-0.0206424454919457,0.236520164301066,
-0.799731423587888));
#79784=CARTESIAN_POINT('Ctrl Pts',(-0.00773759091582227,0.237058496772595,
-0.800632917265799));
#79785=CARTESIAN_POINT('Ctrl Pts',(-0.00558869131939521,0.237118891153116,
-0.800781705334997));
#79786=CARTESIAN_POINT('Ctrl Pts',(-0.00239573691432892,0.237165195726478,
-0.801000528277506));
#79787=CARTESIAN_POINT('Ctrl Pts',(-0.00135218428014268,0.237173441431424,
-0.801071688460254));
#79788=CARTESIAN_POINT('Ctrl Pts',(0.000521048498413145,0.237175878683289,
-0.801198742591875));
#79789=CARTESIAN_POINT('Ctrl Pts',(0.00135067642484936,0.23717260518958,
-0.801254769673511));
#79790=CARTESIAN_POINT('Ctrl Pts',(0.00320559434414651,0.237155552499976,
-0.801379495737443));
#79791=CARTESIAN_POINT('Ctrl Pts',(0.00423082805610003,0.237139478173074,
-0.801448068472577));
#79792=CARTESIAN_POINT('Ctrl Pts',(0.00731158285574852,0.237071189915555,
-0.801653115216069));
#79793=CARTESIAN_POINT('Ctrl Pts',(0.00936662263562405,0.236998893271651,
-0.801788542367449));
#79794=CARTESIAN_POINT('Ctrl Pts',(0.0141660993478863,0.236767518537997,
-0.802102213752993));
#79795=CARTESIAN_POINT('Ctrl Pts',(0.0169092692564717,0.236587434541174,
-0.802279494950369));
#79796=CARTESIAN_POINT('Ctrl Pts',(0.0267707555675258,0.235767639680444,
-0.802911582093368));
#79797=CARTESIAN_POINT('Ctrl Pts',(0.0338628208650324,0.234853948012336,
-0.803356400021272));
#79798=CARTESIAN_POINT('Ctrl Pts',(0.0578518690443821,0.230653861070634,
-0.804858891986051));
#79799=CARTESIAN_POINT('Ctrl Pts',(0.0744262271455292,0.225851175732788,
-0.805897325575825));
#79800=CARTESIAN_POINT('Ctrl Pts',(0.0951789250522059,0.217302547967147,
-0.807323036174596));
#79801=CARTESIAN_POINT('Ctrl Pts',(0.0999550525873154,0.215147405769776,
-0.807660058752244));
#79802=CARTESIAN_POINT('Ctrl Pts',(0.106587427359322,0.211886136863276,
-0.808143063357768));
#79803=CARTESIAN_POINT('Ctrl Pts',(0.108506124442552,0.210910016648227,
-0.808284610420606));
#79804=CARTESIAN_POINT('Ctrl Pts',(0.111743984749855,0.209206907655467,
-0.808526725806087));
#79805=CARTESIAN_POINT('Ctrl Pts',(0.113070017559556,0.208493211616066,
-0.808626824018616));
#79806=CARTESIAN_POINT('Ctrl Pts',(0.115750026286485,0.207017693544718,
-0.808831101478219));
#79807=CARTESIAN_POINT('Ctrl Pts',(0.117103490873556,0.206255099943955,
-0.808935304531674));
#79808=CARTESIAN_POINT('Ctrl Pts',(0.120458173629493,0.204321279883737,
-0.809196236131926));
#79809=CARTESIAN_POINT('Ctrl Pts',(0.122449854276526,0.203133920190778,
-0.809353539219415));
#79810=CARTESIAN_POINT('Ctrl Pts',(0.130349808864888,0.198265884837244,
-0.809987319821));
#79811=CARTESIAN_POINT('Ctrl Pts',(0.136111661532759,0.194355427874229,
-0.810472073058823));
#79812=CARTESIAN_POINT('Ctrl Pts',(0.151725078004736,0.182723798572182,
-0.811850733306218));
#79813=CARTESIAN_POINT('Ctrl Pts',(0.161149405734649,0.17446861236761,-0.81276156678856));
#79814=CARTESIAN_POINT('Ctrl Pts',(0.178334889008115,0.156829572738885,
-0.814559265563252));
#79815=CARTESIAN_POINT('Ctrl Pts',(0.186114967456051,0.147513121454618,
-0.81544313942304));
#79816=CARTESIAN_POINT('Ctrl Pts',(0.194480916801083,0.13577340810298,-0.816451003309508));
#79817=CARTESIAN_POINT('Ctrl Pts',(0.195785380974853,0.133885514207047,
-0.816610034666844));
#79818=CARTESIAN_POINT('Ctrl Pts',(0.197658237439339,0.131089086919469,
-0.816840836304333));
#79819=CARTESIAN_POINT('Ctrl Pts',(0.198248155764343,0.130195224122643,
-0.816913910393796));
#79820=CARTESIAN_POINT('Ctrl Pts',(0.1992848767388,0.12860096655052,-0.817042961276389));
#79821=CARTESIAN_POINT('Ctrl Pts',(0.199734078162534,0.127902184438335,
-0.817099090955306));
#79822=CARTESIAN_POINT('Ctrl Pts',(0.200716795547122,0.126355656022187,
-0.817222357081028));
#79823=CARTESIAN_POINT('Ctrl Pts',(0.201248621552795,0.125506877253641,
-0.817289384784154));
#79824=CARTESIAN_POINT('Ctrl Pts',(0.202793535346434,0.123006169340596,
-0.817485118898756));
#79825=CARTESIAN_POINT('Ctrl Pts',(0.203791802079835,0.121345118035626,
-0.817612914212986));
#79826=CARTESIAN_POINT('Ctrl Pts',(0.206053099904848,0.117475831025437,
-0.817905962876084));
#79827=CARTESIAN_POINT('Ctrl Pts',(0.20730120577119,0.115259108322226,-0.818070419497504));
#79828=CARTESIAN_POINT('Ctrl Pts',(0.211521920149926,0.107472387532533,
-0.818637790437155));
#79829=CARTESIAN_POINT('Ctrl Pts',(0.214307785370698,0.101803834609038,
-0.819032767262254));
#79830=CARTESIAN_POINT('Ctrl Pts',(0.225594897074708,0.0763143162073501,
-0.820759022301788));
#79831=CARTESIAN_POINT('Ctrl Pts',(0.231595545126583,0.0555014073332016,
-0.822049855728221));
#79832=CARTESIAN_POINT('Ctrl Pts',(0.235122646530788,0.0312709182436343,
-0.823630897655418));
#79833=CARTESIAN_POINT('Ctrl Pts',(0.235490257000925,0.0283701761924342,
-0.823821193578872));
#79834=CARTESIAN_POINT('Ctrl Pts',(0.23600271011883,0.0236246121801196,
-0.824134573250991));
#79835=CARTESIAN_POINT('Ctrl Pts',(0.236179759789948,0.0217835310958926,
-0.824256654046997));
#79836=CARTESIAN_POINT('Ctrl Pts',(0.236459398030211,0.0184692706802739,
-0.824477411771021));
#79837=CARTESIAN_POINT('Ctrl Pts',(0.236569795975551,0.0169968332302047,
-0.824575839407845));
#79838=CARTESIAN_POINT('Ctrl Pts',(0.236776632342303,0.0138434682858655,
-0.824787426670993));
#79839=CARTESIAN_POINT('Ctrl Pts',(0.236868934157923,0.0121623605964905,
-0.824900709980918));
#79840=CARTESIAN_POINT('Ctrl Pts',(0.237073024718818,0.00754825537854731,
-0.825213028893489));
#79841=CARTESIAN_POINT('Ctrl Pts',(0.237148275612999,0.00461402659129783,
-0.825413185681062));
#79842=CARTESIAN_POINT('Ctrl Pts',(0.23727814123191,-0.0137273667745005,
-0.826674517661553));
#79843=CARTESIAN_POINT('Ctrl Pts',(0.235885745392215,-0.0291052450653689,
-0.827780535774551));
#79844=CARTESIAN_POINT('Ctrl Pts',(0.230180700180887,-0.059155944858936,
-0.830009825768871));
#79845=CARTESIAN_POINT('Ctrl Pts',(0.225921901876457,-0.0737695390719033,
-0.831126936641177));
#79846=CARTESIAN_POINT('Ctrl Pts',(0.219493212181919,-0.0898854205187167,
-0.832338150587589));
#79847=CARTESIAN_POINT('Ctrl Pts',(0.218664327372071,-0.0918834684372917,
-0.832487885336042));
#79848=CARTESIAN_POINT('Ctrl Pts',(0.217394148488585,-0.0948306870701711,
-0.832707819121343));
#79849=CARTESIAN_POINT('Ctrl Pts',(0.216973746867276,-0.0957886646831998,
-0.832779159479583));
#79850=CARTESIAN_POINT('Ctrl Pts',(0.216208581340307,-0.0975013761813056,
-0.832906398213576));
#79851=CARTESIAN_POINT('Ctrl Pts',(0.215866182390205,-0.0982571135452776,
-0.832962431593476));
#79852=CARTESIAN_POINT('Ctrl Pts',(0.21509278039432,-0.0999405963812236,
-0.833087005315389));
#79853=CARTESIAN_POINT('Ctrl Pts',(0.214659734911456,-0.100867364828591,
-0.833155421168655));
#79854=CARTESIAN_POINT('Ctrl Pts',(0.213343465269904,-0.103637465355318,
-0.833359511830507));
#79855=CARTESIAN_POINT('Ctrl Pts',(0.212442369088613,-0.105472266036051,
-0.833494154143036));
#79856=CARTESIAN_POINT('Ctrl Pts',(0.20522117803054,-0.119707835901997,
-0.834536346054862));
#79857=CARTESIAN_POINT('Ctrl Pts',(0.197843421773374,-0.131543849740473,
-0.835389216138793));
#79858=CARTESIAN_POINT('Ctrl Pts',(0.179850938551566,-0.155439020156128,
-0.837223677738599));
#79859=CARTESIAN_POINT('Ctrl Pts',(0.168966982884659,-0.16720566685208,
-0.83820260917595));
#79860=CARTESIAN_POINT('Ctrl Pts',(0.154657817767472,-0.179840373342346,
-0.839432955434803));
#79861=CARTESIAN_POINT('Ctrl Pts',(0.152292897754663,-0.18184738753357,
-0.839634540738782));
#79862=CARTESIAN_POINT('Ctrl Pts',(0.148416025697946,-0.185008860028065,
-0.839962691842541));
#79863=CARTESIAN_POINT('Ctrl Pts',(0.146928309207657,-0.186192552420041,
-0.840088085510707));
#79864=CARTESIAN_POINT('Ctrl Pts',(0.144256117361922,-0.188266695189936,
-0.840312474077857));
#79865=CARTESIAN_POINT('Ctrl Pts',(0.143077211867114,-0.189164180510896,
-0.840411184602881));
#79866=CARTESIAN_POINT('Ctrl Pts',(0.14056633942817,-0.191038774898792,
-0.840620870140371));
#79867=CARTESIAN_POINT('Ctrl Pts',(0.139232423437442,-0.192013127988283,
-0.840731945086161));
#79868=CARTESIAN_POINT('Ctrl Pts',(0.135622406275613,-0.194592652480213,
-0.841031757625378));
#79869=CARTESIAN_POINT('Ctrl Pts',(0.133328088124021,-0.196171754474485,
-0.841221470777826));
#79870=CARTESIAN_POINT('Ctrl Pts',(0.118615927055236,-0.205920323341553,
-0.842433284075799));
#79871=CARTESIAN_POINT('Ctrl Pts',(0.105483112612292,-0.212946206355859,
-0.843497207005598));
#79872=CARTESIAN_POINT('Ctrl Pts',(0.0768930563187806,-0.224944776934417,
-0.845754454897625));
#79873=CARTESIAN_POINT('Ctrl Pts',(0.0614043772829213,-0.2296568510206,
-0.846945182757649));
#79874=CARTESIAN_POINT('Ctrl Pts',(0.0435224776969564,-0.233156747777846,
-0.848215756403463));
#79875=CARTESIAN_POINT('Ctrl Pts',(0.0414835367088001,-0.233528139651552,
-0.848359092360264));
#79876=CARTESIAN_POINT('Ctrl Pts',(0.038425713185093,-0.234043805790342,
-0.848571502632581));
#79877=CARTESIAN_POINT('Ctrl Pts',(0.0374103952715134,-0.234208242569475,
-0.848641611970352));
#79878=CARTESIAN_POINT('Ctrl Pts',(0.0355742498664127,-0.234493372173651,
-0.848767605397444));
#79879=CARTESIAN_POINT('Ctrl Pts',(0.0347538321768465,-0.234616367818152,
-0.848823611645411));
#79880=CARTESIAN_POINT('Ctrl Pts',(0.0329032437455452,-0.234883884493721,
-0.848949296615929));
#79881=CARTESIAN_POINT('Ctrl Pts',(0.0318727513889932,-0.235025935726976,
-0.849018838306567));
#79882=CARTESIAN_POINT('Ctrl Pts',(0.0287272171535784,-0.235438471760219,
-0.849229846032715));
#79883=CARTESIAN_POINT('Ctrl Pts',(0.0266093672971932,-0.235687227777629,
-0.849370173467309));
#79884=CARTESIAN_POINT('Ctrl Pts',(0.0126418887242216,-0.237137121539453,
-0.85028590792747));
#79885=CARTESIAN_POINT('Ctrl Pts',(0.000718042601137179,-0.237472919934315,
-0.851022069231414));
#79886=CARTESIAN_POINT('Ctrl Pts',(-0.0292519667418776,-0.236058382514719,
-0.852865126087821));
#79887=CARTESIAN_POINT('Ctrl Pts',(-0.0471631501467768,-0.233141155909607,
-0.853964325181293));
#79888=CARTESIAN_POINT('Ctrl Pts',(-0.0674324281551723,-0.227406484930319,
-0.855323736490781));
#79889=CARTESIAN_POINT('Ctrl Pts',(-0.0702811419881151,-0.226542273257707,
-0.855517397569422));
#79890=CARTESIAN_POINT('Ctrl Pts',(-0.0748869501440595,-0.225049780471825,
-0.855835185707767));
#79891=CARTESIAN_POINT('Ctrl Pts',(-0.0766542751552424,-0.224453961342068,
-0.855958260632406));
#79892=CARTESIAN_POINT('Ctrl Pts',(-0.0798091627026552,-0.223348746221201,
-0.856180096272979));
#79893=CARTESIAN_POINT('Ctrl Pts',(-0.0811993514392261,-0.222847100153498,
-0.856278597178528));
#79894=CARTESIAN_POINT('Ctrl Pts',(-0.0841534494289636,-0.22174980940939,
-0.856489556940586));
#79895=CARTESIAN_POINT('Ctrl Pts',(-0.0857159174386802,-0.221150542104236,
-0.856602131977871));
#79896=CARTESIAN_POINT('Ctrl Pts',(-0.0899561287354448,-0.219472570186539,
-0.856910426842706));
#79897=CARTESIAN_POINT('Ctrl Pts',(-0.0926206529295792,-0.218361460738713,
-0.857107220059606));
#79898=CARTESIAN_POINT('Ctrl Pts',(-0.098503298920414,-0.215781350585711,
-0.857548741898548));
#79899=CARTESIAN_POINT('Ctrl Pts',(-0.101710121856105,-0.214288450483594,
-0.857794226949027));
#79900=CARTESIAN_POINT('Ctrl Pts',(-0.111882859661351,-0.209272857421391,
-0.858588615694429));
#79901=CARTESIAN_POINT('Ctrl Pts',(-0.118708218240034,-0.205478082047925,
-0.859145841925031));
#79902=CARTESIAN_POINT('Ctrl Pts',(-0.138078098720645,-0.1934212305751,
-0.860794735045849));
#79903=CARTESIAN_POINT('Ctrl Pts',(-0.150040295602851,-0.184296591813715,
-0.861903131385808));
#79904=CARTESIAN_POINT('Ctrl Pts',(-0.165036758918983,-0.17042359398197,
-0.863367505551587));
#79905=CARTESIAN_POINT('Ctrl Pts',(-0.168886921020689,-0.166608976985486,
-0.863750910674673));
#79906=CARTESIAN_POINT('Ctrl Pts',(-0.173642117154723,-0.16156326864552,
-0.864230594587012));
#79907=CARTESIAN_POINT('Ctrl Pts',(-0.1746703484961,-0.160451065064583,
-0.864334705246915));
#79908=CARTESIAN_POINT('Ctrl Pts',(-0.176300314283349,-0.158653745351712,
-0.86450026108293));
#79909=CARTESIAN_POINT('Ctrl Pts',(-0.176908855424301,-0.157974898872121,
-0.864562189082302));
#79910=CARTESIAN_POINT('Ctrl Pts',(-0.17807980834442,-0.156653412680118,
-0.864681552493512));
#79911=CARTESIAN_POINT('Ctrl Pts',(-0.178642683408639,-0.156011222462758,
-0.864739019284844));
#79912=CARTESIAN_POINT('Ctrl Pts',(-0.180015346096379,-0.154427967317936,
-0.864879418477489));
#79913=CARTESIAN_POINT('Ctrl Pts',(-0.180821251566946,-0.153483540060386,
-0.864962072178599));
#79914=CARTESIAN_POINT('Ctrl Pts',(-0.183675999509331,-0.150084411941833,
-0.865255846228854));
#79915=CARTESIAN_POINT('Ctrl Pts',(-0.18568267523755,-0.147594546041182,
-0.865464203683312));
#79916=CARTESIAN_POINT('Ctrl Pts',(-0.193190259396895,-0.137883626336553,
-0.866254381989254));
#79917=CARTESIAN_POINT('Ctrl Pts',(-0.198325726549276,-0.130389060151497,
-0.866817997511125));
#79918=CARTESIAN_POINT('Ctrl Pts',(-0.209883835834251,-0.111252222847797,
-0.868194353797005));
#79919=CARTESIAN_POINT('Ctrl Pts',(-0.215781610133051,-0.099330592018818,
-0.869000276477057));
#79920=CARTESIAN_POINT('Ctrl Pts',(-0.2234437995909,-0.0798927662217952,
-0.870309197419156));
#79921=CARTESIAN_POINT('Ctrl Pts',(-0.225893669858742,-0.0726774928777872,
-0.870793708034588));
#79922=CARTESIAN_POINT('Ctrl Pts',(-0.228668639172929,-0.06299731507165,
-0.871449296863225));
#79923=CARTESIAN_POINT('Ctrl Pts',(-0.229308479676761,-0.0606269631479993,
-0.871610239816516));
#79924=CARTESIAN_POINT('Ctrl Pts',(-0.230299849166122,-0.0567138612169758,
-0.871876818091302));
#79925=CARTESIAN_POINT('Ctrl Pts',(-0.230672951872816,-0.0551767310511085,
-0.871981756396661));
#79926=CARTESIAN_POINT('Ctrl Pts',(-0.231371085821785,-0.0521696035377968,
-0.872187537240103));
#79927=CARTESIAN_POINT('Ctrl Pts',(-0.231697551301291,-0.0507000140896716,
-0.872288328384588));
#79928=CARTESIAN_POINT('Ctrl Pts',(-0.232318588727858,-0.0477730514545132,
-0.87248956036089));
#79929=CARTESIAN_POINT('Ctrl Pts',(-0.232613490476748,-0.0463158178941775,
-0.872589985581281));
#79930=CARTESIAN_POINT('Ctrl Pts',(-0.233272741333017,-0.0428929485776275,
-0.872826467599483));
#79931=CARTESIAN_POINT('Ctrl Pts',(-0.233625972873291,-0.0409253132170732,
-0.872962867722792));
#79932=CARTESIAN_POINT('Ctrl Pts',(-0.234678820381688,-0.0346019227963592,
-0.873402768668219));
#79933=CARTESIAN_POINT('Ctrl Pts',(-0.235281766051343,-0.0302312419375767,
-0.873709196959671));
#79934=CARTESIAN_POINT('Ctrl Pts',(-0.236711368924702,-0.0171909327698615,
-0.874630663518059));
#79935=CARTESIAN_POINT('Ctrl Pts',(-0.237182793595308,-0.008490628075348,
-0.875255150768821));
#79936=CARTESIAN_POINT('Ctrl Pts',(-0.237174902566701,0.000214982501742253,
-0.87588669733343));
#79937=CARTESIAN_POINT('Ctrl Pts',(-0.23717490269649,0.000214839266908004,
-0.875886686942491));
#79938=CARTESIAN_POINT('Ctrl Pts',(-0.237160436115023,0.0161854302161968,
-0.877045269750223));
#79939=CARTESIAN_POINT('Ctrl Pts',(-0.235532942994856,0.0321144320544727,
-0.878225659313285));
#79940=CARTESIAN_POINT('Ctrl Pts',(-0.231758761892673,0.0504730591886212,
-0.879551285230372));
#79941=CARTESIAN_POINT('Ctrl Pts',(-0.231153454613579,0.0531764548900551,
-0.879745483075348));
#79942=CARTESIAN_POINT('Ctrl Pts',(-0.230220788146122,0.0570244099532458,
-0.880019889551011));
#79943=CARTESIAN_POINT('Ctrl Pts',(-0.229931986411869,0.0581779716961225,
-0.880101892122108));
#79944=CARTESIAN_POINT('Ctrl Pts',(-0.229366075977925,0.060368330891023,
-0.880257038402641));
#79945=CARTESIAN_POINT('Ctrl Pts',(-0.229090583242611,0.061405512501592,
-0.880330263927035));
#79946=CARTESIAN_POINT('Ctrl Pts',(-0.228610189196349,0.0631658679588368,
-0.8804540964853));
#79947=CARTESIAN_POINT('Ctrl Pts',(-0.228408878006416,0.0638899834536621,
-0.880504903069019));
#79948=CARTESIAN_POINT('Ctrl Pts',(-0.227941147699356,0.0655419376381564,
-0.88062050309687));
#79949=CARTESIAN_POINT('Ctrl Pts',(-0.227672502856321,0.0664691201189385,
-0.880685168021568));
#79950=CARTESIAN_POINT('Ctrl Pts',(-0.226910778673012,0.0690392750089375,
-0.88086388221992));
#79951=CARTESIAN_POINT('Ctrl Pts',(-0.226405513889538,0.070678615366744,
-0.880977260760265));
#79952=CARTESIAN_POINT('Ctrl Pts',(-0.222747210813616,0.0821060711419424,
-0.88176424633515));
#79953=CARTESIAN_POINT('Ctrl Pts',(-0.218977887177857,0.0916867770309371,
-0.882407013997007));
#79954=CARTESIAN_POINT('Ctrl Pts',(-0.209255150934324,0.112346310699076,
-0.883816233200857));
#79955=CARTESIAN_POINT('Ctrl Pts',(-0.203019981926796,0.123257038955161,
-0.884577205928329));
#79956=CARTESIAN_POINT('Ctrl Pts',(-0.192492860221365,0.138694465400979,
-0.885739931034289));
#79957=CARTESIAN_POINT('Ctrl Pts',(-0.188839378594836,0.1436291651109,-0.886125945113413));
#79958=CARTESIAN_POINT('Ctrl Pts',(-0.182279144853885,0.151806399116678,
-0.886796443276678));
#79959=CARTESIAN_POINT('Ctrl Pts',(-0.179466960670738,0.155120842253829,
-0.887077525421505));
#79960=CARTESIAN_POINT('Ctrl Pts',(-0.175461992822456,0.159586343550733,
-0.887470553022884));
#79961=CARTESIAN_POINT('Ctrl Pts',(-0.174345733097042,0.160805090391318,
-0.887579355544892));
#79962=CARTESIAN_POINT('Ctrl Pts',(-0.173169647989306,0.162062513911321,
-0.88769326396694));
#79963=CARTESIAN_POINT('Ctrl Pts',(-0.173122423481623,0.16211296027101,
-0.887697836639924));
#79964=CARTESIAN_POINT('Ctrl Pts',(-0.173027224790476,0.162214564774533,
-0.887707052154992));
#79965=CARTESIAN_POINT('Ctrl Pts',(-0.172979249949819,0.162265722290524,
-0.887711695024554));
#79966=CARTESIAN_POINT('Ctrl Pts',(-0.172915833791056,0.162333285425153,
-0.88771783063105));
#79967=CARTESIAN_POINT('Ctrl Pts',(-0.172900412777663,0.16234971017496,
-0.887719322509477));
#79968=CARTESIAN_POINT('Ctrl Pts',(-0.172867231935001,0.162385040631729,
-0.887722532257328));
#79969=CARTESIAN_POINT('Ctrl Pts',(-0.172849471345733,0.162403945621211,
-0.887724250158876));
#79970=CARTESIAN_POINT('Ctrl Pts',(-0.17281112655442,0.162444747736535,
-0.88772795871381));
#79971=CARTESIAN_POINT('Ctrl Pts',(-0.172790541292811,0.162466643862455,
-0.887729949412034));
#79972=CARTESIAN_POINT('Ctrl Pts',(-0.172745919821677,0.162514088744458,
-0.887734264043252));
#79973=CARTESIAN_POINT('Ctrl Pts',(-0.172721882107559,0.162539636079017,
-0.887736588039945));
#79974=CARTESIAN_POINT('Ctrl Pts',(-0.17266952791604,0.162595253498637,
-0.8877416490409));
#79975=CARTESIAN_POINT('Ctrl Pts',(-0.172641209253794,0.162625321516726,
-0.887744386137709));
#79976=CARTESIAN_POINT('Ctrl Pts',(-0.172579175490758,0.162691152886866,
-0.887750380984973));
#79977=CARTESIAN_POINT('Ctrl Pts',(-0.172545457131033,0.16272691315257,
-0.887753638873601));
#79978=CARTESIAN_POINT('Ctrl Pts',(-0.172471073335732,0.162805752345842,
-0.88776082455701));
#79979=CARTESIAN_POINT('Ctrl Pts',(-0.172430402880675,0.162848826513648,
-0.887764752564831));
#79980=CARTESIAN_POINT('Ctrl Pts',(-0.172339891753788,0.162944615124906,
-0.887773492316094));
#79981=CARTESIAN_POINT('Ctrl Pts',(-0.172290043041345,0.162997321931075,
-0.887778304401207));
#79982=CARTESIAN_POINT('Ctrl Pts',(-0.172177856387801,0.1631158318827,-0.887789131276454));
#79983=CARTESIAN_POINT('Ctrl Pts',(-0.17211550491725,0.163181622151898,
-0.887795146642349));
#79984=CARTESIAN_POINT('Ctrl Pts',(-0.171973096879435,0.163331711832582,
-0.887808880855109));
#79985=CARTESIAN_POINT('Ctrl Pts',(-0.171893016062611,0.163415988107903,
-0.887816600735816));
#79986=CARTESIAN_POINT('Ctrl Pts',(-0.171691709049339,0.163627529960834,
-0.887835998633214));
#79987=CARTESIAN_POINT('Ctrl Pts',(-0.171570403445524,0.163754719561374,
-0.887847680043757));
#79988=CARTESIAN_POINT('Ctrl Pts',(-0.170430437871161,0.16494732264286,
-0.88795738511415));
#79989=CARTESIAN_POINT('Ctrl Pts',(-0.169402027773762,0.166003331948233,
-0.888055826389046));
#79990=CARTESIAN_POINT('Ctrl Pts',(-0.167086899056528,0.168336673984274,
-0.888276312912292));
#79991=CARTESIAN_POINT('Ctrl Pts',(-0.165795254012181,0.169608965195928,
-0.888398571983746));
#79992=CARTESIAN_POINT('Ctrl Pts',(-0.16247198856065,0.172808198930739,
-0.88871131093992));
#79993=CARTESIAN_POINT('Ctrl Pts',(-0.160420645423922,0.174714155248683,
-0.888902668918628));
#79994=CARTESIAN_POINT('Ctrl Pts',(-0.143707484802519,0.189700267806334,
-0.890449001653943));
#79995=CARTESIAN_POINT('Ctrl Pts',(-0.127508080645291,0.200946322777468,
-0.891880272615361));
#79996=CARTESIAN_POINT('Ctrl Pts',(-0.103218165637264,0.213678689250855,
-0.893880426729042));
#79997=CARTESIAN_POINT('Ctrl Pts',(-0.0961497172639372,0.216951188626471,
-0.894445892296079));
#79998=CARTESIAN_POINT('Ctrl Pts',(-0.0849671138441651,0.221474308544954,
-0.895304106626987));
#79999=CARTESIAN_POINT('Ctrl Pts',(-0.0809585001955723,0.22297086462913,
-0.895604766087735));
#80000=CARTESIAN_POINT('Ctrl Pts',(-0.0756286173282596,0.224797979357973,
-0.895993513610001));
#80001=CARTESIAN_POINT('Ctrl Pts',(-0.0743421361698405,0.225226699771743,
-0.896086513230532));
#80002=CARTESIAN_POINT('Ctrl Pts',(-0.0722175744162482,0.225914523293802,
-0.896238649657227));
#80003=CARTESIAN_POINT('Ctrl Pts',(-0.0713816274285868,0.226180046028471,
-0.89629814365353));
#80004=CARTESIAN_POINT('Ctrl Pts',(-0.0698038938496573,0.226671564795226,
-0.896409715166161));
#80005=CARTESIAN_POINT('Ctrl Pts',(-0.0690624387684199,0.226898570904394,
-0.896461852163554));
#80006=CARTESIAN_POINT('Ctrl Pts',(-0.0672955731796037,0.227430056446354,
-0.896585419587905));
#80007=CARTESIAN_POINT('Ctrl Pts',(-0.0662691794182706,0.22773124667358,
-0.89665666363972));
#80008=CARTESIAN_POINT('Ctrl Pts',(-0.0626045639227825,0.228779736020652,
-0.89690923629057));
#80009=CARTESIAN_POINT('Ctrl Pts',(-0.0599553495863132,0.229488249487896,
-0.897088521173322));
#80010=CARTESIAN_POINT('Ctrl Pts',(-0.0522100329691301,0.231416388623629,
-0.897604712859081));
#80011=CARTESIAN_POINT('Ctrl Pts',(-0.0470876893284127,0.232512641753263,
-0.897936157593881));
#80012=CARTESIAN_POINT('Ctrl Pts',(-0.0419358085112875,0.233438147245699,
-0.898263402204347));
#80013=CARTESIAN_POINT('',(-0.237254449915977,-6.65203262155088E-5,-0.895658993950963));
#80014=CARTESIAN_POINT('Ctrl Pts',(-0.0419358257166344,0.233438144154858,
-0.917832673049623));
#80015=CARTESIAN_POINT('Ctrl Pts',(-0.0558504293696778,0.230938465296363,
-0.916886800148356));
#80016=CARTESIAN_POINT('Ctrl Pts',(-0.0695352643872399,0.227191402517845,
-0.915940927247089));
#80017=CARTESIAN_POINT('Ctrl Pts',(-0.0827588563410773,0.222267749172292,
-0.914995054345823));
#80018=CARTESIAN_POINT('Ctrl Pts',(-0.0960128478354698,0.217332776905218,
-0.91404700698986));
#80019=CARTESIAN_POINT('Ctrl Pts',(-0.108802715093054,0.211216154142449,
-0.913098959633897));
#80020=CARTESIAN_POINT('Ctrl Pts',(-0.120917503389532,0.204036609457819,
-0.912150912277934));
#80021=CARTESIAN_POINT('Ctrl Pts',(-0.126787381578739,0.20055796404352,
-0.911691562732493));
#80022=CARTESIAN_POINT('Ctrl Pts',(-0.132499180445869,0.196830462375787,
-0.911232213187052));
#80023=CARTESIAN_POINT('Ctrl Pts',(-0.138031530126742,0.192871141739428,
-0.910772863641611));
#80024=CARTESIAN_POINT('Ctrl Pts',(-0.149367873262532,0.184758093955488,
-0.909831610039296));
#80025=CARTESIAN_POINT('Ctrl Pts',(-0.160027179815794,0.175612883814287,
-0.908890356436981));
#80026=CARTESIAN_POINT('Ctrl Pts',(-0.169815694091736,0.165573580818746,
-0.907949102834666));
#80027=CARTESIAN_POINT('Ctrl Pts',(-0.17958447881759,0.155554512858444,
-0.907009746405872));
#80028=CARTESIAN_POINT('Ctrl Pts',(-0.188485316369692,0.144645477147395,
-0.906070389977077));
#80029=CARTESIAN_POINT('Ctrl Pts',(-0.196358430816218,0.133023859786102,
-0.905131033548283));
#80030=CARTESIAN_POINT('Ctrl Pts',(-0.204230121710632,0.121404343750536,
-0.90419184696623));
#80031=CARTESIAN_POINT('Ctrl Pts',(-0.211073945122252,0.109073175716272,
-0.903252660384176));
#80032=CARTESIAN_POINT('Ctrl Pts',(-0.216771925601164,0.0962388325789722,
-0.902313473802122));
#80033=CARTESIAN_POINT('Ctrl Pts',(-0.222469382240046,0.0834056693584373,
-0.901374373563559));
#80034=CARTESIAN_POINT('Ctrl Pts',(-0.227020883339142,0.0700702071992786,
-0.900435273324997));
#80035=CARTESIAN_POINT('Ctrl Pts',(-0.230356521300201,0.0564610814585572,
-0.899496173086434));
#80036=CARTESIAN_POINT('Ctrl Pts',(-0.233699367139866,0.0428225481719909,
-0.898555043574732));
#80037=CARTESIAN_POINT('Ctrl Pts',(-0.235820962713621,0.0289100078227147,
-0.897613914063031));
#80038=CARTESIAN_POINT('Ctrl Pts',(-0.236702619460895,0.0149616364529731,
-0.896672784551329));
#80039=CARTESIAN_POINT('Ctrl Pts',(-0.237019194434059,0.00995321871475168,
-0.896334854794841));
#80040=CARTESIAN_POINT('Ctrl Pts',(-0.237176394014881,0.00494019484129286,
-0.895996925038354));
#80041=CARTESIAN_POINT('Ctrl Pts',(-0.237174990683324,-6.64783058782736E-5,
-0.895658995281866));
#80042=CARTESIAN_POINT('Ctrl Pts',(-0.237538664790808,-6.66706272502535E-5,
-0.895658989190502));
#80043=CARTESIAN_POINT('Ctrl Pts',(-0.237552354346597,-0.00372902877874097,
-0.895412173874543));
#80044=CARTESIAN_POINT('Ctrl Pts',(-0.235817901732334,-0.0857960183084813,
-0.889880585092257));
#80045=CARTESIAN_POINT('Ctrl Pts',(-0.141192310182904,-0.242020628383875,
-0.879064222843641));
#80046=CARTESIAN_POINT('Ctrl Pts',(0.126406588917608,-0.25006124709024,
-0.863209902444656));
#80047=CARTESIAN_POINT('Ctrl Pts',(0.278604525080261,-0.029812273024942,
-0.847355582045672));
#80048=CARTESIAN_POINT('Ctrl Pts',(0.181168188818849,0.206234623149449,
-0.832232823074446));
#80049=CARTESIAN_POINT('Ctrl Pts',(0.0247392917291787,0.245026920599375,
-0.82239483756955));
#80050=CARTESIAN_POINT('Ctrl Pts',(-0.0419725940269774,0.233652521193878,
-0.817841625530982));
#80051=CARTESIAN_POINT('Origin',(0.,0.,-1.7456589891905));
#80052=CARTESIAN_POINT('',(-0.0419358257124846,0.233438144155603,-0.697888113229229));
#80053=CARTESIAN_POINT('',(-0.0419358371735614,0.233438142096686,-0.71773215975824));
#80054=CARTESIAN_POINT('',(-0.0419358257166344,0.233438144154858,-1.7456589891905));
#80055=CARTESIAN_POINT('Ctrl Pts',(-0.0419358257124646,0.233438144155607,
-0.69788811322923));
#80056=CARTESIAN_POINT('Ctrl Pts',(-0.0412725130934422,0.233557304468866,
-0.69793329997025));
#80057=CARTESIAN_POINT('Ctrl Pts',(-0.0406086977456027,0.233673636659218,
-0.697978576320819));
#80058=CARTESIAN_POINT('Ctrl Pts',(-0.0377982973546973,0.234153815987307,
-0.698170504273831));
#80059=CARTESIAN_POINT('Ctrl Pts',(-0.0356473144743005,0.234490915060856,
-0.698317994985194));
#80060=CARTESIAN_POINT('Ctrl Pts',(-0.0281718628651947,0.235557226866814,
-0.698832794847702));
#80061=CARTESIAN_POINT('Ctrl Pts',(-0.0228278158251959,0.236135011834267,
-0.699204746382527));
#80062=CARTESIAN_POINT('Ctrl Pts',(-0.000445459285731659,0.237788072973295,
-0.700779755513132));
#80063=CARTESIAN_POINT('Ctrl Pts',(0.0166622754813853,0.237203667853011,
-0.702029844000345));
#80064=CARTESIAN_POINT('Ctrl Pts',(0.0405931708206377,0.233783461845906,
-0.703790846568692));
#80065=CARTESIAN_POINT('Ctrl Pts',(0.0475819246709634,0.232461793583376,
-0.704305869388053));
#80066=CARTESIAN_POINT('Ctrl Pts',(0.0571675330652086,0.230198522675884,
-0.705005415207937));
#80067=CARTESIAN_POINT('Ctrl Pts',(0.0598229510699037,0.229522771377182,
-0.705198447491975));
#80068=CARTESIAN_POINT('Ctrl Pts',(0.0644447600567318,0.228260947380078,
-0.705532435567961));
#80069=CARTESIAN_POINT('Ctrl Pts',(0.0664163334730075,0.227695099974509,
-0.705674267603045));
#80070=CARTESIAN_POINT('Ctrl Pts',(0.0693612119259817,0.226808403973138,
-0.70588490445148));
#80071=CARTESIAN_POINT('Ctrl Pts',(0.0703401242585132,0.226506725838501,
-0.705954719961399));
#80072=CARTESIAN_POINT('Ctrl Pts',(0.0721083366194157,0.225949234892154,
-0.706080422039977));
#80073=CARTESIAN_POINT('Ctrl Pts',(0.072898273271877,0.225695615293672,
-0.706136427678752));
#80074=CARTESIAN_POINT('Ctrl Pts',(0.0746798392025913,0.225113290362607,
-0.706262403854519));
#80075=CARTESIAN_POINT('Ctrl Pts',(0.075670643568685,0.224782173861577,
-0.706332234169308));
#80076=CARTESIAN_POINT('Ctrl Pts',(0.0786987506030232,0.223747920836769,
-0.706545036710449));
#80077=CARTESIAN_POINT('Ctrl Pts',(0.0807287486399363,0.223023530972261,
-0.706686841963383));
#80078=CARTESIAN_POINT('Ctrl Pts',(0.0970899928584773,0.216932461884938,
-0.707824970126772));
#80079=CARTESIAN_POINT('Ctrl Pts',(0.110882979325758,0.210217160741557,
-0.708756077641373));
#80080=CARTESIAN_POINT('Ctrl Pts',(0.137195436773496,0.194090992522556,
-0.710648992683725));
#80081=CARTESIAN_POINT('Ctrl Pts',(0.149623442868847,0.184679837298448,
-0.711607558388222));
#80082=CARTESIAN_POINT('Ctrl Pts',(0.163093244088333,0.172221935031071,
-0.7127975238538));
#80083=CARTESIAN_POINT('Ctrl Pts',(0.165112479337283,0.170287020256893,
-0.712980309158533));
#80084=CARTESIAN_POINT('Ctrl Pts',(0.168270974463446,0.167151417801917,
-0.713273657640761));
#80085=CARTESIAN_POINT('Ctrl Pts',(0.169432733221153,0.165973690686213,
-0.713383219847253));
#80086=CARTESIAN_POINT('Ctrl Pts',(0.171611135338577,0.163718638867498,
-0.713591906253986));
#80087=CARTESIAN_POINT('Ctrl Pts',(0.172630195928064,0.162643751087149,
-0.713690918537525));
#80088=CARTESIAN_POINT('Ctrl Pts',(0.17493119070244,0.160170712417427,-0.71391772663532));
#80089=CARTESIAN_POINT('Ctrl Pts',(0.176206539543232,0.158766601198959,
-0.714045792985131));
#80090=CARTESIAN_POINT('Ctrl Pts',(0.17951259201194,0.15503785653193,-0.714384131193657));
#80091=CARTESIAN_POINT('Ctrl Pts',(0.181514938595392,0.152688680535317,
-0.714595545447361));
#80092=CARTESIAN_POINT('Ctrl Pts',(0.193888879589917,0.137583964803688,
-0.715944562212651));
#80093=CARTESIAN_POINT('Ctrl Pts',(0.202954760662182,0.123820158254631,
-0.717132842792232));
#80094=CARTESIAN_POINT('Ctrl Pts',(0.216812064825179,0.097113011537336,
-0.7193289511933));
#80095=CARTESIAN_POINT('Ctrl Pts',(0.222042744192121,0.0844718863378857,
-0.720327920555699));
#80096=CARTESIAN_POINT('Ctrl Pts',(0.226743498802375,0.0695928095778601,
-0.721414273719591));
#80097=CARTESIAN_POINT('Ctrl Pts',(0.22730732017159,0.067728547901772,-0.721548810022305));
#80098=CARTESIAN_POINT('Ctrl Pts',(0.228126802174816,0.0648933733869678,
-0.721750815913295));
#80099=CARTESIAN_POINT('Ctrl Pts',(0.228399352843517,0.0639274862112577,
-0.721819181754972));
#80100=CARTESIAN_POINT('Ctrl Pts',(0.228886252368911,0.0621591019328021,
-0.721943484782441));
#80101=CARTESIAN_POINT('Ctrl Pts',(0.229102521954586,0.0613571915278185,
-0.721999525647994));
#80102=CARTESIAN_POINT('Ctrl Pts',(0.229587383506215,0.0595210518266504,
-0.722127107771786));
#80103=CARTESIAN_POINT('Ctrl Pts',(0.229853204084155,0.0584861261977165,
-0.722198491767631));
#80104=CARTESIAN_POINT('Ctrl Pts',(0.230664600932059,0.0552360987627232,
-0.722421116651515));
#80105=CARTESIAN_POINT('Ctrl Pts',(0.231185237300466,0.0530148254907443,
-0.722571029091603));
#80106=CARTESIAN_POINT('Ctrl Pts',(0.234427060631319,0.0382264749576697,
-0.723556356512882));
#80107=CARTESIAN_POINT('Ctrl Pts',(0.236154792639585,0.0254618914173424,
-0.724346825836072));
#80108=CARTESIAN_POINT('Ctrl Pts',(0.237154285285275,0.00670265809831208,
-0.725499371379098));
#80109=CARTESIAN_POINT('Ctrl Pts',(0.237247710422204,0.000776829243992221,
-0.725862000528685));
#80110=CARTESIAN_POINT('Ctrl Pts',(0.23694500390142,-0.0131708122621528,
-0.726722141205528));
#80111=CARTESIAN_POINT('Ctrl Pts',(0.236363617371624,-0.0211809168341281,
-0.727221406317558));
#80112=CARTESIAN_POINT('Ctrl Pts',(0.234727607699095,-0.0343931519318241,
-0.728067359657244));
#80113=CARTESIAN_POINT('Ctrl Pts',(0.233902584853899,-0.0396170787934021,
-0.72840768701051));
#80114=CARTESIAN_POINT('Ctrl Pts',(0.23250614692182,-0.0468753790175062,
-0.728891052473623));
#80115=CARTESIAN_POINT('Ctrl Pts',(0.232081073999932,-0.0489365317085573,
-0.729029505816284));
#80116=CARTESIAN_POINT('Ctrl Pts',(0.231303508083531,-0.0524686071292961,
-0.729268949468528));
#80117=CARTESIAN_POINT('Ctrl Pts',(0.230964264410336,-0.0539423393184799,
-0.729369513516864));
#80118=CARTESIAN_POINT('Ctrl Pts',(0.230244226842506,-0.05693891877784,
-0.729575384869119));
#80119=CARTESIAN_POINT('Ctrl Pts',(0.229862362327056,-0.0584614287091833,
-0.729680722025409));
#80120=CARTESIAN_POINT('Ctrl Pts',(0.22885917611664,-0.0622993167888613,
-0.729948175063598));
#80121=CARTESIAN_POINT('Ctrl Pts',(0.228217822408551,-0.064609226644583,
-0.730110927716206));
#80122=CARTESIAN_POINT('Ctrl Pts',(0.225544880266468,-0.0736992740187871,
-0.730758682700036));
#80123=CARTESIAN_POINT('Ctrl Pts',(0.223245419651537,-0.0803961492509822,
-0.731252187816021));
#80124=CARTESIAN_POINT('Ctrl Pts',(0.214960011534496,-0.10141459503311,
-0.732854003245396));
#80125=CARTESIAN_POINT('Ctrl Pts',(0.207867439663697,-0.115255197440044,
-0.733992714310863));
#80126=CARTESIAN_POINT('Ctrl Pts',(0.195866530126652,-0.133913372891324,
-0.735607075104717));
#80127=CARTESIAN_POINT('Ctrl Pts',(0.192022152731297,-0.139369986256464,
-0.736089517425925));
#80128=CARTESIAN_POINT('Ctrl Pts',(0.186346247045105,-0.146744653083869,
-0.736749688956695));
#80129=CARTESIAN_POINT('Ctrl Pts',(0.184705177473427,-0.14880495842335,
-0.736935051888818));
#80130=CARTESIAN_POINT('Ctrl Pts',(0.181764392455744,-0.152373379639254,
-0.737257156581974));
#80131=CARTESIAN_POINT('Ctrl Pts',(0.180479393967894,-0.153893242832383,
-0.737394695947567));
#80132=CARTESIAN_POINT('Ctrl Pts',(0.17851218865146,-0.156161466525623,
-0.737600260082383));
#80133=CARTESIAN_POINT('Ctrl Pts',(0.177844108671842,-0.1569218857589,-0.737669227495669));
#80134=CARTESIAN_POINT('Ctrl Pts',(0.1766193214997,-0.1582980887841,-0.737794102894248));
#80135=CARTESIAN_POINT('Ctrl Pts',(0.176064236033842,-0.158915243053559,
-0.73785012097879));
#80136=CARTESIAN_POINT('Ctrl Pts',(0.174794150653348,-0.160312523602193,
-0.737977000538946));
#80137=CARTESIAN_POINT('Ctrl Pts',(0.174077158499177,-0.161090792169538,
-0.738047712102788));
#80138=CARTESIAN_POINT('Ctrl Pts',(0.171835681275349,-0.163491391400436,
-0.738266051820637));
#80139=CARTESIAN_POINT('Ctrl Pts',(0.170293497032524,-0.165097129488348,
-0.738412423267754));
#80140=CARTESIAN_POINT('Ctrl Pts',(0.158647759741697,-0.17688594891788,
-0.739491693605409));
#80141=CARTESIAN_POINT('Ctrl Pts',(0.147660216672685,-0.186156711101084,
-0.740367942588498));
#80142=CARTESIAN_POINT('Ctrl Pts',(0.122471100144973,-0.203767829853502,
-0.742252702928717));
#80143=CARTESIAN_POINT('Ctrl Pts',(0.108106343461762,-0.211739056874006,
-0.743259151887015));
#80144=CARTESIAN_POINT('Ctrl Pts',(0.0904553046373063,-0.219266248232256,
-0.744503574079788));
#80145=CARTESIAN_POINT('Ctrl Pts',(0.0878557140438428,-0.220320725713338,
-0.744686913416427));
#80146=CARTESIAN_POINT('Ctrl Pts',(0.0836926301445601,-0.221924011954446,
-0.744980942043255));
#80147=CARTESIAN_POINT('Ctrl Pts',(0.082140983340077,-0.222502993337991,
-0.74509062208691));
#80148=CARTESIAN_POINT('Ctrl Pts',(0.079190711674247,-0.223568791690181,
-0.745299400619212));
#80149=CARTESIAN_POINT('Ctrl Pts',(0.0777933370708359,-0.224058853808182,
-0.74539838578155));
#80150=CARTESIAN_POINT('Ctrl Pts',(0.0745988010599739,-0.225145697791662,
-0.745624945197424));
#80151=CARTESIAN_POINT('Ctrl Pts',(0.0727989170514584,-0.225734099481807,
-0.745752787798189));
#80152=CARTESIAN_POINT('Ctrl Pts',(0.068057861652633,-0.227221402946516,
-0.746090126726254));
#80153=CARTESIAN_POINT('Ctrl Pts',(0.0651059974755016,-0.228084734357983,
-0.746300754531325));
#80154=CARTESIAN_POINT('Ctrl Pts',(0.0460115203232367,-0.233268430733042,
-0.747667549970748));
#80155=CARTESIAN_POINT('Ctrl Pts',(0.0294699329641209,-0.235929135672803,
-0.748876284902607));
#80156=CARTESIAN_POINT('Ctrl Pts',(-0.000450035284266839,-0.237544880996643,
-0.751063461568662));
#80157=CARTESIAN_POINT('Ctrl Pts',(-0.013727327331866,-0.237148477525913,
-0.752032725103823));
#80158=CARTESIAN_POINT('Ctrl Pts',(-0.0289269556793946,-0.235413172793825,
-0.753099022095125));
#80159=CARTESIAN_POINT('Ctrl Pts',(-0.0309480029171191,-0.235156017355622,
-0.753239879208319));
#80160=CARTESIAN_POINT('Ctrl Pts',(-0.0339772225012229,-0.2347308513634,
-0.753449365379745));
#80161=CARTESIAN_POINT('Ctrl Pts',(-0.0349879725537008,-0.234582322660133,
-0.753518989499361));
#80162=CARTESIAN_POINT('Ctrl Pts',(-0.0368178645813363,-0.234301331434553,
-0.753644503126043));
#80163=CARTESIAN_POINT('Ctrl Pts',(-0.0376372954166165,-0.234171097933388,
-0.75370050968628));
#80164=CARTESIAN_POINT('Ctrl Pts',(-0.0394897921660676,-0.233866702156411,
-0.753826681377299));
#80165=CARTESIAN_POINT('Ctrl Pts',(-0.0405224042354136,-0.233689993199257,
-0.753896704163329));
#80166=CARTESIAN_POINT('Ctrl Pts',(-0.0436908304922455,-0.233126153236949,
-0.754110708647462));
#80167=CARTESIAN_POINT('Ctrl Pts',(-0.0458225967628157,-0.232716528062168,
-0.754253504176947));
#80168=CARTESIAN_POINT('Ctrl Pts',(-0.0626830524583758,-0.229236064178477,
-0.755375602730882));
#80169=CARTESIAN_POINT('Ctrl Pts',(-0.0770968331509615,-0.224798890260848,
-0.756292022945539));
#80170=CARTESIAN_POINT('Ctrl Pts',(-0.0953643953620943,-0.217209587021275,
-0.757505226182876));
#80171=CARTESIAN_POINT('Ctrl Pts',(-0.0996789223548126,-0.21526375420334,
-0.757795655804547));
#80172=CARTESIAN_POINT('Ctrl Pts',(-0.114093881390425,-0.208236321503507,
-0.758786382857383));
#80173=CARTESIAN_POINT('Ctrl Pts',(-0.123887091487939,-0.202562881419221,
-0.759495123866013));
#80174=CARTESIAN_POINT('Ctrl Pts',(-0.135438908112064,-0.194718673629606,
-0.760402061029963));
#80175=CARTESIAN_POINT('Ctrl Pts',(-0.137614665101858,-0.193187118388579,
-0.760576160564215));
#80176=CARTESIAN_POINT('Ctrl Pts',(-0.141077287895743,-0.190661535795931,
-0.760858848743168));
#80177=CARTESIAN_POINT('Ctrl Pts',(-0.142380539295186,-0.189690284939572,
-0.760966562446334));
#80178=CARTESIAN_POINT('Ctrl Pts',(-0.144857710766146,-0.187804256751526,
-0.761173901067231));
#80179=CARTESIAN_POINT('Ctrl Pts',(-0.14603320861826,-0.186891671910509,
-0.761273436860246));
#80180=CARTESIAN_POINT('Ctrl Pts',(-0.148705600975533,-0.184776383337047,
-0.761502414107902));
#80181=CARTESIAN_POINT('Ctrl Pts',(-0.150196616516627,-0.183566455571589,
-0.761632139405864));
#80182=CARTESIAN_POINT('Ctrl Pts',(-0.15495227656492,-0.179610606194345,
-0.762052423205687));
#80183=CARTESIAN_POINT('Ctrl Pts',(-0.158157421693699,-0.176794806959135,
-0.762345786150206));
#80184=CARTESIAN_POINT('Ctrl Pts',(-0.174700717364953,-0.161451109919493,
-0.763915565279011));
#80185=CARTESIAN_POINT('Ctrl Pts',(-0.186629735940235,-0.147498905900202,
-0.76525254706866));
#80186=CARTESIAN_POINT('Ctrl Pts',(-0.202395590662303,-0.124045783968887,
-0.767312497208922));
#80187=CARTESIAN_POINT('Ctrl Pts',(-0.20742993936851,-0.11543045729609,
-0.768034470365256));
#80188=CARTESIAN_POINT('Ctrl Pts',(-0.212932754758037,-0.104483649791722,
-0.768890955541647));
#80189=CARTESIAN_POINT('Ctrl Pts',(-0.213928520410646,-0.102429391454638,
-0.769049149074406));
#80190=CARTESIAN_POINT('Ctrl Pts',(-0.215346756242341,-0.09939264262794,
-0.769278974305295));
#80191=CARTESIAN_POINT('Ctrl Pts',(-0.21579245643712,-0.0984212308811093,
-0.769351894779467));
#80192=CARTESIAN_POINT('Ctrl Pts',(-0.216540175153328,-0.0967620652989943,
-0.76947538770417));
#80193=CARTESIAN_POINT('Ctrl Pts',(-0.216845512364745,-0.0960758479588558,
-0.769526156731377));
#80194=CARTESIAN_POINT('Ctrl Pts',(-0.217537019213532,-0.0945016583608133,
-0.769641915119431));
#80195=CARTESIAN_POINT('Ctrl Pts',(-0.217921016690719,-0.0936127594339133,
-0.769706773694072));
#80196=CARTESIAN_POINT('Ctrl Pts',(-0.218975374785192,-0.0911304238207894,
-0.769886557328217));
#80197=CARTESIAN_POINT('Ctrl Pts',(-0.219633790319206,-0.0895319355612892,
-0.77000079869276));
#80198=CARTESIAN_POINT('Ctrl Pts',(-0.22460517327538,-0.0770775342941728,
-0.770880156858521));
#80199=CARTESIAN_POINT('Ctrl Pts',(-0.22812886775872,-0.0659220982807263,
-0.771605297876332));
#80200=CARTESIAN_POINT('Ctrl Pts',(-0.233916099083184,-0.0414351821100818,
-0.773153112735934));
#80201=CARTESIAN_POINT('Ctrl Pts',(-0.235892217846397,-0.0280795464162583,
-0.773971664702166));
#80202=CARTESIAN_POINT('Ctrl Pts',(-0.237022625879822,-0.00978702504729879,
-0.775122709844574));
#80203=CARTESIAN_POINT('Ctrl Pts',(-0.237173198549217,-0.00493765826265566,
-0.775430490916757));
#80204=CARTESIAN_POINT('Ctrl Pts',(-0.237176321307005,0.00354594764316934,
-0.77597615790983));
#80205=CARTESIAN_POINT('Ctrl Pts',(-0.237094172917024,0.00717858131304308,
-0.776212119449384));
#80206=CARTESIAN_POINT('Ctrl Pts',(-0.236844378892338,0.0126545945124642,
-0.776572023971867));
#80207=CARTESIAN_POINT('Ctrl Pts',(-0.236738543718849,0.0145003507130851,
-0.776694054263467));
#80208=CARTESIAN_POINT('Ctrl Pts',(-0.236509392449921,0.0178176308153644,
-0.776914757519388));
#80209=CARTESIAN_POINT('Ctrl Pts',(-0.23639389035667,0.01928961167207,-0.777013181726927));
#80210=CARTESIAN_POINT('Ctrl Pts',(-0.236117235945196,0.0224380909768913,
-0.77722480229707));
#80211=CARTESIAN_POINT('Ctrl Pts',(-0.235951955408882,0.024114135323785,
-0.777338122733985));
#80212=CARTESIAN_POINT('Ctrl Pts',(-0.235449435426202,0.0287084214039525,
-0.777650652975377));
#80213=CARTESIAN_POINT('Ctrl Pts',(-0.235075815729186,0.031622296198115,
-0.777850986499745));
#80214=CARTESIAN_POINT('Ctrl Pts',(-0.23239536169275,0.0498381481449627,
-0.779117175203863));
#80215=CARTESIAN_POINT('Ctrl Pts',(-0.228650028799432,0.0648879872156889,
-0.780228297654479));
#80216=CARTESIAN_POINT('Ctrl Pts',(-0.218405834054344,0.0936967215075056,
-0.78245693669531));
#80217=CARTESIAN_POINT('Ctrl Pts',(-0.211995954671028,0.107414938899316,
-0.78356799163188));
#80218=CARTESIAN_POINT('Ctrl Pts',(-0.2032236080024,0.122298174456709,-0.784774058630043));
#80219=CARTESIAN_POINT('Ctrl Pts',(-0.202097460001408,0.124150295255836,
-0.784924108303636));
#80220=CARTESIAN_POINT('Ctrl Pts',(-0.200389876753717,0.126873851099288,
-0.785144411453641));
#80221=CARTESIAN_POINT('Ctrl Pts',(-0.199827841005109,0.127757234087742,
-0.785215811599965));
#80222=CARTESIAN_POINT('Ctrl Pts',(-0.198809953066832,0.129333953760501,
-0.785343111757685));
#80223=CARTESIAN_POINT('Ctrl Pts',(-0.198356294400421,0.130028649017712,
-0.785399147393608));
#80224=CARTESIAN_POINT('Ctrl Pts',(-0.197335623114046,0.131573847006154,
-0.7855236712991));
#80225=CARTESIAN_POINT('Ctrl Pts',(-0.19676674965107,0.132423078405076,
-0.785592035657926));
#80226=CARTESIAN_POINT('Ctrl Pts',(-0.19504613101071,0.134956099842965,
-0.785795813032913));
#80227=CARTESIAN_POINT('Ctrl Pts',(-0.193878100474194,0.136628785209857,
-0.785930198237594));
#80228=CARTESIAN_POINT('Ctrl Pts',(-0.184799900621261,0.149278382478264,
-0.786946831425683));
#80229=CARTESIAN_POINT('Ctrl Pts',(-0.175983970036034,0.159576878659336,
-0.787777426648224));
#80230=CARTESIAN_POINT('Ctrl Pts',(-0.154639014385431,0.180576965926637,
-0.789614163443029));
#80231=CARTESIAN_POINT('Ctrl Pts',(-0.14177996248732,0.190839287104341,
-0.790617268570057));
#80232=CARTESIAN_POINT('Ctrl Pts',(-0.125365621644718,0.20135783012493,
-0.79187398431795));
#80233=CARTESIAN_POINT('Ctrl Pts',(-0.122733673070178,0.202972803435727,
-0.792074691715093));
#80234=CARTESIAN_POINT('Ctrl Pts',(-0.118434953456661,0.205496330072761,
-0.792401696018708));
#80235=CARTESIAN_POINT('Ctrl Pts',(-0.116787441787272,0.206437092032937,
-0.792526834378161));
#80236=CARTESIAN_POINT('Ctrl Pts',(-0.113833868078978,0.208076969109135,
-0.792750939416655));
#80237=CARTESIAN_POINT('Ctrl Pts',(-0.112532194435493,0.208783810773455,
-0.792849624430142));
#80238=CARTESIAN_POINT('Ctrl Pts',(-0.109763066733463,0.210254098341952,
-0.793059438338978));
#80239=CARTESIAN_POINT('Ctrl Pts',(-0.108294081455782,0.211014474314036,
-0.793170668878473));
#80240=CARTESIAN_POINT('Ctrl Pts',(-0.104321243936692,0.213018483310317,
-0.793471359079341));
#80241=CARTESIAN_POINT('Ctrl Pts',(-0.101803224320464,0.214233280622895,
-0.793661804240626));
#80242=CARTESIAN_POINT('Ctrl Pts',(-0.0851960266152346,0.221886385936839,
-0.794917486609948));
#80243=CARTESIAN_POINT('Ctrl Pts',(-0.0705288967850475,0.22697454678074,
-0.796028446405133));
#80244=CARTESIAN_POINT('Ctrl Pts',(-0.0509872451510689,0.23167557173731,
-0.797493011601209));
#80245=CARTESIAN_POINT('Ctrl Pts',(-0.0464728068161583,0.232623102023117,
-0.797830002151534));
#80246=CARTESIAN_POINT('Ctrl Pts',(-0.0419357988072473,0.233438148988973,
-0.798166224572096));
#80247=CARTESIAN_POINT('',(-0.237109827361837,0.000214302678508487,-0.79565902906244));
#80248=CARTESIAN_POINT('Ctrl Pts',(-0.0419725940269774,0.233652521193878,
-0.817841625530982));
#80249=CARTESIAN_POINT('Ctrl Pts',(-0.052691146551867,0.231825004311616,
-0.817110064103221));
#80250=CARTESIAN_POINT('Ctrl Pts',(-0.139632908759117,0.210569229449833,
-0.811093729209133));
#80251=CARTESIAN_POINT('Ctrl Pts',(-0.22545258634803,0.119877253208548,
-0.803699530386285));
#80252=CARTESIAN_POINT('Ctrl Pts',(-0.237291832349283,0.0207557962214839,
-0.797036892991199));
#80253=CARTESIAN_POINT('Ctrl Pts',(-0.237109827361837,0.000214302678508487,
-0.79565902906244));
#80254=CARTESIAN_POINT('Ctrl Pts',(-0.237174905727117,0.000211467096690729,
-0.795696433125957));
#80255=CARTESIAN_POINT('Ctrl Pts',(-0.237183570743107,-0.00950694481013415,
-0.795099524121233));
#80256=CARTESIAN_POINT('Ctrl Pts',(-0.236594901708461,-0.0192163662911197,
-0.794499015434566));
#80257=CARTESIAN_POINT('Ctrl Pts',(-0.234853264355434,-0.0334220249162563,
-0.793591602292384));
#80258=CARTESIAN_POINT('Ctrl Pts',(-0.234161842675524,-0.0379646516319011,
-0.793297117129415));
#80259=CARTESIAN_POINT('Ctrl Pts',(-0.232991163280162,-0.0443944688046205,
-0.792872515283452));
#80260=CARTESIAN_POINT('Ctrl Pts',(-0.232619907358163,-0.0463004251536392,
-0.792745675415652));
#80261=CARTESIAN_POINT('Ctrl Pts',(-0.231927291970332,-0.0496373047693558,
-0.792521771257462));
#80262=CARTESIAN_POINT('Ctrl Pts',(-0.231615981515141,-0.0510702235320288,
-0.792425024249665));
#80263=CARTESIAN_POINT('Ctrl Pts',(-0.230960616551684,-0.0539574595370931,
-0.792228824920733));
#80264=CARTESIAN_POINT('Ctrl Pts',(-0.230616063924194,-0.0554115937654241,
-0.792129360808724));
#80265=CARTESIAN_POINT('Ctrl Pts',(-0.229873022859243,-0.0584204565614054,
-0.791922154891479));
#80266=CARTESIAN_POINT('Ctrl Pts',(-0.229472449671661,-0.0599745863349541,
-0.791814350645875));
#80267=CARTESIAN_POINT('Ctrl Pts',(-0.22839047461548,-0.0640027871121505,
-0.791532841402084));
#80268=CARTESIAN_POINT('Ctrl Pts',(-0.227684652809592,-0.0664700205364123,
-0.791358358494667));
#80269=CARTESIAN_POINT('Ctrl Pts',(-0.224384687695233,-0.077335281477275,
-0.790580521099673));
#80270=CARTESIAN_POINT('Ctrl Pts',(-0.221365207361706,-0.0855958276906676,
-0.78996362248931));
#80271=CARTESIAN_POINT('Ctrl Pts',(-0.21191323810314,-0.107583193448354,
-0.788252258217256));
#80272=CARTESIAN_POINT('Ctrl Pts',(-0.204612912815062,-0.120891934098815,
-0.787136939922067));
#80273=CARTESIAN_POINT('Ctrl Pts',(-0.191659696691151,-0.139931064890045,
-0.785467694818033));
#80274=CARTESIAN_POINT('Ctrl Pts',(-0.186901989987256,-0.146225215028108,
-0.784902570338719));
#80275=CARTESIAN_POINT('Ctrl Pts',(-0.18070583495538,-0.153624534668491,
-0.784231721414135));
#80276=CARTESIAN_POINT('Ctrl Pts',(-0.179557446660631,-0.154965222698083,
-0.784109900299498));
#80277=CARTESIAN_POINT('Ctrl Pts',(-0.177735861010109,-0.157044395839245,
-0.783920717238714));
#80278=CARTESIAN_POINT('Ctrl Pts',(-0.177072810544419,-0.157791629723499,
-0.783852673171487));
#80279=CARTESIAN_POINT('Ctrl Pts',(-0.175849814478085,-0.159152484582014,
-0.783728689310069));
#80280=CARTESIAN_POINT('Ctrl Pts',(-0.175291355754397,-0.159767365998479,
-0.783672649127169));
#80281=CARTESIAN_POINT('Ctrl Pts',(-0.174003716286925,-0.161170220039398,
-0.783544734773989));
#80282=CARTESIAN_POINT('Ctrl Pts',(-0.173272403664542,-0.16195618959638,
-0.783473021590144));
#80283=CARTESIAN_POINT('Ctrl Pts',(-0.17100674495327,-0.164358265995882,
-0.783253603660484));
#80284=CARTESIAN_POINT('Ctrl Pts',(-0.169454889654996,-0.165957788812911,
-0.78310714472481));
#80285=CARTESIAN_POINT('Ctrl Pts',(-0.158274679900464,-0.177161047115611,
-0.782076702621502));
#80286=CARTESIAN_POINT('Ctrl Pts',(-0.147857320472774,-0.185944131613457,
-0.781243350392742));
#80287=CARTESIAN_POINT('Ctrl Pts',(-0.127351052415479,-0.200414141010939,
-0.779704140511035));
#80288=CARTESIAN_POINT('Ctrl Pts',(-0.117489796512099,-0.206349810329616,
-0.779000549495292));
#80289=CARTESIAN_POINT('Ctrl Pts',(-0.101318976654128,-0.214547146283394,
-0.777858103836911));
#80290=CARTESIAN_POINT('Ctrl Pts',(-0.0952774781192003,-0.217297498570509,
-0.777433781701499));
#80291=CARTESIAN_POINT('Ctrl Pts',(-0.0870150278964188,-0.220648066866,
-0.77685209289067));
#80292=CARTESIAN_POINT('Ctrl Pts',(-0.0848888392242636,-0.221474758996812,
-0.776702299506462));
#80293=CARTESIAN_POINT('Ctrl Pts',(-0.0813026221925531,-0.222809903727811,
-0.776449297925693));
#80294=CARTESIAN_POINT('Ctrl Pts',(-0.0798489213170164,-0.223334993109952,
-0.776346647789129));
#80295=CARTESIAN_POINT('Ctrl Pts',(-0.0769638557515132,-0.224345335497279,
-0.776142688458797));
#80296=CARTESIAN_POINT('Ctrl Pts',(-0.0755327782592826,-0.224831189734997,
-0.776041404801921));
#80297=CARTESIAN_POINT('Ctrl Pts',(-0.0723520621148056,-0.225877255555812,
-0.775815995957368));
#80298=CARTESIAN_POINT('Ctrl Pts',(-0.0706003757388539,-0.226430877058226,
-0.775691661881254));
#80299=CARTESIAN_POINT('Ctrl Pts',(-0.0644760839380083,-0.228288490011239,
-0.775256183001657));
#80300=CARTESIAN_POINT('Ctrl Pts',(-0.0600726618567288,-0.229486536465834,
-0.77494167094121));
#80301=CARTESIAN_POINT('Ctrl Pts',(-0.0342912756779752,-0.235708068884862,
-0.773091154058116));
#80302=CARTESIAN_POINT('Ctrl Pts',(-0.012334723404674,-0.23786911401318,
-0.771465216336041));
#80303=CARTESIAN_POINT('Ctrl Pts',(0.0142702793627001,-0.236791460666137,
-0.769543698707242));
#80304=CARTESIAN_POINT('Ctrl Pts',(0.0189351741726104,-0.236464164594614,
-0.76920921404585));
#80305=CARTESIAN_POINT('Ctrl Pts',(0.0266148865212963,-0.235696594005048,
-0.768665484015001));
#80306=CARTESIAN_POINT('Ctrl Pts',(0.0296362452449061,-0.235335785030437,
-0.768453355713495));
#80307=CARTESIAN_POINT('Ctrl Pts',(0.0338346405148792,-0.234752269905424,
-0.768161824163811));
#80308=CARTESIAN_POINT('Ctrl Pts',(0.0350180576949475,-0.234578658262423,
-0.768080009261075));
#80309=CARTESIAN_POINT('Ctrl Pts',(0.0370359409354392,-0.234267016299158,
-0.767941176819243));
#80310=CARTESIAN_POINT('Ctrl Pts',(0.0378710642517986,-0.234133462864492,
-0.767883917651591));
#80311=CARTESIAN_POINT('Ctrl Pts',(0.039621576743821,-0.233843908322147,
-0.767764331222161));
#80312=CARTESIAN_POINT('Ctrl Pts',(0.0405367861275198,-0.233686995460666,
-0.767702054533213));
#80313=CARTESIAN_POINT('Ctrl Pts',(0.0430192709528315,-0.233246349788409,
-0.767533740606762));
#80314=CARTESIAN_POINT('Ctrl Pts',(0.0445846808497148,-0.2329521923832,
-0.767428266699933));
#80315=CARTESIAN_POINT('Ctrl Pts',(0.0524348418444053,-0.231395029778182,
-0.766902127638843));
#80316=CARTESIAN_POINT('Ctrl Pts',(0.0586700948759226,-0.229893253939525,
-0.76649320281935));
#80317=CARTESIAN_POINT('Ctrl Pts',(0.0662048283548098,-0.227751887474845,
-0.76600167283361));
#80318=CARTESIAN_POINT('Ctrl Pts',(0.0675687648985846,-0.227350970230419,
-0.765912804064903));
#80319=CARTESIAN_POINT('Ctrl Pts',(0.0899020344941972,-0.220567567022637,
-0.764458242766159));
#80320=CARTESIAN_POINT('Ctrl Pts',(0.109889800372382,-0.211321289523077,
-0.763153778113318));
#80321=CARTESIAN_POINT('Ctrl Pts',(0.131722773197877,-0.197274995830279,
-0.761488973731165));
#80322=CARTESIAN_POINT('Ctrl Pts',(0.135064870568817,-0.195002027196108,
-0.761227066196734));
#80323=CARTESIAN_POINT('Ctrl Pts',(0.139891081222704,-0.191536104288281,
-0.76083729983917));
#80324=CARTESIAN_POINT('Ctrl Pts',(0.141421617645303,-0.190408822182136,
-0.760711925659996));
#80325=CARTESIAN_POINT('Ctrl Pts',(0.14412042064837,-0.188370589690317,
-0.760487583921135));
#80326=CARTESIAN_POINT('Ctrl Pts',(0.145294026137241,-0.187466851755349,
-0.760388900747177));
#80327=CARTESIAN_POINT('Ctrl Pts',(0.147757850932039,-0.185532543362412,
-0.760179286483267));
#80328=CARTESIAN_POINT('Ctrl Pts',(0.149045921789106,-0.18449937701233,
-0.760068255638467));
#80329=CARTESIAN_POINT('Ctrl Pts',(0.152476097930082,-0.181688657168324,
-0.759768596998929));
#80330=CARTESIAN_POINT('Ctrl Pts',(0.154597815934039,-0.17988674978199,
-0.759578994951345));
#80331=CARTESIAN_POINT('Ctrl Pts',(0.167450880452792,-0.168575689988455,
-0.758403419182736));
#80332=CARTESIAN_POINT('Ctrl Pts',(0.177331528405163,-0.158148535889789,
-0.75737876480446));
#80333=CARTESIAN_POINT('Ctrl Pts',(0.19376050250694,-0.137322632022481,
-0.755449329762304));
#80334=CARTESIAN_POINT('Ctrl Pts',(0.200562681729688,-0.127181996869711,
-0.754553017852833));
#80335=CARTESIAN_POINT('Ctrl Pts',(0.209265022608862,-0.111761060622614,
-0.75328367448168));
#80336=CARTESIAN_POINT('Ctrl Pts',(0.211806899978007,-0.106865486382851,
-0.752893510079721));
#80337=CARTESIAN_POINT('Ctrl Pts',(0.214809111322174,-0.100554454992311,
-0.752410318534097));
#80338=CARTESIAN_POINT('Ctrl Pts',(0.215429827972977,-0.0992176507569932,
-0.752309066816212));
#80339=CARTESIAN_POINT('Ctrl Pts',(0.216410519045071,-0.0970529879635057,
-0.752146975166385));
#80340=CARTESIAN_POINT('Ctrl Pts',(0.216778287851915,-0.0962287338101404,
-0.752085685914123));
#80341=CARTESIAN_POINT('Ctrl Pts',(0.217482753559935,-0.0946253290524609,
-0.751967324707513));
#80342=CARTESIAN_POINT('Ctrl Pts',(0.217819986106068,-0.0938464420023404,
-0.751910223227109));
#80343=CARTESIAN_POINT('Ctrl Pts',(0.21864740524201,-0.0919069100884264,
-0.751768973313796));
#80344=CARTESIAN_POINT('Ctrl Pts',(0.219132547910465,-0.0907441158534499,
-0.751685122162888));
#80345=CARTESIAN_POINT('Ctrl Pts',(0.220829804977394,-0.0865831153656113,
-0.751387829635319));
#80346=CARTESIAN_POINT('Ctrl Pts',(0.221989897870175,-0.0835639057725772,
-0.751177203677069));
#80347=CARTESIAN_POINT('Ctrl Pts',(0.228898777052709,-0.0644226445820406,
-0.749867963497479));
#80348=CARTESIAN_POINT('Ctrl Pts',(0.23295052181949,-0.0477400874244471,
-0.748839220775789));
#80349=CARTESIAN_POINT('Ctrl Pts',(0.2362326420317,-0.0226512805388733,
-0.74728005788235));
#80350=CARTESIAN_POINT('Ctrl Pts',(0.236873409534906,-0.0144884324855405,
-0.746771477834052));
#80351=CARTESIAN_POINT('Ctrl Pts',(0.237188001756677,-0.00266660625486337,
-0.746020367335511));
#80352=CARTESIAN_POINT('Ctrl Pts',(0.237200971930077,0.000977646550547964,
-0.745786873236991));
#80353=CARTESIAN_POINT('Ctrl Pts',(0.237072432994858,0.00757426651137478,
-0.745359648491185));
#80354=CARTESIAN_POINT('Ctrl Pts',(0.236959701431725,0.010526473306441,
-0.745166795065436));
#80355=CARTESIAN_POINT('Ctrl Pts',(0.236695990931515,0.0151603322331561,
-0.744861109222533));
#80356=CARTESIAN_POINT('Ctrl Pts',(0.236582146687212,0.0168438540210009,
-0.744749432854298));
#80357=CARTESIAN_POINT('Ctrl Pts',(0.236335087941687,0.0199971080462435,
-0.744539035603704));
#80358=CARTESIAN_POINT('Ctrl Pts',(0.236206100040325,0.0214670970900954,
-0.744440451623429));
#80359=CARTESIAN_POINT('Ctrl Pts',(0.235885195639102,0.0247699651876454,
-0.744217775165685));
#80360=CARTESIAN_POINT('Ctrl Pts',(0.235685618385446,0.0266019858427822,
-0.744093448440545));
#80361=CARTESIAN_POINT('Ctrl Pts',(0.235017783912248,0.0321328838702285,
-0.743715549810751));
#80362=CARTESIAN_POINT('Ctrl Pts',(0.234483658093562,0.0358230699105591,
-0.743459944580654));
#80363=CARTESIAN_POINT('Ctrl Pts',(0.230715549343527,0.0581330366572575,
-0.741892646899228));
#80364=CARTESIAN_POINT('Ctrl Pts',(0.225352893163457,0.076321280890389,
-0.740513586993792));
#80365=CARTESIAN_POINT('Ctrl Pts',(0.213879115252791,0.103009220083144,
-0.73839550128084));
#80366=CARTESIAN_POINT('Ctrl Pts',(0.209270984531721,0.112075288506107,
-0.737659156215842));
#80367=CARTESIAN_POINT('Ctrl Pts',(0.20292265519373,0.122799326892156,-0.736787793651319));
#80368=CARTESIAN_POINT('Ctrl Pts',(0.201721300988386,0.124762960779748,
-0.736628249504553));
#80369=CARTESIAN_POINT('Ctrl Pts',(0.199918736181254,0.127615159527899,
-0.736396863250624));
#80370=CARTESIAN_POINT('Ctrl Pts',(0.199339824249572,0.128517565326425,
-0.736323707961385));
#80371=CARTESIAN_POINT('Ctrl Pts',(0.198344866478263,0.130045603410437,
-0.736199966154704));
#80372=CARTESIAN_POINT('Ctrl Pts',(0.197931941809173,0.130673224091904,
-0.736149180673524));
#80373=CARTESIAN_POINT('Ctrl Pts',(0.196981561896402,0.132102902952194,
-0.736033592095689));
#80374=CARTESIAN_POINT('Ctrl Pts',(0.196442184261917,0.132903653149059,
-0.735968917779509));
#80375=CARTESIAN_POINT('Ctrl Pts',(0.194930145149593,0.135119082237537,
-0.73579010040145));
#80376=CARTESIAN_POINT('Ctrl Pts',(0.19394696846424,0.136526560475476,-0.735676629559511));
#80377=CARTESIAN_POINT('Ctrl Pts',(0.186701717207357,0.146662345511946,
-0.734859472681156));
#80378=CARTESIAN_POINT('Ctrl Pts',(0.179867522040419,0.154968089685708,
-0.734189516803673));
#80379=CARTESIAN_POINT('Ctrl Pts',(0.171514596426131,0.163819276462219,
-0.733439291905644));
#80380=CARTESIAN_POINT('Ctrl Pts',(0.170527020822667,0.164847042260522,
-0.733351585801587));
#80381=CARTESIAN_POINT('Ctrl Pts',(0.162741367645642,0.172804699767231,
-0.732667307776094));
#80382=CARTESIAN_POINT('Ctrl Pts',(0.155533027485139,0.179320077836887,
-0.732075486152717));
#80383=CARTESIAN_POINT('Ctrl Pts',(0.142718693961479,0.189547040782069,
-0.731058517166502));
#80384=CARTESIAN_POINT('Ctrl Pts',(0.137317809386962,0.193495518692476,
-0.730639364687499));
#80385=CARTESIAN_POINT('Ctrl Pts',(0.127885098388096,0.199797578191137,
-0.729915321819036));
#80386=CARTESIAN_POINT('Ctrl Pts',(0.123937464666749,0.202270044446317,
-0.729614560020163));
#80387=CARTESIAN_POINT('Ctrl Pts',(0.118188578525612,0.205639167167795,
-0.729178185644532));
#80388=CARTESIAN_POINT('Ctrl Pts',(0.116444586969378,0.206631713257822,
-0.729046017603098));
#80389=CARTESIAN_POINT('Ctrl Pts',(0.113379146882102,0.208325194034733,
-0.728813955615001));
#80390=CARTESIAN_POINT('Ctrl Pts',(0.112063253908587,0.209035988208327,
-0.728714418841939));
#80391=CARTESIAN_POINT('Ctrl Pts',(0.109324243271386,0.210482199589635,
-0.728507352556175));
#80392=CARTESIAN_POINT('Ctrl Pts',(0.10790022507186,0.211215737393647,-0.728399763247817));
#80393=CARTESIAN_POINT('Ctrl Pts',(0.104188824945857,0.213080220173569,
-0.728119463688626));
#80394=CARTESIAN_POINT('Ctrl Pts',(0.101890479069181,0.214188750556311,
-0.72794598801542));
#80395=CARTESIAN_POINT('Ctrl Pts',(0.0918328649533584,0.218841193512923,
-0.727187028668554));
#80396=CARTESIAN_POINT('Ctrl Pts',(0.0839043062420878,0.222001756949136,
-0.726588852080559));
#80397=CARTESIAN_POINT('Ctrl Pts',(0.0556350911330214,0.231539822584417,
-0.724457845182605));
#80398=CARTESIAN_POINT('Ctrl Pts',(0.0346231366805335,0.235599420765083,
-0.722867160341234));
#80399=CARTESIAN_POINT('Ctrl Pts',(0.0101497653412854,0.236979439200232,
-0.72113770438752));
#80400=CARTESIAN_POINT('Ctrl Pts',(0.00694325102918205,0.237095057059841,
-0.720913758441859));
#80401=CARTESIAN_POINT('Ctrl Pts',(0.00251482073951898,0.237164807630886,
-0.720608984977922));
#80402=CARTESIAN_POINT('Ctrl Pts',(0.00129428535896178,0.237174609283586,
-0.720525458491378));
#80403=CARTESIAN_POINT('Ctrl Pts',(-0.000776229268319339,0.237175252642923,
-0.720384627420986));
#80404=CARTESIAN_POINT('Ctrl Pts',(-0.00162617263924265,0.237170948166812,
-0.7203270638331));
#80405=CARTESIAN_POINT('Ctrl Pts',(-0.00339484677249993,0.237152482204098,
-0.720207813836742));
#80406=CARTESIAN_POINT('Ctrl Pts',(-0.00431354279396595,0.237137551266237,
-0.720146169317013));
#80407=CARTESIAN_POINT('Ctrl Pts',(-0.00677979150403611,0.237083131871023,
-0.719981425867255));
#80408=CARTESIAN_POINT('Ctrl Pts',(-0.0083271139171756,0.237033829817099,
-0.719878850377708));
#80409=CARTESIAN_POINT('Ctrl Pts',(-0.0156375495891087,0.236729223125891,
-0.719397463961534));
#80410=CARTESIAN_POINT('Ctrl Pts',(-0.0213910559553792,0.236278845228366,
-0.719028103608231));
#80411=CARTESIAN_POINT('Ctrl Pts',(-0.0320841269560271,0.235047929974299,
-0.718349970038989));
#80412=CARTESIAN_POINT('Ctrl Pts',(-0.0370242168771452,0.234320486803334,
-0.718040032741223));
#80413=CARTESIAN_POINT('Ctrl Pts',(-0.0419358371735614,0.233438142096686,
-0.71773215975824));
#80414=CARTESIAN_POINT('Origin',(0.,0.,-1.7456589891905));
#80415=CARTESIAN_POINT('',(-0.0419358081412419,0.233438147312176,-0.598166693585937));
#80416=CARTESIAN_POINT('',(-0.0419358257187831,0.233438144154472,-0.618049599588275));
#80417=CARTESIAN_POINT('',(-0.0419358257166344,0.233438144154858,-1.7456589891905));
#80418=CARTESIAN_POINT('',(-0.237174993928743,-0.0001557562965092,-0.676096353182709));
#80419=CARTESIAN_POINT('Ctrl Pts',(-0.0419358081412227,0.233438147312179,
-0.598166693585938));
#80420=CARTESIAN_POINT('Ctrl Pts',(-0.0254221450267922,0.236404731034887,
-0.599196757273924));
#80421=CARTESIAN_POINT('Ctrl Pts',(-0.00862997878185331,0.237612619833391,
-0.600218908972521));
#80422=CARTESIAN_POINT('Ctrl Pts',(0.0119921080420857,0.236902656990329,
-0.601544371140064));
#80423=CARTESIAN_POINT('Ctrl Pts',(0.0158198069622217,0.236677862496629,
-0.601793151172967));
#80424=CARTESIAN_POINT('Ctrl Pts',(0.0214968765434211,0.23620613017656,
-0.60216707457608));
#80425=CARTESIAN_POINT('Ctrl Pts',(0.0233516142688545,0.236029984145217,
-0.602290022757764));
#80426=CARTESIAN_POINT('Ctrl Pts',(0.0266734177630653,0.235674973507113,
-0.602511720379031));
#80427=CARTESIAN_POINT('Ctrl Pts',(0.0281412653325034,0.23550421093767,
-0.602610211349407));
#80428=CARTESIAN_POINT('Ctrl Pts',(0.0312689983012018,0.235110686713298,
-0.602821248214161));
#80429=CARTESIAN_POINT('Ctrl Pts',(0.0329283042571606,0.234884039030316,
-0.602933911226548));
#80430=CARTESIAN_POINT('Ctrl Pts',(0.0374468861669076,0.234218016968055,
-0.603242705178056));
#80431=CARTESIAN_POINT('Ctrl Pts',(0.040300665144993,0.233743885183556,
-0.603439915385624));
#80432=CARTESIAN_POINT('Ctrl Pts',(0.0585602015538563,0.230365896083917,
-0.604716348384372));
#80433=CARTESIAN_POINT('Ctrl Pts',(0.0736519686150716,0.225993287091945,
-0.605842255293825));
#80434=CARTESIAN_POINT('Ctrl Pts',(0.102101467728049,0.214596245297013,
-0.608076415713036));
#80435=CARTESIAN_POINT('Ctrl Pts',(0.115445624116596,0.207722496911975,
-0.609177482037637));
#80436=CARTESIAN_POINT('Ctrl Pts',(0.129882729989079,0.198462041042995,
-0.610374961558479));
#80437=CARTESIAN_POINT('Ctrl Pts',(0.131696184824981,0.197263329130861,
-0.610525449874029));
#80438=CARTESIAN_POINT('Ctrl Pts',(0.134359360904778,0.195449843766908,
-0.610746267349269));
#80439=CARTESIAN_POINT('Ctrl Pts',(0.135221840899336,0.194854132980955,
-0.610817750646774));
#80440=CARTESIAN_POINT('Ctrl Pts',(0.136759936686426,0.193776646679321,
-0.610945136366521));
#80441=CARTESIAN_POINT('Ctrl Pts',(0.137437002081487,0.193297024291547,
-0.611001175275601));
#80442=CARTESIAN_POINT('Ctrl Pts',(0.138941630224246,0.192219266786862,
-0.611125630498796));
#80443=CARTESIAN_POINT('Ctrl Pts',(0.139767860574496,0.191619331958714,
-0.611193923701551));
#80444=CARTESIAN_POINT('Ctrl Pts',(0.142228711015798,0.189808096342956,
-0.611397268602092));
#80445=CARTESIAN_POINT('Ctrl Pts',(0.14385169473178,0.188581044319087,-0.611531298938028));
#80446=CARTESIAN_POINT('Ctrl Pts',(0.155723433502437,0.179362986695429,
-0.612512767818748));
#80447=CARTESIAN_POINT('Ctrl Pts',(0.165317106780871,0.170561464048922,
-0.613312587419873));
#80448=CARTESIAN_POINT('Ctrl Pts',(0.185685693554085,0.148532550951544,
-0.615153658607073));
#80449=CARTESIAN_POINT('Ctrl Pts',(0.195851971144819,0.134844448967748,
-0.61619079048841));
#80450=CARTESIAN_POINT('Ctrl Pts',(0.206018158725287,0.117549417105015,
-0.617484360355525));
#80451=CARTESIAN_POINT('Ctrl Pts',(0.207517777186748,0.114881321239951,
-0.617683337203257));
#80452=CARTESIAN_POINT('Ctrl Pts',(0.209858952545478,0.110520451363784,
-0.618008079954614));
#80453=CARTESIAN_POINT('Ctrl Pts',(0.210732664128625,0.108845275777767,
-0.618132713877082));
#80454=CARTESIAN_POINT('Ctrl Pts',(0.212255097573913,0.105839244220124,
-0.618356260416211));
#80455=CARTESIAN_POINT('Ctrl Pts',(0.21291155406122,0.104512401373171,-0.618454896715161));
#80456=CARTESIAN_POINT('Ctrl Pts',(0.2142770926733,0.101686081651301,-0.618664972572333));
#80457=CARTESIAN_POINT('Ctrl Pts',(0.214982949032665,0.100185143755965,
-0.61877651720911));
#80458=CARTESIAN_POINT('Ctrl Pts',(0.216844954679859,0.0961154568577069,
-0.619078980509639));
#80459=CARTESIAN_POINT('Ctrl Pts',(0.217971147074729,0.093533380531618,
-0.619270904883523));
#80460=CARTESIAN_POINT('Ctrl Pts',(0.225327756282748,0.0758116349300416,
-0.620588836354732));
#80461=CARTESIAN_POINT('Ctrl Pts',(0.230020923519952,0.0600848518164682,
-0.621766366989002));
#80462=CARTESIAN_POINT('Ctrl Pts',(0.235717451081462,0.0299140326794427,
-0.624005869970449));
#80463=CARTESIAN_POINT('Ctrl Pts',(0.237094742794941,0.0156114064133701,
-0.625058306584018));
#80464=CARTESIAN_POINT('Ctrl Pts',(0.237183531140776,-0.000956382651459844,
-0.626215759581499));
#80465=CARTESIAN_POINT('Ctrl Pts',(0.23716408975447,-0.00318394967359194,
-0.626370049883849));
#80466=CARTESIAN_POINT('Ctrl Pts',(0.237089120648149,-0.00646913497271217,
-0.626595318404422));
#80467=CARTESIAN_POINT('Ctrl Pts',(0.237057890662872,-0.00752711226960892,
-0.626667516378383));
#80468=CARTESIAN_POINT('Ctrl Pts',(0.236989533019771,-0.00941439762022854,
-0.626795643777125));
#80469=CARTESIAN_POINT('Ctrl Pts',(0.236955133153033,-0.0102437581127221,
-0.626851717077923));
#80470=CARTESIAN_POINT('Ctrl Pts',(0.236869132238768,-0.0120838279260917,
-0.626975609732613));
#80471=CARTESIAN_POINT('Ctrl Pts',(0.236815416311022,-0.0130944032460889,
-0.627043312639457));
#80472=CARTESIAN_POINT('Ctrl Pts',(0.236636943089448,-0.0160901910361994,
-0.627243088790108));
#80473=CARTESIAN_POINT('Ctrl Pts',(0.236493675453163,-0.0180742687312584,
-0.627374193136596));
#80474=CARTESIAN_POINT('Ctrl Pts',(0.236102893316887,-0.022678874836118,
-0.627676144350482));
#80475=CARTESIAN_POINT('Ctrl Pts',(0.235836682221959,-0.0252975913978463,
-0.627846124830268));
#80476=CARTESIAN_POINT('Ctrl Pts',(0.234742661646349,-0.0345293345070006,
-0.62844089282821));
#80477=CARTESIAN_POINT('Ctrl Pts',(0.233679764606343,-0.0411117012407693,
-0.62885690197077));
#80478=CARTESIAN_POINT('Ctrl Pts',(0.229229620746353,-0.0628146747479831,
-0.63022648121314));
#80479=CARTESIAN_POINT('Ctrl Pts',(0.224639485495002,-0.0776466328464153,
-0.631161557424502));
#80480=CARTESIAN_POINT('Ctrl Pts',(0.215881452904409,-0.0984768579057991,
-0.632580891960774));
#80481=CARTESIAN_POINT('Ctrl Pts',(0.212833942722427,-0.104900864653528,
-0.633034050834307));
#80482=CARTESIAN_POINT('Ctrl Pts',(0.208377679281489,-0.113298212396497,
-0.633653354842134));
#80483=CARTESIAN_POINT('Ctrl Pts',(0.207220420950265,-0.115401207132185,
-0.6338107861835));
#80484=CARTESIAN_POINT('Ctrl Pts',(0.205253617800437,-0.118850321237735,
-0.6340730813022));
#80485=CARTESIAN_POINT('Ctrl Pts',(0.2044622455822,-0.120206640454447,-0.634177293001574));
#80486=CARTESIAN_POINT('Ctrl Pts',(0.20288262444362,-0.122853193269345,
-0.6343827998943));
#80487=CARTESIAN_POINT('Ctrl Pts',(0.202095389948195,-0.124143947000845,
-0.634484054651069));
#80488=CARTESIAN_POINT('Ctrl Pts',(0.200184120121785,-0.127211313384452,
-0.634727194825757));
#80489=CARTESIAN_POINT('Ctrl Pts',(0.199048714417582,-0.128980653574054,
-0.634869493261507));
#80490=CARTESIAN_POINT('Ctrl Pts',(0.194983686028365,-0.135133793066106,
-0.635371747363606));
#80491=CARTESIAN_POINT('Ctrl Pts',(0.191931734639848,-0.139434506144744,
-0.635736208131257));
#80492=CARTESIAN_POINT('Ctrl Pts',(0.183898819826625,-0.149990305384879,
-0.636665798194291));
#80493=CARTESIAN_POINT('Ctrl Pts',(0.178740416319221,-0.156101601947246,
-0.637236961096213));
#80494=CARTESIAN_POINT('Ctrl Pts',(0.162893501051262,-0.173058544879358,
-0.638915688254464));
#80495=CARTESIAN_POINT('Ctrl Pts',(0.151457539839905,-0.183150655761056,
-0.640039666721596));
#80496=CARTESIAN_POINT('Ctrl Pts',(0.13509613273099,-0.195002232324807,
-0.641484270233975));
#80497=CARTESIAN_POINT('Ctrl Pts',(0.130967052994491,-0.197799076981264,
-0.64183628707571));
#80498=CARTESIAN_POINT('Ctrl Pts',(0.125505612222618,-0.201252325275129,
-0.642283043813516));
#80499=CARTESIAN_POINT('Ctrl Pts',(0.124251299019681,-0.202029136752836,
-0.642384399980747));
#80500=CARTESIAN_POINT('Ctrl Pts',(0.122217637220845,-0.203262503360613,
-0.642546629224881));
#80501=CARTESIAN_POINT('Ctrl Pts',(0.121442810269847,-0.203726385190649,
-0.642607952739965));
#80502=CARTESIAN_POINT('Ctrl Pts',(0.119925862543786,-0.204622838186182,
-0.642727037779076));
#80503=CARTESIAN_POINT('Ctrl Pts',(0.119184014324925,-0.205055819654559,
-0.642784822840843));
#80504=CARTESIAN_POINT('Ctrl Pts',(0.117341439604361,-0.206117865386348,
-0.642927270717096));
#80505=CARTESIAN_POINT('Ctrl Pts',(0.116237969485084,-0.206742164319824,
-0.643011635539818));
#80506=CARTESIAN_POINT('Ctrl Pts',(0.112027475051262,-0.209079923734588,
-0.643330184690371));
#80507=CARTESIAN_POINT('Ctrl Pts',(0.108886975712574,-0.210732530503391,
-0.643560886242645));
#80508=CARTESIAN_POINT('Ctrl Pts',(0.100485327899274,-0.214915677979137,
-0.644163197051283));
#80509=CARTESIAN_POINT('Ctrl Pts',(0.0951656623110755,-0.217323619336894,
-0.644529540295748));
#80510=CARTESIAN_POINT('Ctrl Pts',(0.0734052644079443,-0.226220971319432,
-0.645989150630036));
#80511=CARTESIAN_POINT('Ctrl Pts',(0.0563525568726708,-0.231059862047319,
-0.647050118704931));
#80512=CARTESIAN_POINT('Ctrl Pts',(0.0326517920539688,-0.235002604092262,
-0.64856554051873));
#80513=CARTESIAN_POINT('Ctrl Pts',(0.0263442896189105,-0.235792983379444,
-0.648972092401514));
#80514=CARTESIAN_POINT('Ctrl Pts',(0.0177048424013525,-0.236524597525799,
-0.649537507771648));
#80515=CARTESIAN_POINT('Ctrl Pts',(0.0153939593854007,-0.236686231269615,
-0.649689563931334));
#80516=CARTESIAN_POINT('Ctrl Pts',(0.0116853925224909,-0.236891085300731,
-0.649935068895511));
#80517=CARTESIAN_POINT('Ctrl Pts',(0.0102890119420583,-0.236955841424199,
-0.650027844177806));
#80518=CARTESIAN_POINT('Ctrl Pts',(0.00739135622624884,-0.237064556770727,
-0.650221100073976));
#80519=CARTESIAN_POINT('Ctrl Pts',(0.00589007661193041,-0.237106606914802,
-0.65032163580469));
#80520=CARTESIAN_POINT('Ctrl Pts',(0.0023451099182259,-0.237172211847015,
-0.650560044518362));
#80521=CARTESIAN_POINT('Ctrl Pts',(0.00030134593148767,-0.237183613155478,
-0.650698289079158));
#80522=CARTESIAN_POINT('Ctrl Pts',(-0.00662944787624838,-0.237132699095051,
-0.651169931887045));
#80523=CARTESIAN_POINT('Ctrl Pts',(-0.0115140257062346,-0.236945748439082,
-0.651507131789606));
#80524=CARTESIAN_POINT('Ctrl Pts',(-0.0235319717630752,-0.236113305609175,
-0.652349115436499));
#80525=CARTESIAN_POINT('Ctrl Pts',(-0.0306482200249554,-0.235295383454555,
-0.652858545101209));
#80526=CARTESIAN_POINT('Ctrl Pts',(-0.0515773785350495,-0.23192428909589,
-0.654385705086018));
#80527=CARTESIAN_POINT('Ctrl Pts',(-0.0652123119607416,-0.228465379814004,
-0.655420086630226));
#80528=CARTESIAN_POINT('Ctrl Pts',(-0.0852700433744059,-0.221434103803698,
-0.656956059504935));
#80529=CARTESIAN_POINT('Ctrl Pts',(-0.0919674338717087,-0.218737410346294,
-0.657471028387694));
#80530=CARTESIAN_POINT('Ctrl Pts',(-0.100023740761862,-0.215057948624918,
-0.658084992788055));
#80531=CARTESIAN_POINT('Ctrl Pts',(-0.10150839749602,-0.214361180242974,
-0.658197896359277));
#80532=CARTESIAN_POINT('Ctrl Pts',(-0.103831569298598,-0.213241336199695,
-0.658374051223744));
#80533=CARTESIAN_POINT('Ctrl Pts',(-0.104674970217722,-0.212828599896492,
-0.658437894269272));
#80534=CARTESIAN_POINT('Ctrl Pts',(-0.106270291710927,-0.212036117764972,
-0.658558419102347));
#80535=CARTESIAN_POINT('Ctrl Pts',(-0.10702264465679,-0.211657373339644,
-0.65861515412681));
#80536=CARTESIAN_POINT('Ctrl Pts',(-0.108818387676643,-0.2107413493865,
-0.658750349768238));
#80537=CARTESIAN_POINT('Ctrl Pts',(-0.109859833910577,-0.210200320822271,
-0.658828578959192));
#80538=CARTESIAN_POINT('Ctrl Pts',(-0.11345639737131,-0.208297883409675,
-0.659098269207776));
#80539=CARTESIAN_POINT('Ctrl Pts',(-0.115990686519285,-0.206897377477604,
-0.659287478418883));
#80540=CARTESIAN_POINT('Ctrl Pts',(-0.122276027636513,-0.203272150498366,
-0.659756273393061));
#80541=CARTESIAN_POINT('Ctrl Pts',(-0.125992653494476,-0.200989675967165,
-0.66003305837453));
#80542=CARTESIAN_POINT('Ctrl Pts',(-0.144382831962948,-0.188985075673307,
-0.661411338882494));
#80543=CARTESIAN_POINT('Ctrl Pts',(-0.158004883305195,-0.177753415174447,
-0.662465008083218));
#80544=CARTESIAN_POINT('Ctrl Pts',(-0.176035409497053,-0.159161404786691,
-0.664081942404345));
#80545=CARTESIAN_POINT('Ctrl Pts',(-0.18149448785661,-0.152906988412833,
-0.664608077367209));
#80546=CARTESIAN_POINT('Ctrl Pts',(-0.188185156633312,-0.144377302101673,
-0.66531310005692));
#80547=CARTESIAN_POINT('Ctrl Pts',(-0.189723601015048,-0.142349615176432,
-0.665479810184046));
#80548=CARTESIAN_POINT('Ctrl Pts',(-0.192175986657686,-0.139006954004205,
-0.665753440965162));
#80549=CARTESIAN_POINT('Ctrl Pts',(-0.193109792681398,-0.137706756798118,
-0.665859588495997));
#80550=CARTESIAN_POINT('Ctrl Pts',(-0.194891057151493,-0.135172839099616,
-0.666065962731003));
#80551=CARTESIAN_POINT('Ctrl Pts',(-0.195740141373546,-0.133940350403645,
-0.66616612093219));
#80552=CARTESIAN_POINT('Ctrl Pts',(-0.197702763545825,-0.131032983914976,
-0.666401919341045));
#80553=CARTESIAN_POINT('Ctrl Pts',(-0.198806759563053,-0.12935183611636,
-0.666537908407954));
#80554=CARTESIAN_POINT('Ctrl Pts',(-0.202409960729904,-0.123709829521019,
-0.666993235027753));
#80555=CARTESIAN_POINT('Ctrl Pts',(-0.204813079676133,-0.11968922743183,
-0.667316025101611));
#80556=CARTESIAN_POINT('Ctrl Pts',(-0.210380587762926,-0.109715160684738,
-0.66811322386183));
#80557=CARTESIAN_POINT('Ctrl Pts',(-0.213413072176007,-0.10369308188169,
-0.668591649728554));
#80558=CARTESIAN_POINT('Ctrl Pts',(-0.221146560693454,-0.086554646524819,
-0.669943005404033));
#80559=CARTESIAN_POINT('Ctrl Pts',(-0.225261943314332,-0.0751966571714988,
-0.670827943183893));
#80560=CARTESIAN_POINT('Ctrl Pts',(-0.230594554077849,-0.0560309185231766,
-0.672275595529859));
#80561=CARTESIAN_POINT('Ctrl Pts',(-0.232318998884028,-0.0483860977031188,
-0.672841283419945));
#80562=CARTESIAN_POINT('Ctrl Pts',(-0.23416464690543,-0.0377821103525075,
-0.673599178279029));
#80563=CARTESIAN_POINT('Ctrl Pts',(-0.234613658122349,-0.0348855709440824,
-0.67380348000132));
#80564=CARTESIAN_POINT('Ctrl Pts',(-0.235172281465171,-0.0307806264262929,
-0.674088505595738));
#80565=CARTESIAN_POINT('Ctrl Pts',(-0.235326475929421,-0.029578688570418,
-0.674171417730161));
#80566=CARTESIAN_POINT('Ctrl Pts',(-0.235571977813158,-0.0275414203955394,
-0.674310973167934));
#80567=CARTESIAN_POINT('Ctrl Pts',(-0.235668069094306,-0.0267067008142211,
-0.674367874033798));
#80568=CARTESIAN_POINT('Ctrl Pts',(-0.235844305886976,-0.0251007016344489,
-0.674476797423961));
#80569=CARTESIAN_POINT('Ctrl Pts',(-0.235925107203615,-0.0243295227284101,
-0.674528858597173));
#80570=CARTESIAN_POINT('Ctrl Pts',(-0.236093302054964,-0.0226445566463216,
-0.674642106499908));
#80571=CARTESIAN_POINT('Ctrl Pts',(-0.236179176032279,-0.0217306257910065,
-0.674703210718419));
#80572=CARTESIAN_POINT('Ctrl Pts',(-0.236377821313897,-0.0194760413468157,
-0.674853207377661));
#80573=CARTESIAN_POINT('Ctrl Pts',(-0.236484497302592,-0.0181348649376064,
-0.674941789389455));
#80574=CARTESIAN_POINT('Ctrl Pts',(-0.236972764746139,-0.0112560792173358,
-0.675393144633294));
#80575=CARTESIAN_POINT('Ctrl Pts',(-0.237171311127635,-0.00570685717802064,
-0.675747402338223));
#80576=CARTESIAN_POINT('Ctrl Pts',(-0.23717494907381,-0.000155424694679885,
-0.676096452130946));
#80577=CARTESIAN_POINT('Ctrl Pts',(-0.237174948853082,-0.000155761157073058,
-0.676096430975656));
#80578=CARTESIAN_POINT('Ctrl Pts',(-0.237176131619272,0.00164521744310811,
-0.676209668702917));
#80579=CARTESIAN_POINT('Ctrl Pts',(-0.237156800878312,0.00344619272531007,
-0.6763223419202));
#80580=CARTESIAN_POINT('Ctrl Pts',(-0.236632262479393,0.0271514288203653,
-0.677799910882799));
#80581=CARTESIAN_POINT('Ctrl Pts',(-0.233114967187122,0.0488821808950842,
-0.679103892791132));
#80582=CARTESIAN_POINT('Ctrl Pts',(-0.225475340087641,0.0736829308826454,
-0.680768049409323));
#80583=CARTESIAN_POINT('Ctrl Pts',(-0.224187565790029,0.0775128089572374,
-0.681029881008752));
#80584=CARTESIAN_POINT('Ctrl Pts',(-0.222150985036203,0.0830935264079915,
-0.681419577313486));
#80585=CARTESIAN_POINT('Ctrl Pts',(-0.221477872125114,0.0848713502481855,
-0.681544959336536));
#80586=CARTESIAN_POINT('Ctrl Pts',(-0.220242232828114,0.0880200814149191,
-0.681769334959095));
#80587=CARTESIAN_POINT('Ctrl Pts',(-0.219688086723308,0.0893941845715376,
-0.681868044308226));
#80588=CARTESIAN_POINT('Ctrl Pts',(-0.218488931293419,0.0922892005166868,
-0.682077735640644));
#80589=CARTESIAN_POINT('Ctrl Pts',(-0.217840835400568,0.0938087406520756,
-0.682188817634891));
#80590=CARTESIAN_POINT('Ctrl Pts',(-0.216057395657699,0.0978720691405405,
-0.682488669923413));
#80591=CARTESIAN_POINT('Ctrl Pts',(-0.214893052349189,0.100402764109508,
-0.682678416226039));
#80592=CARTESIAN_POINT('Ctrl Pts',(-0.207670117940391,0.115400282809999,
-0.683821390903903));
#80593=CARTESIAN_POINT('Ctrl Pts',(-0.200573694635737,0.127334903380162,
-0.684810557140656));
#80594=CARTESIAN_POINT('Ctrl Pts',(-0.186601645312739,0.146741038340641,
-0.686548379433072));
#80595=CARTESIAN_POINT('Ctrl Pts',(-0.180212864392938,0.15451999834099,
-0.687286219524909));
#80596=CARTESIAN_POINT('Ctrl Pts',(-0.169734318855455,0.165741673566535,
-0.688397856163317));
#80597=CARTESIAN_POINT('Ctrl Pts',(-0.165990068450785,0.169491431897337,
-0.688778278300537));
#80598=CARTESIAN_POINT('Ctrl Pts',(-0.160464972112714,0.174665779451608,
-0.689312879864408));
#80599=CARTESIAN_POINT('Ctrl Pts',(-0.158784487460708,0.176194861345632,
-0.689472141933913));
#80600=CARTESIAN_POINT('Ctrl Pts',(-0.155799362502275,0.178833640589542,
-0.689748883834113));
#80601=CARTESIAN_POINT('Ctrl Pts',(-0.154504210802291,0.17995377636246,
-0.689866982724218));
#80602=CARTESIAN_POINT('Ctrl Pts',(-0.152461338841841,0.181682276015678,
-0.690050059905405));
#80603=CARTESIAN_POINT('Ctrl Pts',(-0.151721878280214,0.182300249569067,
-0.690115685402815));
#80604=CARTESIAN_POINT('Ctrl Pts',(-0.150337771614902,0.18344270390224,
-0.690237297219541));
#80605=CARTESIAN_POINT('Ctrl Pts',(-0.149694126168726,0.183968311996618,
-0.690293359573696));
#80606=CARTESIAN_POINT('Ctrl Pts',(-0.14821110017765,0.185166430862028,
-0.69042142577379));
#80607=CARTESIAN_POINT('Ctrl Pts',(-0.147369893469756,0.185836627026,-0.690493267371959));
#80608=CARTESIAN_POINT('Ctrl Pts',(-0.144764757480524,0.187883345862392,
-0.690713404002494));
#80609=CARTESIAN_POINT('Ctrl Pts',(-0.142985828835886,0.189240694085377,
-0.690860441850481));
#80610=CARTESIAN_POINT('Ctrl Pts',(-0.130517234159927,0.198478188423581,
-0.691870589540606));
#80611=CARTESIAN_POINT('Ctrl Pts',(-0.119200025047789,0.205474535221661,
-0.692685528778348));
#80612=CARTESIAN_POINT('Ctrl Pts',(-0.0969139759614693,0.216787395682156,
-0.694218519411117));
#80613=CARTESIAN_POINT('Ctrl Pts',(-0.08609487775866,0.221306899623514,
-0.694934605455638));
#80614=CARTESIAN_POINT('Ctrl Pts',(-0.0686238496959238,0.227129330944396,
-0.696094590288248));
#80615=CARTESIAN_POINT('Ctrl Pts',(-0.0621742311787725,0.228978859401097,
-0.696523336191721));
#80616=CARTESIAN_POINT('Ctrl Pts',(-0.0534293545572765,0.231089870871603,
-0.697110187416785));
#80617=CARTESIAN_POINT('Ctrl Pts',(-0.0511957778673838,0.231594939659332,
-0.697260540388271));
#80618=CARTESIAN_POINT('Ctrl Pts',(-0.04744093726038,0.232387033733086,
-0.697514239950016));
#80619=CARTESIAN_POINT('Ctrl Pts',(-0.0459235145597242,0.232691655616345,
-0.697617021929088));
#80620=CARTESIAN_POINT('Ctrl Pts',(-0.0435815719511394,0.233137999666587,
-0.697776085609751));
#80621=CARTESIAN_POINT('Ctrl Pts',(-0.0427590860370097,0.233290250153061,
-0.697832030395872));
#80622=CARTESIAN_POINT('Ctrl Pts',(-0.0419358257124646,0.233438144155607,
-0.69788811322923));
#80623=CARTESIAN_POINT('Ctrl Pts',(-0.0419358371735614,0.233438142096686,
-0.71773215975824));
#80624=CARTESIAN_POINT('Ctrl Pts',(-0.0497809610582963,0.232028810121706,
-0.717240407231273));
#80625=CARTESIAN_POINT('Ctrl Pts',(-0.0575534454763789,0.230224291883822,
-0.716753801969153));
#80626=CARTESIAN_POINT('Ctrl Pts',(-0.0777437884470259,0.224449250421988,
-0.715462294220634));
#80627=CARTESIAN_POINT('Ctrl Pts',(-0.0899463043198536,0.219843497183554,
-0.714652378345264));
#80628=CARTESIAN_POINT('Ctrl Pts',(-0.104290403395135,0.213034414205457,
-0.713623231945516));
#80629=CARTESIAN_POINT('Ctrl Pts',(-0.106849984504534,0.211762200464446,
-0.713436507906509));
#80630=CARTESIAN_POINT('Ctrl Pts',(-0.110865054017541,0.209675224037858,
-0.713138344505617));
#80631=CARTESIAN_POINT('Ctrl Pts',(-0.112336063979543,0.208890804653252,
-0.713027965765718));
#80632=CARTESIAN_POINT('Ctrl Pts',(-0.115095743069493,0.207381619634535,
-0.712818663123878));
#80633=CARTESIAN_POINT('Ctrl Pts',(-0.116386148092833,0.206660181450482,
-0.712719861125174));
#80634=CARTESIAN_POINT('Ctrl Pts',(-0.119296637216579,0.204997083302212,
-0.712494841744148));
#80635=CARTESIAN_POINT('Ctrl Pts',(-0.120912458625922,0.20404820218007,
-0.712368369180192));
#80636=CARTESIAN_POINT('Ctrl Pts',(-0.125092352936989,0.201526503145301,
-0.71203705987452));
#80637=CARTESIAN_POINT('Ctrl Pts',(-0.12763797860691,0.199923918561245,
-0.711831156067895));
#80638=CARTESIAN_POINT('Ctrl Pts',(-0.144989126303658,0.188534129067977,
-0.710398330320745));
#80639=CARTESIAN_POINT('Ctrl Pts',(-0.15868331935262,0.177161924747622,
-0.709111149375821));
#80640=CARTESIAN_POINT('Ctrl Pts',(-0.179634174439599,0.155368957725207,
-0.706904462847015));
#80641=CARTESIAN_POINT('Ctrl Pts',(-0.187565676274929,0.145695333283181,
-0.705994121694069));
#80642=CARTESIAN_POINT('Ctrl Pts',(-0.195812214687322,0.133840792063366,
-0.704988726080134));
#80643=CARTESIAN_POINT('Ctrl Pts',(-0.196905748387745,0.132226729162066,
-0.704854051504146));
#80644=CARTESIAN_POINT('Ctrl Pts',(-0.198532033526139,0.129761396000316,
-0.704651893581959));
#80645=CARTESIAN_POINT('Ctrl Pts',(-0.199079455958728,0.128919969499633,
-0.704583511755803));
#80646=CARTESIAN_POINT('Ctrl Pts',(-0.200069889246839,0.127376251390834,
-0.704459211648246));
#80647=CARTESIAN_POINT('Ctrl Pts',(-0.200514564652106,0.126675093865161,
-0.704403189354044));
#80648=CARTESIAN_POINT('Ctrl Pts',(-0.201522544378047,0.125067118944162,
-0.704275692053643));
#80649=CARTESIAN_POINT('Ctrl Pts',(-0.202083418431739,0.124158818606778,
-0.704204373731682));
#80650=CARTESIAN_POINT('Ctrl Pts',(-0.203821306968238,0.121301440608357,
-0.703982102936987));
#80651=CARTESIAN_POINT('Ctrl Pts',(-0.204976439902245,0.119339116326712,
-0.703832473244526));
#80652=CARTESIAN_POINT('Ctrl Pts',(-0.212561699531826,0.106018213238358,
-0.70283474663507));
#80653=CARTESIAN_POINT('Ctrl Pts',(-0.218073788449209,0.0941607532235971,
-0.70203302924614));
#80654=CARTESIAN_POINT('Ctrl Pts',(-0.226678090051916,0.0707789930563413,
-0.70050466134681));
#80655=CARTESIAN_POINT('Ctrl Pts',(-0.229933024046881,0.0593582772207219,
-0.699779855484976));
#80656=CARTESIAN_POINT('Ctrl Pts',(-0.23323330035082,0.0432988444536064,
-0.698747429124093));
#80657=CARTESIAN_POINT('Ctrl Pts',(-0.234018790889593,0.0388299380059672,
-0.69845888792319));
#80658=CARTESIAN_POINT('Ctrl Pts',(-0.235181894355,0.030881757958909,-0.697941394202021));
#80659=CARTESIAN_POINT('Ctrl Pts',(-0.235611580532224,0.0274114480724389,
-0.697714014523));
#80660=CARTESIAN_POINT('Ctrl Pts',(-0.236145818593704,0.0221442059688947,
-0.697366102018109));
#80661=CARTESIAN_POINT('Ctrl Pts',(-0.23630690264025,0.0203534017962825,
-0.697247330401912));
#80662=CARTESIAN_POINT('Ctrl Pts',(-0.236562873147734,0.0170926033191336,
-0.697030101135011));
#80663=CARTESIAN_POINT('Ctrl Pts',(-0.236664456661271,0.0156232143271007,
-0.696931857921645));
#80664=CARTESIAN_POINT('Ctrl Pts',(-0.236855074759771,0.012434542356552,
-0.69671785016859));
#80665=CARTESIAN_POINT('Ctrl Pts',(-0.236939088379264,0.0107150553093824,
-0.696601934500364));
#80666=CARTESIAN_POINT('Ctrl Pts',(-0.237119375959961,0.00596467357892588,
-0.69628021117362));
#80667=CARTESIAN_POINT('Ctrl Pts',(-0.237176249981581,0.00293270419723155,
-0.696073195639592));
#80668=CARTESIAN_POINT('Ctrl Pts',(-0.237173375069643,-0.0039267215022098,
-0.695600864395705));
#80669=CARTESIAN_POINT('Ctrl Pts',(-0.237079128968467,-0.00775324162117441,
-0.695334562375428));
#80670=CARTESIAN_POINT('Ctrl Pts',(-0.236460123592357,-0.0204210329279014,
-0.694443552130688));
#80671=CARTESIAN_POINT('Ctrl Pts',(-0.23553286031713,-0.029234452003265,
-0.693808094571009));
#80672=CARTESIAN_POINT('Ctrl Pts',(-0.232027304357261,-0.0508463405152379,
-0.692219132727626));
#80673=CARTESIAN_POINT('Ctrl Pts',(-0.228881506087228,-0.0635238651221662,
-0.691259090747293));
#80674=CARTESIAN_POINT('Ctrl Pts',(-0.222895001689386,-0.0812525098720437,
-0.689915947723244));
#80675=CARTESIAN_POINT('Ctrl Pts',(-0.22088802153123,-0.0865600686243203,
-0.689514018016929));
#80676=CARTESIAN_POINT('Ctrl Pts',(-0.218096355597563,-0.0932112264920674,
-0.689014758242921));
#80677=CARTESIAN_POINT('Ctrl Pts',(-0.217486401012915,-0.0946256770487317,
-0.688908846944395));
#80678=CARTESIAN_POINT('Ctrl Pts',(-0.216491349620017,-0.096872685689174,
-0.68874112913286));
#80679=CARTESIAN_POINT('Ctrl Pts',(-0.216115140610536,-0.0977090976504158,
-0.68867881808495));
#80680=CARTESIAN_POINT('Ctrl Pts',(-0.215380602657762,-0.0993171707701197,
-0.688559279495476));
#80681=CARTESIAN_POINT('Ctrl Pts',(-0.215022961774339,-0.100089112015394,
-0.688502015529004));
#80682=CARTESIAN_POINT('Ctrl Pts',(-0.214140212545222,-0.101967890829651,
-0.688362901099698));
#80683=CARTESIAN_POINT('Ctrl Pts',(-0.213610658090264,-0.103072636042486,
-0.688281317520654));
#80684=CARTESIAN_POINT('Ctrl Pts',(-0.211649654915818,-0.10708360739301,
-0.687985729717637));
#80685=CARTESIAN_POINT('Ctrl Pts',(-0.21016719184699,-0.109964673282344,
-0.687774595004255));
#80686=CARTESIAN_POINT('Ctrl Pts',(-0.198457035282409,-0.131620056804292,
-0.68618981993618));
#80687=CARTESIAN_POINT('Ctrl Pts',(-0.185791137629021,-0.148966148066146,
-0.684925302574473));
#80688=CARTESIAN_POINT('Ctrl Pts',(-0.165144446418681,-0.170440453499752,
-0.683066374212442));
#80689=CARTESIAN_POINT('Ctrl Pts',(-0.159001190135598,-0.176185229856029,
-0.682533581290394));
#80690=CARTESIAN_POINT('Ctrl Pts',(-0.150610429427199,-0.183234838187202,
-0.681820936514482));
#80691=CARTESIAN_POINT('Ctrl Pts',(-0.148628041200286,-0.184846454987654,
-0.681653613557027));
#80692=CARTESIAN_POINT('Ctrl Pts',(-0.145360461258616,-0.187416341160832,
-0.681379252808125));
#80693=CARTESIAN_POINT('Ctrl Pts',(-0.144090873772623,-0.188394183864958,
-0.681272996589062));
#80694=CARTESIAN_POINT('Ctrl Pts',(-0.14161763865643,-0.190259457206785,
-0.681066605371749));
#80695=CARTESIAN_POINT('Ctrl Pts',(-0.14041531253571,-0.191148519388809,
-0.680966540739044));
#80696=CARTESIAN_POINT('Ctrl Pts',(-0.137581413691669,-0.193202885525309,
-0.680731266241497));
#80697=CARTESIAN_POINT('Ctrl Pts',(-0.135943333132698,-0.194358972308561,
-0.680595711665435));
#80698=CARTESIAN_POINT('Ctrl Pts',(-0.130460587147331,-0.198125236627198,
-0.680143331100566));
#80699=CARTESIAN_POINT('Ctrl Pts',(-0.126554091645045,-0.200643043347481,
-0.67982311295567));
#80700=CARTESIAN_POINT('Ctrl Pts',(-0.116868907982918,-0.20648991825204,
-0.679033770493161));
#80701=CARTESIAN_POINT('Ctrl Pts',(-0.111019142644893,-0.209693025059665,
-0.678560733097515));
#80702=CARTESIAN_POINT('Ctrl Pts',(-0.0963130041397121,-0.216957573281092,
-0.677382369391234));
#80703=CARTESIAN_POINT('Ctrl Pts',(-0.0873264861444057,-0.220727999368955,
-0.67667121862558));
#80704=CARTESIAN_POINT('Ctrl Pts',(-0.0767708078064536,-0.224411026785209,
-0.675855343415898));
#80705=CARTESIAN_POINT('Ctrl Pts',(-0.075403057561884,-0.224874286686873,
-0.675750002718781));
#80706=CARTESIAN_POINT('Ctrl Pts',(-0.063836581913,-0.228674484062525,-0.674862673465194));
#80707=CARTESIAN_POINT('Ctrl Pts',(-0.0534252491664702,-0.231328603825695,
-0.674086164177664));
#80708=CARTESIAN_POINT('Ctrl Pts',(-0.0411805023556501,-0.233578881526921,
-0.673221892608352));
#80709=CARTESIAN_POINT('Ctrl Pts',(-0.0394887006923036,-0.233870841732882,
-0.673103559393579));
#80710=CARTESIAN_POINT('Ctrl Pts',(-0.0368407293192654,-0.23429825721371,
-0.672920183032073));
#80711=CARTESIAN_POINT('Ctrl Pts',(-0.0358866887351938,-0.234446280253622,
-0.672854485188488));
#80712=CARTESIAN_POINT('Ctrl Pts',(-0.0341886597303467,-0.234699127815619,
-0.672738245038672));
#80713=CARTESIAN_POINT('Ctrl Pts',(-0.0334450657983187,-0.234806244908847,
-0.672687579562099));
#80714=CARTESIAN_POINT('Ctrl Pts',(-0.031639065265474,-0.235057651669759,
-0.67256508935813));
#80715=CARTESIAN_POINT('Ctrl Pts',(-0.030576172226623,-0.235198273509777,
-0.672493468784139));
#80716=CARTESIAN_POINT('Ctrl Pts',(-0.0272283710684135,-0.235618112574036,
-0.672269255998134));
#80717=CARTESIAN_POINT('Ctrl Pts',(-0.024940252569674,-0.235871286780743,
-0.672118019671748));
#80718=CARTESIAN_POINT('Ctrl Pts',(-0.0125357968794163,-0.237061271821679,
-0.67130720664883));
#80719=CARTESIAN_POINT('Ctrl Pts',(-0.00236979563541106,-0.237380756664839,
-0.670675071047823));
#80720=CARTESIAN_POINT('Ctrl Pts',(0.02667528972997,-0.236426702984017,
-0.668885040097899));
#80721=CARTESIAN_POINT('Ctrl Pts',(0.0454205656265901,-0.233551008332624,
-0.667743562940171));
#80722=CARTESIAN_POINT('Ctrl Pts',(0.067214476873861,-0.227482030501407,
-0.666289018797446));
#80723=CARTESIAN_POINT('Ctrl Pts',(0.0707792206248311,-0.226398232287836,
-0.666047108111816));
#80724=CARTESIAN_POINT('Ctrl Pts',(0.0760663453928736,-0.22465370204087,
-0.665681531292506));
#80725=CARTESIAN_POINT('Ctrl Pts',(0.0778090522498146,-0.224056077380419,
-0.66555991619019));
#80726=CARTESIAN_POINT('Ctrl Pts',(0.0809347093315071,-0.222943335459164,
-0.665339686154698));
#80727=CARTESIAN_POINT('Ctrl Pts',(0.0823201623337703,-0.222435493357917,
-0.665241315814294));
#80728=CARTESIAN_POINT('Ctrl Pts',(0.0852798943336163,-0.221319155664848,
-0.665029503822648));
#80729=CARTESIAN_POINT('Ctrl Pts',(0.0868525896664512,-0.220706720457173,
-0.664915935210272));
#80730=CARTESIAN_POINT('Ctrl Pts',(0.091161461730791,-0.218975583762136,
-0.664601894799887));
#80731=CARTESIAN_POINT('Ctrl Pts',(0.0938833887148409,-0.217822465192704,
-0.664400280638196));
#80732=CARTESIAN_POINT('Ctrl Pts',(0.0999136342908254,-0.215133784179527,
-0.663946145673182));
#80733=CARTESIAN_POINT('Ctrl Pts',(0.10320945973299,-0.213572199422351,
-0.663692800221025));
#80734=CARTESIAN_POINT('Ctrl Pts',(0.11378908353738,-0.208257419717737,
-0.662862591075651));
#80735=CARTESIAN_POINT('Ctrl Pts',(0.120914175099086,-0.204202958413524,
-0.662276542144161));
#80736=CARTESIAN_POINT('Ctrl Pts',(0.142297045516728,-0.190523261239037,
-0.660438921805837));
#80737=CARTESIAN_POINT('Ctrl Pts',(0.155729030114944,-0.179711021292023,
-0.659165269547456));
#80738=CARTESIAN_POINT('Ctrl Pts',(0.170111737662663,-0.165299756541713,
-0.657728510122017));
#80739=CARTESIAN_POINT('Ctrl Pts',(0.17230418013173,-0.163013142683692,
-0.657507333299815));
#80740=CARTESIAN_POINT('Ctrl Pts',(0.175296570385308,-0.159764368448068,
-0.657203212197398));
#80741=CARTESIAN_POINT('Ctrl Pts',(0.176135609654607,-0.158838874959991,
-0.657117684094636));
#80742=CARTESIAN_POINT('Ctrl Pts',(0.177531046905761,-0.157274997801759,
-0.656975071066078));
#80743=CARTESIAN_POINT('Ctrl Pts',(0.178091401725699,-0.156640193654241,
-0.656917701760471));
#80744=CARTESIAN_POINT('Ctrl Pts',(0.179244294060752,-0.15531994246384,
-0.656799479952646));
#80745=CARTESIAN_POINT('Ctrl Pts',(0.179836321832816,-0.154634080651831,
-0.656738663496734));
#80746=CARTESIAN_POINT('Ctrl Pts',(0.181391283892511,-0.15281165422978,
-0.656578589403994));
#80747=CARTESIAN_POINT('Ctrl Pts',(0.182347484216062,-0.151669360193929,
-0.656479804818328));
#80748=CARTESIAN_POINT('Ctrl Pts',(0.186916659113732,-0.146105263366896,
-0.656005629259628));
#80749=CARTESIAN_POINT('Ctrl Pts',(0.190380220469429,-0.141562596827126,
-0.655639608548447));
#80750=CARTESIAN_POINT('Ctrl Pts',(0.201233263612913,-0.126208338461148,
-0.654453832250033));
#80751=CARTESIAN_POINT('Ctrl Pts',(0.207892159793196,-0.11490980851155,
-0.653660126171383));
#80752=CARTESIAN_POINT('Ctrl Pts',(0.219333967335642,-0.0912109707662079,
-0.652041796883372));
#80753=CARTESIAN_POINT('Ctrl Pts',(0.224076500957956,-0.0788447051066105,
-0.651219416223988));
#80754=CARTESIAN_POINT('Ctrl Pts',(0.228538139955312,-0.0634823452933401,
-0.650181677229295));
#80755=CARTESIAN_POINT('Ctrl Pts',(0.229265604869487,-0.0608027215825348,
-0.650000171513463));
#80756=CARTESIAN_POINT('Ctrl Pts',(0.230350043845137,-0.0565115876114314,
-0.649708414154583));
#80757=CARTESIAN_POINT('Ctrl Pts',(0.230737541783148,-0.0549080031897362,
-0.649599144672579));
#80758=CARTESIAN_POINT('Ctrl Pts',(0.231441221123417,-0.051856887477658,
-0.649390721187275));
#80759=CARTESIAN_POINT('Ctrl Pts',(0.231760630050444,-0.0504101755747332,
-0.649291675901047));
#80760=CARTESIAN_POINT('Ctrl Pts',(0.232459409331316,-0.047098058220372,
-0.64906437461256));
#80761=CARTESIAN_POINT('Ctrl Pts',(0.232829913564717,-0.0452309082106214,
-0.648935843310124));
#80762=CARTESIAN_POINT('Ctrl Pts',(0.233919441232704,-0.0393716734037575,
-0.648531170491749));
#80763=CARTESIAN_POINT('Ctrl Pts',(0.23455852191895,-0.0353656605317828,
-0.648252548093306));
#80764=CARTESIAN_POINT('Ctrl Pts',(0.236472466262991,-0.0210108475294014,
-0.647246683151982));
#80765=CARTESIAN_POINT('Ctrl Pts',(0.237167278972143,-0.0105979302036642,
-0.646502588272292));
#80766=CARTESIAN_POINT('Ctrl Pts',(0.237188334714832,0.0180657516161505,
-0.644425580965743));
#80767=CARTESIAN_POINT('Ctrl Pts',(0.235097651825952,0.0362466276559837,
-0.643072523006146));
#80768=CARTESIAN_POINT('Ctrl Pts',(0.230437222458539,0.0561748729503284,
-0.641642806018916));
#80769=CARTESIAN_POINT('Ctrl Pts',(0.229900148569626,0.0583339731404771,
-0.641488710495671));
#80770=CARTESIAN_POINT('Ctrl Pts',(0.22906301165779,0.0615080160677536,
-0.641263682237236));
#80771=CARTESIAN_POINT('Ctrl Pts',(0.228786428497264,0.062528950040999,
-0.641191533018034));
#80772=CARTESIAN_POINT('Ctrl Pts',(0.228280681744097,0.0643474906123157,
-0.641063472246041));
#80773=CARTESIAN_POINT('Ctrl Pts',(0.228054152340937,0.0651457816736615,
-0.641007417178605));
#80774=CARTESIAN_POINT('Ctrl Pts',(0.22754206427591,0.0669149735573436,
-0.640883543102224));
#80775=CARTESIAN_POINT('Ctrl Pts',(0.227254477446639,0.0678852507958265,
-0.640815840694982));
#80776=CARTESIAN_POINT('Ctrl Pts',(0.22638298457389,0.0707579312079799,
-0.640616008007378));
#80777=CARTESIAN_POINT('Ctrl Pts',(0.22578132051995,0.0726549136375739,
-0.640484847731503));
#80778=CARTESIAN_POINT('Ctrl Pts',(0.221873288167833,0.0844588710812766,
-0.639672402924839));
#80779=CARTESIAN_POINT('Ctrl Pts',(0.217939021690352,0.0941471862273387,
-0.639021682597547));
#80780=CARTESIAN_POINT('Ctrl Pts',(0.205368938778352,0.120050599719358,
-0.637247352033516));
#80781=CARTESIAN_POINT('Ctrl Pts',(0.195472413233766,0.13556931214982,-0.636139691031507));
#80782=CARTESIAN_POINT('Ctrl Pts',(0.181484080917818,0.152741545198905,
-0.634721382224162));
#80783=CARTESIAN_POINT('Ctrl Pts',(0.179011082511387,0.155632519264186,
-0.634475376237373));
#80784=CARTESIAN_POINT('Ctrl Pts',(0.175210457091288,0.159865033102803,
-0.634103317586575));
#80785=CARTESIAN_POINT('Ctrl Pts',(0.173934535455955,0.16125231819046,-0.63397937597583));
#80786=CARTESIAN_POINT('Ctrl Pts',(0.171692310623751,0.163632669259151,
-0.633763121960138));
#80787=CARTESIAN_POINT('Ctrl Pts',(0.170733576172517,0.164632760426267,
-0.633671133465988));
#80788=CARTESIAN_POINT('Ctrl Pts',(0.168711424152924,0.166705480475458,
-0.633478062703468));
#80789=CARTESIAN_POINT('Ctrl Pts',(0.16764641503315,0.167776462011229,-0.633376913412475));
#80790=CARTESIAN_POINT('Ctrl Pts',(0.165079425871609,0.17030900047167,-0.633134331201958));
#80791=CARTESIAN_POINT('Ctrl Pts',(0.163568182593125,0.171760943294273,
-0.632992489780897));
#80792=CARTESIAN_POINT('Ctrl Pts',(0.158218673777876,0.176765910200489,
-0.6324936098271));
#80793=CARTESIAN_POINT('Ctrl Pts',(0.154282539011918,0.180211615868024,
-0.632132145934058));
#80794=CARTESIAN_POINT('Ctrl Pts',(0.144123526002445,0.188527954813937,
-0.631212341802383));
#80795=CARTESIAN_POINT('Ctrl Pts',(0.137765448175933,0.193222776378575,
-0.630648132597597));
#80796=CARTESIAN_POINT('Ctrl Pts',(0.118612623209255,0.205938788591801,
-0.628985964176629));
#80797=CARTESIAN_POINT('Ctrl Pts',(0.105272048381554,0.21306695670932,-0.627871504673812));
#80798=CARTESIAN_POINT('Ctrl Pts',(0.086527055803709,0.220889796031191,
-0.626417135630659));
#80799=CARTESIAN_POINT('Ctrl Pts',(0.0816438535334476,0.222740934141769,
-0.626048074958132));
#80800=CARTESIAN_POINT('Ctrl Pts',(0.0752866581696856,0.224913629020329,
-0.625583407315999));
#80801=CARTESIAN_POINT('Ctrl Pts',(0.0738655759217275,0.225384334859567,
-0.625480535055415));
#80802=CARTESIAN_POINT('Ctrl Pts',(0.0715758433478631,0.226118780816097,
-0.625316486020974));
#80803=CARTESIAN_POINT('Ctrl Pts',(0.0707099969692648,0.226391035129728,
-0.625254840991053));
#80804=CARTESIAN_POINT('Ctrl Pts',(0.0690247620257171,0.226910324144542,
-0.625135641701001));
#80805=CARTESIAN_POINT('Ctrl Pts',(0.0682055703903536,0.227157903607117,
-0.625078059468311));
#80806=CARTESIAN_POINT('Ctrl Pts',(0.0661844373101452,0.227756819698458,
-0.624936839032766));
#80807=CARTESIAN_POINT('Ctrl Pts',(0.0649809966951789,0.228103088320623,
-0.624853487470422));
#80808=CARTESIAN_POINT('Ctrl Pts',(0.0604674581817824,0.229363158416313,
-0.624543422911201));
#80809=CARTESIAN_POINT('Ctrl Pts',(0.0571402086120012,0.230214620378768,
-0.624319959093754));
#80810=CARTESIAN_POINT('Ctrl Pts',(0.0483776114019962,0.232255316823351,
-0.623741924689744));
#80811=CARTESIAN_POINT('Ctrl Pts',(0.0429167050884711,0.233326145086436,
-0.623392109630557));
#80812=CARTESIAN_POINT('Ctrl Pts',(0.0274435196089473,0.235798566131327,
-0.622417597690498));
#80813=CARTESIAN_POINT('Ctrl Pts',(0.017372204448269,0.236753730539024,
-0.621802360808144));
#80814=CARTESIAN_POINT('Ctrl Pts',(-0.00611972685676392,0.237474197682057,
-0.620357482006399));
#80815=CARTESIAN_POINT('Ctrl Pts',(-0.0195188929546864,0.236749640504096,
-0.619524916046828));
#80816=CARTESIAN_POINT('Ctrl Pts',(-0.0355422385575826,0.234513292344952,
-0.618475492117298));
#80817=CARTESIAN_POINT('Ctrl Pts',(-0.0382930840154859,0.234079844637703,
-0.61829346440237));
#80818=CARTESIAN_POINT('Ctrl Pts',(-0.0413357597826485,0.233545345668206,
-0.61808983353491));
#80819=CARTESIAN_POINT('Ctrl Pts',(-0.0416358457657131,0.233492033835083,
-0.618069725516726));
#80820=CARTESIAN_POINT('Ctrl Pts',(-0.0419358257187832,0.233438144154472,
-0.618049599588275));
#80821=CARTESIAN_POINT('Origin',(0.,0.,-1.7456589891905));
#80822=CARTESIAN_POINT('',(-0.0419358198037385,0.233438145217075,-0.498265075600824));
#80823=CARTESIAN_POINT('',(-0.0419358519811599,0.233438139436584,-0.517821408604163));
#80824=CARTESIAN_POINT('',(-0.0419358257166344,0.233438144154858,-1.7456589891905));
#80825=CARTESIAN_POINT('Ctrl Pts',(-0.0419358198037385,0.233438145217075,
-0.498265075600824));
#80826=CARTESIAN_POINT('Ctrl Pts',(-0.0375883549594239,0.234219142265114,
-0.498582125924067));
#80827=CARTESIAN_POINT('Ctrl Pts',(-0.0332186597349509,0.234878765261937,
-0.498896098541358));
#80828=CARTESIAN_POINT('Ctrl Pts',(-0.0265571725459339,0.235694609176903,
-0.499365299141105));
#80829=CARTESIAN_POINT('Ctrl Pts',(-0.024278510161308,0.23594021937747,
-0.499524127877175));
#80830=CARTESIAN_POINT('Ctrl Pts',(-0.0209307484076507,0.23625204797198,
-0.499754693432862));
#80831=CARTESIAN_POINT('Ctrl Pts',(-0.0198642672782424,0.236344108021554,
-0.499827730419059));
#80832=CARTESIAN_POINT('Ctrl Pts',(-0.0180482770250548,0.236488487485063,
-0.499951352910418));
#80833=CARTESIAN_POINT('Ctrl Pts',(-0.0172990963333227,0.23654447011165,
-0.500002136128038));
#80834=CARTESIAN_POINT('Ctrl Pts',(-0.01558486823416,0.236664378022562,
-0.500117833281334));
#80835=CARTESIAN_POINT('Ctrl Pts',(-0.0146196822255146,0.236725961645799,
-0.500182617302202));
#80836=CARTESIAN_POINT('Ctrl Pts',(-0.01193345735436,0.236880864072485,
-0.500361988976412));
#80837=CARTESIAN_POINT('Ctrl Pts',(-0.0102116975495199,0.236961331919338,
-0.500475897940956));
#80838=CARTESIAN_POINT('Ctrl Pts',(0.00296514757714645,0.237433270247909,
-0.501340594883976));
#80839=CARTESIAN_POINT('Ctrl Pts',(0.0144357251006429,0.23701272044814,
-0.50205289783394));
#80840=CARTESIAN_POINT('Ctrl Pts',(0.0345366386813281,0.234810301773894,
-0.503297368493959));
#80841=CARTESIAN_POINT('Ctrl Pts',(0.0431815134247895,0.233375263829393,
-0.503831327322732));
#80842=CARTESIAN_POINT('Ctrl Pts',(0.0592174646790345,0.229791597463751,
-0.504845784942641));
#80843=CARTESIAN_POINT('Ctrl Pts',(0.066621554414768,0.227755223370391,
-0.505324091005131));
#80844=CARTESIAN_POINT('Ctrl Pts',(0.0772386537588829,0.224273085124907,
-0.506034857091523));
#80845=CARTESIAN_POINT('Ctrl Pts',(0.0805390933980615,0.223109118840424,
-0.506259383769652));
#80846=CARTESIAN_POINT('Ctrl Pts',(0.086490611084208,0.220860930981155,
-0.506671717218466));
#80847=CARTESIAN_POINT('Ctrl Pts',(0.0891501328898553,0.21980088557117,
-0.506858740091548));
#80848=CARTESIAN_POINT('Ctrl Pts',(0.0933280935790383,0.218047313802549,
-0.50715729059242));
#80849=CARTESIAN_POINT('Ctrl Pts',(0.0948595716735321,0.217385430814567,
-0.507267753223869));
#80850=CARTESIAN_POINT('Ctrl Pts',(0.0977349915773449,0.216106544497265,
-0.50747715981706));
#80851=CARTESIAN_POINT('Ctrl Pts',(0.0990803997808114,0.215493019289291,
-0.50757598119883));
#80852=CARTESIAN_POINT('Ctrl Pts',(0.102116864171814,0.214073901072198,
-0.507800969348095));
#80853=CARTESIAN_POINT('Ctrl Pts',(0.10380427292183,0.213260783179708,-0.507927390576691));
#80854=CARTESIAN_POINT('Ctrl Pts',(0.108172770581271,0.211091588875938,
-0.508258407020709));
#80855=CARTESIAN_POINT('Ctrl Pts',(0.11083796344327,0.20970443871449,-0.508464065781227));
#80856=CARTESIAN_POINT('Ctrl Pts',(0.129099793055952,0.199754335158907,
-0.509899680948459));
#80857=CARTESIAN_POINT('Ctrl Pts',(0.143713405327172,0.189511966330684,
-0.511190243030281));
#80858=CARTESIAN_POINT('Ctrl Pts',(0.166277594503469,0.169574842144839,
-0.513388153288189));
#80859=CARTESIAN_POINT('Ctrl Pts',(0.174863980731367,0.1607062986969,-0.514286391851252));
#80860=CARTESIAN_POINT('Ctrl Pts',(0.184015391639358,0.149647676612415,
-0.515286755274764));
#80861=CARTESIAN_POINT('Ctrl Pts',(0.185288000276779,0.148069068725514,
-0.515426932016381));
#80862=CARTESIAN_POINT('Ctrl Pts',(0.187169976343504,0.1456723044142,-0.515635614672604));
#80863=CARTESIAN_POINT('Ctrl Pts',(0.187794529194794,0.144866266670738,
-0.515705104799717));
#80864=CARTESIAN_POINT('Ctrl Pts',(0.188917871590798,0.143397025590746,
-0.515830487131399));
#80865=CARTESIAN_POINT('Ctrl Pts',(0.189418393817325,0.142735213898974,
-0.515886494974548));
#80866=CARTESIAN_POINT('Ctrl Pts',(0.190544234189313,0.141230227953549,
-0.516012806368266));
#80867=CARTESIAN_POINT('Ctrl Pts',(0.191167438408812,0.140385515873453,
-0.516082966066488));
#80868=CARTESIAN_POINT('Ctrl Pts',(0.193068497315001,0.137772621171741,
-0.516297828033628));
#80869=CARTESIAN_POINT('Ctrl Pts',(0.194327622094212,0.135990867039419,
-0.516441330344064));
#80870=CARTESIAN_POINT('Ctrl Pts',(0.206000307951497,0.118979900380611,
-0.517785796782713));
#80871=CARTESIAN_POINT('Ctrl Pts',(0.214629547991921,0.102599713274845,
-0.518892390619855));
#80872=CARTESIAN_POINT('Ctrl Pts',(0.225780245552282,0.0737021693525357,
-0.520800049852848));
#80873=CARTESIAN_POINT('Ctrl Pts',(0.229354922309966,0.0616846028405787,
-0.52158114330555));
#80874=CARTESIAN_POINT('Ctrl Pts',(0.232530606303196,0.0467854239757479,
-0.522570002945124));
#80875=CARTESIAN_POINT('Ctrl Pts',(0.233051147508421,0.0441193882974078,
-0.522747659297159));
#80876=CARTESIAN_POINT('Ctrl Pts',(0.233811863977681,0.0398330684480232,
-0.52303471191078));
#80877=CARTESIAN_POINT('Ctrl Pts',(0.234081252256196,0.0382181657660059,
-0.523143182460735));
#80878=CARTESIAN_POINT('Ctrl Pts',(0.234563050249881,0.0351334762793155,
-0.523351049241446));
#80879=CARTESIAN_POINT('Ctrl Pts',(0.234778417793315,0.0336642252858814,
-0.523450346847231));
#80880=CARTESIAN_POINT('Ctrl Pts',(0.235237407553536,0.0303140205149874,
-0.523677470688439));
#80881=CARTESIAN_POINT('Ctrl Pts',(0.235472289624631,0.028431992692877,
-0.523805565071687));
#80882=CARTESIAN_POINT('Ctrl Pts',(0.236037995425773,0.0234097251846036,
-0.524148817374211));
#80883=CARTESIAN_POINT('Ctrl Pts',(0.236328712864905,0.0202654467845767,
-0.524365203284477));
#80884=CARTESIAN_POINT('Ctrl Pts',(0.238088962274773,-0.00406197373877007,
-0.526051507546298));
#80885=CARTESIAN_POINT('Ctrl Pts',(0.236769984116047,-0.0253471746040464,
-0.527610539026501));
#80886=CARTESIAN_POINT('Ctrl Pts',(0.231422192653109,-0.0522951858488935,
-0.529607266595906));
#80887=CARTESIAN_POINT('Ctrl Pts',(0.229964238286799,-0.058373595532827,
-0.530058198019026));
#80888=CARTESIAN_POINT('Ctrl Pts',(0.227581831603811,-0.066819727901037,
-0.530679967620756));
#80889=CARTESIAN_POINT('Ctrl Pts',(0.226856966191137,-0.0692407691678647,
-0.53085761864426));
#80890=CARTESIAN_POINT('Ctrl Pts',(0.225511066207966,-0.0734878010213719,
-0.531167711359621));
#80891=CARTESIAN_POINT('Ctrl Pts',(0.224906204401071,-0.0753186410947042,
-0.531300875005119));
#80892=CARTESIAN_POINT('Ctrl Pts',(0.223953934343624,-0.0780872277014383,
-0.531501251890974));
#80893=CARTESIAN_POINT('Ctrl Pts',(0.223622828849311,-0.0790304393703134,
-0.531569340514381));
#80894=CARTESIAN_POINT('Ctrl Pts',(0.223005606492748,-0.0807537642648298,
-0.531693384051082));
#80895=CARTESIAN_POINT('Ctrl Pts',(0.222721348406415,-0.0815344833431992,
-0.531749439668476));
#80896=CARTESIAN_POINT('Ctrl Pts',(0.222060425609967,-0.0833204675690925,
-0.531877364399071));
#80897=CARTESIAN_POINT('Ctrl Pts',(0.221681032699646,-0.084324686719036,
-0.53194907271531));
#80898=CARTESIAN_POINT('Ctrl Pts',(0.220464454834838,-0.0874798958991241,
-0.532173783637711));
#80899=CARTESIAN_POINT('Ctrl Pts',(0.219602653408803,-0.089621334609479,
-0.532325422142099));
#80900=CARTESIAN_POINT('Ctrl Pts',(0.21415101443046,-0.102616723749072,
-0.533242294387226));
#80901=CARTESIAN_POINT('Ctrl Pts',(0.208788204351879,-0.113130023458433,
-0.533970138933407));
#80902=CARTESIAN_POINT('Ctrl Pts',(0.196048695235886,-0.134086300132742,
-0.535476355091687));
#80903=CARTESIAN_POINT('Ctrl Pts',(0.188566378778727,-0.144419277645282,
-0.536252143095314));
#80904=CARTESIAN_POINT('Ctrl Pts',(0.175723333456434,-0.159444999330548,
-0.537494995589133));
#80905=CARTESIAN_POINT('Ctrl Pts',(0.170920926674716,-0.16458256349757,
-0.537943706370263));
#80906=CARTESIAN_POINT('Ctrl Pts',(0.164235279476827,-0.171126168016622,
-0.538553695224271));
#80907=CARTESIAN_POINT('Ctrl Pts',(0.162548954310412,-0.172728773598101,
-0.538706382941143));
#80908=CARTESIAN_POINT('Ctrl Pts',(0.159696518283608,-0.17536083056381,
-0.538962910933206));
#80909=CARTESIAN_POINT('Ctrl Pts',(0.15854334015026,-0.176404104110063,
-0.539066158197234));
#80910=CARTESIAN_POINT('Ctrl Pts',(0.156254269792768,-0.178434436354531,
-0.539270257360314));
#80911=CARTESIAN_POINT('Ctrl Pts',(0.15511907661864,-0.17942217475756,-0.539371074063216));
#80912=CARTESIAN_POINT('Ctrl Pts',(0.152341973058737,-0.181792494464919,
-0.539616795024525));
#80913=CARTESIAN_POINT('Ctrl Pts',(0.150690569890604,-0.183163695690997,
-0.539762153255346));
#80914=CARTESIAN_POINT('Ctrl Pts',(0.144971382117922,-0.187782782379225,
-0.540263138158497));
#80915=CARTESIAN_POINT('Ctrl Pts',(0.140815663005643,-0.190918874807781,
-0.540623091915124));
#80916=CARTESIAN_POINT('Ctrl Pts',(0.122462669202594,-0.203843535584079,
-0.542196497947033));
#80917=CARTESIAN_POINT('Ctrl Pts',(0.107325918587912,-0.212203385980076,
-0.543458867873501));
#80918=CARTESIAN_POINT('Ctrl Pts',(0.0848168176051991,-0.2216061768329,
-0.54523607730703));
#80919=CARTESIAN_POINT('Ctrl Pts',(0.078091824737247,-0.224064432010551,
-0.545754643894827));
#80920=CARTESIAN_POINT('Ctrl Pts',(0.0686417217721561,-0.227041543815893,
-0.546458452923269));
#80921=CARTESIAN_POINT('Ctrl Pts',(0.0660035482354762,-0.227822478254188,
-0.546652301406675));
#80922=CARTESIAN_POINT('Ctrl Pts',(0.0613696016778201,-0.229106930487794,
-0.546987550567844));
#80923=CARTESIAN_POINT('Ctrl Pts',(0.059379783949287,-0.229630693895293,
-0.547129836055955));
#80924=CARTESIAN_POINT('Ctrl Pts',(0.0563882120447176,-0.230376652416537,
-0.5473410078229));
#80925=CARTESIAN_POINT('Ctrl Pts',(0.0553914811282593,-0.230618334815579,
-0.547410912106422));
#80926=CARTESIAN_POINT('Ctrl Pts',(0.0535856686995562,-0.231043816251955,
-0.547536701953626));
#80927=CARTESIAN_POINT('Ctrl Pts',(0.0527771653459403,-0.231229841904709,
-0.547592707521551));
#80928=CARTESIAN_POINT('Ctrl Pts',(0.0509497327318144,-0.231640224902985,
-0.547718594588154));
#80929=CARTESIAN_POINT('Ctrl Pts',(0.049930283151621,-0.231862105539919,
-0.547788336837096));
#80930=CARTESIAN_POINT('Ctrl Pts',(0.046807390723548,-0.232520242965561,
-0.548000590780165));
#80931=CARTESIAN_POINT('Ctrl Pts',(0.0446993908286672,-0.232934669953599,
-0.548141944210076));
#80932=CARTESIAN_POINT('Ctrl Pts',(0.0274407459353899,-0.236084741458193,
-0.549285753559833));
#80933=CARTESIAN_POINT('Ctrl Pts',(0.0120601726350038,-0.237368245572755,
-0.550222132516388));
#80934=CARTESIAN_POINT('Ctrl Pts',(-0.0185666797360126,-0.236937158791131,
-0.552100953068818));
#80935=CARTESIAN_POINT('Ctrl Pts',(-0.0337373252665069,-0.235256567050508,
-0.553039736109136));
#80936=CARTESIAN_POINT('Ctrl Pts',(-0.0515073272439723,-0.231533045447863,
-0.554215673175061));
#80937=CARTESIAN_POINT('Ctrl Pts',(-0.0543619616769597,-0.230879474600708,
-0.554406876652346));
#80938=CARTESIAN_POINT('Ctrl Pts',(-0.0588362220554446,-0.229767511754084,
-0.554710558223767));
#80939=CARTESIAN_POINT('Ctrl Pts',(-0.060464379537721,-0.229344433212693,
-0.554821906503719));
#80940=CARTESIAN_POINT('Ctrl Pts',(-0.0635131079695817,-0.228517497157275,
-0.555032054984985));
#80941=CARTESIAN_POINT('Ctrl Pts',(-0.0649346817345278,-0.228117619507407,
-0.555130722334271));
#80942=CARTESIAN_POINT('Ctrl Pts',(-0.0681301118843269,-0.227186480843713,
-0.555354085823322));
#80943=CARTESIAN_POINT('Ctrl Pts',(-0.0699016497940442,-0.226647674248373,
-0.555479021931647));
#80944=CARTESIAN_POINT('Ctrl Pts',(-0.0744605875897065,-0.225202557562395,
-0.555803477752482));
#80945=CARTESIAN_POINT('Ctrl Pts',(-0.0772377498396402,-0.224265244087222,
-0.556003992587263));
#80946=CARTESIAN_POINT('Ctrl Pts',(-0.0974639087437562,-0.217018513151767,
-0.557486028829603));
#80947=CARTESIAN_POINT('Ctrl Pts',(-0.114133369744747,-0.208733253629731,
-0.558834304664219));
#80948=CARTESIAN_POINT('Ctrl Pts',(-0.139493979346946,-0.192175011021335,
-0.56104463700019));
#80949=CARTESIAN_POINT('Ctrl Pts',(-0.148835034916867,-0.185035115594045,
-0.561898553909415));
#80950=CARTESIAN_POINT('Ctrl Pts',(-0.15910640261384,-0.175900953603726,
-0.562856191099542));
#80951=CARTESIAN_POINT('Ctrl Pts',(-0.16058634673467,-0.174550905855101,
-0.562994642183365));
#80952=CARTESIAN_POINT('Ctrl Pts',(-0.162790040343816,-0.172488878325497,
-0.563201285045851));
#80953=CARTESIAN_POINT('Ctrl Pts',(-0.16352657188922,-0.171790776128469,
-0.563270433751032));
#80954=CARTESIAN_POINT('Ctrl Pts',(-0.164857309801192,-0.1705131574164,
-0.56339548399767));
#80955=CARTESIAN_POINT('Ctrl Pts',(-0.165452971114631,-0.169935234259086,
-0.563451497563454));
#80956=CARTESIAN_POINT('Ctrl Pts',(-0.166799058831083,-0.168615444085486,
-0.563578175788218));
#80957=CARTESIAN_POINT('Ctrl Pts',(-0.167547580644793,-0.167871684142795,
-0.563648692669994));
#80958=CARTESIAN_POINT('Ctrl Pts',(-0.16984864201145,-0.165554538270222,
-0.563865801583666));
#80959=CARTESIAN_POINT('Ctrl Pts',(-0.171384219948038,-0.163964375233955,
-0.564011157143056));
#80960=CARTESIAN_POINT('Ctrl Pts',(-0.182803540994591,-0.151803391812325,
-0.565097882627663));
#80961=CARTESIAN_POINT('Ctrl Pts',(-0.191724735420941,-0.140367884275242,
-0.565981452779055));
#80962=CARTESIAN_POINT('Ctrl Pts',(-0.208254055294894,-0.114637119904861,
-0.567856873775612));
#80963=CARTESIAN_POINT('Ctrl Pts',(-0.215555498941033,-0.100235534255107,
-0.568846493988605));
#80964=CARTESIAN_POINT('Ctrl Pts',(-0.222383403021873,-0.082498606103918,
-0.570077812052136));
#80965=CARTESIAN_POINT('Ctrl Pts',(-0.22337588701495,-0.0797722373792972,
-0.57026728620456));
#80966=CARTESIAN_POINT('Ctrl Pts',(-0.224862561752073,-0.0754428233801306,
-0.570568845477473));
#80967=CARTESIAN_POINT('Ctrl Pts',(-0.225390206946424,-0.0738515107999818,
-0.570679827795996));
#80968=CARTESIAN_POINT('Ctrl Pts',(-0.226351040965419,-0.0708475113464099,
-0.57088966596689));
#80969=CARTESIAN_POINT('Ctrl Pts',(-0.226787986780161,-0.0694361036690015,
-0.570988393188257));
#80970=CARTESIAN_POINT('Ctrl Pts',(-0.227745231768381,-0.0662385893067274,
-0.571212409527991));
#80971=CARTESIAN_POINT('Ctrl Pts',(-0.228257755312397,-0.0644502762147806,
-0.571337944457645));
#80972=CARTESIAN_POINT('Ctrl Pts',(-0.229531271061465,-0.0598008424156719,
-0.571665040179902));
#80973=CARTESIAN_POINT('Ctrl Pts',(-0.230259803064214,-0.0569312468706134,
-0.571867623375197));
#80974=CARTESIAN_POINT('Ctrl Pts',(-0.235097244188112,-0.0362623323546038,
-0.573332326245545));
#80975=CARTESIAN_POINT('Ctrl Pts',(-0.237190554660419,-0.0180574514021879,
-0.574658835074574));
#80976=CARTESIAN_POINT('Ctrl Pts',(-0.237172803082784,0.0026663364785689,
-0.576171385937248));
#80977=CARTESIAN_POINT('Ctrl Pts',(-0.237132321338845,0.0051293477589973,
-0.576351064670178));
#80978=CARTESIAN_POINT('Ctrl Pts',(-0.236734694563812,0.017546042617712,
-0.577255440399193));
#80979=CARTESIAN_POINT('Ctrl Pts',(-0.235789128579883,0.0274719871528137,
-0.577974166226661));
#80980=CARTESIAN_POINT('Ctrl Pts',(-0.233952710119945,0.0390005177114497,
-0.578784514752619));
#80981=CARTESIAN_POINT('Ctrl Pts',(-0.233665119673794,0.0406881214142345,
-0.578902505150956));
#80982=CARTESIAN_POINT('Ctrl Pts',(-0.233186958817902,0.0433215088412519,
-0.579085478400203));
#80983=CARTESIAN_POINT('Ctrl Pts',(-0.233008854426747,0.0442694559772227,
-0.579151111288395));
#80984=CARTESIAN_POINT('Ctrl Pts',(-0.2326816563759,0.0459542434779231,
-0.579267315044433));
#80985=CARTESIAN_POINT('Ctrl Pts',(-0.232534840653077,0.0466914725878568,
-0.579318008233905));
#80986=CARTESIAN_POINT('Ctrl Pts',(-0.232169692325919,0.0484806008444676,
-0.579440668495545));
#80987=CARTESIAN_POINT('Ctrl Pts',(-0.231947714701398,0.0495317317385739,
-0.579512430049519));
#80988=CARTESIAN_POINT('Ctrl Pts',(-0.2312254099009,0.0528406880505038,
-0.579737484619724));
#80989=CARTESIAN_POINT('Ctrl Pts',(-0.230699182093782,0.0550928021906593,
-0.579889407614677));
#80990=CARTESIAN_POINT('Ctrl Pts',(-0.227658898644796,0.0672959440329634,
-0.580707575322966));
#80991=CARTESIAN_POINT('Ctrl Pts',(-0.22453359798498,0.0770845605851778,
-0.581345831714881));
#80992=CARTESIAN_POINT('Ctrl Pts',(-0.21375521406658,0.104550703093417,
-0.583162756291909));
#80993=CARTESIAN_POINT('Ctrl Pts',(-0.20457470143206,0.121537112333389,
-0.584325100980924));
#80994=CARTESIAN_POINT('Ctrl Pts',(-0.191651140315015,0.139754857617948,
-0.58576478929569));
#80995=CARTESIAN_POINT('Ctrl Pts',(-0.189809237127245,0.142246377444869,
-0.585966163085969));
#80996=CARTESIAN_POINT('Ctrl Pts',(-0.186759815583291,0.146206575151737,
-0.586294037921658));
#80997=CARTESIAN_POINT('Ctrl Pts',(-0.185582484971241,0.147698111894396,
-0.58641937011502));
#80998=CARTESIAN_POINT('Ctrl Pts',(-0.183455545628686,0.15032710458339,
-0.586643690360722));
#80999=CARTESIAN_POINT('Ctrl Pts',(-0.182512950409314,0.151470123645603,
-0.586742394691361));
#81000=CARTESIAN_POINT('Ctrl Pts',(-0.180496528876385,0.153869146121517,
-0.586952110885188));
#81001=CARTESIAN_POINT('Ctrl Pts',(-0.179420165310126,0.155122903226704,
-0.587063223091992));
#81002=CARTESIAN_POINT('Ctrl Pts',(-0.176492976072893,0.15846129152175,
-0.587363245771734));
#81003=CARTESIAN_POINT('Ctrl Pts',(-0.17461840129346,0.160524653226724,
-0.58755313418008));
#81004=CARTESIAN_POINT('Ctrl Pts',(-0.162428734019602,0.173475716438283,
-0.588774350092515));
#81005=CARTESIAN_POINT('Ctrl Pts',(-0.151138614504918,0.183395445942116,
-0.589848317462613));
#81006=CARTESIAN_POINT('Ctrl Pts',(-0.12604326829651,0.20154493371799,-0.592103481063444));
#81007=CARTESIAN_POINT('Ctrl Pts',(-0.112182861796049,0.209576580361854,
-0.593281251479492));
#81008=CARTESIAN_POINT('Ctrl Pts',(-0.0957132382716444,0.217014586382776,
-0.594541671383385));
#81009=CARTESIAN_POINT('Ctrl Pts',(-0.0937957946198494,0.217850187839875,
-0.594686356036743));
#81010=CARTESIAN_POINT('Ctrl Pts',(-0.09091578846773,0.219060187155237,
-0.594900355020677));
#81011=CARTESIAN_POINT('Ctrl Pts',(-0.0899614857575037,0.219453816029182,
-0.594970726401677));
#81012=CARTESIAN_POINT('Ctrl Pts',(-0.0882356873261827,0.220152520494593,
-0.595096981663368));
#81013=CARTESIAN_POINT('Ctrl Pts',(-0.0874651348033049,0.220459790088123,
-0.595152990449377));
#81014=CARTESIAN_POINT('Ctrl Pts',(-0.0857283062017472,0.221141837221146,
-0.595278424542304));
#81015=CARTESIAN_POINT('Ctrl Pts',(-0.0847611708582154,0.22151433061782,
-0.595347715595423));
#81016=CARTESIAN_POINT('Ctrl Pts',(-0.0818154273540733,0.222626769923098,
-0.595557171993992));
#81017=CARTESIAN_POINT('Ctrl Pts',(-0.0798292863690017,0.223346655744975,
-0.595696222981916));
#81018=CARTESIAN_POINT('Ctrl Pts',(-0.0698910794199254,0.22679928795754,
-0.59638248911384));
#81019=CARTESIAN_POINT('Ctrl Pts',(-0.0618064595746589,0.229134613958218,
-0.596910738589662));
#81020=CARTESIAN_POINT('Ctrl Pts',(-0.0497394519529199,0.231934880622287,
-0.597678287747428));
#81021=CARTESIAN_POINT('Ctrl Pts',(-0.0458454425556047,0.232735804183639,
-0.597922824468853));
#81022=CARTESIAN_POINT('Ctrl Pts',(-0.041935808141222,0.233438147312179,
-0.598166693585938));
#81023=CARTESIAN_POINT('',(-0.23717495367369,-0.000148239275689535,-0.595517855191994));
#81024=CARTESIAN_POINT('Ctrl Pts',(-0.0419358257187832,0.233438144154472,
-0.618049599588275));
#81025=CARTESIAN_POINT('Ctrl Pts',(-0.043261267264733,0.233200036171422,
-0.617960674506957));
#81026=CARTESIAN_POINT('Ctrl Pts',(-0.0445846388219844,0.23295064713677,
-0.617871399567289));
#81027=CARTESIAN_POINT('Ctrl Pts',(-0.0473589822366303,0.232403316159762,
-0.617683176786025));
#81028=CARTESIAN_POINT('Ctrl Pts',(-0.0488094201177938,0.232103026471708,
-0.617584158513549));
#81029=CARTESIAN_POINT('Ctrl Pts',(-0.0521141759339126,0.231386483710759,
-0.617357098771406));
#81030=CARTESIAN_POINT('Ctrl Pts',(-0.0539664738729612,0.230961493565805,
-0.617228784121711));
#81031=CARTESIAN_POINT('Ctrl Pts',(-0.0597388950774482,0.229563842479385,
-0.616825521116593));
#81032=CARTESIAN_POINT('Ctrl Pts',(-0.0636392294354985,0.228513322098101,
-0.616548116573238));
#81033=CARTESIAN_POINT('Ctrl Pts',(-0.0769248959133572,0.224568437561562,
-0.615585648317777));
#81034=CARTESIAN_POINT('Ctrl Pts',(-0.0861553277255563,0.22119141263378,
-0.614885981884922));
#81035=CARTESIAN_POINT('Ctrl Pts',(-0.100117496526592,0.21507647180833,
-0.613783285543507));
#81036=CARTESIAN_POINT('Ctrl Pts',(-0.105009771953825,0.212730690667721,
-0.613388088063443));
#81037=CARTESIAN_POINT('Ctrl Pts',(-0.12167625656499,0.204024228059665,
-0.612015753684163));
#81038=CARTESIAN_POINT('Ctrl Pts',(-0.132990857487771,0.196836204636743,
-0.611036325282556));
#81039=CARTESIAN_POINT('Ctrl Pts',(-0.145416446004458,0.187379358035906,
-0.609945033831103));
#81040=CARTESIAN_POINT('Ctrl Pts',(-0.147174189294137,0.186001950225975,
-0.609790300561723));
#81041=CARTESIAN_POINT('Ctrl Pts',(-0.149748556034612,0.183925270150464,
-0.609563460954093));
#81042=CARTESIAN_POINT('Ctrl Pts',(-0.150580244910027,0.183244986260299,
-0.609490142375625));
#81043=CARTESIAN_POINT('Ctrl Pts',(-0.152046705492474,0.18202876153103,
-0.609360846359321));
#81044=CARTESIAN_POINT('Ctrl Pts',(-0.152683318982438,0.181495109714958,
-0.609304713393471));
#81045=CARTESIAN_POINT('Ctrl Pts',(-0.154044239389705,0.180342066894852,
-0.609184710844777));
#81046=CARTESIAN_POINT('Ctrl Pts',(-0.15476762772162,0.179721646635547,
-0.609120916605017));
#81047=CARTESIAN_POINT('Ctrl Pts',(-0.156777883706203,0.17797639435524,
-0.608943549582705));
#81048=CARTESIAN_POINT('Ctrl Pts',(-0.158056391158489,0.176841961628248,
-0.60883064551502));
#81049=CARTESIAN_POINT('Ctrl Pts',(-0.160996557754893,0.17417576066291,
-0.608570456465529));
#81050=CARTESIAN_POINT('Ctrl Pts',(-0.162648833598105,0.172633846474256,
-0.608423824387011));
#81051=CARTESIAN_POINT('Ctrl Pts',(-0.168069123482315,0.1674286847578,-0.60794038026738));
#81052=CARTESIAN_POINT('Ctrl Pts',(-0.171737599276426,0.163663675874433,
-0.607609183614968));
#81053=CARTESIAN_POINT('Ctrl Pts',(-0.182083974518938,0.152313710171214,
-0.606652077767214));
#81054=CARTESIAN_POINT('Ctrl Pts',(-0.188406023777705,0.144420304126392,
-0.606036742920574));
#81055=CARTESIAN_POINT('Ctrl Pts',(-0.202174241128331,0.124780841230472,
-0.604563286455234));
#81056=CARTESIAN_POINT('Ctrl Pts',(-0.209128574463145,0.112737973919794,
-0.603702134340606));
#81057=CARTESIAN_POINT('Ctrl Pts',(-0.216165652168537,0.0976327143499137,
-0.602621229964496));
#81058=CARTESIAN_POINT('Ctrl Pts',(-0.217297083025429,0.095087921094545,
-0.60243918985202));
#81059=CARTESIAN_POINT('Ctrl Pts',(-0.219027673533699,0.0910032215589308,
-0.602146776462821));
#81060=CARTESIAN_POINT('Ctrl Pts',(-0.219656025809943,0.0894759084946242,
-0.60203739326548));
#81061=CARTESIAN_POINT('Ctrl Pts',(-0.220817572614232,0.0865665880153049,
-0.60182888234272));
#81062=CARTESIAN_POINT('Ctrl Pts',(-0.221353872650469,0.0851858992293554,
-0.601729864704213));
#81063=CARTESIAN_POINT('Ctrl Pts',(-0.222548634272274,0.0820225412931475,
-0.601502810661118));
#81064=CARTESIAN_POINT('Ctrl Pts',(-0.223198665654398,0.080236819365599,
-0.601374501126548));
#81065=CARTESIAN_POINT('Ctrl Pts',(-0.225162848683154,0.0746323095690608,
-0.600971271365395));
#81066=CARTESIAN_POINT('Ctrl Pts',(-0.226400908304402,0.0707878190028559,
-0.600693895531664));
#81067=CARTESIAN_POINT('Ctrl Pts',(-0.230306603458723,0.0575065138158185,
-0.599732492157616));
#81068=CARTESIAN_POINT('Ctrl Pts',(-0.232486671899685,0.0479378456830597,
-0.599033915382798));
#81069=CARTESIAN_POINT('Ctrl Pts',(-0.236144099433985,0.025563921753949,
-0.597393894565987));
#81070=CARTESIAN_POINT('Ctrl Pts',(-0.237182995334464,0.0127179900854283,
-0.596446869367945));
#81071=CARTESIAN_POINT('Ctrl Pts',(-0.23717495367369,-0.000148239275689535,
-0.595517855191994));
#81072=CARTESIAN_POINT('Ctrl Pts',(-0.237174953469599,-0.000148565452673495,
-0.595517831640184));
#81073=CARTESIAN_POINT('Ctrl Pts',(-0.237170571033214,-0.00714483630179842,
-0.595012661700368));
#81074=CARTESIAN_POINT('Ctrl Pts',(-0.236856620653765,-0.0141383359309857,
-0.594513810019502));
#81075=CARTESIAN_POINT('Ctrl Pts',(-0.236127862419447,-0.0222941772729193,
-0.593946293421482));
#81076=CARTESIAN_POINT('Ctrl Pts',(-0.236012986451005,-0.023479099616672,
-0.593864197745905));
#81077=CARTESIAN_POINT('Ctrl Pts',(-0.235800019478486,-0.0255160103719254,
-0.593723742363697));
#81078=CARTESIAN_POINT('Ctrl Pts',(-0.235706221607482,-0.0263684114726592,
-0.593665166932078));
#81079=CARTESIAN_POINT('Ctrl Pts',(-0.235517961562506,-0.0279979134593863,
-0.593553600840225));
#81080=CARTESIAN_POINT('Ctrl Pts',(-0.235424270861452,-0.0287750957074899,
-0.593500569017096));
#81081=CARTESIAN_POINT('Ctrl Pts',(-0.235228397920248,-0.0303348688435763,
-0.593394513947027));
#81082=CARTESIAN_POINT('Ctrl Pts',(-0.235126155099939,-0.0311174338551282,
-0.593341493704201));
#81083=CARTESIAN_POINT('Ctrl Pts',(-0.234838181567596,-0.0332390836017287,
-0.593198226441276));
#81084=CARTESIAN_POINT('Ctrl Pts',(-0.234644901663677,-0.0345771389395796,
-0.593108390262976));
#81085=CARTESIAN_POINT('Ctrl Pts',(-0.233849768574976,-0.0397676971172572,
-0.592761656087875));
#81086=CARTESIAN_POINT('Ctrl Pts',(-0.233164356334744,-0.0436070071547999,
-0.592508950891954));
#81087=CARTESIAN_POINT('Ctrl Pts',(-0.230668938886948,-0.0558339063420614,
-0.591711224099113));
#81088=CARTESIAN_POINT('Ctrl Pts',(-0.228498361566743,-0.0641412995133093,
-0.591179800987735));
#81089=CARTESIAN_POINT('Ctrl Pts',(-0.220882056361195,-0.0879320307572641,
-0.589643286051157));
#81090=CARTESIAN_POINT('Ctrl Pts',(-0.214275964442334,-0.102988813273946,
-0.588649074421898));
#81091=CARTESIAN_POINT('Ctrl Pts',(-0.203718441821695,-0.121553967374537,
-0.587288910779183));
#81092=CARTESIAN_POINT('Ctrl Pts',(-0.201132701741115,-0.125786331973154,
-0.586969194049667));
#81093=CARTESIAN_POINT('Ctrl Pts',(-0.197290780904103,-0.131653141390029,
-0.586510260190062));
#81094=CARTESIAN_POINT('Ctrl Pts',(-0.196142947705431,-0.133357210134684,
-0.586375013184672));
#81095=CARTESIAN_POINT('Ctrl Pts',(-0.194117171488417,-0.136281929510222,
-0.586139366362959));
#81096=CARTESIAN_POINT('Ctrl Pts',(-0.193249479894379,-0.137509559381093,
-0.58603935737916));
#81097=CARTESIAN_POINT('Ctrl Pts',(-0.191443371428481,-0.140014023842918,
-0.585833013704774));
#81098=CARTESIAN_POINT('Ctrl Pts',(-0.190503713741527,-0.141289865796199,
-0.585726634623225));
#81099=CARTESIAN_POINT('Ctrl Pts',(-0.188066892970437,-0.144530011031782,
-0.585453163990089));
#81100=CARTESIAN_POINT('Ctrl Pts',(-0.186551734289412,-0.14648047635436,
-0.585285376165629));
#81101=CARTESIAN_POINT('Ctrl Pts',(-0.180149392728657,-0.154461740881651,
-0.584585270508451));
#81102=CARTESIAN_POINT('Ctrl Pts',(-0.174998554358182,-0.160273877673241,
-0.584042574976139));
#81103=CARTESIAN_POINT('Ctrl Pts',(-0.15820562877943,-0.177446567665429,
-0.5823334956234));
#81104=CARTESIAN_POINT('Ctrl Pts',(-0.145674155830269,-0.187870316300923,
-0.581135934635838));
#81105=CARTESIAN_POINT('Ctrl Pts',(-0.127503371734501,-0.200066379325894,
-0.579549088820918));
#81106=CARTESIAN_POINT('Ctrl Pts',(-0.122719064259667,-0.203036216333502,
-0.579144104826531));
#81107=CARTESIAN_POINT('Ctrl Pts',(-0.114829122977856,-0.207552971986113,
-0.57850127846909));
#81108=CARTESIAN_POINT('Ctrl Pts',(-0.111787426958215,-0.209206926019219,
-0.578259212400673));
#81109=CARTESIAN_POINT('Ctrl Pts',(-0.107594141871095,-0.211369483997706,
-0.577934308234557));
#81110=CARTESIAN_POINT('Ctrl Pts',(-0.106473272205527,-0.211936312630657,
-0.577848302430748));
#81111=CARTESIAN_POINT('Ctrl Pts',(-0.104580572317317,-0.212874653421189,
-0.577704547922996));
#81112=CARTESIAN_POINT('Ctrl Pts',(-0.103811146385501,-0.213250932359655,
-0.577646514890303));
#81113=CARTESIAN_POINT('Ctrl Pts',(-0.10222329911387,-0.214016820054254,
-0.577527611243384));
#81114=CARTESIAN_POINT('Ctrl Pts',(-0.101404657674275,-0.214405917873048,
-0.577466770938083));
#81115=CARTESIAN_POINT('Ctrl Pts',(-0.0992332517249813,-0.215422761814901,
-0.577306562351128));
#81116=CARTESIAN_POINT('Ctrl Pts',(-0.0978767371693001,-0.216042470729354,
-0.577207668544413));
#81117=CARTESIAN_POINT('Ctrl Pts',(-0.0918028108879673,-0.218748324530533,
-0.576769754274855));
#81118=CARTESIAN_POINT('Ctrl Pts',(-0.0870235789505664,-0.220693205908022,
-0.576438245038698));
#81119=CARTESIAN_POINT('Ctrl Pts',(-0.0680042510002974,-0.227718939208846,
-0.575155353259361));
#81120=CARTESIAN_POINT('Ctrl Pts',(-0.0533549519811368,-0.231589740948118,
-0.574243803806477));
#81121=CARTESIAN_POINT('Ctrl Pts',(-0.0306124204402045,-0.235324710741681,
-0.572822317099033));
#81122=CARTESIAN_POINT('Ctrl Pts',(-0.0227298134306724,-0.23621638676001,
-0.572328895185088));
#81123=CARTESIAN_POINT('Ctrl Pts',(-0.0095847230980491,-0.237039250280026,
-0.571491733839251));
#81124=CARTESIAN_POINT('Ctrl Pts',(-0.00434255531961072,-0.237193188926543,
-0.571154175118985));
#81125=CARTESIAN_POINT('Ctrl Pts',(0.0029977252870206,-0.23716533111237,
-0.570674104885457));
#81126=CARTESIAN_POINT('Ctrl Pts',(0.00509507551264766,-0.237129543453933,
-0.570536093177132));
#81127=CARTESIAN_POINT('Ctrl Pts',(0.00870164498915564,-0.237020134735887,
-0.570297193966059));
#81128=CARTESIAN_POINT('Ctrl Pts',(0.0102111662738607,-0.236959901248115,
-0.570196727977712));
#81129=CARTESIAN_POINT('Ctrl Pts',(0.0132890723122393,-0.236807620780158,
-0.569990860649144));
#81130=CARTESIAN_POINT('Ctrl Pts',(0.0148573210608145,-0.236714402832266,
-0.569885427695738));
#81131=CARTESIAN_POINT('Ctrl Pts',(0.018823949479914,-0.236439050647876,
-0.569617330492226));
#81132=CARTESIAN_POINT('Ctrl Pts',(0.0212206502947203,-0.236236002773485,
-0.569454022828449));
#81133=CARTESIAN_POINT('Ctrl Pts',(0.0307360445602773,-0.235283894054256,
-0.56880018671674));
#81134=CARTESIAN_POINT('Ctrl Pts',(0.0378216918353701,-0.23424926143078,
-0.568300944889594));
#81135=CARTESIAN_POINT('Ctrl Pts',(0.0600180576564708,-0.229974873993864,
-0.566697618462069));
#81136=CARTESIAN_POINT('Ctrl Pts',(0.0748641676677131,-0.225578977197656,
-0.565563841336754));
#81137=CARTESIAN_POINT('Ctrl Pts',(0.0953396875244777,-0.217270745662714,
-0.563955934867405));
#81138=CARTESIAN_POINT('Ctrl Pts',(0.101396255566271,-0.214511173094511,
-0.56347492500311));
#81139=CARTESIAN_POINT('Ctrl Pts',(0.109673318024955,-0.210310851647791,
-0.562816505942914));
#81140=CARTESIAN_POINT('Ctrl Pts',(0.111997678700695,-0.209082309646988,
-0.562631500235571));
#81141=CARTESIAN_POINT('Ctrl Pts',(0.116042399495685,-0.20685765861291,
-0.562309958084017));
#81142=CARTESIAN_POINT('Ctrl Pts',(0.117771533730135,-0.205878109318699,
-0.562172627484544));
#81143=CARTESIAN_POINT('Ctrl Pts',(0.120361894354139,-0.204367360289341,
-0.56196732250584));
#81144=CARTESIAN_POINT('Ctrl Pts',(0.121232319573422,-0.203852221841296,
-0.561898408625373));
#81145=CARTESIAN_POINT('Ctrl Pts',(0.122810871420843,-0.202904310265034,
-0.561773602227446));
#81146=CARTESIAN_POINT('Ctrl Pts',(0.123520040234958,-0.202473378419569,
-0.561717600021444));
#81147=CARTESIAN_POINT('Ctrl Pts',(0.125128531446269,-0.201484369996454,
-0.561590723830709));
#81148=CARTESIAN_POINT('Ctrl Pts',(0.126026395111273,-0.200923987061535,
-0.561520000033162));
#81149=CARTESIAN_POINT('Ctrl Pts',(0.128802767844681,-0.199165238637102,
-0.561301517375187));
#81150=CARTESIAN_POINT('Ctrl Pts',(0.130668224430713,-0.197946359622002,
-0.561155017910066));
#81151=CARTESIAN_POINT('Ctrl Pts',(0.144398683263895,-0.188696245190025,
-0.560076776764178));
#81152=CARTESIAN_POINT('Ctrl Pts',(0.15553291219144,-0.179629829442218,
-0.559201530061659));
#81153=CARTESIAN_POINT('Ctrl Pts',(0.168966584928727,-0.166499574943449,
-0.55804959600846));
#81154=CARTESIAN_POINT('Ctrl Pts',(0.172063182665283,-0.16329750678787,
-0.557776502456426));
#81155=CARTESIAN_POINT('Ctrl Pts',(0.180518784697646,-0.154046200394293,
-0.557003911623883));
#81156=CARTESIAN_POINT('Ctrl Pts',(0.185661164826487,-0.14780791880536,
-0.556501472186896));
#81157=CARTESIAN_POINT('Ctrl Pts',(0.193639478498566,-0.137054513971805,
-0.555650774396388));
#81158=CARTESIAN_POINT('Ctrl Pts',(0.196659656027989,-0.132684439403903,
-0.555308976907627));
#81159=CARTESIAN_POINT('Ctrl Pts',(0.200669800806683,-0.126443874884412,
-0.554823898612598));
#81160=CARTESIAN_POINT('Ctrl Pts',(0.201785435705773,-0.124655765678032,
-0.554685248479597));
#81161=CARTESIAN_POINT('Ctrl Pts',(0.2036605072712,-0.121559310652525,-0.554445594362856));
#81162=CARTESIAN_POINT('Ctrl Pts',(0.204431540988378,-0.120258110317989,
-0.55434501904546));
#81163=CARTESIAN_POINT('Ctrl Pts',(0.205976522316863,-0.117592992638369,
-0.554139241449768));
#81164=CARTESIAN_POINT('Ctrl Pts',(0.206749491963677,-0.116228598168285,
-0.554034010386121));
#81165=CARTESIAN_POINT('Ctrl Pts',(0.208666928367412,-0.112764410568471,
-0.553767065634044));
#81166=CARTESIAN_POINT('Ctrl Pts',(0.209793249284913,-0.110654828689662,
-0.553604719697252));
#81167=CARTESIAN_POINT('Ctrl Pts',(0.214102231794804,-0.102281828780174,
-0.552960986520942));
#81168=CARTESIAN_POINT('Ctrl Pts',(0.217037558936247,-0.0958958745226785,
-0.552471232167991));
#81169=CARTESIAN_POINT('Ctrl Pts',(0.225549943492971,-0.0749757395474853,
-0.550870359882693));
#81170=CARTESIAN_POINT('Ctrl Pts',(0.22998163644367,-0.0600207486190322,
-0.549728371006473));
#81171=CARTESIAN_POINT('Ctrl Pts',(0.234177667245787,-0.0381770367935283,
-0.548109687204103));
#81172=CARTESIAN_POINT('Ctrl Pts',(0.235160681997152,-0.031561539969732,
-0.547626259335225));
#81173=CARTESIAN_POINT('Ctrl Pts',(0.236139905032703,-0.0222907727159821,
-0.546964905663577));
#81174=CARTESIAN_POINT('Ctrl Pts',(0.236373139771617,-0.0196640111848082,
-0.546779319352579));
#81175=CARTESIAN_POINT('Ctrl Pts',(0.236705579665014,-0.015047140340816,
-0.546456875225081));
#81176=CARTESIAN_POINT('Ctrl Pts',(0.236823603878279,-0.0130586819255909,
-0.546319217429605));
#81177=CARTESIAN_POINT('Ctrl Pts',(0.236963813573957,-0.0100576591424868,
-0.546113525185883));
#81178=CARTESIAN_POINT('Ctrl Pts',(0.237004585284174,-0.00904610966653566,
-0.546044546128703));
#81179=CARTESIAN_POINT('Ctrl Pts',(0.237066989210801,-0.00720498548137484,
-0.545919677059108));
#81180=CARTESIAN_POINT('Ctrl Pts',(0.237090745836903,-0.0063755370884557,
-0.545863676665504));
#81181=CARTESIAN_POINT('Ctrl Pts',(0.237134872344849,-0.00448895970372778,
-0.545736873689137));
#81182=CARTESIAN_POINT('Ctrl Pts',(0.237152527466102,-0.00343180186491667,
-0.545666220519968));
#81183=CARTESIAN_POINT('Ctrl Pts',(0.23718536327195,-0.000152238589986392,
-0.545448185140647));
#81184=CARTESIAN_POINT('Ctrl Pts',(0.237176377841256,0.00207036045988246,
-0.545302054945404));
#81185=CARTESIAN_POINT('Ctrl Pts',(0.236805863563745,0.0225386779013626,
-0.543968670879194));
#81186=CARTESIAN_POINT('Ctrl Pts',(0.234370786503552,0.0406882938431326,
-0.542873267876422));
#81187=CARTESIAN_POINT('Ctrl Pts',(0.226764188929052,0.0706395626200742,
-0.540970577724566));
#81188=CARTESIAN_POINT('Ctrl Pts',(0.222675799951735,0.0826279229933428,
-0.540181913606909));
#81189=CARTESIAN_POINT('Ctrl Pts',(0.216570648452122,0.0967291974654365,
-0.539184515668556));
#81190=CARTESIAN_POINT('Ctrl Pts',(0.215446794278926,0.0992071633394274,
-0.539006569644532));
#81191=CARTESIAN_POINT('Ctrl Pts',(0.213578524376315,0.103144932803993,
-0.538719181810877));
#81192=CARTESIAN_POINT('Ctrl Pts',(0.212861157193617,0.104617354055069,
-0.538610670091569));
#81193=CARTESIAN_POINT('Ctrl Pts',(0.2114647565378,0.107409684363715,-0.538402811921996));
#81194=CARTESIAN_POINT('Ctrl Pts',(0.210788467752124,0.108730884496113,
-0.538303564940414));
#81195=CARTESIAN_POINT('Ctrl Pts',(0.209221111752811,0.111723290956537,
-0.53807667978722));
#81196=CARTESIAN_POINT('Ctrl Pts',(0.208322347445643,0.113390328241956,
-0.537948775078477));
#81197=CARTESIAN_POINT('Ctrl Pts',(0.205406906734066,0.118646237104622,
-0.537540588909763));
#81198=CARTESIAN_POINT('Ctrl Pts',(0.203316807541324,0.122193285513064,
-0.53725772417659));
#81199=CARTESIAN_POINT('Ctrl Pts',(0.191353001000619,0.141339300531332,
-0.535688868771899));
#81200=CARTESIAN_POINT('Ctrl Pts',(0.179777465363339,0.155796684328052,
-0.534340476054183));
#81201=CARTESIAN_POINT('Ctrl Pts',(0.159516208535676,0.175803767857263,
-0.532264712286895));
#81202=CARTESIAN_POINT('Ctrl Pts',(0.151946522763103,0.182386070587964,
-0.531538773433789));
#81203=CARTESIAN_POINT('Ctrl Pts',(0.142164478862654,0.189859093628788,
-0.530678194329031));
#81204=CARTESIAN_POINT('Ctrl Pts',(0.140326431730872,0.191221620126433,
-0.530519639398288));
#81205=CARTESIAN_POINT('Ctrl Pts',(0.137600564696794,0.193181803138787,
-0.530289405587618));
#81206=CARTESIAN_POINT('Ctrl Pts',(0.136728020222686,0.193800343306433,
-0.530216431323708));
#81207=CARTESIAN_POINT('Ctrl Pts',(0.135235727363386,0.194843123120728,
-0.530092891104572));
#81208=CARTESIAN_POINT('Ctrl Pts',(0.134618110535349,0.195270348380001,
-0.530042127949405));
#81209=CARTESIAN_POINT('Ctrl Pts',(0.133200402178315,0.196241099073671,
-0.529926445585333));
#81210=CARTESIAN_POINT('Ctrl Pts',(0.132399004028769,0.196782671800986,
-0.529861656500242));
#81211=CARTESIAN_POINT('Ctrl Pts',(0.130159456182275,0.19827624930605,-0.529682205389604));
#81212=CARTESIAN_POINT('Ctrl Pts',(0.12871416865677,0.199217515003067,-0.529568223258868));
#81213=CARTESIAN_POINT('Ctrl Pts',(0.117527278183369,0.206330575616943,
-0.528698854616319));
#81214=CARTESIAN_POINT('Ctrl Pts',(0.107356168235146,0.211801066195356,
-0.527982430923913));
#81215=CARTESIAN_POINT('Ctrl Pts',(0.0963342165446225,0.216730223379704,
-0.527239474662252));
#81216=CARTESIAN_POINT('Ctrl Pts',(0.0958415504323145,0.216948538175205,
-0.527206333863953));
#81217=CARTESIAN_POINT('Ctrl Pts',(0.0867021829958203,0.220961252137059,
-0.526592741027069));
#81218=CARTESIAN_POINT('Ctrl Pts',(0.0778373824196349,0.224237557498435,
-0.526017005720486));
#81219=CARTESIAN_POINT('Ctrl Pts',(0.0622043465669194,0.228976228976599,
-0.525004832202367));
#81220=CARTESIAN_POINT('Ctrl Pts',(0.0555241199896826,0.230687138434034,
-0.524573342802406));
#81221=CARTESIAN_POINT('Ctrl Pts',(0.0441227348075537,0.233083258425263,
-0.523830302763292));
#81222=CARTESIAN_POINT('Ctrl Pts',(0.0394381383633985,0.233921459956155,
-0.523523191092661));
#81223=CARTESIAN_POINT('Ctrl Pts',(0.0327306075814457,0.234914410486938,
-0.52307924688592));
#81224=CARTESIAN_POINT('Ctrl Pts',(0.0307258166930042,0.235185026514933,
-0.522946030726012));
#81225=CARTESIAN_POINT('Ctrl Pts',(0.0272307318153744,0.235611358650051,
-0.522712753333736));
#81226=CARTESIAN_POINT('Ctrl Pts',(0.0257419485388233,0.235778661015362,
-0.522613060676727));
#81227=CARTESIAN_POINT('Ctrl Pts',(0.0228563769567727,0.236075272275144,
-0.522419163805604));
#81228=CARTESIAN_POINT('Ctrl Pts',(0.0214598268016012,0.236206316246989,
-0.522325018369448));
#81229=CARTESIAN_POINT('Ctrl Pts',(0.0177264699098827,0.236523250326617,
-0.522072490182803));
#81230=CARTESIAN_POINT('Ctrl Pts',(0.015387982503259,0.236686892306821,
-0.521913421021383));
#81231=CARTESIAN_POINT('Ctrl Pts',(0.00647182722471014,0.237178133753775,
-0.521303332392777));
#81232=CARTESIAN_POINT('Ctrl Pts',(-0.000115500270155912,0.237266356424297,
-0.520845047669498));
#81233=CARTESIAN_POINT('Ctrl Pts',(-0.0185264746784814,0.23674625214578,
-0.519542729368853));
#81234=CARTESIAN_POINT('Ctrl Pts',(-0.0303055268150793,0.235527462097546,
-0.518683880692026));
#81235=CARTESIAN_POINT('Ctrl Pts',(-0.0419358519811635,0.233438139436584,
-0.517821408604163));
#81236=CARTESIAN_POINT('Origin',(0.,0.,-1.7456589891905));
#81237=CARTESIAN_POINT('',(-0.0419358190075303,0.23343814536011,-0.397909151625197));
#81238=CARTESIAN_POINT('',(-0.0419358280420692,0.233438143737107,-0.417646538149483));
#81239=CARTESIAN_POINT('',(-0.0419358257166344,0.233438144154858,-1.7456589891905));
#81240=CARTESIAN_POINT('',(-0.237174999766729,1.05191258440349E-5,-0.475718588717799));
#81241=CARTESIAN_POINT('Ctrl Pts',(-0.0419358190075306,0.23343814536011,
-0.397909151625197));
#81242=CARTESIAN_POINT('Ctrl Pts',(-0.0317267657812627,0.235272143002931,
-0.398629247492366));
#81243=CARTESIAN_POINT('Ctrl Pts',(-0.0214074572156793,0.236434631915132,
-0.399369272295089));
#81244=CARTESIAN_POINT('Ctrl Pts',(0.00738320527071984,0.237776723418298,
-0.401457010517832));
#81245=CARTESIAN_POINT('Ctrl Pts',(0.0258479393168837,0.236483004057781,
-0.402826067786711));
#81246=CARTESIAN_POINT('Ctrl Pts',(0.0461210455182574,0.232657672366057,
-0.404266587768362));
#81247=CARTESIAN_POINT('Ctrl Pts',(0.0482599787164858,0.232223423984624,
-0.404417693361836));
#81248=CARTESIAN_POINT('Ctrl Pts',(0.0514185785498025,0.231536633337051,
-0.4046392343386));
#81249=CARTESIAN_POINT('Ctrl Pts',(0.0524429840939502,0.23130675805443,
-0.404710834404866));
#81250=CARTESIAN_POINT('Ctrl Pts',(0.0542742712242867,0.230883028039117,
-0.404838340543364));
#81251=CARTESIAN_POINT('Ctrl Pts',(0.0550816961518037,0.230691733626287,
-0.404894384312414));
#81252=CARTESIAN_POINT('Ctrl Pts',(0.0568789448163363,0.230255956854864,
-0.405018744253081));
#81253=CARTESIAN_POINT('Ctrl Pts',(0.0578682115086129,0.230009326383489,
-0.405086938427213));
#81254=CARTESIAN_POINT('Ctrl Pts',(0.0608192982060854,0.22925335673267,
-0.405289682272511));
#81255=CARTESIAN_POINT('Ctrl Pts',(0.062776269233406,0.228725226637899,
-0.405423219512599));
#81256=CARTESIAN_POINT('Ctrl Pts',(0.0765161741268056,0.224827583118753,
-0.406355925518777));
#81257=CARTESIAN_POINT('Ctrl Pts',(0.0880307032054034,0.220573889043712,
-0.407112816160427));
#81258=CARTESIAN_POINT('Ctrl Pts',(0.115402750124721,0.207975163111058,
-0.408963351674379));
#81259=CARTESIAN_POINT('Ctrl Pts',(0.130740838185398,0.198691268582307,
-0.410050228211231));
#81260=CARTESIAN_POINT('Ctrl Pts',(0.147263095680553,0.185942314809714,
-0.411396725322285));
#81261=CARTESIAN_POINT('Ctrl Pts',(0.149600985678177,0.184066584642513,
-0.411591683826283));
#81262=CARTESIAN_POINT('Ctrl Pts',(0.153339512501802,0.180948819037631,
-0.411911170446299));
#81263=CARTESIAN_POINT('Ctrl Pts',(0.154762137032554,0.1797335856563,-0.412034627183156));
#81264=CARTESIAN_POINT('Ctrl Pts',(0.157282935565084,0.177528151940406,
-0.412256879616822));
#81265=CARTESIAN_POINT('Ctrl Pts',(0.158386519553255,0.176544263022267,
-0.412355411462506));
#81266=CARTESIAN_POINT('Ctrl Pts',(0.160716663593573,0.174427413304002,
-0.412566143884982));
#81267=CARTESIAN_POINT('Ctrl Pts',(0.161940597171378,0.173291694000308,
-0.412678457851815));
#81268=CARTESIAN_POINT('Ctrl Pts',(0.165234778927277,0.170169562049885,
-0.412985272807564));
#81269=CARTESIAN_POINT('Ctrl Pts',(0.167281080933843,0.168158409614102,
-0.413180829833688));
#81270=CARTESIAN_POINT('Ctrl Pts',(0.171747995182962,0.163605991729049,
-0.41361913320721));
#81271=CARTESIAN_POINT('Ctrl Pts',(0.17414966057941,0.161047160453219,-0.413862619142252));
#81272=CARTESIAN_POINT('Ctrl Pts',(0.181643002601502,0.152699778260872,
-0.414648040684364));
#81273=CARTESIAN_POINT('Ctrl Pts',(0.18650925610152,0.146716327730293,-0.415198089982703));
#81274=CARTESIAN_POINT('Ctrl Pts',(0.196371682246179,0.133304439355165,
-0.416400678330391));
#81275=CARTESIAN_POINT('Ctrl Pts',(0.201256497807493,0.125808279816814,
-0.417054690773567));
#81276=CARTESIAN_POINT('Ctrl Pts',(0.211296143348545,0.108314521535111,
-0.418525580639704));
#81277=CARTESIAN_POINT('Ctrl Pts',(0.21618776935157,0.0981885952475901,
-0.419339669702313));
#81278=CARTESIAN_POINT('Ctrl Pts',(0.220980133269461,0.0861552067457863,
-0.420238886342993));
#81279=CARTESIAN_POINT('Ctrl Pts',(0.221599135776701,0.0845503542282169,
-0.420357450220177));
#81280=CARTESIAN_POINT('Ctrl Pts',(0.222538565721099,0.0820335369102421,
-0.420541116925352));
#81281=CARTESIAN_POINT('Ctrl Pts',(0.222870956498742,0.0811261440211782,
-0.420606877422912));
#81282=CARTESIAN_POINT('Ctrl Pts',(0.223451938448637,0.0795095996800856,
-0.420723188858775));
#81283=CARTESIAN_POINT('Ctrl Pts',(0.223702709728511,0.0788012875589661,
-0.420773863502451));
#81284=CARTESIAN_POINT('Ctrl Pts',(0.224302944833988,0.0770799443931066,
-0.420896327160993));
#81285=CARTESIAN_POINT('Ctrl Pts',(0.224648915304766,0.0760657206086813,
-0.420967912487646));
#81286=CARTESIAN_POINT('Ctrl Pts',(0.225715133389289,0.0728693320672463,
-0.421191830837947));
#81287=CARTESIAN_POINT('Ctrl Pts',(0.226410573852171,0.0706789502045201,
-0.421342813362654));
#81288=CARTESIAN_POINT('Ctrl Pts',(0.229995291247247,0.0587920952940921,
-0.422150687754273));
#81289=CARTESIAN_POINT('Ctrl Pts',(0.232294009029654,0.0489273353770943,
-0.422780358952519));
#81290=CARTESIAN_POINT('Ctrl Pts',(0.237037196548168,0.0204333440642143,
-0.424559824887115));
#81291=CARTESIAN_POINT('Ctrl Pts',(0.237910626745225,0.00162320656105648,
-0.425693173782317));
#81292=CARTESIAN_POINT('Ctrl Pts',(0.236281458244531,-0.0209238098545081,
-0.427145191866027));
#81293=CARTESIAN_POINT('Ctrl Pts',(0.235911642837729,-0.0247472712159931,
-0.427394415795856));
#81294=CARTESIAN_POINT('Ctrl Pts',(0.235224669817445,-0.0304107089922827,
-0.427768876627486));
#81295=CARTESIAN_POINT('Ctrl Pts',(0.234978357855017,-0.0322587588364578,
-0.427891908846852));
#81296=CARTESIAN_POINT('Ctrl Pts',(0.234497786365661,-0.0355661763147119,
-0.428113697962805));
#81297=CARTESIAN_POINT('Ctrl Pts',(0.234271621834312,-0.0370266355786783,
-0.428212195500903));
#81298=CARTESIAN_POINT('Ctrl Pts',(0.233760220369477,-0.0401365397177466,
-0.428423181146927));
#81299=CARTESIAN_POINT('Ctrl Pts',(0.233471141859209,-0.0417852619702745,
-0.4285357857508));
#81300=CARTESIAN_POINT('Ctrl Pts',(0.232635654857207,-0.0462707020427143,
-0.428844248329243));
#81301=CARTESIAN_POINT('Ctrl Pts',(0.232054846738631,-0.0491006375164009,
-0.429041181667275));
#81302=CARTESIAN_POINT('Ctrl Pts',(0.230647547267472,-0.0553734821709733,
-0.429483068607392));
#81303=CARTESIAN_POINT('Ctrl Pts',(0.229795369112122,-0.0588098602010125,
-0.429728780561197));
#81304=CARTESIAN_POINT('Ctrl Pts',(0.22681593787761,-0.0697682278568901,
-0.4305241902922));
#81305=CARTESIAN_POINT('Ctrl Pts',(0.224393821554575,-0.0772040686177263,
-0.431082234557229));
#81306=CARTESIAN_POINT('Ctrl Pts',(0.218471271451999,-0.0927353802134014,
-0.432283580479144));
#81307=CARTESIAN_POINT('Ctrl Pts',(0.214877388010344,-0.100783164098656,
-0.432927873152766));
#81308=CARTESIAN_POINT('Ctrl Pts',(0.205720516194495,-0.11855903740418,
-0.434385998512226));
#81309=CARTESIAN_POINT('Ctrl Pts',(0.19989851080186,-0.128132030393042,
-0.435196995646673));
#81310=CARTESIAN_POINT('Ctrl Pts',(0.192426520690626,-0.138661356039739,
-0.436093329800331));
#81311=CARTESIAN_POINT('Ctrl Pts',(0.191416109038451,-0.140052886982261,
-0.436211864544351));
#81312=CARTESIAN_POINT('Ctrl Pts',(0.189814427230167,-0.142208992147377,
-0.436395496025108));
#81313=CARTESIAN_POINT('Ctrl Pts',(0.189233490750703,-0.142981118661772,
-0.436461250042873));
#81314=CARTESIAN_POINT('Ctrl Pts',(0.188192408239198,-0.144347368324564,
-0.436577555989376));
#81315=CARTESIAN_POINT('Ctrl Pts',(0.187734150674308,-0.144942864449243,
-0.436628231553306));
#81316=CARTESIAN_POINT('Ctrl Pts',(0.186615425696446,-0.146382417226087,
-0.436750705099931));
#81317=CARTESIAN_POINT('Ctrl Pts',(0.185952057020649,-0.147224188845206,
-0.43682229930223));
#81318=CARTESIAN_POINT('Ctrl Pts',(0.183848013998961,-0.14985717242962,
-0.437046274789012));
#81319=CARTESIAN_POINT('Ctrl Pts',(0.182386943663814,-0.151632015481593,
-0.437197304596227));
#81320=CARTESIAN_POINT('Ctrl Pts',(0.174352344697524,-0.161107889310539,
-0.438005693813822));
#81321=CARTESIAN_POINT('Ctrl Pts',(0.16731589362262,-0.168404068336461,
-0.438635794415341));
#81322=CARTESIAN_POINT('Ctrl Pts',(0.145951821760804,-0.187891172976979,
-0.440417107446991));
#81323=CARTESIAN_POINT('Ctrl Pts',(0.130615686373842,-0.198858030215526,
-0.441551878486942));
#81324=CARTESIAN_POINT('Ctrl Pts',(0.110797626131273,-0.209739036233017,
-0.443004327343519));
#81325=CARTESIAN_POINT('Ctrl Pts',(0.107404866139155,-0.211496499678295,
-0.44325226101781));
#81326=CARTESIAN_POINT('Ctrl Pts',(0.102299024186799,-0.213986803282064,
-0.443625159537624));
#81327=CARTESIAN_POINT('Ctrl Pts',(0.100617262931436,-0.214782700421526,
-0.443747947240952));
#81328=CARTESIAN_POINT('Ctrl Pts',(0.0975834953430446,-0.216174987266577,
-0.443969470349743));
#81329=CARTESIAN_POINT('Ctrl Pts',(0.0962349369635496,-0.216778689962615,
-0.444067948984091));
#81330=CARTESIAN_POINT('Ctrl Pts',(0.0933445112548619,-0.218040346946825,
-0.444279084663897));
#81331=CARTESIAN_POINT('Ctrl Pts',(0.0918011396541931,-0.218694629989974,
-0.444391860021977));
#81332=CARTESIAN_POINT('Ctrl Pts',(0.0875687722106209,-0.220436165808188,
-0.444701291613612));
#81333=CARTESIAN_POINT('Ctrl Pts',(0.0848666375347113,-0.22149050905599,
-0.444899034646894));
#81334=CARTESIAN_POINT('Ctrl Pts',(0.0672399178255367,-0.227998357025257,
-0.446190713948813));
#81335=CARTESIAN_POINT('Ctrl Pts',(0.0518212622284608,-0.23198888563968,
-0.447332708186704));
#81336=CARTESIAN_POINT('Ctrl Pts',(0.0215639511476443,-0.236651556718902,
-0.449565000241521));
#81337=CARTESIAN_POINT('Ctrl Pts',(0.00682702320658603,-0.23753404809969,
-0.450647289008711));
#81338=CARTESIAN_POINT('Ctrl Pts',(-0.0100821772995698,-0.236970691288998,
-0.451828654756668));
#81339=CARTESIAN_POINT('Ctrl Pts',(-0.0122658630892032,-0.236867702057497,
-0.45198001066124));
#81340=CARTESIAN_POINT('Ctrl Pts',(-0.0154964764630396,-0.236670537742254,
-0.45220184493084));
#81341=CARTESIAN_POINT('Ctrl Pts',(-0.0165446342782324,-0.236599576077304,
-0.452273492266951));
#81342=CARTESIAN_POINT('Ctrl Pts',(-0.0184198200825886,-0.236460101102001,
-0.452401047239234));
#81343=CARTESIAN_POINT('Ctrl Pts',(-0.0192469952684292,-0.236394209784147,
-0.452457093061742));
#81344=CARTESIAN_POINT('Ctrl Pts',(-0.0210890951357676,-0.236237737991364,
-0.45258141481195));
#81345=CARTESIAN_POINT('Ctrl Pts',(-0.0221037976542683,-0.236144957621462,
-0.452649569190236));
#81346=CARTESIAN_POINT('Ctrl Pts',(-0.0251320036130714,-0.235848380463946,
-0.452852071771195));
#81347=CARTESIAN_POINT('Ctrl Pts',(-0.0271435884547158,-0.235625343390627,
-0.452985411116749));
#81348=CARTESIAN_POINT('Ctrl Pts',(-0.0410187650969288,-0.233906857716986,
-0.453898509300437));
#81349=CARTESIAN_POINT('Ctrl Pts',(-0.0527588509959145,-0.231541647410529,
-0.454638053952543));
#81350=CARTESIAN_POINT('Ctrl Pts',(-0.081833207260524,-0.223356568271885,
-0.456493799154509));
#81351=CARTESIAN_POINT('Ctrl Pts',(-0.0987636935471548,-0.216403528414672,
-0.45760176503617));
#81352=CARTESIAN_POINT('Ctrl Pts',(-0.117321196317661,-0.206146759942251,
-0.458970328473414));
#81353=CARTESIAN_POINT('Ctrl Pts',(-0.119885792636932,-0.204665935659423,
-0.459163005165487));
#81354=CARTESIAN_POINT('Ctrl Pts',(-0.124015415670018,-0.202177196611678,
-0.459479504181893));
#81355=CARTESIAN_POINT('Ctrl Pts',(-0.125597532954304,-0.201198164855224,
-0.459602288867322));
#81356=CARTESIAN_POINT('Ctrl Pts',(-0.128415108292639,-0.199408434206802,
-0.45982380869762));
#81357=CARTESIAN_POINT('Ctrl Pts',(-0.129654830168006,-0.198604603461101,
-0.459922287103312));
#81358=CARTESIAN_POINT('Ctrl Pts',(-0.132284910727145,-0.196864149033034,
-0.460133424656518));
#81359=CARTESIAN_POINT('Ctrl Pts',(-0.133673005024473,-0.195924266640102,
-0.460246202139215));
#81360=CARTESIAN_POINT('Ctrl Pts',(-0.137435399363368,-0.193318144268977,
-0.460555645790244));
#81361=CARTESIAN_POINT('Ctrl Pts',(-0.139789214189776,-0.191622984538444,
-0.460753398900938));
#81362=CARTESIAN_POINT('Ctrl Pts',(-0.154329659723102,-0.180740821885757,
-0.462001905387607));
#81363=CARTESIAN_POINT('Ctrl Pts',(-0.165634784178891,-0.170440176212749,
-0.463096667166265));
#81364=CARTESIAN_POINT('Ctrl Pts',(-0.186216135830429,-0.147693253771091,
-0.465331831430279));
#81365=CARTESIAN_POINT('Ctrl Pts',(-0.195422617626257,-0.135276818324557,
-0.46646686491421));
#81366=CARTESIAN_POINT('Ctrl Pts',(-0.204463497857814,-0.12021341569495,
-0.467693015300844));
#81367=CARTESIAN_POINT('Ctrl Pts',(-0.205543037438675,-0.11835813378653,
-0.467841574297239));
#81368=CARTESIAN_POINT('Ctrl Pts',(-0.207109519474475,-0.115579908537943,
-0.468060128327291));
#81369=CARTESIAN_POINT('Ctrl Pts',(-0.207615765331557,-0.114668053108156,
-0.468131244810757));
#81370=CARTESIAN_POINT('Ctrl Pts',(-0.208513893208211,-0.113024887714944,
-0.468258254284673));
#81371=CARTESIAN_POINT('Ctrl Pts',(-0.208907968994988,-0.112294832705891,
-0.468314279953584));
#81372=CARTESIAN_POINT('Ctrl Pts',(-0.209780797345346,-0.110657354895528,
-0.468439043474671));
#81373=CARTESIAN_POINT('Ctrl Pts',(-0.210257500768808,-0.109748879700463,
-0.468507654649401));
#81374=CARTESIAN_POINT('Ctrl Pts',(-0.211673219549259,-0.107007797666467,
-0.468712936030852));
#81375=CARTESIAN_POINT('Ctrl Pts',(-0.212594307452354,-0.105165972525613,
-0.468848555841296));
#81376=CARTESIAN_POINT('Ctrl Pts',(-0.214690953255747,-0.100833326201437,
-0.469162751974511));
#81377=CARTESIAN_POINT('Ctrl Pts',(-0.215847364245524,-0.0983335232871611,
-0.469340360800791));
#81378=CARTESIAN_POINT('Ctrl Pts',(-0.219856024708428,-0.0892563660339403,
-0.469974153753983));
#81379=CARTESIAN_POINT('Ctrl Pts',(-0.222453436923456,-0.0825702926907982,
-0.470420292817272));
#81380=CARTESIAN_POINT('Ctrl Pts',(-0.230389034410373,-0.0590342197491395,
-0.471952509570555));
#81381=CARTESIAN_POINT('Ctrl Pts',(-0.234145224059022,-0.0417148708401526,
-0.473018460337774));
#81382=CARTESIAN_POINT('Ctrl Pts',(-0.236440546165004,-0.019279789755122,
-0.47445454883603));
#81383=CARTESIAN_POINT('Ctrl Pts',(-0.236787440327543,-0.0144064228236565,
-0.474769392670411));
#81384=CARTESIAN_POINT('Ctrl Pts',(-0.237061123541786,-0.00759790565451577,
-0.475215058726645));
#81385=CARTESIAN_POINT('Ctrl Pts',(-0.237115093450983,-0.00566891181169765,
-0.475341968622919));
#81386=CARTESIAN_POINT('Ctrl Pts',(-0.237165227962936,-0.00248958002820659,
-0.47555229713523));
#81387=CARTESIAN_POINT('Ctrl Pts',(-0.237175055208515,-0.00123952823062238,
-0.475635288893505));
#81388=CARTESIAN_POINT('Ctrl Pts',(-0.237174999766729,1.05191258440349E-5,
-0.475718588717799));
#81389=CARTESIAN_POINT('Ctrl Pts',(-0.23717499976624,1.0530156552288E-5,
-0.475718589452856));
#81390=CARTESIAN_POINT('Ctrl Pts',(-0.237174948687184,0.00116100449970449,
-0.475795253998586));
#81391=CARTESIAN_POINT('Ctrl Pts',(-0.237166526634602,0.00231144960027964,
-0.475872177768488));
#81392=CARTESIAN_POINT('Ctrl Pts',(-0.237123304695454,0.00527237912689858,
-0.476070854539049));
#81393=CARTESIAN_POINT('Ctrl Pts',(-0.237076140530004,0.00708257631464626,
-0.476192988308165));
#81394=CARTESIAN_POINT('Ctrl Pts',(-0.236878960709074,0.0123382190362649,
-0.476549618360509));
#81395=CARTESIAN_POINT('Ctrl Pts',(-0.236674524732556,0.0157810282805962,
-0.47678578196556));
#81396=CARTESIAN_POINT('Ctrl Pts',(-0.235117606002505,0.0349322337340345,
-0.478114321511021));
#81397=CARTESIAN_POINT('Ctrl Pts',(-0.23227662357456,0.0504773375061679,
-0.479252328537395));
#81398=CARTESIAN_POINT('Ctrl Pts',(-0.224035792179592,0.0790985965470245,
-0.481425694060155));
#81399=CARTESIAN_POINT('Ctrl Pts',(-0.218968026705839,0.0922046536630583,
-0.482453287762943));
#81400=CARTESIAN_POINT('Ctrl Pts',(-0.211867864855361,0.106621623481787,
-0.483573513488986));
#81401=CARTESIAN_POINT('Ctrl Pts',(-0.210940617270537,0.108444545454168,
-0.483714924562397));
#81402=CARTESIAN_POINT('Ctrl Pts',(-0.209514248503541,0.111161176174543,
-0.48392506466096));
#81403=CARTESIAN_POINT('Ctrl Pts',(-0.209032760534276,0.112063966267974,
-0.483994797618628));
#81404=CARTESIAN_POINT('Ctrl Pts',(-0.208150265699311,0.113693165538168,
-0.484120418281874));
#81405=CARTESIAN_POINT('Ctrl Pts',(-0.207751277711071,0.114420608546443,
-0.484176424188112));
#81406=CARTESIAN_POINT('Ctrl Pts',(-0.206840686760009,0.11606034995594,
-0.484302484120207));
#81407=CARTESIAN_POINT('Ctrl Pts',(-0.206326858655653,0.116971372701702,
-0.484372397012738));
#81408=CARTESIAN_POINT('Ctrl Pts',(-0.204732579325275,0.119754853165022,
-0.48458571473549));
#81409=CARTESIAN_POINT('Ctrl Pts',(-0.203632506803046,0.121616022270201,
-0.48472794438393));
#81410=CARTESIAN_POINT('Ctrl Pts',(-0.194592140694416,0.136444380172736,
-0.485860013904881));
#81411=CARTESIAN_POINT('Ctrl Pts',(-0.185445969751487,0.14863744590539,
-0.486785537049803));
#81412=CARTESIAN_POINT('Ctrl Pts',(-0.164651975309836,0.171424323933707,
-0.488677612033645));
#81413=CARTESIAN_POINT('Ctrl Pts',(-0.152994632713465,0.181904176188249,
-0.489641117585276));
#81414=CARTESIAN_POINT('Ctrl Pts',(-0.13813676467458,0.192816082915931,
-0.490836695426189));
#81415=CARTESIAN_POINT('Ctrl Pts',(-0.135852834256483,0.194432029091879,
-0.491019553968737));
#81416=CARTESIAN_POINT('Ctrl Pts',(-0.132173578805488,0.196938729538459,
-0.491312992359567));
#81417=CARTESIAN_POINT('Ctrl Pts',(-0.130796546645268,0.197855960938178,
-0.491422570144538));
#81418=CARTESIAN_POINT('Ctrl Pts',(-0.128168842334359,0.199566836420298,
-0.491631268692151));
#81419=CARTESIAN_POINT('Ctrl Pts',(-0.126920107262241,0.200363321358311,
-0.491730277351478));
#81420=CARTESIAN_POINT('Ctrl Pts',(-0.124055679386195,0.202152826793797,
-0.49195705238228));
#81421=CARTESIAN_POINT('Ctrl Pts',(-0.122435389493696,0.203138258350459,
-0.492085088998462));
#81422=CARTESIAN_POINT('Ctrl Pts',(-0.117348365169996,0.206149125047098,
-0.492486426520427));
#81423=CARTESIAN_POINT('Ctrl Pts',(-0.11384205862814,0.208105941418819,
-0.492762149445229));
#81424=CARTESIAN_POINT('Ctrl Pts',(-0.0938456168706689,0.218609051507495,
-0.494330456337261));
#81425=CARTESIAN_POINT('Ctrl Pts',(-0.0764481626599829,0.225282854049497,
-0.495686712086374));
#81426=CARTESIAN_POINT('Ctrl Pts',(-0.0529915936470424,0.231248019875964,
-0.497451181145954));
#81427=CARTESIAN_POINT('Ctrl Pts',(-0.0474817943861408,0.232441842789692,
-0.497860620798539));
#81428=CARTESIAN_POINT('Ctrl Pts',(-0.0419358198037385,0.233438145217075,
-0.498265075600824));
#81429=CARTESIAN_POINT('Ctrl Pts',(-0.0419358519811633,0.233438139436584,
-0.517821408604162));
#81430=CARTESIAN_POINT('Ctrl Pts',(-0.0474363747086211,0.232450001390785,
-0.517413505363854));
#81431=CARTESIAN_POINT('Ctrl Pts',(-0.0529036475820301,0.231267149309306,
-0.5170050099961));
#81432=CARTESIAN_POINT('Ctrl Pts',(-0.0639541237075591,0.228463454109606,
-0.516177751915909));
#81433=CARTESIAN_POINT('Ctrl Pts',(-0.0695269999125132,0.226829637732628,
-0.515759708792094));
#81434=CARTESIAN_POINT('Ctrl Pts',(-0.0783878880691696,0.22387455112594,
-0.51509885600743));
#81435=CARTESIAN_POINT('Ctrl Pts',(-0.0817159586215557,0.222681344036066,
-0.514851553249294));
#81436=CARTESIAN_POINT('Ctrl Pts',(-0.0861979953421363,0.220960377579042,
-0.514520868445073));
#81437=CARTESIAN_POINT('Ctrl Pts',(-0.0873760566340872,0.220497183127309,
-0.514434176928649));
#81438=CARTESIAN_POINT('Ctrl Pts',(-0.0893466811362861,0.219704091872445,
-0.514289608902803));
#81439=CARTESIAN_POINT('Ctrl Pts',(-0.0901412532691321,0.219379287910176,
-0.514231441019731));
#81440=CARTESIAN_POINT('Ctrl Pts',(-0.0916655664153254,0.218746501361038,
-0.514120110990824));
#81441=CARTESIAN_POINT('Ctrl Pts',(-0.0923955502470242,0.218439168339515,
-0.51406690886264));
#81442=CARTESIAN_POINT('Ctrl Pts',(-0.0943806966640465,0.217591663149007,
-0.513922501548323));
#81443=CARTESIAN_POINT('Ctrl Pts',(-0.0956327760756426,0.217044281506648,
-0.513831718758105));
#81444=CARTESIAN_POINT('Ctrl Pts',(-0.100543664870647,0.214846600592293,
-0.513476561634498));
#81445=CARTESIAN_POINT('Ctrl Pts',(-0.104165289009907,0.213114258979825,
-0.513216643371228));
#81446=CARTESIAN_POINT('Ctrl Pts',(-0.120457596759089,0.204806479119431,
-0.512048756835134));
#81447=CARTESIAN_POINT('Ctrl Pts',(-0.132563602642342,0.19718695061971,
-0.511183473043809));
#81448=CARTESIAN_POINT('Ctrl Pts',(-0.155046227311638,0.180024635124865,
-0.509446079772267));
#81449=CARTESIAN_POINT('Ctrl Pts',(-0.16540444082263,0.170556444231113,
-0.508577361498009));
#81450=CARTESIAN_POINT('Ctrl Pts',(-0.176734137257871,0.158191879370237,
-0.507489332179975));
#81451=CARTESIAN_POINT('Ctrl Pts',(-0.178566269267511,0.156120826327559,
-0.507308559973476));
#81452=CARTESIAN_POINT('Ctrl Pts',(-0.181431441977682,0.152765591810468,
-0.507017703061679));
#81453=CARTESIAN_POINT('Ctrl Pts',(-0.18248806497027,0.151501815475246,
-0.506908589691881));
#81454=CARTESIAN_POINT('Ctrl Pts',(-0.184470158768019,0.149080306092478,
-0.506700285174179));
#81455=CARTESIAN_POINT('Ctrl Pts',(-0.185398112555181,0.147924699865153,
-0.506601200855444));
#81456=CARTESIAN_POINT('Ctrl Pts',(-0.187495795921603,0.145261652111095,
-0.506373554833203));
#81457=CARTESIAN_POINT('Ctrl Pts',(-0.188658274194058,0.143748656589063,
-0.506244714806875));
#81458=CARTESIAN_POINT('Ctrl Pts',(-0.192161078473539,0.13907398448482,
-0.505848042663517));
#81459=CARTESIAN_POINT('Ctrl Pts',(-0.194441008678585,0.135868113211522,
-0.505577923443962));
#81460=CARTESIAN_POINT('Ctrl Pts',(-0.207043826142121,0.117179694422902,
-0.504013223461699));
#81461=CARTESIAN_POINT('Ctrl Pts',(-0.215594320143711,0.100583709091513,
-0.502654496642408));
#81462=CARTESIAN_POINT('Ctrl Pts',(-0.225646731605244,0.0737352194672967,
-0.50056445184781));
#81463=CARTESIAN_POINT('Ctrl Pts',(-0.228573212470532,0.0640909969134751,
-0.499834974724211));
#81464=CARTESIAN_POINT('Ctrl Pts',(-0.231402801853073,0.0520574648619317,
-0.49897072711782));
#81465=CARTESIAN_POINT('Ctrl Pts',(-0.231895201443057,0.0498181981701591,
-0.498811834512575));
#81466=CARTESIAN_POINT('Ctrl Pts',(-0.232569772829281,0.0465234041106976,
-0.498581207215899));
#81467=CARTESIAN_POINT('Ctrl Pts',(-0.232777373582377,0.0454732979136019,
-0.498508171077071));
#81468=CARTESIAN_POINT('Ctrl Pts',(-0.233118535025439,0.0436840172180781,
-0.498384562006488));
#81469=CARTESIAN_POINT('Ctrl Pts',(-0.233255702961347,0.0429455681829708,
-0.498333791271857));
#81470=CARTESIAN_POINT('Ctrl Pts',(-0.233561377126923,0.0412552790365975,
-0.498218141215521));
#81471=CARTESIAN_POINT('Ctrl Pts',(-0.233727575216785,0.04030304702857,
-0.498153391556591));
#81472=CARTESIAN_POINT('Ctrl Pts',(-0.234173638929645,0.0376517269303887,
-0.497974158228261));
#81473=CARTESIAN_POINT('Ctrl Pts',(-0.234440836215068,0.0359505277811405,
-0.497860351811799));
#81474=CARTESIAN_POINT('Ctrl Pts',(-0.236334195744034,0.0229754365276078,
-0.497000407236665));
#81475=CARTESIAN_POINT('Ctrl Pts',(-0.23716503959585,0.0115989474799725,
-0.496292275500453));
#81476=CARTESIAN_POINT('Ctrl Pts',(-0.237191861597142,-0.0193587470715879,
-0.494386761147839));
#81477=CARTESIAN_POINT('Ctrl Pts',(-0.234788242447255,-0.0388477650666085,
-0.493204015519732));
#81478=CARTESIAN_POINT('Ctrl Pts',(-0.229333442885873,-0.0605480423193224,
-0.491757564325757));
#81479=CARTESIAN_POINT('Ctrl Pts',(-0.228599223550157,-0.0632636338908996,
-0.491574315511196));
#81480=CARTESIAN_POINT('Ctrl Pts',(-0.227311658198912,-0.0677103437442107,
-0.491270199866006));
#81481=CARTESIAN_POINT('Ctrl Pts',(-0.22678639377019,-0.0694493477119902,
-0.491150236588488));
#81482=CARTESIAN_POINT('Ctrl Pts',(-0.225798883753325,-0.0725879941771109,
-0.490931763194872));
#81483=CARTESIAN_POINT('Ctrl Pts',(-0.225343464352043,-0.0739897000198598,
-0.490833480176166));
#81484=CARTESIAN_POINT('Ctrl Pts',(-0.224332568282615,-0.0770051422215605,
-0.490620458013356));
#81485=CARTESIAN_POINT('Ctrl Pts',(-0.223772681184231,-0.0786173009756907,
-0.490505578316715));
#81486=CARTESIAN_POINT('Ctrl Pts',(-0.222165130873761,-0.0830897944873623,
-0.490184035258809));
#81487=CARTESIAN_POINT('Ctrl Pts',(-0.221079720355334,-0.0859361104186254,
-0.489976137257953));
#81488=CARTESIAN_POINT('Ctrl Pts',(-0.218521157628301,-0.0922759698600765,
-0.489505476684963));
#81489=CARTESIAN_POINT('Ctrl Pts',(-0.21701847390357,-0.095756619461184,
-0.489241795583941));
#81490=CARTESIAN_POINT('Ctrl Pts',(-0.211786229519685,-0.10711955407712,
-0.48836328070516));
#81491=CARTESIAN_POINT('Ctrl Pts',(-0.207705743164228,-0.114831633191772,
-0.487738029556811));
#81492=CARTESIAN_POINT('Ctrl Pts',(-0.196664308342083,-0.133177639686777,
-0.486184792103082));
#81493=CARTESIAN_POINT('Ctrl Pts',(-0.189255644617005,-0.143511100302924,
-0.485250529200367));
#81494=CARTESIAN_POINT('Ctrl Pts',(-0.177075470136653,-0.157905747709544,
-0.483893797334847));
#81495=CARTESIAN_POINT('Ctrl Pts',(-0.172913167082312,-0.162453064112888,
-0.483456129411124));
#81496=CARTESIAN_POINT('Ctrl Pts',(-0.16746906007165,-0.167954101850235,
-0.482920138893986));
#81497=CARTESIAN_POINT('Ctrl Pts',(-0.166348838695005,-0.169063688027147,
-0.482811677001675));
#81498=CARTESIAN_POINT('Ctrl Pts',(-0.164553929112457,-0.170806442289736,
-0.482640882851405));
#81499=CARTESIAN_POINT('Ctrl Pts',(-0.163886481172157,-0.171446952952293,
-0.48257801483154));
#81500=CARTESIAN_POINT('Ctrl Pts',(-0.162600626980336,-0.172666541088275,
-0.48245815277016));
#81501=CARTESIAN_POINT('Ctrl Pts',(-0.161982846085595,-0.173246229111305,
-0.482401115458312));
#81502=CARTESIAN_POINT('Ctrl Pts',(-0.160479178310591,-0.174642105022481,
-0.482263579109867));
#81503=CARTESIAN_POINT('Ctrl Pts',(-0.159590139608728,-0.175454891671309,
-0.482183332203441));
#81504=CARTESIAN_POINT('Ctrl Pts',(-0.156391825620771,-0.178334465188169,
-0.481898276826869));
#81505=CARTESIAN_POINT('Ctrl Pts',(-0.154048173734127,-0.180362820378453,
-0.481696077325965));
#81506=CARTESIAN_POINT('Ctrl Pts',(-0.147975952278621,-0.18541339204013,
-0.481186910370073));
#81507=CARTESIAN_POINT('Ctrl Pts',(-0.144194083644675,-0.18836953127005,
-0.480883400976566));
#81508=CARTESIAN_POINT('Ctrl Pts',(-0.126034239725389,-0.201696715798944,
-0.479474880747289));
#81509=CARTESIAN_POINT('Ctrl Pts',(-0.110612835566416,-0.210549375116307,
-0.478413363290233));
#81510=CARTESIAN_POINT('Ctrl Pts',(-0.0873439737509716,-0.22063838791123,
-0.476824649177911));
#81511=CARTESIAN_POINT('Ctrl Pts',(-0.08019749745354,-0.22333520018733,
-0.476338998764583));
#81512=CARTESIAN_POINT('Ctrl Pts',(-0.0705963671478269,-0.22643800129007,
-0.475682121669746));
#81513=CARTESIAN_POINT('Ctrl Pts',(-0.0682472868567034,-0.227157043876955,
-0.475521084603522));
#81514=CARTESIAN_POINT('Ctrl Pts',(-0.0643680360670255,-0.228278861281466,
-0.475254412055304));
#81515=CARTESIAN_POINT('Ctrl Pts',(-0.0628442151540498,-0.228703054181387,
-0.47514947499829));
#81516=CARTESIAN_POINT('Ctrl Pts',(-0.059862728825461,-0.229500977144621,
-0.47494374245077));
#81517=CARTESIAN_POINT('Ctrl Pts',(-0.0584055222583933,-0.229876139698764,
-0.474842998757251));
#81518=CARTESIAN_POINT('Ctrl Pts',(-0.0549422779374243,-0.230732707765821,
-0.474603067246757));
#81519=CARTESIAN_POINT('Ctrl Pts',(-0.052933362995506,-0.231201848939181,
-0.474463494162119));
#81520=CARTESIAN_POINT('Ctrl Pts',(-0.0460224206253254,-0.232720967451871,
-0.473981852283147));
#81521=CARTESIAN_POINT('Ctrl Pts',(-0.0410936578333632,-0.23364164149369,
-0.473635758173797));
#81522=CARTESIAN_POINT('Ctrl Pts',(-0.0287998332566006,-0.235537056444383,
-0.472765583326596));
#81523=CARTESIAN_POINT('Ctrl Pts',(-0.0214114705284497,-0.236323225247371,
-0.472236432372466));
#81524=CARTESIAN_POINT('Ctrl Pts',(-0.00500772401503966,-0.23729312773985,
-0.471051021716483));
#81525=CARTESIAN_POINT('Ctrl Pts',(0.0040062119849757,-0.237312124539667,
-0.470392508379135));
#81526=CARTESIAN_POINT('Ctrl Pts',(0.0245962114854714,-0.23618193827456,
-0.468888181766194));
#81527=CARTESIAN_POINT('Ctrl Pts',(0.0361323536563384,-0.234694256886078,
-0.468045052995556));
#81528=CARTESIAN_POINT('Ctrl Pts',(0.0492054890819199,-0.232021078533424,
-0.467118600397889));
#81529=CARTESIAN_POINT('Ctrl Pts',(0.0508931145627777,-0.231656755485669,
-0.466999585794828));
#81530=CARTESIAN_POINT('Ctrl Pts',(0.0535201861045875,-0.231059530277086,
-0.466815385709719));
#81531=CARTESIAN_POINT('Ctrl Pts',(0.054462400505281,-0.230839259804835,
-0.466749536432177));
#81532=CARTESIAN_POINT('Ctrl Pts',(0.0561334095516349,-0.230437811227578,
-0.466633167763421));
#81533=CARTESIAN_POINT('Ctrl Pts',(0.0568627035468804,-0.230258935722715,
-0.466582523562648));
#81534=CARTESIAN_POINT('Ctrl Pts',(0.0586281207009968,-0.229817028811714,
-0.466460263420599));
#81535=CARTESIAN_POINT('Ctrl Pts',(0.0596633316924259,-0.229550452471458,
-0.466388849487474));
#81536=CARTESIAN_POINT('Ctrl Pts',(0.0629053871605886,-0.228692179432054,
-0.466165965575008));
#81537=CARTESIAN_POINT('Ctrl Pts',(0.0651055805920964,-0.228075568583827,
-0.466015828782985));
#81538=CARTESIAN_POINT('Ctrl Pts',(0.0768764022367824,-0.224592535889649,
-0.465216946794672));
#81539=CARTESIAN_POINT('Ctrl Pts',(0.0862686413014294,-0.221155047170527,
-0.464594762711305));
#81540=CARTESIAN_POINT('Ctrl Pts',(0.112231371224865,-0.209746084648454,
-0.462847169024363));
#81541=CARTESIAN_POINT('Ctrl Pts',(0.128129273282322,-0.200429900160325,
-0.461738256465763));
#81542=CARTESIAN_POINT('Ctrl Pts',(0.146147297677237,-0.186843778130154,
-0.460292991855457));
#81543=CARTESIAN_POINT('Ctrl Pts',(0.149433723081102,-0.184225918383934,
-0.46002098582327));
#81544=CARTESIAN_POINT('Ctrl Pts',(0.154109529990292,-0.180293861019471,
-0.459620413415811));
#81545=CARTESIAN_POINT('Ctrl Pts',(0.155555397168203,-0.179047875200486,
-0.459494581118363));
#81546=CARTESIAN_POINT('Ctrl Pts',(0.158100075016996,-0.176800892755009,
-0.45926948927998));
#81547=CARTESIAN_POINT('Ctrl Pts',(0.159204822273176,-0.175806751272082,
-0.459170516950115));
#81548=CARTESIAN_POINT('Ctrl Pts',(0.161501654315041,-0.173700472032592,
-0.458962057394118));
#81549=CARTESIAN_POINT('Ctrl Pts',(0.162691757211531,-0.172586297940097,
-0.458852486818846));
#81550=CARTESIAN_POINT('Ctrl Pts',(0.16581135277148,-0.169604791959639,
-0.458561048180622));
#81551=CARTESIAN_POINT('Ctrl Pts',(0.167720735058996,-0.167716857133169,
-0.458378296916408));
#81552=CARTESIAN_POINT('Ctrl Pts',(0.177853310873583,-0.157352009520242,
-0.457384106102446));
#81553=CARTESIAN_POINT('Ctrl Pts',(0.18546547780925,-0.148303524315382,
-0.456547097401718));
#81554=CARTESIAN_POINT('Ctrl Pts',(0.201168075150133,-0.126528911262841,
-0.45460647208975));
#81555=CARTESIAN_POINT('Ctrl Pts',(0.208784357212976,-0.113521997333308,
-0.453495982675036));
#81556=CARTESIAN_POINT('Ctrl Pts',(0.217358324734248,-0.0950560159413913,
-0.452037395009256));
#81557=CARTESIAN_POINT('Ctrl Pts',(0.219436103982255,-0.0901559394699398,
-0.451661069967338));
#81558=CARTESIAN_POINT('Ctrl Pts',(0.221888315157406,-0.0837843883339581,
-0.451188799170902));
#81559=CARTESIAN_POINT('Ctrl Pts',(0.222415806514101,-0.0823738880858151,
-0.451085303282932));
#81560=CARTESIAN_POINT('Ctrl Pts',(0.223240318901954,-0.0801034827217346,
-0.450920501158236));
#81561=CARTESIAN_POINT('Ctrl Pts',(0.223545879012346,-0.0792467537152166,
-0.450858719302756));
#81562=CARTESIAN_POINT('Ctrl Pts',(0.224128986056774,-0.0775816260578697,
-0.450739454934526));
#81563=CARTESIAN_POINT('Ctrl Pts',(0.224407102023338,-0.0767734568742039,
-0.450681942686566));
#81564=CARTESIAN_POINT('Ctrl Pts',(0.22508004407438,-0.0747830718956505,
-0.450541176337997));
#81565=CARTESIAN_POINT('Ctrl Pts',(0.22546993872044,-0.0735991914731807,
-0.450458204608852));
#81566=CARTESIAN_POINT('Ctrl Pts',(0.226885885281138,-0.0691829195967079,
-0.450151305012192));
#81567=CARTESIAN_POINT('Ctrl Pts',(0.227851960497856,-0.0659315420715444,
-0.449930541175777));
#81568=CARTESIAN_POINT('Ctrl Pts',(0.230191148893845,-0.0573920975881784,
-0.44936145706513));
#81569=CARTESIAN_POINT('Ctrl Pts',(0.231451938620924,-0.0520751931532557,
-0.449017710949226));
#81570=CARTESIAN_POINT('Ctrl Pts',(0.234506021520461,-0.036874581640039,
-0.44805283837193));
#81571=CARTESIAN_POINT('Ctrl Pts',(0.235856854352183,-0.0269140399993006,
-0.447441360666662));
#81572=CARTESIAN_POINT('Ctrl Pts',(0.237540433790436,-0.00334335838640604,
-0.445989117417048));
#81573=CARTESIAN_POINT('Ctrl Pts',(0.237341843897199,0.0102672828883438,
-0.445145320104005));
#81574=CARTESIAN_POINT('Ctrl Pts',(0.235698533997672,0.0265710807385324,
-0.444082592714595));
#81575=CARTESIAN_POINT('Ctrl Pts',(0.23536841938081,0.0293517860144907,
-0.443899578232512));
#81576=CARTESIAN_POINT('Ctrl Pts',(0.234765023559825,0.0337654045215603,
-0.44360596868346));
#81577=CARTESIAN_POINT('Ctrl Pts',(0.234523736615272,0.0354024795756392,
-0.44349637820177));
#81578=CARTESIAN_POINT('Ctrl Pts',(0.234034144551942,0.0384992444855046,
-0.443287706248749));
#81579=CARTESIAN_POINT('Ctrl Pts',(0.233789261356166,0.0399594012206306,
-0.443188737350116));
#81580=CARTESIAN_POINT('Ctrl Pts',(0.233199881109878,0.043282624234656,
-0.442962125832387));
#81581=CARTESIAN_POINT('Ctrl Pts',(0.232846701875595,0.0451440270073093,
-0.442834213972802));
#81582=CARTESIAN_POINT('Ctrl Pts',(0.23167723951048,0.0509283012195884,
-0.442433562950964));
#81583=CARTESIAN_POINT('Ctrl Pts',(0.230783860115667,0.0548346761049098,
-0.44215841301894));
#81584=CARTESIAN_POINT('Ctrl Pts',(0.226210987774366,0.0727310457667311,
-0.440875957642474));
#81585=CARTESIAN_POINT('Ctrl Pts',(0.221355918781468,0.0863866515042328,
-0.439832420772612));
#81586=CARTESIAN_POINT('Ctrl Pts',(0.209308573419601,0.112450118617004,
-0.437737996345271));
#81587=CARTESIAN_POINT('Ctrl Pts',(0.202174241546572,0.124822876991005,
-0.436692094656722));
#81588=CARTESIAN_POINT('Ctrl Pts',(0.192684002517075,0.138310743835322,
-0.43553981688051));
#81589=CARTESIAN_POINT('Ctrl Pts',(0.191370603419139,0.140122374148513,
-0.435384821033287));
#81590=CARTESIAN_POINT('Ctrl Pts',(0.189397388534701,0.142764609239526,
-0.435158740443828));
#81591=CARTESIAN_POINT('Ctrl Pts',(0.188757368299707,0.143609750559554,
-0.435086423464367));
#81592=CARTESIAN_POINT('Ctrl Pts',(0.18760623413405,0.1451088222302,-0.434958187119187));
#81593=CARTESIAN_POINT('Ctrl Pts',(0.187097331179468,0.145764392447521,
-0.43490212250994));
#81594=CARTESIAN_POINT('Ctrl Pts',(0.18596151183434,0.147211808867722,-0.434778373972197));
#81595=CARTESIAN_POINT('Ctrl Pts',(0.185332969538141,0.148002334608258,
-0.434710805129797));
#81596=CARTESIAN_POINT('Ctrl Pts',(0.183457409672624,0.150330565343857,
-0.4345117755574));
#81597=CARTESIAN_POINT('Ctrl Pts',(0.18219613187673,0.151856742353953,-0.434381273204359));
#81598=CARTESIAN_POINT('Ctrl Pts',(0.179224250213282,0.155362453789661,
-0.434080933991697));
#81599=CARTESIAN_POINT('Ctrl Pts',(0.177499686395286,0.157329865053322,
-0.433911950848822));
#81600=CARTESIAN_POINT('Ctrl Pts',(0.171310352369061,0.164159412161296,
-0.433322135447074));
#81601=CARTESIAN_POINT('Ctrl Pts',(0.16667529190237,0.168863579460885,-0.432909927488604));
#81602=CARTESIAN_POINT('Ctrl Pts',(0.146598175691034,0.187606747740174,
-0.431211477253744));
#81603=CARTESIAN_POINT('Ctrl Pts',(0.129535996403746,0.199769128416463,
-0.429959671403605));
#81604=CARTESIAN_POINT('Ctrl Pts',(0.108392180397272,0.21097992788225,-0.428416658049038));
#81605=CARTESIAN_POINT('Ctrl Pts',(0.105653876589978,0.212364431400599,
-0.428217188673281));
#81606=CARTESIAN_POINT('Ctrl Pts',(0.101185545933529,0.214515833468829,
-0.427891820819048));
#81607=CARTESIAN_POINT('Ctrl Pts',(0.0994717988380659,0.215315857303474,
-0.427767062057602));
#81608=CARTESIAN_POINT('Ctrl Pts',(0.0964000803457126,0.216705320834227,
-0.427543402880788));
#81609=CARTESIAN_POINT('Ctrl Pts',(0.0950457985746646,0.21730270953729,
-0.427444780326438));
#81610=CARTESIAN_POINT('Ctrl Pts',(0.0921641005951461,0.218541766529488,
-0.427234852314439));
#81611=CARTESIAN_POINT('Ctrl Pts',(0.0906353814136036,0.219180182843437,
-0.427123442951149));
#81612=CARTESIAN_POINT('Ctrl Pts',(0.0864967862554318,0.220857822300506,
-0.426821648550179));
#81613=CARTESIAN_POINT('Ctrl Pts',(0.0838749988925018,0.221866750749245,
-0.426630265010702));
#81614=CARTESIAN_POINT('Ctrl Pts',(0.0780271231807158,0.223998692301575,
-0.426202777279461));
#81615=CARTESIAN_POINT('Ctrl Pts',(0.0747934942543724,0.22509903882262,
-0.425965988385402));
#81616=CARTESIAN_POINT('Ctrl Pts',(0.0644913744791733,0.228358179068569,
-0.425210191062396));
#81617=CARTESIAN_POINT('Ctrl Pts',(0.0573456574394171,0.230256495304766,
-0.424683738611355));
#81618=CARTESIAN_POINT('Ctrl Pts',(0.0412858622062586,0.23372893323647,
-0.423498652320382));
#81619=CARTESIAN_POINT('Ctrl Pts',(0.032346435169881,0.235132798464378,
-0.422837608714053));
#81620=CARTESIAN_POINT('Ctrl Pts',(0.0117668686477449,0.237168679492262,
-0.421328945360437));
#81621=CARTESIAN_POINT('Ctrl Pts',(0.000114663382083139,0.237460498622356,
-0.420483994371155));
#81622=CARTESIAN_POINT('Ctrl Pts',(-0.013237917530875,0.236811572088418,
-0.419555818733266));
#81623=CARTESIAN_POINT('Ctrl Pts',(-0.0149619725548211,0.236708899168758,
-0.419436761457891));
#81624=CARTESIAN_POINT('Ctrl Pts',(-0.0176501399456274,0.236519321989584,
-0.419252509798154));
#81625=CARTESIAN_POINT('Ctrl Pts',(-0.018615062249009,0.236445335448843,
-0.419186651046793));
#81626=CARTESIAN_POINT('Ctrl Pts',(-0.0203278645731972,0.236303454058981,
-0.419070274300169));
#81627=CARTESIAN_POINT('Ctrl Pts',(-0.0210758870510178,0.236237912890664,
-0.419019631392924));
#81628=CARTESIAN_POINT('Ctrl Pts',(-0.0228878334594393,0.236070476613085,
-0.418897385477494));
#81629=CARTESIAN_POINT('Ctrl Pts',(-0.023951396821383,0.235964941355194,
-0.418825984344563));
#81630=CARTESIAN_POINT('Ctrl Pts',(-0.0272851828667561,0.235611363545848,
-0.418603182578419));
#81631=CARTESIAN_POINT('Ctrl Pts',(-0.0295526355931031,0.235337711610666,
-0.418453113735775));
#81632=CARTESIAN_POINT('Ctrl Pts',(-0.0352008980436093,0.234573113764485,
-0.418082165477073));
#81633=CARTESIAN_POINT('Ctrl Pts',(-0.0385749975013287,0.234041897731114,
-0.417863152886784));
#81634=CARTESIAN_POINT('Ctrl Pts',(-0.0419358280420692,0.233438143737107,
-0.417646538149483));
#81635=CARTESIAN_POINT('Origin',(0.,0.,-1.7456589891905));
#81636=CARTESIAN_POINT('',(-0.0419358007114473,0.233438148646895,-0.298061760785893));
#81637=CARTESIAN_POINT('',(-0.0419358257618152,0.233438144146741,-0.318008956663326));
#81638=CARTESIAN_POINT('',(-0.0419358257166344,0.233438144154858,-1.7456589891905));
#81639=CARTESIAN_POINT('Ctrl Pts',(-0.0419358007114439,0.233438148646895,
-0.298061760785893));
#81640=CARTESIAN_POINT('Ctrl Pts',(-0.0297893085885032,0.23562019505175,
-0.298821763567408));
#81641=CARTESIAN_POINT('Ctrl Pts',(-0.0174860841807818,0.236851817310879,
-0.299591780052587));
#81642=CARTESIAN_POINT('Ctrl Pts',(-0.00231027385586464,0.237180603483249,
-0.300575944362926));
#81643=CARTESIAN_POINT('Ctrl Pts',(0.000517444212155474,0.237191288158712,
-0.30076071581006));
#81644=CARTESIAN_POINT('Ctrl Pts',(0.00500531661435507,0.237127995007377,
-0.301056502375512));
#81645=CARTESIAN_POINT('Ctrl Pts',(0.00666572203421282,0.237087129816031,
-0.301166486719452));
#81646=CARTESIAN_POINT('Ctrl Pts',(0.00980455108933783,0.23697687991778,
-0.30137550591229));
#81647=CARTESIAN_POINT('Ctrl Pts',(0.011283027490894,0.236911088718465,
-0.30147442381241));
#81648=CARTESIAN_POINT('Ctrl Pts',(0.0146434567019853,0.23673002476781,
-0.301700355023327));
#81649=CARTESIAN_POINT('Ctrl Pts',(0.0165248249644296,0.236606139511143,
-0.301827631146487));
#81650=CARTESIAN_POINT('Ctrl Pts',(0.0214423077496373,0.236223395172807,
-0.302162445564757));
#81651=CARTESIAN_POINT('Ctrl Pts',(0.0244751778925771,0.235928440765466,
-0.302371087982261));
#81652=CARTESIAN_POINT('Ctrl Pts',(0.0446116223629093,0.233577681224988,
-0.303771171124661));
#81653=CARTESIAN_POINT('Ctrl Pts',(0.0614503940892971,0.229722388557461,
-0.305018912125014));
#81654=CARTESIAN_POINT('Ctrl Pts',(0.0898160050584016,0.219884011388673,
-0.307210581904954));
#81655=CARTESIAN_POINT('Ctrl Pts',(0.101553576667183,0.214715691855634,
-0.308145159063142));
#81656=CARTESIAN_POINT('Ctrl Pts',(0.114605246062226,0.20765776921121,-0.309179293645274));
#81657=CARTESIAN_POINT('Ctrl Pts',(0.116380623189711,0.206668001329654,
-0.309319818881318));
#81658=CARTESIAN_POINT('Ctrl Pts',(0.119028126340582,0.205147087378855,
-0.309528913082343));
#81659=CARTESIAN_POINT('Ctrl Pts',(0.119909853005656,0.204632963056893,
-0.309598471812567));
#81660=CARTESIAN_POINT('Ctrl Pts',(0.121502335724596,0.203690577886412,
-0.309723921279298));
#81661=CARTESIAN_POINT('Ctrl Pts',(0.122214184277925,0.203264267190231,
-0.309779928378966));
#81662=CARTESIAN_POINT('Ctrl Pts',(0.123820596145058,0.202290731803867,
-0.309906167867792));
#81663=CARTESIAN_POINT('Ctrl Pts',(0.124713782161633,0.201741301786073,
-0.309976257179257));
#81664=CARTESIAN_POINT('Ctrl Pts',(0.127449042647001,0.200033638892799,
-0.310190677841086));
#81665=CARTESIAN_POINT('Ctrl Pts',(0.12927890500043,0.198855929514595,-0.310333816342355));
#81666=CARTESIAN_POINT('Ctrl Pts',(0.143531765398326,0.189402797415757,
-0.311448461280709));
#81667=CARTESIAN_POINT('Ctrl Pts',(0.155166284561794,0.179995371079051,
-0.312358127668875));
#81668=CARTESIAN_POINT('Ctrl Pts',(0.177200036976499,0.158444388930571,
-0.314248327045214));
#81669=CARTESIAN_POINT('Ctrl Pts',(0.187413037060893,0.146221559955588,
-0.31522627794353));
#81670=CARTESIAN_POINT('Ctrl Pts',(0.197898272716074,0.130752048413538,
-0.316438274970184));
#81671=CARTESIAN_POINT('Ctrl Pts',(0.199428396994282,0.128406144338102,
-0.316621326644017));
#81672=CARTESIAN_POINT('Ctrl Pts',(0.201796128833071,0.124631627794973,
-0.31691500223915));
#81673=CARTESIAN_POINT('Ctrl Pts',(0.202660965195212,0.123220344145537,
-0.317024621216795));
#81674=CARTESIAN_POINT('Ctrl Pts',(0.204271501626648,0.120529364084131,
-0.317233352126886));
#81675=CARTESIAN_POINT('Ctrl Pts',(0.205020127302784,0.119251504029019,
-0.317332351464893));
#81676=CARTESIAN_POINT('Ctrl Pts',(0.206699401028356,0.11632252715147,-0.317559040102009));
#81677=CARTESIAN_POINT('Ctrl Pts',(0.207622313192363,0.114667115648396,
-0.317686998882905));
#81678=CARTESIAN_POINT('Ctrl Pts',(0.209993279512116,0.110291871343819,
-0.318024856183737));
#81679=CARTESIAN_POINT('Ctrl Pts',(0.211408303113036,0.107554647299553,
-0.318235891834305));
#81680=CARTESIAN_POINT('Ctrl Pts',(0.220093510702782,0.0899200009154866,
-0.319593910405852));
#81681=CARTESIAN_POINT('Ctrl Pts',(0.225837072913105,0.0743249208342053,
-0.320792519713154));
#81682=CARTESIAN_POINT('Ctrl Pts',(0.233194449599296,0.0452918296322218,
-0.322978693785453));
#81683=CARTESIAN_POINT('Ctrl Pts',(0.235378100138485,0.0320658496346263,
-0.323957191538426));
#81684=CARTESIAN_POINT('Ctrl Pts',(0.23659559034029,0.0166931846818326,
-0.325032039068426));
#81685=CARTESIAN_POINT('Ctrl Pts',(0.236730329093093,0.0146590506293287,
-0.325172984316573));
#81686=CARTESIAN_POINT('Ctrl Pts',(0.236893215690123,0.0116029780654488,
-0.325382574634235));
#81687=CARTESIAN_POINT('Ctrl Pts',(0.2369410074006,0.0105822421729668,-0.325452216171253));
#81688=CARTESIAN_POINT('Ctrl Pts',(0.237015650075542,0.00873216322104528,
-0.3255777469698));
#81689=CARTESIAN_POINT('Ctrl Pts',(0.237044747402458,0.00790296359198541,
-0.325633753467595));
#81690=CARTESIAN_POINT('Ctrl Pts',(0.237100729613421,0.00602673356105983,
-0.325759907420457));
#81691=CARTESIAN_POINT('Ctrl Pts',(0.237125031534582,0.0049796610259576,
-0.325829912724129));
#81692=CARTESIAN_POINT('Ctrl Pts',(0.237178362713998,0.00176356806922175,
-0.326043807821247));
#81693=CARTESIAN_POINT('Ctrl Pts',(0.237184573830235,-0.000405786584734266,
-0.326186513199995));
#81694=CARTESIAN_POINT('Ctrl Pts',(0.236997365511169,-0.0176478373770175,
-0.327310400882714));
#81695=CARTESIAN_POINT('Ctrl Pts',(0.23539712196086,-0.0326728870351739,
-0.328228446985695));
#81696=CARTESIAN_POINT('Ctrl Pts',(0.22922884080715,-0.0628838900572946,
-0.330119553265089));
#81697=CARTESIAN_POINT('Ctrl Pts',(0.224546803012788,-0.0779672542575167,
-0.331089803351203));
#81698=CARTESIAN_POINT('Ctrl Pts',(0.217313081367398,-0.0950517779112877,
-0.332293045867123));
#81699=CARTESIAN_POINT('Ctrl Pts',(0.216176194067849,-0.0976097733871866,
-0.332475998376491));
#81700=CARTESIAN_POINT('Ctrl Pts',(0.214295579824038,-0.101647054202413,
-0.332769552101947));
#81701=CARTESIAN_POINT('Ctrl Pts',(0.213581154359888,-0.103139756781484,
-0.332879149852138));
#81702=CARTESIAN_POINT('Ctrl Pts',(0.212197843102551,-0.105953997307736,
-0.333087863937538));
#81703=CARTESIAN_POINT('Ctrl Pts',(0.211532081613161,-0.107276989332966,
-0.333186867930015));
#81704=CARTESIAN_POINT('Ctrl Pts',(0.209985945376274,-0.110279089698537,
-0.333413600520709));
#81705=CARTESIAN_POINT('Ctrl Pts',(0.209097749912335,-0.111954032976298,
-0.333541598990835));
#81706=CARTESIAN_POINT('Ctrl Pts',(0.206712601455663,-0.116324490267696,
-0.333879633991582));
#81707=CARTESIAN_POINT('Ctrl Pts',(0.205183041720243,-0.119001699484301,
-0.334090809600304));
#81708=CARTESIAN_POINT('Ctrl Pts',(0.195124766642023,-0.13583616441064,
-0.335445608342885));
#81709=CARTESIAN_POINT('Ctrl Pts',(0.185189378096135,-0.149096784624521,
-0.336640516861855));
#81710=CARTESIAN_POINT('Ctrl Pts',(0.164833840858079,-0.171061400033419,
-0.338826345686244));
#81711=CARTESIAN_POINT('Ctrl Pts',(0.154888436952225,-0.180116178070267,
-0.339808246668663));
#81712=CARTESIAN_POINT('Ctrl Pts',(0.142610835718936,-0.189521205107273,
-0.340886243862465));
#81713=CARTESIAN_POINT('Ctrl Pts',(0.140976283305255,-0.190740205227509,
-0.341027221409113));
#81714=CARTESIAN_POINT('Ctrl Pts',(0.138499149962718,-0.192538334836794,
-0.341236849740157));
#81715=CARTESIAN_POINT('Ctrl Pts',(0.137668261964386,-0.193133308021363,
-0.341306497512754));
#81716=CARTESIAN_POINT('Ctrl Pts',(0.13615583113173,-0.194201592933205,
-0.341432034339472));
#81717=CARTESIAN_POINT('Ctrl Pts',(0.13547563034235,-0.194676713249751,
-0.341488040696597));
#81718=CARTESIAN_POINT('Ctrl Pts',(0.133931262067865,-0.195743440068335,
-0.341614187851057));
#81719=CARTESIAN_POINT('Ctrl Pts',(0.133065656027571,-0.196332902434561,
-0.341684186568501));
#81720=CARTESIAN_POINT('Ctrl Pts',(0.130395619751379,-0.198125379449999,
-0.341898040608991));
#81721=CARTESIAN_POINT('Ctrl Pts',(0.128578513749884,-0.199309433413533,
-0.342040712173639));
#81722=CARTESIAN_POINT('Ctrl Pts',(0.113995770282891,-0.208529312537002,
-0.343165248683038));
#81723=CARTESIAN_POINT('Ctrl Pts',(0.10050445425452,-0.215356657366352,
-0.344083885091623));
#81724=CARTESIAN_POINT('Ctrl Pts',(0.0719574549628525,-0.226531385666714,
-0.345964079833396));
#81725=CARTESIAN_POINT('Ctrl Pts',(0.0569389721016377,-0.230764414914573,
-0.346922668523748));
#81726=CARTESIAN_POINT('Ctrl Pts',(0.0387637899545327,-0.234003712007533,
-0.348118793231333));
#81727=CARTESIAN_POINT('Ctrl Pts',(0.0359035505199509,-0.234459596772095,
-0.348307944715936));
#81728=CARTESIAN_POINT('Ctrl Pts',(0.031376679006716,-0.235096345591903,
-0.348609107946534));
#81729=CARTESIAN_POINT('Ctrl Pts',(0.0297151904271129,-0.235312122322688,
-0.348720021898876));
#81730=CARTESIAN_POINT('Ctrl Pts',(0.0265843208329051,-0.235685039690455,
-0.348929802641364));
#81731=CARTESIAN_POINT('Ctrl Pts',(0.0251154794176729,-0.235846086615878,
-0.349028541592293));
#81732=CARTESIAN_POINT('Ctrl Pts',(0.0217925963526855,-0.23617902146097,
-0.349252682596646));
#81733=CARTESIAN_POINT('Ctrl Pts',(0.0199378613752886,-0.236342820442584,
-0.349378331574464));
#81734=CARTESIAN_POINT('Ctrl Pts',(0.0151239323796517,-0.236710889589636,
-0.349705930961519));
#81735=CARTESIAN_POINT('Ctrl Pts',(0.0121625701170361,-0.236881508543861,
-0.349908909017341));
#81736=CARTESIAN_POINT('Ctrl Pts',(-0.00899732842890131,-0.237702819168099,
-0.351370133998079));
#81737=CARTESIAN_POINT('Ctrl Pts',(-0.0272112440068833,-0.236311007626842,
-0.352692305438812));
#81738=CARTESIAN_POINT('Ctrl Pts',(-0.0568483972826379,-0.230572894833667,
-0.354895619269897));
#81739=CARTESIAN_POINT('Ctrl Pts',(-0.0684256939039571,-0.227406206223094,
-0.355768100042965));
#81740=CARTESIAN_POINT('Ctrl Pts',(-0.0816212137539605,-0.222697226599945,
-0.356744476529759));
#81741=CARTESIAN_POINT('Ctrl Pts',(-0.0835187791176015,-0.221992548265628,
-0.356884406017405));
#81742=CARTESIAN_POINT('Ctrl Pts',(-0.0863577643822186,-0.220896707593825,
-0.357092796561104));
#81743=CARTESIAN_POINT('Ctrl Pts',(-0.0873060087839281,-0.220523649121268,
-0.3571622379));
#81744=CARTESIAN_POINT('Ctrl Pts',(-0.0890220557447235,-0.219835717711923,
-0.357287572559194));
#81745=CARTESIAN_POINT('Ctrl Pts',(-0.089790632133962,-0.219522918211441,
-0.357343581002454));
#81746=CARTESIAN_POINT('Ctrl Pts',(-0.0915284653788229,-0.218804991071039,
-0.357469943850697));
#81747=CARTESIAN_POINT('Ctrl Pts',(-0.0924966881684012,-0.218397451620967,
-0.357540153849912));
#81748=CARTESIAN_POINT('Ctrl Pts',(-0.0954709386570211,-0.217122217495248,
-0.357755331342528));
#81749=CARTESIAN_POINT('Ctrl Pts',(-0.0974677699745459,-0.216233189185981,
-0.357899093783551));
#81750=CARTESIAN_POINT('Ctrl Pts',(-0.112828832734564,-0.20913810312954,
-0.359001713644842));
#81751=CARTESIAN_POINT('Ctrl Pts',(-0.125602570435149,-0.201725566547404,
-0.359900411589748));
#81752=CARTESIAN_POINT('Ctrl Pts',(-0.150471696916894,-0.184010142553203,
-0.361772908805763));
#81753=CARTESIAN_POINT('Ctrl Pts',(-0.162387222234084,-0.173585055958464,
-0.362744184737375));
#81754=CARTESIAN_POINT('Ctrl Pts',(-0.175192874676087,-0.159900393967547,
-0.363957810890037));
#81755=CARTESIAN_POINT('Ctrl Pts',(-0.177167651876346,-0.157709546972967,
-0.364150354506782));
#81756=CARTESIAN_POINT('Ctrl Pts',(-0.180206689772604,-0.154208865985483,
-0.364455680534753));
#81757=CARTESIAN_POINT('Ctrl Pts',(-0.181298743208269,-0.152923480380442,
-0.364567312004296));
#81758=CARTESIAN_POINT('Ctrl Pts',(-0.183320716388196,-0.150491444160723,
-0.364777704068082));
#81759=CARTESIAN_POINT('Ctrl Pts',(-0.184253824306558,-0.149347540595696,
-0.364876328565223));
#81760=CARTESIAN_POINT('Ctrl Pts',(-0.18632909156537,-0.146754403212297,
-0.365099203826542));
#81761=CARTESIAN_POINT('Ctrl Pts',(-0.187465128034384,-0.145300415219578,
-0.365223690170512));
#81762=CARTESIAN_POINT('Ctrl Pts',(-0.190348086560378,-0.141520485216699,
-0.365546167866041));
#81763=CARTESIAN_POINT('Ctrl Pts',(-0.192069346640967,-0.139175452478701,
-0.365745134118932));
#81764=CARTESIAN_POINT('Ctrl Pts',(-0.206226152748358,-0.11912538256697,
-0.367437797750914));
#81765=CARTESIAN_POINT('Ctrl Pts',(-0.216226212613638,-0.0998294975689819,
-0.369025617893774));
#81766=CARTESIAN_POINT('Ctrl Pts',(-0.225576756778854,-0.0735297021672426,
-0.371054503469704));
#81767=CARTESIAN_POINT('Ctrl Pts',(-0.227446285401341,-0.0675254581974951,
-0.371508238048471));
#81768=CARTESIAN_POINT('Ctrl Pts',(-0.229732408050907,-0.0590036928393934,
-0.372133437064782));
#81769=CARTESIAN_POINT('Ctrl Pts',(-0.230350346826438,-0.0565432039888334,
-0.372311786264622));
#81770=CARTESIAN_POINT('Ctrl Pts',(-0.231369574270329,-0.0521904190140774,
-0.372622969092079));
#81771=CARTESIAN_POINT('Ctrl Pts',(-0.231787406936192,-0.0503022695201936,
-0.37275653137942));
#81772=CARTESIAN_POINT('Ctrl Pts',(-0.232386378680184,-0.0474294544524633,
-0.372957381533114));
#81773=CARTESIAN_POINT('Ctrl Pts',(-0.232584443055373,-0.0464484562307289,
-0.373025550821621));
#81774=CARTESIAN_POINT('Ctrl Pts',(-0.232935556149919,-0.0446508398639056,
-0.37314966958429));
#81775=CARTESIAN_POINT('Ctrl Pts',(-0.23309052732003,-0.0438346544808771,
-0.373205720629513));
#81776=CARTESIAN_POINT('Ctrl Pts',(-0.233435647618594,-0.0419634152558728,
-0.373333544425463));
#81777=CARTESIAN_POINT('Ctrl Pts',(-0.233622935946281,-0.0409078685523452,
-0.37340515741755));
#81778=CARTESIAN_POINT('Ctrl Pts',(-0.234189554032502,-0.0375835646168496,
-0.373629253886288));
#81779=CARTESIAN_POINT('Ctrl Pts',(-0.234543053375111,-0.0353104605006836,
-0.373780383812952));
#81780=CARTESIAN_POINT('Ctrl Pts',(-0.236392755853335,-0.0221589320369147,
-0.374644540480458));
#81781=CARTESIAN_POINT('Ctrl Pts',(-0.237165284880642,-0.0111909665116149,
-0.37532525327104));
#81782=CARTESIAN_POINT('Ctrl Pts',(-0.237191493369619,0.0187185899535097,
-0.377164510361014));
#81783=CARTESIAN_POINT('Ctrl Pts',(-0.234942750240432,0.0375768454921921,
-0.378311200860805));
#81784=CARTESIAN_POINT('Ctrl Pts',(-0.229795218082391,0.0587748961201941,
-0.37972022844811));
#81785=CARTESIAN_POINT('Ctrl Pts',(-0.229062104665875,0.0615701365391166,
-0.379908353209227));
#81786=CARTESIAN_POINT('Ctrl Pts',(-0.227779024317824,0.0661217101173076,
-0.380218886285169));
#81787=CARTESIAN_POINT('Ctrl Pts',(-0.227259349215754,0.0678863192732277,
-0.380340322820557));
#81788=CARTESIAN_POINT('Ctrl Pts',(-0.226285862923904,0.0710553781983971,
-0.380560387944717));
#81789=CARTESIAN_POINT('Ctrl Pts',(-0.225839364538556,0.0724619885642481,
-0.380658774060869));
#81790=CARTESIAN_POINT('Ctrl Pts',(-0.224853275206923,0.0754708108511365,
-0.380870797048019));
#81791=CARTESIAN_POINT('Ctrl Pts',(-0.22430962432184,0.0770715955594267,
-0.380984562659641));
#81792=CARTESIAN_POINT('Ctrl Pts',(-0.222764472840155,0.0814664323528264,
-0.381299630123455));
#81793=CARTESIAN_POINT('Ctrl Pts',(-0.221727594261927,0.0842476261770411,
-0.38150208632574));
#81794=CARTESIAN_POINT('Ctrl Pts',(-0.219294058701362,0.0904186589882814,
-0.381958411186321));
#81795=CARTESIAN_POINT('Ctrl Pts',(-0.217870466972286,0.0937969892427897,
-0.382213116366277));
#81796=CARTESIAN_POINT('Ctrl Pts',(-0.212986009098468,0.104676517985949,
-0.38304953251337));
#81797=CARTESIAN_POINT('Ctrl Pts',(-0.209211739274275,0.112029633332087,
-0.383640581428881));
#81798=CARTESIAN_POINT('Ctrl Pts',(-0.196160273416756,0.134487904265748,
-0.385521508250884));
#81799=CARTESIAN_POINT('Ctrl Pts',(-0.185570382196961,0.148759914260615,
-0.386834955047876));
#81800=CARTESIAN_POINT('Ctrl Pts',(-0.171648423741659,0.163695118860609,
-0.38826959436283));
#81801=CARTESIAN_POINT('Ctrl Pts',(-0.169773365624433,0.165639002527922,
-0.388457540313142));
#81802=CARTESIAN_POINT('Ctrl Pts',(-0.167114535338839,0.168302829685472,
-0.388716303540888));
#81803=CARTESIAN_POINT('Ctrl Pts',(-0.166358584181959,0.16905008718543,
-0.38878902830247));
#81804=CARTESIAN_POINT('Ctrl Pts',(-0.164988781964261,0.170386049085651,
-0.388919252011855));
#81805=CARTESIAN_POINT('Ctrl Pts',(-0.164376740598118,0.170976580654513,
-0.388976887572525));
#81806=CARTESIAN_POINT('Ctrl Pts',(-0.163110170091353,0.172185550590766,
-0.389095010160604));
#81807=CARTESIAN_POINT('Ctrl Pts',(-0.162455274465474,0.172803574285227,
-0.389155466703759));
#81808=CARTESIAN_POINT('Ctrl Pts',(-0.160726859932221,0.174416165033227,
-0.389313456883498));
#81809=CARTESIAN_POINT('Ctrl Pts',(-0.159647608707725,0.175404570720446,
-0.389410539540783));
#81810=CARTESIAN_POINT('Ctrl Pts',(-0.154553642300095,0.179983785697007,
-0.389861871671207));
#81811=CARTESIAN_POINT('Ctrl Pts',(-0.150426187316355,0.183447441148556,
-0.390207809704147));
#81812=CARTESIAN_POINT('Ctrl Pts',(-0.137015780565877,0.193943827601388,
-0.391284185469541));
#81813=CARTESIAN_POINT('Ctrl Pts',(-0.12733098548676,0.20043549773552,-0.391993687697713));
#81814=CARTESIAN_POINT('Ctrl Pts',(-0.105223255307046,0.213002567344061,
-0.393554017526574));
#81815=CARTESIAN_POINT('Ctrl Pts',(-0.0926687609802247,0.218756640405711,
-0.394404727205633));
#81816=CARTESIAN_POINT('Ctrl Pts',(-0.0767126472496483,0.224448478057488,
-0.395496024686669));
#81817=CARTESIAN_POINT('Ctrl Pts',(-0.07371806084191,0.225449762830957,
-0.395701147488995));
#81818=CARTESIAN_POINT('Ctrl Pts',(-0.0688941546345913,0.226956324106241,
-0.396032569872519));
#81819=CARTESIAN_POINT('Ctrl Pts',(-0.067077150095072,0.227499963039657,
-0.396157627081568));
#81820=CARTESIAN_POINT('Ctrl Pts',(-0.063826228876646,0.22843029175073,
-0.396381865089275));
#81821=CARTESIAN_POINT('Ctrl Pts',(-0.0623948167249027,0.228825418947979,
-0.396480766970879));
#81822=CARTESIAN_POINT('Ctrl Pts',(-0.0593775881632067,0.229627879782371,
-0.396689636329218));
#81823=CARTESIAN_POINT('Ctrl Pts',(-0.0577910809438523,0.230032284430195,
-0.396799692364146));
#81824=CARTESIAN_POINT('Ctrl Pts',(-0.0535615332678821,0.231063890482319,
-0.397093766576584));
#81825=CARTESIAN_POINT('Ctrl Pts',(-0.0509117554811016,0.231662149304147,
-0.397278696334734));
#81826=CARTESIAN_POINT('Ctrl Pts',(-0.0461519654293381,0.232651195874028,
-0.397612253452573));
#81827=CARTESIAN_POINT('Ctrl Pts',(-0.0440462491475563,0.233059018734323,
-0.397760292373697));
#81828=CARTESIAN_POINT('Ctrl Pts',(-0.0419358190075303,0.23343814536011,
-0.397909151625197));
#81829=CARTESIAN_POINT('',(-0.237174999987694,-2.41604215922389E-6,-0.395881110820101));
#81830=CARTESIAN_POINT('Ctrl Pts',(-0.0419358280420692,0.233438143737107,
-0.417646538149483));
#81831=CARTESIAN_POINT('Ctrl Pts',(-0.0483941564159259,0.232277941964639,
-0.417230281189441));
#81832=CARTESIAN_POINT('Ctrl Pts',(-0.0548034836274561,0.230849877704686,
-0.416822836231435));
#81833=CARTESIAN_POINT('Ctrl Pts',(-0.0788615774794773,0.224430337698852,
-0.41528836043212));
#81834=CARTESIAN_POINT('Ctrl Pts',(-0.0959667408439773,0.217665948128303,
-0.414181402220041));
#81835=CARTESIAN_POINT('Ctrl Pts',(-0.115849964572538,0.20699919152677,
-0.412736627724306));
#81836=CARTESIAN_POINT('Ctrl Pts',(-0.119523702368301,0.20489987955341,
-0.412462752788253));
#81837=CARTESIAN_POINT('Ctrl Pts',(-0.124774783994876,0.201709931403471,
-0.4120599376928));
#81838=CARTESIAN_POINT('Ctrl Pts',(-0.126398277385047,0.200696582596506,
-0.411933776238562));
#81839=CARTESIAN_POINT('Ctrl Pts',(-0.129261025383699,0.198861204898509,
-0.411708309998145));
#81840=CARTESIAN_POINT('Ctrl Pts',(-0.130505160002671,0.19804695033732,
-0.411609295859604));
#81841=CARTESIAN_POINT('Ctrl Pts',(-0.133095031755873,0.196316944111657,
-0.411400970105855));
#81842=CARTESIAN_POINT('Ctrl Pts',(-0.134439157830142,0.19539893202587,
-0.411291577185917));
#81843=CARTESIAN_POINT('Ctrl Pts',(-0.137965456980013,0.192936929492227,
-0.411001137208692));
#81844=CARTESIAN_POINT('Ctrl Pts',(-0.140131105597443,0.191369794667348,
-0.410819217769311));
#81845=CARTESIAN_POINT('Ctrl Pts',(-0.151519566253012,0.182831756154235,
-0.409843069200494));
#81846=CARTESIAN_POINT('Ctrl Pts',(-0.160248600106373,0.175231116741886,
-0.40902440537741));
#81847=CARTESIAN_POINT('Ctrl Pts',(-0.174632194790189,0.160730212548615,
-0.407549105142471));
#81848=CARTESIAN_POINT('Ctrl Pts',(-0.180518482802464,0.154089818467004,
-0.406900553218716));
#81849=CARTESIAN_POINT('Ctrl Pts',(-0.193047831359062,0.138249370361049,
-0.405427567273631));
#81850=CARTESIAN_POINT('Ctrl Pts',(-0.19943171814169,0.12886970325819,-0.404605931764943));
#81851=CARTESIAN_POINT('Ctrl Pts',(-0.205984989500111,0.117580296747157,
-0.403699690114774));
#81852=CARTESIAN_POINT('Ctrl Pts',(-0.206832732350692,0.116082571212904,
-0.403581062139185));
#81853=CARTESIAN_POINT('Ctrl Pts',(-0.208130962768453,0.113729577578987,
-0.403397329401662));
#81854=CARTESIAN_POINT('Ctrl Pts',(-0.208592632349877,0.112880593069727,
-0.403331566013175));
#81855=CARTESIAN_POINT('Ctrl Pts',(-0.209403901641078,0.111366740061696,
-0.403215270377044));
#81856=CARTESIAN_POINT('Ctrl Pts',(-0.209755537858412,0.110703022431092,
-0.403164614249093));
#81857=CARTESIAN_POINT('Ctrl Pts',(-0.210600800098982,0.109089092487864,
-0.403042224241637));
#81858=CARTESIAN_POINT('Ctrl Pts',(-0.211091152667851,0.108137192851263,
-0.402970693582124));
#81859=CARTESIAN_POINT('Ctrl Pts',(-0.21261191762856,0.105135233741133,
-0.402747059652105));
#81860=CARTESIAN_POINT('Ctrl Pts',(-0.213619074247803,0.103073454206785,
-0.402596302356005));
#81861=CARTESIAN_POINT('Ctrl Pts',(-0.218890923811409,0.09187197693539,
-0.401790705884823));
#81862=CARTESIAN_POINT('Ctrl Pts',(-0.222599727624839,0.0824809305655365,
-0.401162921282223));
#81863=CARTESIAN_POINT('Ctrl Pts',(-0.231717481545343,0.0542449732917915,
-0.399334907779679));
#81864=CARTESIAN_POINT('Ctrl Pts',(-0.235403594222045,0.0349369987405584,
-0.398152900227539));
#81865=CARTESIAN_POINT('Ctrl Pts',(-0.236888596139364,0.012108871306242,
-0.396677277300176));
#81866=CARTESIAN_POINT('Ctrl Pts',(-0.237033915765791,0.00881775525041497,
-0.396462892892614));
#81867=CARTESIAN_POINT('Ctrl Pts',(-0.237136523561489,0.00441408874215108,
-0.396173378021457));
#81868=CARTESIAN_POINT('Ctrl Pts',(-0.237154598636204,0.00330321997630701,
-0.396100119721302));
#81869=CARTESIAN_POINT('Ctrl Pts',(-0.237171630092345,0.00146072643667166,
-0.395978221412552));
#81870=CARTESIAN_POINT('Ctrl Pts',(-0.237175007440005,0.00072915308448074,
-0.395929718572334));
#81871=CARTESIAN_POINT('Ctrl Pts',(-0.237174999987694,-2.41604215922389E-6,
-0.395881110820101));
#81872=CARTESIAN_POINT('Ctrl Pts',(-0.237174999987369,-2.44774490620395E-6,
-0.395881108713671));
#81873=CARTESIAN_POINT('Ctrl Pts',(-0.237174993974579,-0.000585058863951221,
-0.395842398197246));
#81874=CARTESIAN_POINT('Ctrl Pts',(-0.237172841219915,-0.00116766457214191,
-0.395803621328249));
#81875=CARTESIAN_POINT('Ctrl Pts',(-0.237161772411672,-0.00266754656485543,
-0.395703617536787));
#81876=CARTESIAN_POINT('Ctrl Pts',(-0.237149681418993,-0.00358478177326851,
-0.39564229268734));
#81877=CARTESIAN_POINT('Ctrl Pts',(-0.237099735243235,-0.00621563015734606,
-0.395465900968798));
#81878=CARTESIAN_POINT('Ctrl Pts',(-0.237048625224458,-0.00792890424153297,
-0.395350424275536));
#81879=CARTESIAN_POINT('Ctrl Pts',(-0.23685292236543,-0.0127391275306386,
-0.395024435453109));
#81880=CARTESIAN_POINT('Ctrl Pts',(-0.236666173587936,-0.0158339162863413,
-0.394812629851663));
#81881=CARTESIAN_POINT('Ctrl Pts',(-0.234832601539564,-0.0387408175958628,
-0.393228832044568));
#81882=CARTESIAN_POINT('Ctrl Pts',(-0.23076131366614,-0.058276175430853,
-0.391779006268009));
#81883=CARTESIAN_POINT('Ctrl Pts',(-0.221016901985021,-0.0866361353605369,
-0.389592688110286));
#81884=CARTESIAN_POINT('Ctrl Pts',(-0.217121161428312,-0.095982976466006,
-0.388859627519287));
#81885=CARTESIAN_POINT('Ctrl Pts',(-0.211622486291035,-0.107112939240905,
-0.387991666613779));
#81886=CARTESIAN_POINT('Ctrl Pts',(-0.210574986470963,-0.109157842151878,
-0.387832433415779));
#81887=CARTESIAN_POINT('Ctrl Pts',(-0.208995674938438,-0.112133563804,-0.387601409330168));
#81888=CARTESIAN_POINT('Ctrl Pts',(-0.208487040827164,-0.113076444023026,
-0.387528310866675));
#81889=CARTESIAN_POINT('Ctrl Pts',(-0.207610916169756,-0.114674549800816,
-0.387404632389075));
#81890=CARTESIAN_POINT('Ctrl Pts',(-0.207246679373072,-0.115331517079058,
-0.387353853964854));
#81891=CARTESIAN_POINT('Ctrl Pts',(-0.206406909183692,-0.11682936960034,
-0.387238236183036));
#81892=CARTESIAN_POINT('Ctrl Pts',(-0.205929353364056,-0.117669092227257,
-0.387173526025823));
#81893=CARTESIAN_POINT('Ctrl Pts',(-0.20458765041009,-0.119995123437729,
-0.386994510821711));
#81894=CARTESIAN_POINT('Ctrl Pts',(-0.203712433149011,-0.121475023565959,
-0.386880880386286));
#81895=CARTESIAN_POINT('Ctrl Pts',(-0.197027683394357,-0.132502760768627,
-0.386035123330123));
#81896=CARTESIAN_POINT('Ctrl Pts',(-0.190565080013029,-0.141640056492486,
-0.385339569328659));
#81897=CARTESIAN_POINT('Ctrl Pts',(-0.177889010979282,-0.157115773896804,
-0.384107670433089));
#81898=CARTESIAN_POINT('Ctrl Pts',(-0.171920076202272,-0.163625653209715,
-0.383569640121974));
#81899=CARTESIAN_POINT('Ctrl Pts',(-0.160008888310081,-0.175243214047791,
-0.382542961627802));
#81900=CARTESIAN_POINT('Ctrl Pts',(-0.154149743607366,-0.180418600405547,
-0.382056402338797));
#81901=CARTESIAN_POINT('Ctrl Pts',(-0.145281232134576,-0.187504318853361,
-0.381334621668707));
#81902=CARTESIAN_POINT('Ctrl Pts',(-0.142467274622731,-0.189651205457337,
-0.381107628539409));
#81903=CARTESIAN_POINT('Ctrl Pts',(-0.137271783344386,-0.193434170918486,
-0.380691200948543));
#81904=CARTESIAN_POINT('Ctrl Pts',(-0.134906359347164,-0.195091245350535,
-0.380502575621173));
#81905=CARTESIAN_POINT('Ctrl Pts',(-0.131123503851417,-0.197639590092998,
-0.38020207844178));
#81906=CARTESIAN_POINT('Ctrl Pts',(-0.129725833889909,-0.198559785996061,
-0.380091296432875));
#81907=CARTESIAN_POINT('Ctrl Pts',(-0.127076053231611,-0.200264425458137,
-0.379881660685141));
#81908=CARTESIAN_POINT('Ctrl Pts',(-0.125826116327033,-0.201052111875229,
-0.379782933554974));
#81909=CARTESIAN_POINT('Ctrl Pts',(-0.122982905127233,-0.202806950995464,
-0.379558677108675));
#81910=CARTESIAN_POINT('Ctrl Pts',(-0.121385441637704,-0.203767093859447,
-0.379432899391021));
#81911=CARTESIAN_POINT('Ctrl Pts',(-0.117210453102132,-0.206209921428293,
-0.379104666458924));
#81912=CARTESIAN_POINT('Ctrl Pts',(-0.114616133542342,-0.20766309868266,
-0.378901176574523));
#81913=CARTESIAN_POINT('Ctrl Pts',(-0.0960223525775907,-0.21762361395977,
-0.377445516736402));
#81914=CARTESIAN_POINT('Ctrl Pts',(-0.0791241837443924,-0.224319991031289,
-0.376130139497006));
#81915=CARTESIAN_POINT('Ctrl Pts',(-0.0497411862481437,-0.232227129515415,
-0.3739091874719));
#81916=CARTESIAN_POINT('Ctrl Pts',(-0.0376173718029788,-0.23449652921264,
-0.373012471423046));
#81917=CARTESIAN_POINT('Ctrl Pts',(-0.0235130872898481,-0.236013998223146,
-0.372025889664875));
#81918=CARTESIAN_POINT('Ctrl Pts',(-0.0216527479674377,-0.236191938218795,
-0.371896903655876));
#81919=CARTESIAN_POINT('Ctrl Pts',(-0.0188066256142253,-0.236430256340702,
-0.371701506288426));
#81920=CARTESIAN_POINT('Ctrl Pts',(-0.0178222949964452,-0.236506492870208,
-0.371634281665537));
#81921=CARTESIAN_POINT('Ctrl Pts',(-0.0160077947327807,-0.23663563345837,
-0.371511046849067));
#81922=CARTESIAN_POINT('Ctrl Pts',(-0.015177809912862,-0.23669031800133,
-0.371454945134281));
#81923=CARTESIAN_POINT('Ctrl Pts',(-0.0132784714627283,-0.23680542618126,
-0.371327159705849));
#81924=CARTESIAN_POINT('Ctrl Pts',(-0.0122089772759333,-0.236862974432931,
-0.371255634383294));
#81925=CARTESIAN_POINT('Ctrl Pts',(-0.00886793475978442,-0.23702006238442,
-0.371033429807722));
#81926=CARTESIAN_POINT('Ctrl Pts',(-0.00659524485003055,-0.237094187847428,
-0.370884062621256));
#81927=CARTESIAN_POINT('Ctrl Pts',(0.00675570713104867,-0.237337505760676,
-0.370015227401446));
#81928=CARTESIAN_POINT('Ctrl Pts',(0.0178350639157828,-0.236762961152023,
-0.369328709654773));
#81929=CARTESIAN_POINT('Ctrl Pts',(0.0382324760196458,-0.234264594675536,
-0.368065243619044));
#81930=CARTESIAN_POINT('Ctrl Pts',(0.0475526833224055,-0.232551847795849,
-0.36748803611714));
#81931=CARTESIAN_POINT('Ctrl Pts',(0.0634779240609387,-0.228627670120237,
-0.36647197562288));
#81932=CARTESIAN_POINT('Ctrl Pts',(0.0701339394012187,-0.226674388421198,
-0.366038036275399));
#81933=CARTESIAN_POINT('Ctrl Pts',(0.0812158685449806,-0.22288740050702,
-0.365291233632475));
#81934=CARTESIAN_POINT('Ctrl Pts',(0.0856892424813818,-0.221206146781791,
-0.364982872399261));
#81935=CARTESIAN_POINT('Ctrl Pts',(0.091982764675391,-0.218621263392434,
-0.364537440056293));
#81936=CARTESIAN_POINT('Ctrl Pts',(0.0938469744334933,-0.217827525289157,
-0.364404019639248));
#81937=CARTESIAN_POINT('Ctrl Pts',(0.0970719794289436,-0.216405308185208,
-0.364170504774761));
#81938=CARTESIAN_POINT('Ctrl Pts',(0.0984374293911331,-0.215787624576422,
-0.364070781131217));
#81939=CARTESIAN_POINT('Ctrl Pts',(0.101068608136367,-0.214567197463086,
-0.363876911924916));
#81940=CARTESIAN_POINT('Ctrl Pts',(0.102335029862304,-0.213966089124163,
-0.363782825904919));
#81941=CARTESIAN_POINT('Ctrl Pts',(0.105700619898416,-0.212331893952013,
-0.363530671094749));
#81942=CARTESIAN_POINT('Ctrl Pts',(0.107789910343504,-0.21127893596652,
-0.363371919606703));
#81943=CARTESIAN_POINT('Ctrl Pts',(0.115664714784849,-0.207162994895937,
-0.362764878063084));
#81944=CARTESIAN_POINT('Ctrl Pts',(0.121337654230917,-0.203892109137735,
-0.36230941781622));
#81945=CARTESIAN_POINT('Ctrl Pts',(0.141629542878925,-0.191045310288335,
-0.360611635300381));
#81946=CARTESIAN_POINT('Ctrl Pts',(0.155312416164008,-0.18009763042746,
-0.359325138942754));
#81947=CARTESIAN_POINT('Ctrl Pts',(0.171776699757586,-0.163641402702207,
-0.357635966006275));
#81948=CARTESIAN_POINT('Ctrl Pts',(0.17573432256495,-0.159383812274255,
-0.357217517641067));
#81949=CARTESIAN_POINT('Ctrl Pts',(0.181843129396594,-0.152307477944915,
-0.356556107030273));
#81950=CARTESIAN_POINT('Ctrl Pts',(0.184094446661538,-0.149578506136751,
-0.35630864322923));
#81951=CARTESIAN_POINT('Ctrl Pts',(0.187067664509862,-0.145805598354543,
-0.355977780911847));
#81952=CARTESIAN_POINT('Ctrl Pts',(0.187843362624387,-0.144804885670027,
-0.355891068520842));
#81953=CARTESIAN_POINT('Ctrl Pts',(0.189131488712093,-0.143115329341787,
-0.355746475702147));
#81954=CARTESIAN_POINT('Ctrl Pts',(0.189648250690643,-0.142429837514248,
-0.355688303685997));
#81955=CARTESIAN_POINT('Ctrl Pts',(0.190701049408829,-0.141017396395389,
-0.355569472246095));
#81956=CARTESIAN_POINT('Ctrl Pts',(0.191236673278507,-0.140290167843728,
-0.355508840019971));
#81957=CARTESIAN_POINT('Ctrl Pts',(0.192637012331282,-0.138365972917941,
-0.355349805070545));
#81958=CARTESIAN_POINT('Ctrl Pts',(0.193494742432673,-0.137163938068432,
-0.355251864452558));
#81959=CARTESIAN_POINT('Ctrl Pts',(0.197208019048673,-0.131855943819113,
-0.354825130352847));
#81960=CARTESIAN_POINT('Ctrl Pts',(0.199944723020725,-0.127667962240653,
-0.354503383072239));
#81961=CARTESIAN_POINT('Ctrl Pts',(0.210455794275979,-0.110414701567894,
-0.353223602361746));
#81962=CARTESIAN_POINT('Ctrl Pts',(0.217098665669008,-0.0967020480646991,
-0.352307009499785));
#81963=CARTESIAN_POINT('Ctrl Pts',(0.225774312722978,-0.0733013063227795,
-0.350768079017187));
#81964=CARTESIAN_POINT('Ctrl Pts',(0.228597312827624,-0.0639559467898985,
-0.350159990894307));
#81965=CARTESIAN_POINT('Ctrl Pts',(0.231763926708487,-0.050534748710045,
-0.349275668647977));
#81966=CARTESIAN_POINT('Ctrl Pts',(0.232590464665895,-0.0465827352123217,
-0.349014030468047));
#81967=CARTESIAN_POINT('Ctrl Pts',(0.233657086023342,-0.0407425708161299,
-0.348624589016904));
#81968=CARTESIAN_POINT('Ctrl Pts',(0.23397597876732,-0.0388694216129775,
-0.34849926427914));
#81969=CARTESIAN_POINT('Ctrl Pts',(0.234503342971433,-0.0355296578314993,
-0.348274977503675));
#81970=CARTESIAN_POINT('Ctrl Pts',(0.234720647558662,-0.0340645253916771,
-0.34817629932733));
#81971=CARTESIAN_POINT('Ctrl Pts',(0.235151214861497,-0.0309615039651739,
-0.347966660475668));
#81972=CARTESIAN_POINT('Ctrl Pts',(0.235361118564136,-0.0293232366562086,
-0.347855599716007));
#81973=CARTESIAN_POINT('Ctrl Pts',(0.235879016549694,-0.0249164482390856,
-0.34755577235751));
#81974=CARTESIAN_POINT('Ctrl Pts',(0.236155367964125,-0.0221445450537729,
-0.347366029599048));
#81975=CARTESIAN_POINT('Ctrl Pts',(0.23751046768031,-0.00560624734037188,
-0.346226658835146));
#81976=CARTESIAN_POINT('Ctrl Pts',(0.237433928022695,0.00822586002365591,
-0.34524138713463));
#81977=CARTESIAN_POINT('Ctrl Pts',(0.235236684636191,0.0318433002732485,
-0.34351778588038));
#81978=CARTESIAN_POINT('Ctrl Pts',(0.233700000996211,0.0416485604805146,
-0.342790382467661));
#81979=CARTESIAN_POINT('Ctrl Pts',(0.230381028079536,0.0566210787946362,
-0.341679370526248));
#81980=CARTESIAN_POINT('Ctrl Pts',(0.229026726820277,0.06187188684724,-0.341289812628266));
#81981=CARTESIAN_POINT('Ctrl Pts',(0.226539582632591,0.0703077412721777,
-0.340668407658541));
#81982=CARTESIAN_POINT('Ctrl Pts',(0.225516589695409,0.0735230004870905,
-0.34043264699572));
#81983=CARTESIAN_POINT('Ctrl Pts',(0.224022930278894,0.0778925842135554,
-0.340114724893984));
#81984=CARTESIAN_POINT('Ctrl Pts',(0.223611312149806,0.0790664860436689,
-0.340029562707809));
#81985=CARTESIAN_POINT('Ctrl Pts',(0.222901488889101,0.0810409558474153,
-0.339886806265693));
#81986=CARTESIAN_POINT('Ctrl Pts',(0.222608163424756,0.0818432400531308,
-0.33982893632245));
#81987=CARTESIAN_POINT('Ctrl Pts',(0.221993270591163,0.083497288927274,
-0.339709931767458));
#81988=CARTESIAN_POINT('Ctrl Pts',(0.221671124477625,0.0843488120177309,
-0.339648831284284));
#81989=CARTESIAN_POINT('Ctrl Pts',(0.220801782097975,0.0866073475331657,
-0.339487155774716));
#81990=CARTESIAN_POINT('Ctrl Pts',(0.220246031454146,0.0880110535381722,
-0.339387070857342));
#81991=CARTESIAN_POINT('Ctrl Pts',(0.217654855955397,0.0943775137010561,
-0.338934539598695));
#81992=CARTESIAN_POINT('Ctrl Pts',(0.215464683960568,0.0992760354568723,
-0.338590237194432));
#81993=CARTESIAN_POINT('Ctrl Pts',(0.20652272585129,0.117582339628132,-0.337303045731337));
#81994=CARTESIAN_POINT('Ctrl Pts',(0.198669760953754,0.130413305210078,
-0.336397946234262));
#81995=CARTESIAN_POINT('Ctrl Pts',(0.184945088287598,0.148690452585697,
-0.334987773883554));
#81996=CARTESIAN_POINT('Ctrl Pts',(0.179925859152281,0.154726235288953,
-0.334499280238685));
#81997=CARTESIAN_POINT('Ctrl Pts',(0.172215736731027,0.163114413980044,
-0.333774917352308));
#81998=CARTESIAN_POINT('Ctrl Pts',(0.169756198608849,0.165672578046288,
-0.333547346141803));
#81999=CARTESIAN_POINT('Ctrl Pts',(0.165188318718798,0.170215083086525,
-0.333129957242076));
#82000=CARTESIAN_POINT('Ctrl Pts',(0.163099248543014,0.1722178535817,-0.332940954623932));
#82001=CARTESIAN_POINT('Ctrl Pts',(0.159744275359288,0.175318428889826,
-0.3326399943499));
#82002=CARTESIAN_POINT('Ctrl Pts',(0.158502445760494,0.176441943609541,
-0.332529132375849));
#82003=CARTESIAN_POINT('Ctrl Pts',(0.156142963260916,0.178531615989263,
-0.332319429764708));
#82004=CARTESIAN_POINT('Ctrl Pts',(0.155027973240739,0.179500669154759,
-0.332220716664099));
#82005=CARTESIAN_POINT('Ctrl Pts',(0.152487404560057,0.181667384353392,
-0.331996607533027));
#82006=CARTESIAN_POINT('Ctrl Pts',(0.151056643554464,0.182858790279001,
-0.331870964414313));
#82007=CARTESIAN_POINT('Ctrl Pts',(0.146640869377827,0.186448647871401,
-0.331484812161052));
#82008=CARTESIAN_POINT('Ctrl Pts',(0.143611800593303,0.188791659351642,
-0.331222136529913));
#82009=CARTESIAN_POINT('Ctrl Pts',(0.125397349609529,0.202188646110562,
-0.329654568159222));
#82010=CARTESIAN_POINT('Ctrl Pts',(0.109001148624927,0.211478722522018,
-0.328283626173752));
#82011=CARTESIAN_POINT('Ctrl Pts',(0.0823499098869818,0.222649799466091,
-0.32617672611718));
#82012=CARTESIAN_POINT('Ctrl Pts',(0.0727726864805359,0.225961537904021,
-0.325443107747218));
#82013=CARTESIAN_POINT('Ctrl Pts',(0.0607968002134912,0.229261882958715,
-0.324574569025959));
#82014=CARTESIAN_POINT('Ctrl Pts',(0.0585724281075908,0.229840234802622,
-0.324415282928699));
#82015=CARTESIAN_POINT('Ctrl Pts',(0.0552991464789388,0.230640701026333,
-0.324184197217415));
#82016=CARTESIAN_POINT('Ctrl Pts',(0.0542566538772727,0.230888163821148,
-0.324111089074754));
#82017=CARTESIAN_POINT('Ctrl Pts',(0.0524804574162301,0.231297095740523,
-0.323987399813118));
#82018=CARTESIAN_POINT('Ctrl Pts',(0.0517476178585353,0.2314621546013,-0.323936620189704));
#82019=CARTESIAN_POINT('Ctrl Pts',(0.0500706866346547,0.231831490350322,
-0.323821007403158));
#82020=CARTESIAN_POINT('Ctrl Pts',(0.04912611799872,0.232033485064156,-0.32375630336873));
#82021=CARTESIAN_POINT('Ctrl Pts',(0.0464973582687399,0.232578869581847,
-0.323577321928129));
#82022=CARTESIAN_POINT('Ctrl Pts',(0.0448105898301258,0.232909738657296,
-0.323463718725321));
#82023=CARTESIAN_POINT('Ctrl Pts',(0.032177102441422,0.2352455361084,-0.322621104706866));
#82024=CARTESIAN_POINT('Ctrl Pts',(0.021103542522077,0.236496371368418,
-0.321928350421202));
#82025=CARTESIAN_POINT('Ctrl Pts',(0.0010892911798639,0.237339442916482,
-0.320694626488137));
#82026=CARTESIAN_POINT('Ctrl Pts',(-0.00781722545426386,0.237213172340247,
-0.320152075868688));
#82027=CARTESIAN_POINT('Ctrl Pts',(-0.024473012866557,0.236037798100911,
-0.319121716253824));
#82028=CARTESIAN_POINT('Ctrl Pts',(-0.0322181478482891,0.235105822802945,
-0.318636142384706));
#82029=CARTESIAN_POINT('Ctrl Pts',(-0.0405811005292778,0.233678471844009,
-0.318096673108255));
#82030=CARTESIAN_POINT('Ctrl Pts',(-0.0412587354183974,0.233559779549431,
-0.318052853219164));
#82031=CARTESIAN_POINT('Ctrl Pts',(-0.0419358257618152,0.233438144146741,
-0.318008956663326));
#82032=CARTESIAN_POINT('Origin',(0.,0.,-1.7456589891905));
#82033=CARTESIAN_POINT('',(-0.0419358257146564,0.233438144155213,-0.198327653695922));
#82034=CARTESIAN_POINT('',(-0.0419358573824119,0.23343813846628,-0.21792431326882));
#82035=CARTESIAN_POINT('',(-0.0419358257166344,0.233438144154858,-1.7456589891905));
#82036=CARTESIAN_POINT('',(-0.237174957655792,0.000141724990824578,-0.276089073795202));
#82037=CARTESIAN_POINT('Ctrl Pts',(-0.0419358257146564,0.233438144155213,
-0.198327653695922));
#82038=CARTESIAN_POINT('Ctrl Pts',(-0.0409295018561971,0.233618924473252,
-0.198398144126953));
#82039=CARTESIAN_POINT('Ctrl Pts',(-0.0399219914476528,0.233793200733438,
-0.198468316308305));
#82040=CARTESIAN_POINT('Ctrl Pts',(-0.0379917462161784,0.23411424712948,
-0.198601948924105));
#82041=CARTESIAN_POINT('Ctrl Pts',(-0.0370692168767604,0.234262089816906,
-0.198665464692559));
#82042=CARTESIAN_POINT('Ctrl Pts',(-0.0353118932121755,0.234533073978755,
-0.19878575615995));
#82043=CARTESIAN_POINT('Ctrl Pts',(-0.034477289734947,0.234657216180683,
-0.198842582756937));
#82044=CARTESIAN_POINT('Ctrl Pts',(-0.0324705827651871,0.234944764444413,
-0.198978518044225));
#82045=CARTESIAN_POINT('Ctrl Pts',(-0.0312978674836229,0.235103859437134,
-0.199057389664625));
#82046=CARTESIAN_POINT('Ctrl Pts',(-0.0271889308576364,0.235630003235974,
-0.199331905422777));
#82047=CARTESIAN_POINT('Ctrl Pts',(-0.0242469412288661,0.235950893558866,
-0.199525188091554));
#82048=CARTESIAN_POINT('Ctrl Pts',(-0.0168220143442844,0.236620396099102,
-0.200006512303282));
#82049=CARTESIAN_POINT('Ctrl Pts',(-0.0123336234078155,0.236896767771464,
-0.200291556632799));
#82050=CARTESIAN_POINT('Ctrl Pts',(0.0113721108625147,0.23768079081269,
-0.201778359613328));
#82051=CARTESIAN_POINT('Ctrl Pts',(0.0305901720537581,0.235978359998802,
-0.20292502075045));
#82052=CARTESIAN_POINT('Ctrl Pts',(0.0560615728204603,0.230554918206611,
-0.20456330421721));
#82053=CARTESIAN_POINT('Ctrl Pts',(0.0626655378895886,0.22884817563284,
-0.2049985933393));
#82054=CARTESIAN_POINT('Ctrl Pts',(0.0714532723348395,0.226168139172614,
-0.205597320091774));
#82055=CARTESIAN_POINT('Ctrl Pts',(0.073709589115798,0.225442882151697,
-0.20575280414045));
#82056=CARTESIAN_POINT('Ctrl Pts',(0.0774361015453184,0.224183131596434,
-0.206012719189443));
#82057=CARTESIAN_POINT('Ctrl Pts',(0.0789125884266836,0.223667676485543,
-0.206116522411113));
#82058=CARTESIAN_POINT('Ctrl Pts',(0.0818097755059774,0.222623984373176,
-0.206321883865032));
#82059=CARTESIAN_POINT('Ctrl Pts',(0.0832307245350489,0.222096654851263,
-0.206423407875292));
#82060=CARTESIAN_POINT('Ctrl Pts',(0.0866307240737717,0.220797667863252,
-0.206668314559968));
#82061=CARTESIAN_POINT('Ctrl Pts',(0.0886046224538898,0.220012983383521,
-0.206812126083803));
#82062=CARTESIAN_POINT('Ctrl Pts',(0.0955806457836407,0.217130699638356,
-0.207326343025699));
#82063=CARTESIAN_POINT('Ctrl Pts',(0.100520721818551,0.214888289170165,
-0.207701546929794));
#82064=CARTESIAN_POINT('Ctrl Pts',(0.112847654321066,0.208774719773076,
-0.208666807060047));
#82065=CARTESIAN_POINT('Ctrl Pts',(0.120114872362343,0.204679922594302,
-0.209263525395607));
#82066=CARTESIAN_POINT('Ctrl Pts',(0.142733935714427,0.190314940920863,
-0.211204424988388));
#82067=CARTESIAN_POINT('Ctrl Pts',(0.157108495119061,0.178632917160131,
-0.212574485897301));
#82068=CARTESIAN_POINT('Ctrl Pts',(0.17150327087572,0.163839435516765,-0.214015687243499));
#82069=CARTESIAN_POINT('Ctrl Pts',(0.173001946396445,0.162256155304988,
-0.214166618343512));
#82070=CARTESIAN_POINT('Ctrl Pts',(0.175189386874293,0.15988045645427,-0.214387948933597));
#82071=CARTESIAN_POINT('Ctrl Pts',(0.175895016843176,0.159103817629245,
-0.214459510329381));
#82072=CARTESIAN_POINT('Ctrl Pts',(0.177149349376817,0.15770471479123,-0.214586973506717));
#82073=CARTESIAN_POINT('Ctrl Pts',(0.177699963334139,0.157084028926035,
-0.214643012607144));
#82074=CARTESIAN_POINT('Ctrl Pts',(0.178920151978048,0.155693930677102,
-0.214767393848887));
#82075=CARTESIAN_POINT('Ctrl Pts',(0.179588031563946,0.154923077198476,
-0.214835613669686));
#82076=CARTESIAN_POINT('Ctrl Pts',(0.181569456349057,0.152606123050205,
-0.215038507143711));
#82077=CARTESIAN_POINT('Ctrl Pts',(0.182868197495589,0.151047407424668,
-0.215172166210084));
#82078=CARTESIAN_POINT('Ctrl Pts',(0.191983046944001,0.139818087640798,
-0.21611666488759));
#82079=CARTESIAN_POINT('Ctrl Pts',(0.19904901951974,0.129561401520513,-0.21688396384605));
#82080=CARTESIAN_POINT('Ctrl Pts',(0.214123429576822,0.103513068382687,
-0.218731839225787));
#82081=CARTESIAN_POINT('Ctrl Pts',(0.221232787789981,0.087291327449634,
-0.219806414719049));
#82082=CARTESIAN_POINT('Ctrl Pts',(0.227371487580681,0.0675520607829406,
-0.22113993249783));
#82083=CARTESIAN_POINT('Ctrl Pts',(0.228211958917473,0.0646558178095527,
-0.2213360583988));
#82084=CARTESIAN_POINT('Ctrl Pts',(0.229485439364699,0.059932750458057,
-0.221657077139612));
#82085=CARTESIAN_POINT('Ctrl Pts',(0.229952396058286,0.0581153737704889,
-0.221780881259894));
#82086=CARTESIAN_POINT('Ctrl Pts',(0.230748790532733,0.054855847936956,
-0.222003520359543));
#82087=CARTESIAN_POINT('Ctrl Pts',(0.231086396188675,0.0534157814926653,
-0.222102087881052));
#82088=CARTESIAN_POINT('Ctrl Pts',(0.231775697230703,0.0503466400727279,
-0.222312639924505));
#82089=CARTESIAN_POINT('Ctrl Pts',(0.232123733810521,0.0487168343575298,
-0.222424735411401));
#82090=CARTESIAN_POINT('Ctrl Pts',(0.233021104798295,0.0442864535046422,
-0.222730290557363));
#82091=CARTESIAN_POINT('Ctrl Pts',(0.233537097698428,0.0414794890363676,
-0.222924791395834));
#82092=CARTESIAN_POINT('Ctrl Pts',(0.236644508588403,0.0226728140927505,
-0.224234542005628));
#82093=CARTESIAN_POINT('Ctrl Pts',(0.23764010807973,0.00645582023651468,
-0.225400098459223));
#82094=CARTESIAN_POINT('Ctrl Pts',(0.23638211304355,-0.0241735396929289,
-0.227635834337646));
#82095=CARTESIAN_POINT('Ctrl Pts',(0.234470267849405,-0.038530825471946,
-0.228696964040031));
#82096=CARTESIAN_POINT('Ctrl Pts',(0.2307718722995,-0.0547833980533723,
-0.229861202801916));
#82097=CARTESIAN_POINT('Ctrl Pts',(0.230250654967697,-0.0569342999416245,
-0.230014468222843));
#82098=CARTESIAN_POINT('Ctrl Pts',(0.2294364166732,-0.0601001321103912,
-0.230238542524708));
#82099=CARTESIAN_POINT('Ctrl Pts',(0.22916661759314,-0.0611208365723519,
-0.23031055314345));
#82100=CARTESIAN_POINT('Ctrl Pts',(0.22867254113044,-0.0629407537955865,
-0.230438488454017));
#82101=CARTESIAN_POINT('Ctrl Pts',(0.228450874581588,-0.0637406269324779,
-0.230494555054434));
#82102=CARTESIAN_POINT('Ctrl Pts',(0.227948962014029,-0.0655154972710364,
-0.23061860220317));
#82103=CARTESIAN_POINT('Ctrl Pts',(0.227666655946991,-0.0664898753987113,
-0.230686464540052));
#82104=CARTESIAN_POINT('Ctrl Pts',(0.226808868083418,-0.069380998084145,
-0.230887197120308));
#82105=CARTESIAN_POINT('Ctrl Pts',(0.226215352852066,-0.0712923580666077,
-0.231019084582089));
#82106=CARTESIAN_POINT('Ctrl Pts',(0.224778952662249,-0.0757194897754526,
-0.231323150652912));
#82107=CARTESIAN_POINT('Ctrl Pts',(0.223917895770443,-0.0782291242891998,
-0.231494445886704));
#82108=CARTESIAN_POINT('Ctrl Pts',(0.220717668370193,-0.0870703521247797,
-0.232095836284813));
#82109=CARTESIAN_POINT('Ctrl Pts',(0.218150436507448,-0.0933163167867047,
-0.232516944114112));
#82110=CARTESIAN_POINT('Ctrl Pts',(0.208700143588238,-0.11377833226479,
-0.233909753533043));
#82111=CARTESIAN_POINT('Ctrl Pts',(0.200665771464921,-0.127414675726643,
-0.234862761617255));
#82112=CARTESIAN_POINT('Ctrl Pts',(0.187341707435098,-0.145604802054904,
-0.236281685003211));
#82113=CARTESIAN_POINT('Ctrl Pts',(0.183116299598353,-0.150884332270434,
-0.236713344727211));
#82114=CARTESIAN_POINT('Ctrl Pts',(0.177116914925679,-0.157756670092081,
-0.237307901715248));
#82115=CARTESIAN_POINT('Ctrl Pts',(0.175535849385921,-0.159514054029838,
-0.237462996884774));
#82116=CARTESIAN_POINT('Ctrl Pts',(0.172866359926882,-0.162393486435211,
-0.237722448513469));
#82117=CARTESIAN_POINT('Ctrl Pts',(0.171792615037167,-0.163528957838641,
-0.237826182215525));
#82118=CARTESIAN_POINT('Ctrl Pts',(0.16965479235176,-0.165745384617747,
-0.238031549997146));
#82119=CARTESIAN_POINT('Ctrl Pts',(0.1685914099205,-0.16682690852156,-0.238133151193444));
#82120=CARTESIAN_POINT('Ctrl Pts',(0.166010401503156,-0.169402069418534,
-0.238378490683021));
#82121=CARTESIAN_POINT('Ctrl Pts',(0.164482914501138,-0.170885589954701,
-0.238522661425185));
#82122=CARTESIAN_POINT('Ctrl Pts',(0.158968707943325,-0.176098644612035,
-0.239039660542118));
#82123=CARTESIAN_POINT('Ctrl Pts',(0.1548737179677,-0.179710616909112,-0.239417355775723));
#82124=CARTESIAN_POINT('Ctrl Pts',(0.144157279857009,-0.188524550826298,
-0.240390960346584));
#82125=CARTESIAN_POINT('Ctrl Pts',(0.137377103152433,-0.193520890712681,
-0.240993682564937));
#82126=CARTESIAN_POINT('Ctrl Pts',(0.115081230103722,-0.20818778225116,
-0.242927398593638));
#82127=CARTESIAN_POINT('Ctrl Pts',(0.0987066923786381,-0.216432154076649,
-0.244282923447387));
#82128=CARTESIAN_POINT('Ctrl Pts',(0.0794644365894028,-0.223477751461063,
-0.245714329730063));
#82129=CARTESIAN_POINT('Ctrl Pts',(0.0773705599006154,-0.224211282997807,
-0.245867983877223));
#82130=CARTESIAN_POINT('Ctrl Pts',(0.0742645410349022,-0.22525069402127,
-0.246092507625092));
#82131=CARTESIAN_POINT('Ctrl Pts',(0.0732602205408174,-0.225579337275491,
-0.246164585931202));
#82132=CARTESIAN_POINT('Ctrl Pts',(0.0714631790824603,-0.226154114571549,
-0.246292587290453));
#82133=CARTESIAN_POINT('Ctrl Pts',(0.0706713268466481,-0.226402811660227,
-0.246348652998078));
#82134=CARTESIAN_POINT('Ctrl Pts',(0.0689097245733172,-0.226945935125436,
-0.246472632548486));
#82135=CARTESIAN_POINT('Ctrl Pts',(0.067939378164787,-0.227238307949446,
-0.246540428871454));
#82136=CARTESIAN_POINT('Ctrl Pts',(0.0650521016142871,-0.2280881186778,
-0.246740771526688));
#82137=CARTESIAN_POINT('Ctrl Pts',(0.0631299201846156,-0.228627600319104,
-0.246872340681428));
#82138=CARTESIAN_POINT('Ctrl Pts',(0.0586462310286548,-0.229825135888949,
-0.247175547936488));
#82139=CARTESIAN_POINT('Ctrl Pts',(0.0560800355443542,-0.230464757272304,
-0.247346309527518));
#82140=CARTESIAN_POINT('Ctrl Pts',(0.0469618253401709,-0.232576130648339,
-0.247945011676506));
#82141=CARTESIAN_POINT('Ctrl Pts',(0.0403582345617251,-0.233812520889941,
-0.248364049529611));
#82142=CARTESIAN_POINT('Ctrl Pts',(0.0182028173772347,-0.236993860421164,
-0.249747412432378));
#82143=CARTESIAN_POINT('Ctrl Pts',(0.00251303484284274,-0.237678587525126,
-0.250693120635765));
#82144=CARTESIAN_POINT('Ctrl Pts',(-0.0200199974816856,-0.236429277364393,
-0.252112193814768));
#82145=CARTESIAN_POINT('Ctrl Pts',(-0.0268898286998592,-0.23574674345327,
-0.252552598600587));
#82146=CARTESIAN_POINT('Ctrl Pts',(-0.0360743234931796,-0.234427563424361,
-0.253157222044048));
#82147=CARTESIAN_POINT('Ctrl Pts',(-0.0384236640166671,-0.234053969590932,
-0.253313273930226));
#82148=CARTESIAN_POINT('Ctrl Pts',(-0.0423094383433683,-0.233375971025366,
-0.253573888222162));
#82149=CARTESIAN_POINT('Ctrl Pts',(-0.0438492212495575,-0.233091565745727,
-0.253677815895445));
#82150=CARTESIAN_POINT('Ctrl Pts',(-0.0468727081328813,-0.232502094693021,
-0.253883232867947));
#82151=CARTESIAN_POINT('Ctrl Pts',(-0.048356530564873,-0.232198020173935,
-0.253984686155312));
#82152=CARTESIAN_POINT('Ctrl Pts',(-0.0519079600649834,-0.231434720732135,
-0.254229098546829));
#82153=CARTESIAN_POINT('Ctrl Pts',(-0.0539724958372374,-0.230961978399432,
-0.254372481922059));
#82154=CARTESIAN_POINT('Ctrl Pts',(-0.0612581645060652,-0.229190669965657,
-0.254883240960526));
#82155=CARTESIAN_POINT('Ctrl Pts',(-0.0664408052724592,-0.227742260616885,
-0.255255328663669));
#82156=CARTESIAN_POINT('Ctrl Pts',(-0.0794212189962251,-0.223633803746686,
-0.256210163212567));
#82157=CARTESIAN_POINT('Ctrl Pts',(-0.087137563490602,-0.220741546854758,
-0.256799383868919));
#82158=CARTESIAN_POINT('Ctrl Pts',(-0.110726080089186,-0.210470269257686,
-0.258662201734215));
#82159=CARTESIAN_POINT('Ctrl Pts',(-0.12594301130912,-0.201733443822673,
-0.259958703337694));
#82160=CARTESIAN_POINT('Ctrl Pts',(-0.142397655557306,-0.189692573614097,
-0.261393974947682));
#82161=CARTESIAN_POINT('Ctrl Pts',(-0.144703008694772,-0.187939899750234,
-0.261595776834146));
#82162=CARTESIAN_POINT('Ctrl Pts',(-0.147923341950101,-0.185397203533312,
-0.261878049370054));
#82163=CARTESIAN_POINT('Ctrl Pts',(-0.148865174718396,-0.184641810227938,
-0.261960650594842));
#82164=CARTESIAN_POINT('Ctrl Pts',(-0.150458507916976,-0.183343766660157,
-0.262100411187563));
#82165=CARTESIAN_POINT('Ctrl Pts',(-0.151112933831447,-0.182804761154152,
-0.262157820056457));
#82166=CARTESIAN_POINT('Ctrl Pts',(-0.152430692339048,-0.181707501843111,
-0.262273410618339));
#82167=CARTESIAN_POINT('Ctrl Pts',(-0.153093870381759,-0.181149107380981,
-0.262331582198368));
#82168=CARTESIAN_POINT('Ctrl Pts',(-0.154799170583816,-0.179697194516189,
-0.262481208074137));
#82169=CARTESIAN_POINT('Ctrl Pts',(-0.155836641508467,-0.178798227939612,
-0.26257227953416));
#82170=CARTESIAN_POINT('Ctrl Pts',(-0.158166006212268,-0.176744159684211,
-0.262777008956114));
#82171=CARTESIAN_POINT('Ctrl Pts',(-0.159453176054601,-0.175583793505985,
-0.262890318573197));
#82172=CARTESIAN_POINT('Ctrl Pts',(-0.163325162380227,-0.172015551546312,
-0.263232142502596));
#82173=CARTESIAN_POINT('Ctrl Pts',(-0.165869105982434,-0.169563855076502,
-0.263458070893069));
#82174=CARTESIAN_POINT('Ctrl Pts',(-0.176142383352577,-0.159210550523479,
-0.264380904150731));
#82175=CARTESIAN_POINT('Ctrl Pts',(-0.183369911272575,-0.150829862892916,
-0.265055985185981));
#82176=CARTESIAN_POINT('Ctrl Pts',(-0.198724041381375,-0.130283418644556,
-0.266629107176469));
#82177=CARTESIAN_POINT('Ctrl Pts',(-0.20636227527214,-0.117811541647545,
-0.267527285381611));
#82178=CARTESIAN_POINT('Ctrl Pts',(-0.21418755505127,-0.101909122793188,
-0.268669301252688));
#82179=CARTESIAN_POINT('Ctrl Pts',(-0.215513764223123,-0.0990736797484941,
-0.268872694215964));
#82180=CARTESIAN_POINT('Ctrl Pts',(-0.217557964764391,-0.0944677621900607,
-0.269203206296615));
#82181=CARTESIAN_POINT('Ctrl Pts',(-0.218311382219074,-0.0927133548378095,
-0.269329125099819));
#82182=CARTESIAN_POINT('Ctrl Pts',(-0.21961205622331,-0.0895808210678317,
-0.269554099520366));
#82183=CARTESIAN_POINT('Ctrl Pts',(-0.220167731420872,-0.088206284427222,
-0.26965286519967));
#82184=CARTESIAN_POINT('Ctrl Pts',(-0.221313563593816,-0.0852936170948401,
-0.269862298268792));
#82185=CARTESIAN_POINT('Ctrl Pts',(-0.221900652202324,-0.0837543722016801,
-0.269973062139128));
#82186=CARTESIAN_POINT('Ctrl Pts',(-0.22342971788904,-0.0796164668709136,
-0.270271117734031));
#82187=CARTESIAN_POINT('Ctrl Pts',(-0.224342356768258,-0.0770073144024099,
-0.270459365215664));
#82188=CARTESIAN_POINT('Ctrl Pts',(-0.229585288078088,-0.0611332879802501,
-0.271606971425387));
#82189=CARTESIAN_POINT('Ctrl Pts',(-0.232782897997094,-0.0475256227456584,
-0.272602837934513));
#82190=CARTESIAN_POINT('Ctrl Pts',(-0.236376712548598,-0.0225032534968295,
-0.274440149136895));
#82191=CARTESIAN_POINT('Ctrl Pts',(-0.237181727633546,-0.0111877461047197,
-0.275272490505346));
#82192=CARTESIAN_POINT('Ctrl Pts',(-0.237174957655792,0.000141724990824578,
-0.276089073795202));
#82193=CARTESIAN_POINT('Ctrl Pts',(-0.237174957457087,0.000142057132016532,
-0.276089097734616));
#82194=CARTESIAN_POINT('Ctrl Pts',(-0.237171123206076,0.00654362463918838,
-0.276550497106281));
#82195=CARTESIAN_POINT('Ctrl Pts',(-0.236908112528632,0.012943138279542,
-0.277006175155684));
#82196=CARTESIAN_POINT('Ctrl Pts',(-0.236286385740191,0.0205482695635013,
-0.277535497651701));
#82197=CARTESIAN_POINT('Ctrl Pts',(-0.236176867875511,0.021770960076209,
-0.27762021817767));
#82198=CARTESIAN_POINT('Ctrl Pts',(-0.235973345262132,0.0238604473347336,
-0.27776428851774));
#82199=CARTESIAN_POINT('Ctrl Pts',(-0.235884046417673,0.0247276631767218,
-0.277823873369331));
#82200=CARTESIAN_POINT('Ctrl Pts',(-0.235706331929214,0.0263648697496518,
-0.277935941863676));
#82201=CARTESIAN_POINT('Ctrl Pts',(-0.235618919917507,0.027134957061119,
-0.277988478882682));
#82202=CARTESIAN_POINT('Ctrl Pts',(-0.23543630164553,0.0286763387713665,
-0.278093263611178));
#82203=CARTESIAN_POINT('Ctrl Pts',(-0.235341076468838,0.029447619740959,
-0.278145509817826));
#82204=CARTESIAN_POINT('Ctrl Pts',(-0.235078125829394,0.0314946170376426,
-0.278283710842499));
#82205=CARTESIAN_POINT('Ctrl Pts',(-0.234903804536596,0.0327694819225507,
-0.278369305355628));
#82206=CARTESIAN_POINT('Ctrl Pts',(-0.234228363170439,0.0374265174654742,
-0.278680442328267));
#82207=CARTESIAN_POINT('Ctrl Pts',(-0.23366447574511,0.0407993380059595,
-0.278902811857691));
#82208=CARTESIAN_POINT('Ctrl Pts',(-0.23150980970564,0.0521695515704485,
-0.279645968361694));
#82209=CARTESIAN_POINT('Ctrl Pts',(-0.229579620685065,0.0600972033888468,
-0.280153297476245));
#82210=CARTESIAN_POINT('Ctrl Pts',(-0.222417162287063,0.0840645845238832,
-0.281695453450788));
#82211=CARTESIAN_POINT('Ctrl Pts',(-0.215881182356292,0.0996570917218917,
-0.282714097051292));
#82212=CARTESIAN_POINT('Ctrl Pts',(-0.205148301362771,0.119143517555824,
-0.284126770614526));
#82213=CARTESIAN_POINT('Ctrl Pts',(-0.202389371298119,0.123772124403427,
-0.284473340961328));
#82214=CARTESIAN_POINT('Ctrl Pts',(-0.198329116547582,0.130084712040769,
-0.284964076005512));
#82215=CARTESIAN_POINT('Ctrl Pts',(-0.197159019835836,0.131851398154596,
-0.285103460646346));
#82216=CARTESIAN_POINT('Ctrl Pts',(-0.195112106652395,0.134853777393515,
-0.285344007064877));
#82217=CARTESIAN_POINT('Ctrl Pts',(-0.194246819411867,0.136097202054448,
-0.285444732111356));
#82218=CARTESIAN_POINT('Ctrl Pts',(-0.192463183464042,0.138608638349725,
-0.285650481024354));
#82219=CARTESIAN_POINT('Ctrl Pts',(-0.191544073393037,0.139876014238715,
-0.285755530668955));
#82220=CARTESIAN_POINT('Ctrl Pts',(-0.189197759539961,0.143044890688382,
-0.286021339884536));
#82221=CARTESIAN_POINT('Ctrl Pts',(-0.187754413618233,0.144934165810404,
-0.286182720369332));
#82222=CARTESIAN_POINT('Ctrl Pts',(-0.182019556237,0.152211388141673,-0.286815998338447));
#82223=CARTESIAN_POINT('Ctrl Pts',(-0.177522917977595,0.157432597239822,
-0.287295909786507));
#82224=CARTESIAN_POINT('Ctrl Pts',(-0.162066449515711,0.173874349211572,
-0.288894211410407));
#82225=CARTESIAN_POINT('Ctrl Pts',(-0.150221505017259,0.184204298527142,
-0.290044704432539));
#82226=CARTESIAN_POINT('Ctrl Pts',(-0.131971006368453,0.197182064023182,
-0.291674537374458));
#82227=CARTESIAN_POINT('Ctrl Pts',(-0.126332738989519,0.200841139320602,
-0.292160449990694));
#82228=CARTESIAN_POINT('Ctrl Pts',(-0.118268344683921,0.205600526103471,
-0.292824831013015));
#82229=CARTESIAN_POINT('Ctrl Pts',(-0.11596785407051,0.206906828706353,
-0.293011025212574));
#82230=CARTESIAN_POINT('Ctrl Pts',(-0.111893289307474,0.209131201553266,
-0.293334420813143));
#82231=CARTESIAN_POINT('Ctrl Pts',(-0.110128601965627,0.210065845247152,
-0.293472428184499));
#82232=CARTESIAN_POINT('Ctrl Pts',(-0.107450690220867,0.211441143085923,
-0.29367854597882));
#82233=CARTESIAN_POINT('Ctrl Pts',(-0.106546150592695,0.211898385334806,
-0.293747606371846));
#82234=CARTESIAN_POINT('Ctrl Pts',(-0.104895559291557,0.212719512911488,
-0.293872571110933));
#82235=CARTESIAN_POINT('Ctrl Pts',(-0.104150509410119,0.213085290360015,
-0.293928586546284));
#82236=CARTESIAN_POINT('Ctrl Pts',(-0.102452612427634,0.213907828887981,
-0.294055361508047));
#82237=CARTESIAN_POINT('Ctrl Pts',(-0.101498617774442,0.214362141594273,
-0.294125972225777));
#82238=CARTESIAN_POINT('Ctrl Pts',(-0.0985327658483198,0.215750305011249,
-0.29434367445231));
#82239=CARTESIAN_POINT('Ctrl Pts',(-0.0965107564119194,0.216662352108946,
-0.294489519747987));
#82240=CARTESIAN_POINT('Ctrl Pts',(-0.0813113264516549,0.223263182334507,
-0.295568894712545));
#82241=CARTESIAN_POINT('Ctrl Pts',(-0.0676528558566008,0.22777441008224,
-0.296445644416075));
#82242=CARTESIAN_POINT('Ctrl Pts',(-0.0497766623182696,0.23192720841488,
-0.297571054174985));
#82243=CARTESIAN_POINT('Ctrl Pts',(-0.0458644337506357,0.232732392654763,
-0.297815947261534));
#82244=CARTESIAN_POINT('Ctrl Pts',(-0.041935800711444,0.233438148646895,
-0.298061760785893));
#82245=CARTESIAN_POINT('Ctrl Pts',(-0.0419358257618152,0.233438144146741,
-0.318008956663326));
#82246=CARTESIAN_POINT('Ctrl Pts',(-0.044737224506651,0.232934888905049,
-0.317827338718805));
#82247=CARTESIAN_POINT('Ctrl Pts',(-0.0475293014180542,0.232381253280233,
-0.31764440450371));
#82248=CARTESIAN_POINT('Ctrl Pts',(-0.0531300061965072,0.231165538094296,
-0.317273042601415));
#82249=CARTESIAN_POINT('Ctrl Pts',(-0.0559377967065655,0.230502202348022,
-0.317084609932621));
#82250=CARTESIAN_POINT('Ctrl Pts',(-0.0603533376871241,0.229373610792194,
-0.316784349244478));
#82251=CARTESIAN_POINT('Ctrl Pts',(-0.061969518210354,0.228942257501103,
-0.316673608092285));
#82252=CARTESIAN_POINT('Ctrl Pts',(-0.065004402940657,0.228097766931276,
-0.316464006431609));
#82253=CARTESIAN_POINT('Ctrl Pts',(-0.0664240784855643,0.227688395199332,
-0.316365272057344));
#82254=CARTESIAN_POINT('Ctrl Pts',(-0.0696266824510545,0.226732404246507,
-0.31614093994205));
#82255=CARTESIAN_POINT('Ctrl Pts',(-0.0714071569589592,0.226177973363719,
-0.316015093125072));
#82256=CARTESIAN_POINT('Ctrl Pts',(-0.0768381431734285,0.224416272751221,
-0.315627653325478));
#82257=CARTESIAN_POINT('Ctrl Pts',(-0.0804658345185623,0.223141233765613,
-0.315363872686392));
#82258=CARTESIAN_POINT('Ctrl Pts',(-0.101606714570959,0.215128206394684,
-0.313796252903389));
#82259=CARTESIAN_POINT('Ctrl Pts',(-0.118298783878005,0.206420020816826,
-0.312426568457534));
#82260=CARTESIAN_POINT('Ctrl Pts',(-0.142140668815194,0.190132472464896,
-0.310321402256422));
#82261=CARTESIAN_POINT('Ctrl Pts',(-0.150121291795257,0.183896612738681,
-0.309588208050902));
#82262=CARTESIAN_POINT('Ctrl Pts',(-0.159396122117666,0.17564206652246,
-0.308720108761738));
#82263=CARTESIAN_POINT('Ctrl Pts',(-0.161090171560196,0.174089680564432,
-0.308560862914296));
#82264=CARTESIAN_POINT('Ctrl Pts',(-0.163540709299311,0.171777660790436,
-0.308329824110731));
#82265=CARTESIAN_POINT('Ctrl Pts',(-0.164314976743271,0.171037179800256,
-0.308256723350301));
#82266=CARTESIAN_POINT('Ctrl Pts',(-0.1656235622732,0.16976860872937,-0.308133042336726));
#82267=CARTESIAN_POINT('Ctrl Pts',(-0.166160422846664,0.169243194331276,
-0.308082263650794));
#82268=CARTESIAN_POINT('Ctrl Pts',(-0.167381944514523,0.168036300736565,
-0.307966647150124));
#82269=CARTESIAN_POINT('Ctrl Pts',(-0.168064948531303,0.167353180048676,
-0.307901938518283));
#82270=CARTESIAN_POINT('Ctrl Pts',(-0.169951821676863,0.165442782567326,
-0.307722931605015));
#82271=CARTESIAN_POINT('Ctrl Pts',(-0.171146577587408,0.164206532743473,
-0.307609307835896));
#82272=CARTESIAN_POINT('Ctrl Pts',(-0.179999188518044,0.154844873753818,
-0.306764280778705));
#82273=CARTESIAN_POINT('Ctrl Pts',(-0.187089178391121,0.146199684170916,
-0.306069376668011));
#82274=CARTESIAN_POINT('Ctrl Pts',(-0.194093647528112,0.136310454038169,
-0.305323084695238));
#82275=CARTESIAN_POINT('Ctrl Pts',(-0.194638311143868,0.135531589448686,
-0.305264618339877));
#82276=CARTESIAN_POINT('Ctrl Pts',(-0.199832467761139,0.128008097442224,
-0.304702643742296));
#82277=CARTESIAN_POINT('Ctrl Pts',(-0.204134223151693,0.121030185759319,
-0.304202629271089));
#82278=CARTESIAN_POINT('Ctrl Pts',(-0.211726254429488,0.107154623293612,
-0.303225921147974));
#82279=CARTESIAN_POINT('Ctrl Pts',(-0.215061272561181,0.100293350834665,
-0.302750604068203));
#82280=CARTESIAN_POINT('Ctrl Pts',(-0.219430434859827,0.090080003930204,
-0.30204385172456));
#82281=CARTESIAN_POINT('Ctrl Pts',(-0.220730131667224,0.0868465887399211,
-0.301820244975571));
#82282=CARTESIAN_POINT('Ctrl Pts',(-0.222963637299589,0.080915624169825,
-0.301409453376225));
#82283=CARTESIAN_POINT('Ctrl Pts',(-0.223920891601717,0.078227584397045,
-0.301223043338473));
#82284=CARTESIAN_POINT('Ctrl Pts',(-0.225359900312026,0.0739437058484087,
-0.300925265407773));
#82285=CARTESIAN_POINT('Ctrl Pts',(-0.225873744756608,0.0723588798611643,
-0.300814953344303));
#82286=CARTESIAN_POINT('Ctrl Pts',(-0.22681201159711,0.0693576104274131,
-0.300605705159269));
#82287=CARTESIAN_POINT('Ctrl Pts',(-0.227239969496744,0.0679423492532866,
-0.300506890159107));
#82288=CARTESIAN_POINT('Ctrl Pts',(-0.228180704954914,0.0647229793272365,
-0.300281741536621));
#82289=CARTESIAN_POINT('Ctrl Pts',(-0.228685365605001,0.0629166223994482,
-0.300155151586595));
#82290=CARTESIAN_POINT('Ctrl Pts',(-0.229944988481716,0.0581924880857962,
-0.299823321492983));
#82291=CARTESIAN_POINT('Ctrl Pts',(-0.230665831395072,0.0552660490577273,
-0.299617008753984));
#82292=CARTESIAN_POINT('Ctrl Pts',(-0.235230687917048,0.0350853430291806,
-0.298188580713162));
#82293=CARTESIAN_POINT('Ctrl Pts',(-0.237190255440108,0.017464876297323,
-0.296906754664287));
#82294=CARTESIAN_POINT('Ctrl Pts',(-0.237164491901432,-0.0122038927658462,
-0.294741033499129));
#82295=CARTESIAN_POINT('Ctrl Pts',(-0.236243679131832,-0.02418489130466,
-0.293866282665382));
#82296=CARTESIAN_POINT('Ctrl Pts',(-0.234070332528061,-0.0383190626295442,
-0.292866418383835));
#82297=CARTESIAN_POINT('Ctrl Pts',(-0.233687694842236,-0.040587355012341,
-0.292706990211092));
#82298=CARTESIAN_POINT('Ctrl Pts',(-0.233078462852458,-0.0439039807099018,
-0.292475739015903));
#82299=CARTESIAN_POINT('Ctrl Pts',(-0.232877676313772,-0.0449568387911039,
-0.2924026049039));
#82300=CARTESIAN_POINT('Ctrl Pts',(-0.232508644788786,-0.0468230765778575,
-0.292273505401584));
#82301=CARTESIAN_POINT('Ctrl Pts',(-0.232343256747318,-0.0476369763435173,
-0.29221738637369));
#82302=CARTESIAN_POINT('Ctrl Pts',(-0.231969239368831,-0.0494292756284665,
-0.292094214046769));
#82303=CARTESIAN_POINT('Ctrl Pts',(-0.231758692633005,-0.0504072393866343,
-0.292027268710623));
#82304=CARTESIAN_POINT('Ctrl Pts',(-0.231123292757905,-0.0532704287460914,
-0.291831966983464));
#82305=CARTESIAN_POINT('Ctrl Pts',(-0.230681567704826,-0.055151880680277,
-0.291704515881314));
#82306=CARTESIAN_POINT('Ctrl Pts',(-0.229607414813284,-0.0594881542306176,
-0.29141237831822));
#82307=CARTESIAN_POINT('Ctrl Pts',(-0.228958522904757,-0.061938690007187,
-0.291248481805874));
#82308=CARTESIAN_POINT('Ctrl Pts',(-0.226566109956297,-0.070421608189004,
-0.290683806939825));
#82309=CARTESIAN_POINT('Ctrl Pts',(-0.224622351775801,-0.0763951232515684,
-0.290290886308136));
#82310=CARTESIAN_POINT('Ctrl Pts',(-0.214932176059995,-0.102590943123617,
-0.288560987456185));
#82311=CARTESIAN_POINT('Ctrl Pts',(-0.204676490544675,-0.121771291991963,
-0.287265233888708));
#82312=CARTESIAN_POINT('Ctrl Pts',(-0.190255229946048,-0.141645209744189,
-0.285679416188456));
#82313=CARTESIAN_POINT('Ctrl Pts',(-0.188506295092459,-0.14396455639597,
-0.285490333663751));
#82314=CARTESIAN_POINT('Ctrl Pts',(-0.185578386823007,-0.147702546010807,
-0.285178563053428));
#82315=CARTESIAN_POINT('Ctrl Pts',(-0.184424650583428,-0.149140630585426,
-0.285056860638317));
#82316=CARTESIAN_POINT('Ctrl Pts',(-0.18231747702811,-0.151705292892896,
-0.284836536656718));
#82317=CARTESIAN_POINT('Ctrl Pts',(-0.181370059009402,-0.152836709753627,
-0.284738160605091));
#82318=CARTESIAN_POINT('Ctrl Pts',(-0.179317206485874,-0.155242279451977,
-0.284526407489484));
#82319=CARTESIAN_POINT('Ctrl Pts',(-0.178208618999928,-0.156513621550609,
-0.284412904149812));
#82320=CARTESIAN_POINT('Ctrl Pts',(-0.175123201405693,-0.159976736714004,
-0.28409923632388));
#82321=CARTESIAN_POINT('Ctrl Pts',(-0.173118929309267,-0.162143537988935,
-0.283897933977972));
#82322=CARTESIAN_POINT('Ctrl Pts',(-0.160083332301166,-0.175718940144487,
-0.282603459960778));
#82323=CARTESIAN_POINT('Ctrl Pts',(-0.14797273206907,-0.186031502910855,
-0.281462496582422));
#82324=CARTESIAN_POINT('Ctrl Pts',(-0.122878564582116,-0.203389830309261,
-0.279237459876383));
#82325=CARTESIAN_POINT('Ctrl Pts',(-0.110084202406319,-0.210589889922625,
-0.278161402006479));
#82326=CARTESIAN_POINT('Ctrl Pts',(-0.0947049310682703,-0.217457493067885,
-0.276985231664967));
#82327=CARTESIAN_POINT('Ctrl Pts',(-0.0926910865022384,-0.218323495290598,
-0.276833449300373));
#82328=CARTESIAN_POINT('Ctrl Pts',(-0.089693808526222,-0.219563446341538,
-0.276611127888372));
#82329=CARTESIAN_POINT('Ctrl Pts',(-0.0887194933516494,-0.219958945856709,
-0.276539412422915));
#82330=CARTESIAN_POINT('Ctrl Pts',(-0.0869718292039139,-0.220654865709612,
-0.276411802896522));
#82331=CARTESIAN_POINT('Ctrl Pts',(-0.086199501251897,-0.220957721933588,
-0.276355769800023));
#82332=CARTESIAN_POINT('Ctrl Pts',(-0.0844764353274816,-0.221622985324765,
-0.276231559155315));
#82333=CARTESIAN_POINT('Ctrl Pts',(-0.0835249399719161,-0.221983333266375,
-0.276163502216342));
#82334=CARTESIAN_POINT('Ctrl Pts',(-0.0806801648442189,-0.223039818330449,
-0.275961529198533));
#82335=CARTESIAN_POINT('Ctrl Pts',(-0.0787802369266001,-0.223717957466329,
-0.275828614448493));
#82336=CARTESIAN_POINT('Ctrl Pts',(-0.065550073507352,-0.228250731312771,
-0.274915176004379));
#82337=CARTESIAN_POINT('Ctrl Pts',(-0.0539494389249483,-0.231267681349453,
-0.27417497891087));
#82338=CARTESIAN_POINT('Ctrl Pts',(-0.0242180253288097,-0.236639463413832,
-0.272318726146063));
#82339=CARTESIAN_POINT('Ctrl Pts',(-0.00595455369689349,-0.23780078972795,
-0.271210896862154));
#82340=CARTESIAN_POINT('Ctrl Pts',(0.0152194618640961,-0.236704721490966,
-0.269842414849665));
#82341=CARTESIAN_POINT('Ctrl Pts',(0.018174788174134,-0.236496158582522,
-0.269649658192206));
#82342=CARTESIAN_POINT('Ctrl Pts',(0.0229785367224207,-0.236066578130393,
-0.269333073140798));
#82343=CARTESIAN_POINT('Ctrl Pts',(0.024829682379341,-0.235879055884054,
-0.269210283762994));
#82344=CARTESIAN_POINT('Ctrl Pts',(0.028146143825838,-0.235503624450238,
-0.268988785116284));
#82345=CARTESIAN_POINT('Ctrl Pts',(0.0296122870441792,-0.235323765966861,
-0.268890332864579));
#82346=CARTESIAN_POINT('Ctrl Pts',(0.0327376114709803,-0.234910698954546,
-0.26867928436136));
#82347=CARTESIAN_POINT('Ctrl Pts',(0.0343961853875026,-0.234673581532916,
-0.268566570155466));
#82348=CARTESIAN_POINT('Ctrl Pts',(0.0389160629527017,-0.233978454397253,
-0.268257389180577));
#82349=CARTESIAN_POINT('Ctrl Pts',(0.0417716257831052,-0.233485560724004,
-0.268059838120755));
#82350=CARTESIAN_POINT('Ctrl Pts',(0.0598124875004766,-0.23003002077837,
-0.266797127522385));
#82351=CARTESIAN_POINT('Ctrl Pts',(0.0746836961509353,-0.225640268093727,
-0.265686620470406));
#82352=CARTESIAN_POINT('Ctrl Pts',(0.10309832759062,-0.214134163914343,
-0.263452353107394));
#82353=CARTESIAN_POINT('Ctrl Pts',(0.116598202778023,-0.20709329908703,
-0.26233492838413));
#82354=CARTESIAN_POINT('Ctrl Pts',(0.131145348479145,-0.197629842440134,
-0.261123466124225));
#82355=CARTESIAN_POINT('Ctrl Pts',(0.132941909799233,-0.19642582948905,
-0.260973763481388));
#82356=CARTESIAN_POINT('Ctrl Pts',(0.135582579598143,-0.194603285051045,
-0.260753879875164));
#82357=CARTESIAN_POINT('Ctrl Pts',(0.136439412404792,-0.194003508447241,
-0.260682558006626));
#82358=CARTESIAN_POINT('Ctrl Pts',(0.137968610652286,-0.192917938673726,
-0.26055535453712));
#82359=CARTESIAN_POINT('Ctrl Pts',(0.138642422930922,-0.192434267246748,
-0.260499337976279));
#82360=CARTESIAN_POINT('Ctrl Pts',(0.14014125784733,-0.191346424169191,
-0.260374806708731));
#82361=CARTESIAN_POINT('Ctrl Pts',(0.140964923683091,-0.190740442961656,
-0.260306416362147));
#82362=CARTESIAN_POINT('Ctrl Pts',(0.143422351635631,-0.188907869606034,
-0.260102419339643));
#82363=CARTESIAN_POINT('Ctrl Pts',(0.145044259696085,-0.187665440516178,
-0.259967844062063));
#82364=CARTESIAN_POINT('Ctrl Pts',(0.157534261770296,-0.177839060107151,
-0.258930226621931));
#82365=CARTESIAN_POINT('Ctrl Pts',(0.167649169349661,-0.168337861946153,
-0.258081321272123));
#82366=CARTESIAN_POINT('Ctrl Pts',(0.187580879846075,-0.146025671495544,
-0.256246405739105));
#82367=CARTESIAN_POINT('Ctrl Pts',(0.197037607658726,-0.132989440744198,
-0.255263098502526));
#82368=CARTESIAN_POINT('Ctrl Pts',(0.206660021572981,-0.1164182971209,-0.254027992627695));
#82369=CARTESIAN_POINT('Ctrl Pts',(0.208163459012305,-0.113708211380189,
-0.253826571581315));
#82370=CARTESIAN_POINT('Ctrl Pts',(0.210502338947981,-0.109290239056547,
-0.253498653809637));
#82371=CARTESIAN_POINT('Ctrl Pts',(0.211371129998348,-0.10760035366967,
-0.253373326877886));
#82372=CARTESIAN_POINT('Ctrl Pts',(0.212880850105106,-0.104574940189114,
-0.253149037770916));
#82373=CARTESIAN_POINT('Ctrl Pts',(0.213529755160749,-0.103243488647643,
-0.253050359481818));
#82374=CARTESIAN_POINT('Ctrl Pts',(0.214875783557254,-0.100414670961389,
-0.252840722074069));
#82375=CARTESIAN_POINT('Ctrl Pts',(0.215569818697656,-0.0989159316360683,
-0.252729662886937));
#82376=CARTESIAN_POINT('Ctrl Pts',(0.217392135345646,-0.0948704314916453,
-0.252429843993907));
#82377=CARTESIAN_POINT('Ctrl Pts',(0.218491268708121,-0.0923109074411124,
-0.252240108221553));
#82378=CARTESIAN_POINT('Ctrl Pts',(0.225184781710279,-0.0759341871235249,
-0.251025340990785));
#82379=CARTESIAN_POINT('Ctrl Pts',(0.229510133731044,-0.061637165720413,
-0.249958226679802));
#82380=CARTESIAN_POINT('Ctrl Pts',(0.235656506295156,-0.0312570795072213,
-0.247701568476758));
#82381=CARTESIAN_POINT('Ctrl Pts',(0.23723424670619,-0.0151979632950478,
-0.246514887085686));
#82382=CARTESIAN_POINT('Ctrl Pts',(0.237165430903666,0.00297621288797808,
-0.245247490743187));
#82383=CARTESIAN_POINT('Ctrl Pts',(0.237130247962653,0.00505427478992429,
-0.245103740710931));
#82384=CARTESIAN_POINT('Ctrl Pts',(0.237036797149612,0.00816071496787572,
-0.244890854639971));
#82385=CARTESIAN_POINT('Ctrl Pts',(0.236999140809376,0.00918954987237131,
-0.244820676720547));
#82386=CARTESIAN_POINT('Ctrl Pts',(0.236919055571126,0.0110466977904574,
-0.244694631186582));
#82387=CARTESIAN_POINT('Ctrl Pts',(0.236878980505837,0.0118750609268024,
-0.244638640548759));
#82388=CARTESIAN_POINT('Ctrl Pts',(0.236778933743643,0.0137402962778775,
-0.244513080280148));
#82389=CARTESIAN_POINT('Ctrl Pts',(0.236716496140876,0.0147770011340075,
-0.244443646627491));
#82390=CARTESIAN_POINT('Ctrl Pts',(0.236505596892895,0.0179331272526227,
-0.244233248820455));
#82391=CARTESIAN_POINT('Ctrl Pts',(0.23633546116401,0.0200510592879945,
-0.244093413980158));
#82392=CARTESIAN_POINT('Ctrl Pts',(0.235341043720841,0.0306444569417719,
-0.243399493207613));
#82393=CARTESIAN_POINT('Ctrl Pts',(0.23408912166504,0.0390743318283394,
-0.242864849516497));
#82394=CARTESIAN_POINT('Ctrl Pts',(0.228060541885727,0.068618348108636,
-0.24099737152617));
#82395=CARTESIAN_POINT('Ctrl Pts',(0.220855101704296,0.089123979595825,
-0.239702457676735));
#82396=CARTESIAN_POINT('Ctrl Pts',(0.209641029013294,0.110955286301882,
-0.238117460143258));
#82397=CARTESIAN_POINT('Ctrl Pts',(0.208264951189478,0.113517159623033,
-0.237928173712019));
#82398=CARTESIAN_POINT('Ctrl Pts',(0.205939567314313,0.117661709463617,
-0.237616135206286));
#82399=CARTESIAN_POINT('Ctrl Pts',(0.205018252915175,0.119259795870082,
-0.237494371711622));
#82400=CARTESIAN_POINT('Ctrl Pts',(0.203326458989841,0.12211678694886,-0.237273981226376));
#82401=CARTESIAN_POINT('Ctrl Pts',(0.202562684228262,0.123379566258158,
-0.237175600386978));
#82402=CARTESIAN_POINT('Ctrl Pts',(0.200901116304354,0.126069683966955,
-0.236963885770057));
#82403=CARTESIAN_POINT('Ctrl Pts',(0.199999791057501,0.127494733501093,
-0.23685042618563));
#82404=CARTESIAN_POINT('Ctrl Pts',(0.197480812258102,0.131384941425137,
-0.236537010710989));
#82405=CARTESIAN_POINT('Ctrl Pts',(0.195832311531961,0.133829662049031,
-0.236335920028601));
#82406=CARTESIAN_POINT('Ctrl Pts',(0.1850717872156,0.149162821672237,-0.235047572658002));
#82407=CARTESIAN_POINT('Ctrl Pts',(0.17473940732281,0.161143060871856,-0.233913077632657));
#82408=CARTESIAN_POINT('Ctrl Pts',(0.15259804829544,0.182163169599489,-0.231686982579052));
#82409=CARTESIAN_POINT('Ctrl Pts',(0.140974861054286,0.191300136693265,
-0.23060308542215));
#82410=CARTESIAN_POINT('Ctrl Pts',(0.12674175486475,0.200482616674133,-0.229420379300678));
#82411=CARTESIAN_POINT('Ctrl Pts',(0.124889887881046,0.201641436129321,
-0.229269133627125));
#82412=CARTESIAN_POINT('Ctrl Pts',(0.122124451376495,0.203319211082609,
-0.229047440720122));
#82413=CARTESIAN_POINT('Ctrl Pts',(0.12122307888493,0.203857912454156,-0.228975826285862));
#82414=CARTESIAN_POINT('Ctrl Pts',(0.11960326456342,0.204811444662896,-0.228848321537439));
#82415=CARTESIAN_POINT('Ctrl Pts',(0.11888619397236,0.205228510941119,-0.228792293228712));
#82416=CARTESIAN_POINT('Ctrl Pts',(0.11728365425391,0.206149370156308,-0.2286680026274));
#82417=CARTESIAN_POINT('Ctrl Pts',(0.116397114079517,0.206651228645653,
-0.228599861891554));
#82418=CARTESIAN_POINT('Ctrl Pts',(0.113739891180856,0.208132921448531,
-0.228397378344447));
#82419=CARTESIAN_POINT('Ctrl Pts',(0.111959821231756,0.209095851071455,
-0.228264044434999));
#82420=CARTESIAN_POINT('Ctrl Pts',(0.0995565237143344,0.215601601108312,
-0.227349329052414));
#82421=CARTESIAN_POINT('Ctrl Pts',(0.0885375182843082,0.22035592507667,
-0.226608334829467));
#82422=CARTESIAN_POINT('Ctrl Pts',(0.0599853404440585,0.230185583827689,
-0.224753132956455));
#82423=CARTESIAN_POINT('Ctrl Pts',(0.0421420985265483,0.234110254978682,
-0.223647029432988));
#82424=CARTESIAN_POINT('Ctrl Pts',(0.0210759898834814,0.236255322603898,
-0.222280354114845));
#82425=CARTESIAN_POINT('Ctrl Pts',(0.0181204824398082,0.23650036294834,
-0.222087408859593));
#82426=CARTESIAN_POINT('Ctrl Pts',(0.0133036130396962,0.236808909277324,
-0.221770577768577));
#82427=CARTESIAN_POINT('Ctrl Pts',(0.0114446761111455,0.236906025024711,
-0.221647733749127));
#82428=CARTESIAN_POINT('Ctrl Pts',(0.00810885019312719,0.237040944266894,
-0.221426177069523));
#82429=CARTESIAN_POINT('Ctrl Pts',(0.0066323724036509,0.23708684944135,
-0.221327722020929));
#82430=CARTESIAN_POINT('Ctrl Pts',(0.00348115318510966,0.237155365240182,
-0.221116711741436));
#82431=CARTESIAN_POINT('Ctrl Pts',(0.00180641587100689,0.2371740337858,
-0.221004038979407));
#82432=CARTESIAN_POINT('Ctrl Pts',(-0.00276325770148828,0.237176570449328,
-0.220695088179958));
#82433=CARTESIAN_POINT('Ctrl Pts',(-0.00565784294585478,0.237125175148811,
-0.220497728528713));
#82434=CARTESIAN_POINT('Ctrl Pts',(-0.0197582379176476,0.236616495735213,
-0.219527834492675));
#82435=CARTESIAN_POINT('Ctrl Pts',(-0.0309145038583286,0.235418063051798,
-0.218733292196062));
#82436=CARTESIAN_POINT('Ctrl Pts',(-0.0419358573824117,0.23343813846628,
-0.21792431326882));
#82437=CARTESIAN_POINT('Origin',(0.,0.,-1.7456589891905));
#82438=CARTESIAN_POINT('',(-0.0419357865133591,0.233438151197498,-0.0979694843087456));
#82439=CARTESIAN_POINT('',(-0.0419358257166351,0.233438144154857,-0.117607078812657));
#82440=CARTESIAN_POINT('',(-0.0419358257166344,0.233438144154858,-1.7456589891905));
#82441=CARTESIAN_POINT('Ctrl Pts',(-0.0419357865133626,0.233438151197497,
-0.0979694843087454));
#82442=CARTESIAN_POINT('Ctrl Pts',(-0.0296502970070915,0.235645166899533,
-0.0988623235472579));
#82443=CARTESIAN_POINT('Ctrl Pts',(-0.0172022719087811,0.236880230763759,
-0.0997773423278653));
#82444=CARTESIAN_POINT('Ctrl Pts',(0.00526639588502789,0.237326279997791,
-0.101416241531675));
#82445=CARTESIAN_POINT('Ctrl Pts',(0.0152438555841809,0.23689483305609,
-0.102139040137741));
#82446=CARTESIAN_POINT('Ctrl Pts',(0.0274385970011549,0.235593570823695,
-0.102996550783393));
#82447=CARTESIAN_POINT('Ctrl Pts',(0.0297083461511621,0.235318130091136,
-0.103155020639958));
#82448=CARTESIAN_POINT('Ctrl Pts',(0.0330342406462287,0.234865631355384,
-0.103385226295336));
#82449=CARTESIAN_POINT('Ctrl Pts',(0.0340936593597889,0.234714184381017,
-0.103458255688368));
#82450=CARTESIAN_POINT('Ctrl Pts',(0.0358939585432025,0.234444379689392,
-0.103581805818235));
#82451=CARTESIAN_POINT('Ctrl Pts',(0.0366353544226617,0.234329670118397,
-0.10363252559559));
#82452=CARTESIAN_POINT('Ctrl Pts',(0.0383259100939763,0.234059885739427,
-0.103747802115136));
#82453=CARTESIAN_POINT('Ctrl Pts',(0.0392746864652687,0.233902553602965,
-0.103812231261498));
#82454=CARTESIAN_POINT('Ctrl Pts',(0.041912373716246,0.233448653431822,
-0.103990674570355));
#82455=CARTESIAN_POINT('Ctrl Pts',(0.0435991041550788,0.233139527744794,
-0.104104011653244));
#82456=CARTESIAN_POINT('Ctrl Pts',(0.0563400609601184,0.23066138783625,
-0.104955287501612));
#82457=CARTESIAN_POINT('Ctrl Pts',(0.0672320017415795,0.227725281444977,
-0.105655775882896));
#82458=CARTESIAN_POINT('Ctrl Pts',(0.0790729838427031,0.223609150026908,
-0.106427197102565));
#82459=CARTESIAN_POINT('Ctrl Pts',(0.0802674417935084,0.223183168194255,
-0.106505123941752));
#82460=CARTESIAN_POINT('Ctrl Pts',(0.0935508502138204,0.218325448147053,
-0.107373494122607));
#82461=CARTESIAN_POINT('Ctrl Pts',(0.105262485500107,0.212926167066963,
-0.108156791943747));
#82462=CARTESIAN_POINT('Ctrl Pts',(0.122629804939815,0.203134901026933,
-0.109409586985152));
#82463=CARTESIAN_POINT('Ctrl Pts',(0.128623298879774,0.199393804944908,
-0.109860150855383));
#82464=CARTESIAN_POINT('Ctrl Pts',(0.136351794999779,0.19407614654249,-0.110471684636701));
#82465=CARTESIAN_POINT('Ctrl Pts',(0.13824355289158,0.192733188924514,-0.110623915464666));
#82466=CARTESIAN_POINT('Ctrl Pts',(0.141362616754455,0.190449419196269,
-0.110879365283801));
#82467=CARTESIAN_POINT('Ctrl Pts',(0.142600994878233,0.189523947707758,
-0.11098198798307));
#82468=CARTESIAN_POINT('Ctrl Pts',(0.145016645453251,0.187681590911978,
-0.111184596387472));
#82469=CARTESIAN_POINT('Ctrl Pts',(0.146194488975136,0.186765570281374,
-0.111284544872751));
#82470=CARTESIAN_POINT('Ctrl Pts',(0.149025636432859,0.184520567151784,
-0.111527662042611));
#82471=CARTESIAN_POINT('Ctrl Pts',(0.150669880487639,0.183180420948124,
-0.111671274290903));
#82472=CARTESIAN_POINT('Ctrl Pts',(0.156208400688382,0.178541211467236,
-0.112163487267368));
#82473=CARTESIAN_POINT('Ctrl Pts',(0.160013833270068,0.175138787437171,
-0.112516267672541));
#82474=CARTESIAN_POINT('Ctrl Pts',(0.17919013169737,0.156846364889147,-0.114372903367958));
#82475=CARTESIAN_POINT('Ctrl Pts',(0.192602417110062,0.140049669047372,
-0.115959227321972));
#82476=CARTESIAN_POINT('Ctrl Pts',(0.205961363579348,0.117700783204675,
-0.117838972832013));
#82477=CARTESIAN_POINT('Ctrl Pts',(0.208227142396897,0.113644269778579,
-0.118171408062634));
#82478=CARTESIAN_POINT('Ctrl Pts',(0.21176934589466,0.10684042088923,-0.118711904040006));
#82479=CARTESIAN_POINT('Ctrl Pts',(0.213114874962106,0.104130608332205,
-0.118922846291999));
#82480=CARTESIAN_POINT('Ctrl Pts',(0.214916077539252,0.100321837949637,
-0.119212636339154));
#82481=CARTESIAN_POINT('Ctrl Pts',(0.215415829334444,0.0992442047540888,
-0.119293892916657));
#82482=CARTESIAN_POINT('Ctrl Pts',(0.216255501052316,0.0973973611503321,
-0.11943184250332));
#82483=CARTESIAN_POINT('Ctrl Pts',(0.216599458075126,0.0966300292158377,
-0.119488774312477));
#82484=CARTESIAN_POINT('Ctrl Pts',(0.217314403298719,0.095012061626186,
-0.119607998972777));
#82485=CARTESIAN_POINT('Ctrl Pts',(0.217684487627134,0.0941610623125813,
-0.119670238888293));
#82486=CARTESIAN_POINT('Ctrl Pts',(0.21867442692235,0.0918476906086514,
-0.119838223970688));
#82487=CARTESIAN_POINT('Ctrl Pts',(0.219284615626328,0.0903811979696927,
-0.119943410308313));
#82488=CARTESIAN_POINT('Ctrl Pts',(0.222252324054333,0.0830417550943661,
-0.120463910861526));
#82489=CARTESIAN_POINT('Ctrl Pts',(0.224389071118317,0.0770817012009295,
-0.120867797357706));
#82490=CARTESIAN_POINT('Ctrl Pts',(0.230055927068213,0.0590316652519871,
-0.122055535693422));
#82491=CARTESIAN_POINT('Ctrl Pts',(0.232864730298824,0.0467388204712098,
-0.122819020413789));
#82492=CARTESIAN_POINT('Ctrl Pts',(0.23594012342884,0.0256847102230647,
-0.12412812249881));
#82493=CARTESIAN_POINT('Ctrl Pts',(0.23672244495599,0.0170268520257548,
-0.124666668127815));
#82494=CARTESIAN_POINT('Ctrl Pts',(0.237224436192984,0.00277035666120866,
-0.12557144375578));
#82495=CARTESIAN_POINT('Ctrl Pts',(0.237223951580282,-0.00281018967891917,
-0.125930037078752));
#82496=CARTESIAN_POINT('Ctrl Pts',(0.236950725223211,-0.0105335445401973,
-0.126435150991745));
#82497=CARTESIAN_POINT('Ctrl Pts',(0.236845522297355,-0.0126806866194454,
-0.126576515422812));
#82498=CARTESIAN_POINT('Ctrl Pts',(0.236615915622534,-0.0163465636875743,
-0.126819617219337));
#82499=CARTESIAN_POINT('Ctrl Pts',(0.236506033809207,-0.017866098022569,
-0.126920898222681));
#82500=CARTESIAN_POINT('Ctrl Pts',(0.23626870837976,-0.0207601382877996,
-0.127114818793256));
#82501=CARTESIAN_POINT('Ctrl Pts',(0.2361438890667,-0.0221348010830024,
-0.127207372442139));
#82502=CARTESIAN_POINT('Ctrl Pts',(0.235788703276618,-0.0257006251974836,
-0.12744863959502));
#82503=CARTESIAN_POINT('Ctrl Pts',(0.235539795532364,-0.0278897630292103,
-0.127597925128941));
#82504=CARTESIAN_POINT('Ctrl Pts',(0.234557521020033,-0.0355735508544045,
-0.128126176961274));
#82505=CARTESIAN_POINT('Ctrl Pts',(0.233662114391534,-0.0410452892270384,
-0.128510099895484));
#82506=CARTESIAN_POINT('Ctrl Pts',(0.228956189674062,-0.064592586781429,
-0.130196829830423));
#82507=CARTESIAN_POINT('Ctrl Pts',(0.223233293707215,-0.0822183391911368,
-0.13155519211993));
#82508=CARTESIAN_POINT('Ctrl Pts',(0.213052851899309,-0.104381792501776,
-0.133324915147205));
#82509=CARTESIAN_POINT('Ctrl Pts',(0.210379075050698,-0.109671007246825,
-0.133751626709029));
#82510=CARTESIAN_POINT('Ctrl Pts',(0.205773711537953,-0.11799158313073,
-0.134424555871511));
#82511=CARTESIAN_POINT('Ctrl Pts',(0.203966535122649,-0.121088768858699,
-0.134675413868254));
#82512=CARTESIAN_POINT('Ctrl Pts',(0.201421854732821,-0.125231166540058,
-0.135010272661717));
#82513=CARTESIAN_POINT('Ctrl Pts',(0.200745213416078,-0.126312976807091,
-0.135097660143353));
#82514=CARTESIAN_POINT('Ctrl Pts',(0.199596312420747,-0.128117280316379,
-0.135243236113761));
#82515=CARTESIAN_POINT('Ctrl Pts',(0.199128786446996,-0.128842741121642,
-0.135301720381014));
#82516=CARTESIAN_POINT('Ctrl Pts',(0.198163444429932,-0.130322857406912,
-0.135420919112081));
#82517=CARTESIAN_POINT('Ctrl Pts',(0.197665256220833,-0.131077246014573,
-0.135481608294959));
#82518=CARTESIAN_POINT('Ctrl Pts',(0.196342369979463,-0.133055750942652,
-0.135640657651683));
#82519=CARTESIAN_POINT('Ctrl Pts',(0.195510522389097,-0.134275072208138,
-0.135738557599815));
#82520=CARTESIAN_POINT('Ctrl Pts',(0.191822389533644,-0.139574186748402,
-0.136163876183264));
#82521=CARTESIAN_POINT('Ctrl Pts',(0.188849182762526,-0.143571504638587,
-0.136484323789983));
#82522=CARTESIAN_POINT('Ctrl Pts',(0.176295664600405,-0.159383547039957,
-0.13776353729087));
#82523=CARTESIAN_POINT('Ctrl Pts',(0.165714901945666,-0.170358201862381,
-0.138680749379591));
#82524=CARTESIAN_POINT('Ctrl Pts',(0.145037245659004,-0.188042895364414,
-0.140358765807748));
#82525=CARTESIAN_POINT('Ctrl Pts',(0.135341716696507,-0.19513712982678,
-0.141108930978769));
#82526=CARTESIAN_POINT('Ctrl Pts',(0.122863008083415,-0.202888942367795,
-0.142062787531925));
#82527=CARTESIAN_POINT('Ctrl Pts',(0.120550077429619,-0.204271680758161,
-0.142239068440764));
#82528=CARTESIAN_POINT('Ctrl Pts',(0.116798390582325,-0.206428640332843,
-0.142524466897245));
#82529=CARTESIAN_POINT('Ctrl Pts',(0.115374277767884,-0.207227950328199,
-0.1426326794694));
#82530=CARTESIAN_POINT('Ctrl Pts',(0.112637969237295,-0.208726805699705,
-0.14284042856344));
#82531=CARTESIAN_POINT('Ctrl Pts',(0.11132722252084,-0.209428844441946,
-0.142939870303248));
#82532=CARTESIAN_POINT('Ctrl Pts',(0.108320533248837,-0.211003031619845,
-0.143167854295474));
#82533=CARTESIAN_POINT('Ctrl Pts',(0.106620517609702,-0.211867133203949,
-0.143296671171745));
#82534=CARTESIAN_POINT('Ctrl Pts',(0.101155608140235,-0.21456246333258,
-0.143710594915352));
#82535=CARTESIAN_POINT('Ctrl Pts',(0.097352754746615,-0.216314458661817,
-0.143998386545142));
#82536=CARTESIAN_POINT('Ctrl Pts',(0.076587470532443,-0.225222653805274,
-0.145569461166284));
#82537=CARTESIAN_POINT('Ctrl Pts',(0.0588841223995243,-0.230484972980918,
-0.14691448185796));
#82538=CARTESIAN_POINT('Ctrl Pts',(0.0308961087109997,-0.235366855482296,
-0.148985768307353));
#82539=CARTESIAN_POINT('Ctrl Pts',(0.0209377253252353,-0.23646094135097,
-0.149710785513475));
#82540=CARTESIAN_POINT('Ctrl Pts',(0.00865477628305593,-0.237028067937734,
-0.150570420715818));
#82541=CARTESIAN_POINT('Ctrl Pts',(0.00636888330677741,-0.237100502804236,
-0.15072891438379));
#82542=CARTESIAN_POINT('Ctrl Pts',(0.0030129791589171,-0.237158272360684,
-0.150959080476967));
#82543=CARTESIAN_POINT('Ctrl Pts',(0.00194362205948525,-0.237169447097857,
-0.151032047743092));
#82544=CARTESIAN_POINT('Ctrl Pts',(0.000123397125888366,-0.237176156287328,
-0.151155570988071));
#82545=CARTESIAN_POINT('Ctrl Pts',(-0.000627420688090736,-0.237175358626607,
-0.151206324337761));
#82546=CARTESIAN_POINT('Ctrl Pts',(-0.00234487118603359,-0.237165378127367,
-0.151321959629161));
#82547=CARTESIAN_POINT('Ctrl Pts',(-0.00331146528490936,-0.237153851504941,
-0.151386711623283));
#82548=CARTESIAN_POINT('Ctrl Pts',(-0.00600141592165971,-0.237105324315642,
-0.15156606430459));
#82549=CARTESIAN_POINT('Ctrl Pts',(-0.00772452011704736,-0.237055445044221,
-0.151679985054861));
#82550=CARTESIAN_POINT('Ctrl Pts',(-0.0209506145951181,-0.23652821412298,
-0.152548034431701));
#82551=CARTESIAN_POINT('Ctrl Pts',(-0.0324072025590242,-0.235232583416807,
-0.153263286616282));
#82552=CARTESIAN_POINT('Ctrl Pts',(-0.0442734976490555,-0.233006756850052,
-0.154006167339822));
#82553=CARTESIAN_POINT('Ctrl Pts',(-0.0448209908590255,-0.232902061203127,
-0.154040446250534));
#82554=CARTESIAN_POINT('Ctrl Pts',(-0.0546570822746849,-0.230985164146947,
-0.154656425495733));
#82555=CARTESIAN_POINT('Ctrl Pts',(-0.0638292257565803,-0.228620579608439,
-0.155233379005194));
#82556=CARTESIAN_POINT('Ctrl Pts',(-0.0793861270860631,-0.223600542396664,
-0.156246223577628));
#82557=CARTESIAN_POINT('Ctrl Pts',(-0.0858412260355698,-0.221202697185943,
-0.156677095946507));
#82558=CARTESIAN_POINT('Ctrl Pts',(-0.0965617681928096,-0.216680398596723,
-0.157419157318497));
#82559=CARTESIAN_POINT('Ctrl Pts',(-0.100884160695088,-0.214702006151476,
-0.157725917847034));
#82560=CARTESIAN_POINT('Ctrl Pts',(-0.106955765509068,-0.211699150489251,
-0.158169391279693));
#82561=CARTESIAN_POINT('Ctrl Pts',(-0.108755968918634,-0.210779991697385,
-0.158302493265481));
#82562=CARTESIAN_POINT('Ctrl Pts',(-0.111868656451764,-0.209140205320798,
-0.158535580709895));
#82563=CARTESIAN_POINT('Ctrl Pts',(-0.113186490573348,-0.208429940158595,
-0.158635197973423));
#82564=CARTESIAN_POINT('Ctrl Pts',(-0.115725062858082,-0.20703056612243,
-0.158828953862965));
#82565=CARTESIAN_POINT('Ctrl Pts',(-0.116946592074119,-0.20634301524124,
-0.158923033795038));
#82566=CARTESIAN_POINT('Ctrl Pts',(-0.120193190949362,-0.204477543302115,
-0.159175395607942));
#82567=CARTESIAN_POINT('Ctrl Pts',(-0.122206978977638,-0.203280403556447,
-0.159334363762111));
#82568=CARTESIAN_POINT('Ctrl Pts',(-0.129809096186403,-0.198607372570047,
-0.159944025178804));
#82569=CARTESIAN_POINT('Ctrl Pts',(-0.135269166933451,-0.194929546079957,
-0.160401980760352));
#82570=CARTESIAN_POINT('Ctrl Pts',(-0.156276049181342,-0.179471677087928,
-0.162246144590844));
#82571=CARTESIAN_POINT('Ctrl Pts',(-0.170496885396524,-0.166020864733996,
-0.163690208444125));
#82572=CARTESIAN_POINT('Ctrl Pts',(-0.185783894244829,-0.147501610085427,
-0.165421610853591));
#82573=CARTESIAN_POINT('Ctrl Pts',(-0.188559241875037,-0.143936782942163,
-0.165744446181988));
#82574=CARTESIAN_POINT('Ctrl Pts',(-0.192987113327554,-0.137901291045558,
-0.166271461189346));
#82575=CARTESIAN_POINT('Ctrl Pts',(-0.19469800369272,-0.135475021090899,
-0.166478325900128));
#82576=CARTESIAN_POINT('Ctrl Pts',(-0.19702713335062,-0.132036705832587,
-0.166763888942078));
#82577=CARTESIAN_POINT('Ctrl Pts',(-0.197683947227924,-0.131051288128644,
-0.166844878600389));
#82578=CARTESIAN_POINT('Ctrl Pts',(-0.198795915797674,-0.129355618169833,
-0.166982734377129));
#82579=CARTESIAN_POINT('Ctrl Pts',(-0.199254706253551,-0.128647791348568,
-0.167039834035365));
#82580=CARTESIAN_POINT('Ctrl Pts',(-0.200213320589415,-0.127151399690861,
-0.167159593043341));
#82581=CARTESIAN_POINT('Ctrl Pts',(-0.200712276150341,-0.12636231424909,
-0.167222197294596));
#82582=CARTESIAN_POINT('Ctrl Pts',(-0.202061497451522,-0.124200400006544,
-0.167392288613574));
#82583=CARTESIAN_POINT('Ctrl Pts',(-0.202902441524335,-0.122821772055035,
-0.167499192470464));
#82584=CARTESIAN_POINT('Ctrl Pts',(-0.207170059161103,-0.115662045762974,
-0.168046956485997));
#82585=CARTESIAN_POINT('Ctrl Pts',(-0.210364301721418,-0.109745253559405,
-0.168474892278541));
#82586=CARTESIAN_POINT('Ctrl Pts',(-0.219580861595622,-0.090787515397533,
-0.169795237678399));
#82587=CARTESIAN_POINT('Ctrl Pts',(-0.224673269829578,-0.0773310182121016,
-0.170661704553817));
#82588=CARTESIAN_POINT('Ctrl Pts',(-0.231347718129668,-0.0533101887918559,
-0.172203453400025));
#82589=CARTESIAN_POINT('Ctrl Pts',(-0.233493482912646,-0.0429476118216739,
-0.172866752055428));
#82590=CARTESIAN_POINT('Ctrl Pts',(-0.235331768237854,-0.029649432772079,
-0.173736915432756));
#82591=CARTESIAN_POINT('Ctrl Pts',(-0.23567157363426,-0.0268148885641986,
-0.173923419753141));
#82592=CARTESIAN_POINT('Ctrl Pts',(-0.236128644959213,-0.0223164269138676,
-0.17422136407572));
#82593=CARTESIAN_POINT('Ctrl Pts',(-0.236279670300917,-0.0206561623852188,
-0.174331747677524));
#82594=CARTESIAN_POINT('Ctrl Pts',(-0.236531678892094,-0.0175195586972447,
-0.174541143305403));
#82595=CARTESIAN_POINT('Ctrl Pts',(-0.236636373061018,-0.0160435915765055,
-0.174640034194312));
#82596=CARTESIAN_POINT('Ctrl Pts',(-0.236842542188051,-0.0126930992496076,
-0.174865374608882));
#82597=CARTESIAN_POINT('Ctrl Pts',(-0.236935584727386,-0.0108181743880108,
-0.174992080937197));
#82598=CARTESIAN_POINT('Ctrl Pts',(-0.237120120327206,-0.00592729861421873,
-0.175324266635088));
#82599=CARTESIAN_POINT('Ctrl Pts',(-0.237176331506308,-0.00291043915855068,
-0.175530820825717));
#82600=CARTESIAN_POINT('Ctrl Pts',(-0.237169629823592,0.0120064184497657,
-0.176560669106382));
#82601=CARTESIAN_POINT('Ctrl Pts',(-0.236268727446282,0.0238872698427732,
-0.177409033635695));
#82602=CARTESIAN_POINT('Ctrl Pts',(-0.232595665367843,0.0480468528614814,
-0.179181181641774));
#82603=CARTESIAN_POINT('Ctrl Pts',(-0.22973046826708,0.0602756598030736,
-0.180103840466648));
#82604=CARTESIAN_POINT('Ctrl Pts',(-0.223972964181899,0.0782856049083706,
-0.181465462863492));
#82605=CARTESIAN_POINT('Ctrl Pts',(-0.221790416919298,0.0842707001371504,
-0.181918159224013));
#82606=CARTESIAN_POINT('Ctrl Pts',(-0.218764640787951,0.0916326550916187,
-0.182469493903072));
#82607=CARTESIAN_POINT('Ctrl Pts',(-0.218145061551391,0.093098034363224,
-0.182578952955352));
#82608=CARTESIAN_POINT('Ctrl Pts',(-0.217140509370585,0.0954088166548229,
-0.182750987278822));
#82609=CARTESIAN_POINT('Ctrl Pts',(-0.21676524798063,0.0962583526113689,
-0.182814109999193));
#82610=CARTESIAN_POINT('Ctrl Pts',(-0.216038396768121,0.0978780281791985,
-0.182934188207076));
#82611=CARTESIAN_POINT('Ctrl Pts',(-0.215687663061853,0.0986485139394347,
-0.182991189472202));
#82612=CARTESIAN_POINT('Ctrl Pts',(-0.214830378888533,0.100505351189763,
-0.183128300551818));
#82613=CARTESIAN_POINT('Ctrl Pts',(-0.214319696103869,0.101589789470971,
-0.183208162754854));
#82614=CARTESIAN_POINT('Ctrl Pts',(-0.212477328474379,0.105426337412689,
-0.183490102194614));
#82615=CARTESIAN_POINT('Ctrl Pts',(-0.211100614825139,0.108156646974326,
-0.183689646358448));
#82616=CARTESIAN_POINT('Ctrl Pts',(-0.20747130783064,0.115020834465941,
-0.184190429503946));
#82617=CARTESIAN_POINT('Ctrl Pts',(-0.205147679212546,0.11911578843044,
-0.184488354641332));
#82618=CARTESIAN_POINT('Ctrl Pts',(-0.190996797101151,0.142410049123834,
-0.186193920512833));
#82619=CARTESIAN_POINT('Ctrl Pts',(-0.176602377519959,0.159912672971394,
-0.187531056512033));
#82620=CARTESIAN_POINT('Ctrl Pts',(-0.156885554463896,0.177921778831899,
-0.189241229014651));
#82621=CARTESIAN_POINT('Ctrl Pts',(-0.153745479005323,0.180642079648262,
-0.189510140310479));
#82622=CARTESIAN_POINT('Ctrl Pts',(-0.149044783077938,0.184502996840263,
-0.189908856633506));
#82623=CARTESIAN_POINT('Ctrl Pts',(-0.147538978764656,0.18570932283121,
-0.190036022723369));
#82624=CARTESIAN_POINT('Ctrl Pts',(-0.144844910826985,0.187814139659975,
-0.190262662666932));
#82625=CARTESIAN_POINT('Ctrl Pts',(-0.143662571948544,0.188720069142855,
-0.190361835606296));
#82626=CARTESIAN_POINT('Ctrl Pts',(-0.141175845133713,0.190588533401589,
-0.190569859540911));
#82627=CARTESIAN_POINT('Ctrl Pts',(-0.139869969087599,0.191548948927301,
-0.190678786045187));
#82628=CARTESIAN_POINT('Ctrl Pts',(-0.136411550309813,0.194038244058697,
-0.190966501124822));
#82629=CARTESIAN_POINT('Ctrl Pts',(-0.134243196607195,0.195544660889043,
-0.191146132365549));
#82630=CARTESIAN_POINT('Ctrl Pts',(-0.12297638748398,0.203096310757125,
-0.192075994484177));
#82631=CARTESIAN_POINT('Ctrl Pts',(-0.113494563711403,0.208543103336196,
-0.192847885563617));
#82632=CARTESIAN_POINT('Ctrl Pts',(-0.0907806086982198,0.219582141372441,
-0.194668225909773));
#82633=CARTESIAN_POINT('Ctrl Pts',(-0.077348037838596,0.224665734697365,
-0.195724955588978));
#82634=CARTESIAN_POINT('Ctrl Pts',(-0.0569941024071704,0.230325426267022,
-0.197249209986626));
#82635=CARTESIAN_POINT('Ctrl Pts',(-0.0503732679658347,0.231863497808429,
-0.197733162821848));
#82636=CARTESIAN_POINT('Ctrl Pts',(-0.0431089756126745,0.233225110688087,
-0.19824534105726));
#82637=CARTESIAN_POINT('Ctrl Pts',(-0.0425226023732719,0.233332733088914,
-0.198286551480927));
#82638=CARTESIAN_POINT('Ctrl Pts',(-0.0419358257146564,0.233438144155213,
-0.198327653695922));
#82639=CARTESIAN_POINT('',(-0.237174999736212,0.000149622570500169,-0.195497187201803));
#82640=CARTESIAN_POINT('Ctrl Pts',(-0.0419358573824119,0.23343813846628,
-0.21792431326882));
#82641=CARTESIAN_POINT('Ctrl Pts',(-0.0475813473021413,0.232423957742928,
-0.217509928377795));
#82642=CARTESIAN_POINT('Ctrl Pts',(-0.0531914539463961,0.231204729662501,
-0.217091959100834));
#82643=CARTESIAN_POINT('Ctrl Pts',(-0.0718995017673666,0.226421103070235,
-0.21568278922388));
#82644=CARTESIAN_POINT('Ctrl Pts',(-0.08473246436092,0.221938116056266,
-0.214689093391387));
#82645=CARTESIAN_POINT('Ctrl Pts',(-0.0989682866032168,0.215549057935862,
-0.213598669945546));
#82646=CARTESIAN_POINT('Ctrl Pts',(-0.100813330008522,0.214692317737573,
-0.21345762059194));
#82647=CARTESIAN_POINT('Ctrl Pts',(-0.103578434075613,0.21336484175236,
-0.213246895731129));
#82648=CARTESIAN_POINT('Ctrl Pts',(-0.104506763191787,0.212911681800699,
-0.213176262852819));
#82649=CARTESIAN_POINT('Ctrl Pts',(-0.106187000873629,0.212077843371299,
-0.213048666863625));
#82650=CARTESIAN_POINT('Ctrl Pts',(-0.10693989715422,0.211699195298644,
-0.212991583686003));
#82651=CARTESIAN_POINT('Ctrl Pts',(-0.10850471271827,0.210901736530197,
-0.212873154268009));
#82652=CARTESIAN_POINT('Ctrl Pts',(-0.109316253104794,0.210482236854643,
-0.212811851042991));
#82653=CARTESIAN_POINT('Ctrl Pts',(-0.111475115727062,0.209350428110302,
-0.21264902875134));
#82654=CARTESIAN_POINT('Ctrl Pts',(-0.112818056847528,0.208629790598616,
-0.21254801217778));
#82655=CARTESIAN_POINT('Ctrl Pts',(-0.119562607976484,0.20492641666531,
-0.212041568395363));
#82656=CARTESIAN_POINT('Ctrl Pts',(-0.124853786587566,0.201746375086211,
-0.211647122413952));
#82657=CARTESIAN_POINT('Ctrl Pts',(-0.139575678231878,0.192097048014007,
-0.210540364956864));
#82658=CARTESIAN_POINT('Ctrl Pts',(-0.148670991652626,0.185147538116201,
-0.209844614970619));
#82659=CARTESIAN_POINT('Ctrl Pts',(-0.167970311510928,0.168058769231198,
-0.208261922196304));
#82660=CARTESIAN_POINT('Ctrl Pts',(-0.177824246589785,0.157595170912801,
-0.207373553800128));
#82661=CARTESIAN_POINT('Ctrl Pts',(-0.1883891081727,0.14411548477092,-0.206262633302431));
#82662=CARTESIAN_POINT('Ctrl Pts',(-0.190067462902371,0.141894635264199,
-0.206080674187128));
#82663=CARTESIAN_POINT('Ctrl Pts',(-0.192678509028361,0.13831015640968,
-0.205788360392234));
#82664=CARTESIAN_POINT('Ctrl Pts',(-0.193636744596031,0.136965390218447,
-0.205678994601114));
#82665=CARTESIAN_POINT('Ctrl Pts',(-0.195427773767813,0.134395535352883,
-0.205470497454414));
#82666=CARTESIAN_POINT('Ctrl Pts',(-0.196263287427143,0.133172431531167,
-0.205371475979964));
#82667=CARTESIAN_POINT('Ctrl Pts',(-0.198144701979407,0.130362075661904,
-0.205144385638657));
#82668=CARTESIAN_POINT('Ctrl Pts',(-0.199183076085089,0.128769932552469,
-0.205016043318625));
#82669=CARTESIAN_POINT('Ctrl Pts',(-0.202368897983294,0.123754355414727,
-0.204612599241643));
#82670=CARTESIAN_POINT('Ctrl Pts',(-0.20444796145925,0.120288565313191,
-0.204335038133216));
#82671=CARTESIAN_POINT('Ctrl Pts',(-0.217230163614773,0.0976912409873149,
-0.202532016808482));
#82672=CARTESIAN_POINT('Ctrl Pts',(-0.225324127245524,0.0772088528636334,
-0.200913870670797));
#82673=CARTESIAN_POINT('Ctrl Pts',(-0.232174844739072,0.0489682894189661,
-0.198810257691918));
#82674=CARTESIAN_POINT('Ctrl Pts',(-0.233544999494523,0.0419500199357592,
-0.198298686662149));
#82675=CARTESIAN_POINT('Ctrl Pts',(-0.23488572077168,0.0329325829767082,
-0.197663620432129));
#82676=CARTESIAN_POINT('Ctrl Pts',(-0.235151015032261,0.030981568729426,
-0.197527537215044));
#82677=CARTESIAN_POINT('Ctrl Pts',(-0.235516870281126,0.028014737500568,
-0.19732282445107));
#82678=CARTESIAN_POINT('Ctrl Pts',(-0.23563521377347,0.0270012561039096,
-0.197253286522257));
#82679=CARTESIAN_POINT('Ctrl Pts',(-0.235830586734086,0.0252288869015158,
-0.197132401553093));
#82680=CARTESIAN_POINT('Ctrl Pts',(-0.235910499416103,0.0244703633485507,
-0.197080899613214));
#82681=CARTESIAN_POINT('Ctrl Pts',(-0.236066270194763,0.0229200630103421,
-0.196976111803439));
#82682=CARTESIAN_POINT('Ctrl Pts',(-0.236141805411595,0.0221282849541749,
-0.196922843244826));
#82683=CARTESIAN_POINT('Ctrl Pts',(-0.236304116651473,0.0203313289297527,
-0.196802483779544));
#82684=CARTESIAN_POINT('Ctrl Pts',(-0.236388465503058,0.0193259397540431,
-0.196735522155818));
#82685=CARTESIAN_POINT('Ctrl Pts',(-0.236643307830565,0.0160365523661593,
-0.196517588783739));
#82686=CARTESIAN_POINT('Ctrl Pts',(-0.236787139955247,0.0137505420066819,
-0.196367941629022));
#82687=CARTESIAN_POINT('Ctrl Pts',(-0.237080167909662,0.0076945842123848,
-0.195975440832477));
#82688=CARTESIAN_POINT('Ctrl Pts',(-0.237172572604718,0.00392248085024846,
-0.195734988776373));
#82689=CARTESIAN_POINT('Ctrl Pts',(-0.237174952801866,0.000149627646716525,
-0.195497106204122));
#82690=CARTESIAN_POINT('Ctrl Pts',(-0.0419358257166351,0.233438144154857,
-0.117607078812657));
#82691=CARTESIAN_POINT('Ctrl Pts',(-0.0419265777945186,0.233439805491104,
-0.117607705924788));
#82692=CARTESIAN_POINT('Ctrl Pts',(-0.0419173297741229,0.233441466277719,
-0.1176083330665));
#82693=CARTESIAN_POINT('Ctrl Pts',(-0.0409907050910767,0.233607815415776,
-0.117671173135956));
#82694=CARTESIAN_POINT('Ctrl Pts',(-0.0400723854496901,0.233767091732025,
-0.117733675692303));
#82695=CARTESIAN_POINT('Ctrl Pts',(-0.0383210922081365,0.234060219319985,
-0.117853342829096));
#82696=CARTESIAN_POINT('Ctrl Pts',(-0.0374883115568983,0.234195044310303,
-0.117910453369518));
#82697=CARTESIAN_POINT('Ctrl Pts',(-0.0354829573920695,0.234508736072031,
-0.118048451574336));
#82698=CARTESIAN_POINT('Ctrl Pts',(-0.0343097379480292,0.234683253114481,
-0.118129574214464));
#82699=CARTESIAN_POINT('Ctrl Pts',(-0.0301829751756676,0.23526550599523,
-0.118416165989855));
#82700=CARTESIAN_POINT('Ctrl Pts',(-0.0272232321177378,0.235626322622069,
-0.118623946951721));
#82701=CARTESIAN_POINT('Ctrl Pts',(-0.0197365438543336,0.236396078507233,
-0.119153890339818));
#82702=CARTESIAN_POINT('Ctrl Pts',(-0.0152032701702621,0.236730844555789,
-0.119478771799242));
#82703=CARTESIAN_POINT('Ctrl Pts',(0.00920816932607272,0.237829501948512,
-0.121240927099465));
#82704=CARTESIAN_POINT('Ctrl Pts',(0.029117201024944,0.236220327226059,
-0.122714309179163));
#82705=CARTESIAN_POINT('Ctrl Pts',(0.0546850039237533,0.230868546420666,
-0.12455747527582));
#82706=CARTESIAN_POINT('Ctrl Pts',(0.0607261396610016,0.229353621366613,
-0.124990094419032));
#82707=CARTESIAN_POINT('Ctrl Pts',(0.0689058507610582,0.226956477003981,
-0.125572115740927));
#82708=CARTESIAN_POINT('Ctrl Pts',(0.0711010985469295,0.226278353260724,
-0.125727952190311));
#82709=CARTESIAN_POINT('Ctrl Pts',(0.0746111610970285,0.225137948932055,
-0.125976616958903));
#82710=CARTESIAN_POINT('Ctrl Pts',(0.0759323120642836,0.224695806675034,
-0.126070095440765));
#82711=CARTESIAN_POINT('Ctrl Pts',(0.0786694219798809,0.223752895107317,
-0.126263549669242));
#82712=CARTESIAN_POINT('Ctrl Pts',(0.0800846776646495,0.223250264509662,
-0.126363459171373));
#82713=CARTESIAN_POINT('Ctrl Pts',(0.0834227956687519,0.222028897449522,
-0.126598885737254));
#82714=CARTESIAN_POINT('Ctrl Pts',(0.0853413098005264,0.221298566237656,
-0.126734012150409));
#82715=CARTESIAN_POINT('Ctrl Pts',(0.0918571664609958,0.218720799321267,
-0.127192565796493));
#82716=CARTESIAN_POINT('Ctrl Pts',(0.0964061735817152,0.216754197831421,
-0.127512024565827));
#82717=CARTESIAN_POINT('Ctrl Pts',(0.107500114491197,0.211539699948246,
-0.128292681016182));
#82718=CARTESIAN_POINT('Ctrl Pts',(0.113963004897077,0.20812920176753,-0.128748775612309));
#82719=CARTESIAN_POINT('Ctrl Pts',(0.132637893181025,0.197143225015587,
-0.130088438292451));
#82720=CARTESIAN_POINT('Ctrl Pts',(0.14432942615202,0.188751799029415,-0.130954950075696));
#82721=CARTESIAN_POINT('Ctrl Pts',(0.160275312239641,0.17495437793864,-0.132275617936893));
#82722=CARTESIAN_POINT('Ctrl Pts',(0.165171099072202,0.170339954697062,
-0.132703770185722));
#82723=CARTESIAN_POINT('Ctrl Pts',(0.17098777834711,0.164370783049533,-0.133251513148062));
#82724=CARTESIAN_POINT('Ctrl Pts',(0.172099999711381,0.163205895766076,
-0.13335813626804));
#82725=CARTESIAN_POINT('Ctrl Pts',(0.173836818389356,0.161349339878685,
-0.133527824433443));
#82726=CARTESIAN_POINT('Ctrl Pts',(0.174469374019223,0.160665137356043,
-0.133590308920945));
#82727=CARTESIAN_POINT('Ctrl Pts',(0.175667159942027,0.159354139858835,
-0.133709979431747));
#82728=CARTESIAN_POINT('Ctrl Pts',(0.176233098705831,0.15872803091911,-0.133767111668537));
#82729=CARTESIAN_POINT('Ctrl Pts',(0.177586372071624,0.157214719786741,
-0.133905130840699));
#82730=CARTESIAN_POINT('Ctrl Pts',(0.178370409101057,0.15632461313397,-0.133986252581333));
#82731=CARTESIAN_POINT('Ctrl Pts',(0.181098680804904,0.15317999643998,-0.134272523215124));
#82732=CARTESIAN_POINT('Ctrl Pts',(0.183007025887036,0.150894897072971,
-0.134479973806765));
#82733=CARTESIAN_POINT('Ctrl Pts',(0.187712012965702,0.145040470726881,
-0.135008779438561));
#82734=CARTESIAN_POINT('Ctrl Pts',(0.190450190727485,0.141425803641111,
-0.135332836228307));
#82735=CARTESIAN_POINT('Ctrl Pts',(0.204538553060434,0.12167614015856,-0.137082022024091));
#82736=CARTESIAN_POINT('Ctrl Pts',(0.213947939084654,0.104247613409395,
-0.138542944563336));
#82737=CARTESIAN_POINT('Ctrl Pts',(0.223395288667307,0.0799191575166064,
-0.140385964958119));
#82738=CARTESIAN_POINT('Ctrl Pts',(0.225460482240546,0.0738925624869005,
-0.140828739120122));
#82739=CARTESIAN_POINT('Ctrl Pts',(0.227943403377497,0.0655679821931603,
-0.141422053878623));
#82740=CARTESIAN_POINT('Ctrl Pts',(0.228573449965457,0.0633366723610477,
-0.14157934297761));
#82741=CARTESIAN_POINT('Ctrl Pts',(0.229530911741545,0.0597452637186364,
-0.141829808941046));
#82742=CARTESIAN_POINT('Ctrl Pts',(0.229879175347535,0.0583909313838091,
-0.141923650985323));
#82743=CARTESIAN_POINT('Ctrl Pts',(0.230576592878991,0.055575812476405,
-0.14211748185522));
#82744=CARTESIAN_POINT('Ctrl Pts',(0.230923890977936,0.0541146271189418,
-0.142217407357086));
#82745=CARTESIAN_POINT('Ctrl Pts',(0.231710764031525,0.0506584182208344,
-0.14245221316225));
#82746=CARTESIAN_POINT('Ctrl Pts',(0.232138494345643,0.0486607991953727,
-0.142586711381885));
#82747=CARTESIAN_POINT('Ctrl Pts',(0.233500400352394,0.0418731283491117,
-0.143039850555427));
#82748=CARTESIAN_POINT('Ctrl Pts',(0.23431257204386,0.0370596773168619,
-0.143354663842213));
#82749=CARTESIAN_POINT('Ctrl Pts',(0.235946557497328,0.0251448581549002,
-0.144121031418296));
#82750=CARTESIAN_POINT('Ctrl Pts',(0.236597039528159,0.0180248174690313,
-0.144567751118608));
#82751=CARTESIAN_POINT('Ctrl Pts',(0.237570878337871,-0.00317030612551152,
-0.145880865478057));
#82752=CARTESIAN_POINT('Ctrl Pts',(0.23696454687095,-0.0172553458568963,
-0.146730525182806));
#82753=CARTESIAN_POINT('Ctrl Pts',(0.234167407682442,-0.0383317056288286,
-0.148058975761636));
#82754=CARTESIAN_POINT('Ctrl Pts',(0.232897686118451,-0.0454130042510966,
-0.148515652040689));
#82755=CARTESIAN_POINT('Ctrl Pts',(0.230946169735583,-0.0540234569482967,
-0.149095638372124));
#82756=CARTESIAN_POINT('Ctrl Pts',(0.230567319856711,-0.0556181432819762,
-0.149204111617994));
#82757=CARTESIAN_POINT('Ctrl Pts',(0.229945489618602,-0.0581199979109375,
-0.14937614491087));
#82758=CARTESIAN_POINT('Ctrl Pts',(0.229713588661616,-0.0590299031092129,
-0.149439099770317));
#82759=CARTESIAN_POINT('Ctrl Pts',(0.229263384083825,-0.0607535277025079,
-0.149559133198301));
#82760=CARTESIAN_POINT('Ctrl Pts',(0.229046139894657,-0.0615674923705631,
-0.149616152561482));
#82761=CARTESIAN_POINT('Ctrl Pts',(0.2285157073984,-0.0635132357561912,
-0.149753238110809));
#82762=CARTESIAN_POINT('Ctrl Pts',(0.22819844397826,-0.0646438679636609,
-0.149833530292068));
#82763=CARTESIAN_POINT('Ctrl Pts',(0.22706846509421,-0.0685587739201833,
-0.150113644419974));
#82764=CARTESIAN_POINT('Ctrl Pts',(0.226213116631161,-0.071330339370902,
-0.150315643008835));
#82765=CARTESIAN_POINT('Ctrl Pts',(0.223941650125932,-0.0782382865753364,
-0.150827255781619));
#82766=CARTESIAN_POINT('Ctrl Pts',(0.222461605151747,-0.0823524250290794,
-0.151139370333243));
#82767=CARTESIAN_POINT('Ctrl Pts',(0.214411683574856,-0.102925367467154,
-0.152730596968696));
#82768=CARTESIAN_POINT('Ctrl Pts',(0.206124467374483,-0.118654114988966,
-0.154041890305366));
#82769=CARTESIAN_POINT('Ctrl Pts',(0.191566349298557,-0.140075608869588,
-0.155888979932513));
#82770=CARTESIAN_POINT('Ctrl Pts',(0.186623159193027,-0.146596949990851,
-0.156461833166066));
#82771=CARTESIAN_POINT('Ctrl Pts',(0.179719788495819,-0.154787582462731,
-0.157195319250065));
#82772=CARTESIAN_POINT('Ctrl Pts',(0.178056210160813,-0.156698388469869,
-0.157367530699892));
#82773=CARTESIAN_POINT('Ctrl Pts',(0.175293853077611,-0.159770457507143,
-0.157646313907743));
#82774=CARTESIAN_POINT('Ctrl Pts',(0.174213424026886,-0.16094787082695,
-0.157753635465204));
#82775=CARTESIAN_POINT('Ctrl Pts',(0.172097823575316,-0.163207111328723,
-0.157960535940788));
#82776=CARTESIAN_POINT('Ctrl Pts',(0.171064148464539,-0.164290229024031,
-0.15806017129055));
#82777=CARTESIAN_POINT('Ctrl Pts',(0.168614193105888,-0.166809176932296,
-0.158292991796427));
#82778=CARTESIAN_POINT('Ctrl Pts',(0.167189704132289,-0.168236889155858,
-0.158425812702684));
#82779=CARTESIAN_POINT('Ctrl Pts',(0.162371625139891,-0.172944229295513,
-0.15886687300084));
#82780=CARTESIAN_POINT('Ctrl Pts',(0.158898266649461,-0.176140843480554,
-0.159171561999456));
#82781=CARTESIAN_POINT('Ctrl Pts',(0.150182941314529,-0.183693996772097,
-0.159907308336116));
#82782=CARTESIAN_POINT('Ctrl Pts',(0.144844125561484,-0.187932407448559,
-0.160334047367573));
#82783=CARTESIAN_POINT('Ctrl Pts',(0.131589775265627,-0.197554020956514,
-0.161349293366636));
#82784=CARTESIAN_POINT('Ctrl Pts',(0.123516850480698,-0.2026994111859,-0.161932412291567));
#82785=CARTESIAN_POINT('Ctrl Pts',(0.114501104060991,-0.207706614298023,
-0.162566348917039));
#82786=CARTESIAN_POINT('Ctrl Pts',(0.113845283084768,-0.20806679688921,
-0.162612370318857));
#82787=CARTESIAN_POINT('Ctrl Pts',(0.103213836423129,-0.213840366633772,
-0.163357087997546));
#82788=CARTESIAN_POINT('Ctrl Pts',(0.092865228265687,-0.218533245999777,
-0.164062655014361));
#82789=CARTESIAN_POINT('Ctrl Pts',(0.080607470294182,-0.223063622081155,
-0.164919701229648));
#82790=CARTESIAN_POINT('Ctrl Pts',(0.0789864511814116,-0.223642759486695,
-0.165033463254584));
#82791=CARTESIAN_POINT('Ctrl Pts',(0.0764457488195572,-0.224519402520991,
-0.165212638335533));
#82792=CARTESIAN_POINT('Ctrl Pts',(0.0755302693831734,-0.224829030476986,
-0.16527737471599));
#82793=CARTESIAN_POINT('Ctrl Pts',(0.0739000429001116,-0.225369315422509,
-0.165393006492608));
#82794=CARTESIAN_POINT('Ctrl Pts',(0.0731860555935161,-0.22560218501491,
-0.165443772311477));
#82795=CARTESIAN_POINT('Ctrl Pts',(0.0714517422664168,-0.226158738451587,
-0.165567376111735));
#82796=CARTESIAN_POINT('Ctrl Pts',(0.070430327076123,-0.226478907114379,
-0.16564041194777));
#82797=CARTESIAN_POINT('Ctrl Pts',(0.0672140418516335,-0.227463209645694,
-0.165871067604539));
#82798=CARTESIAN_POINT('Ctrl Pts',(0.0650117612637484,-0.228102409222718,
-0.166029989598631));
#82799=CARTESIAN_POINT('Ctrl Pts',(0.0530858793934686,-0.231377101078858,
-0.166894636839782));
#82800=CARTESIAN_POINT('Ctrl Pts',(0.0432119074080155,-0.233422717921159,
-0.167624510497337));
#82801=CARTESIAN_POINT('Ctrl Pts',(0.0148055467333385,-0.237443408314525,
-0.169716111386987));
#82802=CARTESIAN_POINT('Ctrl Pts',(-0.00387450207890598,-0.237873493384784,
-0.171075953190418));
#82803=CARTESIAN_POINT('Ctrl Pts',(-0.0259760064417461,-0.235775372336707,
-0.172616887618995));
#82804=CARTESIAN_POINT('Ctrl Pts',(-0.0295295429081284,-0.235356724164988,
-0.172862799016053));
#82805=CARTESIAN_POINT('Ctrl Pts',(-0.0348849999033451,-0.234602574580965,
-0.173230770590165));
#82806=CARTESIAN_POINT('Ctrl Pts',(-0.036694606063742,-0.234326348135469,
-0.173354652287345));
#82807=CARTESIAN_POINT('Ctrl Pts',(-0.0399902925233111,-0.233784164398225,
-0.173579484750334));
#82808=CARTESIAN_POINT('Ctrl Pts',(-0.0414773628497172,-0.233524918525139,
-0.173680640838416));
#82809=CARTESIAN_POINT('Ctrl Pts',(-0.0444835890997039,-0.23297121079324,
-0.173884583261272));
#82810=CARTESIAN_POINT('Ctrl Pts',(-0.0460025416331815,-0.232676043273171,
-0.173987341925818));
#82811=CARTESIAN_POINT('Ctrl Pts',(-0.0497625273489416,-0.231907131444321,
-0.174241059670093));
#82812=CARTESIAN_POINT('Ctrl Pts',(-0.0519998231382932,-0.231415742199298,
-0.174391453281907));
#82813=CARTESIAN_POINT('Ctrl Pts',(-0.0607685582511844,-0.229356225207998,
-0.174979029842838));
#82814=CARTESIAN_POINT('Ctrl Pts',(-0.0672396073726376,-0.227543278559063,
-0.17540843185929));
#82815=CARTESIAN_POINT('Ctrl Pts',(-0.0847875059113642,-0.221812843167166,
-0.17657111944796));
#82816=CARTESIAN_POINT('Ctrl Pts',(-0.0956639400839108,-0.217343716207261,
-0.177289149619266));
#82817=CARTESIAN_POINT('Ctrl Pts',(-0.118000538669546,-0.206162648559552,
-0.178821277424981));
#82818=CARTESIAN_POINT('Ctrl Pts',(-0.129318028224345,-0.199258430833094,
-0.179633441489538));
#82819=CARTESIAN_POINT('Ctrl Pts',(-0.141829310345399,-0.190109357917505,
-0.18064238423881));
#82820=CARTESIAN_POINT('Ctrl Pts',(-0.143640102587277,-0.188744910521885,
-0.180791386041895));
#82821=CARTESIAN_POINT('Ctrl Pts',(-0.14627275780133,-0.186701356468941,
-0.181012892041752));
#82822=CARTESIAN_POINT('Ctrl Pts',(-0.147110107769845,-0.186042286229062,
-0.181084086028159));
#82823=CARTESIAN_POINT('Ctrl Pts',(-0.148557252977984,-0.184887373533538,
-0.181208477415839));
#82824=CARTESIAN_POINT('Ctrl Pts',(-0.149169068496573,-0.184394108573547,
-0.181261494207584));
#82825=CARTESIAN_POINT('Ctrl Pts',(-0.150532094357359,-0.183283970887871,
-0.181380578017171));
#82826=CARTESIAN_POINT('Ctrl Pts',(-0.151281957126289,-0.182665527069756,
-0.181446753165607));
#82827=CARTESIAN_POINT('Ctrl Pts',(-0.153315314723421,-0.18096742228859,
-0.181627959386198));
#82828=CARTESIAN_POINT('Ctrl Pts',(-0.154591164189701,-0.179878751433083,
-0.181743594837502));
#82829=CARTESIAN_POINT('Ctrl Pts',(-0.157528416585325,-0.177318090858562,
-0.182014135621691));
#82830=CARTESIAN_POINT('Ctrl Pts',(-0.159180894756273,-0.175836143431599,
-0.182169630790074));
#82831=CARTESIAN_POINT('Ctrl Pts',(-0.164570582929584,-0.170864414105881,
-0.182687122092148));
#82832=CARTESIAN_POINT('Ctrl Pts',(-0.16821558618414,-0.167277120099077,
-0.183053885108616));
#82833=CARTESIAN_POINT('Ctrl Pts',(-0.178810446120136,-0.15615331099749,
-0.18416513338657));
#82834=CARTESIAN_POINT('Ctrl Pts',(-0.185390717457096,-0.148281196006734,
-0.184917292934201));
#82835=CARTESIAN_POINT('Ctrl Pts',(-0.199681143153089,-0.128741083458007,
-0.186676919771659));
#82836=CARTESIAN_POINT('Ctrl Pts',(-0.206911612059503,-0.116766995786366,
-0.187673666215287));
#82837=CARTESIAN_POINT('Ctrl Pts',(-0.214270990595344,-0.101723520058102,
-0.18882355529731));
#82838=CARTESIAN_POINT('Ctrl Pts',(-0.215450359037064,-0.0992011889059501,
-0.189013213581285));
#82839=CARTESIAN_POINT('Ctrl Pts',(-0.217258097298813,-0.0951505485358067,
-0.189312944690432));
#82840=CARTESIAN_POINT('Ctrl Pts',(-0.217915354369932,-0.0936354969931824,
-0.189423992418324));
#82841=CARTESIAN_POINT('Ctrl Pts',(-0.219132039914642,-0.090748685131472,
-0.189633629024345));
#82842=CARTESIAN_POINT('Ctrl Pts',(-0.219694542086868,-0.0893783145813873,
-0.189732317761885));
#82843=CARTESIAN_POINT('Ctrl Pts',(-0.220949413534856,-0.0862377516615316,
-0.189956659415953));
#82844=CARTESIAN_POINT('Ctrl Pts',(-0.221633421666249,-0.0844643114152518,
-0.190082028081883));
#82845=CARTESIAN_POINT('Ctrl Pts',(-0.223704465682497,-0.0788962255196485,
-0.190471729477082));
#82846=CARTESIAN_POINT('Ctrl Pts',(-0.22501595872422,-0.0750741218466543,
-0.190733579167669));
#82847=CARTESIAN_POINT('Ctrl Pts',(-0.232809958768127,-0.050316666738961,
-0.192398034470159));
#82848=CARTESIAN_POINT('Ctrl Pts',(-0.236461512232343,-0.0286036546426776,
-0.193702262630212));
#82849=CARTESIAN_POINT('Ctrl Pts',(-0.237144870573307,-0.00441616317524204,
-0.195210186855258));
#82850=CARTESIAN_POINT('Ctrl Pts',(-0.237176389888194,-0.00213345270163669,
-0.195353155554687));
#82851=CARTESIAN_POINT('Ctrl Pts',(-0.237174953014705,0.000149289894911542,
-0.195497084908503));
#82852=CARTESIAN_POINT('Origin',(0.,0.,-0.7775));
#82853=CARTESIAN_POINT('',(-0.294199934127337,0.000196874250640231,-1.52858238829104));
#82854=CARTESIAN_POINT('',(0.129149509984275,0.264863564072709,-1.56079685779694));
#82855=CARTESIAN_POINT('Ctrl Pts',(-0.294538311519035,0.00019710068779305,
-1.52858238829104));
#82856=CARTESIAN_POINT('Ctrl Pts',(-0.294613795190814,0.0107826090470038,
-1.52915696469556));
#82857=CARTESIAN_POINT('Ctrl Pts',(-0.289298612898278,0.118649030238792,
-1.53501631456641));
#82858=CARTESIAN_POINT('Ctrl Pts',(-0.161137893181224,0.303346279680123,
-1.54575447106838));
#82859=CARTESIAN_POINT('Ctrl Pts',(0.0481708578874521,0.303785786120914,
-1.55591805116582));
#82860=CARTESIAN_POINT('Ctrl Pts',(0.129149509984275,0.264863564072709,
-1.56079685779694));
#82861=CARTESIAN_POINT('',(-0.128892185405329,0.264462557919714,-1.5608));
#82862=CARTESIAN_POINT('Origin',(0.,0.,-1.5608));
#82863=CARTESIAN_POINT('',(-0.294219088584387,0.0003134260107802,-1.54301761170896));
#82864=CARTESIAN_POINT('Ctrl Pts',(-0.128892185405329,0.264462557919714,
-1.5608));
#82865=CARTESIAN_POINT('Ctrl Pts',(-0.216707535766418,0.221663635799285,
-1.55551522653367));
#82866=CARTESIAN_POINT('Ctrl Pts',(-0.288573197476053,0.121171389152581,
-1.54958776376999));
#82867=CARTESIAN_POINT('Ctrl Pts',(-0.294558913961987,0.012149256643495,
-1.54366030100631));
#82868=CARTESIAN_POINT('Ctrl Pts',(-0.294466535937668,0.000313689611749063,
-1.54301761170896));
#82869=CARTESIAN_POINT('',(-0.29419997848679,0.000112509433066526,-1.44301761171429));
#82870=CARTESIAN_POINT('Ctrl Pts',(-0.294199833067583,0.000313405498243621,
-1.54301761170896));
#82871=CARTESIAN_POINT('Ctrl Pts',(-0.294217023327698,-0.0158234258104146,
-1.54214055457276));
#82872=CARTESIAN_POINT('Ctrl Pts',(-0.292902300314846,-0.0320212444901405,
-1.54126349743655));
#82873=CARTESIAN_POINT('Ctrl Pts',(-0.290252026430234,-0.0480354156133036,
-1.54038644030035));
#82874=CARTESIAN_POINT('Ctrl Pts',(-0.287606426933038,-0.0640213419424432,
-1.5395109300627));
#82875=CARTESIAN_POINT('Ctrl Pts',(-0.283630014961905,-0.0798234427950474,
-1.53863541982506));
#82876=CARTESIAN_POINT('Ctrl Pts',(-0.278370984510483,-0.0952010240631088,
-1.53775990958741));
#82877=CARTESIAN_POINT('Ctrl Pts',(-0.273111814349831,-0.110579013845637,
-1.53688437609132));
#82878=CARTESIAN_POINT('Ctrl Pts',(-0.266570184910628,-0.125531664434472,
-1.53600884259523));
#82879=CARTESIAN_POINT('Ctrl Pts',(-0.258844231073643,-0.139833129264471,
-1.53513330909914));
#82880=CARTESIAN_POINT('Ctrl Pts',(-0.251117939135543,-0.154135219951332,
-1.53425773728819));
#82881=CARTESIAN_POINT('Ctrl Pts',(-0.242207642809512,-0.167785355035112,
-1.53338216547723));
#82882=CARTESIAN_POINT('Ctrl Pts',(-0.232256525314706,-0.180583904179579,
-1.53250659366628));
#82883=CARTESIAN_POINT('Ctrl Pts',(-0.22228391538919,-0.193410095639677,
-1.5316291307947));
#82884=CARTESIAN_POINT('Ctrl Pts',(-0.211266563528022,-0.205380423780031,
-1.53075166792313));
#82885=CARTESIAN_POINT('Ctrl Pts',(-0.199386261618759,-0.216330207501624,
-1.52987420505155));
#82886=CARTESIAN_POINT('Ctrl Pts',(-0.195853179539396,-0.219586562848073,
-1.52961325643504));
#82887=CARTESIAN_POINT('Ctrl Pts',(-0.192243996622234,-0.222752935046479,
-1.52935230781854));
#82888=CARTESIAN_POINT('Ctrl Pts',(-0.188564008153101,-0.225825717820706,
-1.52909135920203));
#82889=CARTESIAN_POINT('Ctrl Pts',(-0.175876360259589,-0.236419877617578,
-1.52819167590349));
#82890=CARTESIAN_POINT('Ctrl Pts',(-0.162253493509079,-0.245974552757455,
-1.52729199260495));
#82891=CARTESIAN_POINT('Ctrl Pts',(-0.147890921192098,-0.254326395462509,
-1.5263923093064));
#82892=CARTESIAN_POINT('Ctrl Pts',(-0.133556120734875,-0.262662088817767,
-1.52549436565991));
#82893=CARTESIAN_POINT('Ctrl Pts',(-0.118485095219775,-0.269799118991503,
-1.52459642201342));
#82894=CARTESIAN_POINT('Ctrl Pts',(-0.102903127863606,-0.275616738018369,
-1.52369847836693));
#82895=CARTESIAN_POINT('Ctrl Pts',(-0.0873242018146189,-0.281433221555337,
-1.52280070998216));
#82896=CARTESIAN_POINT('Ctrl Pts',(-0.0712352500269611,-0.285930481905613,
-1.52190294159739));
#82897=CARTESIAN_POINT('Ctrl Pts',(-0.0548822808447564,-0.289035595125025,
-1.52100517321262));
#82898=CARTESIAN_POINT('Ctrl Pts',(-0.0385337861512818,-0.292139858725389,
-1.52010765047465));
#82899=CARTESIAN_POINT('Ctrl Pts',(-0.0219221940289531,-0.293852594565548,
-1.51921012773668));
#82900=CARTESIAN_POINT('Ctrl Pts',(-0.00530292333947626,-0.294152203806219,
-1.51831260499871));
#82901=CARTESIAN_POINT('Ctrl Pts',(0.0113551230825498,-0.294452512088865,
-1.51741298817958));
#82902=CARTESIAN_POINT('Ctrl Pts',(0.0280200919670017,-0.293333120120612,
-1.51651337136045));
#82903=CARTESIAN_POINT('Ctrl Pts',(0.0444369333245589,-0.290824687667173,
-1.51561375454132));
#82904=CARTESIAN_POINT('Ctrl Pts',(0.0588942609324966,-0.288615661644938,
-1.51482151596189));
#82905=CARTESIAN_POINT('Ctrl Pts',(0.0731588662054835,-0.285330278632224,
-1.51402927738247));
#82906=CARTESIAN_POINT('Ctrl Pts',(0.0870651703785879,-0.281021878342145,
-1.51323703880304));
#82907=CARTESIAN_POINT('Ctrl Pts',(0.102861402450364,-0.276127947503798,
-1.51233713151631));
#82908=CARTESIAN_POINT('Ctrl Pts',(0.118291944426169,-0.269883086688625,
-1.51143722422959));
#82909=CARTESIAN_POINT('Ctrl Pts',(0.133113420325067,-0.262363216418312,
-1.51053731694286));
#82910=CARTESIAN_POINT('Ctrl Pts',(0.147907029704503,-0.254857484592285,
-1.50963910161205));
#82911=CARTESIAN_POINT('Ctrl Pts',(0.162093122993974,-0.246081798862244,
-1.50874088628125));
#82912=CARTESIAN_POINT('Ctrl Pts',(0.175448032739809,-0.236160174050857,
-1.50784267095044));
#82913=CARTESIAN_POINT('Ctrl Pts',(0.188801379043309,-0.226239710751495,
-1.50694456077257));
#82914=CARTESIAN_POINT('Ctrl Pts',(0.201323074164483,-0.215174002594547,
-1.50604645059469));
#82915=CARTESIAN_POINT('Ctrl Pts',(0.212818425931049,-0.203130395520293,
-1.50514834041681));
#82916=CARTESIAN_POINT('Ctrl Pts',(0.224311133852135,-0.191089558386165,
-1.50425043679761));
#82917=CARTESIAN_POINT('Ctrl Pts',(0.234777431857193,-0.178071847420231,
-1.5033525331784));
#82918=CARTESIAN_POINT('Ctrl Pts',(0.244060688518756,-0.164280310201043,
-1.50245462955919));
#82919=CARTESIAN_POINT('Ctrl Pts',(0.253366195528285,-0.150455717071274,
-1.50155457382152));
#82920=CARTESIAN_POINT('Ctrl Pts',(0.261482578973351,-0.135854264949523,
-1.50065451808386));
#82921=CARTESIAN_POINT('Ctrl Pts',(0.268297333756601,-0.120707003521333,
-1.4997544623462));
#82922=CARTESIAN_POINT('Ctrl Pts',(0.274283205037668,-0.107402114342831,
-1.49896388103215));
#82923=CARTESIAN_POINT('Ctrl Pts',(0.279265420715235,-0.0936768370847798,
-1.49817329971811));
#82924=CARTESIAN_POINT('Ctrl Pts',(0.283199357402271,-0.0796979545969695,
-1.49738271840406));
#82925=CARTESIAN_POINT('Ctrl Pts',(0.287663489115224,-0.0638350728095948,
-1.49648558675288));
#82926=CARTESIAN_POINT('Ctrl Pts',(0.290805227469212,-0.0475442036619822,
-1.49558845510169));
#82927=CARTESIAN_POINT('Ctrl Pts',(0.292554872675635,-0.0310690597498993,
-1.49469132345051));
#82928=CARTESIAN_POINT('Ctrl Pts',(0.294301078016627,-0.014626306563552,
-1.49379595559243));
#82929=CARTESIAN_POINT('Ctrl Pts',(0.294660472434726,0.00199922976480145,
-1.49290058773435));
#82930=CARTESIAN_POINT('Ctrl Pts',(0.293614361666323,0.0185538843177906,
-1.49200521987627));
#82931=CARTESIAN_POINT('Ctrl Pts',(0.292568453553665,0.0351053318529641,
-1.49111002547157));
#82932=CARTESIAN_POINT('Ctrl Pts',(0.290117576849656,0.0515851321130972,
-1.49021483106686));
#82933=CARTESIAN_POINT('Ctrl Pts',(0.28629515761753,0.0677401116381822,
-1.48931963666216));
#82934=CARTESIAN_POINT('Ctrl Pts',(0.282473802126637,0.0838905953932358,
-1.48842469138114));
#82935=CARTESIAN_POINT('Ctrl Pts',(0.27728185476015,0.099715667866776,-1.48752974610013));
#82936=CARTESIAN_POINT('Ctrl Pts',(0.270803446863671,0.114974489199799,
-1.48663480081912));
#82937=CARTESIAN_POINT('Ctrl Pts',(0.264309524078873,0.130269853293429,
-1.4857377122683));
#82938=CARTESIAN_POINT('Ctrl Pts',(0.256523323413169,0.144995534646025,
-1.48484062371747));
#82939=CARTESIAN_POINT('Ctrl Pts',(0.247576534598606,0.158932374034195,
-1.48394353516664));
#82940=CARTESIAN_POINT('Ctrl Pts',(0.239547701724778,0.1714392696988,-1.48313848944612));
#82941=CARTESIAN_POINT('Ctrl Pts',(0.230585110038212,0.183310912449293,
-1.4823334437256));
#82942=CARTESIAN_POINT('Ctrl Pts',(0.220811679822929,0.194411527574309,
-1.48152839800507));
#82943=CARTESIAN_POINT('Ctrl Pts',(0.209902410249452,0.206802223590211,
-1.48062979223507));
#82944=CARTESIAN_POINT('Ctrl Pts',(0.197912414603261,0.218311041742577,
-1.47973118646507));
#82945=CARTESIAN_POINT('Ctrl Pts',(0.185009421737734,0.228746921002818,
-1.47883258069506));
#82946=CARTESIAN_POINT('Ctrl Pts',(0.172131383146893,0.23916261736438,-1.47793571282072));
#82947=CARTESIAN_POINT('Ctrl Pts',(0.158344418734345,0.248508951470909,
-1.47703884494637));
#82948=CARTESIAN_POINT('Ctrl Pts',(0.143852220535281,0.256632380355771,
-1.47614197707202));
#82949=CARTESIAN_POINT('Ctrl Pts',(0.129362538240474,0.264754398980502,
-1.47524526489756));
#82950=CARTESIAN_POINT('Ctrl Pts',(0.114168527049344,0.271653502815025,
-1.47434855272311));
#82951=CARTESIAN_POINT('Ctrl Pts',(0.0985016927601044,0.277220231086034,
-1.47345184054865));
#82952=CARTESIAN_POINT('Ctrl Pts',(0.0828389927852362,0.282785490355439,
-1.4725553650072));
#82953=CARTESIAN_POINT('Ctrl Pts',(0.0667044661733018,0.287018817653418,
-1.47165888946574));
#82954=CARTESIAN_POINT('Ctrl Pts',(0.0503467484441305,0.289860043678158,
-1.47076241392429));
#82955=CARTESIAN_POINT('Ctrl Pts',(0.0339501292217874,0.292708026631745,
-1.46986380640833));
#82956=CARTESIAN_POINT('Ctrl Pts',(0.0173300454633171,0.294157186473883,
-1.46896519889237));
#82957=CARTESIAN_POINT('Ctrl Pts',(0.000742728730556185,0.294199062462872,
-1.46806659137641));
#82958=CARTESIAN_POINT('Ctrl Pts',(-0.0139783380277216,0.294236226956648,
-1.4672690867863));
#82959=CARTESIAN_POINT('Ctrl Pts',(-0.0286731558972058,0.293165762192075,
-1.4664715821962));
#82960=CARTESIAN_POINT('Ctrl Pts',(-0.0431663430276392,0.291015990676836,
-1.46567407760609));
#82961=CARTESIAN_POINT('Ctrl Pts',(-0.0594954107105255,0.288593903370631,
-1.46477555153918));
#82962=CARTESIAN_POINT('Ctrl Pts',(-0.0756716406703319,0.284785528261025,
-1.46387702547228));
#82963=CARTESIAN_POINT('Ctrl Pts',(-0.0914435276617728,0.279627826313424,
-1.46297849940537));
#82964=CARTESIAN_POINT('Ctrl Pts',(-0.107184988715157,0.274480074216469,
-1.46208170670737));
#82965=CARTESIAN_POINT('Ctrl Pts',(-0.122522891907933,0.267988343099318,
-1.46118491400936));
#82966=CARTESIAN_POINT('Ctrl Pts',(-0.137217684288146,0.260240171992333,
-1.46028812131136));
#82967=CARTESIAN_POINT('Ctrl Pts',(-0.151910059462569,0.252493275413328,
-1.45939147613041));
#82968=CARTESIAN_POINT('Ctrl Pts',(-0.165958812148944,0.243490670498873,
-1.45849483094946));
#82969=CARTESIAN_POINT('Ctrl Pts',(-0.179146280018388,0.233367200685044,
-1.45759818576851));
#82970=CARTESIAN_POINT('Ctrl Pts',(-0.192330331990485,0.223246353113332,
-1.45670177284199));
#82971=CARTESIAN_POINT('Ctrl Pts',(-0.204652921497238,0.212005707492377,
-1.45580535991548));
#82972=CARTESIAN_POINT('Ctrl Pts',(-0.215928460295286,0.199821270225437,
-1.45490894698896));
#82973=CARTESIAN_POINT('Ctrl Pts',(-0.227230926056984,0.187607735466548,
-1.45401039335071));
#82974=CARTESIAN_POINT('Ctrl Pts',(-0.237480827513171,0.174446508563989,
-1.45311183971245));
#82975=CARTESIAN_POINT('Ctrl Pts',(-0.246531858943066,0.16054806920694,
-1.4522132860742));
#82976=CARTESIAN_POINT('Ctrl Pts',(-0.254568442804848,0.148207379164488,
-1.4514154431185));
#82977=CARTESIAN_POINT('Ctrl Pts',(-0.261660267585032,0.135286274905178,
-1.4506176001628));
#82978=CARTESIAN_POINT('Ctrl Pts',(-0.267735737189512,0.12194759133164,
-1.4498197572071));
#82979=CARTESIAN_POINT('Ctrl Pts',(-0.275189887420251,0.105582016699494,
-1.44884086312327));
#82980=CARTESIAN_POINT('Ctrl Pts',(-0.281154975269878,0.0884973724728511,
-1.44786196903944));
#82981=CARTESIAN_POINT('Ctrl Pts',(-0.285512149944728,0.0709679662519578,
-1.44688307495561));
#82982=CARTESIAN_POINT('Ctrl Pts',(-0.289842117365214,0.0535480178906884,
-1.44591029332362));
#82983=CARTESIAN_POINT('Ctrl Pts',(-0.292583943111203,0.0356893481811567,
-1.44493751169162));
#82984=CARTESIAN_POINT('Ctrl Pts',(-0.29366817978795,0.0176816339751797,
-1.44396473005963));
#82985=CARTESIAN_POINT('Ctrl Pts',(-0.294020057473362,0.0118374184729343,
-1.44364902394452));
#82986=CARTESIAN_POINT('Ctrl Pts',(-0.294197735516373,0.00597763407621125,
-1.4433333178294));
#82987=CARTESIAN_POINT('Ctrl Pts',(-0.29419997848679,0.000112509433066627,
-1.44301761171429));
#82988=CARTESIAN_POINT('',(-0.294199881040649,-0.000264566943933203,-1.34301761170622));
#82989=CARTESIAN_POINT('Ctrl Pts',(-0.294199978486827,0.000112509333972839,
-1.44301761170896));
#82990=CARTESIAN_POINT('Ctrl Pts',(-0.294206483659082,-0.0168978263402081,
-1.44210198462188));
#82991=CARTESIAN_POINT('Ctrl Pts',(-0.292733371950329,-0.0338987372162774,
-1.44118635753479));
#82992=CARTESIAN_POINT('Ctrl Pts',(-0.289811541802209,-0.050625193710509,
-1.44027073044771));
#82993=CARTESIAN_POINT('Ctrl Pts',(-0.286887052022081,-0.0673668756685116,
-1.43935426989975));
#82994=CARTESIAN_POINT('Ctrl Pts',(-0.282511400153008,-0.0838328853838791,
-1.4384378093518));
#82995=CARTESIAN_POINT('Ctrl Pts',(-0.276766242696575,-0.0997701704098992,
-1.43752134880384));
#82996=CARTESIAN_POINT('Ctrl Pts',(-0.27100445262236,-0.115753594949471,
-1.43660223504087));
#82997=CARTESIAN_POINT('Ctrl Pts',(-0.263865555093411,-0.131204564891129,
-1.4356831212779));
#82998=CARTESIAN_POINT('Ctrl Pts',(-0.255478857719724,-0.145891032137774,
-1.43476400751493));
#82999=CARTESIAN_POINT('Ctrl Pts',(-0.253049934293915,-0.150144470976485,
-1.43449781727933));
#83000=CARTESIAN_POINT('Ctrl Pts',(-0.250516628906551,-0.154333967966321,
-1.43423162704372));
#83001=CARTESIAN_POINT('Ctrl Pts',(-0.247882742893601,-0.158454364962109,
-1.43396543680811));
#83002=CARTESIAN_POINT('Ctrl Pts',(-0.238993368333329,-0.172360719319312,
-1.43306704382643));
#83003=CARTESIAN_POINT('Ctrl Pts',(-0.22890188787328,-0.185560863680223,
-1.43216865084475));
#83004=CARTESIAN_POINT('Ctrl Pts',(-0.21774480709357,-0.197840438191447,
-1.43127025786306));
#83005=CARTESIAN_POINT('Ctrl Pts',(-0.206609320701942,-0.210096245742237,
-1.43037360370958));
#83006=CARTESIAN_POINT('Ctrl Pts',(-0.194412805089058,-0.221434397337263,
-1.4294769495561));
#83007=CARTESIAN_POINT('Ctrl Pts',(-0.181333039984309,-0.231672114442047,
-1.42858029540262));
#83008=CARTESIAN_POINT('Ctrl Pts',(-0.168255519859482,-0.2419080743693,
-1.42768379514873));
#83009=CARTESIAN_POINT('Ctrl Pts',(-0.154295639738224,-0.251043447384909,
-1.42678729489485));
#83010=CARTESIAN_POINT('Ctrl Pts',(-0.139665399961993,-0.258934771812239,
-1.42589079464096));
#83011=CARTESIAN_POINT('Ctrl Pts',(-0.125039011724739,-0.266824018779181,
-1.42499453039863));
#83012=CARTESIAN_POINT('Ctrl Pts',(-0.109743315736894,-0.273469501436223,
-1.4240982661563));
#83013=CARTESIAN_POINT('Ctrl Pts',(-0.0940147633797387,-0.278773858650075,
-1.42320200191398));
#83014=CARTESIAN_POINT('Ctrl Pts',(-0.0782486995485523,-0.284090866377042,
-1.42230360014544));
#83015=CARTESIAN_POINT('Ctrl Pts',(-0.0620484787177007,-0.288060131993999,
-1.42140519837691));
#83016=CARTESIAN_POINT('Ctrl Pts',(-0.0456659476067264,-0.290634239602253,
-1.42050679660837));
#83017=CARTESIAN_POINT('Ctrl Pts',(-0.0311040493667709,-0.292922280003103,
-1.41970823654196));
#83018=CARTESIAN_POINT('Ctrl Pts',(-0.0163986702893981,-0.294108744107576,
-1.41890967647555));
#83019=CARTESIAN_POINT('Ctrl Pts',(-0.00172821287218314,-0.294194923953947,
-1.41811111640913));
#83020=CARTESIAN_POINT('Ctrl Pts',(0.0147757332526237,-0.294291874410302,
-1.41721275366974));
#83021=CARTESIAN_POINT('Ctrl Pts',(0.0313402951844906,-0.292996035529911,
-1.41631439093035));
#83022=CARTESIAN_POINT('Ctrl Pts',(0.047711361023731,-0.290305470202101,
-1.41541602819095));
#83023=CARTESIAN_POINT('Ctrl Pts',(0.0640507438107881,-0.287620111946484,
-1.41451940406001));
#83024=CARTESIAN_POINT('Ctrl Pts',(0.0801965916035031,-0.283545447123526,
-1.41362277992908));
#83025=CARTESIAN_POINT('Ctrl Pts',(0.0958988663854379,-0.278131349232674,
-1.41272615579814));
#83026=CARTESIAN_POINT('Ctrl Pts',(0.111598459935975,-0.272718175822477,
-1.41182968476966));
#83027=CARTESIAN_POINT('Ctrl Pts',(0.126853868205815,-0.265966230750605,
-1.41093321374117));
#83028=CARTESIAN_POINT('Ctrl Pts',(0.141429454492969,-0.257975482171894,
-1.41003674271269));
#83029=CARTESIAN_POINT('Ctrl Pts',(0.156001209790034,-0.249986833850284,
-1.40914050730914));
#83030=CARTESIAN_POINT('Ctrl Pts',(0.169892809329383,-0.240760418453787,
-1.4082442719056));
#83031=CARTESIAN_POINT('Ctrl Pts',(0.182894023142827,-0.230441785053473,
-1.40734803650205));
#83032=CARTESIAN_POINT('Ctrl Pts',(0.195926263307315,-0.220098527064504,
-1.4064496623048));
#83033=CARTESIAN_POINT('Ctrl Pts',(0.208063268358004,-0.20865836005635,
-1.40555128810755));
#83034=CARTESIAN_POINT('Ctrl Pts',(0.219128364473481,-0.196306902281039,
-1.4046529139103));
#83035=CARTESIAN_POINT('Ctrl Pts',(0.228965866838071,-0.185325750937871,
-1.40385420794358));
#83036=CARTESIAN_POINT('Ctrl Pts',(0.237956405352934,-0.173625154600472,
-1.40305550197687));
#83037=CARTESIAN_POINT('Ctrl Pts',(0.24600404911102,-0.161355656303034,
-1.40225679601015));
#83038=CARTESIAN_POINT('Ctrl Pts',(0.25505536946571,-0.147555945105597,
-1.40135847796933));
#83039=CARTESIAN_POINT('Ctrl Pts',(0.26297071114369,-0.132948365572465,
-1.40046015992852));
#83040=CARTESIAN_POINT('Ctrl Pts',(0.269610320154723,-0.117745128417561,
-1.3995618418877));
#83041=CARTESIAN_POINT('Ctrl Pts',(0.276237069189704,-0.102571337765516,
-1.39866526376085));
#83042=CARTESIAN_POINT('Ctrl Pts',(0.28159261699149,-0.086804869870417,
-1.39776868563401));
#83043=CARTESIAN_POINT('Ctrl Pts',(0.285582909949582,-0.0706826820708495,
-1.39687210750716));
#83044=CARTESIAN_POINT('Ctrl Pts',(0.289572515582222,-0.0545632713079921,
-1.39597568381534));
#83045=CARTESIAN_POINT('Ctrl Pts',(0.292197092671192,-0.0380890151960811,
-1.39507926012351));
#83046=CARTESIAN_POINT('Ctrl Pts',(0.293412462568779,-0.0215120154640292,
-1.39418283643168));
#83047=CARTESIAN_POINT('Ctrl Pts',(0.294627511901832,-0.00493938806193824,
-1.39328664917952));
#83048=CARTESIAN_POINT('Ctrl Pts',(0.294434045039363,0.0117351391589708,
-1.39239046192735));
#83049=CARTESIAN_POINT('Ctrl Pts',(0.292839952512838,0.0282560119669929,
-1.39149427467518));
#83050=CARTESIAN_POINT('Ctrl Pts',(0.291242056236625,0.0448163061158407,
-1.39059594898254));
#83051=CARTESIAN_POINT('Ctrl Pts',(0.288236962203357,0.0612214253628249,
-1.3896976232899));
#83052=CARTESIAN_POINT('Ctrl Pts',(0.283884433831552,0.0772222003580513,
-1.38879929759725));
#83053=CARTESIAN_POINT('Ctrl Pts',(0.280013441465023,0.0914527515627984,
-1.38800035693522));
#83054=CARTESIAN_POINT('Ctrl Pts',(0.275077547695713,0.10536325850791,-1.38720141627319));
#83055=CARTESIAN_POINT('Ctrl Pts',(0.269151047893426,0.118791217764071,
-1.38640247561116));
#83056=CARTESIAN_POINT('Ctrl Pts',(0.262487121855226,0.133889999559775,
-1.38550412385915));
#83057=CARTESIAN_POINT('Ctrl Pts',(0.254527548677776,0.148474275772685,
-1.38460577210714));
#83058=CARTESIAN_POINT('Ctrl Pts',(0.245374517644184,0.162311386202213,
-1.38370742035513));
#83059=CARTESIAN_POINT('Ctrl Pts',(0.236239207109633,0.176121707636796,
-1.38281080783477));
#83060=CARTESIAN_POINT('Ctrl Pts',(0.225915401710059,0.189187046186855,
-1.38191419531442));
#83061=CARTESIAN_POINT('Ctrl Pts',(0.214550900598436,0.201299654874021,
-1.38101758279407));
#83062=CARTESIAN_POINT('Ctrl Pts',(0.203188350100266,0.21341018454186,-1.38012112416912));
#83063=CARTESIAN_POINT('Ctrl Pts',(0.190785959733452,0.224567697913147,
-1.37922466554417));
#83064=CARTESIAN_POINT('Ctrl Pts',(0.177531347443001,0.234598083272376,
-1.37832820691922));
#83065=CARTESIAN_POINT('Ctrl Pts',(0.164280225750256,0.24462582713298,-1.37743198437634));
#83066=CARTESIAN_POINT('Ctrl Pts',(0.150177965276877,0.253526563565899,
-1.37653576183347));
#83067=CARTESIAN_POINT('Ctrl Pts',(0.135443381568157,0.26116801180348,-1.3756395392906));
#83068=CARTESIAN_POINT('Ctrl Pts',(0.120673642665631,0.268827691746758,
-1.37474117845337));
#83069=CARTESIAN_POINT('Ctrl Pts',(0.105269284870452,0.275221740729953,
-1.37384281761614));
#83070=CARTESIAN_POINT('Ctrl Pts',(0.089471957604124,0.280264890420627,
-1.37294445677891));
#83071=CARTESIAN_POINT('Ctrl Pts',(0.0754259460574661,0.284748948868774,
-1.37214568959));
#83072=CARTESIAN_POINT('Ctrl Pts',(0.0610699287857648,0.288165653089362,
-1.37134692240109));
#83073=CARTESIAN_POINT('Ctrl Pts',(0.046580566216322,0.290489054614743,
-1.37054815521218));
#83074=CARTESIAN_POINT('Ctrl Pts',(0.0302848996917963,0.293102100998165,
-1.36964981039689));
#83075=CARTESIAN_POINT('Ctrl Pts',(0.0137168745443692,0.294347968966909,
-1.36875146558159));
#83076=CARTESIAN_POINT('Ctrl Pts',(-0.00287267759169578,0.294185974722545,
-1.3678531207663));
#83077=CARTESIAN_POINT('Ctrl Pts',(-0.0194301111209985,0.294024294111087,
-1.36695651521338));
#83078=CARTESIAN_POINT('Ctrl Pts',(-0.0360082063535757,0.292460103685732,
-1.36605990966046));
#83079=CARTESIAN_POINT('Ctrl Pts',(-0.0523522525572313,0.289504545132169,
-1.36516330410754));
#83080=CARTESIAN_POINT('Ctrl Pts',(-0.0686934944870301,0.286549493686544,
-1.36426685239214));
#83081=CARTESIAN_POINT('Ctrl Pts',(-0.0847999817327795,0.282203636625161,
-1.36337040067673));
#83082=CARTESIAN_POINT('Ctrl Pts',(-0.100423593422299,0.276529820967202,
-1.36247394896133));
#83083=CARTESIAN_POINT('Ctrl Pts',(-0.116043090950082,0.270857499393694,
-1.36157773330834));
#83084=CARTESIAN_POINT('Ctrl Pts',(-0.131179225375831,0.263858193884227,
-1.36068151765534));
#83085=CARTESIAN_POINT('Ctrl Pts',(-0.145602031196717,0.255643674890247,
-1.35978530200234));
#83086=CARTESIAN_POINT('Ctrl Pts',(-0.160059251500703,0.247409555103702,
-1.35888694787513));
#83087=CARTESIAN_POINT('Ctrl Pts',(-0.173799066667942,0.237954846934015,
-1.35798859374791));
#83088=CARTESIAN_POINT('Ctrl Pts',(-0.186618561891959,0.227436040146185,
-1.35709023962069));
#83089=CARTESIAN_POINT('Ctrl Pts',(-0.19801744460195,0.218082891466906,
-1.35629143801819));
#83090=CARTESIAN_POINT('Ctrl Pts',(-0.208688840866842,0.207889311073367,
-1.35549263641569));
#83091=CARTESIAN_POINT('Ctrl Pts',(-0.218514934030968,0.196989501256899,
-1.35469383481319));
#83092=CARTESIAN_POINT('Ctrl Pts',(-0.22945360436519,0.184855540760436,
-1.35380458745453));
#83093=CARTESIAN_POINT('Ctrl Pts',(-0.239416908998826,0.171764825371417,
-1.35291534009586));
#83094=CARTESIAN_POINT('Ctrl Pts',(-0.248235545782208,0.157901088692287,
-1.3520260927372));
#83095=CARTESIAN_POINT('Ctrl Pts',(-0.257037908143505,0.144062936954223,
-1.35113848644701));
#83096=CARTESIAN_POINT('Ctrl Pts',(-0.264699303159667,0.129455229767417,
-1.35025088015683));
#83097=CARTESIAN_POINT('Ctrl Pts',(-0.271091546655065,0.11429354020313,
-1.34936327386664));
#83098=CARTESIAN_POINT('Ctrl Pts',(-0.277477009665882,0.0991479331930178,
-1.34847660909265));
#83099=CARTESIAN_POINT('Ctrl Pts',(-0.28259565539752,0.0834502416635364,
-1.34758994431865));
#83100=CARTESIAN_POINT('Ctrl Pts',(-0.286366446301408,0.067438108163728,
-1.34670327954466));
#83101=CARTESIAN_POINT('Ctrl Pts',(-0.290139385992626,0.051416850140588,
-1.34581610950425));
#83102=CARTESIAN_POINT('Ctrl Pts',(-0.292562755010656,0.0350815797868516,
-1.34492893946383));
#83103=CARTESIAN_POINT('Ctrl Pts',(-0.293606252845568,0.0186817635672989,
-1.34404176942342));
#83104=CARTESIAN_POINT('Ctrl Pts',(-0.294007794192005,0.0123710611721357,
-1.3437003835186));
#83105=CARTESIAN_POINT('Ctrl Pts',(-0.294205560350854,0.00605085811264825,
-1.34335899761378));
#83106=CARTESIAN_POINT('Ctrl Pts',(-0.294199881040695,-0.000264566893242766,
-1.34301761170896));
#83107=CARTESIAN_POINT('',(-0.29419998971568,7.7790063860881E-5,-1.24301761170439));
#83108=CARTESIAN_POINT('Ctrl Pts',(-0.294199881040649,-0.000264566943932752,
-1.34301761170622));
#83109=CARTESIAN_POINT('Ctrl Pts',(-0.294180940205162,-0.0213268790539207,
-1.34187906972835));
#83110=CARTESIAN_POINT('Ctrl Pts',(-0.291896264550366,-0.0422876901627163,
-1.34074052775048));
#83111=CARTESIAN_POINT('Ctrl Pts',(-0.287433256096504,-0.0627356620253717,
-1.33960198577262));
#83112=CARTESIAN_POINT('Ctrl Pts',(-0.286436977175878,-0.0673002698559217,
-1.33934782865315));
#83113=CARTESIAN_POINT('Ctrl Pts',(-0.285332333255084,-0.0718394125108084,
-1.33909367153368));
#83114=CARTESIAN_POINT('Ctrl Pts',(-0.2841206116624,-0.0763486609482029,
-1.33883951441421));
#83115=CARTESIAN_POINT('Ctrl Pts',(-0.279837657272212,-0.0922870625645441,
-1.33794116997833));
#83116=CARTESIAN_POINT('Ctrl Pts',(-0.2741957617379,-0.107914611675097,
-1.33704282554245));
#83117=CARTESIAN_POINT('Ctrl Pts',(-0.267260427871627,-0.122985786552246,
-1.33614448110656));
#83118=CARTESIAN_POINT('Ctrl Pts',(-0.260338521832277,-0.138027781417061,
-1.3352478759977));
#83119=CARTESIAN_POINT('Ctrl Pts',(-0.252128415570261,-0.152514802477171,
-1.33435127088884));
#83120=CARTESIAN_POINT('Ctrl Pts',(-0.242744488248793,-0.166218992371003,
-1.33345466577998));
#83121=CARTESIAN_POINT('Ctrl Pts',(-0.233362171982384,-0.179920829496778,
-1.33255821460243));
#83122=CARTESIAN_POINT('Ctrl Pts',(-0.222806836889673,-0.192839421876937,
-1.33166176342487));
#83123=CARTESIAN_POINT('Ctrl Pts',(-0.211237345551264,-0.204774080011255,
-1.33076531224732));
#83124=CARTESIAN_POINT('Ctrl Pts',(-0.199670901482741,-0.216705594694987,
-1.32986909718461));
#83125=CARTESIAN_POINT('Ctrl Pts',(-0.187091390110108,-0.227653129150242,
-1.32897288212191));
#83126=CARTESIAN_POINT('Ctrl Pts',(-0.173694887112703,-0.237452576719869,
-1.3280766670592));
#83127=CARTESIAN_POINT('Ctrl Pts',(-0.160266419626245,-0.247275406088062,
-1.32717831359839));
#83128=CARTESIAN_POINT('Ctrl Pts',(-0.146017724105643,-0.255944229945598,
-1.32627996013759));
#83129=CARTESIAN_POINT('Ctrl Pts',(-0.131174613722805,-0.263337921148233,
-1.32538160667678));
#83130=CARTESIAN_POINT('Ctrl Pts',(-0.117976312901667,-0.269912295262152,
-1.32458280245626));
#83131=CARTESIAN_POINT('Ctrl Pts',(-0.104308786152013,-0.27547899508879,
-1.32378399823574));
#83132=CARTESIAN_POINT('Ctrl Pts',(-0.0903426948984102,-0.279985423689328,
-1.32298519401522));
#83133=CARTESIAN_POINT('Ctrl Pts',(-0.0746362911582433,-0.285053397665801,
-1.32208685092344));
#83134=CARTESIAN_POINT('Ctrl Pts',(-0.0584521846111506,-0.288811738808585,
-1.32118850783167));
#83135=CARTESIAN_POINT('Ctrl Pts',(-0.0420320653633554,-0.291181980007848,
-1.32029016473989));
#83136=CARTESIAN_POINT('Ctrl Pts',(-0.0256437381718955,-0.293547632029614,
-1.31939356098835));
#83137=CARTESIAN_POINT('Ctrl Pts',(-0.00902106987274824,-0.294530342122439,
-1.31849695723682));
#83138=CARTESIAN_POINT('Ctrl Pts',(0.00758251067853928,-0.294102270531545,
-1.31760035348528));
#83139=CARTESIAN_POINT('Ctrl Pts',(0.0241832406835549,-0.293674272433104,
-1.31670390366503));
#83140=CARTESIAN_POINT('Ctrl Pts',(0.0407640997441511,-0.291835941239725,
-1.31580745384478));
#83141=CARTESIAN_POINT('Ctrl Pts',(0.0570702851055986,-0.288611542662392,
-1.31491100402452));
#83142=CARTESIAN_POINT('Ctrl Pts',(0.0733721755573099,-0.285387993364062,
-1.31401479032149));
#83143=CARTESIAN_POINT('Ctrl Pts',(0.0893987618351136,-0.280779265739622,
-1.31311857661845));
#83144=CARTESIAN_POINT('Ctrl Pts',(0.104905721807555,-0.274860745709597,
-1.31222236291541));
#83145=CARTESIAN_POINT('Ctrl Pts',(0.120449682375012,-0.268928103713493,
-1.31132401078935));
#83146=CARTESIAN_POINT('Ctrl Pts',(0.135470807684591,-0.261679735676709,
-1.31042565866328));
#83147=CARTESIAN_POINT('Ctrl Pts',(0.149744688774196,-0.253239349596225,
-1.30952730653722));
#83148=CARTESIAN_POINT('Ctrl Pts',(0.162436964464623,-0.24573419340257,
-1.30872849556356));
#83149=CARTESIAN_POINT('Ctrl Pts',(0.174538440607036,-0.237287454248982,
-1.3079296845899));
#83150=CARTESIAN_POINT('Ctrl Pts',(0.185912204337808,-0.22801379843829,
-1.30713087361624));
#83151=CARTESIAN_POINT('Ctrl Pts',(0.198703134631412,-0.217584648699535,
-1.30623253110415));
#83152=CARTESIAN_POINT('Ctrl Pts',(0.210654423871686,-0.206042693857774,
-1.30533418859206));
#83153=CARTESIAN_POINT('Ctrl Pts',(0.221568841233891,-0.193548155750116,
-1.30443584607996));
#83154=CARTESIAN_POINT('Ctrl Pts',(0.23246212621466,-0.181077809437253,
-1.30353924292931));
#83155=CARTESIAN_POINT('Ctrl Pts',(0.242321960369317,-0.167659086567259,
-1.30264263977865));
#83156=CARTESIAN_POINT('Ctrl Pts',(0.250987228407161,-0.153489580025784,
-1.30174603662799));
#83157=CARTESIAN_POINT('Ctrl Pts',(0.259651008537639,-0.139322506520779,
-1.30084958743245));
#83158=CARTESIAN_POINT('Ctrl Pts',(0.267120173459694,-0.124405550612861,
-1.29995313823692));
#83159=CARTESIAN_POINT('Ctrl Pts',(0.273276597785878,-0.108965779502444,
-1.29905668904139));
#83160=CARTESIAN_POINT('Ctrl Pts',(0.279431400464002,-0.093530075342835,
-1.29816047597725));
#83161=CARTESIAN_POINT('Ctrl Pts',(0.284273866166556,-0.0775725684430892,
-1.29726426291312));
#83162=CARTESIAN_POINT('Ctrl Pts',(0.2877344757355,-0.0613393142545369,
-1.29636804984899));
#83163=CARTESIAN_POINT('Ctrl Pts',(0.291203342505222,-0.0450673266473652,
-1.29546969837222));
#83164=CARTESIAN_POINT('Ctrl Pts',(0.293283628383432,-0.0285190601876433,
-1.29457134689546));
#83165=CARTESIAN_POINT('Ctrl Pts',(0.293957198634491,-0.0119501201233388,
-1.2936729954187));
#83166=CARTESIAN_POINT('Ctrl Pts',(0.294556137252256,0.00278298016478098,
-1.29287418135155));
#83167=CARTESIAN_POINT('Ctrl Pts',(0.294043594649531,0.0175319521840072,
-1.2920753672844));
#83168=CARTESIAN_POINT('Ctrl Pts',(0.292441404009112,0.0321195457810242,
-1.29127655321725));
#83169=CARTESIAN_POINT('Ctrl Pts',(0.290639586612288,0.0485246971143476,
-1.29037821000721));
#83170=CARTESIAN_POINT('Ctrl Pts',(0.287447319294331,0.0648299086200134,
-1.28947986679716));
#83171=CARTESIAN_POINT('Ctrl Pts',(0.28289188937104,0.0807825409855569,
-1.28858152358712));
#83172=CARTESIAN_POINT('Ctrl Pts',(0.278345279537461,0.0967042863325372,
-1.28768491972283));
#83173=CARTESIAN_POINT('Ctrl Pts',(0.272440897570094,0.112274037639596,
-1.28678831585854));
#83174=CARTESIAN_POINT('Ctrl Pts',(0.265257029552737,0.127249158240274,
-1.28589171199425));
#83175=CARTESIAN_POINT('Ctrl Pts',(0.258074394962931,0.142221707701522,
-1.28499526207153));
#83176=CARTESIAN_POINT('Ctrl Pts',(0.24961300411642,0.156599095364782,-1.28409881214881));
#83177=CARTESIAN_POINT('Ctrl Pts',(0.239999249875403,0.170158749581806,
-1.28320236222609));
#83178=CARTESIAN_POINT('Ctrl Pts',(0.230388027873357,0.183714832219614,
-1.28230614842605));
#83179=CARTESIAN_POINT('Ctrl Pts',(0.219625511684055,0.1964529698853,-1.28140993462602));
#83180=CARTESIAN_POINT('Ctrl Pts',(0.20788045172467,0.208181069722362,-1.28051372082598));
#83181=CARTESIAN_POINT('Ctrl Pts',(0.196107367454748,0.219937153402248,
-1.27961536861422));
#83182=CARTESIAN_POINT('Ctrl Pts',(0.18334763810206,0.230677843492465,-1.27871701640246));
#83183=CARTESIAN_POINT('Ctrl Pts',(0.169805959154214,0.240248988001443,
-1.27781866419071));
#83184=CARTESIAN_POINT('Ctrl Pts',(0.157764763491979,0.248759603574887,
-1.27701985373323));
#83185=CARTESIAN_POINT('Ctrl Pts',(0.14510612512367,0.256345890152774,-1.27622104327575));
#83186=CARTESIAN_POINT('Ctrl Pts',(0.131990690368428,0.262929834092797,
-1.27542223281827));
#83187=CARTESIAN_POINT('Ctrl Pts',(0.117241060436347,0.270334143474923,
-1.27452388984653));
#83188=CARTESIAN_POINT('Ctrl Pts',(0.101819564026194,0.276517006092301,
-1.27362554687479));
#83189=CARTESIAN_POINT('Ctrl Pts',(0.0859530949446297,0.281364008838088,
-1.27272720390305));
#83190=CARTESIAN_POINT('Ctrl Pts',(0.0701173461179693,0.286201626940126,
-1.27183060028018));
#83191=CARTESIAN_POINT('Ctrl Pts',(0.0538390633948679,0.289708227895976,
-1.27093399665731));
#83192=CARTESIAN_POINT('Ctrl Pts',(0.0373644639970419,0.291817643109894,
-1.27003739303444));
#83193=CARTESIAN_POINT('Ctrl Pts',(0.0208926932127655,0.293926696146845,
-1.26914094335432));
#83194=CARTESIAN_POINT('Ctrl Pts',(0.00422544821317553,0.294638887359161,
-1.2682444936742));
#83195=CARTESIAN_POINT('Ctrl Pts',(-0.0123817484947549,0.293939334394383,
-1.26734804399409));
#83196=CARTESIAN_POINT('Ctrl Pts',(-0.0289845708872543,0.293239965691005,
-1.26645183043772));
#83197=CARTESIAN_POINT('Ctrl Pts',(-0.045526586286276,0.291129635322151,
-1.26555561688136));
#83198=CARTESIAN_POINT('Ctrl Pts',(-0.06175483299394,0.287645581578947,
-1.264659403325));
#83199=CARTESIAN_POINT('Ctrl Pts',(-0.0780218011952776,0.284153214690928,
-1.26376105135355));
#83200=CARTESIAN_POINT('Ctrl Pts',(-0.0939727343393061,0.279280770795784,
-1.26286269938211));
#83201=CARTESIAN_POINT('Ctrl Pts',(-0.109366980510989,0.2731162821472,-1.26196434741066));
#83202=CARTESIAN_POINT('Ctrl Pts',(-0.123055494354213,0.267634838803923,
-1.26116553574687));
#83203=CARTESIAN_POINT('Ctrl Pts',(-0.136303736560469,0.261132715282318,
-1.26036672408307));
#83204=CARTESIAN_POINT('Ctrl Pts',(-0.148958906168924,0.253702353700075,
-1.25956791241928));
#83205=CARTESIAN_POINT('Ctrl Pts',(-0.163190899122558,0.245346175398775,
-1.25866956950314));
#83206=CARTESIAN_POINT('Ctrl Pts',(-0.17676280583108,0.235762144364244,
-1.25777122658699));
#83207=CARTESIAN_POINT('Ctrl Pts',(-0.189455265116077,0.22507852523019,
-1.25687288367085));
#83208=CARTESIAN_POINT('Ctrl Pts',(-0.202123149546261,0.214415591479732,
-1.25597628010609));
#83209=CARTESIAN_POINT('Ctrl Pts',(-0.213914325929049,0.202657748893602,
-1.25507967654134));
#83210=CARTESIAN_POINT('Ctrl Pts',(-0.2246394260358,0.189975704421135,-1.25418307297659));
#83211=CARTESIAN_POINT('Ctrl Pts',(-0.235362684655307,0.177295837440989,
-1.25328662335763));
#83212=CARTESIAN_POINT('Ctrl Pts',(-0.245019680993877,0.16369265179071,
-1.25239017373867));
#83213=CARTESIAN_POINT('Ctrl Pts',(-0.253459038149679,0.149372540917799,
-1.25149372411971));
#83214=CARTESIAN_POINT('Ctrl Pts',(-0.261896172372185,0.135056201973327,
-1.25059751062628));
#83215=CARTESIAN_POINT('Ctrl Pts',(-0.269115911868186,0.12002399997494,
-1.24970129713285));
#83216=CARTESIAN_POINT('Ctrl Pts',(-0.275012021059745,0.104508508135148,
-1.24880508363943));
#83217=CARTESIAN_POINT('Ctrl Pts',(-0.280922198683778,0.0889559955004315,
-1.24790673173258));
#83218=CARTESIAN_POINT('Ctrl Pts',(-0.285502181001382,0.0729186419795194,
-1.24700837982573));
#83219=CARTESIAN_POINT('Ctrl Pts',(-0.288695059045791,0.0566462962826991,
-1.24611002791888));
#83220=CARTESIAN_POINT('Ctrl Pts',(-0.291534157142027,0.0421769726672756,
-1.24531121595269));
#83221=CARTESIAN_POINT('Ctrl Pts',(-0.29327720565083,0.0275224345870245,
-1.24451240398649));
#83222=CARTESIAN_POINT('Ctrl Pts',(-0.293918747058194,0.0128611868714064,
-1.2437135920203));
#83223=CARTESIAN_POINT('Ctrl Pts',(-0.294105065494125,0.00860322205134901,
-1.24348159858318));
#83224=CARTESIAN_POINT('Ctrl Pts',(-0.294198862422386,0.00434117925284497,
-1.24324960514607));
#83225=CARTESIAN_POINT('Ctrl Pts',(-0.294199989715657,7.77901478423249E-5,
-1.24301761170896));
#83226=CARTESIAN_POINT('',(-0.294199926066577,0.000208572338548644,-1.14301761549734));
#83227=CARTESIAN_POINT('Ctrl Pts',(-0.29419998971568,7.7790063860881E-5,
-1.24301761170439));
#83228=CARTESIAN_POINT('Ctrl Pts',(-0.294204324649468,-0.0163168162983833,
-1.24212549489629));
#83229=CARTESIAN_POINT('Ctrl Pts',(-0.292833941317543,-0.0327664949589083,
-1.24123337808819));
#83230=CARTESIAN_POINT('Ctrl Pts',(-0.290087364073985,-0.049020008206928,
-1.2403412612801));
#83231=CARTESIAN_POINT('Ctrl Pts',(-0.287345972973171,-0.0652428312422471,
-1.23945082898501));
#83232=CARTESIAN_POINT('Ctrl Pts',(-0.283233611214606,-0.0812694299995112,
-1.23856039668993));
#83233=CARTESIAN_POINT('Ctrl Pts',(-0.277800605409854,-0.0968527936299139,
-1.23766996439484));
#83234=CARTESIAN_POINT('Ctrl Pts',(-0.272368270947906,-0.112434231663436,
-1.23677964212823));
#83235=CARTESIAN_POINT('Ctrl Pts',(-0.265615832979466,-0.127571770699677,
-1.23588931986161));
#83236=CARTESIAN_POINT('Ctrl Pts',(-0.257643608018651,-0.142033134328338,
-1.234998997595));
#83237=CARTESIAN_POINT('Ctrl Pts',(-0.249672686289359,-0.156492133936285,
-1.23410882087069));
#83238=CARTESIAN_POINT('Ctrl Pts',(-0.240482776121732,-0.170274482609805,
-1.23321864414639));
#83239=CARTESIAN_POINT('Ctrl Pts',(-0.230219515778441,-0.183173727796156,
-1.23232846742209));
#83240=CARTESIAN_POINT('Ctrl Pts',(-0.21993289399697,-0.196102334502035,
-1.23143626445974));
#83241=CARTESIAN_POINT('Ctrl Pts',(-0.208568576975701,-0.208143220205496,
-1.2305440614974));
#83242=CARTESIAN_POINT('Ctrl Pts',(-0.196311668216858,-0.219124094799988,
-1.22965185853506));
#83243=CARTESIAN_POINT('Ctrl Pts',(-0.188102932771615,-0.226478240635376,
-1.22905432956381));
#83244=CARTESIAN_POINT('Ctrl Pts',(-0.179494641423396,-0.233357703304351,
-1.22845680059256));
#83245=CARTESIAN_POINT('Ctrl Pts',(-0.170549960397698,-0.239721402899999,
-1.22785927162131));
#83246=CARTESIAN_POINT('Ctrl Pts',(-0.157102258724431,-0.249288779696857,
-1.22696092864817));
#83247=CARTESIAN_POINT('Ctrl Pts',(-0.14280424939101,-0.257751478428811,
-1.22606258567502));
#83248=CARTESIAN_POINT('Ctrl Pts',(-0.12786272044659,-0.264961817475645,
-1.22516424270188));
#83249=CARTESIAN_POINT('Ctrl Pts',(-0.112950120925454,-0.272158196040184,
-1.22426763907845));
#83250=CARTESIAN_POINT('Ctrl Pts',(-0.0973971506760092,-0.278106629008214,
-1.22337103545502));
#83251=CARTESIAN_POINT('Ctrl Pts',(-0.0814370536116031,-0.282704167459662,
-1.22247443183159));
#83252=CARTESIAN_POINT('Ctrl Pts',(-0.0654796968465792,-0.287300916527955,
-1.22157798215223));
#83253=CARTESIAN_POINT('Ctrl Pts',(-0.0491160952757681,-0.290546962713943,
-1.22068153247288));
#83254=CARTESIAN_POINT('Ctrl Pts',(-0.0325965117074827,-0.292388623965612,
-1.21978508279352));
#83255=CARTESIAN_POINT('Ctrl Pts',(-0.0160812793908451,-0.29422980012445,
-1.21888886923865));
#83256=CARTESIAN_POINT('Ctrl Pts',(0.000589065745059934,-0.294667248985264,
-1.21799265568378));
#83257=CARTESIAN_POINT('Ctrl Pts',(0.0171588419832219,-0.293699189889579,
-1.21709644212891));
#83258=CARTESIAN_POINT('Ctrl Pts',(0.0337681546013056,-0.292728820952672,
-1.21619809016015));
#83259=CARTESIAN_POINT('Ctrl Pts',(0.0502756275678593,-0.29034631909139,
-1.21529973819139));
#83260=CARTESIAN_POINT('Ctrl Pts',(0.0664299975163362,-0.286601980854947,
-1.21440138622263));
#83261=CARTESIAN_POINT('Ctrl Pts',(0.0807944110567974,-0.28327252739838,
-1.21360257455587));
#83262=CARTESIAN_POINT('Ctrl Pts',(0.0948793846356908,-0.278867183381866,
-1.2128037628891));
#83263=CARTESIAN_POINT('Ctrl Pts',(0.108519805313765,-0.273454003179077,
-1.21200495122233));
#83264=CARTESIAN_POINT('Ctrl Pts',(0.123859811631003,-0.267366344999985,
-1.21110660825303));
#83265=CARTESIAN_POINT('Ctrl Pts',(0.138734734387574,-0.259964520171745,
-1.21020826528372));
#83266=CARTESIAN_POINT('Ctrl Pts',(0.152908215344758,-0.25134183432147,
-1.20930992231442));
#83267=CARTESIAN_POINT('Ctrl Pts',(0.167054253949881,-0.242735843507617,
-1.20841331869511));
#83268=CARTESIAN_POINT('Ctrl Pts',(0.180500844368606,-0.232914034008152,
-1.2075167150758));
#83269=CARTESIAN_POINT('Ctrl Pts',(0.193034796828567,-0.222016231869099,
-1.20662011145649));
#83270=CARTESIAN_POINT('Ctrl Pts',(0.205566597242393,-0.211120300853545,
-1.20572366178162));
#83271=CARTESIAN_POINT('Ctrl Pts',(0.217185441152932,-0.199149221706712,
-1.20482721210676));
#83272=CARTESIAN_POINT('Ctrl Pts',(0.22771024248155,-0.186283884082853,
-1.20393076243189));
#83273=CARTESIAN_POINT('Ctrl Pts',(0.238232271579244,-0.173421935186789,
-1.20303454888172));
#83274=CARTESIAN_POINT('Ctrl Pts',(0.247660337680816,-0.159666814838694,
-1.20213833533156));
#83275=CARTESIAN_POINT('Ctrl Pts',(0.255853974761835,-0.145232171362169,
-1.20124212178139));
#83276=CARTESIAN_POINT('Ctrl Pts',(0.264067162300656,-0.130763086051645,
-1.20034376981759));
#83277=CARTESIAN_POINT('Ctrl Pts',(0.271039669204752,-0.115611943382271,
-1.19944541785379));
#83278=CARTESIAN_POINT('Ctrl Pts',(0.276677143951878,-0.10001698863009,
-1.19854706589));
#83279=CARTESIAN_POINT('Ctrl Pts',(0.281689968440806,-0.0861500048133908,
-1.19774825420111));
#83280=CARTESIAN_POINT('Ctrl Pts',(0.285647818470339,-0.0719327978885206,
-1.19694944251223));
#83281=CARTESIAN_POINT('Ctrl Pts',(0.288518073790726,-0.0575409514701437,
-1.19615063082334));
#83282=CARTESIAN_POINT('Ctrl Pts',(0.291745960613989,-0.0413558925709045,
-1.19525228784092));
#83283=CARTESIAN_POINT('Ctrl Pts',(0.293617963536819,-0.0248469267792773,
-1.1943539448585));
#83284=CARTESIAN_POINT('Ctrl Pts',(0.29408393377337,-0.00826316503406248,
-1.19345560187609));
#83285=CARTESIAN_POINT('Ctrl Pts',(0.294549001809768,0.00828848763804503,
-1.19255899824334));
#83286=CARTESIAN_POINT('Ctrl Pts',(0.293613353229563,0.024913869004309,
-1.19166239461059));
#83287=CARTESIAN_POINT('Ctrl Pts',(0.291278480747702,0.04135803009466,-1.19076579097784));
#83288=CARTESIAN_POINT('Ctrl Pts',(0.288944009156409,0.0577993677721069,
-1.18986934128923));
#83289=CARTESIAN_POINT('Ctrl Pts',(0.285210849393363,0.0740587587732578,
-1.18897289160062));
#83290=CARTESIAN_POINT('Ctrl Pts',(0.280132411880159,0.0898858821740374,
-1.18807644191201));
#83291=CARTESIAN_POINT('Ctrl Pts',(0.275055312025453,0.105708836716569,
-1.18718022834791));
#83292=CARTESIAN_POINT('Ctrl Pts',(0.268633890113283,0.121098999628384,
-1.18628401478381));
#83293=CARTESIAN_POINT('Ctrl Pts',(0.260971132125323,0.135822340567474,
-1.1853878012197));
#83294=CARTESIAN_POINT('Ctrl Pts',(0.253290090385631,0.15058081218808,-1.18448944924195));
#83295=CARTESIAN_POINT('Ctrl Pts',(0.244362187410983,0.164668591742709,
-1.18359109726419));
#83296=CARTESIAN_POINT('Ctrl Pts',(0.234336120307431,0.177876987604527,
-1.18269274528643));
#83297=CARTESIAN_POINT('Ctrl Pts',(0.225420974450966,0.189621849714649,
-1.18189393366574));
#83298=CARTESIAN_POINT('Ctrl Pts',(0.215638442611246,0.200671536696332,
-1.18109512204505));
#83299=CARTESIAN_POINT('Ctrl Pts',(0.205118177365467,0.210903232109584,
-1.18029631042436));
#83300=CARTESIAN_POINT('Ctrl Pts',(0.193287094611401,0.222409789436847,
-1.17939796744835));
#83301=CARTESIAN_POINT('Ctrl Pts',(0.180447161138358,0.232954288037526,
-1.17849962447234));
#83302=CARTESIAN_POINT('Ctrl Pts',(0.166780220179905,0.242359233693999,
-1.17760128149633));
#83303=CARTESIAN_POINT('Ctrl Pts',(0.153139740819474,0.25174596972389,-1.1767046778701));
#83304=CARTESIAN_POINT('Ctrl Pts',(0.138676039276032,0.259997034964698,
-1.17580807424387));
#83305=CARTESIAN_POINT('Ctrl Pts',(0.123603927998681,0.266975109295411,
-1.17491147061763));
#83306=CARTESIAN_POINT('Ctrl Pts',(0.108534404558633,0.273951985511228,
-1.17401502093561));
#83307=CARTESIAN_POINT('Ctrl Pts',(0.0928573723032582,0.27965592568008,
-1.1731185712536));
#83308=CARTESIAN_POINT('Ctrl Pts',(0.0768119779240554,0.283995704276305,
-1.17222212157158));
#83309=CARTESIAN_POINT('Ctrl Pts',(0.0607708098965294,0.288334339776255,
-1.17132590801411));
#83310=CARTESIAN_POINT('Ctrl Pts',(0.044362239060206,0.291309331073124,
-1.17042969445665));
#83311=CARTESIAN_POINT('Ctrl Pts',(0.0278386839225503,0.292879920236025,
-1.16953348089918));
#83312=CARTESIAN_POINT('Ctrl Pts',(0.0112757026943745,0.294454256909071,
-1.16863512892801));
#83313=CARTESIAN_POINT('Ctrl Pts',(-0.0054020174295768,0.294617450173523,
-1.16773677695684));
#83314=CARTESIAN_POINT('Ctrl Pts',(-0.0219384814675519,0.293380883887989,
-1.16683842498566));
#83315=CARTESIAN_POINT('Ctrl Pts',(-0.0366426515522562,0.292281333165311,
-1.16603961333223));
#83316=CARTESIAN_POINT('Ctrl Pts',(-0.0512347525468744,0.290075858562765,
-1.1652408016788));
#83317=CARTESIAN_POINT('Ctrl Pts',(-0.0655412233709042,0.28680653416379,
-1.16444199002537));
#83318=CARTESIAN_POINT('Ctrl Pts',(-0.0816302695457364,0.283129854438748,
-1.16354364704931));
#83319=CARTESIAN_POINT('Ctrl Pts',(-0.0974601184399902,0.278083447173002,
-1.16264530407324));
#83320=CARTESIAN_POINT('Ctrl Pts',(-0.112782945798443,0.271723475498576,
-1.16174696109718));
#83321=CARTESIAN_POINT('Ctrl Pts',(-0.128076105471513,0.265375817846509,
-1.16085035747092));
#83322=CARTESIAN_POINT('Ctrl Pts',(-0.142863444807933,0.257719883201405,
-1.15995375384466));
#83323=CARTESIAN_POINT('Ctrl Pts',(-0.156912941363351,0.248861344593132,
-1.1590571502184));
#83324=CARTESIAN_POINT('Ctrl Pts',(-0.17096002566075,0.240004326970377,
-1.1581607005364));
#83325=CARTESIAN_POINT('Ctrl Pts',(-0.184268823550014,0.229945491424742,
-1.1572642508544));
#83326=CARTESIAN_POINT('Ctrl Pts',(-0.196632777383233,0.218835990775182,
-1.1563678011724));
#83327=CARTESIAN_POINT('Ctrl Pts',(-0.208993474554697,0.207729416364784,
-1.15547158761497));
#83328=CARTESIAN_POINT('Ctrl Pts',(-0.220409240524934,0.195573263295305,
-1.15457537405755));
#83329=CARTESIAN_POINT('Ctrl Pts',(-0.230708665875729,0.18255725537442,
-1.15367916050012));
#83330=CARTESIAN_POINT('Ctrl Pts',(-0.241032666208446,0.169510190559731,
-1.15278080852903));
#83331=CARTESIAN_POINT('Ctrl Pts',(-0.250234533990658,0.155599812781374,
-1.15188245655793));
#83332=CARTESIAN_POINT('Ctrl Pts',(-0.25818468306756,0.141047188661468,
-1.15098410458684));
#83333=CARTESIAN_POINT('Ctrl Pts',(-0.26525392979255,0.128107042583133,
-1.15018529293336));
#83334=CARTESIAN_POINT('Ctrl Pts',(-0.271333964041315,0.114659860226817,
-1.14938648127987));
#83335=CARTESIAN_POINT('Ctrl Pts',(-0.276365766182724,0.100874195323859,
-1.14858766962639));
#83336=CARTESIAN_POINT('Ctrl Pts',(-0.282866466672747,0.0830641789377884,
-1.14755566654652));
#83337=CARTESIAN_POINT('Ctrl Pts',(-0.287651798522018,0.0645963176383724,
-1.14652366346665));
#83338=CARTESIAN_POINT('Ctrl Pts',(-0.290615313155387,0.0457862398499426,
-1.14549166038678));
#83339=CARTESIAN_POINT('Ctrl Pts',(-0.292983480581905,0.030754961445827,
-1.14466697875697));
#83340=CARTESIAN_POINT('Ctrl Pts',(-0.294189081238035,0.015505652370611,
-1.14384229712716));
#83341=CARTESIAN_POINT('Ctrl Pts',(-0.294199926066577,0.000208572338548644,
-1.14301761549734));
#83342=CARTESIAN_POINT('',(-0.293910006811105,-0.000218120950975208,-1.04301761170896));
#83343=CARTESIAN_POINT('Ctrl Pts',(-0.293887912717633,0.000208280940901665,
-1.14301761170896));
#83344=CARTESIAN_POINT('Ctrl Pts',(-0.29347111625565,-0.0633124552653269,
-1.13958952421511));
#83345=CARTESIAN_POINT('Ctrl Pts',(-0.242085158539587,-0.225371926112401,
-1.13087666325494));
#83346=CARTESIAN_POINT('Ctrl Pts',(0.0248432358882371,-0.346674479333956,
-1.11687902882842));
#83347=CARTESIAN_POINT('Ctrl Pts',(0.3044975180128,-0.167575781385358,-1.10102470842943));
#83348=CARTESIAN_POINT('Ctrl Pts',(0.306165446002828,0.164508664378986,
-1.08517038803045));
#83349=CARTESIAN_POINT('Ctrl Pts',(0.0283243105090556,0.346407439901074,
-1.06931606763146));
#83350=CARTESIAN_POINT('Ctrl Pts',(-0.240829917627408,0.227340704164944,
-1.05526514219097));
#83351=CARTESIAN_POINT('Ctrl Pts',(-0.29346455100378,0.0642778682396108,
-1.0464989902168));
#83352=CARTESIAN_POINT('Ctrl Pts',(-0.293910006811105,-0.000218120950975208,
-1.04301761170896));
#83353=CARTESIAN_POINT('',(-0.294664342707076,-6.04394989484003E-5,-0.943017611708961));
#83354=CARTESIAN_POINT('Ctrl Pts',(-0.293910006811105,-0.000218120950975208,
-1.04301761170896));
#83355=CARTESIAN_POINT('Ctrl Pts',(-0.294140758151515,-0.0336278009059762,
-1.04121421675047));
#83356=CARTESIAN_POINT('Ctrl Pts',(-0.273471204903555,-0.164666211870492,
-1.03412604832565));
#83357=CARTESIAN_POINT('Ctrl Pts',(-0.0808290374716516,-0.338034092489328,
-1.02175310643452));
#83358=CARTESIAN_POINT('Ctrl Pts',(0.23980855062429,-0.251579490481548,
-1.00589878603552));
#83359=CARTESIAN_POINT('Ctrl Pts',(0.341516588451039,0.0645507613917535,
-0.990044465636539));
#83360=CARTESIAN_POINT('Ctrl Pts',(0.131442277715391,0.321750382459031,
-0.97419014523755));
#83361=CARTESIAN_POINT('Ctrl Pts',(-0.194909829171702,0.28562474370573,
-0.958514527261694));
#83362=CARTESIAN_POINT('Ctrl Pts',(-0.294400112794844,0.0939112419462086,
-0.948123682752163));
#83363=CARTESIAN_POINT('Ctrl Pts',(-0.294664342707076,-6.04394989484003E-5,
-0.943017611708961));
#83364=CARTESIAN_POINT('',(-0.294199883530078,0.00026178404932804,-0.843017611708961));
#83365=CARTESIAN_POINT('Ctrl Pts',(-0.294664342707076,-6.04394989484003E-5,
-0.943017611708961));
#83366=CARTESIAN_POINT('Ctrl Pts',(-0.294673590233242,-0.00334926314386741,
-0.942838909285835));
#83367=CARTESIAN_POINT('Ctrl Pts',(-0.293135403529261,-0.103889734782347,
-0.93737543339637));
#83368=CARTESIAN_POINT('Ctrl Pts',(-0.178979626789081,-0.297937366199709,
-0.926627184040607));
#83369=CARTESIAN_POINT('Ctrl Pts',(0.152803789238326,-0.312172040672919,
-0.910772863641607));
#83370=CARTESIAN_POINT('Ctrl Pts',(0.345087321836773,-0.0414140228791957,
-0.894918543242629));
#83371=CARTESIAN_POINT('Ctrl Pts',(0.222328659415099,0.267152293993907,
-0.879064222843639));
#83372=CARTESIAN_POINT('Ctrl Pts',(-0.103401553816396,0.331826008100429,
-0.863209902444658));
#83373=CARTESIAN_POINT('Ctrl Pts',(-0.278720695596675,0.151254505853962,
-0.851194384871808));
#83374=CARTESIAN_POINT('Ctrl Pts',(-0.294314128361141,0.027011048903306,
-0.844463640765287));
#83375=CARTESIAN_POINT('Ctrl Pts',(-0.294082633309355,0.000262760320685067,
-0.843017670125095));
#83376=CARTESIAN_POINT('',(-0.294199973461913,-0.000124960031393308,-0.743017611706046));
#83377=CARTESIAN_POINT('Ctrl Pts',(-0.294199883530078,0.00026178404932804,
-0.843017611708961));
#83378=CARTESIAN_POINT('Ctrl Pts',(-0.294214504485591,-0.0161696349771595,
-0.842129701439759));
#83379=CARTESIAN_POINT('Ctrl Pts',(-0.292848235671175,-0.0326311939379088,
-0.841241791170558));
#83380=CARTESIAN_POINT('Ctrl Pts',(-0.290112361285408,-0.0488718510945222,
-0.840353880901356));
#83381=CARTESIAN_POINT('Ctrl Pts',(-0.287376021304854,-0.0651152721080342,
-0.83946581952639));
#83382=CARTESIAN_POINT('Ctrl Pts',(-0.283269711147539,-0.0811369162079659,
-0.838577758151423));
#83383=CARTESIAN_POINT('Ctrl Pts',(-0.277856351568672,-0.0966927499502755,
-0.837689696776457));
#83384=CARTESIAN_POINT('Ctrl Pts',(-0.27244232273868,-0.112250506853071,
-0.836801525610876));
#83385=CARTESIAN_POINT('Ctrl Pts',(-0.26572121935906,-0.127341588578431,
-0.835913354445295));
#83386=CARTESIAN_POINT('Ctrl Pts',(-0.257804613108441,-0.141740683856143,
-0.835025183279714));
#83387=CARTESIAN_POINT('Ctrl Pts',(-0.249870591876541,-0.15617145431976,
-0.834135058311741));
#83388=CARTESIAN_POINT('Ctrl Pts',(-0.240736264007773,-0.169906526785005,
-0.833244933343769));
#83389=CARTESIAN_POINT('Ctrl Pts',(-0.230557071075997,-0.182748671614481,
-0.832354808375797));
#83390=CARTESIAN_POINT('Ctrl Pts',(-0.227303439228586,-0.186853477534391,
-0.832070292799426));
#83391=CARTESIAN_POINT('Ctrl Pts',(-0.22394335567284,-0.190867321422932,
-0.831785777223056));
#83392=CARTESIAN_POINT('Ctrl Pts',(-0.220482689971872,-0.194784556427781,
-0.831501261646685));
#83393=CARTESIAN_POINT('Ctrl Pts',(-0.20955581992897,-0.207153020048383,
-0.830602918669694));
#83394=CARTESIAN_POINT('Ctrl Pts',(-0.19755022185266,-0.218638487290109,
-0.829704575692702));
#83395=CARTESIAN_POINT('Ctrl Pts',(-0.184633792939896,-0.229050218302947,
-0.82880623271571));
#83396=CARTESIAN_POINT('Ctrl Pts',(-0.171742372501976,-0.239441790375967,
-0.827909629088495));
#83397=CARTESIAN_POINT('Ctrl Pts',(-0.157944189321307,-0.248763210945512,
-0.827013025461279));
#83398=CARTESIAN_POINT('Ctrl Pts',(-0.143443054015968,-0.256861305483275,
-0.826116421834064));
#83399=CARTESIAN_POINT('Ctrl Pts',(-0.128944408513228,-0.264958009601846,
-0.825219972151074));
#83400=CARTESIAN_POINT('Ctrl Pts',(-0.113743713373344,-0.27183137425185,
-0.824323522468084));
#83401=CARTESIAN_POINT('Ctrl Pts',(-0.0980725302068118,-0.27737234688922,
-0.823427072785094));
#83402=CARTESIAN_POINT('Ctrl Pts',(-0.0824054748249273,-0.282911860036165,
-0.822530859226665));
#83403=CARTESIAN_POINT('Ctrl Pts',(-0.0662689271156775,-0.287119424498268,
-0.821634645668236));
#83404=CARTESIAN_POINT('Ctrl Pts',(-0.0499114997054081,-0.289935306917176,
-0.820738432109806));
#83405=CARTESIAN_POINT('Ctrl Pts',(-0.0335150425948892,-0.292757908182758,
-0.819840080137697));
#83406=CARTESIAN_POINT('Ctrl Pts',(-0.0168974405960642,-0.294182086879795,
-0.818941728165588));
#83407=CARTESIAN_POINT('Ctrl Pts',(-0.000314816413647557,-0.294199831561178,
-0.818043376193478));
#83408=CARTESIAN_POINT('Ctrl Pts',(0.0144303990168213,-0.294215610074088,
-0.817244564544886));
#83409=CARTESIAN_POINT('Ctrl Pts',(0.02914751516652,-0.293120156158774,
-0.816445752896294));
#83410=CARTESIAN_POINT('Ctrl Pts',(0.0436602857802432,-0.290942295731624,
-0.815646941247702));
#83411=CARTESIAN_POINT('Ctrl Pts',(0.0599813366568894,-0.288493075539295,
-0.81474859827071));
#83412=CARTESIAN_POINT('Ctrl Pts',(0.0761475348421451,-0.284658446591712,
-0.813850255293718));
#83413=CARTESIAN_POINT('Ctrl Pts',(0.0919075179817019,-0.27947566645138,
-0.812951912316726));
#83414=CARTESIAN_POINT('Ctrl Pts',(0.107636987026026,-0.274302921083635,
-0.812055308689511));
#83415=CARTESIAN_POINT('Ctrl Pts',(0.12296103885853,-0.267787387647584,
-0.811158705062295));
#83416=CARTESIAN_POINT('Ctrl Pts',(0.137640322889568,-0.260016886980164,
-0.81026210143508));
#83417=CARTESIAN_POINT('Ctrl Pts',(0.152317086530392,-0.252247720485024,
-0.80936565175209));
#83418=CARTESIAN_POINT('Ctrl Pts',(0.166348580559642,-0.243224336992414,
-0.8084692020691));
#83419=CARTESIAN_POINT('Ctrl Pts',(0.179517406282843,-0.233081832928868,
-0.80757275238611));
#83420=CARTESIAN_POINT('Ctrl Pts',(0.19268276334155,-0.222942000397656,
-0.80667653882768));
#83421=CARTESIAN_POINT('Ctrl Pts',(0.204985283023187,-0.211684124036696,
-0.805780325269251));
#83422=CARTESIAN_POINT('Ctrl Pts',(0.216239696783704,-0.199484419278528,
-0.804884111710821));
#83423=CARTESIAN_POINT('Ctrl Pts',(0.227520964179854,-0.187255605369643,
-0.803985759738711));
#83424=CARTESIAN_POINT('Ctrl Pts',(0.237748611876534,-0.174081076772951,
-0.803087407766602));
#83425=CARTESIAN_POINT('Ctrl Pts',(0.246776704110147,-0.160171465338034,
-0.802189055794492));
#83426=CARTESIAN_POINT('Ctrl Pts',(0.254804454329073,-0.14780308413939,
-0.8013902441459));
#83427=CARTESIAN_POINT('Ctrl Pts',(0.261884176472585,-0.134854298041266,
-0.800591432497308));
#83428=CARTESIAN_POINT('Ctrl Pts',(0.267944271076834,-0.121488713867191,
-0.799792620848715));
#83429=CARTESIAN_POINT('Ctrl Pts',(0.274759448894066,-0.106457787994576,
-0.798894277871724));
#83430=CARTESIAN_POINT('Ctrl Pts',(0.280327563692435,-0.0908038287342872,
-0.797995934894732));
#83431=CARTESIAN_POINT('Ctrl Pts',(0.284543265378996,-0.0747580773392285,
-0.79709759191774));
#83432=CARTESIAN_POINT('Ctrl Pts',(0.288750804726704,-0.0587433933369265,
-0.796200988290524));
#83433=CARTESIAN_POINT('Ctrl Pts',(0.29161086635382,-0.0423391625408519,
-0.795304384663309));
#83434=CARTESIAN_POINT('Ctrl Pts',(0.293067071160927,-0.0257940264626506,
-0.794407781036093));
#83435=CARTESIAN_POINT('Ctrl Pts',(0.294523025941919,-0.00925173113602084,
-0.793511331353103));
#83436=CARTESIAN_POINT('Ctrl Pts',(0.294575480890083,0.0074306404827253,
-0.792614881670114));
#83437=CARTESIAN_POINT('Ctrl Pts',(0.293219671041644,0.0239971772137955,
-0.791718431987124));
#83438=CARTESIAN_POINT('Ctrl Pts',(0.291864218313086,0.0405593503243735,
-0.790822218428694));
#83439=CARTESIAN_POINT('Ctrl Pts',(0.289101312695973,0.0570049613871002,
-0.789926004870265));
#83440=CARTESIAN_POINT('Ctrl Pts',(0.284978167813586,0.0730827193638239,
-0.789029791311836));
#83441=CARTESIAN_POINT('Ctrl Pts',(0.280845184886083,0.0891988397345135,
-0.788131439339727));
#83442=CARTESIAN_POINT('Ctrl Pts',(0.275345703668974,0.104944591145454,
-0.787233087367617));
#83443=CARTESIAN_POINT('Ctrl Pts',(0.268577205164191,0.120082991577459,
-0.786334735395508));
#83444=CARTESIAN_POINT('Ctrl Pts',(0.262558678331769,0.133544007951413,
-0.785535923746915));
#83445=CARTESIAN_POINT('Ctrl Pts',(0.255537682367956,0.146524729915943,
-0.784737112098323));
#83446=CARTESIAN_POINT('Ctrl Pts',(0.247612630236219,0.158876132088812,
-0.783938300449731));
#83447=CARTESIAN_POINT('Ctrl Pts',(0.238700122591408,0.172766509648471,
-0.783039957472739));
#83448=CARTESIAN_POINT('Ctrl Pts',(0.228586828719118,0.185948756421437,
-0.782141614495747));
#83449=CARTESIAN_POINT('Ctrl Pts',(0.217409588544599,0.198208755631198,
-0.781243271518755));
#83450=CARTESIAN_POINT('Ctrl Pts',(0.206253989470077,0.21044501732931,-0.78034666789154));
#83451=CARTESIAN_POINT('Ctrl Pts',(0.19403901135192,0.2217619537564,-0.779450064264324));
#83452=CARTESIAN_POINT('Ctrl Pts',(0.18094271701787,0.231977096193118,-0.778553460637108));
#83453=CARTESIAN_POINT('Ctrl Pts',(0.16784867127933,0.242190484719696,-0.777657010954118));
#83454=CARTESIAN_POINT('Ctrl Pts',(0.153874199203373,0.251301928323536,
-0.776760561271128));
#83455=CARTESIAN_POINT('Ctrl Pts',(0.139231519657763,0.25916833127099,-0.775864111588138));
#83456=CARTESIAN_POINT('Ctrl Pts',(0.12459269698927,0.26703266221042,-0.774967898029708));
#83457=CARTESIAN_POINT('Ctrl Pts',(0.109286718519198,0.273652238764066,
-0.774071684471278));
#83458=CARTESIAN_POINT('Ctrl Pts',(0.0935501770825538,0.278930106599884,
-0.773175470912849));
#83459=CARTESIAN_POINT('Ctrl Pts',(0.0777760874129412,0.284220567711797,
-0.772277118940739));
#83460=CARTESIAN_POINT('Ctrl Pts',(0.0615701445870226,0.28816269889627,
-0.771378766968629));
#83461=CARTESIAN_POINT('Ctrl Pts',(0.045184252581767,0.290709517076113,
-0.77048041499652));
#83462=CARTESIAN_POINT('Ctrl Pts',(0.0306139707626918,0.292974139509263,
-0.769681603347928));
#83463=CARTESIAN_POINT('Ctrl Pts',(0.0159019676247145,0.294136245662769,
-0.768882791699337));
#83464=CARTESIAN_POINT('Ctrl Pts',(0.00122682394808608,0.294197442040206,
-0.768083980050745));
#83465=CARTESIAN_POINT('Ctrl Pts',(-0.0152768315525506,0.294266263440075,
-0.767185637073753));
#83466=CARTESIAN_POINT('Ctrl Pts',(-0.0318387570596783,0.292942267055195,
-0.766287294096761));
#83467=CARTESIAN_POINT('Ctrl Pts',(-0.0482048485476907,0.290223935223293,
-0.765388951119769));
#83468=CARTESIAN_POINT('Ctrl Pts',(-0.0645392524082683,0.287510866559228,
-0.764492347492553));
#83469=CARTESIAN_POINT('Ctrl Pts',(-0.0806777927326734,0.283408884511531,
-0.763595743865337));
#83470=CARTESIAN_POINT('Ctrl Pts',(-0.0963705245024942,0.277968275181025,
-0.762699140238121));
#83471=CARTESIAN_POINT('Ctrl Pts',(-0.112060561876071,0.272528599987262,
-0.761802690555131));
#83472=CARTESIAN_POINT('Ctrl Pts',(-0.12730418032624,0.265750962427366,
-0.760906240872141));
#83473=CARTESIAN_POINT('Ctrl Pts',(-0.141865919124776,0.257735719276321,
-0.76000979118915));
#83474=CARTESIAN_POINT('Ctrl Pts',(-0.156423822365954,0.249722587337767,
-0.759113577630721));
#83475=CARTESIAN_POINT('Ctrl Pts',(-0.170299514631689,0.240472888163074,
-0.758217364072292));
#83476=CARTESIAN_POINT('Ctrl Pts',(-0.183283017687103,0.23013251710158,
-0.757321150513862));
#83477=CARTESIAN_POINT('Ctrl Pts',(-0.196297500078069,0.219767473359417,
-0.756422798541753));
#83478=CARTESIAN_POINT('Ctrl Pts',(-0.208414936754856,0.208307075917067,
-0.755524446569643));
#83479=CARTESIAN_POINT('Ctrl Pts',(-0.219458972650302,0.19593723312141,
-0.754626094597533));
#83480=CARTESIAN_POINT('Ctrl Pts',(-0.229279293409457,0.184938009183379,
-0.753827282948942));
#83481=CARTESIAN_POINT('Ctrl Pts',(-0.238251205363472,0.173220572478498,
-0.753028471300351));
#83482=CARTESIAN_POINT('Ctrl Pts',(-0.246278992508625,0.160935694763271,
-0.752229659651761));
#83483=CARTESIAN_POINT('Ctrl Pts',(-0.255487172745188,0.146844468110076,
-0.751313392005111));
#83484=CARTESIAN_POINT('Ctrl Pts',(-0.263509256906277,0.131919432687266,
-0.750397124358462));
#83485=CARTESIAN_POINT('Ctrl Pts',(-0.270201849148427,0.116381273050137,
-0.749480856711813));
#83486=CARTESIAN_POINT('Ctrl Pts',(-0.276879016293115,0.100878925788558,
-0.748566700880322));
#83487=CARTESIAN_POINT('Ctrl Pts',(-0.28223242070145,0.0847669120513509,
-0.747652545048832));
#83488=CARTESIAN_POINT('Ctrl Pts',(-0.286164346184093,0.0682906067701156,
-0.746738389217342));
#83489=CARTESIAN_POINT('Ctrl Pts',(-0.290089851922504,0.0518412027275383,
-0.745825725948885));
#83490=CARTESIAN_POINT('Ctrl Pts',(-0.292598275702172,0.0350294021982569,
-0.744913062680429));
#83491=CARTESIAN_POINT('Ctrl Pts',(-0.29364173715284,0.0181154685797119,
-0.744000399411972));
#83492=CARTESIAN_POINT('Ctrl Pts',(-0.29401628240508,0.01204429697153,-0.743672803510968));
#83493=CARTESIAN_POINT('Ctrl Pts',(-0.294202558046068,0.00596006500085705,
-0.743345207609965));
#83494=CARTESIAN_POINT('Ctrl Pts',(-0.294199973461936,-0.000124959977242106,
-0.743017611708961));
#83495=CARTESIAN_POINT('',(-0.29419994452424,-0.000180670788710602,-0.643017611712501));
#83496=CARTESIAN_POINT('Ctrl Pts',(-0.294199973461913,-0.000124960031394621,
-0.743017611706046));
#83497=CARTESIAN_POINT('Ctrl Pts',(-0.294192255021624,-0.0182968899125074,
-0.742039300234221));
#83498=CARTESIAN_POINT('Ctrl Pts',(-0.292496705742507,-0.0364142011968275,
-0.741060988762396));
#83499=CARTESIAN_POINT('Ctrl Pts',(-0.289168196490808,-0.0541792777568467,
-0.740082677290572));
#83500=CARTESIAN_POINT('Ctrl Pts',(-0.28581688854588,-0.0720660365776137,
-0.739097664854008));
#83501=CARTESIAN_POINT('Ctrl Pts',(-0.280810398565039,-0.0895952168965191,
-0.738112652417445));
#83502=CARTESIAN_POINT('Ctrl Pts',(-0.274254017629792,-0.106481800388225,
-0.737127639980882));
#83503=CARTESIAN_POINT('Ctrl Pts',(-0.272584877908559,-0.110780828699772,
-0.736876873071513));
#83504=CARTESIAN_POINT('Ctrl Pts',(-0.270815523574129,-0.115038324182596,
-0.736626106162144));
#83505=CARTESIAN_POINT('Ctrl Pts',(-0.268948167693537,-0.11924983477678,
-0.736375339252776));
#83506=CARTESIAN_POINT('Ctrl Pts',(-0.262258584745376,-0.134337076448095,
-0.735476996275783));
#83507=CARTESIAN_POINT('Ctrl Pts',(-0.254274257069447,-0.148907623949626,
-0.734578653298791));
#83508=CARTESIAN_POINT('Ctrl Pts',(-0.245097765117353,-0.162728994142036,
-0.733680310321798));
#83509=CARTESIAN_POINT('Ctrl Pts',(-0.235939040465313,-0.176523603734355,
-0.732783706694582));
#83510=CARTESIAN_POINT('Ctrl Pts',(-0.225593111081812,-0.189571227491716,
-0.731887103067366));
#83511=CARTESIAN_POINT('Ctrl Pts',(-0.21420812514189,-0.201664372468704,
-0.73099049944015));
#83512=CARTESIAN_POINT('Ctrl Pts',(-0.20282509397082,-0.213755441088002,
-0.73009404975716));
#83513=CARTESIAN_POINT('Ctrl Pts',(-0.190403862688639,-0.224891746030959,
-0.729197600074169));
#83514=CARTESIAN_POINT('Ctrl Pts',(-0.177132341269818,-0.234899496968965,
-0.728301150391179));
#83515=CARTESIAN_POINT('Ctrl Pts',(-0.163864315565505,-0.244904611868566,
-0.727404936832749));
#83516=CARTESIAN_POINT('Ctrl Pts',(-0.149747082751248,-0.253781295277588,
-0.726508723274319));
#83517=CARTESIAN_POINT('Ctrl Pts',(-0.134999679343011,-0.261397640726316,
-0.725612509715889));
#83518=CARTESIAN_POINT('Ctrl Pts',(-0.120217087838255,-0.269032159184309,
-0.724714157743779));
#83519=CARTESIAN_POINT('Ctrl Pts',(-0.10480204073917,-0.275399992731581,
-0.723815805771669));
#83520=CARTESIAN_POINT('Ctrl Pts',(-0.0889963284700256,-0.280416286115581,
-0.722917453799559));
#83521=CARTESIAN_POINT('Ctrl Pts',(-0.0749419405832901,-0.284876757859713,
-0.72211864215097));
#83522=CARTESIAN_POINT('Ctrl Pts',(-0.0605793272098095,-0.288269229543724,
-0.72131983050238));
#83523=CARTESIAN_POINT('Ctrl Pts',(-0.0460852246718732,-0.290568050664458,
-0.72052101885379));
#83524=CARTESIAN_POINT('Ctrl Pts',(-0.0297851678991138,-0.293153303161486,
-0.719622675876799));
#83525=CARTESIAN_POINT('Ctrl Pts',(-0.013215082003028,-0.294370922283767,
-0.718724332899807));
#83526=CARTESIAN_POINT('Ctrl Pts',(0.00337413362794727,-0.294180650659184,
-0.717825989922815));
#83527=CARTESIAN_POINT('Ctrl Pts',(0.0199312296239529,-0.293990747433883,
-0.7169293862956));
#83528=CARTESIAN_POINT('Ctrl Pts',(0.0365065991775859,-0.292398307581924,
-0.716032782668384));
#83529=CARTESIAN_POINT('Ctrl Pts',(0.0528455518248773,-0.289414905718977,
-0.715136179041169));
#83530=CARTESIAN_POINT('Ctrl Pts',(0.0691816991216972,-0.28643201609742,
-0.714239729358179));
#83531=CARTESIAN_POINT('Ctrl Pts',(0.0852807248679252,-0.282058728504559,
-0.713343279675189));
#83532=CARTESIAN_POINT('Ctrl Pts',(0.100894616336768,-0.276358311606972,
-0.712446829992199));
#83533=CARTESIAN_POINT('Ctrl Pts',(0.116504395111576,-0.270659396197379,
-0.711550616433769));
#83534=CARTESIAN_POINT('Ctrl Pts',(0.131628553785732,-0.263634327153267,
-0.71065440287534));
#83535=CARTESIAN_POINT('Ctrl Pts',(0.14603731815087,-0.255395265632121,
-0.70975818931691));
#83536=CARTESIAN_POINT('Ctrl Pts',(0.160480462601583,-0.247136545267719,
-0.708859837344801));
#83537=CARTESIAN_POINT('Ctrl Pts',(0.174204127161342,-0.237658464649597,
-0.707961485372691));
#83538=CARTESIAN_POINT('Ctrl Pts',(0.187005664358342,-0.227117858165964,
-0.707063133400582));
#83539=CARTESIAN_POINT('Ctrl Pts',(0.198388749552488,-0.21774518520062,
-0.706264321751989));
#83540=CARTESIAN_POINT('Ctrl Pts',(0.20904289889353,-0.207533298554993,
-0.705465510103397));
#83541=CARTESIAN_POINT('Ctrl Pts',(0.218850519695666,-0.19661660669673,
-0.704666698454805));
#83542=CARTESIAN_POINT('Ctrl Pts',(0.229880162646069,-0.184339703273834,
-0.703768355477813));
#83543=CARTESIAN_POINT('Ctrl Pts',(0.239908600155231,-0.17109278725329,
-0.702870012500821));
#83544=CARTESIAN_POINT('Ctrl Pts',(0.248765668658983,-0.157064579382651,
-0.70197166952383));
#83545=CARTESIAN_POINT('Ctrl Pts',(0.257605588322575,-0.143063532586175,
-0.701075065896615));
#83546=CARTESIAN_POINT('Ctrl Pts',(0.26527816780488,-0.12828482274366,-0.700178462269399));
#83547=CARTESIAN_POINT('Ctrl Pts',(0.271654690118552,-0.112948525163427,
-0.699281858642184));
#83548=CARTESIAN_POINT('Ctrl Pts',(0.278030117601958,-0.0976148607807189,
-0.698385408959195));
#83549=CARTESIAN_POINT('Ctrl Pts',(0.283109578367738,-0.0817245067042235,
-0.697488959276205));
#83550=CARTESIAN_POINT('Ctrl Pts',(0.286811376364256,-0.0655200304337614,
-0.696592509593215));
#83551=CARTESIAN_POINT('Ctrl Pts',(0.290512199308362,-0.0493198224171825,
-0.695696296034786));
#83552=CARTESIAN_POINT('Ctrl Pts',(0.292835914388295,-0.0328064303094779,
-0.694800082476357));
#83553=CARTESIAN_POINT('Ctrl Pts',(0.293751778554187,-0.0162336870812481,
-0.693903868917928));
#83554=CARTESIAN_POINT('Ctrl Pts',(0.294669828021164,0.0003785996023382,
-0.693005516945819));
#83555=CARTESIAN_POINT('Ctrl Pts',(0.294173300279452,0.0170497255797299,
-0.692107164973709));
#83556=CARTESIAN_POINT('Ctrl Pts',(0.292283694721163,0.0335243463790987,
-0.6912088130016));
#83557=CARTESIAN_POINT('Ctrl Pts',(0.290603463611231,0.0481735255530376,
-0.690410001353007));
#83558=CARTESIAN_POINT('Ctrl Pts',(0.287822606151975,0.0626669847273044,
-0.689611189704414));
#83559=CARTESIAN_POINT('Ctrl Pts',(0.283990027738915,0.0768329626192458,
-0.688812378055821));
#83560=CARTESIAN_POINT('Ctrl Pts',(0.279679912948768,0.0927640106627477,
-0.687914035078829));
#83561=CARTESIAN_POINT('Ctrl Pts',(0.274011393354672,0.108381892354642,
-0.687015692101837));
#83562=CARTESIAN_POINT('Ctrl Pts',(0.267050389441296,0.123441198549156,
-0.686117349124845));
#83563=CARTESIAN_POINT('Ctrl Pts',(0.260102863254034,0.138471347282061,
-0.68522074549763));
#83564=CARTESIAN_POINT('Ctrl Pts',(0.251868088519605,0.152944329890869,
-0.684324141870414));
#83565=CARTESIAN_POINT('Ctrl Pts',(0.24246083193315,0.16663248476298,-0.683427538243199));
#83566=CARTESIAN_POINT('Ctrl Pts',(0.233055190545188,0.18031828941886,-0.682531088560209));
#83567=CARTESIAN_POINT('Ctrl Pts',(0.222477870275601,0.193218854145344,
-0.681634638877219));
#83568=CARTESIAN_POINT('Ctrl Pts',(0.21088807490934,0.205133760900133,-0.680738189194228));
#83569=CARTESIAN_POINT('Ctrl Pts',(0.199301332291482,0.217045529272281,
-0.679841975635799));
#83570=CARTESIAN_POINT('Ctrl Pts',(0.186703203618274,0.227971595563905,
-0.678945762077369));
#83571=CARTESIAN_POINT('Ctrl Pts',(0.173290043395749,0.237748187921379,
-0.67804954851894));
#83572=CARTESIAN_POINT('Ctrl Pts',(0.159844878652601,0.247548107753255,
-0.67715119654683));
#83573=CARTESIAN_POINT('Ctrl Pts',(0.145581456020645,0.256192629485234,
-0.676252844574721));
#83574=CARTESIAN_POINT('Ctrl Pts',(0.13072579421455,0.263561011393899,-0.675354492602611));
#83575=CARTESIAN_POINT('Ctrl Pts',(0.117516188106169,0.27011295259585,-0.674555680954019));
#83576=CARTESIAN_POINT('Ctrl Pts',(0.103839065152268,0.275656402311337,
-0.673756869305427));
#83577=CARTESIAN_POINT('Ctrl Pts',(0.0898651813964756,0.280139053279935,
-0.672958057656835));
#83578=CARTESIAN_POINT('Ctrl Pts',(0.0741501622734572,0.285180239175313,
-0.672059714679843));
#83579=CARTESIAN_POINT('Ctrl Pts',(0.0579596738832171,0.288910980203061,
-0.671161371702851));
#83580=CARTESIAN_POINT('Ctrl Pts',(0.0415355396605274,0.291253221347179,
-0.670263028725859));
#83581=CARTESIAN_POINT('Ctrl Pts',(0.0251432054462076,0.293590927501082,
-0.669366425098644));
#83582=CARTESIAN_POINT('Ctrl Pts',(0.00851888820143327,0.294545294656183,
-0.668469821471429));
#83583=CARTESIAN_POINT('Ctrl Pts',(-0.00808393619602547,0.294088915084501,
-0.667573217844213));
#83584=CARTESIAN_POINT('Ctrl Pts',(-0.0246839099370022,0.293632613871858,
-0.666676768161224));
#83585=CARTESIAN_POINT('Ctrl Pts',(-0.0412616084004215,0.291766015895987,
-0.665780318478234));
#83586=CARTESIAN_POINT('Ctrl Pts',(-0.0575622706264213,0.288513821159976,
-0.664883868795244));
#83587=CARTESIAN_POINT('Ctrl Pts',(-0.0738586392631893,0.285262483051021,
-0.663987655236814));
#83588=CARTESIAN_POINT('Ctrl Pts',(-0.0898773427086045,0.280626438335591,
-0.663091441678385));
#83589=CARTESIAN_POINT('Ctrl Pts',(-0.10537418774529,0.274681489287175,
-0.662195228119956));
#83590=CARTESIAN_POINT('Ctrl Pts',(-0.120908009086468,0.268722355271065,
-0.661296876147846));
#83591=CARTESIAN_POINT('Ctrl Pts',(-0.135916752965931,0.261448388793748,
-0.660398524175737));
#83592=CARTESIAN_POINT('Ctrl Pts',(-0.150176221676798,0.252983680190801,
-0.659500172203628));
#83593=CARTESIAN_POINT('Ctrl Pts',(-0.162855694826091,0.245456888861901,
-0.658701360555035));
#83594=CARTESIAN_POINT('Ctrl Pts',(-0.174942762960054,0.236989521445209,
-0.657902548906443));
#83595=CARTESIAN_POINT('Ctrl Pts',(-0.186300708506579,0.227696477816295,
-0.657103737257851));
#83596=CARTESIAN_POINT('Ctrl Pts',(-0.198905453671994,0.217383305748889,
-0.656217237386512));
#83597=CARTESIAN_POINT('Ctrl Pts',(-0.210696351313985,0.205983107096295,
-0.655330737515173));
#83598=CARTESIAN_POINT('Ctrl Pts',(-0.22147910828788,0.193650831632621,
-0.654444237643834));
#83599=CARTESIAN_POINT('Ctrl Pts',(-0.232240944388006,0.181342483442729,
-0.653559457773414));
#83600=CARTESIAN_POINT('Ctrl Pts',(-0.24199793812666,0.168106205160555,
-0.652674677902993));
#83601=CARTESIAN_POINT('Ctrl Pts',(-0.250591645736961,0.154134574599086,
-0.651789898032573));
#83602=CARTESIAN_POINT('Ctrl Pts',(-0.25918261293684,0.140167399390736,
-0.650905400305797));
#83603=CARTESIAN_POINT('Ctrl Pts',(-0.266610566372324,0.125466004264436,
-0.65002090257902));
#83604=CARTESIAN_POINT('Ctrl Pts',(-0.272760083063504,0.110252333704057,
-0.649136404852244));
#83605=CARTESIAN_POINT('Ctrl Pts',(-0.278908646488963,0.0950410214868358,
-0.648252044235651));
#83606=CARTESIAN_POINT('Ctrl Pts',(-0.283778880199586,0.0793183525715875,
-0.647367683619057));
#83607=CARTESIAN_POINT('Ctrl Pts',(-0.287303993989222,0.0633249953639239,
-0.646483323002464));
#83608=CARTESIAN_POINT('Ctrl Pts',(-0.290835491119008,0.0473026770942102,
-0.645597360969586));
#83609=CARTESIAN_POINT('Ctrl Pts',(-0.293016886047028,0.0310094971912828,
-0.644711398936707));
#83610=CARTESIAN_POINT('Ctrl Pts',(-0.293832794792137,0.0146945127391705,
-0.643825436903829));
#83611=CARTESIAN_POINT('Ctrl Pts',(-0.29408077819461,0.00973581437986222,
-0.643556161840053));
#83612=CARTESIAN_POINT('Ctrl Pts',(-0.294202987909769,0.00477510463055562,
-0.643286886776277));
#83613=CARTESIAN_POINT('Ctrl Pts',(-0.29419994452424,-0.000180670788711742,
-0.643017611712501));
#83614=CARTESIAN_POINT('',(-0.294199888424845,0.000256224137824597,-0.543017611708961));
#83615=CARTESIAN_POINT('Ctrl Pts',(-0.2941999445242,-0.000180670853884201,
-0.64301761170896));
#83616=CARTESIAN_POINT('Ctrl Pts',(-0.294193283057564,-0.011028038166241,
-0.642428213425595));
#83617=CARTESIAN_POINT('Ctrl Pts',(-0.293586727488202,-0.0218568137071715,
-0.64183881514223));
#83618=CARTESIAN_POINT('Ctrl Pts',(-0.292386214611939,-0.0326181162071238,
-0.641249416858865));
#83619=CARTESIAN_POINT('Ctrl Pts',(-0.290556429317991,-0.0490201669035152,
-0.640351073881873));
#83620=CARTESIAN_POINT('Ctrl Pts',(-0.287336367282512,-0.0653199074971147,
-0.639452730904881));
#83621=CARTESIAN_POINT('Ctrl Pts',(-0.282753746412743,-0.0812647456746065,
-0.638554387927889));
#83622=CARTESIAN_POINT('Ctrl Pts',(-0.278179998301807,-0.097178711845047,
-0.637657784300673));
#83623=CARTESIAN_POINT('Ctrl Pts',(-0.272249080833386,-0.112738369890925,
-0.636761180673457));
#83624=CARTESIAN_POINT('Ctrl Pts',(-0.265039693558183,-0.127701217059919,
-0.635864577046242));
#83625=CARTESIAN_POINT('Ctrl Pts',(-0.257831544113728,-0.142661495151736,
-0.634968127363251));
#83626=CARTESIAN_POINT('Ctrl Pts',(-0.249345655567605,-0.157024432522995,
-0.634071677680261));
#83627=CARTESIAN_POINT('Ctrl Pts',(-0.239708799974846,-0.170567673416211,
-0.63317522799727));
#83628=CARTESIAN_POINT('Ctrl Pts',(-0.230074482726777,-0.184107347024094,
-0.63227901443884));
#83629=CARTESIAN_POINT('Ctrl Pts',(-0.219290268003284,-0.196827114454101,
-0.631382800880411));
#83630=CARTESIAN_POINT('Ctrl Pts',(-0.207525233393089,-0.208535170906838,
-0.630486587321981));
#83631=CARTESIAN_POINT('Ctrl Pts',(-0.195732126778491,-0.220271163411035,
-0.629588235349871));
#83632=CARTESIAN_POINT('Ctrl Pts',(-0.182954108098386,-0.230990082188767,
-0.628689883377761));
#83633=CARTESIAN_POINT('Ctrl Pts',(-0.169396135275969,-0.240538124532402,
-0.627791531405651));
#83634=CARTESIAN_POINT('Ctrl Pts',(-0.157340429986674,-0.249028212696192,
-0.626992719757061));
#83635=CARTESIAN_POINT('Ctrl Pts',(-0.144668856891886,-0.256592917736481,
-0.626193908108471));
#83636=CARTESIAN_POINT('Ctrl Pts',(-0.131542195880845,-0.263154499681927,
-0.62539509645988));
#83637=CARTESIAN_POINT('Ctrl Pts',(-0.116779962816974,-0.270533649784523,
-0.624496753482888));
#83638=CARTESIAN_POINT('Ctrl Pts',(-0.101347946836035,-0.276690209350932,
-0.623598410505896));
#83639=CARTESIAN_POINT('Ctrl Pts',(-0.0854732364897492,-0.281510152292892,
-0.622700067528904));
#83640=CARTESIAN_POINT('Ctrl Pts',(-0.0696292623707145,-0.286320762978807,
-0.621803463901689));
#83641=CARTESIAN_POINT('Ctrl Pts',(-0.0533450244017,-0.289799603919447,
-0.620906860274473));
#83642=CARTESIAN_POINT('Ctrl Pts',(-0.0368668522651501,-0.291880926413597,
-0.620010256647257));
#83643=CARTESIAN_POINT('Ctrl Pts',(-0.0203915093826523,-0.29396189155075,
-0.619113806964267));
#83644=CARTESIAN_POINT('Ctrl Pts',(-0.00372307423914003,-0.294645663599207,
-0.618217357281277));
#83645=CARTESIAN_POINT('Ctrl Pts',(0.012882905653892,-0.293917795891833,
-0.617320907598286));
#83646=CARTESIAN_POINT('Ctrl Pts',(0.029484511537114,-0.29319011990458,
-0.616424694039857));
#83647=CARTESIAN_POINT('Ctrl Pts',(0.0460229048034565,-0.291051587968063,
-0.615528480481427));
#83648=CARTESIAN_POINT('Ctrl Pts',(0.0622451876113885,-0.287539869616759,
-0.614632266922998));
#83649=CARTESIAN_POINT('Ctrl Pts',(0.078506177657293,-0.284019772116878,
-0.613733914950888));
#83650=CARTESIAN_POINT('Ctrl Pts',(0.0944487800500677,-0.279120138447055,
-0.612835562978778));
#83651=CARTESIAN_POINT('Ctrl Pts',(0.10983249331608,-0.27292941104244,-0.611937211006669));
#83652=CARTESIAN_POINT('Ctrl Pts',(0.123511641063281,-0.267424636391091,
-0.611138399358077));
#83653=CARTESIAN_POINT('Ctrl Pts',(0.136748777549695,-0.260899933740103,
-0.610339587709486));
#83654=CARTESIAN_POINT('Ctrl Pts',(0.149391259655662,-0.253448005591866,
-0.609540776060895));
#83655=CARTESIAN_POINT('Ctrl Pts',(0.163608985488364,-0.245067572821736,
-0.608642433083903));
#83656=CARTESIAN_POINT('Ctrl Pts',(0.177164532338704,-0.235460414421937,
-0.607744090106912));
#83657=CARTESIAN_POINT('Ctrl Pts',(0.189838758032202,-0.22475516890339,
-0.60684574712992));
#83658=CARTESIAN_POINT('Ctrl Pts',(0.202488444198825,-0.214070650620292,
-0.605949143502705));
#83659=CARTESIAN_POINT('Ctrl Pts',(0.214259556556526,-0.202292719801003,
-0.605052539875489));
#83660=CARTESIAN_POINT('Ctrl Pts',(0.224963018208994,-0.189592406067068,
-0.604155936248274));
#83661=CARTESIAN_POINT('Ctrl Pts',(0.235664642108343,-0.176894272939925,
-0.603259486565284));
#83662=CARTESIAN_POINT('Ctrl Pts',(0.245298430800219,-0.163274640426973,
-0.602363036882294));
#83663=CARTESIAN_POINT('Ctrl Pts',(0.253713359510653,-0.148940159815337,
-0.601466587199305));
#83664=CARTESIAN_POINT('Ctrl Pts',(0.262126071731548,-0.134609454901324,
-0.600570373640875));
#83665=CARTESIAN_POINT('Ctrl Pts',(0.26932017023549,-0.119564963637371,
-0.599674160082446));
#83666=CARTESIAN_POINT('Ctrl Pts',(0.275189816146444,-0.104039440066191,
-0.598777946524017));
#83667=CARTESIAN_POINT('Ctrl Pts',(0.281073467347761,-0.0884768717619945,
-0.597879594551908));
#83668=CARTESIAN_POINT('Ctrl Pts',(0.285626098317954,-0.0724317313013547,
-0.596981242579798));
#83669=CARTESIAN_POINT('Ctrl Pts',(0.288791226176685,-0.056153964093078,
-0.596082890607689));
#83670=CARTESIAN_POINT('Ctrl Pts',(0.291605647563108,-0.0416798264913989,
-0.595284078959096));
#83671=CARTESIAN_POINT('Ctrl Pts',(0.293323706045839,-0.0270223436892772,
-0.594485267310503));
#83672=CARTESIAN_POINT('Ctrl Pts',(0.293940248477391,-0.01236002933045,
-0.593686455661911));
#83673=CARTESIAN_POINT('Ctrl Pts',(0.294633611630492,0.00412919832901943,
-0.59278811268492));
#83674=CARTESIAN_POINT('Ctrl Pts',(0.293937360080827,0.0207293663013482,
-0.591889769707929));
#83675=CARTESIAN_POINT('Ctrl Pts',(0.29184036052926,0.0371866100384445,
-0.590991426730939));
#83676=CARTESIAN_POINT('Ctrl Pts',(0.289747421137114,0.0536119896613369,
-0.590094823103724));
#83677=CARTESIAN_POINT('Ctrl Pts',(0.286259150804987,0.0698942103517408,
-0.58919821947651));
#83678=CARTESIAN_POINT('Ctrl Pts',(0.281416340284715,0.0857816030437603,
-0.588301615849295));
#83679=CARTESIAN_POINT('Ctrl Pts',(0.276574361260873,0.101666267916833,
-0.587405166166306));
#83680=CARTESIAN_POINT('Ctrl Pts',(0.270378483389427,0.117155469695785,
-0.586508716483318));
#83681=CARTESIAN_POINT('Ctrl Pts',(0.262920080392568,0.132010118272675,
-0.585612266800329));
#83682=CARTESIAN_POINT('Ctrl Pts',(0.25546364193668,0.146860854139867,-0.5847160532419));
#83683=CARTESIAN_POINT('Ctrl Pts',(0.246745703427356,0.161076666421359,
-0.583819839683472));
#83684=CARTESIAN_POINT('Ctrl Pts',(0.236904108937943,0.174442205811321,
-0.582923626125044));
#83685=CARTESIAN_POINT('Ctrl Pts',(0.22703903187555,0.187839636096043,-0.582025274152935));
#83686=CARTESIAN_POINT('Ctrl Pts',(0.216045436576349,0.20038211765071,-0.581126922180827));
#83687=CARTESIAN_POINT('Ctrl Pts',(0.204102423935433,0.211886385932841,
-0.580228570208718));
#83688=CARTESIAN_POINT('Ctrl Pts',(0.193482735981139,0.222115943831838,
-0.57942975856012));
#83689=CARTESIAN_POINT('Ctrl Pts',(0.182113241232746,0.231524881934175,
-0.578630946911523));
#83690=CARTESIAN_POINT('Ctrl Pts',(0.170140981002164,0.240011846756824,
-0.577832135262925));
#83691=CARTESIAN_POINT('Ctrl Pts',(0.156676986184649,0.24955628098961,-0.57693379228593));
#83692=CARTESIAN_POINT('Ctrl Pts',(0.142364568443402,0.257994588955791,
-0.576035449308936));
#83693=CARTESIAN_POINT('Ctrl Pts',(0.12741076732988,0.26517944182838,-0.575137106331942));
#83694=CARTESIAN_POINT('Ctrl Pts',(0.112485919401599,0.272350383563956,
-0.574240502704724));
#83695=CARTESIAN_POINT('Ctrl Pts',(0.0969228294530991,0.278272289657258,
-0.573343899077506));
#83696=CARTESIAN_POINT('Ctrl Pts',(0.0809549165910538,0.28284260902441,
-0.572447295450288));
#83697=CARTESIAN_POINT('Ctrl Pts',(0.064989745373034,0.287412143681069,
-0.571550845767296));
#83698=CARTESIAN_POINT('Ctrl Pts',(0.0486206329227484,0.290630284749886,
-0.570654396084304));
#83699=CARTESIAN_POINT('Ctrl Pts',(0.032097933215732,0.292443776961108,
-0.569757946401311));
#83700=CARTESIAN_POINT('Ctrl Pts',(0.0155795855825511,0.29425679149906,
-0.56886173284288));
#83701=CARTESIAN_POINT('Ctrl Pts',(-0.00109148125168673,0.294665816296967,
-0.567965519284448));
#83702=CARTESIAN_POINT('Ctrl Pts',(-0.0176595829037503,0.293669506642528,
-0.567069305726016));
#83703=CARTESIAN_POINT('Ctrl Pts',(-0.0342672169361189,0.292670819739748,
-0.566170953753905));
#83704=CARTESIAN_POINT('Ctrl Pts',(-0.0507706037386733,0.290260175593658,
-0.565272601781793));
#83705=CARTESIAN_POINT('Ctrl Pts',(-0.066918566065098,0.286488299090541,
-0.564374249809681));
#83706=CARTESIAN_POINT('Ctrl Pts',(-0.0812772815882203,0.283134358785145,
-0.563575438161101));
#83707=CARTESIAN_POINT('Ctrl Pts',(-0.0953547231456902,0.278705005984337,
-0.56277662651252));
#83708=CARTESIAN_POINT('Ctrl Pts',(-0.108985894084055,0.273268576478707,
-0.561977814863939));
#83709=CARTESIAN_POINT('Ctrl Pts',(-0.124315498631508,0.267154771960502,
-0.561079471886949));
#83710=CARTESIAN_POINT('Ctrl Pts',(-0.139177779585522,0.259727595661658,
-0.560181128909958));
#83711=CARTESIAN_POINT('Ctrl Pts',(-0.153336538137476,0.251080756076635,
-0.559282785932967));
#83712=CARTESIAN_POINT('Ctrl Pts',(-0.167467882846218,0.242450658291663,
-0.558386182305753));
#83713=CARTESIAN_POINT('Ctrl Pts',(-0.18089770736005,0.232605936149883,
-0.557489578678539));
#83714=CARTESIAN_POINT('Ctrl Pts',(-0.19341306062255,0.221686778993737,
-0.556592975051324));
#83715=CARTESIAN_POINT('Ctrl Pts',(-0.205926265035431,0.210769496624997,
-0.555696525368335));
#83716=CARTESIAN_POINT('Ctrl Pts',(-0.21752468109241,0.198778624291577,
-0.554800075685346));
#83717=CARTESIAN_POINT('Ctrl Pts',(-0.228027531399338,0.185895360146304,
-0.553903626002357));
#83718=CARTESIAN_POINT('Ctrl Pts',(-0.238527615258844,0.173015489448698,
-0.553007412443928));
#83719=CARTESIAN_POINT('Ctrl Pts',(-0.247932214807086,0.159244313826685,
-0.5521111988855));
#83720=CARTESIAN_POINT('Ctrl Pts',(-0.2561012284999,0.144795720796031,-0.551214985327071));
#83721=CARTESIAN_POINT('Ctrl Pts',(-0.264289733898089,0.130312652646466,
-0.550316633354963));
#83722=CARTESIAN_POINT('Ctrl Pts',(-0.271236397514644,0.115149643520624,
-0.549418281382854));
#83723=CARTESIAN_POINT('Ctrl Pts',(-0.276847274179232,0.0995450992240658,
-0.548519929410745));
#83724=CARTESIAN_POINT('Ctrl Pts',(-0.281836447440568,0.0856695892434102,
-0.547721117762148));
#83725=CARTESIAN_POINT('Ctrl Pts',(-0.285770050743515,0.0714456554660817,
-0.546922306113551));
#83726=CARTESIAN_POINT('Ctrl Pts',(-0.288615763265484,0.0570489368409436,
-0.546123494464955));
#83727=CARTESIAN_POINT('Ctrl Pts',(-0.292303929082806,0.0383901703264396,
-0.545088200212957));
#83728=CARTESIAN_POINT('Ctrl Pts',(-0.294183248271218,0.0193626650139326,
-0.544052905960959));
#83729=CARTESIAN_POINT('Ctrl Pts',(-0.294199888424845,0.000256224137824597,
-0.543017611708961));
#83730=CARTESIAN_POINT('',(-0.293720787035063,-5.32817649356945E-6,-0.443017611708961));
#83731=CARTESIAN_POINT('Ctrl Pts',(-0.294309160300636,0.000255261948186358,
-0.543017554436766));
#83732=CARTESIAN_POINT('Ctrl Pts',(-0.293592516521209,-0.0781986943848365,
-0.538768094313166));
#83733=CARTESIAN_POINT('Ctrl Pts',(-0.221008030116168,-0.25539079515841,
-0.529233860723241));
#83734=CARTESIAN_POINT('Ctrl Pts',(0.0780070236891849,-0.338696449993926,
-0.514414853666984));
#83735=CARTESIAN_POINT('Ctrl Pts',(0.326697109816754,-0.118614414899743,
-0.498560533268));
#83736=CARTESIAN_POINT('Ctrl Pts',(0.277134063845491,0.2097548369844,-0.482706212869015));
#83737=CARTESIAN_POINT('Ctrl Pts',(-0.0254342890729399,0.346631617026237,
-0.466851892470028));
#83738=CARTESIAN_POINT('Ctrl Pts',(-0.258534819861522,0.196786222189288,
-0.453622358750011));
#83739=CARTESIAN_POINT('Ctrl Pts',(-0.293712791820078,0.0493531751511997,
-0.445677598496322));
#83740=CARTESIAN_POINT('Ctrl Pts',(-0.293720787035063,-5.32817649356945E-6,
-0.443017611708961));
#83741=CARTESIAN_POINT('',(-0.294328611994138,-0.000252932005302681,-0.343017611708961));
#83742=CARTESIAN_POINT('Ctrl Pts',(-0.293720787035063,-5.32817649356945E-6,
-0.443017611708961));
#83743=CARTESIAN_POINT('Ctrl Pts',(-0.293728676447855,-0.0487106610916299,
-0.440392825029993));
#83744=CARTESIAN_POINT('Ctrl Pts',(-0.25921725196049,-0.195469311288766,
-0.432483264884698));
#83745=CARTESIAN_POINT('Ctrl Pts',(-0.0277336353910758,-0.346455230082455,
-0.419288931273073));
#83746=CARTESIAN_POINT('Ctrl Pts',(0.275736237085626,-0.211589008666704,
-0.403434610874089));
#83747=CARTESIAN_POINT('Ctrl Pts',(0.327476926891764,0.116444163611204,
-0.387580290475104));
#83748=CARTESIAN_POINT('Ctrl Pts',(0.0802525630696079,0.338171416792465,
-0.371725970076119));
#83749=CARTESIAN_POINT('Ctrl Pts',(-0.220020588114288,0.25665829857542,
-0.356871743820737));
#83750=CARTESIAN_POINT('Ctrl Pts',(-0.293610504889156,0.0788377678713336,
-0.347302291031685));
#83751=CARTESIAN_POINT('Ctrl Pts',(-0.294328611994138,-0.000252932005302681,
-0.343017611708961));
#83752=CARTESIAN_POINT('',(-0.294199939266707,0.000189038265259436,-0.24301761170896));
#83753=CARTESIAN_POINT('Ctrl Pts',(-0.294328611994138,-0.000252932005302681,
-0.343017611708961));
#83754=CARTESIAN_POINT('Ctrl Pts',(-0.294496226570651,-0.0187136241137339,
-0.342017517565357));
#83755=CARTESIAN_POINT('Ctrl Pts',(-0.28451436399033,-0.134545057927369,
-0.335732649955417));
#83756=CARTESIAN_POINT('Ctrl Pts',(-0.130893495664707,-0.321974027223704,
-0.324163008879169));
#83757=CARTESIAN_POINT('Ctrl Pts',(0.199116261936156,-0.2848738263823,-0.308308688480176));
#83758=CARTESIAN_POINT('Ctrl Pts',(0.347345858346149,0.0122975804198618,
-0.292454368081194));
#83759=CARTESIAN_POINT('Ctrl Pts',(0.178471389733922,0.298242097044996,
-0.276600047682209));
#83760=CARTESIAN_POINT('Ctrl Pts',(-0.153335856191516,0.311911054555737,
-0.260745727283223));
#83761=CARTESIAN_POINT('Ctrl Pts',(-0.288773891993813,0.12050769107895,
-0.249551581958806));
#83762=CARTESIAN_POINT('Ctrl Pts',(-0.294606220383172,0.0116992042168328,
-0.243642210100719));
#83763=CARTESIAN_POINT('Ctrl Pts',(-0.294520052322006,0.000189243954005722,
-0.24301761170896));
#83764=CARTESIAN_POINT('',(-0.294169629819823,0.000115538129147393,-0.143017616992071));
#83765=CARTESIAN_POINT('Ctrl Pts',(-0.294199939266707,0.000189038265259436,
-0.24301761170896));
#83766=CARTESIAN_POINT('Ctrl Pts',(-0.294210413722791,-0.0161123403967751,
-0.242132035518253));
#83767=CARTESIAN_POINT('Ctrl Pts',(-0.292861724548747,-0.0324669545263656,
-0.241246459327547));
#83768=CARTESIAN_POINT('Ctrl Pts',(-0.290153646990399,-0.0486261363689395,
-0.24036088313684));
#83769=CARTESIAN_POINT('Ctrl Pts',(-0.287450020653816,-0.0647587576347344,
-0.239476762552899));
#83770=CARTESIAN_POINT('Ctrl Pts',(-0.283391515145389,-0.0806957786567614,
-0.238592641968958));
#83771=CARTESIAN_POINT('Ctrl Pts',(-0.278029686489317,-0.0961932088593155,
-0.237708521385016));
#83772=CARTESIAN_POINT('Ctrl Pts',(-0.272667312880232,-0.111692214153473,
-0.236824310942892));
#83773=CARTESIAN_POINT('Ctrl Pts',(-0.266001583678496,-0.126750759356636,
-0.235940100500768));
#83774=CARTESIAN_POINT('Ctrl Pts',(-0.25813384502719,-0.141140207068994,
-0.235055890058644));
#83775=CARTESIAN_POINT('Ctrl Pts',(-0.250265301789429,-0.155531126303888,
-0.234171589193621));
#83776=CARTESIAN_POINT('Ctrl Pts',(-0.241194924416618,-0.169252114418672,
-0.233287288328597));
#83777=CARTESIAN_POINT('Ctrl Pts',(-0.231068947211838,-0.182101020410136,
-0.232402987463573));
#83778=CARTESIAN_POINT('Ctrl Pts',(-0.220921403518602,-0.194977292232783,
-0.231516803198655));
#83779=CARTESIAN_POINT('Ctrl Pts',(-0.209714330199498,-0.206977181085204,
-0.230630618933737));
#83780=CARTESIAN_POINT('Ctrl Pts',(-0.197632477220963,-0.217933576916237,
-0.229744434668819));
#83781=CARTESIAN_POINT('Ctrl Pts',(-0.194417917489317,-0.220848691750443,
-0.229508651940963));
#83782=CARTESIAN_POINT('Ctrl Pts',(-0.191141609549977,-0.223690161447638,
-0.229272869213108));
#83783=CARTESIAN_POINT('Ctrl Pts',(-0.187807393754267,-0.226455344055356,
-0.229037086485253));
#83784=CARTESIAN_POINT('Ctrl Pts',(-0.175103930922266,-0.236990773263638,
-0.228138747174525));
#83785=CARTESIAN_POINT('Ctrl Pts',(-0.161470816744965,-0.246487426797759,
-0.227240407863797));
#83786=CARTESIAN_POINT('Ctrl Pts',(-0.14710335224885,-0.254782738342202,
-0.226342068553069));
#83787=CARTESIAN_POINT('Ctrl Pts',(-0.132763705733188,-0.263061988680128,
-0.225445468587887));
#83788=CARTESIAN_POINT('Ctrl Pts',(-0.117693175521697,-0.270144066179261,
-0.224548868622706));
#83789=CARTESIAN_POINT('Ctrl Pts',(-0.10211675364506,-0.275909058613512,
-0.223652268657524));
#83790=CARTESIAN_POINT('Ctrl Pts',(-0.0865430051706365,-0.281673061594365,
-0.222755822576999));
#83791=CARTESIAN_POINT('Ctrl Pts',(-0.0704642587339777,-0.286120105226655,
-0.221859376496474));
#83792=CARTESIAN_POINT('Ctrl Pts',(-0.054126121438416,-0.289178150934738,
-0.220962930415949));
#83793=CARTESIAN_POINT('Ctrl Pts',(-0.0377922871394121,-0.292235391241328,
-0.220066720433599));
#83794=CARTESIAN_POINT('Ctrl Pts',(-0.0211999773968291,-0.293904225111132,
-0.219170510451249));
#83795=CARTESIAN_POINT('Ctrl Pts',(-0.00460404081541506,-0.294163972654997,
-0.218274300468899));
#83796=CARTESIAN_POINT('Ctrl Pts',(0.012031496910059,-0.294424340007203,
-0.217375951954599));
#83797=CARTESIAN_POINT('Ctrl Pts',(0.0286698840294532,-0.293268919895812,
-0.2164776034403));
#83798=CARTESIAN_POINT('Ctrl Pts',(0.0450568278068779,-0.290729293790601,
-0.215579254926));
#83799=CARTESIAN_POINT('Ctrl Pts',(0.0596284286406299,-0.288471007048743,
-0.214780425312756));
#83800=CARTESIAN_POINT('Ctrl Pts',(0.074000894406622,-0.285119064062116,
-0.213981595699512));
#83801=CARTESIAN_POINT('Ctrl Pts',(0.0880045204636365,-0.28072912990633,
-0.213182766086268));
#83802=CARTESIAN_POINT('Ctrl Pts',(0.103752671668509,-0.275792312357557,
-0.212284420937299));
#83803=CARTESIAN_POINT('Ctrl Pts',(0.1191341754452,-0.269510533335221,-0.211386075788329));
#83804=CARTESIAN_POINT('Ctrl Pts',(0.133906420974025,-0.261959367883508,
-0.21048773063936));
#83805=CARTESIAN_POINT('Ctrl Pts',(0.148650064165126,-0.254422823159838,
-0.209591124885481));
#83806=CARTESIAN_POINT('Ctrl Pts',(0.162786064520269,-0.245622068074354,
-0.208694519131603));
#83807=CARTESIAN_POINT('Ctrl Pts',(0.176091476700562,-0.235680783759337,
-0.207797913377724));
#83808=CARTESIAN_POINT('Ctrl Pts',(0.189394602919401,-0.225741207425437,
-0.206901461666889));
#83809=CARTESIAN_POINT('Ctrl Pts',(0.201866761036284,-0.214661920754577,
-0.206005009956054));
#83810=CARTESIAN_POINT('Ctrl Pts',(0.21331398541005,-0.202609929738108,
-0.205108558245219));
#83811=CARTESIAN_POINT('Ctrl Pts',(0.224758193948028,-0.190561113886608,
-0.20421234270964));
#83812=CARTESIAN_POINT('Ctrl Pts',(0.235177467856935,-0.177540683728999,
-0.203316127174062));
#83813=CARTESIAN_POINT('Ctrl Pts',(0.244415928217322,-0.163751317654744,
-0.202419911638483));
#83814=CARTESIAN_POINT('Ctrl Pts',(0.253676430712878,-0.149929051393764,
-0.201521557813275));
#83815=CARTESIAN_POINT('Ctrl Pts',(0.261750072845164,-0.135334859899756,
-0.200623203988068));
#83816=CARTESIAN_POINT('Ctrl Pts',(0.268525145292401,-0.120199360837298,
-0.19972485016286));
#83817=CARTESIAN_POINT('Ctrl Pts',(0.274549428627597,-0.10674112323439,
-0.198926048671001));
#83818=CARTESIAN_POINT('Ctrl Pts',(0.279547545477995,-0.0928556306069915,
-0.198127247179142));
#83819=CARTESIAN_POINT('Ctrl Pts',(0.283473983847011,-0.0787155669604466,
-0.197328445687283));
#83820=CARTESIAN_POINT('Ctrl Pts',(0.287889753237969,-0.0628133027789086,
-0.19643009383614));
#83821=CARTESIAN_POINT('Ctrl Pts',(0.290977268887811,-0.0464877677436698,
-0.195531741984997));
#83822=CARTESIAN_POINT('Ctrl Pts',(0.29266810287148,-0.0299836882589333,
-0.194633390133854));
#83823=CARTESIAN_POINT('Ctrl Pts',(0.294355663284042,-0.0135115618093629,
-0.1937367775538));
#83824=CARTESIAN_POINT('Ctrl Pts',(0.294651764465417,0.00313765176718028,
-0.192840164973746));
#83825=CARTESIAN_POINT('Ctrl Pts',(0.29353904714589,0.0197095865173061,
-0.191943552393691));
#83826=CARTESIAN_POINT('Ctrl Pts',(0.292426520889953,0.0362786757169076,
-0.191047093770096));
#83827=CARTESIAN_POINT('Ctrl Pts',(0.289905656740242,0.0527697220904914,
-0.190150635146501));
#83828=CARTESIAN_POINT('Ctrl Pts',(0.286011213202392,0.0689291369632328,
-0.189254176522906));
#83829=CARTESIAN_POINT('Ctrl Pts',(0.282117795410594,0.0850842956551185,
-0.188357954014917));
#83830=CARTESIAN_POINT('Ctrl Pts',(0.276851712539556,0.100907229606026,
-0.187461731506927));
#83831=CARTESIAN_POINT('Ctrl Pts',(0.27029836736703,0.116156930911237,-0.186565508998938));
#83832=CARTESIAN_POINT('Ctrl Pts',(0.26372938699065,0.13144301549588,-0.185667148251433));
#83833=CARTESIAN_POINT('Ctrl Pts',(0.255867348588167,0.146152416636982,
-0.184768787503927));
#83834=CARTESIAN_POINT('Ctrl Pts',(0.24684511433834,0.160066016153623,-0.183870426756422));
#83835=CARTESIAN_POINT('Ctrl Pts',(0.238823098224119,0.172437133599555,
-0.18307165960038));
#83836=CARTESIAN_POINT('Ctrl Pts',(0.229884776593514,0.184179177484849,
-0.182272892444339));
#83837=CARTESIAN_POINT('Ctrl Pts',(0.220150343724061,0.19516010391004,-0.181474125288298));
#83838=CARTESIAN_POINT('Ctrl Pts',(0.209202719326891,0.207509570966636,
-0.18057580867115));
#83839=CARTESIAN_POINT('Ctrl Pts',(0.197177922521696,0.218974268614063,
-0.179677492054003));
#83840=CARTESIAN_POINT('Ctrl Pts',(0.184244161819628,0.229363747866533,
-0.178779175436855));
#83841=CARTESIAN_POINT('Ctrl Pts',(0.171335443855333,0.239733110695752,
-0.17788259816745));
#83842=CARTESIAN_POINT('Ctrl Pts',(0.157521823952818,0.249030846584296,
-0.176986020898045));
#83843=CARTESIAN_POINT('Ctrl Pts',(0.143007361014738,0.257104132008026,
-0.176089443628641));
#83844=CARTESIAN_POINT('Ctrl Pts',(0.128495383990392,0.265176034708109,
-0.175193019917363));
#83845=CARTESIAN_POINT('Ctrl Pts',(0.113283465872141,0.272023473939963,
-0.174296596206086));
#83846=CARTESIAN_POINT('Ctrl Pts',(0.0976033421864677,0.277537794892932,
-0.173400172494808));
#83847=CARTESIAN_POINT('Ctrl Pts',(0.0819273458496677,0.283050664356944,
-0.172503984741707));
#83848=CARTESIAN_POINT('Ctrl Pts',(0.0657841387658264,0.287230860039296,
-0.171607796988606));
#83849=CARTESIAN_POINT('Ctrl Pts',(0.049422423466539,0.290019075335906,
-0.170711609235505));
#83850=CARTESIAN_POINT('Ctrl Pts',(0.0330216522433993,0.292813946189243,
-0.169813282254335));
#83851=CARTESIAN_POINT('Ctrl Pts',(0.0164021187292266,0.294210093330215,
-0.168914955273163));
#83852=CARTESIAN_POINT('Ctrl Pts',(-0.000180052817078031,0.294199944903093,
-0.168016628291992));
#83853=CARTESIAN_POINT('Ctrl Pts',(-0.0149276661258505,0.294190919240895,
-0.167217687157766));
#83854=CARTESIAN_POINT('Ctrl Pts',(-0.0296452847826954,0.293070348302885,
-0.166418746023539));
#83855=CARTESIAN_POINT('Ctrl Pts',(-0.044156621559926,0.290867380041856,
-0.165619804889313));
#83856=CARTESIAN_POINT('Ctrl Pts',(-0.0604738211404214,0.288390263471789,
-0.164721439553274));
#83857=CARTESIAN_POINT('Ctrl Pts',(-0.0766337890607189,0.284527946234074,
-0.163823074217236));
#83858=CARTESIAN_POINT('Ctrl Pts',(-0.0923852179586884,0.279318118822832,
-0.162924708881197));
#83859=CARTESIAN_POINT('Ctrl Pts',(-0.10810614497223,0.274118379991783,
-0.162028083186422));
#83860=CARTESIAN_POINT('Ctrl Pts',(-0.123419340305597,0.267576493686629,
-0.161131457491645));
#83861=CARTESIAN_POINT('Ctrl Pts',(-0.138085594998159,0.259780692997006,
-0.160234831796869));
#83862=CARTESIAN_POINT('Ctrl Pts',(-0.152749319206812,0.251986237377996,
-0.159338360803954));
#83863=CARTESIAN_POINT('Ctrl Pts',(-0.166765603379859,0.242938620565314,
-0.158441889811039));
#83864=CARTESIAN_POINT('Ctrl Pts',(-0.179917271215686,0.232773313587064,
-0.157545418818124));
#83865=CARTESIAN_POINT('Ctrl Pts',(-0.193065469434417,0.222610688376883,
-0.156649184328374));
#83866=CARTESIAN_POINT('Ctrl Pts',(-0.205348884843153,0.211331450939192,
-0.155752949838626));
#83867=CARTESIAN_POINT('Ctrl Pts',(-0.216582540762771,0.199112136839377,
-0.154856715348876));
#83868=CARTESIAN_POINT('Ctrl Pts',(-0.227842986920704,0.186863681884695,
-0.153958343501909));
#83869=CARTESIAN_POINT('Ctrl Pts',(-0.238048155564684,0.173671275485725,
-0.153059971654942));
#83870=CARTESIAN_POINT('Ctrl Pts',(-0.247052460849956,0.15974580303714,
-0.152161599807974));
#83871=CARTESIAN_POINT('Ctrl Pts',(-0.255057814791698,0.14736524371301,
-0.151362894702092));
#83872=CARTESIAN_POINT('Ctrl Pts',(-0.262114403808015,0.134406053636018,
-0.15056418959621));
#83873=CARTESIAN_POINT('Ctrl Pts',(-0.268150931039178,0.121031889115316,
-0.149765484490327));
#83874=CARTESIAN_POINT('Ctrl Pts',(-0.275566463726504,0.1046024835364,-0.148784320388287));
#83875=CARTESIAN_POINT('Ctrl Pts',(-0.281483199746428,0.087456415148466,
-0.147803156286247));
#83876=CARTESIAN_POINT('Ctrl Pts',(-0.285782874348049,0.0698697984065166,
-0.146821992184207));
#83877=CARTESIAN_POINT('Ctrl Pts',(-0.290055134026178,0.0523953147437289,
-0.145847084029717));
#83878=CARTESIAN_POINT('Ctrl Pts',(-0.292730644909085,0.0344863793794888,
-0.144872175875227));
#83879=CARTESIAN_POINT('Ctrl Pts',(-0.293740628263162,0.0164342114980555,
-0.143897267720738));
#83880=CARTESIAN_POINT('Ctrl Pts',(-0.294044394380078,0.0110047785107428,
-0.14360405094321));
#83881=CARTESIAN_POINT('Ctrl Pts',(-0.29419783782663,0.0055625008341258,
-0.143310834165682));
#83882=CARTESIAN_POINT('Ctrl Pts',(-0.294199977305384,0.0001155573961467,
-0.143017617388154));
#83883=CARTESIAN_POINT('',(-0.294174533184472,-0.000257752421235655,-0.0430176117089602));
#83884=CARTESIAN_POINT('Ctrl Pts',(-0.293764843131769,0.000115281138339288,
-0.143017611708961));
#83885=CARTESIAN_POINT('Ctrl Pts',(-0.293566552975499,-0.0561900665379691,
-0.139982129169754));
#83886=CARTESIAN_POINT('Ctrl Pts',(-0.250873929139425,-0.210802370330722,
-0.13166187316422));
#83887=CARTESIAN_POINT('Ctrl Pts',(-0.000847465076883103,-0.347563185600196,
-0.118056843692358));
#83888=CARTESIAN_POINT('Ctrl Pts',(0.29125633667054,-0.189629242622781,
-0.10220252329337));
#83889=CARTESIAN_POINT('Ctrl Pts',(0.317524590866241,0.141418773562067,
-0.0863482028943878));
#83890=CARTESIAN_POINT('Ctrl Pts',(0.0537942024322259,0.343370337337008,
-0.0704938824954019));
#83891=CARTESIAN_POINT('Ctrl Pts',(-0.231000450644502,0.241754108313963,
-0.05605035210026));
#83892=CARTESIAN_POINT('Ctrl Pts',(-0.293533922271702,0.0713929714457434,
-0.0468915951714457));
#83893=CARTESIAN_POINT('Ctrl Pts',(-0.294174533184472,-0.000257752421235655,
-0.0430176117089602));
#83894=CARTESIAN_POINT('',(-0.288931858183476,-0.0555073112399963,-0.0399923557954013));
#83895=CARTESIAN_POINT('Origin',(0.000858682044037384,0.000109768145102293,
-0.0410035060336729));
#83896=CARTESIAN_POINT('',(-0.2942,-3.60291088309151E-17,-0.04));
#83897=CARTESIAN_POINT('Origin',(0.,0.,-0.04));
#83898=CARTESIAN_POINT('',(-0.221686865784456,0.19341296114445,-0.0399999999999998));
#83899=CARTESIAN_POINT('Origin',(0.,0.,-0.04));
#83900=CARTESIAN_POINT('',(-0.294104385983628,0.00013338358664356,-0.1285823930633));
#83901=CARTESIAN_POINT('Ctrl Pts',(-0.221686865784456,0.19341296114445,
-0.0399999999999998));
#83902=CARTESIAN_POINT('Ctrl Pts',(-0.157463683943977,0.267024552677283,
-0.0452847734663282));
#83903=CARTESIAN_POINT('Ctrl Pts',(0.0489519852740736,0.343994364943719,
-0.0558543203989852));
#83904=CARTESIAN_POINT('Ctrl Pts',(0.315889904847724,0.145505811952091,
-0.0717086407979697));
#83905=CARTESIAN_POINT('Ctrl Pts',(0.293560564371313,-0.185886097454744,
-0.0875629611969554));
#83906=CARTESIAN_POINT('Ctrl Pts',(0.00367026792673841,-0.34753924213355,
-0.10341728159594));
#83907=CARTESIAN_POINT('Ctrl Pts',(-0.249424653403535,-0.213339276299583,
-0.117090423960635));
#83908=CARTESIAN_POINT('Ctrl Pts',(-0.29355313769381,-0.0574282297979894,
-0.125478792859001));
#83909=CARTESIAN_POINT('Ctrl Pts',(-0.293784724436548,0.000133150074073662,
-0.128582388291039));
#83910=CARTESIAN_POINT('',(-0.294199949415823,0.000172521672589196,-0.228582388287483));
#83911=CARTESIAN_POINT('Ctrl Pts',(-0.294199969731792,0.000133453410514708,
-0.12858239449028));
#83912=CARTESIAN_POINT('Ctrl Pts',(-0.294191701222119,0.0183615023300105,
-0.129563829546113));
#83913=CARTESIAN_POINT('Ctrl Pts',(-0.292485195566189,0.0365335283349674,
-0.130545264601945));
#83914=CARTESIAN_POINT('Ctrl Pts',(-0.289136128846234,0.0543501517552088,
-0.131526699657778));
#83915=CARTESIAN_POINT('Ctrl Pts',(-0.285763463296785,0.0722923180485561,
-0.132515050287553));
#83916=CARTESIAN_POINT('Ctrl Pts',(-0.280725230354817,0.0898735663263774,
-0.133503400917329));
#83917=CARTESIAN_POINT('Ctrl Pts',(-0.274127512705431,0.106807053970858,
-0.134491751547104));
#83918=CARTESIAN_POINT('Ctrl Pts',(-0.272716380507792,0.110428819997125,
-0.134703141829373));
#83919=CARTESIAN_POINT('Ctrl Pts',(-0.27123407947722,0.11402103739158,-0.134914532111641));
#83920=CARTESIAN_POINT('Ctrl Pts',(-0.269681920613827,0.117581043089598,
-0.13512592239391));
#83921=CARTESIAN_POINT('Ctrl Pts',(-0.263084384787075,0.132713041295475,
-0.136024448307453));
#83922=CARTESIAN_POINT('Ctrl Pts',(-0.255188419008939,0.147335891811453,
-0.136922974220996));
#83923=CARTESIAN_POINT('Ctrl Pts',(-0.246095307587498,0.161216437075798,
-0.137821500134539));
#83924=CARTESIAN_POINT('Ctrl Pts',(-0.237019737980359,0.175070204932921,
-0.138718292672784));
#83925=CARTESIAN_POINT('Ctrl Pts',(-0.2267519806427,0.188183820408594,-0.139615085211028));
#83926=CARTESIAN_POINT('Ctrl Pts',(-0.215439029375543,0.200348857300769,
-0.140511877749273));
#83927=CARTESIAN_POINT('Ctrl Pts',(-0.20412793911738,0.212511893013718,
-0.141408522762885));
#83928=CARTESIAN_POINT('Ctrl Pts',(-0.191772494739143,0.2237260470423,-0.142305167776498));
#83929=CARTESIAN_POINT('Ctrl Pts',(-0.178559646876333,0.233816364926408,
-0.14320181279011));
#83930=CARTESIAN_POINT('Ctrl Pts',(-0.165350221551189,0.243904069105025,
-0.144098225544835));
#83931=CARTESIAN_POINT('Ctrl Pts',(-0.151284469005638,0.252868043929967,
-0.144994638299561));
#83932=CARTESIAN_POINT('Ctrl Pts',(-0.136580711609862,0.260575035673304,
-0.145891051054287));
#83933=CARTESIAN_POINT('Ctrl Pts',(-0.121841840425093,0.268300432350466,
-0.146789604516824));
#83934=CARTESIAN_POINT('Ctrl Pts',(-0.106462637101275,0.274762505820998,
-0.147688157979362));
#83935=CARTESIAN_POINT('Ctrl Pts',(-0.0906844573864716,0.279874917040669,
-0.148586711441899));
#83936=CARTESIAN_POINT('Ctrl Pts',(-0.0766746926614438,0.284414330310121,
-0.149384555225565));
#83937=CARTESIAN_POINT('Ctrl Pts',(-0.0623510382474998,0.287890292128622,
-0.15018239900923));
#83938=CARTESIAN_POINT('Ctrl Pts',(-0.0478893678051186,0.290276158943903,
-0.150980242792895));
#83939=CARTESIAN_POINT('Ctrl Pts',(-0.0316092376920983,0.292962032774307,
-0.151878410169872));
#83940=CARTESIAN_POINT('Ctrl Pts',(-0.0150504980546004,0.294282606115574,
-0.152776577546849));
#83941=CARTESIAN_POINT('Ctrl Pts',(0.001536311502479,0.294195988665664,
-0.153674744923825));
#83942=CARTESIAN_POINT('Ctrl Pts',(0.0180909301430988,0.294109539318913,
-0.154571169178902));
#83943=CARTESIAN_POINT('Ctrl Pts',(0.0346727279743466,0.292621258171847,
-0.155467593433978));
#83944=CARTESIAN_POINT('Ctrl Pts',(0.0510270319741756,0.289741060272628,
-0.156364017689054));
#83945=CARTESIAN_POINT('Ctrl Pts',(0.0673784699368128,0.286861367118478,
-0.157260284848771));
#83946=CARTESIAN_POINT('Ctrl Pts',(0.0835017070694002,0.282590326317674,
-0.158156552008489));
#83947=CARTESIAN_POINT('Ctrl Pts',(0.099148411371516,0.276989589195162,
-0.159052819168206));
#83948=CARTESIAN_POINT('Ctrl Pts',(0.114790957672683,0.271390340428908,
-0.159948848151268));
#83949=CARTESIAN_POINT('Ctrl Pts',(0.129956480907957,0.264462373902354,
-0.16084487713433));
#83950=CARTESIAN_POINT('Ctrl Pts',(0.144414573058269,0.256316349631462,
-0.161740906117392));
#83951=CARTESIAN_POINT('Ctrl Pts',(0.158907177420407,0.248150880380399,
-0.162639073967861));
#83952=CARTESIAN_POINT('Ctrl Pts',(0.17268829868724,0.238761959669275,-0.163537241818329));
#83953=CARTESIAN_POINT('Ctrl Pts',(0.185554371171481,0.228305092670217,
-0.164435409668798));
#83954=CARTESIAN_POINT('Ctrl Pts',(0.197010167216985,0.218994424184329,
-0.165235127509825));
#83955=CARTESIAN_POINT('Ctrl Pts',(0.207740673292139,0.208837991528443,
-0.166034845350853));
#83956=CARTESIAN_POINT('Ctrl Pts',(0.21762704093381,0.197969975133588,-0.16683456319188));
#83957=CARTESIAN_POINT('Ctrl Pts',(0.228733260419431,0.185760983941939,
-0.167732956028454));
#83958=CARTESIAN_POINT('Ctrl Pts',(0.238844159081668,0.17257571088313,-0.168631348865028));
#83959=CARTESIAN_POINT('Ctrl Pts',(0.247788404176165,0.15860184978691,-0.169529741701603));
#83960=CARTESIAN_POINT('Ctrl Pts',(0.256715337775117,0.144655034956926,
-0.170426395707966));
#83961=CARTESIAN_POINT('Ctrl Pts',(0.264479623162017,0.129923284883128,
-0.171323049714328));
#83962=CARTESIAN_POINT('Ctrl Pts',(0.270951181620278,0.114625900993516,
-0.172219703720691));
#83963=CARTESIAN_POINT('Ctrl Pts',(0.277421629308804,0.0993311427266418,
-0.173116203826547));
#83964=CARTESIAN_POINT('Ctrl Pts',(0.282599434943443,0.0834716491056846,
-0.174012703932402));
#83965=CARTESIAN_POINT('Ctrl Pts',(0.286401401731565,0.0672895020504313,
-0.174909204038257));
#83966=CARTESIAN_POINT('Ctrl Pts',(0.290202367615189,0.0511116151017642,
-0.175805468131796));
#83967=CARTESIAN_POINT('Ctrl Pts',(0.292628043471786,0.0346120160572335,
-0.176701732225335));
#83968=CARTESIAN_POINT('Ctrl Pts',(0.293646114971536,0.0180443664927103,
-0.177597996318874));
#83969=CARTESIAN_POINT('Ctrl Pts',(0.294666614501627,0.00143720422616354,
-0.178496397940487));
#83970=CARTESIAN_POINT('Ctrl Pts',(0.294272782802821,-0.015237538264258,
-0.1793947995621));
#83971=CARTESIAN_POINT('Ctrl Pts',(0.292484537501183,-0.0317243648119074,
-0.180293201183713));
#83972=CARTESIAN_POINT('Ctrl Pts',(0.29089502278017,-0.0463789837706543,
-0.181091761986097));
#83973=CARTESIAN_POINT('Ctrl Pts',(0.288204638700452,-0.0608847794893923,
-0.181890322788482));
#83974=CARTESIAN_POINT('Ctrl Pts',(0.284461167510929,-0.0750698619841497,
-0.182688883590866));
#83975=CARTESIAN_POINT('Ctrl Pts',(0.280249847676779,-0.0910277567387323,
-0.183587246307071));
#83976=CARTESIAN_POINT('Ctrl Pts',(0.274678143546929,-0.106680871673802,
-0.184485609023275));
#83977=CARTESIAN_POINT('Ctrl Pts',(0.267810467978768,-0.121783386555775,
-0.18538397173948));
#83978=CARTESIAN_POINT('Ctrl Pts',(0.26095608348652,-0.136856673401306,
-0.186280595846029));
#83979=CARTESIAN_POINT('Ctrl Pts',(0.25281096995915,-0.151380736369602,
-0.187177219952578));
#83980=CARTESIAN_POINT('Ctrl Pts',(0.24348849462934,-0.16512720243236,-0.188073844059127));
#83981=CARTESIAN_POINT('Ctrl Pts',(0.234167611168175,-0.178871321203489,
-0.188970315061725));
#83982=CARTESIAN_POINT('Ctrl Pts',(0.223670164123284,-0.19183742451964,
-0.189866786064323));
#83983=CARTESIAN_POINT('Ctrl Pts',(0.212154124729109,-0.203824108879263,
-0.190763257066921));
#83984=CARTESIAN_POINT('Ctrl Pts',(0.200641112176925,-0.215807642693953,
-0.191659492443713));
#83985=CARTESIAN_POINT('Ctrl Pts',(0.188110594892172,-0.22681170567809,
-0.192555727820504));
#83986=CARTESIAN_POINT('Ctrl Pts',(0.17475791996057,-0.236671310916755,
-0.193451963197295));
#83987=CARTESIAN_POINT('Ctrl Pts',(0.161373379956778,-0.246554445301025,
-0.194350337366885));
#83988=CARTESIAN_POINT('Ctrl Pts',(0.147163418609258,-0.255287216820715,
-0.195248711536474));
#83989=CARTESIAN_POINT('Ctrl Pts',(0.132353312221677,-0.262747484752854,
-0.196147085706064));
#83990=CARTESIAN_POINT('Ctrl Pts',(0.119186279337399,-0.269380090260021,
-0.196945791800659));
#83991=CARTESIAN_POINT('Ctrl Pts',(0.105545630605282,-0.275007390975032,
-0.197744497895255));
#83992=CARTESIAN_POINT('Ctrl Pts',(0.0916017203586297,-0.279576044802375,
-0.198543203989851));
#83993=CARTESIAN_POINT('Ctrl Pts',(0.075918771298104,-0.284714486170827,
-0.199441522092471));
#83994=CARTESIAN_POINT('Ctrl Pts',(0.0597522313714575,-0.288545548764624,
-0.20033984019509));
#83995=CARTESIAN_POINT('Ctrl Pts',(0.0433434185875271,-0.290989670031681,
-0.20123815829771));
#83996=CARTESIAN_POINT('Ctrl Pts',(0.0269663873069511,-0.293429057388413,
-0.20213473648775));
#83997=CARTESIAN_POINT('Ctrl Pts',(0.0103487783849169,-0.294486655384115,
-0.20303131467779));
#83998=CARTESIAN_POINT('Ctrl Pts',(-0.00625612079583699,-0.294133474722936,
-0.203927892867829));
#83999=CARTESIAN_POINT('Ctrl Pts',(-0.022858159815875,-0.29378035489642,
-0.204824316624066));
#84000=CARTESIAN_POINT('Ctrl Pts',(-0.0394467038434414,-0.292016902995582,
-0.205720740380304));
#84001=CARTESIAN_POINT('Ctrl Pts',(-0.055766854845611,-0.288866228383708,
-0.206617164136541));
#84002=CARTESIAN_POINT('Ctrl Pts',(-0.072082701278467,-0.285716384787261,
-0.2075133514539));
#84003=CARTESIAN_POINT('Ctrl Pts',(-0.0881295203357389,-0.281180205650575,
-0.208409538771259));
#84004=CARTESIAN_POINT('Ctrl Pts',(-0.103662662809,-0.275331967521658,-0.209305726088618));
#84005=CARTESIAN_POINT('Ctrl Pts',(-0.119232869743055,-0.269469774599421,
-0.210204051846396));
#84006=CARTESIAN_POINT('Ctrl Pts',(-0.134286217966099,-0.262289574713627,
-0.211102377604173));
#84007=CARTESIAN_POINT('Ctrl Pts',(-0.148597752722107,-0.253914056101547,
-0.212000703361951));
#84008=CARTESIAN_POINT('Ctrl Pts',(-0.161325944447373,-0.246465155022065,
-0.212799643704246));
#84009=CARTESIAN_POINT('Ctrl Pts',(-0.173467401274235,-0.238071699307785,
-0.213598584046541));
#84010=CARTESIAN_POINT('Ctrl Pts',(-0.184884624867529,-0.228847799831227,
-0.214397524388836));
#84011=CARTESIAN_POINT('Ctrl Pts',(-0.197558202061853,-0.21860890058452,
-0.215284380288521));
#84012=CARTESIAN_POINT('Ctrl Pts',(-0.209423871849072,-0.207277209066597,
-0.216171236188206));
#84013=CARTESIAN_POINT('Ctrl Pts',(-0.220286301231099,-0.195006629348649,
-0.217058092087892));
#84014=CARTESIAN_POINT('Ctrl Pts',(-0.231127668029687,-0.182759842660794,
-0.21794322834681));
#84015=CARTESIAN_POINT('Ctrl Pts',(-0.240969068641305,-0.169578334548641,
-0.218828364605729));
#84016=CARTESIAN_POINT('Ctrl Pts',(-0.24965079348673,-0.15565385093677,
-0.219713500864648));
#84017=CARTESIAN_POINT('Ctrl Pts',(-0.25832987956455,-0.141733599603267,
-0.220598368090751));
#84018=CARTESIAN_POINT('Ctrl Pts',(-0.265849521406037,-0.1270714842788,
-0.221483235316853));
#84019=CARTESIAN_POINT('Ctrl Pts',(-0.272092843718152,-0.111888893092072,
-0.222368102542956));
#84020=CARTESIAN_POINT('Ctrl Pts',(-0.278335182273219,-0.0967086942183384,
-0.22325283034099));
#84021=CARTESIAN_POINT('Ctrl Pts',(-0.283301309523408,-0.0810089409982683,
-0.224137558139024));
#84022=CARTESIAN_POINT('Ctrl Pts',(-0.286922867717612,-0.0650300544417854,
-0.225022285937058));
#84023=CARTESIAN_POINT('Ctrl Pts',(-0.290551131806588,-0.0490215804187825,
-0.225908651950246));
#84024=CARTESIAN_POINT('Ctrl Pts',(-0.292829730847923,-0.0327337450470522,
-0.226795017963435));
#84025=CARTESIAN_POINT('Ctrl Pts',(-0.293741661854769,-0.0164157269348249,
-0.227681383976623));
#84026=CARTESIAN_POINT('Ctrl Pts',(-0.294050659024542,-0.0108865571016537,
-0.22798171874691));
#84027=CARTESIAN_POINT('Ctrl Pts',(-0.294203190180107,-0.00535393001506612,
-0.228282053517196));
#84028=CARTESIAN_POINT('Ctrl Pts',(-0.294199949415822,0.000172521672587396,
-0.228582388287483));
#84029=CARTESIAN_POINT('',(-0.294199886004729,-0.000258988038798538,-0.328582388295919));
#84030=CARTESIAN_POINT('Ctrl Pts',(-0.294199949415784,0.000172521738035792,
-0.22858238829104));
#84031=CARTESIAN_POINT('Ctrl Pts',(-0.294193944653124,0.010412395801695,
-0.229138873789967));
#84032=CARTESIAN_POINT('Ctrl Pts',(-0.293653364929884,0.0206363609331256,
-0.229695359288894));
#84033=CARTESIAN_POINT('Ctrl Pts',(-0.292582944662443,0.0308035792182318,
-0.230251844787821));
#84034=CARTESIAN_POINT('Ctrl Pts',(-0.290854945465596,0.0472167073747313,
-0.231150189601024));
#84035=CARTESIAN_POINT('Ctrl Pts',(-0.28773605490522,0.0635361486740394,
-0.232048534414226));
#84036=CARTESIAN_POINT('Ctrl Pts',(-0.283252424887927,0.0795091428397342,
-0.232946879227429));
#84037=CARTESIAN_POINT('Ctrl Pts',(-0.278777475512749,0.0954512120974134,
-0.233843484778072));
#84038=CARTESIAN_POINT('Ctrl Pts',(-0.27294317949145,0.111047395018861,
-0.234740090328715));
#84039=CARTESIAN_POINT('Ctrl Pts',(-0.265826731931281,0.126054704754464,
-0.235636695879358));
#84040=CARTESIAN_POINT('Ctrl Pts',(-0.25871150539682,0.141059439566153,
-0.23653314759223));
#84041=CARTESIAN_POINT('Ctrl Pts',(-0.250314854427535,0.155474766692411,
-0.237429599305103));
#84042=CARTESIAN_POINT('Ctrl Pts',(-0.240762170601427,0.169077547910092,
-0.238326051017975));
#84043=CARTESIAN_POINT('Ctrl Pts',(-0.231212002282678,0.182676747108638,
-0.2392222666683));
#84044=CARTESIAN_POINT('Ctrl Pts',(-0.220506869199112,0.19546318396303,
-0.240118482318625));
#84045=CARTESIAN_POINT('Ctrl Pts',(-0.208814657038346,0.207244008371672,
-0.241014697968949));
#84046=CARTESIAN_POINT('Ctrl Pts',(-0.197094545909162,0.219052943187789,
-0.24191305209331));
#84047=CARTESIAN_POINT('Ctrl Pts',(-0.184383230203443,0.229850928152899,
-0.24281140621767));
#84048=CARTESIAN_POINT('Ctrl Pts',(-0.170884710868931,0.239482892063801,
-0.243709760342031));
#84049=CARTESIAN_POINT('Ctrl Pts',(-0.158882050947728,0.24804747491403,
-0.244508561956956));
#84050=CARTESIAN_POINT('Ctrl Pts',(-0.146257812316769,0.255690536204456,
-0.245307363571881));
#84051=CARTESIAN_POINT('Ctrl Pts',(-0.133172282886074,0.262333343421898,
-0.246106165186807));
#84052=CARTESIAN_POINT('Ctrl Pts',(-0.118456177850664,0.269803904644476,
-0.247004504725146));
#84053=CARTESIAN_POINT('Ctrl Pts',(-0.103062719738412,0.276056066664602,
-0.247902844263485));
#84054=CARTESIAN_POINT('Ctrl Pts',(-0.0872182828589932,0.280974395871098,
-0.248801183801824));
#84055=CARTESIAN_POINT('Ctrl Pts',(-0.0714045251525122,0.285883201844082,
-0.249697783908572));
#84056=CARTESIAN_POINT('Ctrl Pts',(-0.0551422493111504,0.289463006917553,
-0.25059438401532));
#84057=CARTESIAN_POINT('Ctrl Pts',(-0.0386773703079941,0.291646534397476,
-0.251490984122068));
#84058=CARTESIAN_POINT('Ctrl Pts',(-0.0222153196436664,0.293829686790796,
-0.252387430210746));
#84059=CARTESIAN_POINT('Ctrl Pts',(-0.00555150976642623,0.294616881939503,
-0.253283876299423));
#84060=CARTESIAN_POINT('Ctrl Pts',(0.0110586081036425,0.293992086945908,
-0.254180322388101));
#84061=CARTESIAN_POINT('Ctrl Pts',(0.0276643499883317,0.293367456556428,
-0.255076532305367));
#84062=CARTESIAN_POINT('Ctrl Pts',(0.0442156376475864,0.291331615258301,
-0.255972742222633));
#84063=CARTESIAN_POINT('Ctrl Pts',(0.0604593459098051,0.287920661801404,
-0.256868952139899));
#84064=CARTESIAN_POINT('Ctrl Pts',(0.0767418126579441,0.284501569599992,
-0.257767300469091));
#84065=CARTESIAN_POINT('Ctrl Pts',(0.0927144622668592,0.279701001499387,
-0.258665648798282));
#84066=CARTESIAN_POINT('Ctrl Pts',(0.108136250535384,0.273605905126605,
-0.259563997127474));
#84067=CARTESIAN_POINT('Ctrl Pts',(0.121849616272327,0.268186022276024,
-0.26036282661358));
#84068=CARTESIAN_POINT('Ctrl Pts',(0.135127289411086,0.261743441032272,
-0.261161656099686));
#84069=CARTESIAN_POINT('Ctrl Pts',(0.147816043666688,0.254369922032318,
-0.261960485585791));
#84070=CARTESIAN_POINT('Ctrl Pts',(0.162085511569116,0.24607783988002,-0.262858830015976));
#84071=CARTESIAN_POINT('Ctrl Pts',(0.175700419929859,0.236554944148342,
-0.26375717444616));
#84072=CARTESIAN_POINT('Ctrl Pts',(0.18844083243448,0.225928512302897,-0.264655518876344));
#84073=CARTESIAN_POINT('Ctrl Pts',(0.201156577624219,0.215322654794453,
-0.265552123979413));
#84074=CARTESIAN_POINT('Ctrl Pts',(0.213000545222434,0.203617952657063,
-0.266448729082483));
#84075=CARTESIAN_POINT('Ctrl Pts',(0.223782600749857,0.190984260088705,
-0.267345334185551));
#84076=CARTESIAN_POINT('Ctrl Pts',(0.234562805187525,0.178352736503693,
-0.268241785357256));
#84077=CARTESIAN_POINT('Ctrl Pts',(0.244280907548326,0.164793104827646,
-0.26913823652896));
#84078=CARTESIAN_POINT('Ctrl Pts',(0.252784603828789,0.150511076227374,
-0.270034687700664));
#84079=CARTESIAN_POINT('Ctrl Pts',(0.261286060333827,0.136232809348548,
-0.27093090275748));
#84080=CARTESIAN_POINT('Ctrl Pts',(0.268573350408997,0.121233208783969,
-0.271827117814295));
#84081=CARTESIAN_POINT('Ctrl Pts',(0.27453919317641,0.10574436821905,-0.27272333287111));
#84082=CARTESIAN_POINT('Ctrl Pts',(0.280519270637902,0.0902185707788522,
-0.27362168632608));
#84083=CARTESIAN_POINT('Ctrl Pts',(0.285171342869688,0.0742019527911405,
-0.27452003978105));
#84084=CARTESIAN_POINT('Ctrl Pts',(0.288437377398787,0.057944105129944,
-0.275418393236019));
#84085=CARTESIAN_POINT('Ctrl Pts',(0.291341492974571,0.0434878376897345,
-0.276217197485605));
#84086=CARTESIAN_POINT('Ctrl Pts',(0.293150424617141,0.0288414314146981,
-0.277016001735191));
#84087=CARTESIAN_POINT('Ctrl Pts',(0.293857911790558,0.0141833591963492,
-0.277814805984776));
#84088=CARTESIAN_POINT('Ctrl Pts',(0.29465355880314,-0.00230125255203541,
-0.278713149076639));
#84089=CARTESIAN_POINT('Ctrl Pts',(0.294060305604828,-0.018905423218435,
-0.279611492168502));
#84090=CARTESIAN_POINT('Ctrl Pts',(0.292065444299675,-0.0353753621328946,
-0.280509835260364));
#84091=CARTESIAN_POINT('Ctrl Pts',(0.290074445374746,-0.0518134125315055,
-0.281406439011962));
#84092=CARTESIAN_POINT('Ctrl Pts',(0.286687253816457,-0.0681169628772702,
-0.282303042763559));
#84093=CARTESIAN_POINT('Ctrl Pts',(0.28194309840091,-0.0840340958426677,
-0.283199646515156));
#84094=CARTESIAN_POINT('Ctrl Pts',(0.277199757474612,-0.099948496112248,
-0.284096096335432));
#84095=CARTESIAN_POINT('Ctrl Pts',(0.271100090040711,-0.115475839928488,
-0.284992546155707));
#84096=CARTESIAN_POINT('Ctrl Pts',(0.263733984905181,-0.130376474894951,
-0.285888995975982));
#84097=CARTESIAN_POINT('Ctrl Pts',(0.256369819938901,-0.145273185161287,
-0.286785209679022));
#84098=CARTESIAN_POINT('Ctrl Pts',(0.247740240005153,-0.159542809832304,
-0.287681423382063));
#84099=CARTESIAN_POINT('Ctrl Pts',(0.237981750640039,-0.172969148585238,
-0.288577637085103));
#84100=CARTESIAN_POINT('Ctrl Pts',(0.228199976897607,-0.186427523437801,
-0.289475989211135));
#84101=CARTESIAN_POINT('Ctrl Pts',(0.21728440252953,-0.199037966770191,
-0.290374341337167));
#84102=CARTESIAN_POINT('Ctrl Pts',(0.205412988136211,-0.210616106470879,
-0.291272693463199));
#84103=CARTESIAN_POINT('Ctrl Pts',(0.194856975840137,-0.220911340130224,
-0.29207150443672));
#84104=CARTESIAN_POINT('Ctrl Pts',(0.183546081686859,-0.230390622836365,
-0.29287031541024));
#84105=CARTESIAN_POINT('Ctrl Pts',(0.171626714977173,-0.238951691155648,
-0.293669126383761));
#84106=CARTESIAN_POINT('Ctrl Pts',(0.158222199756597,-0.248579465297118,
-0.294567468897565));
#84107=CARTESIAN_POINT('Ctrl Pts',(0.143962416157296,-0.25710639961715,
-0.295465811411368));
#84108=CARTESIAN_POINT('Ctrl Pts',(0.129053485385659,-0.26438388360453,
-0.296364153925172));
#84109=CARTESIAN_POINT('Ctrl Pts',(0.114173421130027,-0.271647277003442,
-0.297260757077585));
#84110=CARTESIAN_POINT('Ctrl Pts',(0.0986473784290514,-0.277665619974595,
-0.298157360229998));
#84111=CARTESIAN_POINT('Ctrl Pts',(0.0827081353827211,-0.282334915200925,
-0.299053963382412));
#84112=CARTESIAN_POINT('Ctrl Pts',(0.0667716292524032,-0.287003408665915,
-0.29995041257974));
#84113=CARTESIAN_POINT('Ctrl Pts',(0.0504228056499476,-0.290323042082076,
-0.300846861777067));
#84114=CARTESIAN_POINT('Ctrl Pts',(0.0339116830863558,-0.292239007920316,
-0.301743310974395));
#84115=CARTESIAN_POINT('Ctrl Pts',(0.017404909675056,-0.294154469078927,
-0.302639524040348));
#84116=CARTESIAN_POINT('Ctrl Pts',(0.000736709434253774,-0.294666916399377,
-0.3035357371063));
#84117=CARTESIAN_POINT('Ctrl Pts',(-0.0158372467384842,-0.293773418837962,
-0.304431950172253));
#84118=CARTESIAN_POINT('Ctrl Pts',(-0.032450749263123,-0.292877789343251,
-0.30533030165084));
#84119=CARTESIAN_POINT('Ctrl Pts',(-0.0489687667855883,-0.290569584354962,
-0.306228653129427));
#84120=CARTESIAN_POINT('Ctrl Pts',(-0.0651398124002172,-0.286897969390626,
-0.307127004608014));
#84121=CARTESIAN_POINT('Ctrl Pts',(-0.0795191047834089,-0.283633169677061,
-0.307925818666258));
#84122=CARTESIAN_POINT('Ctrl Pts',(-0.0936237990135215,-0.279291226420072,
-0.308724632724502));
#84123=CARTESIAN_POINT('Ctrl Pts',(-0.107288476053316,-0.273939451167876,
-0.309523446782746));
#84124=CARTESIAN_POINT('Ctrl Pts',(-0.122655719149766,-0.267920865360209,
-0.310421789991748));
#84125=CARTESIAN_POINT('Ctrl Pts',(-0.137563795122085,-0.260586033187026,
-0.31132013320075));
#84126=CARTESIAN_POINT('Ctrl Pts',(-0.151775928281638,-0.252027196140113,
-0.312218476409752));
#84127=CARTESIAN_POINT('Ctrl Pts',(-0.165960544325783,-0.243484930462476,
-0.313115080272979));
#84128=CARTESIAN_POINT('Ctrl Pts',(-0.179451188460889,-0.233723711154993,
-0.314011684136206));
#84129=CARTESIAN_POINT('Ctrl Pts',(-0.192034043964477,-0.222882403878478,
-0.314908287999433));
#84130=CARTESIAN_POINT('Ctrl Pts',(-0.204614739066192,-0.212042957990307,
-0.315804737921079));
#84131=CARTESIAN_POINT('Ctrl Pts',(-0.216287323190704,-0.200124267192905,
-0.316701187842726));
#84132=CARTESIAN_POINT('Ctrl Pts',(-0.226869898260171,-0.187306404758139,
-0.317597637764372));
#84133=CARTESIAN_POINT('Ctrl Pts',(-0.237449685905562,-0.174491918516607,
-0.318493851563328));
#84134=CARTESIAN_POINT('Ctrl Pts',(-0.246939539186348,-0.160779348005506,
-0.319390065362285));
#84135=CARTESIAN_POINT('Ctrl Pts',(-0.255198032299019,-0.146381707568634,
-0.320286279161241));
#84136=CARTESIAN_POINT('Ctrl Pts',(-0.263476230596468,-0.131949713629094,
-0.321184631371923));
#84137=CARTESIAN_POINT('Ctrl Pts',(-0.270516828579833,-0.11683008743659,
-0.322082983582605));
#84138=CARTESIAN_POINT('Ctrl Pts',(-0.276224403826267,-0.101260647493601,
-0.322981335793287));
#84139=CARTESIAN_POINT('Ctrl Pts',(-0.281299552270207,-0.0874163764173602,
-0.323780146256102));
#84140=CARTESIAN_POINT('Ctrl Pts',(-0.285321315774006,-0.0732171408516279,
-0.324578956718916));
#84141=CARTESIAN_POINT('Ctrl Pts',(-0.288256284627069,-0.0588383750030366,
-0.325377767181731));
#84142=CARTESIAN_POINT('Ctrl Pts',(-0.292181063440704,-0.0396104109618327,
-0.326445974218167));
#84143=CARTESIAN_POINT('Ctrl Pts',(-0.294182527786001,-0.0199772121636394,
-0.327514181254603));
#84144=CARTESIAN_POINT('Ctrl Pts',(-0.29419988600465,-0.000258988128887952,
-0.328582388291039));
#84145=CARTESIAN_POINT('',(-0.29415272857916,1.53286667352925E-5,-0.428582389436499));
#84146=CARTESIAN_POINT('Ctrl Pts',(-0.294199886004729,-0.000258988038800302,
-0.328582388295919));
#84147=CARTESIAN_POINT('Ctrl Pts',(-0.294214252459464,0.016060720643228,
-0.329466485546049));
#84148=CARTESIAN_POINT('Ctrl Pts',(-0.292866399682999,0.0324238984400597,
-0.330350582796178));
#84149=CARTESIAN_POINT('Ctrl Pts',(-0.290161070293889,0.0485818205289264,
-0.331234680046308));
#84150=CARTESIAN_POINT('Ctrl Pts',(-0.28745670063117,0.064734010530484,
-0.332118463659412));
#84151=CARTESIAN_POINT('Ctrl Pts',(-0.28339588448832,0.0806802781392302,
-0.333002247272515));
#84152=CARTESIAN_POINT('Ctrl Pts',(-0.278035191199422,0.0961772969816719,
-0.333886030885619));
#84153=CARTESIAN_POINT('Ctrl Pts',(-0.2726762672925,0.111669200786873,-0.334769522791902));
#84154=CARTESIAN_POINT('Ctrl Pts',(-0.266018593680786,0.126711382273948,
-0.335653014698185));
#84155=CARTESIAN_POINT('Ctrl Pts',(-0.258167955624118,0.141077803671816,
-0.336536506604468));
#84156=CARTESIAN_POINT('Ctrl Pts',(-0.250299611096769,0.155476627355642,
-0.337421991154333));
#84157=CARTESIAN_POINT('Ctrl Pts',(-0.241233352702085,0.169195946460847,
-0.338307475704197));
#84158=CARTESIAN_POINT('Ctrl Pts',(-0.231119882409214,0.182036369869186,
-0.339192960254062));
#84159=CARTESIAN_POINT('Ctrl Pts',(-0.223356655053582,0.19189284083067,
-0.339872669362947));
#84160=CARTESIAN_POINT('Ctrl Pts',(-0.214977367630312,0.201231959199419,
-0.340552378471831));
#84161=CARTESIAN_POINT('Ctrl Pts',(-0.206064928528032,0.20997829704695,
-0.341232087580716));
#84162=CARTESIAN_POINT('Ctrl Pts',(-0.194285732941616,0.221537963597106,
-0.342130430497121));
#84163=CARTESIAN_POINT('Ctrl Pts',(-0.1814933687614,0.232140120048867,-0.343028773413525));
#84164=CARTESIAN_POINT('Ctrl Pts',(-0.167868878810078,0.241606455888594,
-0.34392711632993));
#84165=CARTESIAN_POINT('Ctrl Pts',(-0.154270768290315,0.251054463221398,
-0.344823719894948));
#84166=CARTESIAN_POINT('Ctrl Pts',(-0.139844334731844,0.259370515031801,
-0.345720323459967));
#84167=CARTESIAN_POINT('Ctrl Pts',(-0.124803770583353,0.26641632616673,
-0.346616927024986));
#84168=CARTESIAN_POINT('Ctrl Pts',(-0.10976578888216,0.273460927544117,
-0.347513376644219));
#84169=CARTESIAN_POINT('Ctrl Pts',(-0.0941145777494428,0.27923533905974,
-0.348409826263453));
#84170=CARTESIAN_POINT('Ctrl Pts',(-0.0780888710090381,0.283647260209814,
-0.349306275882687));
#84171=CARTESIAN_POINT('Ctrl Pts',(-0.062067385452284,0.288058019256417,
-0.350202489376392));
#84172=CARTESIAN_POINT('Ctrl Pts',(-0.0456723659216754,0.291106800988731,
-0.351098702870097));
#84173=CARTESIAN_POINT('Ctrl Pts',(-0.0291560449745601,0.292751712277557,
-0.351994916363802));
#84174=CARTESIAN_POINT('Ctrl Pts',(-0.0126003152006319,0.294400548412861,
-0.352893268270927));
#84175=CARTESIAN_POINT('Ctrl Pts',(0.00407650091495812,0.294638771795434,
-0.353791620178052));
#84176=CARTESIAN_POINT('Ctrl Pts',(0.0206183597940802,0.293476614467664,
-0.354689972085177));
#84177=CARTESIAN_POINT('Ctrl Pts',(0.0353273337368774,0.292443227471891,
-0.355488784050018));
#84178=CARTESIAN_POINT('Ctrl Pts',(0.0499292150980614,0.290303422713045,
-0.35628759601486));
#84179=CARTESIAN_POINT('Ctrl Pts',(0.0642502550476124,0.287098493075663,
-0.357086407979701));
#84180=CARTESIAN_POINT('Ctrl Pts',(0.0803556800310626,0.283494232907833,
-0.357984750992566));
#84181=CARTESIAN_POINT('Ctrl Pts',(0.0962080725173854,0.278519092851921,
-0.358883094005431));
#84182=CARTESIAN_POINT('Ctrl Pts',(0.111559358074178,0.272228120564495,
-0.359781437018295));
#84183=CARTESIAN_POINT('Ctrl Pts',(0.126880920858645,0.265949328699114,
-0.360678040682052));
#84184=CARTESIAN_POINT('Ctrl Pts',(0.141702554112727,0.258359997366554,
-0.361574644345809));
#84185=CARTESIAN_POINT('Ctrl Pts',(0.155791762320314,0.249564754709336,
-0.362471248009565));
#84186=CARTESIAN_POINT('Ctrl Pts',(0.169878551459699,0.240771022164788,
-0.363367697729582));
#84187=CARTESIAN_POINT('Ctrl Pts',(0.183232468392925,0.230772162330733,
-0.364264147449598));
#84188=CARTESIAN_POINT('Ctrl Pts',(0.195646277537678,0.219718397239853,
-0.365160597169614));
#84189=CARTESIAN_POINT('Ctrl Pts',(0.208056816893781,0.208667543702969,
-0.3660568107654));
#84190=CARTESIAN_POINT('Ctrl Pts',(0.21952715642872,0.196562870950218,-0.366953024361187));
#84191=CARTESIAN_POINT('Ctrl Pts',(0.229885034909869,0.183593329738551,
-0.367849237956974));
#84192=CARTESIAN_POINT('Ctrl Pts',(0.240267627841583,0.170592842509734,
-0.368747589966206));
#84193=CARTESIAN_POINT('Ctrl Pts',(0.249531983405,0.156724002687977,-0.369645941975438));
#84194=CARTESIAN_POINT('Ctrl Pts',(0.257547522201203,0.142207291683727,
-0.37054429398467));
#84195=CARTESIAN_POINT('Ctrl Pts',(0.264674911264882,0.129299083030145,
-0.371343105449342));
#84196=CARTESIAN_POINT('Ctrl Pts',(0.270815379416652,0.115879393160618,
-0.372141916914014));
#84197=CARTESIAN_POINT('Ctrl Pts',(0.275909149363032,0.102116508448771,
-0.372940728378687));
#84198=CARTESIAN_POINT('Ctrl Pts',(0.281637600494086,0.0866387751934325,
-0.373839071351861));
#84199=CARTESIAN_POINT('Ctrl Pts',(0.28607782017348,0.070628316426023,-0.374737414325036));
#84200=CARTESIAN_POINT('Ctrl Pts',(0.289141178182896,0.0543232830286123,
-0.375635757298211));
#84201=CARTESIAN_POINT('Ctrl Pts',(0.29219860499338,0.0380498190384939,
-0.37653236092167));
#84202=CARTESIAN_POINT('Ctrl Pts',(0.293884252773285,0.0214836689143827,
-0.377428964545129));
#84203=CARTESIAN_POINT('Ctrl Pts',(0.294159576219129,0.00487685539899314,
-0.378325568168588));
#84204=CARTESIAN_POINT('Ctrl Pts',(0.294434852392787,-0.0117271067777837,
-0.379222017847973));
#84205=CARTESIAN_POINT('Ctrl Pts',(0.293300219297199,-0.0283709308565512,
-0.380118467527358));
#84206=CARTESIAN_POINT('Ctrl Pts',(0.29076913219291,-0.0447990152099595,
-0.381014917206743));
#84207=CARTESIAN_POINT('Ctrl Pts',(0.288238711775943,-0.0612227724125754,
-0.381911130761644));
#84208=CARTESIAN_POINT('Ctrl Pts',(0.28431269893803,-0.0774301223399919,
-0.382807344316545));
#84209=CARTESIAN_POINT('Ctrl Pts',(0.279056067068374,-0.0931737700875695,
-0.383703557871446));
#84210=CARTESIAN_POINT('Ctrl Pts',(0.273786892591526,-0.10895498302791,
-0.384601909840232));
#84211=CARTESIAN_POINT('Ctrl Pts',(0.267181034925924,-0.124269538959438,
-0.385500261809018));
#84212=CARTESIAN_POINT('Ctrl Pts',(0.259352589351685,-0.138887992269224,
-0.386398613777804));
#84213=CARTESIAN_POINT('Ctrl Pts',(0.252391560853387,-0.151886673696521,
-0.387197425444426));
#84214=CARTESIAN_POINT('Ctrl Pts',(0.244464776903971,-0.164334952001692,
-0.387996237111049));
#84215=CARTESIAN_POINT('Ctrl Pts',(0.235681004253934,-0.176091181590269,
-0.388795048777672));
#84216=CARTESIAN_POINT('Ctrl Pts',(0.225802780469574,-0.189312228099913,
-0.389693391747013));
#84217=CARTESIAN_POINT('Ctrl Pts',(0.214777197428199,-0.201741502271168,
-0.390591734716355));
#84218=CARTESIAN_POINT('Ctrl Pts',(0.202755982708064,-0.213175166180508,
-0.391490077685696));
#84219=CARTESIAN_POINT('Ctrl Pts',(0.190758043173981,-0.224586692505507,
-0.392386681305044));
#84220=CARTESIAN_POINT('Ctrl Pts',(0.177768819723121,-0.235005848416589,
-0.393283284924392));
#84221=CARTESIAN_POINT('Ctrl Pts',(0.163978906594322,-0.244263296858391,
-0.394179888543739));
#84222=CARTESIAN_POINT('Ctrl Pts',(0.150191361156735,-0.253519155821049,
-0.395076338218643));
#84223=CARTESIAN_POINT('Ctrl Pts',(0.135604024403656,-0.261613220080211,
-0.395972787893546));
#84224=CARTESIAN_POINT('Ctrl Pts',(0.120438758651496,-0.268417855990407,
-0.39686923756845));
#84225=CARTESIAN_POINT('Ctrl Pts',(0.105277487427806,-0.275220699560639,
-0.397765451118659));
#84226=CARTESIAN_POINT('Ctrl Pts',(0.0895393158397275,-0.280734475153809,
-0.398661664668868));
#84227=CARTESIAN_POINT('Ctrl Pts',(0.073467135425447,-0.2848793077996,-0.399557878219076));
#84228=CARTESIAN_POINT('Ctrl Pts',(0.0573566059261533,-0.289034030238524,
-0.400456230182913));
#84229=CARTESIAN_POINT('Ctrl Pts',(0.0409112517815999,-0.291813113504055,
-0.401354582146749));
#84230=CARTESIAN_POINT('Ctrl Pts',(0.0243856814000187,-0.293187616625697,
-0.402252934110586));
#84231=CARTESIAN_POINT('Ctrl Pts',(0.0096911971505409,-0.294409820398726,
-0.403051745799276));
#84232=CARTESIAN_POINT('Ctrl Pts',(-0.00506620492991027,-0.294522218476699,
-0.403850557487967));
#84233=CARTESIAN_POINT('Ctrl Pts',(-0.0197085109287172,-0.293539119363966,
-0.404649369176657));
#84234=CARTESIAN_POINT('Ctrl Pts',(-0.0361752364739775,-0.292433526892775,
-0.405547712159046));
#84235=CARTESIAN_POINT('Ctrl Pts',(-0.0526009849869378,-0.289934500638107,
-0.406446055141434));
#84236=CARTESIAN_POINT('Ctrl Pts',(-0.0687321884564251,-0.286058606355394,
-0.407344398123822));
#84237=CARTESIAN_POINT('Ctrl Pts',(-0.0848321590850295,-0.282190216484218,
-0.408241001756541));
#84238=CARTESIAN_POINT('Ctrl Pts',(-0.100637941009124,-0.276950369006611,
-0.409137605389259));
#84239=CARTESIAN_POINT('Ctrl Pts',(-0.11590380053619,-0.270407006235539,
-0.410034209021978));
#84240=CARTESIAN_POINT('Ctrl Pts',(-0.131167038961171,-0.263864766940141,
-0.410930658710554));
#84241=CARTESIAN_POINT('Ctrl Pts',(-0.145889793476127,-0.256019719010459,
-0.41182710839913));
#84242=CARTESIAN_POINT('Ctrl Pts',(-0.159844340511968,-0.246988717973704,
-0.412723558087707));
#84243=CARTESIAN_POINT('Ctrl Pts',(-0.173795211925462,-0.237960095699165,
-0.413619771651778));
#84244=CARTESIAN_POINT('Ctrl Pts',(-0.18697761925489,-0.227746579614595,
-0.414515985215849));
#84245=CARTESIAN_POINT('Ctrl Pts',(-0.199192496923741,-0.216508635322671,
-0.415412198779921));
#84246=CARTESIAN_POINT('Ctrl Pts',(-0.211436519946146,-0.205243876692652,
-0.416310550757646));
#84247=CARTESIAN_POINT('Ctrl Pts',(-0.222707836000168,-0.192950365449024,
-0.417208902735371));
#84248=CARTESIAN_POINT('Ctrl Pts',(-0.232843764398215,-0.179826086485995,
-0.418107254713096));
#84249=CARTESIAN_POINT('Ctrl Pts',(-0.241856598558109,-0.168156020842599,
-0.418906066333944));
#84250=CARTESIAN_POINT('Ctrl Pts',(-0.249972073146481,-0.155829927224543,
-0.419704877954793));
#84251=CARTESIAN_POINT('Ctrl Pts',(-0.257105442200693,-0.143005005474584,
-0.420503689575642));
#84252=CARTESIAN_POINT('Ctrl Pts',(-0.265498603903353,-0.127915131215549,
-0.421443575771462));
#84253=CARTESIAN_POINT('Ctrl Pts',(-0.272580779171265,-0.112046037639118,
-0.422383461967282));
#84254=CARTESIAN_POINT('Ctrl Pts',(-0.278220391500258,-0.0956402308311883,
-0.423323348163103));
#84255=CARTESIAN_POINT('Ctrl Pts',(-0.28383932615922,-0.0792945760053446,
-0.424259788260948));
#84256=CARTESIAN_POINT('Ctrl Pts',(-0.288025935021425,-0.0624167389765852,
-0.425196228358794));
#84257=CARTESIAN_POINT('Ctrl Pts',(-0.290696210763236,-0.045269780736122,
-0.42613266845664));
#84258=CARTESIAN_POINT('Ctrl Pts',(-0.293024684117832,-0.0303176786928218,
-0.426949241734773));
#84259=CARTESIAN_POINT('Ctrl Pts',(-0.294200789390909,-0.0151615645798832,
-0.427765815012907));
#84260=CARTESIAN_POINT('Ctrl Pts',(-0.294199999601645,1.53098717317831E-5,
-0.42858238829104));
#84261=CARTESIAN_POINT('',(-0.294346683130411,0.000249348936495447,-0.52858238829104));
#84262=CARTESIAN_POINT('Ctrl Pts',(-0.293721445376834,1.55001453468206E-5,
-0.428582399887245));
#84263=CARTESIAN_POINT('Ctrl Pts',(-0.293743763360868,0.04810977684068,
-0.431174269916372));
#84264=CARTESIAN_POINT('Ctrl Pts',(-0.259849801060223,0.194237660365639,
-0.439050913411827));
#84265=CARTESIAN_POINT('Ctrl Pts',(-0.0298824682073853,0.346276530597267,
-0.452212330373611));
#84266=CARTESIAN_POINT('Ctrl Pts',(0.274418277941293,0.213295584266401,
-0.468066650772598));
#84267=CARTESIAN_POINT('Ctrl Pts',(0.328193052433044,-0.114410305001873,
-0.483920971171582));
#84268=CARTESIAN_POINT('Ctrl Pts',(0.0823489968487952,-0.337667055345944,
-0.499775291570567));
#84269=CARTESIAN_POINT('Ctrl Pts',(-0.219090521244163,-0.257841877924801,
-0.514662430610386));
#84270=CARTESIAN_POINT('Ctrl Pts',(-0.293628149939983,-0.0794362743206141,
-0.524264796183877));
#84271=CARTESIAN_POINT('Ctrl Pts',(-0.294346683130411,0.000249348936495447,
-0.52858238829104));
#84272=CARTESIAN_POINT('',(-0.294505057048355,-0.00019672582264435,-0.62858238829104));
#84273=CARTESIAN_POINT('Ctrl Pts',(-0.294346683130411,0.000249348936495447,
-0.52858238829104));
#84274=CARTESIAN_POINT('Ctrl Pts',(-0.294507641342876,0.0180996802079338,
-0.529549569650206));
#84275=CARTESIAN_POINT('Ctrl Pts',(-0.284909911715827,0.133313276848973,
-0.5358015244757));
#84276=CARTESIAN_POINT('Ctrl Pts',(-0.132888470050069,0.3211558065429,-0.547338252767522));
#84277=CARTESIAN_POINT('Ctrl Pts',(0.197345118413126,0.286103655668621,
-0.563192573166507));
#84278=CARTESIAN_POINT('Ctrl Pts',(0.347415497895151,-0.0101424538979736,
-0.579046893565493));
#84279=CARTESIAN_POINT('Ctrl Pts',(0.180318209615228,-0.29712916522912,
-0.594901213964478));
#84280=CARTESIAN_POINT('Ctrl Pts',(-0.151397831555328,-0.312856347464733,
-0.610755534363463));
#84281=CARTESIAN_POINT('Ctrl Pts',(-0.28842246464897,-0.121736620937465,
-0.621982592472317));
#84282=CARTESIAN_POINT('Ctrl Pts',(-0.294598450780843,-0.0123148159016998,
-0.627924877114843));
#84283=CARTESIAN_POINT('Ctrl Pts',(-0.294505057048355,-0.00019672582264435,
-0.62858238829104));
#84284=CARTESIAN_POINT('',(-0.294170636188799,-0.000106379757622669,-0.728582382959596));
#84285=CARTESIAN_POINT('Ctrl Pts',(-0.294505057048355,-0.00019672582264435,
-0.62858238829104));
#84286=CARTESIAN_POINT('Ctrl Pts',(-0.293847794765797,0.0850848378695851,
-0.633209650581171));
#84287=CARTESIAN_POINT('Ctrl Pts',(-0.210031811032951,0.268892279222193,
-0.64312168633763));
#84288=CARTESIAN_POINT('Ctrl Pts',(0.101907672028251,0.332287863050133,
-0.658318495560419));
#84289=CARTESIAN_POINT('Ctrl Pts',(0.334308601219868,0.0950692205661775,
-0.674172815959403));
#84290=CARTESIAN_POINT('Ctrl Pts',(0.261507603601085,-0.228941413482704,
-0.69002713635839));
#84291=CARTESIAN_POINT('Ctrl Pts',(-0.0500327629821309,-0.343943483986855,
-0.705881456757374));
#84292=CARTESIAN_POINT('Ctrl Pts',(-0.265545445146438,-0.182634770131956,
-0.71873318059113));
#84293=CARTESIAN_POINT('Ctrl Pts',(-0.293894681053642,-0.0424423890586008,
-0.72630013095856));
#84294=CARTESIAN_POINT('Ctrl Pts',(-0.293757281291689,-0.000107623531536137,
-0.72858230785966));
#84295=CARTESIAN_POINT('',(-0.294199880503211,0.000265163904499537,-0.828582388296047));
#84296=CARTESIAN_POINT('Ctrl Pts',(-0.294199980798989,-0.000106291460469518,
-0.72858238829104));
#84297=CARTESIAN_POINT('Ctrl Pts',(-0.294206132841855,0.0169217076386292,
-0.72949895127087));
#84298=CARTESIAN_POINT('Ctrl Pts',(-0.292729603762024,0.0339394245619945,
-0.7304155142507));
#84299=CARTESIAN_POINT('Ctrl Pts',(-0.289801721942549,0.0506813768472577,
-0.731332077230531));
#84300=CARTESIAN_POINT('Ctrl Pts',(-0.28687104797667,0.0674392949346736,
-0.732249514281852));
#84301=CARTESIAN_POINT('Ctrl Pts',(-0.282486448202963,0.0839202070110717,
-0.733166951333173));
#84302=CARTESIAN_POINT('Ctrl Pts',(-0.276729988221166,0.0998706844830533,
-0.734084388384494));
#84303=CARTESIAN_POINT('Ctrl Pts',(-0.270956766783648,0.115867605988818,
-0.735004496796436));
#84304=CARTESIAN_POINT('Ctrl Pts',(-0.263804024025265,0.131330338213574,
-0.735924605208378));
#84305=CARTESIAN_POINT('Ctrl Pts',(-0.255401444990078,0.146026510938871,
-0.736844713620321));
#84306=CARTESIAN_POINT('Ctrl Pts',(-0.253132456051998,0.149994989331775,
-0.737093174931995));
#84307=CARTESIAN_POINT('Ctrl Pts',(-0.250772576722466,0.153907732507795,
-0.73734163624367));
#84308=CARTESIAN_POINT('Ctrl Pts',(-0.248324887602851,0.157760547023112,
-0.737590097555344));
#84309=CARTESIAN_POINT('Ctrl Pts',(-0.239474961167038,0.171690880233385,
-0.738488440532336));
#84310=CARTESIAN_POINT('Ctrl Pts',(-0.229421074866712,0.184918492005382,
-0.739386783509328));
#84311=CARTESIAN_POINT('Ctrl Pts',(-0.218299103958587,0.197228652104297,
-0.740285126486319));
#84312=CARTESIAN_POINT('Ctrl Pts',(-0.207198667139453,0.209514977571271,
-0.741181730113535));
#84313=CARTESIAN_POINT('Ctrl Pts',(-0.195034726071907,0.220886753080267,
-0.74207833374075));
#84314=CARTESIAN_POINT('Ctrl Pts',(-0.181984520878497,0.231160710676844,
-0.742974937367966));
#84315=CARTESIAN_POINT('Ctrl Pts',(-0.168936556367226,0.241432904264893,
-0.743871387050956));
#84316=CARTESIAN_POINT('Ctrl Pts',(-0.155003216920538,0.250607125006237,
-0.744767836733946));
#84317=CARTESIAN_POINT('Ctrl Pts',(-0.140396075489323,0.258539323870076,
-0.745664286416936));
#84318=CARTESIAN_POINT('Ctrl Pts',(-0.125792781574502,0.266469433395266,
-0.746560499975365));
#84319=CARTESIAN_POINT('Ctrl Pts',(-0.110516738620478,0.273157802579337,
-0.747456713533794));
#84320=CARTESIAN_POINT('Ctrl Pts',(-0.09480410088293,0.278506413670815,
-0.748352927092224));
#84321=CARTESIAN_POINT('Ctrl Pts',(-0.0790539719479187,0.283867786835596,
-0.749251279064333));
#84322=CARTESIAN_POINT('Ctrl Pts',(-0.062865928264738,0.287882786569572,
-0.750149631036442));
#84323=CARTESIAN_POINT('Ctrl Pts',(-0.0464916598902995,0.290503296987564,
-0.751047983008552));
#84324=CARTESIAN_POINT('Ctrl Pts',(-0.0319317137658783,0.292833446318938,
-0.751846794657144));
#84325=CARTESIAN_POINT('Ctrl Pts',(-0.0172250876784197,0.294061728114009,
-0.752645606305737));
#84326=CARTESIAN_POINT('Ctrl Pts',(-0.00255036782839512,0.294188945448227,
-0.753444417954329));
#84327=CARTESIAN_POINT('Ctrl Pts',(0.0139528110371371,0.294332013966253,
-0.754342760931321));
#84328=CARTESIAN_POINT('Ctrl Pts',(0.0305205254267988,0.293082540944039,
-0.755241103908313));
#84329=CARTESIAN_POINT('Ctrl Pts',(0.0468986807142758,0.290437865553478,
-0.756139446885304));
#84330=CARTESIAN_POINT('Ctrl Pts',(0.0632451250166731,0.28779831071895,
-0.75703605051252));
#84331=CARTESIAN_POINT('Ctrl Pts',(0.0794019563069647,0.283768975391802,
-0.757932654139735));
#84332=CARTESIAN_POINT('Ctrl Pts',(0.0951190058655022,0.278399020693605,
-0.75882925776695));
#84333=CARTESIAN_POINT('Ctrl Pts',(0.110833356852515,0.273029988000954,
-0.75972570744994));
#84334=CARTESIAN_POINT('Ctrl Pts',(0.126107312753752,0.266320998101228,
-0.76062215713293));
#84335=CARTESIAN_POINT('Ctrl Pts',(0.140704963731675,0.258371347446399,
-0.76151860681592));
#84336=CARTESIAN_POINT('Ctrl Pts',(0.155298769692987,0.250423790727017,
-0.762414820374349));
#84337=CARTESIAN_POINT('Ctrl Pts',(0.169215934739101,0.24123661010645,-0.763311033932779));
#84338=CARTESIAN_POINT('Ctrl Pts',(0.182245826395781,0.230954754792619,
-0.764207247491208));
#84339=CARTESIAN_POINT('Ctrl Pts',(0.195306808073703,0.220648366419839,
-0.765105599463317));
#84340=CARTESIAN_POINT('Ctrl Pts',(0.207475680970353,0.209242599739005,
-0.766003951435427));
#84341=CARTESIAN_POINT('Ctrl Pts',(0.218575255425636,0.196922567816942,
-0.766902303407536));
#84342=CARTESIAN_POINT('Ctrl Pts',(0.228444960891387,0.185967635545503,
-0.767701115056129));
#84343=CARTESIAN_POINT('Ctrl Pts',(0.237469497284348,0.174290680893861,
-0.768499926704721));
#84344=CARTESIAN_POINT('Ctrl Pts',(0.245552471266777,0.162042043478779,
-0.769298738353313));
#84345=CARTESIAN_POINT('Ctrl Pts',(0.25464257770566,0.148267235088153,-0.770197081330305));
#84346=CARTESIAN_POINT('Ctrl Pts',(0.262598878608108,0.133681364566294,
-0.771095424307297));
#84347=CARTESIAN_POINT('Ctrl Pts',(0.269281031782881,0.118496269654141,
-0.771993767284289));
#84348=CARTESIAN_POINT('Ctrl Pts',(0.275950247135542,0.103340575752651,
-0.772890370911504));
#84349=CARTESIAN_POINT('Ctrl Pts',(0.281349836516313,0.0875886496786563,
-0.77378697453872));
#84350=CARTESIAN_POINT('Ctrl Pts',(0.285385090316645,0.07147720073534,-0.774683578165935));
#84351=CARTESIAN_POINT('Ctrl Pts',(0.289419651275681,0.0553685180807732,
-0.775580027848925));
#84352=CARTESIAN_POINT('Ctrl Pts',(0.292090099088861,0.0389011873066432,
-0.776476477531915));
#84353=CARTESIAN_POINT('Ctrl Pts',(0.293351557311752,0.0223271991698397,
-0.777372927214905));
#84354=CARTESIAN_POINT('Ctrl Pts',(0.294612683266951,0.00575757661622281,
-0.778269140773334));
#84355=CARTESIAN_POINT('Ctrl Pts',(0.294465507332073,-0.0109178577085512,
-0.779165354331764));
#84356=CARTESIAN_POINT('Ctrl Pts',(0.292917212511679,-0.0274435168006569,
-0.780061567890193));
#84357=CARTESIAN_POINT('Ctrl Pts',(0.291365223376695,-0.0440086070028396,
-0.780959919862303));
#84358=CARTESIAN_POINT('Ctrl Pts',(0.288405539004933,-0.0604224197705049,
-0.781858271834412));
#84359=CARTESIAN_POINT('Ctrl Pts',(0.284097232724547,-0.0764356092293033,
-0.782756623806522));
#84360=CARTESIAN_POINT('Ctrl Pts',(0.280266300807744,-0.0906744851575982,
-0.783555435455115));
#84361=CARTESIAN_POINT('Ctrl Pts',(0.27536993496698,-0.104596379015757,
-0.784354247103707));
#84362=CARTESIAN_POINT('Ctrl Pts',(0.269481935551342,-0.118038664900542,
-0.7851530587523));
#84363=CARTESIAN_POINT('Ctrl Pts',(0.262860295853311,-0.133155849459113,
-0.786051401729291));
#84364=CARTESIAN_POINT('Ctrl Pts',(0.254941599989955,-0.147762169966145,
-0.786949744706283));
#84365=CARTESIAN_POINT('Ctrl Pts',(0.245827381463146,-0.161624684138818,
-0.787848087683274));
#84366=CARTESIAN_POINT('Ctrl Pts',(0.2367308096641,-0.175460358049434,-0.78874469131049));
#84367=CARTESIAN_POINT('Ctrl Pts',(0.226443684555273,-0.188554394765326,
-0.789641294937705));
#84368=CARTESIAN_POINT('Ctrl Pts',(0.215113219328487,-0.200698636941396,
-0.790537898564921));
#84369=CARTESIAN_POINT('Ctrl Pts',(0.203784699509509,-0.212840793986531,
-0.791434348247911));
#84370=CARTESIAN_POINT('Ctrl Pts',(0.191413694727506,-0.224032867745722,
-0.792330797930901));
#84371=CARTESIAN_POINT('Ctrl Pts',(0.17818733119506,-0.234100224266407,
-0.793227247613891));
#84372=CARTESIAN_POINT('Ctrl Pts',(0.164964451482551,-0.244164929048594,
-0.79412346117232));
#84373=CARTESIAN_POINT('Ctrl Pts',(0.150887296586511,-0.25310503423301,
-0.795019674730749));
#84374=CARTESIAN_POINT('Ctrl Pts',(0.136174307376091,-0.260787649267832,
-0.795915888289178));
#84375=CARTESIAN_POINT('Ctrl Pts',(0.121426212183275,-0.268488595434711,
-0.796814240261288));
#84376=CARTESIAN_POINT('Ctrl Pts',(0.106039969144742,-0.274925714845722,
-0.797712592233397));
#84377=CARTESIAN_POINT('Ctrl Pts',(0.0902569844850293,-0.280013065323155,
-0.798610944205506));
#84378=CARTESIAN_POINT('Ctrl Pts',(0.0762228059145374,-0.284536720803427,
-0.799409755854099));
#84379=CARTESIAN_POINT('Ctrl Pts',(0.0618756001821937,-0.287993773698357,
-0.800208567502692));
#84380=CARTESIAN_POINT('Ctrl Pts',(0.0473919864234226,-0.290357778650482,
-0.801007379151284));
#84381=CARTESIAN_POINT('Ctrl Pts',(0.0311037253238565,-0.293016336835076,
-0.801905722128276));
#84382=CARTESIAN_POINT('Ctrl Pts',(0.0145392850277297,-0.294308490311483,
-0.802804065105268));
#84383=CARTESIAN_POINT('Ctrl Pts',(-0.00205061872833332,-0.294192853351048,
-0.803702408082259));
#84384=CARTESIAN_POINT('Ctrl Pts',(-0.0186084015171033,-0.294077440284076,
-0.804599011709475));
#84385=CARTESIAN_POINT('Ctrl Pts',(-0.0351907675097167,-0.292559586994451,
-0.805495615336691));
#84386=CARTESIAN_POINT('Ctrl Pts',(-0.0515429767469632,-0.289649722161203,
-0.806392218963906));
#84387=CARTESIAN_POINT('Ctrl Pts',(-0.0678923783576141,-0.286740356943253,
-0.807288668646896));
#84388=CARTESIAN_POINT('Ctrl Pts',(-0.0840109160382376,-0.282439541045554,
-0.808185118329886));
#84389=CARTESIAN_POINT('Ctrl Pts',(-0.0996502949343614,-0.276809426717182,
-0.809081568012876));
#84390=CARTESIAN_POINT('Ctrl Pts',(-0.115285554423077,-0.271180795359126,
-0.809977781571306));
#84391=CARTESIAN_POINT('Ctrl Pts',(-0.130441164919528,-0.264223839045072,
-0.810873995129736));
#84392=CARTESIAN_POINT('Ctrl Pts',(-0.144886849942095,-0.256049684072949,
-0.811770208688165));
#84393=CARTESIAN_POINT('Ctrl Pts',(-0.159367003144902,-0.247856025128086,
-0.812668560660275));
#84394=CARTESIAN_POINT('Ctrl Pts',(-0.17313316948217,-0.238439781422285,
-0.813566912632384));
#84395=CARTESIAN_POINT('Ctrl Pts',(-0.185981997955222,-0.227956874071794,
-0.814465264604493));
#84396=CARTESIAN_POINT('Ctrl Pts',(-0.197407134398052,-0.218635506987775,
-0.815264076253085));
#84397=CARTESIAN_POINT('Ctrl Pts',(-0.20810711787855,-0.208471655328033,
-0.816062887901677));
#84398=CARTESIAN_POINT('Ctrl Pts',(-0.217963752214611,-0.197599197165696,
-0.816861699550269));
#84399=CARTESIAN_POINT('Ctrl Pts',(-0.228933235913372,-0.185499199487901,
-0.817750699898548));
#84400=CARTESIAN_POINT('Ctrl Pts',(-0.23893064891016,-0.172440167272248,
-0.818639700246826));
#84401=CARTESIAN_POINT('Ctrl Pts',(-0.247786228830629,-0.158605248342844,
-0.819528700595104));
#84402=CARTESIAN_POINT('Ctrl Pts',(-0.256625587779185,-0.144795671156542,
-0.820416072540747));
#84403=CARTESIAN_POINT('Ctrl Pts',(-0.264326770282118,-0.130213661237864,
-0.821303444486391));
#84404=CARTESIAN_POINT('Ctrl Pts',(-0.270761035164523,-0.115074331788787,
-0.822190816432034));
#84405=CARTESIAN_POINT('Ctrl Pts',(-0.277188498774112,-0.0999510052105465,
-0.823077250390385));
#84406=CARTESIAN_POINT('Ctrl Pts',(-0.282351362761424,-0.0842722594194868,
-0.823963684348736));
#84407=CARTESIAN_POINT('Ctrl Pts',(-0.286167972763128,-0.0682754081982774,
-0.824850118307087));
#84408=CARTESIAN_POINT('Ctrl Pts',(-0.289986862924126,-0.0522689999699433,
-0.825737081848138));
#84409=CARTESIAN_POINT('Ctrl Pts',(-0.292457708475443,-0.0359448942765146,
-0.826624045389189));
#84410=CARTESIAN_POINT('Ctrl Pts',(-0.293549560455702,-0.0195523798107569,
-0.82751100893024));
#84411=CARTESIAN_POINT('Ctrl Pts',(-0.293989183064208,-0.0129521078877307,
-0.82786813538384));
#84412=CARTESIAN_POINT('Ctrl Pts',(-0.294205834500301,-0.00634081004028046,
-0.82822526183744));
#84413=CARTESIAN_POINT('Ctrl Pts',(-0.294199880503295,0.000265163811891233,
-0.82858238829104));
#84414=CARTESIAN_POINT('',(-0.294199988411901,-8.25738279543517E-5,-0.928582388295833));
#84415=CARTESIAN_POINT('Ctrl Pts',(-0.294199880503211,0.00026516390450072,
-0.828582388296047));
#84416=CARTESIAN_POINT('Ctrl Pts',(-0.294180819917147,0.0214129221291205,
-0.829725660138392));
#84417=CARTESIAN_POINT('Ctrl Pts',(-0.291877645470538,0.0424583192963313,
-0.830868931980738));
#84418=CARTESIAN_POINT('Ctrl Pts',(-0.287378498393475,0.0629860195687247,
-0.832012203823083));
#84419=CARTESIAN_POINT('Ctrl Pts',(-0.286455249827511,0.0671984112763944,
-0.832246809198474));
#84420=CARTESIAN_POINT('Ctrl Pts',(-0.285439688017423,0.0713890804885765,
-0.832481414573864));
#84421=CARTESIAN_POINT('Ctrl Pts',(-0.284332815343903,0.0755545506148362,
-0.832716019949255));
#84422=CARTESIAN_POINT('Ctrl Pts',(-0.280094415899626,0.0915048280863658,
-0.833614362926246));
#84423=CARTESIAN_POINT('Ctrl Pts',(-0.27449621650345,0.107148053663296,
-0.834512705903237));
#84424=CARTESIAN_POINT('Ctrl Pts',(-0.267603032908877,0.122238524115643,
-0.835411048880228));
#84425=CARTESIAN_POINT('Ctrl Pts',(-0.260723195728369,0.137299776766904,
-0.836307652507442));
#84426=CARTESIAN_POINT('Ctrl Pts',(-0.252553616409181,0.151809660097539,
-0.837204256134657));
#84427=CARTESIAN_POINT('Ctrl Pts',(-0.243208036264824,0.165539998478337,
-0.838100859761872));
#84428=CARTESIAN_POINT('Ctrl Pts',(-0.233864060729297,0.179267979400118,
-0.838997309444861));
#84429=CARTESIAN_POINT('Ctrl Pts',(-0.223344885476473,0.192215999571075,
-0.83989375912785));
#84430=CARTESIAN_POINT('Ctrl Pts',(-0.211808811025279,0.204182926739866,
-0.840790208810839));
#84431=CARTESIAN_POINT('Ctrl Pts',(-0.200275775172416,0.216146701823857,
-0.841686422369268));
#84432=CARTESIAN_POINT('Ctrl Pts',(-0.187726928953047,0.227129334897843,
-0.842582635927696));
#84433=CARTESIAN_POINT('Ctrl Pts',(-0.174357888097682,0.236966172392002,
-0.843478849486125));
#84434=CARTESIAN_POINT('Ctrl Pts',(-0.160956947992875,0.246826481108693,
-0.844377201458233));
#84435=CARTESIAN_POINT('Ctrl Pts',(-0.146732560293176,0.255535084654648,
-0.845275553430342));
#84436=CARTESIAN_POINT('Ctrl Pts',(-0.131910198224532,0.262970225699345,
-0.846173905402451));
#84437=CARTESIAN_POINT('Ctrl Pts',(-0.118730202134191,0.269581528907729,
-0.846972717051047));
#84438=CARTESIAN_POINT('Ctrl Pts',(-0.10507815685663,0.275186454133451,
-0.847771528699643));
#84439=CARTESIAN_POINT('Ctrl Pts',(-0.0911245813838285,0.279731926436047,
-0.848570340348239));
#84440=CARTESIAN_POINT('Ctrl Pts',(-0.0754324009406084,0.284843761156189,
-0.849468683325231));
#84441=CARTESIAN_POINT('Ctrl Pts',(-0.0592588605196882,0.28864730334519,
-0.850367026302223));
#84442=CARTESIAN_POINT('Ctrl Pts',(-0.0428454299491573,0.291063410844565,
-0.851265369279215));
#84443=CARTESIAN_POINT('Ctrl Pts',(-0.0264637786628479,0.293474840335487,
-0.85216197290643));
#84444=CARTESIAN_POINT('Ctrl Pts',(-0.00984392323024985,0.294503988488651,
-0.853058576533646));
#84445=CARTESIAN_POINT('Ctrl Pts',(0.00676078633986324,0.294122307498202,
-0.853955180160861));
#84446=CARTESIAN_POINT('Ctrl Pts',(0.0233626449298178,0.293740692041265,
-0.854851629843851));
#84447=CARTESIAN_POINT('Ctrl Pts',(0.0399485732106359,0.291948693879664,
-0.855748079526841));
#84448=CARTESIAN_POINT('Ctrl Pts',(0.0562637016785053,0.288769866629869,
-0.856644529209831));
#84449=CARTESIAN_POINT('Ctrl Pts',(0.0725745327467388,0.285591876682158,
-0.85754074276826));
#84450=CARTESIAN_POINT('Ctrl Pts',(0.0886139310497688,0.281027944961326,
-0.85843695632669));
#84451=CARTESIAN_POINT('Ctrl Pts',(0.104137364816809,0.27515277438,-0.859333169885119));
#84452=CARTESIAN_POINT('Ctrl Pts',(0.119697838330478,0.269263585326149,
-0.860231521857229));
#84453=CARTESIAN_POINT('Ctrl Pts',(0.134739154957633,0.262057214861473,
-0.861129873829338));
#84454=CARTESIAN_POINT('Ctrl Pts',(0.149036560993871,0.253656743429226,
-0.862028225801448));
#84455=CARTESIAN_POINT('Ctrl Pts',(0.161749767889358,0.246187071583362,
-0.86282703745004));
#84456=CARTESIAN_POINT('Ctrl Pts',(0.173874807294979,0.237774168014653,
-0.863625849098632));
#84457=CARTESIAN_POINT('Ctrl Pts',(0.185274446102504,0.228532316361189,
-0.864424660747224));
#84458=CARTESIAN_POINT('Ctrl Pts',(0.198094471299975,0.218138936968282,
-0.865323003724216));
#84459=CARTESIAN_POINT('Ctrl Pts',(0.210077966267995,0.206630410073749,
-0.866221346701208));
#84460=CARTESIAN_POINT('Ctrl Pts',(0.221027253292019,0.194166406214323,
-0.8671196896782));
#84461=CARTESIAN_POINT('Ctrl Pts',(0.231955340573379,0.18172653485538,-0.868016293305416));
#84462=CARTESIAN_POINT('Ctrl Pts',(0.241852629174775,0.168335402757517,
-0.868912896932632));
#84463=CARTESIAN_POINT('Ctrl Pts',(0.250557452409647,0.154190152221169,
-0.869809500559847));
#84464=CARTESIAN_POINT('Ctrl Pts',(0.259260781051781,0.140047330383046,
-0.870705950242837));
#84465=CARTESIAN_POINT('Ctrl Pts',(0.26677159269054,0.125151291215711,-0.871602399925827));
#84466=CARTESIAN_POINT('Ctrl Pts',(0.272971128054464,0.109728771289363,
-0.872498849608818));
#84467=CARTESIAN_POINT('Ctrl Pts',(0.279169030462751,0.0943103136498444,
-0.873395063167247));
#84468=CARTESIAN_POINT('Ctrl Pts',(0.284056057367643,0.0783663888285661,
-0.874291276725677));
#84469=CARTESIAN_POINT('Ctrl Pts',(0.287562002499989,0.0621428573385242,
-0.875187490284106));
#84470=CARTESIAN_POINT('Ctrl Pts',(0.291076313005703,0.0458806156310878,
-0.876085842256216));
#84471=CARTESIAN_POINT('Ctrl Pts',(0.293202818486535,0.0293382169056149,
-0.876984194228326));
#84472=CARTESIAN_POINT('Ctrl Pts',(0.293922670218187,0.0127712149700344,
-0.877882546200435));
#84473=CARTESIAN_POINT('Ctrl Pts',(0.294562760034155,-0.00196010920939629,
-0.878681357849027));
#84474=CARTESIAN_POINT('Ctrl Pts',(0.294091424201564,-0.0167104098699517,
-0.879480169497618));
#84475=CARTESIAN_POINT('Ctrl Pts',(0.292530000364165,-0.0313023782952973,
-0.880278981146209));
#84476=CARTESIAN_POINT('Ctrl Pts',(0.290774024295327,-0.0477124949711212,
-0.881177324123201));
#84477=CARTESIAN_POINT('Ctrl Pts',(0.287627325274582,-0.0640265572550334,
-0.882075667100193));
#84478=CARTESIAN_POINT('Ctrl Pts',(0.283116484548468,-0.0799918506906604,
-0.882974010077184));
#84479=CARTESIAN_POINT('Ctrl Pts',(0.278614377602224,-0.0959262325142659,
-0.883870613704399));
#84480=CARTESIAN_POINT('Ctrl Pts',(0.272753521046517,-0.111512415528557,
-0.884767217331615));
#84481=CARTESIAN_POINT('Ctrl Pts',(0.26561152264705,-0.126507545376218,
-0.88566382095883));
#84482=CARTESIAN_POINT('Ctrl Pts',(0.258470750507858,-0.141500100603859,
-0.88656027064182));
#84483=CARTESIAN_POINT('Ctrl Pts',(0.250049564838929,-0.15590106953921,
-0.88745672032481));
#84484=CARTESIAN_POINT('Ctrl Pts',(0.240473736062526,-0.169487528343918,
-0.8883531700078));
#84485=CARTESIAN_POINT('Ctrl Pts',(0.23090042955637,-0.18307040847971,-0.889249383566229));
#84486=CARTESIAN_POINT('Ctrl Pts',(0.220173548559716,-0.195838563975285,
-0.890145597124658));
#84487=CARTESIAN_POINT('Ctrl Pts',(0.208461306045207,-0.207599431314073,
-0.891041810683087));
#84488=CARTESIAN_POINT('Ctrl Pts',(0.196721117491071,-0.219388360713931,
-0.891940162655197));
#84489=CARTESIAN_POINT('Ctrl Pts',(0.183991451155372,-0.230164657672262,
-0.892838514627306));
#84490=CARTESIAN_POINT('Ctrl Pts',(0.170476570948616,-0.239773598958687,
-0.893736866599416));
#84491=CARTESIAN_POINT('Ctrl Pts',(0.158459183472808,-0.248317838264157,
-0.894535678248009));
#84492=CARTESIAN_POINT('Ctrl Pts',(0.145821771244907,-0.255939474520686,
-0.895334489896602));
#84493=CARTESIAN_POINT('Ctrl Pts',(0.132724762784979,-0.262560045215701,
-0.896133301545195));
#84494=CARTESIAN_POINT('Ctrl Pts',(0.11799587695776,-0.270005534021504,
-0.897031644522186));
#84495=CARTESIAN_POINT('Ctrl Pts',(0.102591714714734,-0.276231457930542,
-0.897929987499178));
#84496=CARTESIAN_POINT('Ctrl Pts',(0.0867388493208474,-0.281122770366428,
-0.89882833047617));
#84497=CARTESIAN_POINT('Ctrl Pts',(0.070916677858549,-0.286004612362393,
-0.899724934103385));
#84498=CARTESIAN_POINT('Ctrl Pts',(0.0546482555416442,-0.289556678780755,
-0.900621537730601));
#84499=CARTESIAN_POINT('Ctrl Pts',(0.0381796137648128,-0.291712113380246,
-0.901518141357816));
#84500=CARTESIAN_POINT('Ctrl Pts',(0.0217137996056978,-0.293867177897909,
-0.902414591040806));
#84501=CARTESIAN_POINT('Ctrl Pts',(0.00504860934839983,-0.294625932163573,
-0.903311040723796));
#84502=CARTESIAN_POINT('Ctrl Pts',(-0.0115604770754096,-0.293972779981054,
-0.904207490406786));
#84503=CARTESIAN_POINT('Ctrl Pts',(-0.0281651886711505,-0.293319799838611,
-0.905103703965216));
#84504=CARTESIAN_POINT('Ctrl Pts',(-0.0447130355484239,-0.291255693639326,
-0.905999917523645));
#84505=CARTESIAN_POINT('Ctrl Pts',(-0.0609509529546465,-0.287816992781734,
-0.906896131082075));
#84506=CARTESIAN_POINT('Ctrl Pts',(-0.0772276149038328,-0.284370086999225,
-0.907794483054184));
#84507=CARTESIAN_POINT('Ctrl Pts',(-0.0931920987770226,-0.27954222662271,
-0.908692835026294));
#84508=CARTESIAN_POINT('Ctrl Pts',(-0.108603507643358,-0.273420771207235,
-0.909591186998403));
#84509=CARTESIAN_POINT('Ctrl Pts',(-0.122307282228212,-0.267977592983072,
-0.910389998646995));
#84510=CARTESIAN_POINT('Ctrl Pts',(-0.135573638549765,-0.261512508529333,
-0.911188810295588));
#84511=CARTESIAN_POINT('Ctrl Pts',(-0.148249517976513,-0.25411753268858,
-0.91198762194418));
#84512=CARTESIAN_POINT('Ctrl Pts',(-0.162504802410936,-0.245801148440465,
-0.912885964921172));
#84513=CARTESIAN_POINT('Ctrl Pts',(-0.176103433444403,-0.236255071919387,
-0.913784307898164));
#84514=CARTESIAN_POINT('Ctrl Pts',(-0.1888256923921,-0.22560695444211,-0.914682650875156));
#84515=CARTESIAN_POINT('Ctrl Pts',(-0.201523318812107,-0.21497945359036,
-0.915579254502371));
#84516=CARTESIAN_POINT('Ctrl Pts',(-0.213347299436118,-0.203254598677624,
-0.916475858129586));
#84517=CARTESIAN_POINT('Ctrl Pts',(-0.224107789841095,-0.190602566962095,
-0.917372461756802));
#84518=CARTESIAN_POINT('Ctrl Pts',(-0.234866432701281,-0.177952707563477,
-0.918268911439792));
#84519=CARTESIAN_POINT('Ctrl Pts',(-0.244561396867179,-0.164376554051912,
-0.919165361122782));
#84520=CARTESIAN_POINT('Ctrl Pts',(-0.253040729395735,-0.150080076182265,
-0.920061810805772));
#84521=CARTESIAN_POINT('Ctrl Pts',(-0.261517828470805,-0.135787364000332,
-0.920958024364201));
#84522=CARTESIAN_POINT('Ctrl Pts',(-0.26877953739386,-0.12077539030623,
-0.92185423792263));
#84523=CARTESIAN_POINT('Ctrl Pts',(-0.274718971229571,-0.105276430631771,
-0.92275045148106));
#84524=CARTESIAN_POINT('Ctrl Pts',(-0.280672576873383,-0.0897404896071807,
-0.923648803453169));
#84525=CARTESIAN_POINT('Ctrl Pts',(-0.285297346785762,-0.0737159932216456,
-0.924547155425279));
#84526=CARTESIAN_POINT('Ctrl Pts',(-0.288535674185864,-0.0574526302453492,
-0.925445507397388));
#84527=CARTESIAN_POINT('Ctrl Pts',(-0.291415184366136,-0.0429913008398588,
-0.926244319045981));
#84528=CARTESIAN_POINT('Ctrl Pts',(-0.293199167584255,-0.0283416956942673,
-0.927043130694573));
#84529=CARTESIAN_POINT('Ctrl Pts',(-0.293881667635058,-0.0136823034624134,
-0.927841942343165));
#84530=CARTESIAN_POINT('Ctrl Pts',(-0.294092545212991,-0.00915287211042962,
-0.928088757659124));
#84531=CARTESIAN_POINT('Ctrl Pts',(-0.294198715293188,-0.00461852814225763,
-0.928335572975082));
#84532=CARTESIAN_POINT('Ctrl Pts',(-0.294199988411877,-8.25739160334692E-5,
-0.92858238829104));
#84533=CARTESIAN_POINT('',(-0.294199928089091,-0.000205699718015333,-1.0285823844888));
#84534=CARTESIAN_POINT('Ctrl Pts',(-0.294199988411901,-8.25738279557236E-5,
-0.928582388295833));
#84535=CARTESIAN_POINT('Ctrl Pts',(-0.294204588369096,0.0163064853534643,
-0.929474167757955));
#84536=CARTESIAN_POINT('Ctrl Pts',(-0.292835398088322,0.0327506834817695,
-0.930365947220078));
#84537=CARTESIAN_POINT('Ctrl Pts',(-0.290090925180525,0.0489989298649158,
-0.931257726682201));
#84538=CARTESIAN_POINT('Ctrl Pts',(-0.287351618275598,0.065216591691298,
-0.932147827521355));
#84539=CARTESIAN_POINT('Ctrl Pts',(-0.283242232594176,0.0812382391810373,
-0.933037928360509));
#84540=CARTESIAN_POINT('Ctrl Pts',(-0.277813078325176,0.0968170104449095,
-0.933928029199663));
#84541=CARTESIAN_POINT('Ctrl Pts',(-0.272384564382425,0.112393944314655,
-0.934818025058391));
#84542=CARTESIAN_POINT('Ctrl Pts',(-0.265636807836933,0.127527332514309,
-0.935708020917118));
#84543=CARTESIAN_POINT('Ctrl Pts',(-0.257670104915801,0.141985059188213,
-0.936598016775846));
#84544=CARTESIAN_POINT('Ctrl Pts',(-0.249704640544348,0.156440538180369,
-0.937487874270673));
#84545=CARTESIAN_POINT('Ctrl Pts',(-0.240521009294745,0.170219868849409,
-0.938377731765501));
#84546=CARTESIAN_POINT('Ctrl Pts',(-0.230264818119774,0.183116775682261,
-0.939267589260328));
#84547=CARTESIAN_POINT('Ctrl Pts',(-0.219985348277369,0.196042954863879,
-0.940159466481225));
#84548=CARTESIAN_POINT('Ctrl Pts',(-0.208628991984662,0.20808210742422,
-0.941051343702122));
#84549=CARTESIAN_POINT('Ctrl Pts',(-0.196380791085716,0.219062148470585,
-0.941943220923018));
#84550=CARTESIAN_POINT('Ctrl Pts',(-0.188355916554445,0.226256139855299,
-0.942527568196062));
#84551=CARTESIAN_POINT('Ctrl Pts',(-0.179948978537917,0.232996246832922,
-0.943111915469106));
#84552=CARTESIAN_POINT('Ctrl Pts',(-0.171219041481126,0.23924397554439,
-0.94369626274215));
#84553=CARTESIAN_POINT('Ctrl Pts',(-0.157798122095816,0.248848885961546,
-0.944594605719142));
#84554=CARTESIAN_POINT('Ctrl Pts',(-0.143523812053577,0.257351498251228,
-0.945492948696134));
#84555=CARTESIAN_POINT('Ctrl Pts',(-0.128602485997264,0.264603553633211,
-0.946391291673125));
#84556=CARTESIAN_POINT('Ctrl Pts',(-0.113710050248783,0.271841567762318,
-0.947287895300341));
#84557=CARTESIAN_POINT('Ctrl Pts',(-0.0981737596890333,0.277833430257783,
-0.948184498927556));
#84558=CARTESIAN_POINT('Ctrl Pts',(-0.0822265696984143,0.282475540951127,
-0.949081102554771));
#84559=CARTESIAN_POINT('Ctrl Pts',(-0.0662821177937581,0.287116854607618,
-0.949977552237761));
#84560=CARTESIAN_POINT('Ctrl Pts',(-0.0499276489994926,0.290408605631773,
-0.950874001920751));
#84561=CARTESIAN_POINT('Ctrl Pts',(-0.0334132751689965,0.292296412982577,
-0.951770451603741));
#84562=CARTESIAN_POINT('Ctrl Pts',(-0.016903251219302,0.294183723085526,
-0.952666665162171));
#84563=CARTESIAN_POINT('Ctrl Pts',(-0.000234193245550827,0.294667744720733,
-0.9535628787206));
#84564=CARTESIAN_POINT('Ctrl Pts',(0.0163382230062328,0.293745982898488,
-0.954459092279029));
#84565=CARTESIAN_POINT('Ctrl Pts',(0.0329501819331874,0.292822021703033,
-0.955357444251139));
#84566=CARTESIAN_POINT('Ctrl Pts',(0.0494642468985899,0.290485648558417,
-0.956255796223248));
#84567=CARTESIAN_POINT('Ctrl Pts',(0.0656290149933198,0.286786457823598,
-0.957154148195358));
#84568=CARTESIAN_POINT('Ctrl Pts',(0.0800026741511515,0.283497149466652,
-0.95795295984395));
#84569=CARTESIAN_POINT('Ctrl Pts',(0.0940999003317329,0.279131174082159,
-0.958751771492543));
#84570=CARTESIAN_POINT('Ctrl Pts',(0.107755391117469,0.273756124470524,
-0.959550583141136));
#84571=CARTESIAN_POINT('Ctrl Pts',(0.123112345746703,0.267711347734855,
-0.960448926118127));
#84572=CARTESIAN_POINT('Ctrl Pts',(0.138007890201815,0.26035111008134,-0.961347269095119));
#84573=CARTESIAN_POINT('Ctrl Pts',(0.152205406482096,0.251768056428174,
-0.96224561207211));
#84574=CARTESIAN_POINT('Ctrl Pts',(0.166375433877397,0.243201621074292,
-0.963142215699325));
#84575=CARTESIAN_POINT('Ctrl Pts',(0.179849412615261,0.23341741760681,-0.96403881932654));
#84576=CARTESIAN_POINT('Ctrl Pts',(0.192413763100579,0.222554675910156,
-0.964935422953755));
#84577=CARTESIAN_POINT('Ctrl Pts',(0.204975956323599,0.211693799314538,
-0.965831872636745));
#84578=CARTESIAN_POINT('Ctrl Pts',(0.216628200390941,0.199755228104271,
-0.966728322319735));
#84579=CARTESIAN_POINT('Ctrl Pts',(0.227188904550832,0.186919345304313,
-0.967624772002725));
#84580=CARTESIAN_POINT('Ctrl Pts',(0.237746827024616,0.17408684347179,-0.968520985561154));
#84581=CARTESIAN_POINT('Ctrl Pts',(0.247213286139144,0.160358117292406,
-0.969417199119583));
#84582=CARTESIAN_POINT('Ctrl Pts',(0.255447219515767,0.145946421818638,
-0.970313412678013));
#84583=CARTESIAN_POINT('Ctrl Pts',(0.263700799499615,0.131500339265514,
-0.971211764650122));
#84584=CARTESIAN_POINT('Ctrl Pts',(0.270715609235867,0.116368735731305,
-0.972110116622231));
#84585=CARTESIAN_POINT('Ctrl Pts',(0.276396631947984,0.100789591961723,
-0.97300846859434));
#84586=CARTESIAN_POINT('Ctrl Pts',(0.281448178846364,0.0869366680470235,
-0.973807280242934));
#84587=CARTESIAN_POINT('Ctrl Pts',(0.285445733982361,0.072730574988778,
-0.974606091891527));
#84588=CARTESIAN_POINT('Ctrl Pts',(0.288356186683529,0.0583468045511799,
-0.97540490354012));
#84589=CARTESIAN_POINT('Ctrl Pts',(0.291629279594187,0.0421708271752409,
-0.976303246517112));
#84590=CARTESIAN_POINT('Ctrl Pts',(0.293547398864424,0.0256671560261943,
-0.977201589494104));
#84591=CARTESIAN_POINT('Ctrl Pts',(0.294059699922176,0.00908476095888113,
-0.978099932471096));
#84592=CARTESIAN_POINT('Ctrl Pts',(0.294571009075106,-0.00746552767927422,
-0.978996536098311));
#84593=CARTESIAN_POINT('Ctrl Pts',(0.293681813083,-0.0240934581280533,-0.979893139725527));
#84594=CARTESIAN_POINT('Ctrl Pts',(0.291392892362341,-0.0405440782446629,
-0.980789743352743));
#84595=CARTESIAN_POINT('Ctrl Pts',(0.289104364642687,-0.056991873837822,
-0.981686193035733));
#84596=CARTESIAN_POINT('Ctrl Pts',(0.285416645893085,-0.0732616312045314,
-0.982582642718723));
#84597=CARTESIAN_POINT('Ctrl Pts',(0.280382446964167,-0.0891028811789288,
-0.983479092401713));
#84598=CARTESIAN_POINT('Ctrl Pts',(0.275349574041641,-0.104939958573134,
-0.984375305960143));
#84599=CARTESIAN_POINT('Ctrl Pts',(0.268971175164861,-0.120348001876696,
-0.985271519518573));
#84600=CARTESIAN_POINT('Ctrl Pts',(0.261349582064675,-0.135092693935016,
-0.986167733077002));
#84601=CARTESIAN_POINT('Ctrl Pts',(0.253709803434047,-0.149872567620426,
-0.987066085049112));
#84602=CARTESIAN_POINT('Ctrl Pts',(0.244821294629877,-0.163985235418924,
-0.987964437021221));
#84603=CARTESIAN_POINT('Ctrl Pts',(0.234832169121801,-0.177221591081758,
-0.988862788993331));
#84604=CARTESIAN_POINT('Ctrl Pts',(0.225949871244333,-0.188991315439945,
-0.989661600641922));
#84605=CARTESIAN_POINT('Ctrl Pts',(0.216198248486144,-0.20006829068708,
-0.990460412290513));
#84606=CARTESIAN_POINT('Ctrl Pts',(0.20570660980217,-0.210329338618506,
-0.991259223939104));
#84607=CARTESIAN_POINT('Ctrl Pts',(0.19390772085819,-0.22186890537624,-0.992157566916095));
#84608=CARTESIAN_POINT('Ctrl Pts',(0.181097297278634,-0.232449235741734,
-0.993055909893087));
#84609=CARTESIAN_POINT('Ctrl Pts',(0.167456685694875,-0.241892328146404,
-0.993954252870079));
#84610=CARTESIAN_POINT('Ctrl Pts',(0.153842484730798,-0.251317137065721,
-0.994850856497294));
#84611=CARTESIAN_POINT('Ctrl Pts',(0.139401891896317,-0.259608579588606,
-0.995747460124509));
#84612=CARTESIAN_POINT('Ctrl Pts',(0.124349335150208,-0.266628735975141,
-0.996644063751725));
#84613=CARTESIAN_POINT('Ctrl Pts',(0.109299362884145,-0.273647687021319,
-0.997540513434715));
#84614=CARTESIAN_POINT('Ctrl Pts',(0.0936383277748143,-0.279395404277063,
-0.998436963117705));
#84615=CARTESIAN_POINT('Ctrl Pts',(0.077605120709974,-0.283779994431585,
-0.999333412800695));
#84616=CARTESIAN_POINT('Ctrl Pts',(0.0615761367867639,-0.288163429686457,
-1.00022962635912));
#84617=CARTESIAN_POINT('Ctrl Pts',(0.0451759416647873,-0.291184252527466,
-1.00112583991755));
#84618=CARTESIAN_POINT('Ctrl Pts',(0.0286568389950925,-0.292800999962106,
-1.00202205347598));
#84619=CARTESIAN_POINT('Ctrl Pts',(0.0120983208592947,-0.294421605042951,
-1.00292040544809));
#84620=CARTESIAN_POINT('Ctrl Pts',(-0.0045788782537557,-0.29463139278357,
-1.0038187574202));
#84621=CARTESIAN_POINT('Ctrl Pts',(-0.0211187325561017,-0.293441031785304,
-1.00471710939231));
#84622=CARTESIAN_POINT('Ctrl Pts',(-0.0358259171484693,-0.292382566661426,
-1.0055159210409));
#84623=CARTESIAN_POINT('Ctrl Pts',(-0.0504241228796736,-0.290217868882573,
-1.0063147326895));
#84624=CARTESIAN_POINT('Ctrl Pts',(-0.0647396718010162,-0.286988527462505,
-1.00711354433809));
#84625=CARTESIAN_POINT('Ctrl Pts',(-0.0808389273112742,-0.283356812539297,
-1.00801188731508));
#84626=CARTESIAN_POINT('Ctrl Pts',(-0.0966828133703411,-0.278354651258673,
-1.00891023029207));
#84627=CARTESIAN_POINT('Ctrl Pts',(-0.112023349778221,-0.272037514149182,
-1.00980857326906));
#84628=CARTESIAN_POINT('Ctrl Pts',(-0.127334184213414,-0.26573260812659,
-1.01070517689628));
#84629=CARTESIAN_POINT('Ctrl Pts',(-0.142142855419589,-0.258118017026034,
-1.01160178052349));
#84630=CARTESIAN_POINT('Ctrl Pts',(-0.15621704662262,-0.249298765228603,
-1.01249838415071));
#84631=CARTESIAN_POINT('Ctrl Pts',(-0.170288821328098,-0.240481027670966,
-1.0133948338337));
#84632=CARTESIAN_POINT('Ctrl Pts',(-0.183625670208904,-0.230459414214168,
-1.01429128351669));
#84633=CARTESIAN_POINT('Ctrl Pts',(-0.196020614124134,-0.219384499995778,
-1.01518773319967));
#84634=CARTESIAN_POINT('Ctrl Pts',(-0.208412293215094,-0.208312502906257,
-1.0160839467581));
#84635=CARTESIAN_POINT('Ctrl Pts',(-0.219861977160234,-0.196188291252235,
-1.01698016031653));
#84636=CARTESIAN_POINT('Ctrl Pts',(-0.230197727149494,-0.183201109208452,
-1.01787637387496));
#84637=CARTESIAN_POINT('Ctrl Pts',(-0.24055813879329,-0.170182939050861,
-1.01877472584707));
#84638=CARTESIAN_POINT('Ctrl Pts',(-0.249798834234182,-0.156298324222916,
-1.01967307781918));
#84639=CARTESIAN_POINT('Ctrl Pts',(-0.257789610195065,-0.141767968439547,
-1.02057142979129));
#84640=CARTESIAN_POINT('Ctrl Pts',(-0.264894982161803,-0.128847623387292,
-1.02137024143988));
#84641=CARTESIAN_POINT('Ctrl Pts',(-0.271012562110784,-0.115417480327191,
-1.02216905308848));
#84642=CARTESIAN_POINT('Ctrl Pts',(-0.27608285972775,-0.101645927437097,
-1.02296786473708));
#84643=CARTESIAN_POINT('Ctrl Pts',(-0.282617632419822,-0.083896679848063,
-1.0239974004649));
#84644=CARTESIAN_POINT('Ctrl Pts',(-0.287447179404754,-0.0654875880066178,
-1.02502693619272));
#84645=CARTESIAN_POINT('Ctrl Pts',(-0.290464678823977,-0.0467323266667069,
-1.02605647192054));
#84646=CARTESIAN_POINT('Ctrl Pts',(-0.2929324383204,-0.031393972669156,
-1.02689844277663));
#84647=CARTESIAN_POINT('Ctrl Pts',(-0.294189007618607,-0.0158245914797193,
-1.02774041363272));
#84648=CARTESIAN_POINT('Ctrl Pts',(-0.294199928089091,-0.000205699718015333,
-1.0285823844888));
#84649=CARTESIAN_POINT('',(-0.293916367631718,0.000220716887012043,-1.12858238829104));
#84650=CARTESIAN_POINT('Ctrl Pts',(-0.293881989377092,-0.000205406963665611,
-1.02858238829104));
#84651=CARTESIAN_POINT('Ctrl Pts',(-0.293473254748503,0.0630439083385033,
-1.03199565390605));
#84652=CARTESIAN_POINT('Ctrl Pts',(-0.242431600377607,0.22482394576972,
-1.04069369298737));
#84653=CARTESIAN_POINT('Ctrl Pts',(0.0238745824446583,0.346742558480913,
-1.05467650553506));
#84654=CARTESIAN_POINT('Ctrl Pts',(0.304028168071522,0.16842586074448,-1.07053082593402));
#84655=CARTESIAN_POINT('Ctrl Pts',(0.30662388542524,-0.163652651781727,
-1.08638514633302));
#84656=CARTESIAN_POINT('Ctrl Pts',(0.0292920140283848,-0.346326977672701,
-1.10223946673199));
#84657=CARTESIAN_POINT('Ctrl Pts',(-0.240478109422872,-0.227887870294271,
-1.11630521405135));
#84658=CARTESIAN_POINT('Ctrl Pts',(-0.29346304387379,-0.0645463479691509,
-1.12508618790436));
#84659=CARTESIAN_POINT('Ctrl Pts',(-0.293916367631718,0.000220716887012043,
-1.12858238829104));
#84660=CARTESIAN_POINT('',(-0.294666739399022,5.55183184013965E-5,-1.22858238829104));
#84661=CARTESIAN_POINT('Ctrl Pts',(-0.293916367631718,0.000220716887012043,
-1.12858238829104));
#84662=CARTESIAN_POINT('Ctrl Pts',(-0.294148277299391,0.0333540089861818,
-1.13037096137068));
#84663=CARTESIAN_POINT('Ctrl Pts',(-0.273700019748768,0.164109867608507,
-1.13744430791668));
#84664=CARTESIAN_POINT('Ctrl Pts',(-0.0817731457554239,0.337806971788931,
-1.14980242792894));
#84665=CARTESIAN_POINT('Ctrl Pts',(0.239104754541022,0.252248516133763,
-1.16565674832794));
#84666=CARTESIAN_POINT('Ctrl Pts',(0.341695624457678,-0.063596366052773,
-1.18151106872693));
#84667=CARTESIAN_POINT('Ctrl Pts',(0.132340697599494,-0.321381918213206,
-1.19736538912591));
#84668=CARTESIAN_POINT('Ctrl Pts',(-0.194419760005066,-0.286134902300222,
-1.21305582898062));
#84669=CARTESIAN_POINT('Ctrl Pts',(-0.294421732944348,-0.0941869120255346,
-1.22346149536899));
#84670=CARTESIAN_POINT('Ctrl Pts',(-0.294666739399022,5.55183184013965E-5,
-1.22858238829104));
#84671=CARTESIAN_POINT('',(-0.294199884378713,-0.000260828587339853,-1.32858238829104));
#84672=CARTESIAN_POINT('Ctrl Pts',(-0.294666739399022,5.55183184013965E-5,
-1.22858238829104));
#84673=CARTESIAN_POINT('Ctrl Pts',(-0.294674580178307,0.00307149639374388,
-1.22874626883532));
#84674=CARTESIAN_POINT('Ctrl Pts',(-0.293267859366203,0.103338389888432,
-1.23419492284593));
#84675=CARTESIAN_POINT('Ctrl Pts',(-0.179811334202771,0.297436181275677,
-1.24492835032287));
#84676=CARTESIAN_POINT('Ctrl Pts',(0.151931039768365,0.312597754286858,
-1.26078267072184));
#84677=CARTESIAN_POINT('Ctrl Pts',(0.344970294287786,0.0423779900056762,
-1.27663699112084));
#84678=CARTESIAN_POINT('Ctrl Pts',(0.223074190979041,-0.266530119498471,
-1.29249131151981));
#84679=CARTESIAN_POINT('Ctrl Pts',(-0.102474082261184,-0.332113617376057,
-1.30834563191881));
#84680=CARTESIAN_POINT('Ctrl Pts',(-0.278513916599102,-0.151810516675863,
-1.3203759701921));
#84681=CARTESIAN_POINT('Ctrl Pts',(-0.294307334922772,-0.0272861447661987,
-1.32712153499908));
#84682=CARTESIAN_POINT('Ctrl Pts',(-0.294074822703788,-0.000261863787000156,
-1.32858232633972));
#84683=CARTESIAN_POINT('',(-0.294199971607144,0.000129253068963336,-1.42858238829403));
#84684=CARTESIAN_POINT('Ctrl Pts',(-0.294199884378713,-0.000260828587339853,
-1.32858238829104));
#84685=CARTESIAN_POINT('Ctrl Pts',(-0.294214457430896,0.0161767494828003,
-1.32947054750874));
#84686=CARTESIAN_POINT('Ctrl Pts',(-0.292847107883467,0.0326438671053959,
-1.33035870672644));
#84687=CARTESIAN_POINT('Ctrl Pts',(-0.290109413072103,0.0488893490134608,
-1.33124686594414));
#84688=CARTESIAN_POINT('Ctrl Pts',(-0.287371187498568,0.065137980464425,
-1.33213519735098));
#84689=CARTESIAN_POINT('Ctrl Pts',(-0.283262188325697,0.081164091081889,
-1.33302352875782));
#84690=CARTESIAN_POINT('Ctrl Pts',(-0.277845619751207,0.0967235833965424,
-1.33391186016466));
#84691=CARTESIAN_POINT('Ctrl Pts',(-0.272428273701776,0.112285309065243,
-1.33480031907942));
#84692=CARTESIAN_POINT('Ctrl Pts',(-0.265703282052838,0.127379533890134,
-1.33568877799418));
#84693=CARTESIAN_POINT('Ctrl Pts',(-0.257782474987569,0.141780942264056,
-1.33657723690894));
#84694=CARTESIAN_POINT('Ctrl Pts',(-0.249844243100468,0.156214032002386,
-1.33746765032634));
#84695=CARTESIAN_POINT('Ctrl Pts',(-0.240705391305208,0.169950591334069,
-1.33835806374374));
#84696=CARTESIAN_POINT('Ctrl Pts',(-0.230521576920559,0.182793442371598,
-1.33924847716113));
#84697=CARTESIAN_POINT('Ctrl Pts',(-0.22744956856644,0.18666756499283,-1.33951707567968));
#84698=CARTESIAN_POINT('Ctrl Pts',(-0.224282741142796,0.190460603695425,
-1.33978567419823));
#84699=CARTESIAN_POINT('Ctrl Pts',(-0.221026025179474,0.194167804214197,
-1.34005427271677));
#84700=CARTESIAN_POINT('Ctrl Pts',(-0.210133752067151,0.206566748729891,
-1.34095261584971));
#84701=CARTESIAN_POINT('Ctrl Pts',(-0.198160287921806,0.218085713957663,
-1.34185095898264));
#84702=CARTESIAN_POINT('Ctrl Pts',(-0.18527299639449,0.228533491652771,
-1.34274930211558));
#84703=CARTESIAN_POINT('Ctrl Pts',(-0.172410657020504,0.238961040539487,
-1.34364590589191));
#84704=CARTESIAN_POINT('Ctrl Pts',(-0.158638568371357,0.248320975255663,
-1.34454250966825));
#84705=CARTESIAN_POINT('Ctrl Pts',(-0.144160112338002,0.256459552387301,
-1.34543911344458));
#84706=CARTESIAN_POINT('Ctrl Pts',(-0.129684142413037,0.264596732036718,
-1.3463355632643));
#84707=CARTESIAN_POINT('Ctrl Pts',(-0.114502707569499,0.271512538177124,
-1.34723201308401));
#84708=CARTESIAN_POINT('Ctrl Pts',(-0.0988470638600188,0.277097271668729,
-1.34812846290372));
#84709=CARTESIAN_POINT('Ctrl Pts',(-0.0831955439561307,0.282680534102635,
-1.34902467659231));
#84710=CARTESIAN_POINT('Ctrl Pts',(-0.0670708121268936,0.286933164451199,
-1.3499208902809));
#84711=CARTESIAN_POINT('Ctrl Pts',(-0.0507213131812425,0.289794734923135,
-1.35081710396949));
#84712=CARTESIAN_POINT('Ctrl Pts',(-0.0343328037034058,0.292663133212082,
-1.35171545605834));
#84713=CARTESIAN_POINT('Ctrl Pts',(-0.0177192430968529,0.294133731906785,
-1.3526138081472));
#84714=CARTESIAN_POINT('Ctrl Pts',(-0.00113673073858106,0.294197803940186,
-1.35351216023605));
#84715=CARTESIAN_POINT('Ctrl Pts',(0.0136083706295909,0.294254776527147,
-1.35431097119596));
#84716=CARTESIAN_POINT('Ctrl Pts',(0.0283284775460612,0.293200444401833,
-1.35510978215586));
#84717=CARTESIAN_POINT('Ctrl Pts',(0.0428472643703829,0.291063140806208,
-1.35590859311576));
#84718=CARTESIAN_POINT('Ctrl Pts',(0.0591751221422548,0.288659524750202,
-1.35680693757785));
#84719=CARTESIAN_POINT('Ctrl Pts',(0.0753519966548785,0.284870068190489,
-1.35770528203994));
#84720=CARTESIAN_POINT('Ctrl Pts',(0.0911264218009641,0.279731326900926,
-1.35860362650203));
#84721=CARTESIAN_POINT('Ctrl Pts',(0.106870305115145,0.274602535043512,
-1.35950023162431));
#84722=CARTESIAN_POINT('Ctrl Pts',(0.122212521910924,0.268129823766632,
-1.3603968367466));
#84723=CARTESIAN_POINT('Ctrl Pts',(0.136913476641977,0.260400345456389,
-1.36129344186888));
#84724=CARTESIAN_POINT('Ctrl Pts',(0.151611907154874,0.252672194331343,
-1.36218989304015));
#84725=CARTESIAN_POINT('Ctrl Pts',(0.165668571712451,0.243688025021323,
-1.36308634421142));
#84726=CARTESIAN_POINT('Ctrl Pts',(0.178865694570038,0.233582326613076,
-1.36398279538269));
#84727=CARTESIAN_POINT('Ctrl Pts',(0.192059341298967,0.223479290050765,
-1.36487901042828));
#84728=CARTESIAN_POINT('Ctrl Pts',(0.204393274255127,0.212255800656612,
-1.36577522547386));
#84729=CARTESIAN_POINT('Ctrl Pts',(0.215681732862412,0.200087556108488,
-1.36667144051945));
#84730=CARTESIAN_POINT('Ctrl Pts',(0.226997125875596,0.187890277974012,
-1.36756979394555));
#84731=CARTESIAN_POINT('Ctrl Pts',(0.237261541710229,0.17474434307023,-1.36846814737164));
#84732=CARTESIAN_POINT('Ctrl Pts',(0.246328456267685,0.160859975235542,
-1.36936650079773));
#84733=CARTESIAN_POINT('Ctrl Pts',(0.25439063933822,0.148514175063657,-1.37016530503674));
#84734=CARTESIAN_POINT('Ctrl Pts',(0.261506436947392,0.135585335079062,
-1.37096410927574));
#84735=CARTESIAN_POINT('Ctrl Pts',(0.267603794682592,0.122236856436498,
-1.37176291351475));
#84736=CARTESIAN_POINT('Ctrl Pts',(0.274460914295383,0.107225089261934,
-1.37266125283679));
#84737=CARTESIAN_POINT('Ctrl Pts',(0.280072727254961,0.0915868095519443,
-1.37355959215882));
#84738=CARTESIAN_POINT('Ctrl Pts',(0.284333237639734,0.075552961380124,
-1.37445793148086));
#84739=CARTESIAN_POINT('Ctrl Pts',(0.288585498914575,0.0595501576053983,
-1.37535453145734));
#84740=CARTESIAN_POINT('Ctrl Pts',(0.291491386675606,0.0431540444954077,
-1.37625113143382));
#84741=CARTESIAN_POINT('Ctrl Pts',(0.292993827122456,0.0266131033165356,
-1.3771477314103));
#84742=CARTESIAN_POINT('Ctrl Pts',(0.294496009703126,0.0100750010849986,
-1.37804417750193));
#84743=CARTESIAN_POINT('Ctrl Pts',(0.294595099449247,-0.00660709924303613,
-1.37894062359357));
#84744=CARTESIAN_POINT('Ctrl Pts',(0.293285616170215,-0.0231773024240751,
-1.37983706968521));
#84745=CARTESIAN_POINT('Ctrl Pts',(0.291976477771621,-0.039743141487598,
-1.38073327967858));
#84746=CARTESIAN_POINT('Ctrl Pts',(0.289259576137544,-0.0561963539634961,
-1.38162948967196));
#84747=CARTESIAN_POINT('Ctrl Pts',(0.285181422377442,-0.0722855195096436,
-1.38252569966534));
#84748=CARTESIAN_POINT('Ctrl Pts',(0.281093537348228,-0.0884130769382262,
-1.38342404819031));
#84749=CARTESIAN_POINT('Ctrl Pts',(0.275638133828674,-0.10417408897145,
-1.38432239671527));
#84750=CARTESIAN_POINT('Ctrl Pts',(0.268912030090887,-0.11933130382426,
-1.38522074524024));
#84751=CARTESIAN_POINT('Ctrl Pts',(0.262931043507767,-0.132809403806991,
-1.38601957479807));
#84752=CARTESIAN_POINT('Ctrl Pts',(0.255946204099478,-0.145809991572696,
-1.3868184043559));
#84753=CARTESIAN_POINT('Ctrl Pts',(0.248055515898018,-0.158183757170477,
-1.38761723391373));
#84754=CARTESIAN_POINT('Ctrl Pts',(0.239181831423695,-0.172099006242618,
-1.3885155790598));
#84755=CARTESIAN_POINT('Ctrl Pts',(0.229105382710018,-0.185309478845056,
-1.38941392420587));
#84756=CARTESIAN_POINT('Ctrl Pts',(0.217962411488752,-0.197600676056556,
-1.39031226935195));
#84757=CARTESIAN_POINT('Ctrl Pts',(0.206841015525056,-0.209868074790934,
-1.39120887510306));
#84758=CARTESIAN_POINT('Ctrl Pts',(0.194657672567564,-0.221219107756348,
-1.39210548085418));
#84759=CARTESIAN_POINT('Ctrl Pts',(0.181589935508457,-0.231470808790298,
-1.3930020866053));
#84760=CARTESIAN_POINT('Ctrl Pts',(0.168524443573054,-0.241720748514168,
-1.39389853831362));
#84761=CARTESIAN_POINT('Ctrl Pts',(0.154575447180179,-0.250871203132498,
-1.39479499002194));
#84762=CARTESIAN_POINT('Ctrl Pts',(0.139954765137329,-0.25877848387251,
-1.39569144173025));
#84763=CARTESIAN_POINT('Ctrl Pts',(0.125337934993483,-0.266683681395972,
-1.39658765726344));
#84764=CARTESIAN_POINT('Ctrl Pts',(0.110050471734688,-0.273345988513023,
-1.39748387279663));
#84765=CARTESIAN_POINT('Ctrl Pts',(0.0943286970484332,-0.278667789514944,
-1.39838008832982));
#84766=CARTESIAN_POINT('Ctrl Pts',(0.0785694116177297,-0.284002287856787,
-1.3992784421529));
#84767=CARTESIAN_POINT('Ctrl Pts',(0.06237450618845,-0.28798966286102,-1.40017679597598));
#84768=CARTESIAN_POINT('Ctrl Pts',(0.0459957532466042,-0.29058222706022,
-1.40107514979906));
#84769=CARTESIAN_POINT('Ctrl Pts',(0.0314320344127203,-0.292887492680259,
-1.40187395130361));
#84770=CARTESIAN_POINT('Ctrl Pts',(0.0167235182312306,-0.294090670138664,
-1.40267275280817));
#84771=CARTESIAN_POINT('Ctrl Pts',(0.00204878209681707,-0.294192866147226,
-1.40347155431272));
#84772=CARTESIAN_POINT('Ctrl Pts',(-0.0144547871297883,-0.294307798292277,
-1.4043699061337));
#84773=CARTESIAN_POINT('Ctrl Pts',(-0.0310205105826716,-0.29303005215292,
-1.40526825795467));
#84774=CARTESIAN_POINT('Ctrl Pts',(-0.0473942850564051,-0.290357403459929,
-1.40616660977565));
#84775=CARTESIAN_POINT('Ctrl Pts',(-0.0637363587694816,-0.28768992919979,
-1.40706322232532));
#84776=CARTESIAN_POINT('Ctrl Pts',(-0.079886438858722,-0.283632974159542,
-1.407959834875));
#84777=CARTESIAN_POINT('Ctrl Pts',(-0.0955944370975883,-0.278236129206822,
-1.40885644742467));
#84778=CARTESIAN_POINT('Ctrl Pts',(-0.11129973813358,-0.272840210940335,
-1.409752906018));
#84779=CARTESIAN_POINT('Ctrl Pts',(-0.126562345130107,-0.266105066013107,
-1.41064936461133));
#84780=CARTESIAN_POINT('Ctrl Pts',(-0.141146514708509,-0.258130396090117,
-1.41154582320467));
#84781=CARTESIAN_POINT('Ctrl Pts',(-0.155726843005352,-0.250157826591999,
-1.4124420456824));
#84782=CARTESIAN_POINT('Ctrl Pts',(-0.16962839967055,-0.24094676949677,
-1.41333826816014));
#84783=CARTESIAN_POINT('Ctrl Pts',(-0.182640796697551,-0.23064253593317,
-1.41423449063788));
#84784=CARTESIAN_POINT('Ctrl Pts',(-0.195684239174444,-0.220313718154525,
-1.41513285135579));
#84785=CARTESIAN_POINT('Ctrl Pts',(-0.207833678909567,-0.208887028931223,
-1.4160312120737));
#84786=CARTESIAN_POINT('Ctrl Pts',(-0.218912239215287,-0.196547886078048,
-1.4169295727916));
#84787=CARTESIAN_POINT('Ctrl Pts',(-0.22876261624213,-0.185576676287448,
-1.4177283400983));
#84788=CARTESIAN_POINT('Ctrl Pts',(-0.237766686379653,-0.173884970186014,
-1.418527107405));
#84789=CARTESIAN_POINT('Ctrl Pts',(-0.245828328475075,-0.16162324374653,
-1.4193258747117));
#84790=CARTESIAN_POINT('Ctrl Pts',(-0.255067937885253,-0.147569833578445,
-1.42024135791427));
#84791=CARTESIAN_POINT('Ctrl Pts',(-0.263125967190795,-0.132680482413092,
-1.42115684111684));
#84792=CARTESIAN_POINT('Ctrl Pts',(-0.269858553853055,-0.11717508656851,
-1.42207232431942));
#84793=CARTESIAN_POINT('Ctrl Pts',(-0.276575724393973,-0.101705194620988,
-1.42298571126971));
#84794=CARTESIAN_POINT('Ctrl Pts',(-0.281973120566162,-0.0856227113463165,
-1.42389909822));
#84795=CARTESIAN_POINT('Ctrl Pts',(-0.285952486678191,-0.0691723598163232,
-1.4248124851703));
#84796=CARTESIAN_POINT('Ctrl Pts',(-0.289925530565836,-0.0527481438090875,
-1.42572442097559));
#84797=CARTESIAN_POINT('Ctrl Pts',(-0.292484803514074,-0.0359579352967791,
-1.42663635678088));
#84798=CARTESIAN_POINT('Ctrl Pts',(-0.293581844870242,-0.0190614889918173,
-1.42754829258617));
#84799=CARTESIAN_POINT('Ctrl Pts',(-0.293996510664294,-0.0126748762316724,
-1.42789299115446));
#84800=CARTESIAN_POINT('Ctrl Pts',(-0.294202784441153,-0.00627319483703169,
-1.42823768972275));
#84801=CARTESIAN_POINT('Ctrl Pts',(-0.294199971607168,0.000129253013507976,
-1.42858238829104));
#84802=CARTESIAN_POINT('Ctrl Pts',(-0.294199971607144,0.000129253068963212,
-1.42858238829403));
#84803=CARTESIAN_POINT('Ctrl Pts',(-0.294191975027856,0.0183307040540321,
-1.4295623281923));
#84804=CARTESIAN_POINT('Ctrl Pts',(-0.29249067779368,0.036476686751396,
-1.43054226809058));
#84805=CARTESIAN_POINT('Ctrl Pts',(-0.289151433169477,0.054268671404759,
-1.43152220798886));
#84806=CARTESIAN_POINT('Ctrl Pts',(-0.285788906561617,0.0721847058785258,
-1.43250898025411));
#84807=CARTESIAN_POINT('Ctrl Pts',(-0.280765736918653,0.0897412935870321,
-1.43349575251937));
#84808=CARTESIAN_POINT('Ctrl Pts',(-0.27418768992192,0.106652476273555,
-1.43448252478462));
#84809=CARTESIAN_POINT('Ctrl Pts',(-0.272637413883995,0.110638005915544,
-1.43471508155998));
#84810=CARTESIAN_POINT('Ctrl Pts',(-0.271000981417167,0.114587788409907,
-1.43494763833534));
#84811=CARTESIAN_POINT('Ctrl Pts',(-0.269280148701361,0.118498276423637,
-1.4351801951107));
#84812=CARTESIAN_POINT('Ctrl Pts',(-0.262632583131113,0.133604466144566,
-1.43607856041884));
#84813=CARTESIAN_POINT('Ctrl Pts',(-0.254688782871077,0.148197549509576,
-1.43697692572698));
#84814=CARTESIAN_POINT('Ctrl Pts',(-0.245550685018537,0.162044750260313,
-1.43787529103512));
#84815=CARTESIAN_POINT('Ctrl Pts',(-0.236430282646639,0.175865136582404,
-1.43877191670267));
#84816=CARTESIAN_POINT('Ctrl Pts',(-0.226120549143635,0.188941818496891,
-1.43966854237023));
#84817=CARTESIAN_POINT('Ctrl Pts',(-0.214769058735139,0.201066882927106,
-1.44056516803778));
#84818=CARTESIAN_POINT('Ctrl Pts',(-0.203419526870608,0.213189855343769,
-1.44146163900487));
#84819=CARTESIAN_POINT('Ctrl Pts',(-0.191029095476835,0.224360924630009,
-1.44235810997196));
#84820=CARTESIAN_POINT('Ctrl Pts',(-0.177785194385758,0.234405769249006,
-1.44325458093905));
#84821=CARTESIAN_POINT('Ctrl Pts',(-0.164544787233774,0.244447963887831,
-1.4441508154037));
#84822=CARTESIAN_POINT('Ctrl Pts',(-0.150451994427785,0.253364054318814,
-1.44504704986835));
#84823=CARTESIAN_POINT('Ctrl Pts',(-0.135725489750741,0.261021515266312,
-1.445943284333));
#84824=CARTESIAN_POINT('Ctrl Pts',(-0.120963864993721,0.268697237888713,
-1.44684165615657));
#84825=CARTESIAN_POINT('Ctrl Pts',(-0.105566227049724,0.275107993319137,
-1.44774002798013));
#84826=CARTESIAN_POINT('Ctrl Pts',(-0.0897741356302365,0.280168243332188,
-1.4486383998037));
#84827=CARTESIAN_POINT('Ctrl Pts',(-0.0757340402459295,0.284667102347404,
-1.44943710503902));
#84828=CARTESIAN_POINT('Ctrl Pts',(-0.0613828225292932,0.288099109861824,
-1.45023581027434));
#84829=CARTESIAN_POINT('Ctrl Pts',(-0.0468970705487783,0.290438125551627,
-1.45103451550967));
#84830=CARTESIAN_POINT('Ctrl Pts',(-0.0306033336238293,0.293069076734849,
-1.4519329081511));
#84831=CARTESIAN_POINT('Ctrl Pts',(-0.0140357636801972,0.294332984452315,
-1.45283130079253));
#84832=CARTESIAN_POINT('Ctrl Pts',(0.00255482522783669,0.294188906772596,
-1.45372969343397));
#84833=CARTESIAN_POINT('Ctrl Pts',(0.0191133046459322,0.294045107941375,
-1.45462634732281));
#84834=CARTESIAN_POINT('Ctrl Pts',(0.0356939321908188,0.292498673935604,
-1.45552300121165));
#84835=CARTESIAN_POINT('Ctrl Pts',(0.0520419624030031,0.289560484440202,
-1.45641965510049));
#84836=CARTESIAN_POINT('Ctrl Pts',(0.0683871888520291,0.286622798857954,
-1.45731615520903));
#84837=CARTESIAN_POINT('Ctrl Pts',(0.0844991117914871,0.282293919412258,
-1.45821265531756));
#84838=CARTESIAN_POINT('Ctrl Pts',(0.100129522321303,0.276636437874167,
-1.45910915542609));
#84839=CARTESIAN_POINT('Ctrl Pts',(0.115755819145252,0.270980445306244,
-1.46000541958831));
#84840=CARTESIAN_POINT('Ctrl Pts',(0.130900114959361,0.263996824445283,
-1.46090168375053));
#84841=CARTESIAN_POINT('Ctrl Pts',(0.145332304362076,0.25579710965687,-1.46179794791275));
#84842=CARTESIAN_POINT('Ctrl Pts',(0.159798915277226,0.24757783812785,-1.462696349711));
#84843=CARTESIAN_POINT('Ctrl Pts',(0.173549350228455,0.238137095384846,
-1.46359475150924));
#84844=CARTESIAN_POINT('Ctrl Pts',(0.186380506412919,0.227631164011573,
-1.46449315330749));
#84845=CARTESIAN_POINT('Ctrl Pts',(0.197785714225321,0.218292774792987,
-1.46529171417455));
#84846=CARTESIAN_POINT('Ctrl Pts',(0.208464774368804,0.208113689555956,
-1.4660902750416));
#84847=CARTESIAN_POINT('Ctrl Pts',(0.218299831790271,0.197227846513467,
-1.46688883590866));
#84848=CARTESIAN_POINT('Ctrl Pts',(0.229361529350384,0.184984308091408,
-1.4677869942433));
#84849=CARTESIAN_POINT('Ctrl Pts',(0.239425231386049,0.171768251619834,
-1.46868515257794));
#84850=CARTESIAN_POINT('Ctrl Pts',(0.248320266062037,0.157767821379643,
-1.46958331091258));
#84851=CARTESIAN_POINT('Ctrl Pts',(0.257198073101548,0.143794506752994,
-1.47047972972108));
#84852=CARTESIAN_POINT('Ctrl Pts',(0.264911230496258,0.129040458772193,
-1.47137614852958));
#84853=CARTESIAN_POINT('Ctrl Pts',(0.271330418485106,0.113725300635774,
-1.47227256733809));
#84854=CARTESIAN_POINT('Ctrl Pts',(0.277748521405541,0.0984127312994287,
-1.4731688346203));
#84855=CARTESIAN_POINT('Ctrl Pts',(0.282872735543824,0.0825399473615452,
-1.47406510190251));
#84856=CARTESIAN_POINT('Ctrl Pts',(0.286620695905337,0.0663492025478846,
-1.47496136918473));
#84857=CARTESIAN_POINT('Ctrl Pts',(0.290367673058947,0.0501627050759085,
-1.47585740134784));
#84858=CARTESIAN_POINT('Ctrl Pts',(0.292738945429468,0.0336591860535186,
-1.47675343351095));
#84859=CARTESIAN_POINT('Ctrl Pts',(0.293703069443292,0.0170923081995552,
-1.47764946567406));
#84860=CARTESIAN_POINT('Ctrl Pts',(0.294669500245366,0.000485792001759425,
-1.47854764170708));
#84861=CARTESIAN_POINT('Ctrl Pts',(0.294222039052706,-0.0161835908076354,
-1.4794458177401));
#84862=CARTESIAN_POINT('Ctrl Pts',(0.292381480914927,-0.0326605207857176,
-1.48034399377313));
#84863=CARTESIAN_POINT('Ctrl Pts',(0.290742678881914,-0.0473313023229251,
-1.48114371461797));
#84864=CARTESIAN_POINT('Ctrl Pts',(0.288000288634847,-0.0618491557389784,
-1.48194343546281));
#84865=CARTESIAN_POINT('Ctrl Pts',(0.284202955405829,-0.0760415684911374,
-1.48274315630765));
#84866=CARTESIAN_POINT('Ctrl Pts',(0.279936370795273,-0.0919877934292838,
-1.48364170179827));
#84867=CARTESIAN_POINT('Ctrl Pts',(0.274309990599236,-0.107624415566617,
-1.4845402472889));
#84868=CARTESIAN_POINT('Ctrl Pts',(0.26738910759261,-0.122705766534535,
-1.48543879277952));
#84869=CARTESIAN_POINT('Ctrl Pts',(0.260481635580393,-0.137757893498329,
-1.48633559710669));
#84870=CARTESIAN_POINT('Ctrl Pts',(0.252284906269277,-0.15225614735143,
-1.48723240143386));
#84871=CARTESIAN_POINT('Ctrl Pts',(0.242913105765234,-0.16597247677699,
-1.48812920576104));
#84872=CARTESIAN_POINT('Ctrl Pts',(0.233542972951434,-0.179686365413423,
-1.48902585050395));
#84873=CARTESIAN_POINT('Ctrl Pts',(0.222998585385343,-0.192617925420461,
-1.48992249524687));
#84874=CARTESIAN_POINT('Ctrl Pts',(0.211438639738649,-0.204566227969012,
-1.49081913998978));
#84875=CARTESIAN_POINT('Ctrl Pts',(0.199881773859228,-0.216511347285368,
-1.4917155458512));
#84876=CARTESIAN_POINT('Ctrl Pts',(0.18731044474944,-0.227473168339034,
-1.49261195171261));
#84877=CARTESIAN_POINT('Ctrl Pts',(0.173920604502344,-0.237287301239529,
-1.49350835757403));
#84878=CARTESIAN_POINT('Ctrl Pts',(0.160498949731181,-0.247124752713033,
-1.49440689331342));
#84879=CARTESIAN_POINT('Ctrl Pts',(0.146255555677053,-0.255808621693674,
-1.49530542905282));
#84880=CARTESIAN_POINT('Ctrl Pts',(0.131416162592098,-0.263217461824947,
-1.49620396479221));
#84881=CARTESIAN_POINT('Ctrl Pts',(0.118239812598643,-0.269795997082846,
-1.49700180209702));
#84882=CARTESIAN_POINT('Ctrl Pts',(0.104594314999241,-0.275369792109794,
-1.49779963940182));
#84883=CARTESIAN_POINT('Ctrl Pts',(0.0906495987568348,-0.279886209458817,
-1.49859747670663));
#84884=CARTESIAN_POINT('Ctrl Pts',(0.0749437793531616,-0.284973013234692,
-1.49949607431199));
#84885=CARTESIAN_POINT('Ctrl Pts',(0.0587587944839904,-0.288749790801653,
-1.50039467191734));
#84886=CARTESIAN_POINT('Ctrl Pts',(0.0423364127233751,-0.291137885129565,
-1.5012932695227));
#84887=CARTESIAN_POINT('Ctrl Pts',(0.0259457377144457,-0.293521368755147,
-1.50219013220242));
#84888=CARTESIAN_POINT('Ctrl Pts',(0.00931933957586975,-0.294521314058951,
-1.50308699488214));
#84889=CARTESIAN_POINT('Ctrl Pts',(-0.00728924515587781,-0.294109685160243,
-1.50398385756186));
#84890=CARTESIAN_POINT('Ctrl Pts',(-0.0238950319068033,-0.293698125606984,
-1.50488056915077));
#84891=CARTESIAN_POINT('Ctrl Pts',(-0.0404822220529669,-0.291875431161071,
-1.50577728073968));
#84892=CARTESIAN_POINT('Ctrl Pts',(-0.0567958683189227,-0.2886656705289,
-1.50667399232858));
#84893=CARTESIAN_POINT('Ctrl Pts',(-0.0731052556088385,-0.28545674786351,
-1.50757046981451));
#84894=CARTESIAN_POINT('Ctrl Pts',(-0.0891404670749405,-0.280861641434708,
-1.50846694730044));
#84895=CARTESIAN_POINT('Ctrl Pts',(-0.104656992795962,-0.274955548878189,
-1.50936342478637));
#84896=CARTESIAN_POINT('Ctrl Pts',(-0.120210491283834,-0.269035383288374,
-1.51026203839824));
#84897=CARTESIAN_POINT('Ctrl Pts',(-0.135242103164361,-0.261798299921929,
-1.5111606520101));
#84898=CARTESIAN_POINT('Ctrl Pts',(-0.14952718619918,-0.25336783652894,
-1.51205926562197));
#84899=CARTESIAN_POINT('Ctrl Pts',(-0.162205052954496,-0.245885885509028,
-1.51285677611652));
#84900=CARTESIAN_POINT('Ctrl Pts',(-0.174294954879084,-0.237464895427554,
-1.51365428661107));
#84901=CARTESIAN_POINT('Ctrl Pts',(-0.18566054981683,-0.228218755236533,
-1.51445179710562));
#84902=CARTESIAN_POINT('Ctrl Pts',(-0.198280146566755,-0.217952459337103,
-1.51533729943965));
#84903=CARTESIAN_POINT('Ctrl Pts',(-0.210091389466563,-0.206598751621239,
-1.51622280177368));
#84904=CARTESIAN_POINT('Ctrl Pts',(-0.220899703879849,-0.194311504615128,
-1.51710830410771));
#84905=CARTESIAN_POINT('Ctrl Pts',(-0.231686991578213,-0.182048161469517,
-1.51799208376748));
#84906=CARTESIAN_POINT('Ctrl Pts',(-0.241474635807838,-0.16885543968172,
-1.51887586342724));
#84907=CARTESIAN_POINT('Ctrl Pts',(-0.250103755820896,-0.154924986119999,
-1.519759643087));
#84908=CARTESIAN_POINT('Ctrl Pts',(-0.258730243958732,-0.14099878133631,
-1.52064315319462));
#84909=CARTESIAN_POINT('Ctrl Pts',(-0.266198441486775,-0.126335957832702,
-1.52152666330224));
#84910=CARTESIAN_POINT('Ctrl Pts',(-0.272392376581496,-0.111157695101528,
-1.52241017340986));
#84911=CARTESIAN_POINT('Ctrl Pts',(-0.278585354724032,-0.0959817773855132,
-1.5232935470167));
#84912=CARTESIAN_POINT('Ctrl Pts',(-0.283504171834539,-0.0802913404046116,
-1.52417692062355));
#84913=CARTESIAN_POINT('Ctrl Pts',(-0.287081432566884,-0.0643264414945037,
-1.5250602942304));
#84914=CARTESIAN_POINT('Ctrl Pts',(-0.290665314592038,-0.0483319925240926,
-1.52594530290825));
#84915=CARTESIAN_POINT('Ctrl Pts',(-0.292902560389337,-0.03206287409932,
-1.52683031158611));
#84916=CARTESIAN_POINT('Ctrl Pts',(-0.293777160082763,-0.0157676952566583,
-1.52771532026396));
#84917=CARTESIAN_POINT('Ctrl Pts',(-0.294062783432995,-0.010446079426391,
-1.52800434293965));
#84918=CARTESIAN_POINT('Ctrl Pts',(-0.294203493231576,-0.00512168939691457,
-1.52829336561535));
#84919=CARTESIAN_POINT('Ctrl Pts',(-0.294199934127337,0.000196874250640231,
-1.52858238829104));
#84920=CARTESIAN_POINT('Origin',(0.,0.,-1.7456589891905));
#84921=CARTESIAN_POINT('',(0.223369910286723,0.0797362138773924,-0.0399999999999999));
#84922=CARTESIAN_POINT('Ctrl Pts',(0.223369910286723,0.0797362138773924,
-0.0399999999999999));
#84923=CARTESIAN_POINT('Ctrl Pts',(0.227755575186804,0.0674503837928969,
-0.040928151436346));
#84924=CARTESIAN_POINT('Ctrl Pts',(0.231120659856154,0.0548222395137741,
-0.0418874595346435));
#84925=CARTESIAN_POINT('Ctrl Pts',(0.235703470079078,0.0293394869896825,
-0.0437732825007175));
#84926=CARTESIAN_POINT('Ctrl Pts',(0.236946521790301,0.0165336719173053,
-0.0446967234098427));
#84927=CARTESIAN_POINT('Ctrl Pts',(0.237212224835647,-0.000548839537223723,
-0.0458846925810193));
#84928=CARTESIAN_POINT('Ctrl Pts',(0.237164551851847,-0.00478749684408978,
-0.0461760565250585));
#84929=CARTESIAN_POINT('Ctrl Pts',(0.236928918585958,-0.0109768834788314,
-0.046596819997762));
#84930=CARTESIAN_POINT('Ctrl Pts',(0.236830362302173,-0.0129299774393764,
-0.0467289136837998));
#84931=CARTESIAN_POINT('Ctrl Pts',(0.236612945991118,-0.0163881962245446,
-0.0469616636857334));
#84932=CARTESIAN_POINT('Ctrl Pts',(0.236503850297288,-0.0178938022358611,
-0.0470626128115884));
#84933=CARTESIAN_POINT('Ctrl Pts',(0.236243868106829,-0.0210618483813991,
-0.0472742652514253));
#84934=CARTESIAN_POINT('Ctrl Pts',(0.23608979020853,-0.0227239492479335,
-0.0473848652555413));
#84935=CARTESIAN_POINT('Ctrl Pts',(0.235631922462022,-0.0271538172966524,
-0.0476785522005319));
#84936=CARTESIAN_POINT('Ctrl Pts',(0.235296915096025,-0.0299181459330282,
-0.0478606820781113));
#84937=CARTESIAN_POINT('Ctrl Pts',(0.233057158499585,-0.0460201208094515,
-0.0489161062639835));
#84938=CARTESIAN_POINT('Ctrl Pts',(0.230067346158123,-0.0591825102383886,
-0.049755013879734));
#84939=CARTESIAN_POINT('Ctrl Pts',(0.222861512307011,-0.0817917434546498,
-0.0512194598399837));
#84940=CARTESIAN_POINT('Ctrl Pts',(0.21911721236422,-0.0913497372539561,
-0.0518470789759478));
#84941=CARTESIAN_POINT('Ctrl Pts',(0.212726646050054,-0.10498791702506,
-0.0527912725392269));
#84942=CARTESIAN_POINT('Ctrl Pts',(0.210555217960102,-0.109277552227489,
-0.0530958286049878));
#84943=CARTESIAN_POINT('Ctrl Pts',(0.206765840337732,-0.116230602600322,
-0.0536068528397998));
#84944=CARTESIAN_POINT('Ctrl Pts',(0.205223021235037,-0.118933490270836,
-0.0538100018954434));
#84945=CARTESIAN_POINT('Ctrl Pts',(0.203031938095021,-0.122602456126231,
-0.0540931017233831));
#84946=CARTESIAN_POINT('Ctrl Pts',(0.20242901099198,-0.123595410554864,
-0.0541704725068926));
#84947=CARTESIAN_POINT('Ctrl Pts',(0.201811785312619,-0.124595281265935,
-0.0542491903685042));
#84948=CARTESIAN_POINT('Ctrl Pts',(0.201804740776483,-0.124606690851416,
-0.0542500887297526));
#84949=CARTESIAN_POINT('Ctrl Pts',(0.201790589978157,-0.124629605648643,
-0.0542518931965488));
#84950=CARTESIAN_POINT('Ctrl Pts',(0.201783483699253,-0.124641110850562,
-0.0542527993031468));
#84951=CARTESIAN_POINT('Ctrl Pts',(0.201769201986442,-0.12466422879518,
-0.0542546202047113));
#84952=CARTESIAN_POINT('Ctrl Pts',(0.201762026534311,-0.124675841525576,
-0.0542555350007778));
#84953=CARTESIAN_POINT('Ctrl Pts',(0.201747598688302,-0.124699187001194,
-0.054257374270399));
#84954=CARTESIAN_POINT('Ctrl Pts',(0.201740346273374,-0.124710919733412,
-0.0542582987452612));
#84955=CARTESIAN_POINT('Ctrl Pts',(0.201725756314585,-0.124734518313683,
-0.0542601584120372));
#84956=CARTESIAN_POINT('Ctrl Pts',(0.201718418747594,-0.124746384146427,
-0.0542610936053595));
#84957=CARTESIAN_POINT('Ctrl Pts',(0.201703649851505,-0.124770262727592,
-0.0542629758048169));
#84958=CARTESIAN_POINT('Ctrl Pts',(0.201696218495876,-0.124782275460077,
-0.0542639228126168));
#84959=CARTESIAN_POINT('Ctrl Pts',(0.201243071185299,-0.125514638557729,
-0.0543216649507409));
#84960=CARTESIAN_POINT('Ctrl Pts',(0.200793507002238,-0.12623258571485,
-0.0543786991883708));
#84961=CARTESIAN_POINT('Ctrl Pts',(0.199847898651101,-0.127724874967505,
-0.0544981783427748));
#84962=CARTESIAN_POINT('Ctrl Pts',(0.19935118134348,-0.128498765387827,
-0.0545606656932554));
#84963=CARTESIAN_POINT('Ctrl Pts',(0.198013518471803,-0.130556433814375,
-0.0547281802793283));
#84964=CARTESIAN_POINT('Ctrl Pts',(0.197164607935789,-0.131834945972515,
-0.054833698192417));
#84965=CARTESIAN_POINT('Ctrl Pts',(0.193008892955007,-0.137963794258743,
-0.0553461529099942));
#84966=CARTESIAN_POINT('Ctrl Pts',(0.189535438439584,-0.142698095821386,
-0.05576220297476));
#84967=CARTESIAN_POINT('Ctrl Pts',(0.177918393812321,-0.157358800030003,
-0.0571051638411923));
#84968=CARTESIAN_POINT('Ctrl Pts',(0.169143058456079,-0.166755416962442,
-0.0580489718136488));
#84969=CARTESIAN_POINT('Ctrl Pts',(0.151594553358339,-0.182728602446552,
-0.0597692792142245));
#84970=CARTESIAN_POINT('Ctrl Pts',(0.143042067791329,-0.189498474350884,
-0.0605477119705698));
#84971=CARTESIAN_POINT('Ctrl Pts',(0.130695912675107,-0.197957377281211,
-0.0615872527892901));
#84972=CARTESIAN_POINT('Ctrl Pts',(0.127279627262982,-0.200171038878033,
-0.0618668771674415));
#84973=CARTESIAN_POINT('Ctrl Pts',(0.122177258488858,-0.20329376025142,
-0.0622731376752819));
#84974=CARTESIAN_POINT('Ctrl Pts',(0.120534598112089,-0.204271991413951,
-0.0624022531823423));
#84975=CARTESIAN_POINT('Ctrl Pts',(0.117591734899885,-0.205976653643895,
-0.0626306639199171));
#84976=CARTESIAN_POINT('Ctrl Pts',(0.116296197972131,-0.206710891036716,
-0.0627302345586643));
#84977=CARTESIAN_POINT('Ctrl Pts',(0.113542477274176,-0.208237461003023,
-0.0629398516207759));
#84978=CARTESIAN_POINT('Ctrl Pts',(0.112082714370279,-0.209026791786239,
-0.0630497878355391));
#84979=CARTESIAN_POINT('Ctrl Pts',(0.108141162077503,-0.211104924661254,
-0.0633435605812183));
#84980=CARTESIAN_POINT('Ctrl Pts',(0.105644617103683,-0.212365289296648,
-0.0635264032803257));
#84981=CARTESIAN_POINT('Ctrl Pts',(0.0900633192796194,-0.219888614679257,
-0.0646489582964317));
#84982=CARTESIAN_POINT('Ctrl Pts',(0.0764485973721632,-0.22498465108704,
-0.06554716703907));
#84983=CARTESIAN_POINT('Ctrl Pts',(0.0506837805438242,-0.232017117908173,
-0.0671866412882708));
#84984=CARTESIAN_POINT('Ctrl Pts',(0.0386861121709244,-0.234316312254402,
-0.0679284520800586));
#84985=CARTESIAN_POINT('Ctrl Pts',(0.0228676245380731,-0.236099348823575,
-0.068933787660448));
#84986=CARTESIAN_POINT('Ctrl Pts',(0.0191603640519138,-0.236429076493693,
-0.0691713979761933));
#84987=CARTESIAN_POINT('Ctrl Pts',(0.0128708064886722,-0.236839583852149,
-0.0695801684717117));
#84988=CARTESIAN_POINT('Ctrl Pts',(0.0102920760984747,-0.236965647261717,
-0.0697493700725626));
#84989=CARTESIAN_POINT('Ctrl Pts',(0.00658976627498104,-0.237086094478279,
-0.0699952507444404));
#84990=CARTESIAN_POINT('Ctrl Pts',(0.00546738311595209,-0.23711463221513,
-0.070070180856495));
#84991=CARTESIAN_POINT('Ctrl Pts',(0.00351078517608979,-0.237150481635207,
-0.0702015475009433));
#84992=CARTESIAN_POINT('Ctrl Pts',(0.00267666438307106,-0.237161362786392,
-0.0702577877255202));
#84993=CARTESIAN_POINT('Ctrl Pts',(0.000882804323840761,-0.237175298701457,
-0.0703792716987969));
#84994=CARTESIAN_POINT('Ctrl Pts',(-7.68863340875269E-5,-0.237176929030061,
-0.0704445873827406));
#84995=CARTESIAN_POINT('Ctrl Pts',(-0.0027429472510075,-0.23716527728665,
-0.0706268865926895));
#84996=CARTESIAN_POINT('Ctrl Pts',(-0.0044491645413205,-0.237139404200317,
-0.0707445205617118));
#84997=CARTESIAN_POINT('Ctrl Pts',(-0.0161885180090893,-0.236834655441247,
-0.0715598674649074));
#84998=CARTESIAN_POINT('Ctrl Pts',(-0.0261944222053511,-0.235937554081915,
-0.0722845079809336));
#84999=CARTESIAN_POINT('Ctrl Pts',(-0.0383371644445804,-0.234066893115663,
-0.0731794300146716));
#85000=CARTESIAN_POINT('Ctrl Pts',(-0.0405571327612126,-0.233692463477712,
-0.0733437078865619));
#85001=CARTESIAN_POINT('Ctrl Pts',(-0.0523670548376334,-0.231527198235096,
-0.0742203929345932));
#85002=CARTESIAN_POINT('Ctrl Pts',(-0.0618455126808292,-0.229177450263697,
-0.0749331806921317));
#85003=CARTESIAN_POINT('Ctrl Pts',(-0.0806233994391151,-0.223272061809617,
-0.0763472186036685));
#85004=CARTESIAN_POINT('Ctrl Pts',(-0.0898987652493098,-0.219701628220547,
-0.0770466322226461));
#85005=CARTESIAN_POINT('Ctrl Pts',(-0.101257323179697,-0.214488986516255,
-0.0779027805130789));
#85006=CARTESIAN_POINT('Ctrl Pts',(-0.103573042032291,-0.213380403749465,
-0.0780773488717331));
#85007=CARTESIAN_POINT('Ctrl Pts',(-0.107299926305311,-0.211521295718243,
-0.0783584354956205));
#85008=CARTESIAN_POINT('Ctrl Pts',(-0.108722253252174,-0.210793748941424,
-0.078465743405674));
#85009=CARTESIAN_POINT('Ctrl Pts',(-0.111449490585185,-0.209363768099226,
-0.0786716095187473));
#85010=CARTESIAN_POINT('Ctrl Pts',(-0.112755377140241,-0.208663368710152,
-0.0787702335327048));
#85011=CARTESIAN_POINT('Ctrl Pts',(-0.115754579455062,-0.207018397876951,
-0.0789969047242206));
#85012=CARTESIAN_POINT('Ctrl Pts',(-0.117443063077325,-0.206065200924031,
-0.0791246369939908));
#85013=CARTESIAN_POINT('Ctrl Pts',(-0.122947178955313,-0.20286833966744,
-0.0795416118550793));
#85014=CARTESIAN_POINT('Ctrl Pts',(-0.126711846404028,-0.200538485245224,
-0.0798277403004468));
#85015=CARTESIAN_POINT('Ctrl Pts',(-0.145622837675745,-0.188089655647993,
-0.0812745292420112));
#85016=CARTESIAN_POINT('Ctrl Pts',(-0.159631916097633,-0.176355953255343,
-0.0823726212208167));
#85017=CARTESIAN_POINT('Ctrl Pts',(-0.177278096616715,-0.157733356860707,
-0.0839520793447804));
#85018=CARTESIAN_POINT('Ctrl Pts',(-0.182138231918799,-0.152095312609701,
-0.0844139482852281));
#85019=CARTESIAN_POINT('Ctrl Pts',(-0.189286628847751,-0.142967872773016,
-0.0851534698077213));
#85020=CARTESIAN_POINT('Ctrl Pts',(-0.191761668395135,-0.139630576981363,
-0.0854223063960954));
#85021=CARTESIAN_POINT('Ctrl Pts',(-0.194914621004483,-0.135137168462202,
-0.0857847843149075));
#85022=CARTESIAN_POINT('Ctrl Pts',(-0.19567236056301,-0.134037647268601,
-0.0858735208550365));
#85023=CARTESIAN_POINT('Ctrl Pts',(-0.196907283132061,-0.132212919195767,
-0.0860209554798516));
#85024=CARTESIAN_POINT('Ctrl Pts',(-0.197389856318338,-0.131491363752863,
-0.0860792994661674));
#85025=CARTESIAN_POINT('Ctrl Pts',(-0.198296430181172,-0.130119594743281,
-0.0861903331526911));
#85026=CARTESIAN_POINT('Ctrl Pts',(-0.198721217770172,-0.129469922076962,
-0.0862429651524551));
#85027=CARTESIAN_POINT('Ctrl Pts',(-0.199839652964633,-0.127740909111082,
-0.086383135483864));
#85028=CARTESIAN_POINT('Ctrl Pts',(-0.200527732722454,-0.126658023751571,
-0.0864710247082619));
#85029=CARTESIAN_POINT('Ctrl Pts',(-0.203002791940602,-0.122692103540876,
-0.0867931198186491));
#85030=CARTESIAN_POINT('Ctrl Pts',(-0.204736565585314,-0.119776548835057,
-0.0870303112116316));
#85031=CARTESIAN_POINT('Ctrl Pts',(-0.213696265236722,-0.103946498853728,
-0.0883163554729566));
#85032=CARTESIAN_POINT('Ctrl Pts',(-0.219763748477631,-0.0904147503945695,
-0.0894070699715227));
#85033=CARTESIAN_POINT('Ctrl Pts',(-0.228423049350878,-0.0649682780140882,
-0.0913620129888713));
#85034=CARTESIAN_POINT('Ctrl Pts',(-0.23143616194505,-0.0532479326507539,
-0.0922287017789436));
#85035=CARTESIAN_POINT('Ctrl Pts',(-0.234261466371192,-0.0372897763053309,
-0.0933548781232203));
#85036=CARTESIAN_POINT('Ctrl Pts',(-0.234874029562119,-0.0332137915015895,
-0.0936380657761215));
#85037=CARTESIAN_POINT('Ctrl Pts',(-0.235615636658183,-0.0272200597254118,
-0.0940482315604449));
#85038=CARTESIAN_POINT('Ctrl Pts',(-0.235828076924721,-0.0253136010403289,
-0.0941777761363258));
#85039=CARTESIAN_POINT('Ctrl Pts',(-0.236164071525444,-0.0219253723326297,
-0.0944064383914506));
#85040=CARTESIAN_POINT('Ctrl Pts',(-0.236296862671317,-0.0204446446661825,
-0.0945058385743478));
#85041=CARTESIAN_POINT('Ctrl Pts',(-0.236547571661388,-0.0173189593859044,
-0.0947145890644771));
#85042=CARTESIAN_POINT('Ctrl Pts',(-0.236662273466589,-0.0156738176972949,
-0.0948238343004504));
#85043=CARTESIAN_POINT('Ctrl Pts',(-0.236923075804442,-0.0112719521688186,
-0.095114553972766));
#85044=CARTESIAN_POINT('Ctrl Pts',(-0.237038225682992,-0.00851359785458927,
-0.0952950661872727));
#85045=CARTESIAN_POINT('Ctrl Pts',(-0.237406034895552,0.0066433410101141,
-0.096278896824417));
#85046=CARTESIAN_POINT('Ctrl Pts',(-0.236734189313708,0.0190457176630952,
-0.0970529493503612));
#85047=CARTESIAN_POINT('Ctrl Pts',(-0.232800798207848,0.0485518444689856,
-0.0988874096047161));
#85048=CARTESIAN_POINT('Ctrl Pts',(-0.228623424655103,0.0654574093770121,
-0.0999317714500581));
#85049=CARTESIAN_POINT('Ctrl Pts',(-0.221655485484241,0.0844332701974654,
-0.101238640282909));
#85050=CARTESIAN_POINT('Ctrl Pts',(-0.220623138636862,0.0870951221952471,
-0.101425287275785));
#85051=CARTESIAN_POINT('Ctrl Pts',(-0.219100372267507,0.0908205726181262,
-0.101692106218462));
#85052=CARTESIAN_POINT('Ctrl Pts',(-0.218649692287981,0.0919002799766883,
-0.101770106907023));
#85053=CARTESIAN_POINT('Ctrl Pts',(-0.217860194909153,0.0937530182021312,
-0.101905186248613));
#85054=CARTESIAN_POINT('Ctrl Pts',(-0.217525199342231,0.0945276709645965,
-0.101962039591995));
#85055=CARTESIAN_POINT('Ctrl Pts',(-0.216806517994463,0.0961655170133428,
-0.102083067720244));
#85056=CARTESIAN_POINT('Ctrl Pts',(-0.216421804597607,0.0970282192153031,
-0.102147299890636));
#85057=CARTESIAN_POINT('Ctrl Pts',(-0.215345578569769,0.0994033605387357,
-0.102325431172351));
#85058=CARTESIAN_POINT('Ctrl Pts',(-0.214643311330578,0.100910826018539,
-0.102439941787794));
#85059=CARTESIAN_POINT('Ctrl Pts',(-0.210622799138623,0.109309254525945,
-0.10308558382786));
#85060=CARTESIAN_POINT('Ctrl Pts',(-0.206988889152257,0.116043320881076,
-0.103632301245098));
#85061=CARTESIAN_POINT('Ctrl Pts',(-0.191690828878982,0.141380468971707,
-0.105774192769637));
#85062=CARTESIAN_POINT('Ctrl Pts',(-0.177788199330129,0.158510317670842,
-0.107395176475848));
#85063=CARTESIAN_POINT('Ctrl Pts',(-0.158770679954309,0.176238984353413,
-0.109200792951285));
#85064=CARTESIAN_POINT('Ctrl Pts',(-0.155744950341185,0.178918479550083,
-0.109478360597535));
#85065=CARTESIAN_POINT('Ctrl Pts',(-0.151196967155293,0.182743187188463,
-0.109881851380408));
#85066=CARTESIAN_POINT('Ctrl Pts',(-0.149727174977946,0.183949364715039,
-0.110010231779461));
#85067=CARTESIAN_POINT('Ctrl Pts',(-0.147086283895167,0.186063971681287,
-0.110237406491457));
#85068=CARTESIAN_POINT('Ctrl Pts',(-0.145920891178292,0.186979330827736,
-0.110336474111621));
#85069=CARTESIAN_POINT('Ctrl Pts',(-0.143438167322815,0.188892039134169,
-0.110545086270585));
#85070=CARTESIAN_POINT('Ctrl Pts',(-0.142118834418132,0.18988666996184,
-0.110654520695018));
#85071=CARTESIAN_POINT('Ctrl Pts',(-0.138547331954141,0.192521110336148,
-0.110947061476491));
#85072=CARTESIAN_POINT('Ctrl Pts',(-0.136276443313954,0.194135193035347,
-0.111129177257946));
#85073=CARTESIAN_POINT('Ctrl Pts',(-0.12244291154887,0.203605290862651,
-0.112216623359398));
#85074=CARTESIAN_POINT('Ctrl Pts',(-0.110232151627088,0.21046692268304,
-0.113083636319488));
#85075=CARTESIAN_POINT('Ctrl Pts',(-0.088131630129975,0.220431632362591,
-0.114572690029515));
#85076=CARTESIAN_POINT('Ctrl Pts',(-0.0785130769470917,0.224037876441566,
-0.11519760097848));
#85077=CARTESIAN_POINT('Ctrl Pts',(-0.061436611666013,0.22920510102654,
-0.116310526852575));
#85078=CARTESIAN_POINT('Ctrl Pts',(-0.0540812627729639,0.231051136994762,
-0.116791140588702));
#85079=CARTESIAN_POINT('Ctrl Pts',(-0.0450823060151138,0.232856449867392,
-0.117394376773371));
#85080=CARTESIAN_POINT('Ctrl Pts',(-0.0435104905522345,0.233155264635116,
-0.117500298996737));
#85081=CARTESIAN_POINT('Ctrl Pts',(-0.0419358257166351,0.233438144154857,
-0.117607078812657));
#85082=CARTESIAN_POINT('',(0.150502666328434,-0.183305559252938,-0.04));
#85083=CARTESIAN_POINT('Origin',(0.,0.,-0.04));
#85084=CARTESIAN_POINT('',(-0.237174908959558,-0.00020781006993565,-0.0759410108041934));
#85085=CARTESIAN_POINT('Ctrl Pts',(-0.237174908959558,-0.00020781006993565,
-0.0759410108041934));
#85086=CARTESIAN_POINT('Ctrl Pts',(-0.237158965686875,-0.0184039650893944,
-0.0747207381634765));
#85087=CARTESIAN_POINT('Ctrl Pts',(-0.235045118479419,-0.0365055894439177,
-0.073500465522759));
#85088=CARTESIAN_POINT('Ctrl Pts',(-0.230920381200416,-0.0541087624258259,
-0.0722801928820409));
#85089=CARTESIAN_POINT('Ctrl Pts',(-0.230276398834125,-0.0568570909190921,
-0.0720896755206831));
#85090=CARTESIAN_POINT('Ctrl Pts',(-0.229583492057616,-0.0595933149141058,
-0.0718991581593253));
#85091=CARTESIAN_POINT('Ctrl Pts',(-0.228842093394929,-0.0623159443130459,
-0.0717086407979675));
#85092=CARTESIAN_POINT('Ctrl Pts',(-0.225192493135875,-0.0757183274838922,
-0.0707708022957423));
#85093=CARTESIAN_POINT('Ctrl Pts',(-0.220347559650889,-0.0888495540733388,
-0.0698329637935173));
#85094=CARTESIAN_POINT('Ctrl Pts',(-0.214367883493431,-0.101480989113956,
-0.0688951252912922));
#85095=CARTESIAN_POINT('Ctrl Pts',(-0.208400359824408,-0.114086753304811,
-0.0679591927570915));
#85096=CARTESIAN_POINT('Ctrl Pts',(-0.201302959780381,-0.126193945435919,
-0.0670232602228907));
#85097=CARTESIAN_POINT('Ctrl Pts',(-0.193185046329708,-0.137591854771962,
-0.06608732768869));
#85098=CARTESIAN_POINT('Ctrl Pts',(-0.185067115835033,-0.148989788038536,
-0.0651513931894479));
#85099=CARTESIAN_POINT('Ctrl Pts',(-0.175929117518454,-0.159677709738982,
-0.0642154586902058));
#85100=CARTESIAN_POINT('Ctrl Pts',(-0.165924297051288,-0.169473031108303,
-0.0632795241909636));
#85101=CARTESIAN_POINT('Ctrl Pts',(-0.155920418675126,-0.179267430113833,
-0.0623436778227854));
#85102=CARTESIAN_POINT('Ctrl Pts',(-0.145050507587878,-0.188168815215712,
-0.0614078314546073));
#85103=CARTESIAN_POINT('Ctrl Pts',(-0.133503529137789,-0.196032620583299,
-0.060471985086429));
#85104=CARTESIAN_POINT('Ctrl Pts',(-0.121925774218444,-0.20391738556081,
-0.0595336443819963));
#85105=CARTESIAN_POINT('Ctrl Pts',(-0.109668087105897,-0.210758613379555,
-0.0585953036775631));
#85106=CARTESIAN_POINT('Ctrl Pts',(-0.0969465426444049,-0.216456343160224,
-0.0576569629731303));
#85107=CARTESIAN_POINT('Ctrl Pts',(-0.0888001065838006,-0.220104971790916,
-0.0570560821150817));
#85108=CARTESIAN_POINT('Ctrl Pts',(-0.0804639467507705,-0.223285648539055,
-0.0564552012570333));
#85109=CARTESIAN_POINT('Ctrl Pts',(-0.0719980238660825,-0.225982886928146,
-0.0558543203989847));
#85110=CARTESIAN_POINT('Ctrl Pts',(-0.0582706547715472,-0.230356419194777,
-0.0548800009499861));
#85111=CARTESIAN_POINT('Ctrl Pts',(-0.0441059425071512,-0.233486976078622,
-0.0539056815009878));
#85112=CARTESIAN_POINT('Ctrl Pts',(-0.0297453723807863,-0.235302344754421,
-0.0529313620519891));
#85113=CARTESIAN_POINT('Ctrl Pts',(-0.0154188776396131,-0.237113405844493,
-0.0519593545105423));
#85114=CARTESIAN_POINT('Ctrl Pts',(-0.000898203897908545,-0.237615317219415,
-0.0509873469690956));
#85115=CARTESIAN_POINT('Ctrl Pts',(0.0135648054651533,-0.236786774710271,
-0.0500153394276488));
#85116=CARTESIAN_POINT('Ctrl Pts',(0.02800928492293,-0.235959293723928,
-0.0490445772153881));
#85117=CARTESIAN_POINT('Ctrl Pts',(0.0423954714960833,-0.23380474552208,
-0.0480738150031273));
#85118=CARTESIAN_POINT('Ctrl Pts',(0.0564719007170983,-0.230353869197802,
-0.0471030527908667));
#85119=CARTESIAN_POINT('Ctrl Pts',(0.070536700396345,-0.226905843888489,
-0.0461330925944807));
#85120=CARTESIAN_POINT('Ctrl Pts',(0.0842914947997221,-0.222163793119845,
-0.0451631323980948));
#85121=CARTESIAN_POINT('Ctrl Pts',(0.0974964044458938,-0.216209231405883,
-0.0441931722017088));
#85122=CARTESIAN_POINT('Ctrl Pts',(0.110710507203386,-0.210250524192242,
-0.0432225367298155));
#85123=CARTESIAN_POINT('Ctrl Pts',(0.123373253112856,-0.20307794391354,
-0.0422519012579224));
#85124=CARTESIAN_POINT('Ctrl Pts',(0.13526628678023,-0.194820461670966,
-0.0412812657860291));
#85125=CARTESIAN_POINT('Ctrl Pts',(0.140499331718777,-0.191187093023135,
-0.0408541771906861));
#85126=CARTESIAN_POINT('Ctrl Pts',(0.145583704196375,-0.187344263367862,
-0.040427088595343));
#85127=CARTESIAN_POINT('Ctrl Pts',(0.150502666328434,-0.183305559252938,
-0.04));
#85128=CARTESIAN_POINT('Ctrl Pts',(-0.237174909590924,-0.000207088234899032,
-0.0759292533346744));
#85129=CARTESIAN_POINT('Ctrl Pts',(-0.237183607200531,0.00975414772469391,
-0.0765408113412823));
#85130=CARTESIAN_POINT('Ctrl Pts',(-0.236564747866873,0.0197057060827421,
-0.077155976177345));
#85131=CARTESIAN_POINT('Ctrl Pts',(-0.234739333942387,0.0342235074390107,
-0.0780837272251957));
#85132=CARTESIAN_POINT('Ctrl Pts',(-0.234019769798396,0.0388400093584547,
-0.0783832186704287));
#85133=CARTESIAN_POINT('Ctrl Pts',(-0.232806910733985,0.0453512298203194,
-0.0788136472548088));
#85134=CARTESIAN_POINT('Ctrl Pts',(-0.232425745196628,0.0472658898231393,
-0.0789412059275054));
#85135=CARTESIAN_POINT('Ctrl Pts',(-0.231713367225553,0.050627042651014,
-0.0791669932979334));
#85136=CARTESIAN_POINT('Ctrl Pts',(-0.23139213085097,0.0520755567847521,
-0.0792649100086293));
#85137=CARTESIAN_POINT('Ctrl Pts',(-0.23071500242883,0.0549988144949174,
-0.0794638062127938));
#85138=CARTESIAN_POINT('Ctrl Pts',(-0.230358509626961,0.056473345965148,
-0.0795648003562512));
#85139=CARTESIAN_POINT('Ctrl Pts',(-0.22958603411431,0.0595393928033083,
-0.0797762429485215));
#85140=CARTESIAN_POINT('Ctrl Pts',(-0.229167591361299,0.0611301987051148,
-0.0798867644607751));
#85141=CARTESIAN_POINT('Ctrl Pts',(-0.228027033146246,0.0652899164515071,
-0.080177964494201));
#85142=CARTESIAN_POINT('Ctrl Pts',(-0.22727806844499,0.0678511580749889,
-0.0803594829370441));
#85143=CARTESIAN_POINT('Ctrl Pts',(-0.223510081125561,0.0799734192171112,
-0.0812295129399832));
#85144=CARTESIAN_POINT('Ctrl Pts',(-0.219930375181725,0.0893481279248556,
-0.081935521199564));
#85145=CARTESIAN_POINT('Ctrl Pts',(-0.209494610383567,0.112215753794183,
-0.0837381847953898));
#85146=CARTESIAN_POINT('Ctrl Pts',(-0.201921125851801,0.125332348903381,
-0.0848487718477774));
#85147=CARTESIAN_POINT('Ctrl Pts',(-0.190029821487688,0.142019658077279,
-0.0863179540386775));
#85148=CARTESIAN_POINT('Ctrl Pts',(-0.186759756228465,0.146293262151402,
-0.08669947422341));
#85149=CARTESIAN_POINT('Ctrl Pts',(-0.18216687636809,0.151890323565048,
-0.0872027328516464));
#85150=CARTESIAN_POINT('Ctrl Pts',(-0.180969887668527,0.153314518254734,
-0.0873311131371838));
#85151=CARTESIAN_POINT('Ctrl Pts',(-0.179078607620505,0.15551177391918,
-0.0875294977947869));
#85152=CARTESIAN_POINT('Ctrl Pts',(-0.178395812982089,0.156294572983944,
-0.087600239082649));
#85153=CARTESIAN_POINT('Ctrl Pts',(-0.177146057088149,0.157708512009016,
-0.087728094087927));
#85154=CARTESIAN_POINT('Ctrl Pts',(-0.176580824444461,0.158341127997742,
-0.0877853242169888));
#85155=CARTESIAN_POINT('Ctrl Pts',(-0.175288096954773,0.159772434170472,
-0.0879148630181392));
#85156=CARTESIAN_POINT('Ctrl Pts',(-0.174558526178157,0.160569202230658,
-0.0879870193070934));
#85157=CARTESIAN_POINT('Ctrl Pts',(-0.172253464739296,0.163052292630772,
-0.0882121401610231));
#85158=CARTESIAN_POINT('Ctrl Pts',(-0.170658738016339,0.164720679762996,
-0.0883637636735546));
#85159=CARTESIAN_POINT('Ctrl Pts',(-0.161337112849328,0.174192145447494,
-0.0892285400570341));
#85160=CARTESIAN_POINT('Ctrl Pts',(-0.153099188227136,0.181475237755567,
-0.089909831712682));
#85161=CARTESIAN_POINT('Ctrl Pts',(-0.137081351256703,0.19376646526179,
-0.0911527640998902));
#85162=CARTESIAN_POINT('Ctrl Pts',(-0.129457388848606,0.198941001370079,
-0.0917148580242062));
#85163=CARTESIAN_POINT('Ctrl Pts',(-0.11244298369889,0.20909588064915,-0.0929427165481842));
#85164=CARTESIAN_POINT('Ctrl Pts',(-0.102980514660976,0.213914668181631,
-0.0936100598248527));
#85165=CARTESIAN_POINT('Ctrl Pts',(-0.0908108557209554,0.219117045955595,
-0.0944703612258928));
#85166=CARTESIAN_POINT('Ctrl Pts',(-0.0883767057591891,0.220110082306797,
-0.0946424899551439));
#85167=CARTESIAN_POINT('Ctrl Pts',(-0.0844129340528357,0.221650794365439,
-0.0949231338492768));
#85168=CARTESIAN_POINT('Ctrl Pts',(-0.0828932682452703,0.222223589966903,
-0.0950308107466323));
#85169=CARTESIAN_POINT('Ctrl Pts',(-0.0799597677835509,0.223295014301621,
-0.0952388816903031));
#85170=CARTESIAN_POINT('Ctrl Pts',(-0.0785468487422197,0.223795934395491,
-0.0953391942000627));
#85171=CARTESIAN_POINT('Ctrl Pts',(-0.0752836851071221,0.224918110707922,
-0.095571133716558));
#85172=CARTESIAN_POINT('Ctrl Pts',(-0.0734303522955524,0.225529981899466,
-0.0957030606453805));
#85173=CARTESIAN_POINT('Ctrl Pts',(-0.0673601683925233,0.227451278210229,
-0.0961359084387482));
#85174=CARTESIAN_POINT('Ctrl Pts',(-0.0631144862940898,0.22866576782424,
-0.0964398489030841));
#85175=CARTESIAN_POINT('Ctrl Pts',(-0.0532460002596512,0.231192907846172,
-0.0971494803606293));
#85176=CARTESIAN_POINT('Ctrl Pts',(-0.0476082272902688,0.232419130680886,
-0.09755724369748));
#85177=CARTESIAN_POINT('Ctrl Pts',(-0.0419357865133625,0.233438151197497,
-0.0979694843087454));
#85178=CARTESIAN_POINT('Origin',(3.51939854619125E-17,0.,-0.04));
#85179=CARTESIAN_POINT('',(-0.287858644329449,-0.0607539371959678,-0.04));
#85180=CARTESIAN_POINT('Origin',(0.,0.,-0.04));
#85181=CARTESIAN_POINT('Ctrl Pts',(-0.287858644329448,-0.0607539371959718,
-0.0400000000000039));
#85182=CARTESIAN_POINT('Ctrl Pts',(-0.286189983298407,-0.0661913078499225,
-0.0400000000000039));
#85183=CARTESIAN_POINT('Ctrl Pts',(-0.284353083067471,-0.0715709236410684,
-0.040000000000004));
#85184=CARTESIAN_POINT('Ctrl Pts',(-0.282345486243454,-0.076885442432171,
-0.0400000000000038));
#85185=CARTESIAN_POINT('Ctrl Pts',(-0.278227505697077,-0.0877865779257651,
-0.0400000000000036));
#85186=CARTESIAN_POINT('Ctrl Pts',(-0.27339181851782,-0.0984142681665029,
-0.0400000000000037));
#85187=CARTESIAN_POINT('Ctrl Pts',(-0.267892007126804,-0.108722285391854,
-0.0400000000000033));
#85188=CARTESIAN_POINT('Ctrl Pts',(-0.26474927804854,-0.114612542924374,
-0.040000000000003));
#85189=CARTESIAN_POINT('Ctrl Pts',(-0.261388562009413,-0.120399838370053,
-0.0400000000000031));
#85190=CARTESIAN_POINT('Ctrl Pts',(-0.25782193291234,-0.126069559657423,
-0.0400000000000028));
#85191=CARTESIAN_POINT('Ctrl Pts',(-0.252889452406428,-0.133910517873923,
-0.0400000000000024));
#85192=CARTESIAN_POINT('Ctrl Pts',(-0.247573067082612,-0.141511317453255,
-0.0400000000000019));
#85193=CARTESIAN_POINT('Ctrl Pts',(-0.241904248797415,-0.148843967831607,
-0.0400000000000018));
#85194=CARTESIAN_POINT('Ctrl Pts',(-0.236180254585571,-0.156247988601291,
-0.0400000000000017));
#85195=CARTESIAN_POINT('Ctrl Pts',(-0.230095622069276,-0.16338063206386,
-0.0400000000000015));
#85196=CARTESIAN_POINT('Ctrl Pts',(-0.223676361292404,-0.170215298935253,
-0.0400000000000015));
#85197=CARTESIAN_POINT('Ctrl Pts',(-0.219180917476327,-0.17500165393623,
-0.0400000000000015));
#85198=CARTESIAN_POINT('Ctrl Pts',(-0.214519683660013,-0.17964329080041,
-0.0400000000000022));
#85199=CARTESIAN_POINT('Ctrl Pts',(-0.209706358590513,-0.184124977275315,
-0.0400000000000017));
#85200=CARTESIAN_POINT('Ctrl Pts',(-0.205260944507215,-0.18826410186898,
-0.0400000000000013));
#85201=CARTESIAN_POINT('Ctrl Pts',(-0.200692159066689,-0.192260891598814,
-0.0400000000000011));
#85202=CARTESIAN_POINT('Ctrl Pts',(-0.196012274283808,-0.196105089280495,
-0.0400000000000009));
#85203=CARTESIAN_POINT('Ctrl Pts',(-0.183147436316345,-0.206672652924502,
-0.0400000000000005));
#85204=CARTESIAN_POINT('Ctrl Pts',(-0.169432018761062,-0.216101860642565,
-0.0400000000000016));
#85205=CARTESIAN_POINT('Ctrl Pts',(-0.155013008598473,-0.224234519276562,
-0.0400000000000007));
#85206=CARTESIAN_POINT('Ctrl Pts',(-0.145592444993356,-0.229547937262704,
-0.0400000000000001));
#85207=CARTESIAN_POINT('Ctrl Pts',(-0.13587108744713,-0.234307045047568,
-0.0400000000000003));
#85208=CARTESIAN_POINT('Ctrl Pts',(-0.125887328485882,-0.238455560328839,
-0.0400000000000003));
#85209=CARTESIAN_POINT('Ctrl Pts',(-0.120905607334647,-0.240525596915574,
-0.0400000000000003));
#85210=CARTESIAN_POINT('Ctrl Pts',(-0.11585960953477,-0.242442558405335,
-0.04));
#85211=CARTESIAN_POINT('Ctrl Pts',(-0.110772660029015,-0.244193536666844,
-0.04));
#85212=CARTESIAN_POINT('Ctrl Pts',(-0.100827431588364,-0.247616782520891,
-0.0399999999999998));
#85213=CARTESIAN_POINT('Ctrl Pts',(-0.0907100227550067,-0.250413295320921,
-0.0400000000000001));
#85214=CARTESIAN_POINT('Ctrl Pts',(-0.0804585625301252,-0.252538295668516,
-0.0400000000000002));
#85215=CARTESIAN_POINT('Ctrl Pts',(-0.0655592239457918,-0.255626743458011,
-0.0400000000000004));
#85216=CARTESIAN_POINT('Ctrl Pts',(-0.0503757632529026,-0.257298270450147,
-0.0400000000000008));
#85217=CARTESIAN_POINT('Ctrl Pts',(-0.035087887712621,-0.257593498543919,
-0.0400000000000002));
#85218=CARTESIAN_POINT('Ctrl Pts',(-0.0266776628482832,-0.257755910557829,
-0.0399999999999999));
#85219=CARTESIAN_POINT('Ctrl Pts',(-0.0182246094922889,-0.257499357140891,
-0.0400000000000009));
#85220=CARTESIAN_POINT('Ctrl Pts',(-0.00982040497162541,-0.256833045226985,
-0.0400000000000007));
#85221=CARTESIAN_POINT('Ctrl Pts',(0.00491692967266122,-0.255664622727442,
-0.0400000000000002));
#85222=CARTESIAN_POINT('Ctrl Pts',(0.0195312833862859,-0.253242426124699,
-0.0400000000000002));
#85223=CARTESIAN_POINT('Ctrl Pts',(0.0338566095938309,-0.249610755855218,
-0.0400000000000004));
#85224=CARTESIAN_POINT('Ctrl Pts',(0.0444101672705453,-0.246935281587024,
-0.0400000000000006));
#85225=CARTESIAN_POINT('Ctrl Pts',(0.0548058406093567,-0.24360288402174,
-0.04));
#85226=CARTESIAN_POINT('Ctrl Pts',(0.0649723996581922,-0.23961836524148,
-0.04));
#85227=CARTESIAN_POINT('Ctrl Pts',(0.0711875157987854,-0.237182511884928,
-0.04));
#85228=CARTESIAN_POINT('Ctrl Pts',(0.0773193102033957,-0.234500720362044,
-0.0400000000000002));
#85229=CARTESIAN_POINT('Ctrl Pts',(0.0833170489198445,-0.231590456312328,
-0.0400000000000002));
#85230=CARTESIAN_POINT('Ctrl Pts',(0.0966561951856547,-0.225117943976167,
-0.0400000000000002));
#85231=CARTESIAN_POINT('Ctrl Pts',(0.109365981463997,-0.217507780687347,
-0.0399999999999999));
#85232=CARTESIAN_POINT('Ctrl Pts',(0.121261887594827,-0.208786977554813,
-0.0400000000000002));
#85233=CARTESIAN_POINT('Ctrl Pts',(0.130897115114624,-0.201723461634865,
-0.0400000000000004));
#85234=CARTESIAN_POINT('Ctrl Pts',(0.139998199893573,-0.193930449475644,
-0.0400000000000004));
#85235=CARTESIAN_POINT('Ctrl Pts',(0.148446367846058,-0.18540786851733,
-0.0400000000000005));
#85236=CARTESIAN_POINT('Ctrl Pts',(0.149136190345306,-0.184711969935559,
-0.0400000000000004));
#85237=CARTESIAN_POINT('Ctrl Pts',(0.149821647047686,-0.184011201202051,
-0.0400000000000001));
#85238=CARTESIAN_POINT('Ctrl Pts',(0.150502666328434,-0.183305559252938,
-0.04));
#85239=CARTESIAN_POINT('',(0.222488700208077,0.082706301833401,-0.0398895408386927));
#85240=CARTESIAN_POINT('Ctrl Pts',(0.223369910286723,0.0797362138773923,
-0.0399999999999998));
#85241=CARTESIAN_POINT('Ctrl Pts',(0.223023510600583,0.0807066044070377,
-0.0399631802795641));
#85242=CARTESIAN_POINT('Ctrl Pts',(0.222670787293575,0.0816747375972639,
-0.0399263605591283));
#85243=CARTESIAN_POINT('Ctrl Pts',(0.222311770321392,0.0826405312275324,
-0.0398895408386926));
#85244=CARTESIAN_POINT('Ctrl Pts',(0.222665717629832,0.0827839932162159,
-0.0400000000000001));
#85245=CARTESIAN_POINT('Ctrl Pts',(0.221253480978161,0.0887066597966071,
-0.0399999999999969));
#85246=CARTESIAN_POINT('Ctrl Pts',(0.219601459374371,0.0945593417108579,
-0.0399999999999963));
#85247=CARTESIAN_POINT('Ctrl Pts',(0.217708690025739,0.100327411027147,
-0.0399999999999962));
#85248=CARTESIAN_POINT('Ctrl Pts',(0.213879851975831,0.1119955011136,-0.0399999999999962));
#85249=CARTESIAN_POINT('Ctrl Pts',(0.209067649811371,0.123317664354657,
-0.0399999999999959));
#85250=CARTESIAN_POINT('Ctrl Pts',(0.203378325968185,0.134233488491038,
-0.0399999999999964));
#85251=CARTESIAN_POINT('Ctrl Pts',(0.199898449286141,0.140910155688135,
-0.0399999999999962));
#85252=CARTESIAN_POINT('Ctrl Pts',(0.196088082415695,0.147435983260384,
-0.0399999999999961));
#85253=CARTESIAN_POINT('Ctrl Pts',(0.191987668267784,0.153768999827833,
-0.0399999999999963));
#85254=CARTESIAN_POINT('Ctrl Pts',(0.185593130911648,0.163645248800932,
-0.0399999999999965));
#85255=CARTESIAN_POINT('Ctrl Pts',(0.178486227796011,0.173069463514982,
-0.0399999999999978));
#85256=CARTESIAN_POINT('Ctrl Pts',(0.170751201853388,0.181989599778708,
-0.0399999999999976));
#85257=CARTESIAN_POINT('Ctrl Pts',(0.16732716542848,0.18593824477469,-0.0399999999999976));
#85258=CARTESIAN_POINT('Ctrl Pts',(0.163779810148522,0.189788049195326,
-0.0399999999999972));
#85259=CARTESIAN_POINT('Ctrl Pts',(0.16011541559148,0.193534072345585,-0.0399999999999973));
#85260=CARTESIAN_POINT('Ctrl Pts',(0.156842239619411,0.196880162068013,
-0.0399999999999974));
#85261=CARTESIAN_POINT('Ctrl Pts',(0.153481935750538,0.200136982106501,
-0.0399999999999977));
#85262=CARTESIAN_POINT('Ctrl Pts',(0.150041516968305,0.203300204333427,
-0.0399999999999972));
#85263=CARTESIAN_POINT('Ctrl Pts',(0.1381660476245,0.214218860160297,-0.0399999999999957));
#85264=CARTESIAN_POINT('Ctrl Pts',(0.125334099709751,0.224030039279681,
-0.0399999999999991));
#85265=CARTESIAN_POINT('Ctrl Pts',(0.111739635875884,0.232604600158049,
-0.0399999999999995));
#85266=CARTESIAN_POINT('Ctrl Pts',(0.102821755693203,0.238229456530972,
-0.0399999999999998));
#85267=CARTESIAN_POINT('Ctrl Pts',(0.0935746853790765,0.243321776325075,
-0.0399999999999999));
#85268=CARTESIAN_POINT('Ctrl Pts',(0.0840435370389822,0.247837152868998,
-0.0399999999999999));
#85269=CARTESIAN_POINT('Ctrl Pts',(0.0785373322670779,0.250445714501441,
-0.0399999999999998));
#85270=CARTESIAN_POINT('Ctrl Pts',(0.0729353892307488,0.252861193764587,
-0.0400000000000001));
#85271=CARTESIAN_POINT('Ctrl Pts',(0.0672734922871532,0.255064885842267,
-0.0400000000000003));
#85272=CARTESIAN_POINT('Ctrl Pts',(0.0576677102794855,0.258803594957093,
-0.0400000000000006));
#85273=CARTESIAN_POINT('Ctrl Pts',(0.0478720024143959,0.261941980498935,
-0.0400000000000014));
#85274=CARTESIAN_POINT('Ctrl Pts',(0.0379326081771775,0.264446101529577,
-0.0400000000000018));
#85275=CARTESIAN_POINT('Ctrl Pts',(0.0266860283143166,0.267279553597704,
-0.0400000000000022));
#85276=CARTESIAN_POINT('Ctrl Pts',(0.015255426554341,0.269301474714493,
-0.0400000000000019));
#85277=CARTESIAN_POINT('Ctrl Pts',(0.00371085635712924,0.270547759765321,
-0.0400000000000023));
#85278=CARTESIAN_POINT('Ctrl Pts',(-0.00338729350177195,0.271314034984457,
-0.040000000000003));
#85279=CARTESIAN_POINT('Ctrl Pts',(-0.0105286670358888,0.271786812582468,
-0.0400000000000027));
#85280=CARTESIAN_POINT('Ctrl Pts',(-0.0176977769208803,0.271971820819257,
-0.0400000000000024));
#85281=CARTESIAN_POINT('Ctrl Pts',(-0.0232469593148744,0.272115024713018,
-0.0400000000000023));
#85282=CARTESIAN_POINT('Ctrl Pts',(-0.0288098460156715,0.272085302073594,
-0.040000000000003));
#85283=CARTESIAN_POINT('Ctrl Pts',(-0.0343596925541648,0.271886941169997,
-0.0400000000000031));
#85284=CARTESIAN_POINT('Ctrl Pts',(-0.0515871477842762,0.271271202777516,
-0.0400000000000034));
#85285=CARTESIAN_POINT('Ctrl Pts',(-0.0687382048994064,0.269036890911878,
-0.0400000000000034));
#85286=CARTESIAN_POINT('Ctrl Pts',(-0.0855957885720179,0.265293203132554,
-0.0400000000000028));
#85287=CARTESIAN_POINT('Ctrl Pts',(-0.094137880371246,0.263396197885558,
-0.0400000000000026));
#85288=CARTESIAN_POINT('Ctrl Pts',(-0.102604921020482,0.261110692191661,
-0.0400000000000023));
#85289=CARTESIAN_POINT('Ctrl Pts',(-0.110969298043269,0.258445247385233,
-0.0400000000000021));
#85290=CARTESIAN_POINT('Ctrl Pts',(-0.116744071982683,0.25660502172788,
-0.040000000000002));
#85291=CARTESIAN_POINT('Ctrl Pts',(-0.12247203470197,0.254582775191448,
-0.0400000000000022));
#85292=CARTESIAN_POINT('Ctrl Pts',(-0.128136696559136,0.252383171185569,
-0.0400000000000022));
#85293=CARTESIAN_POINT('Ctrl Pts',(-0.133443994806023,0.250322332466753,
-0.0400000000000022));
#85294=CARTESIAN_POINT('Ctrl Pts',(-0.138687644571475,0.248108961431596,
-0.0400000000000018));
#85295=CARTESIAN_POINT('Ctrl Pts',(-0.143855255028261,0.245748938027449,
-0.0400000000000017));
#85296=CARTESIAN_POINT('Ctrl Pts',(-0.159697617720826,0.238513805456196,
-0.0400000000000015));
#85297=CARTESIAN_POINT('Ctrl Pts',(-0.174844413355584,0.229896763780577,
-0.0400000000000008));
#85298=CARTESIAN_POINT('Ctrl Pts',(-0.189088023629515,0.219973317830906,
-0.0400000000000005));
#85299=CARTESIAN_POINT('Ctrl Pts',(-0.200581329367837,0.211965994119865,
-0.0400000000000002));
#85300=CARTESIAN_POINT('Ctrl Pts',(-0.211487041503738,0.203107005513314,
-0.0399999999999997));
#85301=CARTESIAN_POINT('Ctrl Pts',(-0.221686865784456,0.19341296114445,
-0.0399999999999998));
#85302=CARTESIAN_POINT('Ctrl Pts',(-0.103724760116696,0.212823727783082,
-1.59396608746666));
#85303=CARTESIAN_POINT('Ctrl Pts',(-0.174393327975359,0.178381702331853,
-1.58868131400033));
#85304=CARTESIAN_POINT('Ctrl Pts',(-0.277518531248041,0.0341781548206397,
-1.57811176706767));
#85305=CARTESIAN_POINT('Ctrl Pts',(-0.179349083795972,-0.214866166073336,
-1.56225744666869));
#85306=CARTESIAN_POINT('Ctrl Pts',(0.0827902547662305,-0.2670809958049,
-1.5464031262697));
#85307=CARTESIAN_POINT('Ctrl Pts',(0.269226441972677,-0.0758032933439426,
-1.53054880587072));
#85308=CARTESIAN_POINT('Ctrl Pts',(0.209939552040885,0.184851367163293,
-1.51469448547173));
#85309=CARTESIAN_POINT('Ctrl Pts',(-0.041041429718235,0.276658199552224,
-1.49884016507275));
#85310=CARTESIAN_POINT('Ctrl Pts',(-0.254537004881614,0.115941550403291,
-1.48298584467376));
#85311=CARTESIAN_POINT('Ctrl Pts',(-0.235665945800168,-0.150646965377197,
-1.46713152427478));
#85312=CARTESIAN_POINT('Ctrl Pts',(-0.00164253664402765,-0.279691657770853,
-1.45127720387579));
#85313=CARTESIAN_POINT('Ctrl Pts',(0.233877927031332,-0.15340291974329,
-1.43542288347681));
#85314=CARTESIAN_POINT('Ctrl Pts',(0.255884407477275,0.112936223822634,
-1.41956856307782));
#85315=CARTESIAN_POINT('Ctrl Pts',(0.0442844522027617,0.276170107760178,
-1.40371424267884));
#85316=CARTESIAN_POINT('Ctrl Pts',(-0.207743962043941,0.187279687461201,
-1.38785992227985));
#85317=CARTESIAN_POINT('Ctrl Pts',(-0.270115887608575,-0.0725853701266998,
-1.37200560188087));
#85318=CARTESIAN_POINT('Ctrl Pts',(-0.0858895457739192,-0.266184456976842,
-1.35615128148188));
#85319=CARTESIAN_POINT('Ctrl Pts',(0.176748293013421,-0.216774652656855,
-1.3402969610829));
#85320=CARTESIAN_POINT('Ctrl Pts',(0.278026506306114,0.030536329962957,
-1.32444264068391));
#85321=CARTESIAN_POINT('Ctrl Pts',(0.125484657012978,0.249969598727324,
-1.30858832028493));
#85322=CARTESIAN_POINT('Ctrl Pts',(-0.141616484291169,0.241196963701767,
-1.29273399988594));
#85323=CARTESIAN_POINT('Ctrl Pts',(-0.279431025008706,0.0122272374408218,
-1.27687967948696));
#85324=CARTESIAN_POINT('Ctrl Pts',(-0.162143281191983,-0.227905152839578,
-1.26102535908797));
#85325=CARTESIAN_POINT('Ctrl Pts',(0.103170691412443,-0.259975020756189,
-1.24517103868899));
#85326=CARTESIAN_POINT('Ctrl Pts',(0.274296559039192,-0.0547046662863507,
-1.22931671829));
#85327=CARTESIAN_POINT('Ctrl Pts',(0.195007576056607,0.200507476197715,
-1.21346239789102));
#85328=CARTESIAN_POINT('Ctrl Pts',(-0.0623105921992744,0.272669383914658,
-1.19760807749203));
#85329=CARTESIAN_POINT('Ctrl Pts',(-0.262743257945448,0.0959019457480826,
-1.18175375709305));
#85330=CARTESIAN_POINT('Ctrl Pts',(-0.22330848294228,-0.168417707595505,
-1.16589943669406));
#85331=CARTESIAN_POINT('Ctrl Pts',(0.0199923577595259,-0.278982989499441,
-1.15004511629507));
#85332=CARTESIAN_POINT('Ctrl Pts',(0.245041481085025,-0.134855016003514,
-1.13419079589609));
#85333=CARTESIAN_POINT('Ctrl Pts',(0.246383730268811,0.13238678276863,-1.1183364754971));
#85334=CARTESIAN_POINT('Ctrl Pts',(0.0227937194468614,0.278768092056046,
-1.10248215509812));
#85335=CARTESIAN_POINT('Ctrl Pts',(-0.22160546909146,0.170652333305773,
-1.08662783469914));
#85336=CARTESIAN_POINT('Ctrl Pts',(-0.263693332369467,-0.0932578643215929,
-1.07077351430015));
#85337=CARTESIAN_POINT('Ctrl Pts',(-0.0650463990182539,-0.272029720378002,
-1.05491919390117));
#85338=CARTESIAN_POINT('Ctrl Pts',(0.192983649933591,-0.202456201812523,
-1.03906487350218));
#85339=CARTESIAN_POINT('Ctrl Pts',(0.274832225875905,0.051946611190235,
-1.0232105531032));
#85340=CARTESIAN_POINT('Ctrl Pts',(0.10577692264544,0.25892555963007,-1.00735623270421));
#85341=CARTESIAN_POINT('Ctrl Pts',(-0.159845805071481,0.22952237667625,
-0.99150191230523));
#85342=CARTESIAN_POINT('Ctrl Pts',(-0.279539748657917,-0.00941975128844859,
-0.975647591906243));
#85343=CARTESIAN_POINT('Ctrl Pts',(-0.144032152112957,-0.239762261316874,
-0.959793271507259));
#85344=CARTESIAN_POINT('Ctrl Pts',(0.122967395841924,-0.251217480191813,
-0.943938951108274));
#85345=CARTESIAN_POINT('Ctrl Pts',(0.27770573960144,-0.0333275409606875,
-0.928084630709289));
#85346=CARTESIAN_POINT('Ctrl Pts',(0.178916873760631,0.214988267302641,
-0.912230310310303));
#85347=CARTESIAN_POINT('Ctrl Pts',(-0.0832114168254042,0.2670338235205,
-0.896375989911319));
#85348=CARTESIAN_POINT('Ctrl Pts',(-0.269373116497936,0.0752949327794278,
-0.880521669512333));
#85349=CARTESIAN_POINT('Ctrl Pts',(-0.209614747449241,-0.185183315786979,
-0.864667349113349));
#85350=CARTESIAN_POINT('Ctrl Pts',(0.0415082008413281,-0.276601287157137,
-0.848813028714363));
#85351=CARTESIAN_POINT('Ctrl Pts',(0.254736871721806,-0.115500341901908,
-0.832958708315379));
#85352=CARTESIAN_POINT('Ctrl Pts',(0.235407409800871,0.151044874805183,
-0.817104387916392));
#85353=CARTESIAN_POINT('Ctrl Pts',(0.00116635184411073,0.279695982126031,
-0.80125006751741));
#85354=CARTESIAN_POINT('Ctrl Pts',(-0.234139509198369,0.153002918359146,
-0.785395747118422));
#85355=CARTESIAN_POINT('Ctrl Pts',(-0.25569128467731,-0.113371820723387,
-0.769541426719439));
#85356=CARTESIAN_POINT('Ctrl Pts',(-0.0438136106375017,-0.276245489224665,
-0.753687106320452));
#85357=CARTESIAN_POINT('Ctrl Pts',(0.208063029442341,-0.186925061383818,
-0.737832785921468));
#85358=CARTESIAN_POINT('Ctrl Pts',(0.269991707513143,0.0730457436693384,
-0.721978465522483));
#85359=CARTESIAN_POINT('Ctrl Pts',(0.0854355836519637,0.266330553711205,
-0.706124145123497));
#85360=CARTESIAN_POINT('Ctrl Pts',(-0.177117650225534,0.216472956215444,
-0.690269824724514));
#85361=CARTESIAN_POINT('Ctrl Pts',(-0.277974032978924,-0.0310103173718541,
-0.674415504325526));
#85362=CARTESIAN_POINT('Ctrl Pts',(-0.125058271794479,-0.250183195778305,
-0.658561183926543));
#85363=CARTESIAN_POINT('Ctrl Pts',(0.142027526822356,-0.240955150222586,
-0.642706863527556));
#85364=CARTESIAN_POINT('Ctrl Pts',(0.279451466043086,-0.0117507838229697,
-0.626852543128573));
#85365=CARTESIAN_POINT('Ctrl Pts',(0.161754461395924,0.22818128103017,-0.610998222729586));
#85366=CARTESIAN_POINT('Ctrl Pts',(-0.103613805994735,0.259798733640734,
-0.595143902330603));
#85367=CARTESIAN_POINT('Ctrl Pts',(-0.274389433177387,0.0542369039931965,
-0.579289581931617));
#85368=CARTESIAN_POINT('Ctrl Pts',(-0.194665422011536,-0.200839678019582,
-0.563435261532631));
#85369=CARTESIAN_POINT('Ctrl Pts',(0.0627754102712604,-0.272562746279138,
-0.547580941133648));
#85370=CARTESIAN_POINT('Ctrl Pts',(0.262906391415409,-0.0954538220697194,
-0.531726620734661));
#85371=CARTESIAN_POINT('Ctrl Pts',(0.223021001639017,0.168798209768152,
-0.515872300335677));
#85372=CARTESIAN_POINT('Ctrl Pts',(-0.0204680021875169,0.278948496465033,
-0.500017979936691));
#85373=CARTESIAN_POINT('Ctrl Pts',(-0.245271056334415,0.134437017682742,
-0.484163659537707));
#85374=CARTESIAN_POINT('Ctrl Pts',(-0.246157649098411,-0.132806681217667,
-0.468309339138721));
#85375=CARTESIAN_POINT('Ctrl Pts',(-0.0223183792644695,-0.278806550749913,
-0.452455018739736));
#85376=CARTESIAN_POINT('Ctrl Pts',(0.221896113850858,-0.1702742419819,-0.436600698340751));
#85377=CARTESIAN_POINT('Ctrl Pts',(0.263533941788505,0.0937073329898119,
-0.420746377941766));
#85378=CARTESIAN_POINT('Ctrl Pts',(0.0645824867269263,0.272140230804651,
-0.404892057542781));
#85379=CARTESIAN_POINT('Ctrl Pts',(-0.193328563134106,0.202126865260915,
-0.389037737143796));
#85380=CARTESIAN_POINT('Ctrl Pts',(-0.274743255159592,-0.0524151320788667,
-0.373183416744811));
#85381=CARTESIAN_POINT('Ctrl Pts',(-0.105335295510445,-0.259105535627046,
-0.357329096345826));
#85382=CARTESIAN_POINT('Ctrl Pts',(0.160236917697637,-0.229249501915933,
-0.341474775946841));
#85383=CARTESIAN_POINT('Ctrl Pts',(0.279523275373005,0.00989636086202485,
-0.325620455547856));
#85384=CARTESIAN_POINT('Ctrl Pts',(0.143623153177434,0.240007490565944,
-0.30976613514887));
#85385=CARTESIAN_POINT('Ctrl Pts',(-0.123395571661222,0.251007454096603,
-0.293911814749885));
#85386=CARTESIAN_POINT('Ctrl Pts',(-0.277762118238676,0.032853993377835,
-0.2780574943509));
#85387=CARTESIAN_POINT('Ctrl Pts',(-0.178550133277567,-0.215293006392593,
-0.262203173951915));
#85388=CARTESIAN_POINT('Ctrl Pts',(0.0836667492467019,-0.266891570065015,
-0.24634885355293));
#85389=CARTESIAN_POINT('Ctrl Pts',(0.269500811469429,-0.074835511252918,
-0.230494533153945));
#85390=CARTESIAN_POINT('Ctrl Pts',(0.209299260770646,0.185540400134779,
-0.21464021275496));
#85391=CARTESIAN_POINT('Ctrl Pts',(-0.0419808241655782,0.276530198966801,
-0.198785892355975));
#85392=CARTESIAN_POINT('Ctrl Pts',(-0.254931386165377,0.11506567559891,
-0.18293157195699));
#85393=CARTESIAN_POINT('Ctrl Pts',(-0.235153442315408,-0.151445715536821,
-0.167077251558005));
#85394=CARTESIAN_POINT('Ctrl Pts',(-0.000681989459094153,-0.279698167413373,
-0.151222931159019));
#85395=CARTESIAN_POINT('Ctrl Pts',(0.234385766356705,-0.152602329150558,
-0.135368610760035));
#85396=CARTESIAN_POINT('Ctrl Pts',(0.255524894043667,0.113805412776539,
-0.119514290361049));
#85397=CARTESIAN_POINT('Ctrl Pts',(0.0432903726894156,0.276324012658087,
-0.103659969962065));
#85398=CARTESIAN_POINT('Ctrl Pts',(-0.208281425456119,0.186561872885006,
-0.0878056495630792));
#85399=CARTESIAN_POINT('Ctrl Pts',(-0.270060833707632,-0.0734895181549532,
-0.0719513291640941));
#85400=CARTESIAN_POINT('Ctrl Pts',(-0.0845542121726118,-0.266546212100623,
-0.0560944337615691));
#85401=CARTESIAN_POINT('Ctrl Pts',(0.0895616202659112,-0.232850436616742,
-0.0455223118253725));
#85402=CARTESIAN_POINT('Ctrl Pts',(0.150324724191651,-0.182907739666978,
-0.0402349633555041));
#85403=CARTESIAN_POINT('Ctrl Pts',(-0.112169338338267,0.230150416363986,
-1.58283766981155));
#85404=CARTESIAN_POINT('Ctrl Pts',(-0.188591269698735,0.192904350896613,
-1.57755289634522));
#85405=CARTESIAN_POINT('Ctrl Pts',(-0.300112239273236,0.0369607122498147,
-1.56698334941257));
#85406=CARTESIAN_POINT('Ctrl Pts',(-0.193950490108011,-0.232359136358677,
-1.55112902901358));
#85407=CARTESIAN_POINT('Ctrl Pts',(0.0895304851757355,-0.288824949302914,
-1.5352747086146));
#85408=CARTESIAN_POINT('Ctrl Pts',(0.291145063389551,-0.0819746919509459,
-1.51942038821561));
#85409=CARTESIAN_POINT('Ctrl Pts',(0.227031430267615,0.199900732692013,
-1.50356606781663));
#85410=CARTESIAN_POINT('Ctrl Pts',(-0.0443827492179445,0.299181865108354,
-1.48771174741764));
#85411=CARTESIAN_POINT('Ctrl Pts',(-0.275259710295338,0.125380738215436,
-1.47185742701866));
#85412=CARTESIAN_POINT('Ctrl Pts',(-0.254852295435795,-0.162911636623858,
-1.45600310661967));
#85413=CARTESIAN_POINT('Ctrl Pts',(-0.00177626102340334,-0.302462287264814,
-1.44014878622069));
#85414=CARTESIAN_POINT('Ctrl Pts',(0.252918708103212,-0.165891962414805,
-1.4242944658217));
#85415=CARTESIAN_POINT('Ctrl Pts',(0.276716809424425,0.122130737987296,
-1.40844014542272));
#85416=CARTESIAN_POINT('Ctrl Pts',(0.0478897969652389,0.298654036137713,
-1.39258582502373));
#85417=CARTESIAN_POINT('Ctrl Pts',(-0.224657089975649,0.202526750633954,
-1.37673150462475));
#85418=CARTESIAN_POINT('Ctrl Pts',(-0.292106921757353,-0.078494786885889,
-1.36087718422576));
#85419=CARTESIAN_POINT('Ctrl Pts',(-0.0928820997879023,-0.28785542026255,
-1.34502286382677));
#85420=CARTESIAN_POINT('Ctrl Pts',(0.191137960284783,-0.234422999192009,
-1.32916854342779));
#85421=CARTESIAN_POINT('Ctrl Pts',(0.30066157027282,0.0330223942997807,
-1.3133142230288));
#85422=CARTESIAN_POINT('Ctrl Pts',(0.135700780921689,0.270320456392293,
-1.29745990262982));
#85423=CARTESIAN_POINT('Ctrl Pts',(-0.153145953992668,0.260833611928227,
-1.28160558223083));
#85424=CARTESIAN_POINT('Ctrl Pts',(-0.30218043552135,0.0132226975690194,
-1.26575126183185));
#85425=CARTESIAN_POINT('Ctrl Pts',(-0.175343905802614,-0.246459670469582,
-1.24989694143286));
#85426=CARTESIAN_POINT('Ctrl Pts',(0.111570161055234,-0.281140453155943,
-1.23404262103388));
#85427=CARTESIAN_POINT('Ctrl Pts',(0.296627955574683,-0.059158355386433,
-1.21818830063489));
#85428=CARTESIAN_POINT('Ctrl Pts',(0.21088379238101,0.216831457712414,-1.20233398023591));
#85429=CARTESIAN_POINT('Ctrl Pts',(-0.0673835050627706,0.294868306703247,
-1.18647965983692));
#85430=CARTESIAN_POINT('Ctrl Pts',(-0.284134061755598,0.10370964259462,
-1.17062533943794));
#85431=CARTESIAN_POINT('Ctrl Pts',(-0.241488770364737,-0.182129154159352,
-1.15477101903895));
#85432=CARTESIAN_POINT('Ctrl Pts',(0.0216200021979781,-0.301695923948899,
-1.13891669863997));
#85433=CARTESIAN_POINT('Ctrl Pts',(0.264991124277493,-0.145834012049705,
-1.12306237824098));
#85434=CARTESIAN_POINT('Ctrl Pts',(0.266442650438278,0.143164831725639,
-1.107208057842));
#85435=CARTESIAN_POINT('Ctrl Pts',(0.0246494320714388,0.301463530988827,
-1.09135373744301));
#85436=CARTESIAN_POINT('Ctrl Pts',(-0.23964710848369,0.18454570819209,-1.07549941704403));
#85437=CARTESIAN_POINT('Ctrl Pts',(-0.285161484903114,-0.100850297691931,
-1.05964509664504));
#85438=CARTESIAN_POINT('Ctrl Pts',(-0.0703420430276832,-0.294176566027392,
-1.04379077624606));
#85439=CARTESIAN_POINT('Ctrl Pts',(0.208695091690748,-0.218938835570607,
-1.02793645584707));
#85440=CARTESIAN_POINT('Ctrl Pts',(0.297207232832846,0.0561757578380344,
-1.01208213544809));
#85441=CARTESIAN_POINT('Ctrl Pts',(0.1143885742541,0.280005551903859,-0.996227815049101));
#85442=CARTESIAN_POINT('Ctrl Pts',(-0.172859384498394,0.248208557885668,
-0.980373494650116));
#85443=CARTESIAN_POINT('Ctrl Pts',(-0.302298010724994,-0.0101866446174213,
-0.964519174251132));
#85444=CARTESIAN_POINT('Ctrl Pts',(-0.155758289378265,-0.259282105643277,
-0.948664853852145));
#85445=CARTESIAN_POINT('Ctrl Pts',(0.132978581133861,-0.27166993204342,
-0.932810533453161));
#85446=CARTESIAN_POINT('Ctrl Pts',(0.300314688882263,-0.0360408470821843,
-0.916956213054176));
#85447=CARTESIAN_POINT('Ctrl Pts',(0.193483092414029,0.232491178255772,
-0.901101892655191));
#85448=CARTESIAN_POINT('Ctrl Pts',(-0.0899859354410101,0.288773936565713,
-0.885247572256206));
#85449=CARTESIAN_POINT('Ctrl Pts',(-0.291303679176474,0.081424944059558,
-0.86939325185722));
#85450=CARTESIAN_POINT('Ctrl Pts',(-0.226680182252261,-0.200259706358852,
-0.853538931458236));
#85451=CARTESIAN_POINT('Ctrl Pts',(0.0448875217329529,-0.299120319285611,
-0.837684611059252));
#85452=CARTESIAN_POINT('Ctrl Pts',(0.275475848960733,-0.124903609460319,
-0.821830290660265));
#85453=CARTESIAN_POINT('Ctrl Pts',(0.25457271115963,0.163341941183787,-0.80597597026128));
#85454=CARTESIAN_POINT('Ctrl Pts',(0.00126130843278474,0.30246696368015,
-0.790121649862295));
#85455=CARTESIAN_POINT('Ctrl Pts',(-0.253201586545781,0.165459395585599,
-0.77426732946331));
#85456=CARTESIAN_POINT('Ctrl Pts',(-0.276507963854035,-0.122601798282684,
-0.758413009064326));
#85457=CARTESIAN_POINT('Ctrl Pts',(-0.0473806226198084,-0.298735554658316,
-0.74255868866534));
#85458=CARTESIAN_POINT('Ctrl Pts',(0.225002133713745,-0.202143253266375,
-0.726704368266355));
#85459=CARTESIAN_POINT('Ctrl Pts',(0.291972631746717,0.0789926409721084,
-0.71085004786737));
#85460=CARTESIAN_POINT('Ctrl Pts',(0.0923911790974798,0.288013411218696,
-0.694995727468384));
#85461=CARTESIAN_POINT('Ctrl Pts',(-0.191537388097839,0.234096740638372,
-0.679141407069401));
#85462=CARTESIAN_POINT('Ctrl Pts',(-0.300604824917278,-0.0335349706024578,
-0.663287086670414));
#85463=CARTESIAN_POINT('Ctrl Pts',(-0.135239682262291,-0.270551443090672,
-0.647432766271431));
#85464=CARTESIAN_POINT('Ctrl Pts',(0.153590460865475,-0.260572111608241,
-0.631578445872444));
#85465=CARTESIAN_POINT('Ctrl Pts',(0.302202540728427,-0.012707454275101,
-0.615724125473459));
#85466=CARTESIAN_POINT('Ctrl Pts',(0.174923430891825,0.246758279175934,
-0.599869805074475));
#85467=CARTESIAN_POINT('Ctrl Pts',(-0.112049351071656,0.280949813919219,
-0.584015484675488));
#85468=CARTESIAN_POINT('Ctrl Pts',(-0.296728390905827,0.0586525110069064,
-0.568161164276505));
#85469=CARTESIAN_POINT('Ctrl Pts',(-0.210513782435438,-0.217190705191142,
-0.552306843877518));
#85470=CARTESIAN_POINT('Ctrl Pts',(0.0678861655222763,-0.294752987342616,
-0.536452523478534));
#85471=CARTESIAN_POINT('Ctrl Pts',(0.284310476464735,-0.10322503567493,
-0.52059820307955));
#85472=CARTESIAN_POINT('Ctrl Pts',(0.241177884250994,0.182540634281302,
-0.504743882680563));
#85473=CARTESIAN_POINT('Ctrl Pts',(-0.0221343704231927,0.301658622721666,
-0.488889562281578));
#85474=CARTESIAN_POINT('Ctrl Pts',(-0.265239390012636,0.145381983093314,
-0.473035241882593));
#85475=CARTESIAN_POINT('Ctrl Pts',(-0.266198163246733,-0.143618915506068,
-0.457180921483609));
#85476=CARTESIAN_POINT('Ctrl Pts',(-0.0241353928614716,-0.301505120733064,
-0.441326601084624));
#85477=CARTESIAN_POINT('Ctrl Pts',(0.23996141560107,-0.184136835194144,
-0.425472280685638));
#85478=CARTESIAN_POINT('Ctrl Pts',(0.284989117804036,0.10133635910158,-0.409617960286653));
#85479=CARTESIAN_POINT('Ctrl Pts',(0.0698403620914573,0.294296073475977,
-0.393763639887668));
#85480=CARTESIAN_POINT('Ctrl Pts',(-0.209068085423801,0.218582686633334,
-0.377909319488683));
#85481=CARTESIAN_POINT('Ctrl Pts',(-0.297111018714161,-0.0566824225728229,
-0.362054999089698));
#85482=CARTESIAN_POINT('Ctrl Pts',(-0.113910992783014,-0.280200180346236,
-0.346200678690714));
#85483=CARTESIAN_POINT('Ctrl Pts',(0.173282338906218,-0.247913467482185,
-0.330346358291728));
#85484=CARTESIAN_POINT('Ctrl Pts',(0.302280196295086,0.010702056563939,
-0.314492037892742));
#85485=CARTESIAN_POINT('Ctrl Pts',(0.155315992477052,0.259547299822357,
-0.298637717493759));
#85486=CARTESIAN_POINT('Ctrl Pts',(-0.133441616172835,0.271442807024216,
-0.282783397094773));
#85487=CARTESIAN_POINT('Ctrl Pts',(-0.30037565749215,0.0355287464132556,
-0.266929076695788));
#85488=CARTESIAN_POINT('Ctrl Pts',(-0.193086494366649,-0.232820727170103,
-0.251074756296802));
#85489=CARTESIAN_POINT('Ctrl Pts',(0.0904783379914081,-0.288620101782581,
-0.235220435897817));
#85490=CARTESIAN_POINT('Ctrl Pts',(0.291441770220941,-0.0809281194962718,
-0.219366115498832));
#85491=CARTESIAN_POINT('Ctrl Pts',(0.226339010752297,0.200645862132831,
-0.203511795099848));
#85492=CARTESIAN_POINT('Ctrl Pts',(-0.0453986228963076,0.29904344356891,
-0.187657474700862));
#85493=CARTESIAN_POINT('Ctrl Pts',(-0.275686199473072,0.124433555525748,
-0.171803154301878));
#85494=CARTESIAN_POINT('Ctrl Pts',(-0.254298067335225,-0.163775415694561,
-0.155948833902892));
#85495=CARTESIAN_POINT('Ctrl Pts',(-0.000737512492624156,-0.302469326879015,
-0.140094513503908));
#85496=CARTESIAN_POINT('Ctrl Pts',(0.253467892319643,-0.165026193075203,
-0.124240193104921));
#85497=CARTESIAN_POINT('Ctrl Pts',(0.27632802680467,0.12307069050915,-0.108385872705936));
#85498=CARTESIAN_POINT('Ctrl Pts',(0.0468147861274968,0.298820470946009,
-0.0925315523069517));
#85499=CARTESIAN_POINT('Ctrl Pts',(-0.225238310074468,0.201750496382117,
-0.0766772319079666));
#85500=CARTESIAN_POINT('Ctrl Pts',(-0.292047385734954,-0.0794725446167814,
-0.0608229115089816));
#85501=CARTESIAN_POINT('Ctrl Pts',(-0.0914380522302025,-0.28824662707594,
-0.0449660161064564));
#85502=CARTESIAN_POINT('Ctrl Pts',(0.0968531300957259,-0.251807566271467,
-0.0343938941702599));
#85503=CARTESIAN_POINT('Ctrl Pts',(0.162563160710032,-0.197798868007127,
-0.0291065457003915));
#85504=CARTESIAN_POINT('Ctrl Pts',(-0.120613916559838,0.24747710494489,
-1.57170925215644));
#85505=CARTESIAN_POINT('Ctrl Pts',(-0.202789211422113,0.207426999461372,
-1.56642447869011));
#85506=CARTESIAN_POINT('Ctrl Pts',(-0.32270594729843,0.0397432696789904,
-1.55585493175745));
#85507=CARTESIAN_POINT('Ctrl Pts',(-0.20855189642005,-0.249852106644019,
-1.54000061135847));
#85508=CARTESIAN_POINT('Ctrl Pts',(0.0962707155852401,-0.310568902800926,
-1.52414629095948));
#85509=CARTESIAN_POINT('Ctrl Pts',(0.313063684806424,-0.0881460905579498,
-1.5082919705605));
#85510=CARTESIAN_POINT('Ctrl Pts',(0.244123308494345,0.214950098220732,
-1.49243765016151));
#85511=CARTESIAN_POINT('Ctrl Pts',(-0.0477240687176538,0.321705530664484,
-1.47658332976253));
#85512=CARTESIAN_POINT('Ctrl Pts',(-0.295982415709062,0.134819926027581,
-1.46072900936354));
#85513=CARTESIAN_POINT('Ctrl Pts',(-0.274038645071423,-0.175176307870519,
-1.44487468896456));
#85514=CARTESIAN_POINT('Ctrl Pts',(-0.00190998540277913,-0.325232916758775,
-1.42902036856557));
#85515=CARTESIAN_POINT('Ctrl Pts',(0.271959489175091,-0.178381005086319,
-1.41316604816659));
#85516=CARTESIAN_POINT('Ctrl Pts',(0.297549211371575,0.131325252151957,
-1.3973117277676));
#85517=CARTESIAN_POINT('Ctrl Pts',(0.0514951417277158,0.32113796451525,
-1.38145740736861));
#85518=CARTESIAN_POINT('Ctrl Pts',(-0.241570217907355,0.217773813806707,
-1.36560308696963));
#85519=CARTESIAN_POINT('Ctrl Pts',(-0.314097955906133,-0.0844042036450784,
-1.34974876657064));
#85520=CARTESIAN_POINT('Ctrl Pts',(-0.099874653801885,-0.309526383548257,
-1.33389444617166));
#85521=CARTESIAN_POINT('Ctrl Pts',(0.205527627556145,-0.252071345727164,
-1.31804012577267));
#85522=CARTESIAN_POINT('Ctrl Pts',(0.323296634239525,0.0355084586366044,
-1.30218580537369));
#85523=CARTESIAN_POINT('Ctrl Pts',(0.1459169048304,0.290671314057262,-1.2863314849747));
#85524=CARTESIAN_POINT('Ctrl Pts',(-0.164675423694167,0.280470260154686,
-1.27047716457572));
#85525=CARTESIAN_POINT('Ctrl Pts',(-0.324929846033993,0.0142181576972166,
-1.25462284417674));
#85526=CARTESIAN_POINT('Ctrl Pts',(-0.188544530413246,-0.265014188099586,
-1.23876852377775));
#85527=CARTESIAN_POINT('Ctrl Pts',(0.119969630698024,-0.302305885555697,
-1.22291420337877));
#85528=CARTESIAN_POINT('Ctrl Pts',(0.318959352110174,-0.0636120444865149,
-1.20705988297978));
#85529=CARTESIAN_POINT('Ctrl Pts',(0.226760008705413,0.233155439227114,
-1.19120556258079));
#85530=CARTESIAN_POINT('Ctrl Pts',(-0.0724564179262672,0.317067229491835,
-1.17535124218181));
#85531=CARTESIAN_POINT('Ctrl Pts',(-0.305524865565747,0.111517339441156,
-1.15949692178283));
#85532=CARTESIAN_POINT('Ctrl Pts',(-0.259669057787194,-0.1958406007232,
-1.14364260138384));
#85533=CARTESIAN_POINT('Ctrl Pts',(0.0232476466364306,-0.324408858398355,
-1.12778828098485));
#85534=CARTESIAN_POINT('Ctrl Pts',(0.28494076746996,-0.156813008095897,
-1.11193396058587));
#85535=CARTESIAN_POINT('Ctrl Pts',(0.286501570607746,0.15394288068265,-1.09607964018688));
#85536=CARTESIAN_POINT('Ctrl Pts',(0.0265051446960164,0.324158969921607,
-1.0802253197879));
#85537=CARTESIAN_POINT('Ctrl Pts',(-0.25768874787592,0.198439083078409,
-1.06437099938891));
#85538=CARTESIAN_POINT('Ctrl Pts',(-0.306629637436761,-0.108442731062269,
-1.04851667898993));
#85539=CARTESIAN_POINT('Ctrl Pts',(-0.0756376870371126,-0.316323411676782,
-1.03266235859094));
#85540=CARTESIAN_POINT('Ctrl Pts',(0.224406533447907,-0.235421469328689,
-1.01680803819196));
#85541=CARTESIAN_POINT('Ctrl Pts',(0.319582239789786,0.0604049044858338,
-1.00095371779297));
#85542=CARTESIAN_POINT('Ctrl Pts',(0.123000225862759,0.301085544177648,
-0.985099397393988));
#85543=CARTESIAN_POINT('Ctrl Pts',(-0.185872963925308,0.266894739095086,
-0.969245076995004));
#85544=CARTESIAN_POINT('Ctrl Pts',(-0.325056272792072,-0.0109535379463947,
-0.953390756596019));
#85545=CARTESIAN_POINT('Ctrl Pts',(-0.167484426643573,-0.27880194996968,
-0.937536436197032));
#85546=CARTESIAN_POINT('Ctrl Pts',(0.142989766425799,-0.292122383895027,
-0.92168211579805));
#85547=CARTESIAN_POINT('Ctrl Pts',(0.322923638163087,-0.038754153203681,
-0.905827795399063));
#85548=CARTESIAN_POINT('Ctrl Pts',(0.208049311067426,0.249994089208903,
-0.889973475000078));
#85549=CARTESIAN_POINT('Ctrl Pts',(-0.0967604540566158,0.310514049610926,
-0.874119154601094));
#85550=CARTESIAN_POINT('Ctrl Pts',(-0.313234241855012,0.0875549553396883,
-0.858264834202108));
#85551=CARTESIAN_POINT('Ctrl Pts',(-0.243745617055283,-0.215336096930725,
-0.842410513803123));
#85552=CARTESIAN_POINT('Ctrl Pts',(0.0482668426245778,-0.321639351414085,
-0.826556193404139));
#85553=CARTESIAN_POINT('Ctrl Pts',(0.296214826199661,-0.134306877018729,
-0.810701873005152));
#85554=CARTESIAN_POINT('Ctrl Pts',(0.273738012518388,0.175639007562391,
-0.794847552606168));
#85555=CARTESIAN_POINT('Ctrl Pts',(0.00135626502145843,0.325237945234271,
-0.778993232207183));
#85556=CARTESIAN_POINT('Ctrl Pts',(-0.272263663893192,0.177915872812052,
-0.763138911808198));
#85557=CARTESIAN_POINT('Ctrl Pts',(-0.29732464303076,-0.131831775841982,
-0.747284591409212));
#85558=CARTESIAN_POINT('Ctrl Pts',(-0.0509476346021148,-0.321225620091967,
-0.731430271010228));
#85559=CARTESIAN_POINT('Ctrl Pts',(0.241941237985149,-0.217361445148932,
-0.715575950611242));
#85560=CARTESIAN_POINT('Ctrl Pts',(0.313953555980292,0.0849395382748782,
-0.699721630212258));
#85561=CARTESIAN_POINT('Ctrl Pts',(0.0993467745429957,0.309696268726186,
-0.683867309813271));
#85562=CARTESIAN_POINT('Ctrl Pts',(-0.205957125970144,0.251720525061298,
-0.668012989414289));
#85563=CARTESIAN_POINT('Ctrl Pts',(-0.323235616855631,-0.036059623833061,
-0.652158669015301));
#85564=CARTESIAN_POINT('Ctrl Pts',(-0.145421092730103,-0.290919690403039,
-0.636304348616318));
#85565=CARTESIAN_POINT('Ctrl Pts',(0.165153394908594,-0.280189072993896,
-0.620450028217332));
#85566=CARTESIAN_POINT('Ctrl Pts',(0.324953615413767,-0.0136641247272328,
-0.604595707818346));
#85567=CARTESIAN_POINT('Ctrl Pts',(0.188092400387725,0.265335277321699,
-0.588741387419363));
#85568=CARTESIAN_POINT('Ctrl Pts',(-0.120484896148577,0.302100894197703,
-0.572887067020376));
#85569=CARTESIAN_POINT('Ctrl Pts',(-0.319067348634266,0.0630681180206169,
-0.557032746621392));
#85570=CARTESIAN_POINT('Ctrl Pts',(-0.226362142859338,-0.233541732362702,
-0.541178426222406));
#85571=CARTESIAN_POINT('Ctrl Pts',(0.0729969207732917,-0.316943228406093,
-0.525324105823422));
#85572=CARTESIAN_POINT('Ctrl Pts',(0.305714561514062,-0.11099624928014,
-0.509469785424436));
#85573=CARTESIAN_POINT('Ctrl Pts',(0.25933476686297,0.196283058794453,-0.493615465025452));
#85574=CARTESIAN_POINT('Ctrl Pts',(-0.0238007386588687,0.324368748978298,
-0.477761144626466));
#85575=CARTESIAN_POINT('Ctrl Pts',(-0.285207723690857,0.156326948503885,
-0.461906824227481));
#85576=CARTESIAN_POINT('Ctrl Pts',(-0.286238677395056,-0.154431149794468,
-0.446052503828496));
#85577=CARTESIAN_POINT('Ctrl Pts',(-0.0259524064584728,-0.324203690716216,
-0.430198183429511));
#85578=CARTESIAN_POINT('Ctrl Pts',(0.258026717351281,-0.197999428406388,
-0.414343863030526));
#85579=CARTESIAN_POINT('Ctrl Pts',(0.306444293819567,0.108965385213349,
-0.39848954263154));
#85580=CARTESIAN_POINT('Ctrl Pts',(0.0750982374559877,0.316451916147304,
-0.382635222232556));
#85581=CARTESIAN_POINT('Ctrl Pts',(-0.224807607713496,0.235038508005751,
-0.36678090183357));
#85582=CARTESIAN_POINT('Ctrl Pts',(-0.319478782268731,-0.0609497130667787,
-0.350926581434586));
#85583=CARTESIAN_POINT('Ctrl Pts',(-0.122486690055583,-0.301294825065426,
-0.3350722610356));
#85584=CARTESIAN_POINT('Ctrl Pts',(0.186327760114798,-0.266577433048437,
-0.319217940636616));
#85585=CARTESIAN_POINT('Ctrl Pts',(0.325037117217167,0.0115077522658523,
-0.30336362023763));
#85586=CARTESIAN_POINT('Ctrl Pts',(0.16700883177667,0.279087109078769,-0.287509299838645));
#85587=CARTESIAN_POINT('Ctrl Pts',(-0.143487660684447,0.291878159951829,
-0.27165497943966));
#85588=CARTESIAN_POINT('Ctrl Pts',(-0.322989196745625,0.0382034994486758,
-0.255800659040675));
#85589=CARTESIAN_POINT('Ctrl Pts',(-0.207622855455732,-0.250348447947614,
-0.23994633864169));
#85590=CARTESIAN_POINT('Ctrl Pts',(0.0972899267361147,-0.310348633500145,
-0.224092018242705));
#85591=CARTESIAN_POINT('Ctrl Pts',(0.313382728972451,-0.0870207277396255,
-0.20823769784372));
#85592=CARTESIAN_POINT('Ctrl Pts',(0.243378760733948,0.215751324130884,
-0.192383377444734));
#85593=CARTESIAN_POINT('Ctrl Pts',(-0.0488164216270374,0.321556688171018,
-0.17652905704575));
#85594=CARTESIAN_POINT('Ctrl Pts',(-0.296441012780766,0.133801435452586,
-0.160674736646764));
#85595=CARTESIAN_POINT('Ctrl Pts',(-0.273442692355043,-0.176105115852303,
-0.14482041624778));
#85596=CARTESIAN_POINT('Ctrl Pts',(-0.000793035526154019,-0.325240486344656,
-0.128966095848794));
#85597=CARTESIAN_POINT('Ctrl Pts',(0.272550018282581,-0.177450056999848,
-0.11311177544981));
#85598=CARTESIAN_POINT('Ctrl Pts',(0.297131159565674,0.132335968241762,
-0.0972574550508239));
#85599=CARTESIAN_POINT('Ctrl Pts',(0.0503391995655778,0.321316929233932,
-0.0814031346518392));
#85600=CARTESIAN_POINT('Ctrl Pts',(-0.242195194692815,0.216939119879229,
-0.0655488142528539));
#85601=CARTESIAN_POINT('Ctrl Pts',(-0.314033937762277,-0.0854555710786095,
-0.049694493853869));
#85602=CARTESIAN_POINT('Ctrl Pts',(-0.0983218922877928,-0.309947042051257,
-0.0338375984513437));
#85603=CARTESIAN_POINT('Ctrl Pts',(0.104144639925541,-0.270764695926192,
-0.0232654765151473));
#85604=CARTESIAN_POINT('Ctrl Pts',(0.174801597228414,-0.212689996347276,
-0.017978128045279));
#85605=CARTESIAN_POINT('Ctrl Pts',(-0.129058494781408,0.264803793525795,
-1.56058083450132));
#85606=CARTESIAN_POINT('Ctrl Pts',(-0.216987153145491,0.221949648026132,
-1.55529606103499));
#85607=CARTESIAN_POINT('Ctrl Pts',(-0.345299655323625,0.0425258271081653,
-1.54472651410234));
#85608=CARTESIAN_POINT('Ctrl Pts',(-0.223153302732089,-0.267345076929359,
-1.52887219370335));
#85609=CARTESIAN_POINT('Ctrl Pts',(0.103010945994745,-0.33231285629894,
-1.51301787330437));
#85610=CARTESIAN_POINT('Ctrl Pts',(0.334982306223297,-0.0943174891649531,
-1.49716355290538));
#85611=CARTESIAN_POINT('Ctrl Pts',(0.261215186721073,0.229999463749451,
-1.48130923250639));
#85612=CARTESIAN_POINT('Ctrl Pts',(-0.0510653882173629,0.344229196220614,
-1.46545491210741));
#85613=CARTESIAN_POINT('Ctrl Pts',(-0.316705121122787,0.144259113839725,
-1.44960059170842));
#85614=CARTESIAN_POINT('Ctrl Pts',(-0.29322499470705,-0.18744097911718,
-1.43374627130944));
#85615=CARTESIAN_POINT('Ctrl Pts',(-0.00204370978215536,-0.348003546252736,
-1.41789195091045));
#85616=CARTESIAN_POINT('Ctrl Pts',(0.29100027024697,-0.190870047757833,
-1.40203763051147));
#85617=CARTESIAN_POINT('Ctrl Pts',(0.318381613318725,0.140519766316618,
-1.38618331011248));
#85618=CARTESIAN_POINT('Ctrl Pts',(0.0551004864901935,0.343621892892786,
-1.3703289897135));
#85619=CARTESIAN_POINT('Ctrl Pts',(-0.258483345839064,0.233020876979461,
-1.35447466931451));
#85620=CARTESIAN_POINT('Ctrl Pts',(-0.336088990054911,-0.0903136204042676,
-1.33862034891553));
#85621=CARTESIAN_POINT('Ctrl Pts',(-0.106867207815869,-0.331197346833964,
-1.32276602851654));
#85622=CARTESIAN_POINT('Ctrl Pts',(0.219917294827507,-0.269719692262318,
-1.30691170811756));
#85623=CARTESIAN_POINT('Ctrl Pts',(0.345931698206229,0.0379945229734283,
-1.29105738771857));
#85624=CARTESIAN_POINT('Ctrl Pts',(0.156133028739111,0.31102217172223,-1.27520306731959));
#85625=CARTESIAN_POINT('Ctrl Pts',(-0.176204893395666,0.300106908381147,
-1.2593487469206));
#85626=CARTESIAN_POINT('Ctrl Pts',(-0.347679256546638,0.0152136178254138,
-1.24349442652162));
#85627=CARTESIAN_POINT('Ctrl Pts',(-0.201745155023878,-0.283568705729589,
-1.22764010612263));
#85628=CARTESIAN_POINT('Ctrl Pts',(0.128369100340815,-0.323471317955452,
-1.21178578572365));
#85629=CARTESIAN_POINT('Ctrl Pts',(0.341290748645665,-0.0680657335865966,
-1.19593146532466));
#85630=CARTESIAN_POINT('Ctrl Pts',(0.242636225029816,0.249479420741813,
-1.18007714492568));
#85631=CARTESIAN_POINT('Ctrl Pts',(-0.0775293307897633,0.339266152280424,
-1.16422282452669));
#85632=CARTESIAN_POINT('Ctrl Pts',(-0.326915669375897,0.119325036287693,
-1.14836850412771));
#85633=CARTESIAN_POINT('Ctrl Pts',(-0.277849345209651,-0.209552047287046,
-1.13251418372872));
#85634=CARTESIAN_POINT('Ctrl Pts',(0.0248752910748828,-0.347121792847813,
-1.11665986332974));
#85635=CARTESIAN_POINT('Ctrl Pts',(0.304890410662428,-0.167792004142087,
-1.10080554293075));
#85636=CARTESIAN_POINT('Ctrl Pts',(0.306560490777213,0.164720929639658,
-1.08495122253177));
#85637=CARTESIAN_POINT('Ctrl Pts',(0.0283608573205941,0.346854408854388,
-1.06909690213278));
#85638=CARTESIAN_POINT('Ctrl Pts',(-0.275730387268151,0.212332457964726,
-1.0532425817338));
#85639=CARTESIAN_POINT('Ctrl Pts',(-0.328097789970408,-0.116035164432605,
-1.03738826133481));
#85640=CARTESIAN_POINT('Ctrl Pts',(-0.0809333310465426,-0.338470257326172,
-1.02153394093583));
#85641=CARTESIAN_POINT('Ctrl Pts',(0.240117975205065,-0.251904103086773,
-1.00567962053684));
#85642=CARTESIAN_POINT('Ctrl Pts',(0.341957246746726,0.0646340511336335,
-0.989825300137861));
#85643=CARTESIAN_POINT('Ctrl Pts',(0.13161187747142,0.322165536451435,-0.973970979738877));
#85644=CARTESIAN_POINT('Ctrl Pts',(-0.198886543352222,0.285580920304504,
-0.958116659339892));
#85645=CARTESIAN_POINT('Ctrl Pts',(-0.34781453485915,-0.0117204312753678,
-0.942262338940907));
#85646=CARTESIAN_POINT('Ctrl Pts',(-0.179210563908882,-0.298321794296082,
-0.926408018541922));
#85647=CARTESIAN_POINT('Ctrl Pts',(0.153000951717736,-0.312574835746634,
-0.910553698142936));
#85648=CARTESIAN_POINT('Ctrl Pts',(0.34553258744391,-0.041467459325178,
-0.894699377743952));
#85649=CARTESIAN_POINT('Ctrl Pts',(0.222615529720825,0.267497000162033,
-0.878845057344966));
#85650=CARTESIAN_POINT('Ctrl Pts',(-0.103534972672222,0.332254162656138,
-0.86299073694598));
#85651=CARTESIAN_POINT('Ctrl Pts',(-0.33516480453355,0.0936849666198187,
-0.847136416546997));
#85652=CARTESIAN_POINT('Ctrl Pts',(-0.260811051858304,-0.230412487502598,
-0.83128209614801));
#85653=CARTESIAN_POINT('Ctrl Pts',(0.0516461635162027,-0.344158383542559,
-0.815427775749027));
#85654=CARTESIAN_POINT('Ctrl Pts',(0.316953803438588,-0.14371014457714,
-0.799573455350039));
#85655=CARTESIAN_POINT('Ctrl Pts',(0.292903313877147,0.187936073940996,
-0.783719134951057));
#85656=CARTESIAN_POINT('Ctrl Pts',(0.00145122161013225,0.348008926788391,
-0.767864814552071));
#85657=CARTESIAN_POINT('Ctrl Pts',(-0.291325741240603,0.190372350038505,
-0.752010494153085));
#85658=CARTESIAN_POINT('Ctrl Pts',(-0.318141322207485,-0.141061753401278,
-0.7361561737541));
#85659=CARTESIAN_POINT('Ctrl Pts',(-0.0545146465844214,-0.343715685525617,
-0.720301853355115));
#85660=CARTESIAN_POINT('Ctrl Pts',(0.258880342256552,-0.232579637031489,
-0.704447532956129));
#85661=CARTESIAN_POINT('Ctrl Pts',(0.335934480213866,0.0908864355776483,
-0.688593212557146));
#85662=CARTESIAN_POINT('Ctrl Pts',(0.106302369988512,0.331379126233676,
-0.672738892158159));
#85663=CARTESIAN_POINT('Ctrl Pts',(-0.220376863842449,0.269344309484226,
-0.656884571759176));
#85664=CARTESIAN_POINT('Ctrl Pts',(-0.345866408793984,-0.0385842770636646,
-0.641030251360189));
#85665=CARTESIAN_POINT('Ctrl Pts',(-0.155602503197914,-0.311287937715406,
-0.625175930961206));
#85666=CARTESIAN_POINT('Ctrl Pts',(0.176716328951713,-0.29980603437955,
-0.609321610562219));
#85667=CARTESIAN_POINT('Ctrl Pts',(0.347704690099108,-0.0146207951793645,
-0.593467290163235));
#85668=CARTESIAN_POINT('Ctrl Pts',(0.201261369883626,0.283912275467464,
-0.577612969764248));
#85669=CARTESIAN_POINT('Ctrl Pts',(-0.128920441225498,0.323251974476187,
-0.561758649365265));
#85670=CARTESIAN_POINT('Ctrl Pts',(-0.341406306362706,0.0674837250343271,
-0.545904328966279));
#85671=CARTESIAN_POINT('Ctrl Pts',(-0.242210503283238,-0.249892759534263,
-0.530050008567293));
#85672=CARTESIAN_POINT('Ctrl Pts',(0.0781076760243074,-0.339133469469571,
-0.51419568816831));
#85673=CARTESIAN_POINT('Ctrl Pts',(0.327118646563388,-0.11876746288535,
-0.498341367769324));
#85674=CARTESIAN_POINT('Ctrl Pts',(0.277491649474946,0.210025483307604,
-0.482487047370338));
#85675=CARTESIAN_POINT('Ctrl Pts',(-0.0254671068945446,0.347078875234931,
-0.466632726971353));
#85676=CARTESIAN_POINT('Ctrl Pts',(-0.305176057369077,0.167271913914455,
-0.450778406572368));
#85677=CARTESIAN_POINT('Ctrl Pts',(-0.306279191543379,-0.165243384082869,
-0.434924086173383));
#85678=CARTESIAN_POINT('Ctrl Pts',(-0.0277694200554746,-0.346902260699368,
-0.419069765774398));
#85679=CARTESIAN_POINT('Ctrl Pts',(0.276092019101493,-0.211862021618632,
-0.403215445375414));
#85680=CARTESIAN_POINT('Ctrl Pts',(0.327899469835099,0.116594411325117,
-0.387361124976428));
#85681=CARTESIAN_POINT('Ctrl Pts',(0.0803561128205185,0.338607758818632,
-0.371506804577444));
#85682=CARTESIAN_POINT('Ctrl Pts',(-0.240547130003191,0.251494329378168,
-0.355652484178459));
#85683=CARTESIAN_POINT('Ctrl Pts',(-0.3418465458233,-0.0652170035607345,
-0.339798163779473));
#85684=CARTESIAN_POINT('Ctrl Pts',(-0.131062387328152,-0.322389469784616,
-0.323943843380488));
#85685=CARTESIAN_POINT('Ctrl Pts',(0.199373181323377,-0.285241398614689,
-0.308089522981502));
#85686=CARTESIAN_POINT('Ctrl Pts',(0.347794038139249,0.0123134479677662,
-0.292235202582517));
#85687=CARTESIAN_POINT('Ctrl Pts',(0.178701671076287,0.29862691833518,-0.276380882183532));
#85688=CARTESIAN_POINT('Ctrl Pts',(-0.153533705196059,0.312313512879442,
-0.260526561784547));
#85689=CARTESIAN_POINT('Ctrl Pts',(-0.3456027359991,0.0408782524840959,
-0.244672241385563));
#85690=CARTESIAN_POINT('Ctrl Pts',(-0.222159216544815,-0.267876168725123,
-0.228817920986577));
#85691=CARTESIAN_POINT('Ctrl Pts',(0.104101515480821,-0.33207716521771,
-0.212963600587593));
#85692=CARTESIAN_POINT('Ctrl Pts',(0.335323687723963,-0.0931133359829788,
-0.197109280188608));
#85693=CARTESIAN_POINT('Ctrl Pts',(0.260418510715598,0.230856786128936,
-0.181254959789622));
#85694=CARTESIAN_POINT('Ctrl Pts',(-0.0522342203577671,0.344069932773126,
-0.165400639390636));
#85695=CARTESIAN_POINT('Ctrl Pts',(-0.317195826088459,0.143169315379424,
-0.149546318991652));
#85696=CARTESIAN_POINT('Ctrl Pts',(-0.292587317374861,-0.188434816010044,
-0.133691998592666));
#85697=CARTESIAN_POINT('Ctrl Pts',(-0.000848558559683781,-0.348011645810298,
-0.117837678193682));
#85698=CARTESIAN_POINT('Ctrl Pts',(0.291632144245519,-0.189873920924492,
-0.101983357794696));
#85699=CARTESIAN_POINT('Ctrl Pts',(0.317934292326678,0.141601245974372,
-0.0861290373957114));
#85700=CARTESIAN_POINT('Ctrl Pts',(0.053863613003659,0.343813387521854,
-0.0702747169967265));
#85701=CARTESIAN_POINT('Ctrl Pts',(-0.259152079311164,0.23212774337634,
-0.0544203965977413));
#85702=CARTESIAN_POINT('Ctrl Pts',(-0.336020489789599,-0.0914385975404377,
-0.0385660761987564));
#85703=CARTESIAN_POINT('Ctrl Pts',(-0.105205732345383,-0.331647457026574,
-0.0227091807962312));
#85704=CARTESIAN_POINT('Ctrl Pts',(0.111436149755356,-0.289721825580918,
-0.0121370588600346));
#85705=CARTESIAN_POINT('Ctrl Pts',(0.187040033746796,-0.227581124687426,
-0.00684971039016626));
#85706=CARTESIAN_POINT('Ctrl Pts',(-0.289031747819831,-0.055539659978255,
-0.04));
#85707=CARTESIAN_POINT('Ctrl Pts',(-0.288640713323037,-0.0572777523841593,
-0.04));
#85708=CARTESIAN_POINT('Ctrl Pts',(-0.288249678826243,-0.0590158447900636,
-0.04));
#85709=CARTESIAN_POINT('Ctrl Pts',(-0.287858644329449,-0.0607539371959678,
-0.04));
#85710=CARTESIAN_POINT('Ctrl Pts',(-0.13799857747695,-0.193363938662942,
-1.5608));
#85711=CARTESIAN_POINT('Ctrl Pts',(-0.143347841422346,-0.190455713481887,
-1.5608));
#85712=CARTESIAN_POINT('Ctrl Pts',(-0.148566997856137,-0.187334258556034,
-1.5608));
#85713=CARTESIAN_POINT('Ctrl Pts',(-0.15364167413773,-0.184002459902945,
-1.5608));
#85714=CARTESIAN_POINT('Ctrl Pts',(-0.163907115485033,-0.177262644049398,
-1.5608));
#85715=CARTESIAN_POINT('Ctrl Pts',(-0.173582104512979,-0.169663735623815,
-1.5608));
#85716=CARTESIAN_POINT('Ctrl Pts',(-0.182636032389057,-0.161324058116206,
-1.5608));
#85717=CARTESIAN_POINT('Ctrl Pts',(-0.188173868816878,-0.156223093040049,
-1.5608));
#85718=CARTESIAN_POINT('Ctrl Pts',(-0.193479882338644,-0.150842423408572,
-1.5608));
#85719=CARTESIAN_POINT('Ctrl Pts',(-0.198524103660284,-0.145232040158292,
-1.5608));
#85720=CARTESIAN_POINT('Ctrl Pts',(-0.206390733930232,-0.136482461603259,
-1.5608));
#85721=CARTESIAN_POINT('Ctrl Pts',(-0.213635127195895,-0.127163051947901,
-1.5608));
#85722=CARTESIAN_POINT('Ctrl Pts',(-0.220229011985289,-0.117368722208056,
-1.5608));
#85723=CARTESIAN_POINT('Ctrl Pts',(-0.223143397241071,-0.113039794558308,
-1.5608));
#85724=CARTESIAN_POINT('Ctrl Pts',(-0.225930582649798,-0.108617881329991,
-1.5608));
#85725=CARTESIAN_POINT('Ctrl Pts',(-0.228587451034113,-0.104110300495371,
-1.5608));
#85726=CARTESIAN_POINT('Ctrl Pts',(-0.230967501738554,-0.10007236206978,
-1.5608));
#85727=CARTESIAN_POINT('Ctrl Pts',(-0.233238383225063,-0.0959733682384296,
-1.5608));
#85728=CARTESIAN_POINT('Ctrl Pts',(-0.235397692200457,-0.0918213261469215,
-1.5608));
#85729=CARTESIAN_POINT('Ctrl Pts',(-0.242841770000136,-0.0775074300306483,
-1.5608));
#85730=CARTESIAN_POINT('Ctrl Pts',(-0.24896693470216,-0.0625588879644513,
-1.5608));
#85731=CARTESIAN_POINT('Ctrl Pts',(-0.253699085536977,-0.047196706931204,
-1.5608));
#85732=CARTESIAN_POINT('Ctrl Pts',(-0.256802926190838,-0.0371205779811004,
-1.5608));
#85733=CARTESIAN_POINT('Ctrl Pts',(-0.259306827718714,-0.0268655758638595,
-1.5608));
#85734=CARTESIAN_POINT('Ctrl Pts',(-0.261179689706241,-0.0164868296819522,
-1.5608));
#85735=CARTESIAN_POINT('Ctrl Pts',(-0.262261665440453,-0.0104908985374452,
-1.5608));
#85736=CARTESIAN_POINT('Ctrl Pts',(-0.263132275784059,-0.00445291160850025,
-1.5608));
#85737=CARTESIAN_POINT('Ctrl Pts',(-0.263782798320229,0.00158770973103373,
-1.5608));
#85738=CARTESIAN_POINT('Ctrl Pts',(-0.264886445795179,0.0118359580511637,
-1.5608));
#85739=CARTESIAN_POINT('Ctrl Pts',(-0.265361036560997,0.0221109639333779,
-1.5608));
#85740=CARTESIAN_POINT('Ctrl Pts',(-0.265185866874642,0.0323592383439703,
-1.5608));
#85741=CARTESIAN_POINT('Ctrl Pts',(-0.264987655497751,0.0439555631644492,
-1.5608));
#85742=CARTESIAN_POINT('Ctrl Pts',(-0.263958005355191,0.0555178554776766,
-1.5608));
#85743=CARTESIAN_POINT('Ctrl Pts',(-0.262149841841104,0.0669878505690906,
-1.5608));
#85744=CARTESIAN_POINT('Ctrl Pts',(-0.261038096613289,0.0740401509869451,
-1.5608));
#85745=CARTESIAN_POINT('Ctrl Pts',(-0.259631739078235,0.0810576215322809,
-1.5608));
#85746=CARTESIAN_POINT('Ctrl Pts',(-0.25794033900309,0.0880268053398159,
-1.5608));
#85747=CARTESIAN_POINT('Ctrl Pts',(-0.256631126704129,0.0934212364319209,
-1.5608));
#85748=CARTESIAN_POINT('Ctrl Pts',(-0.255151399390779,0.0987837905468475,
-1.5608));
#85749=CARTESIAN_POINT('Ctrl Pts',(-0.253512272984399,0.104089767724613,
-1.5608));
#85750=CARTESIAN_POINT('Ctrl Pts',(-0.248424210607189,0.120560213656933,
-1.5608));
#85751=CARTESIAN_POINT('Ctrl Pts',(-0.241793533995896,0.13653471216082,
-1.5608));
#85752=CARTESIAN_POINT('Ctrl Pts',(-0.233782283533326,0.151832188232471,
-1.5608));
#85753=CARTESIAN_POINT('Ctrl Pts',(-0.229722814977607,0.159583740051364,
-1.5608));
#85754=CARTESIAN_POINT('Ctrl Pts',(-0.225307871711475,0.167161501680917,
-1.5608));
#85755=CARTESIAN_POINT('Ctrl Pts',(-0.220552921268545,0.174541049986005,
-1.5608));
#85756=CARTESIAN_POINT('Ctrl Pts',(-0.217270098793488,0.179635897413433,
-1.5608));
#85757=CARTESIAN_POINT('Ctrl Pts',(-0.213823767062381,0.184638075610162,
-1.5608));
#85758=CARTESIAN_POINT('Ctrl Pts',(-0.210222729269013,0.189532882285389,
-1.5608));
#85759=CARTESIAN_POINT('Ctrl Pts',(-0.206848865553593,0.194118896535493,
-1.5608));
#85760=CARTESIAN_POINT('Ctrl Pts',(-0.203344351977369,0.198603678931769,
-1.5608));
#85761=CARTESIAN_POINT('Ctrl Pts',(-0.199718097012662,0.202976801403612,
-1.5608));
#85762=CARTESIAN_POINT('Ctrl Pts',(-0.188601077808648,0.216383494251783,
-1.5608));
#85763=CARTESIAN_POINT('Ctrl Pts',(-0.176331421703839,0.228758241429328,
-1.5608));
#85764=CARTESIAN_POINT('Ctrl Pts',(-0.163036176043001,0.239920308741562,
-1.5608));
#85765=CARTESIAN_POINT('Ctrl Pts',(-0.15230812646604,0.248927078120766,
-1.5608));
#85766=CARTESIAN_POINT('Ctrl Pts',(-0.140911166079345,0.257144449634528,
-1.5608));
#85767=CARTESIAN_POINT('Ctrl Pts',(-0.128892185405328,0.264462557919714,
-1.5608));
#85768=CARTESIAN_POINT('Origin',(-3.51939854619125E-17,0.,-1.5608));
#85769=CARTESIAN_POINT('',(-0.2942,-3.60291088309151E-17,-1.5608));
#85770=CARTESIAN_POINT('Origin',(0.,0.,-1.5608));
#85771=CARTESIAN_POINT('',(0.133736061201431,0.262046381265468,-1.5608));
#85772=CARTESIAN_POINT('Origin',(0.,0.,-1.5608));
#85773=CARTESIAN_POINT('Ctrl Pts',(0.13373606120143,0.262046381265467,-1.5608));
#85774=CARTESIAN_POINT('Ctrl Pts',(0.138550012611077,0.259017157142651,
-1.5608));
#85775=CARTESIAN_POINT('Ctrl Pts',(0.143264321808573,0.255840579156758,
-1.5608));
#85776=CARTESIAN_POINT('Ctrl Pts',(0.147871259490879,0.252516190150327,
-1.5608));
#85777=CARTESIAN_POINT('Ctrl Pts',(0.157320856382195,0.245697314318481,
-1.5608));
#85778=CARTESIAN_POINT('Ctrl Pts',(0.166319266874593,0.238256907737579,
-1.5608));
#85779=CARTESIAN_POINT('Ctrl Pts',(0.174835840546171,0.230258755145514,
-1.5608));
#85780=CARTESIAN_POINT('Ctrl Pts',(0.179702443415592,0.225688392244233,
-1.5608));
#85781=CARTESIAN_POINT('Ctrl Pts',(0.184412787467239,0.220934445028738,
-1.5608));
#85782=CARTESIAN_POINT('Ctrl Pts',(0.18895591579128,0.216012380917119,-1.5608));
#85783=CARTESIAN_POINT('Ctrl Pts',(0.19523865863058,0.209205603550034,-1.5608));
#85784=CARTESIAN_POINT('Ctrl Pts',(0.201189436575403,0.202090872429547,
-1.5608));
#85785=CARTESIAN_POINT('Ctrl Pts',(0.20678943857,0.194705868097706,-1.5608));
#85786=CARTESIAN_POINT('Ctrl Pts',(0.212443879605949,0.187249072263542,
-1.5608));
#85787=CARTESIAN_POINT('Ctrl Pts',(0.21774229688384,0.179514930803699,-1.5608));
#85788=CARTESIAN_POINT('Ctrl Pts',(0.222665799064572,0.171535487495526,
-1.5608));
#85789=CARTESIAN_POINT('Ctrl Pts',(0.226114144708047,0.165946807413943,
-1.5608));
#85790=CARTESIAN_POINT('Ctrl Pts',(0.229379510809365,0.160235806619833,
-1.5608));
#85791=CARTESIAN_POINT('Ctrl Pts',(0.232450764193899,0.154419684787329,
-1.5608));
#85792=CARTESIAN_POINT('Ctrl Pts',(0.23528691598115,0.149048781685295,-1.5608));
#85793=CARTESIAN_POINT('Ctrl Pts',(0.237953497096427,0.14359591196093,-1.5608));
#85794=CARTESIAN_POINT('Ctrl Pts',(0.240443806796245,0.138075597522685,
-1.5608));
#85795=CARTESIAN_POINT('Ctrl Pts',(0.247289923459264,0.122899687207787,
-1.5608));
#85796=CARTESIAN_POINT('Ctrl Pts',(0.25281522573498,0.107199566527781,-1.5608));
#85797=CARTESIAN_POINT('Ctrl Pts',(0.256905339126335,0.0911583963714125,
-1.5608));
#85798=CARTESIAN_POINT('Ctrl Pts',(0.259577627326119,0.0806778483723795,
-1.5608));
#85799=CARTESIAN_POINT('Ctrl Pts',(0.261636317517558,0.0700514990909618,
-1.5608));
#85800=CARTESIAN_POINT('Ctrl Pts',(0.263037088781112,0.0593310937249914,
-1.5608));
#85801=CARTESIAN_POINT('Ctrl Pts',(0.263736056624588,0.0539817416824344,
-1.5608));
#85802=CARTESIAN_POINT('Ctrl Pts',(0.26427047436316,0.0486102636085355,
-1.5608));
#85803=CARTESIAN_POINT('Ctrl Pts',(0.264633964208612,0.043242546357013,
-1.5608));
#85804=CARTESIAN_POINT('Ctrl Pts',(0.265344592360124,0.0327485778568958,
-1.5608));
#85805=CARTESIAN_POINT('Ctrl Pts',(0.265405260271088,0.0222518652651568,
-1.5608));
#85806=CARTESIAN_POINT('Ctrl Pts',(0.264782683669769,0.0118008989594462,
-1.5608));
#85807=CARTESIAN_POINT('Ctrl Pts',(0.263877775160184,-0.00338947010257891,
-1.5608));
#85808=CARTESIAN_POINT('Ctrl Pts',(0.261530657070704,-0.0184845232811562,
-1.5608));
#85809=CARTESIAN_POINT('Ctrl Pts',(0.257827438680858,-0.0333213284021663,
-1.5608));
#85810=CARTESIAN_POINT('Ctrl Pts',(0.255791351029307,-0.0414788369569387,
-1.5608));
#85811=CARTESIAN_POINT('Ctrl Pts',(0.253340030824081,-0.0495684731839285,
-1.5608));
#85812=CARTESIAN_POINT('Ctrl Pts',(0.250506238567754,-0.0575042321542823,
-1.5608));
#85813=CARTESIAN_POINT('Ctrl Pts',(0.245534376020338,-0.0714274485516459,
-1.5608));
#85814=CARTESIAN_POINT('Ctrl Pts',(0.239384092384913,-0.0849048911441926,
-1.5608));
#85815=CARTESIAN_POINT('Ctrl Pts',(0.232141482928074,-0.0977877984656227,
-1.5608));
#85816=CARTESIAN_POINT('Ctrl Pts',(0.226804087220809,-0.107281776381215,
-1.5608));
#85817=CARTESIAN_POINT('Ctrl Pts',(0.220873249583642,-0.116451756653311,
-1.5608));
#85818=CARTESIAN_POINT('Ctrl Pts',(0.214372210700434,-0.125230152591395,
-1.5608));
#85819=CARTESIAN_POINT('Ctrl Pts',(0.210401710388729,-0.130591545506374,
-1.5608));
#85820=CARTESIAN_POINT('Ctrl Pts',(0.206215774074286,-0.135808510284193,
-1.5608));
#85821=CARTESIAN_POINT('Ctrl Pts',(0.201844453986288,-0.140836689913866,
-1.5608));
#85822=CARTESIAN_POINT('Ctrl Pts',(0.192116839118631,-0.152026031791883,
-1.5608));
#85823=CARTESIAN_POINT('Ctrl Pts',(0.181455103880824,-0.162311068884459,
-1.5608));
#85824=CARTESIAN_POINT('Ctrl Pts',(0.169933457476246,-0.171520717268733,
-1.5608));
#85825=CARTESIAN_POINT('Ctrl Pts',(0.160599905043598,-0.178981346857809,
-1.5608));
#85826=CARTESIAN_POINT('Ctrl Pts',(0.150701251204416,-0.185735832894192,
-1.5608));
#85827=CARTESIAN_POINT('Ctrl Pts',(0.140268421710186,-0.191669440498754,
-1.5608));
#85828=CARTESIAN_POINT('Ctrl Pts',(0.139416665144678,-0.1921538718064,-1.5608));
#85829=CARTESIAN_POINT('Ctrl Pts',(0.138561345670519,-0.192632817908258,
-1.5608));
#85830=CARTESIAN_POINT('Ctrl Pts',(0.137702479013106,-0.193106208855762,
-1.5608));
#85831=CARTESIAN_POINT('Ctrl Pts',(0.170904886030586,-0.239913673682597,
-1.59394040064334));
#85832=CARTESIAN_POINT('Ctrl Pts',(0.250610379973567,-0.183139249212075,
-1.58865305194158));
#85833=CARTESIAN_POINT('Ctrl Pts',(0.34758798138322,0.0150557195712735,
-1.57808092977351));
#85834=CARTESIAN_POINT('Ctrl Pts',(0.175911135758696,0.300519364992409,
-1.56222403413909));
#85835=CARTESIAN_POINT('Ctrl Pts',(-0.156485212151456,0.310711293896572,
-1.54636971374011));
#85836=CARTESIAN_POINT('Ctrl Pts',(-0.345940875846988,0.0376795876694137,
-1.53051539334112));
#85837=CARTESIAN_POINT('Ctrl Pts',(-0.219616959829241,-0.269976713895109,
-1.51466107294214));
#85838=CARTESIAN_POINT('Ctrl Pts',(0.107224807406404,-0.331044119307512,
-1.49880675254315));
#85839=CARTESIAN_POINT('Ctrl Pts',(0.33616586372552,-0.089951456236232,
-1.48295243214416));
#85840=CARTESIAN_POINT('Ctrl Pts',(0.258215431334032,0.233293241644007,
-1.46709811174518));
#85841=CARTESIAN_POINT('Ctrl Pts',(-0.0554719698132699,0.343539578459029,
-1.45124379134619));
#85842=CARTESIAN_POINT('Ctrl Pts',(-0.318515442143559,0.140165531986085,
-1.43538947094721));
#85843=CARTESIAN_POINT('Ctrl Pts',(-0.290775969960518,-0.19117511072713,
-1.41953515054822));
#85844=CARTESIAN_POINT('Ctrl Pts',(0.00242342836231637,-0.34798294308962,
-1.40368083014924));
#85845=CARTESIAN_POINT('Ctrl Pts',(0.29341015959215,-0.187106331189504,
-1.38782650975025));
#85846=CARTESIAN_POINT('Ctrl Pts',(0.31653269414384,0.144586806748901,-1.37197218935127));
#85847=CARTESIAN_POINT('Ctrl Pts',(0.0506814801073806,0.344281283774666,
-1.35611786895228));
#85848=CARTESIAN_POINT('Ctrl Pts',(-0.26143858271537,0.229669606964089,
-1.3402635485533));
#85849=CARTESIAN_POINT('Ctrl Pts',(-0.334882305766732,-0.0946155212339324,
-1.32440922815431));
#85850=CARTESIAN_POINT('Ctrl Pts',(-0.102600337987051,-0.332522806167084,
-1.30855490775533));
#85851=CARTESIAN_POINT('Ctrl Pts',(0.223349035049687,-0.266858504519963,
-1.29270058735634));
#85852=CARTESIAN_POINT('Ctrl Pts',(0.345395323465393,0.042430202855741,
-1.27684626695736));
#85853=CARTESIAN_POINT('Ctrl Pts',(0.152118230161139,0.312982898076324,
-1.26099194655837));
#85854=CARTESIAN_POINT('Ctrl Pts',(-0.180032875201427,0.297802644874621,
-1.24513762615939));
#85855=CARTESIAN_POINT('Ctrl Pts',(-0.347825719725829,0.0107480176866395,
-1.2292833057604));
#85856=CARTESIAN_POINT('Ctrl Pts',(-0.198076390550669,-0.286118846923063,
-1.21342898536142));
#85857=CARTESIAN_POINT('Ctrl Pts',(0.132503751226997,-0.321777884749036,
-1.19757466496243));
#85858=CARTESIAN_POINT('Ctrl Pts',(0.342116618997376,-0.0636747215274613,
-1.18172034456345));
#85859=CARTESIAN_POINT('Ctrl Pts',(0.239399349463731,0.252559305152815,
-1.16586602416446));
#85860=CARTESIAN_POINT('Ctrl Pts',(-0.081873896380812,0.338223175217988,
-1.15001170376548));
#85861=CARTESIAN_POINT('Ctrl Pts',(-0.3284016201621,0.11511136794454,-1.13415738336649));
#85862=CARTESIAN_POINT('Ctrl Pts',(-0.275120105184066,-0.213089602931875,
-1.1183030629675));
#85863=CARTESIAN_POINT('Ctrl Pts',(0.0293281039782686,-0.346753678385599,
-1.10244874256852));
#85864=CARTESIAN_POINT('Ctrl Pts',(0.307001668962005,-0.163854284076304,
-1.08659442216953));
#85865=CARTESIAN_POINT('Ctrl Pts',(0.304402753490565,0.168633373989131,
-1.07074010177055));
#85866=CARTESIAN_POINT('Ctrl Pts',(0.0239039977140675,0.347169771220429,
-1.05488578137156));
#85867=CARTESIAN_POINT('Ctrl Pts',(-0.27841754734824,0.20876283310098,-1.03903146097258));
#85868=CARTESIAN_POINT('Ctrl Pts',(-0.326562048809314,-0.120230942079134,
-1.02317714057359));
#85869=CARTESIAN_POINT('Ctrl Pts',(-0.0765767200594529,-0.33946171669388,
-1.00732282017461));
#85870=CARTESIAN_POINT('Ctrl Pts',(0.243318154618006,-0.248786106503311,
-0.991468499775624));
#85871=CARTESIAN_POINT('Ctrl Pts',(0.341079439712692,0.069014976353469,
-0.975614179376641));
#85872=CARTESIAN_POINT('Ctrl Pts',(0.127457464502766,0.323809891600497,
-0.959759858977655));
#85873=CARTESIAN_POINT('Ctrl Pts',(-0.20252485444545,0.28298751648729,-0.94390553857867));
#85874=CARTESIAN_POINT('Ctrl Pts',(-0.347615203584335,-0.0161839856901046,
-0.928051218179684));
#85875=CARTESIAN_POINT('Ctrl Pts',(-0.175355566706118,-0.300580565541041,
-0.9121968977807));
#85876=CARTESIAN_POINT('Ctrl Pts',(0.156992254084647,-0.310566713144241,
-0.896342577381714));
#85877=CARTESIAN_POINT('Ctrl Pts',(0.346016396495308,-0.0370257277065219,
-0.88048825698273));
#85878=CARTESIAN_POINT('Ctrl Pts',(0.219150159379363,0.270317329817745,
-0.864633936583744));
#85879=CARTESIAN_POINT('Ctrl Pts',(-0.107785865529432,0.33087831350493,
-0.84877961618476));
#85880=CARTESIAN_POINT('Ctrl Pts',(-0.336320432257163,0.0893689991112763,
-0.832925295785774));
#85881=CARTESIAN_POINT('Ctrl Pts',(-0.257816401784462,-0.233728376811007,
-0.81707097538679));
#85882=CARTESIAN_POINT('Ctrl Pts',(0.056057171382673,-0.343447004197692,
-0.801216654987804));
#85883=CARTESIAN_POINT('Ctrl Pts',(0.318754206898361,-0.13962093947683,
-0.785362334588819));
#85884=CARTESIAN_POINT('Ctrl Pts',(0.290449462114917,0.191669927513295,
-0.769508014189834));
#85885=CARTESIAN_POINT('Ctrl Pts',(-0.00301667892052102,0.347978664294359,
-0.753653693790849));
#85886=CARTESIAN_POINT('Ctrl Pts',(-0.293728789052321,0.186605599159438,
-0.737799373391864));
#85887=CARTESIAN_POINT('Ctrl Pts',(-0.316285691536655,-0.145126195033759,
-0.721945052992879));
#85888=CARTESIAN_POINT('Ctrl Pts',(-0.0500944070844066,-0.344367248057443,
-0.706090732593894));
#85889=CARTESIAN_POINT('Ctrl Pts',(0.261829800507703,-0.22922348640986,
-0.690236412194909));
#85890=CARTESIAN_POINT('Ctrl Pts',(0.334720494395002,0.0951863529491743,
-0.674382091795923));
#85891=CARTESIAN_POINT('Ctrl Pts',(0.102033229894396,0.332697266524855,
-0.658527771396939));
#85892=CARTESIAN_POINT('Ctrl Pts',(-0.223803712026459,0.266477296667027,
-0.642673450997953));
#85893=CARTESIAN_POINT('Ctrl Pts',(-0.345322476405579,-0.0430190474666505,
-0.626819130598969));
#85894=CARTESIAN_POINT('Ctrl Pts',(-0.151584364995733,-0.313241809860391,
-0.610964810199983));
#85895=CARTESIAN_POINT('Ctrl Pts',(0.180540375122247,-0.297495250561208,
-0.595110489800998));
#85896=CARTESIAN_POINT('Ctrl Pts',(0.347843539746289,-0.0101549501589795,
-0.579256169402013));
#85897=CARTESIAN_POINT('Ctrl Pts',(0.197588262343984,0.286456156749127,
-0.563401849003027));
#85898=CARTESIAN_POINT('Ctrl Pts',(-0.133052198574159,0.321551494492247,
-0.547547528604043));
#85899=CARTESIAN_POINT('Ctrl Pts',(-0.342224688814901,0.0630913109900864,
-0.531693208205058));
#85900=CARTESIAN_POINT('Ctrl Pts',(-0.238968381085131,-0.252967120384663,
-0.515838887806072));
#85901=CARTESIAN_POINT('Ctrl Pts',(0.0824504569657546,-0.338083086387494,
-0.499984567407088));
#85902=CARTESIAN_POINT('Ctrl Pts',(0.328597410795141,-0.114551267045994,
-0.484130247008102));
#85903=CARTESIAN_POINT('Ctrl Pts',(0.274756381763336,0.213558380362958,
-0.468275926609118));
#85904=CARTESIAN_POINT('Ctrl Pts',(-0.0299192856409278,0.346703169155593,
-0.452421606210132));
#85905=CARTESIAN_POINT('Ctrl Pts',(-0.30728059875184,0.163330599807569,
-0.436567285811148));
#85906=CARTESIAN_POINT('Ctrl Pts',(-0.304114786438363,-0.169152143727808,
-0.420712965412162));
#85907=CARTESIAN_POINT('Ctrl Pts',(-0.0233120294769848,-0.347210023571681,
-0.404858645013177));
#85908=CARTESIAN_POINT('Ctrl Pts',(0.278773089448442,-0.208287820207959,
-0.389004324614192));
#85909=CARTESIAN_POINT('Ctrl Pts',(0.326356576077487,0.120787564287852,
-0.373150004215206));
#85910=CARTESIAN_POINT('Ctrl Pts',(0.0759978194502111,0.339591788806732,
-0.357295683816222));
#85911=CARTESIAN_POINT('Ctrl Pts',(-0.243741991839324,0.248370880552563,
-0.341441363417237));
#85912=CARTESIAN_POINT('Ctrl Pts',(-0.340961264081266,-0.0695964249972271,
-0.325587043018251));
#85913=CARTESIAN_POINT('Ctrl Pts',(-0.126905188939026,-0.324026740554483,
-0.309732722619267));
#85914=CARTESIAN_POINT('Ctrl Pts',(0.203007088642323,-0.282641792479861,
-0.293878402220281));
#85915=CARTESIAN_POINT('Ctrl Pts',(0.34758705207047,0.0167766509282329,
-0.278024081821296));
#85916=CARTESIAN_POINT('Ctrl Pts',(0.174842913459877,0.300879123171855,
-0.262169761422311));
#85917=CARTESIAN_POINT('Ctrl Pts',(-0.157521740789639,0.310298569287209,
-0.246315441023326));
#85918=CARTESIAN_POINT('Ctrl Pts',(-0.346078659673261,0.0364357380205341,
-0.230461120624341));
#85919=CARTESIAN_POINT('Ctrl Pts',(-0.218689637670251,-0.270690653779669,
-0.214606800225356));
#85920=CARTESIAN_POINT('Ctrl Pts',(0.108351193813394,-0.330693940132053,
-0.198752479826371));
#85921=CARTESIAN_POINT('Ctrl Pts',(0.336469780852948,-0.0887956529090298,
-0.182898159427386));
#85922=CARTESIAN_POINT('Ctrl Pts',(0.257422366521119,0.23416803964345,-0.1670438390284));
#85923=CARTESIAN_POINT('Ctrl Pts',(-0.0566519505980647,0.343350125828982,
-0.151189518629416));
#85924=CARTESIAN_POINT('Ctrl Pts',(-0.318974075534328,0.139078781230093,
-0.13533519823043));
#85925=CARTESIAN_POINT('Ctrl Pts',(-0.290156119492426,-0.192167794938009,
-0.119480877831445));
#85926=CARTESIAN_POINT('Ctrl Pts',(0.00367478997105658,-0.347967436446841,
-0.10362655743246));
#85927=CARTESIAN_POINT('Ctrl Pts',(0.29392225292049,-0.1861151230156,-0.0877722370334754));
#85928=CARTESIAN_POINT('Ctrl Pts',(0.316279104812747,0.145685085984127,
-0.0719179166344901));
#85929=CARTESIAN_POINT('Ctrl Pts',(0.0490122977774616,0.344418191703448,
-0.0560635962355054));
#85930=CARTESIAN_POINT('Ctrl Pts',(-0.157657690967761,0.267353546877372,
-0.0454940493028484));
#85931=CARTESIAN_POINT('Ctrl Pts',(-0.221960000566811,0.193651260363756,
-0.04020927583652));
#85932=CARTESIAN_POINT('Ctrl Pts',(0.159724862551269,-0.224219327154077,
-1.58281527225733));
#85933=CARTESIAN_POINT('Ctrl Pts',(0.234216290855694,-0.171158894795468,
-1.57752792355557));
#85934=CARTESIAN_POINT('Ctrl Pts',(0.324849943382959,0.0140708249774791,
-1.56695580138749));
#85935=CARTESIAN_POINT('Ctrl Pts',(0.164403620240946,0.280860397746711,
-1.55109890575308));
#85936=CARTESIAN_POINT('Ctrl Pts',(-0.146248475293588,0.290385604902334,
-1.5352445853541));
#85937=CARTESIAN_POINT('Ctrl Pts',(-0.323310585957363,0.0352147156308222,
-1.51939026495511));
#85938=CARTESIAN_POINT('Ctrl Pts',(-0.205250356133029,-0.252315744274402,
-1.50353594455613));
#85939=CARTESIAN_POINT('Ctrl Pts',(0.100210520733791,-0.309388325184188,
-1.48768162415714));
#85940=CARTESIAN_POINT('Ctrl Pts',(0.314175022289166,-0.0840671341663506,
-1.47182730375816));
#85941=CARTESIAN_POINT('Ctrl Pts',(0.241323845305763,0.218031981537731,
-1.45597298335917));
#85942=CARTESIAN_POINT('Ctrl Pts',(-0.051843179909363,0.321066373377227,
-1.44011866296019));
#85943=CARTESIAN_POINT('Ctrl Pts',(-0.297679231989491,0.130996373777726,
-1.4242643425612));
#85944=CARTESIAN_POINT('Ctrl Pts',(-0.271754382884308,-0.178669077247151,
-1.40841002216222));
#85945=CARTESIAN_POINT('Ctrl Pts',(0.00226489582050245,-0.325219068021424,
-1.39255570176323));
#85946=CARTESIAN_POINT('Ctrl Pts',(0.274216252679952,-0.174866463597575,
-1.37670138136425));
#85947=CARTESIAN_POINT('Ctrl Pts',(0.295826188702755,0.135128423599089,
-1.36084706096526));
#85948=CARTESIAN_POINT('Ctrl Pts',(0.0473660679461038,0.321759558822918,
-1.34499274056628));
#85949=CARTESIAN_POINT('Ctrl Pts',(-0.244336148952099,0.214645392864761,
-1.32913842016729));
#85950=CARTESIAN_POINT('Ctrl Pts',(-0.312975430379855,-0.0884260917010995,
-1.3132840997683));
#85951=CARTESIAN_POINT('Ctrl Pts',(-0.0958885685676773,-0.310770281317141,
-1.29742977936932));
#85952=CARTESIAN_POINT('Ctrl Pts',(0.208738291530677,-0.249401517680771,
-1.28157545897033));
#85953=CARTESIAN_POINT('Ctrl Pts',(0.322800721779757,0.0396545615316289,
-1.26572113857135));
#85954=CARTESIAN_POINT('Ctrl Pts',(0.142167166593946,0.292508608368234,
-1.24986681817236));
#85955=CARTESIAN_POINT('Ctrl Pts',(-0.168255729336558,0.278321396332049,
-1.23401249777338));
#85956=CARTESIAN_POINT('Ctrl Pts',(-0.325072129681891,0.0100449184781619,
-1.21815817737439));
#85957=CARTESIAN_POINT('Ctrl Pts',(-0.185118898529878,-0.267401913190092,
-1.20230385697541));
#85958=CARTESIAN_POINT('Ctrl Pts',(0.123835800975708,-0.300728256560079,
-1.18644953657643));
#85959=CARTESIAN_POINT('Ctrl Pts',(0.319736499143041,-0.0595093351640252,
-1.17059521617744));
#85960=CARTESIAN_POINT('Ctrl Pts',(0.223738648297707,0.236037723897242,
-1.15474089577845));
#85961=CARTESIAN_POINT('Ctrl Pts',(-0.0765179811396485,0.316097751375452,
-1.13888657537947));
#85962=CARTESIAN_POINT('Ctrl Pts',(-0.306918689455241,0.107581168976872,
-1.12303225498049));
#85963=CARTESIAN_POINT('Ctrl Pts',(-0.257122672184753,-0.199149996994861,
-1.1071779345815));
#85964=CARTESIAN_POINT('Ctrl Pts',(0.0274095579454656,-0.324070217684555,
-1.09132361418251));
#85965=CARTESIAN_POINT('Ctrl Pts',(0.28691865116829,-0.153135487289929,
-1.07546929378353));
#85966=CARTESIAN_POINT('Ctrl Pts',(0.284489748015783,0.15760194519629,-1.05961497338455));
#85967=CARTESIAN_POINT('Ctrl Pts',(0.0223402784904676,0.324459091124019,
-1.04376065298556));
#85968=CARTESIAN_POINT('Ctrl Pts',(-0.260204406760496,0.195106269910267,
-1.02790633258657));
#85969=CARTESIAN_POINT('Ctrl Pts',(-0.305199456680208,-0.112365837771089,
-1.01205201218759));
#85970=CARTESIAN_POINT('Ctrl Pts',(-0.0715673282970608,-0.317255271628942,
-0.996197691788603));
#85971=CARTESIAN_POINT('Ctrl Pts',(0.227401098384244,-0.232511355227108,
-0.980343371389616));
#85972=CARTESIAN_POINT('Ctrl Pts',(0.318767168642697,0.0645002484602125,
-0.964489050990633));
#85973=CARTESIAN_POINT('Ctrl Pts',(0.119119625375682,0.302627336349962,
-0.948634730591646));
#85974=CARTESIAN_POINT('Ctrl Pts',(-0.189276358861536,0.26447542387154,
-0.932780410192662));
#85975=CARTESIAN_POINT('Ctrl Pts',(-0.324875384799132,-0.015125283717291,
-0.916926089793677));
#85976=CARTESIAN_POINT('Ctrl Pts',(-0.163884394649323,-0.280917594761059,
-0.901071769394691));
#85977=CARTESIAN_POINT('Ctrl Pts',(0.146722348246946,-0.290250482137093,
-0.885217448995707));
#85978=CARTESIAN_POINT('Ctrl Pts',(0.323381166298586,-0.0346036289900233,
-0.869363128596721));
#85979=CARTESIAN_POINT('Ctrl Pts',(0.204814092200339,0.252634078247699,
-0.853508808197737));
#85980=CARTESIAN_POINT('Ctrl Pts',(-0.100734876319318,0.309233365840177,
-0.837654487798751));
#85981=CARTESIAN_POINT('Ctrl Pts',(-0.31431947946675,0.083522779429712,
-0.821800167399766));
#85982=CARTESIAN_POINT('Ctrl Pts',(-0.240950918928764,-0.218438651623968,
-0.805945847000781));
#85983=CARTESIAN_POINT('Ctrl Pts',(0.0523900995581144,-0.320979855013057,
-0.790091526601796));
#85984=CARTESIAN_POINT('Ctrl Pts',(0.297902377556176,-0.130487406680836,
-0.774237206202811));
#85985=CARTESIAN_POINT('Ctrl Pts',(0.271449234085044,0.17913152478153,-0.758382885803825));
#85986=CARTESIAN_POINT('Ctrl Pts',(-0.0028193379202488,0.325215069130574,
-0.742528565404841));
#85987=CARTESIAN_POINT('Ctrl Pts',(-0.274514038471294,0.174398487774677,
-0.726674245005856));
#85988=CARTESIAN_POINT('Ctrl Pts',(-0.295595344176312,-0.135632526914457,
-0.710819924606871));
#85989=CARTESIAN_POINT('Ctrl Pts',(-0.0468173992679871,-0.321839899611118,
-0.694965604207886));
#85990=CARTESIAN_POINT('Ctrl Pts',(0.244701774590776,-0.214228456018421,
-0.6791112838089));
#85991=CARTESIAN_POINT('Ctrl Pts',(0.312824204164448,0.0889595815232725,
-0.663256963409916));
#85992=CARTESIAN_POINT('Ctrl Pts',(0.0953585587812114,0.310933329064417,
-0.64740264301093));
#85993=CARTESIAN_POINT('Ctrl Pts',(-0.209163225067142,0.249045247164886,
-0.631548322611945));
#85994=CARTESIAN_POINT('Ctrl Pts',(-0.322732640129862,-0.04020488590635,
-0.615694002212961));
#85995=CARTESIAN_POINT('Ctrl Pts',(-0.14166822509411,-0.292750583013215,
-0.599839681813975));
#85996=CARTESIAN_POINT('Ctrl Pts',(0.168730030317533,-0.278034110721911,
-0.58398536141499));
#85997=CARTESIAN_POINT('Ctrl Pts',(0.325088783976481,-0.0094906474357171,
-0.568131041016005));
#85998=CARTESIAN_POINT('Ctrl Pts',(0.18466270203058,0.267717157340548,-0.55227672061702));
#85999=CARTESIAN_POINT('Ctrl Pts',(-0.124348370739959,0.300516675993317,
-0.536422400218035));
#86000=CARTESIAN_POINT('Ctrl Pts',(-0.319837499396171,0.0589640893840041,
-0.520568079819049));
#86001=CARTESIAN_POINT('Ctrl Pts',(-0.223335872422572,-0.236418861226701,
-0.504713759420064));
#86002=CARTESIAN_POINT('Ctrl Pts',(0.077056825068113,-0.315966826685613,
-0.488859439021079));
#86003=CARTESIAN_POINT('Ctrl Pts',(0.307101672122839,-0.107057707997419,
-0.473005118622095));
#86004=CARTESIAN_POINT('Ctrl Pts',(0.256782742328259,0.199588108581286,
-0.457150798223109));
#86005=CARTESIAN_POINT('Ctrl Pts',(-0.0279620664898624,0.324023012598688,
-0.441296477824125));
#86006=CARTESIAN_POINT('Ctrl Pts',(-0.287179334308354,0.152646060686708,
-0.425442157425139));
#86007=CARTESIAN_POINT('Ctrl Pts',(-0.284220618800695,-0.158086778761499,
-0.409587837026154));
#86008=CARTESIAN_POINT('Ctrl Pts',(-0.0217870348267034,-0.324496710301681,
-0.393733516627169));
#86009=CARTESIAN_POINT('Ctrl Pts',(0.260536690490967,-0.194662330764873,
-0.377879196228184));
#86010=CARTESIAN_POINT('Ctrl Pts',(0.305007425284199,0.112886047624917,
-0.362024875829198));
#86011=CARTESIAN_POINT('Ctrl Pts',(0.0710262974208254,0.317376834861157,
-0.346170555430214));
#86012=CARTESIAN_POINT('Ctrl Pts',(-0.227797209598448,0.232123291963083,
-0.330316235031228));
#86013=CARTESIAN_POINT('Ctrl Pts',(-0.318656723664062,-0.0650436606871058,
-0.314461914632243));
#86014=CARTESIAN_POINT('Ctrl Pts',(-0.11860347782392,-0.302829999773896,
-0.298607594233258));
#86015=CARTESIAN_POINT('Ctrl Pts',(0.189727046917343,-0.264152315967197,
-0.282753273834273));
#86016=CARTESIAN_POINT('Ctrl Pts',(0.324849074862728,0.0156791787866342,
-0.266898953435288));
#86017=CARTESIAN_POINT('Ctrl Pts',(0.163405277456162,0.281196621754686,
-0.251044633036303));
#86018=CARTESIAN_POINT('Ctrl Pts',(-0.147217197710538,0.289999879350344,
-0.235190312637318));
#86019=CARTESIAN_POINT('Ctrl Pts',(-0.323439356428613,0.0340522344471882,
-0.219335992238333));
#86020=CARTESIAN_POINT('Ctrl Pts',(-0.204383696274287,-0.252982980610236,
-0.203481671839348));
#86021=CARTESIAN_POINT('Ctrl Pts',(0.101263222726195,-0.30906105355394,
-0.187627351440363));
#86022=CARTESIAN_POINT('Ctrl Pts',(0.314459058179145,-0.0829869396098267,
-0.171773031041377));
#86023=CARTESIAN_POINT('Ctrl Pts',(0.240582660128564,0.218849553190984,
-0.155918710642392));
#86024=CARTESIAN_POINT('Ctrl Pts',(-0.0529459703154303,0.320889314101761,
-0.140064390243407));
#86025=CARTESIAN_POINT('Ctrl Pts',(-0.298107863124639,0.12998071460519,
-0.124210069844422));
#86026=CARTESIAN_POINT('Ctrl Pts',(-0.271175080951416,-0.179596823391934,
-0.108355749445437));
#86027=CARTESIAN_POINT('Ctrl Pts',(0.00343439755682056,-0.32520457577112,
-0.0925014290464522));
#86028=CARTESIAN_POINT('Ctrl Pts',(0.27469484658316,-0.173940096932386,
-0.0766471086474671));
#86029=CARTESIAN_POINT('Ctrl Pts',(0.295589188333754,0.136154857096479,
-0.0607927882484822));
#86030=CARTESIAN_POINT('Ctrl Pts',(0.0458060779164938,0.321887510694949,
-0.044938467849497));
#86031=CARTESIAN_POINT('Ctrl Pts',(-0.147344254484739,0.249864176030283,
-0.0343689209168401));
#86032=CARTESIAN_POINT('Ctrl Pts',(-0.207440123017129,0.180983245493314,
-0.0290841474505119));
#86033=CARTESIAN_POINT('Ctrl Pts',(0.148544839071951,-0.208524980625557,
-1.57169014387133));
#86034=CARTESIAN_POINT('Ctrl Pts',(0.21782220173782,-0.159178540378863,
-1.56640279516957));
#86035=CARTESIAN_POINT('Ctrl Pts',(0.3021119053827,0.0130859303836847,-1.55583067300148));
#86036=CARTESIAN_POINT('Ctrl Pts',(0.152896104723196,0.261201430501014,
-1.53997377736707));
#86037=CARTESIAN_POINT('Ctrl Pts',(-0.136011738435718,0.270059915908096,
-1.52411945696809));
#86038=CARTESIAN_POINT('Ctrl Pts',(-0.300680296067738,0.0327498435922312,
-1.5082651365691));
#86039=CARTESIAN_POINT('Ctrl Pts',(-0.190883752436815,-0.234654774653695,
-1.49241081617012));
#86040=CARTESIAN_POINT('Ctrl Pts',(0.0931962340611783,-0.287732531060864,
-1.47655649577114));
#86041=CARTESIAN_POINT('Ctrl Pts',(0.292184180852812,-0.0781828120964695,
-1.46070217537215));
#86042=CARTESIAN_POINT('Ctrl Pts',(0.224432259277494,0.202770721431455,
-1.44484785497317));
#86043=CARTESIAN_POINT('Ctrl Pts',(-0.0482143900054565,0.298593168295426,
-1.42899353457418));
#86044=CARTESIAN_POINT('Ctrl Pts',(-0.276843021835421,0.121827215569368,
-1.4131392141752));
#86045=CARTESIAN_POINT('Ctrl Pts',(-0.252732795808098,-0.166163043767173,
-1.39728489377621));
#86046=CARTESIAN_POINT('Ctrl Pts',(0.00210636327868856,-0.302455192953229,
-1.38143057337722));
#86047=CARTESIAN_POINT('Ctrl Pts',(0.255022345767755,-0.162626596005646,
-1.36557625297824));
#86048=CARTESIAN_POINT('Ctrl Pts',(0.27511968326167,0.125670040449278,-1.34972193257925));
#86049=CARTESIAN_POINT('Ctrl Pts',(0.0440506557848269,0.299237833871169,
-1.33386761218027));
#86050=CARTESIAN_POINT('Ctrl Pts',(-0.227233715188827,0.199621178765434,
-1.31801329178129));
#86051=CARTESIAN_POINT('Ctrl Pts',(-0.291068554992977,-0.0822366621682676,
-1.3021589713823));
#86052=CARTESIAN_POINT('Ctrl Pts',(-0.0891767991483039,-0.289017756467199,
-1.28630465098332));
#86053=CARTESIAN_POINT('Ctrl Pts',(0.194127548011667,-0.231944530841581,
-1.27045033058433));
#86054=CARTESIAN_POINT('Ctrl Pts',(0.300206120094121,0.0368789202075171,
-1.25459601018535));
#86055=CARTESIAN_POINT('Ctrl Pts',(0.132216103026753,0.272034318660143,
-1.23874168978636));
#86056=CARTESIAN_POINT('Ctrl Pts',(-0.15647858347169,0.258840147789478,
-1.22288736938738));
#86057=CARTESIAN_POINT('Ctrl Pts',(-0.302318539637954,0.00934181926968402,
-1.20703304898839));
#86058=CARTESIAN_POINT('Ctrl Pts',(-0.172161406509086,-0.248684979457122,
-1.19117872858941));
#86059=CARTESIAN_POINT('Ctrl Pts',(0.115167850724418,-0.279678628371122,
-1.17532440819042));
#86060=CARTESIAN_POINT('Ctrl Pts',(0.297356379288707,-0.0553439488005891,
-1.15947008779143));
#86061=CARTESIAN_POINT('Ctrl Pts',(0.208077947131682,0.21951614264167,-1.14361576739245));
#86062=CARTESIAN_POINT('Ctrl Pts',(-0.0711620658984849,0.293972327532916,
-1.12776144699346));
#86063=CARTESIAN_POINT('Ctrl Pts',(-0.285435758748384,0.100050970009206,
-1.11190712659448));
#86064=CARTESIAN_POINT('Ctrl Pts',(-0.23912523918544,-0.185210391057845,
-1.0960528061955));
#86065=CARTESIAN_POINT('Ctrl Pts',(0.0254910119126622,-0.301386756983511,
-1.08019848579651));
#86066=CARTESIAN_POINT('Ctrl Pts',(0.266835633374574,-0.142416690503555,
-1.06434416539752));
#86067=CARTESIAN_POINT('Ctrl Pts',(0.264576742541001,0.146570516403449,
-1.04848984499854));
#86068=CARTESIAN_POINT('Ctrl Pts',(0.0207765592668679,0.301748411027608,
-1.03263552459955));
#86069=CARTESIAN_POINT('Ctrl Pts',(-0.241991266172751,0.181449706719554,
-1.01678120420057));
#86070=CARTESIAN_POINT('Ctrl Pts',(-0.283836864551102,-0.104500733463044,
-1.00092688380158));
#86071=CARTESIAN_POINT('Ctrl Pts',(-0.0665579365346684,-0.295048826564006,
-0.985072563402594));
#86072=CARTESIAN_POINT('Ctrl Pts',(0.211484042150481,-0.216236603950906,
-0.969218243003609));
#86073=CARTESIAN_POINT('Ctrl Pts',(0.296454897572703,0.0599855205669558,
-0.953363922604623));
#86074=CARTESIAN_POINT('Ctrl Pts',(0.110781786248597,0.281444781099428,
-0.93750960220564));
#86075=CARTESIAN_POINT('Ctrl Pts',(-0.176027863277623,0.245963331255792,
-0.921655281806653));
#86076=CARTESIAN_POINT('Ctrl Pts',(-0.30213556601393,-0.014066581744478,
-0.905800961407669));
#86077=CARTESIAN_POINT('Ctrl Pts',(-0.152413222592527,-0.261254623981076,
-0.889946641008684));
#86078=CARTESIAN_POINT('Ctrl Pts',(0.136452442409244,-0.269934251129945,
-0.874092320609698));
#86079=CARTESIAN_POINT('Ctrl Pts',(0.300745936101864,-0.0321815302735241,
-0.858238000210714));
#86080=CARTESIAN_POINT('Ctrl Pts',(0.190478025021315,0.234950826677652,
-0.842383679811728));
#86081=CARTESIAN_POINT('Ctrl Pts',(-0.0936838871092037,0.287588418175423,
-0.826529359412743));
#86082=CARTESIAN_POINT('Ctrl Pts',(-0.292318526676337,0.0776765597481471,
-0.810675039013758));
#86083=CARTESIAN_POINT('Ctrl Pts',(-0.224085436073065,-0.203148926436928,
-0.794820718614773));
#86084=CARTESIAN_POINT('Ctrl Pts',(0.0487230277335556,-0.298512705828424,
-0.778966398215788));
#86085=CARTESIAN_POINT('Ctrl Pts',(0.277050548213993,-0.121353873884843,
-0.763112077816803));
#86086=CARTESIAN_POINT('Ctrl Pts',(0.252449006055172,0.166593122049766,
-0.747257757417818));
#86087=CARTESIAN_POINT('Ctrl Pts',(-0.00262199691997647,0.30245147396679,
-0.731403437018833));
#86088=CARTESIAN_POINT('Ctrl Pts',(-0.255299287890265,0.162191376389917,
-0.715549116619847));
#86089=CARTESIAN_POINT('Ctrl Pts',(-0.27490499681597,-0.126138858795157,
-0.699694796220863));
#86090=CARTESIAN_POINT('Ctrl Pts',(-0.0435403914515674,-0.299312551164792,
-0.683840475821877));
#86091=CARTESIAN_POINT('Ctrl Pts',(0.227573748673849,-0.199233425626985,
-0.667986155422893));
#86092=CARTESIAN_POINT('Ctrl Pts',(0.290927913933894,0.0827328100973711,
-0.652131835023907));
#86093=CARTESIAN_POINT('Ctrl Pts',(0.0886838876680271,0.289169391603979,
-0.636277514624922));
#86094=CARTESIAN_POINT('Ctrl Pts',(-0.194522738107825,0.231613197662744,
-0.620423194225936));
#86095=CARTESIAN_POINT('Ctrl Pts',(-0.300142803854146,-0.0373907243460496,
-0.604568873826953));
#86096=CARTESIAN_POINT('Ctrl Pts',(-0.131752085192487,-0.27225935616604,
-0.588714553427966));
#86097=CARTESIAN_POINT('Ctrl Pts',(0.15691968551282,-0.258572970882614,
-0.572860233028982));
#86098=CARTESIAN_POINT('Ctrl Pts',(0.302334028206672,-0.00882634471245425,
-0.557005912629997));
#86099=CARTESIAN_POINT('Ctrl Pts',(0.171737141717175,0.248978157931968,
-0.541151592231012));
#86100=CARTESIAN_POINT('Ctrl Pts',(-0.115644542905758,0.279481857494389,
-0.525297271832026));
#86101=CARTESIAN_POINT('Ctrl Pts',(-0.29745030997744,0.0548368677779214,
-0.509442951433041));
#86102=CARTESIAN_POINT('Ctrl Pts',(-0.207703363760013,-0.219870602068739,
-0.493588631034056));
#86103=CARTESIAN_POINT('Ctrl Pts',(0.0716631931704711,-0.293850566983732,
-0.477734310635071));
#86104=CARTESIAN_POINT('Ctrl Pts',(0.285605933450537,-0.0995641489488433,
-0.461879990236086));
#86105=CARTESIAN_POINT('Ctrl Pts',(0.238809102893179,0.185617836799614,
-0.446025669837101));
#86106=CARTESIAN_POINT('Ctrl Pts',(-0.0260048473387968,0.301342856041782,
-0.430171349438115));
#86107=CARTESIAN_POINT('Ctrl Pts',(-0.267078069864868,0.141961521565846,
-0.414317029039131));
#86108=CARTESIAN_POINT('Ctrl Pts',(-0.264326451163026,-0.147021413795191,
-0.398462708640145));
#86109=CARTESIAN_POINT('Ctrl Pts',(-0.0202620401764223,-0.301783397031682,
-0.382608388241161));
#86110=CARTESIAN_POINT('Ctrl Pts',(0.242300291533491,-0.181036841321789,
-0.366754067842175));
#86111=CARTESIAN_POINT('Ctrl Pts',(0.283658274490912,0.104984530961983,
-0.350899747443191));
#86112=CARTESIAN_POINT('Ctrl Pts',(0.0660547753914399,0.295161880915583,
-0.335045427044205));
#86113=CARTESIAN_POINT('Ctrl Pts',(-0.211852427357573,0.215875703373602,
-0.319191106645221));
#86114=CARTESIAN_POINT('Ctrl Pts',(-0.296352183246857,-0.0604908963769847,
-0.303336786246235));
#86115=CARTESIAN_POINT('Ctrl Pts',(-0.110301766708814,-0.281633258993308,
-0.28748246584725));
#86116=CARTESIAN_POINT('Ctrl Pts',(0.176447005192364,-0.245662839454535,
-0.271628145448265));
#86117=CARTESIAN_POINT('Ctrl Pts',(0.302111097654986,0.0145817066450353,
-0.25577382504928));
#86118=CARTESIAN_POINT('Ctrl Pts',(0.151967641452447,0.261514120337517,
-0.239919504650295));
#86119=CARTESIAN_POINT('Ctrl Pts',(-0.136912654631436,0.269701189413478,
-0.22406518425131));
#86120=CARTESIAN_POINT('Ctrl Pts',(-0.300800053183967,0.0316687308738422,
-0.208210863852325));
#86121=CARTESIAN_POINT('Ctrl Pts',(-0.190077754878324,-0.235275307440804,
-0.192356543453339));
#86122=CARTESIAN_POINT('Ctrl Pts',(0.0941752516389973,-0.287428166975827,
-0.176502223054355));
#86123=CARTESIAN_POINT('Ctrl Pts',(0.292448335505342,-0.0771782263106231,
-0.160647902655369));
#86124=CARTESIAN_POINT('Ctrl Pts',(0.223742953736009,0.203531066738519,
-0.144793582256384));
#86125=CARTESIAN_POINT('Ctrl Pts',(-0.0492399900327958,0.298428502374539,
-0.128939261857399));
#86126=CARTESIAN_POINT('Ctrl Pts',(-0.277241650714951,0.120882647980286,
-0.113084941458414));
#86127=CARTESIAN_POINT('Ctrl Pts',(-0.252194042410405,-0.167025851845859,
-0.0972306210594291));
#86128=CARTESIAN_POINT('Ctrl Pts',(0.00319400514258442,-0.3024417150954,
-0.081376300660444));
#86129=CARTESIAN_POINT('Ctrl Pts',(0.255467440245829,-0.161765070849173,
-0.0655219802614589));
#86130=CARTESIAN_POINT('Ctrl Pts',(0.274899271854761,0.126624628208832,
-0.0496676598624738));
#86131=CARTESIAN_POINT('Ctrl Pts',(0.0425998580555258,0.299356829686449,
-0.0338133394634889));
#86132=CARTESIAN_POINT('Ctrl Pts',(-0.137030818001717,0.232374805183194,
-0.023243792530832));
#86133=CARTESIAN_POINT('Ctrl Pts',(-0.192920245467447,0.168315230622872,
-0.0179590190645036));
#86134=CARTESIAN_POINT('Ctrl Pts',(0.137364815592633,-0.192830634097036,
-1.56056501548531));
#86135=CARTESIAN_POINT('Ctrl Pts',(0.201428112619947,-0.147198185962257,
-1.55527766678356));
#86136=CARTESIAN_POINT('Ctrl Pts',(0.27937386738244,0.0121010357898901,
-1.54470554461548));
#86137=CARTESIAN_POINT('Ctrl Pts',(0.141388589205448,0.241542463255316,
-1.52884864898106));
#86138=CARTESIAN_POINT('Ctrl Pts',(-0.125775001577849,0.249734226913857,
-1.51299432858207));
#86139=CARTESIAN_POINT('Ctrl Pts',(-0.278050006178113,0.0302849715536401,
-1.49714000818309));
#86140=CARTESIAN_POINT('Ctrl Pts',(-0.176517148740603,-0.216993805032989,
-1.48128568778411));
#86141=CARTESIAN_POINT('Ctrl Pts',(0.0861819473885653,-0.266076736937539,
-1.46543136738512));
#86142=CARTESIAN_POINT('Ctrl Pts',(0.270193339416458,-0.0722984900265885,
-1.44957704698614));
#86143=CARTESIAN_POINT('Ctrl Pts',(0.207540673249225,0.18750946132518,-1.43372272658715));
#86144=CARTESIAN_POINT('Ctrl Pts',(-0.0445856001015495,0.276119963213624,
-1.41786840618817));
#86145=CARTESIAN_POINT('Ctrl Pts',(-0.256006811681353,0.112658057361009,
-1.40201408578918));
#86146=CARTESIAN_POINT('Ctrl Pts',(-0.233711208731888,-0.153657010287193,
-1.3861597653902));
#86147=CARTESIAN_POINT('Ctrl Pts',(0.00194783073687467,-0.279691317885033,
-1.37030544499121));
#86148=CARTESIAN_POINT('Ctrl Pts',(0.235828438855558,-0.150386728413716,
-1.35445112459222));
#86149=CARTESIAN_POINT('Ctrl Pts',(0.254413177820586,0.116211657299466,
-1.33859680419324));
#86150=CARTESIAN_POINT('Ctrl Pts',(0.0407352436235497,0.276716108919421,
-1.32274248379426));
#86151=CARTESIAN_POINT('Ctrl Pts',(-0.210131281425556,0.184596964666106,
-1.30688816339527));
#86152=CARTESIAN_POINT('Ctrl Pts',(-0.269161679606099,-0.076047232635435,
-1.29103384299628));
#86153=CARTESIAN_POINT('Ctrl Pts',(-0.0824650297289307,-0.267265231617256,
-1.2751795225973));
#86154=CARTESIAN_POINT('Ctrl Pts',(0.179516804492658,-0.214487544002391,
-1.25932520219831));
#86155=CARTESIAN_POINT('Ctrl Pts',(0.277611518408485,0.0341032788834053,
-1.24347088179933));
#86156=CARTESIAN_POINT('Ctrl Pts',(0.122265039459559,0.251560028952052,
-1.22761656140035));
#86157=CARTESIAN_POINT('Ctrl Pts',(-0.144701437606821,0.239358899246907,
-1.21176224100136));
#86158=CARTESIAN_POINT('Ctrl Pts',(-0.279564949594017,0.00863872006120638,
-1.19590792060237));
#86159=CARTESIAN_POINT('Ctrl Pts',(-0.159203914488296,-0.229968045724152,
-1.18005360020339));
#86160=CARTESIAN_POINT('Ctrl Pts',(0.106499900473129,-0.258629000182165,
-1.1641992798044));
#86161=CARTESIAN_POINT('Ctrl Pts',(0.274976259434374,-0.0511785624371529,
-1.14834495940542));
#86162=CARTESIAN_POINT('Ctrl Pts',(0.192417245965658,0.202994561386096,
-1.13249063900643));
#86163=CARTESIAN_POINT('Ctrl Pts',(-0.0658061506573216,0.271846903690381,
-1.11663631860745));
#86164=CARTESIAN_POINT('Ctrl Pts',(-0.263952828041526,0.0925207710415389,
-1.10078199820846));
#86165=CARTESIAN_POINT('Ctrl Pts',(-0.221127806186127,-0.17127078512083,
-1.08492767780948));
#86166=CARTESIAN_POINT('Ctrl Pts',(0.0235724658798592,-0.278703296282466,
-1.06907335741049));
#86167=CARTESIAN_POINT('Ctrl Pts',(0.246752615580859,-0.13169789371718,
-1.05321903701151));
#86168=CARTESIAN_POINT('Ctrl Pts',(0.24466373706622,0.135539087610608,-1.03736471661252));
#86169=CARTESIAN_POINT('Ctrl Pts',(0.0192128400432681,0.279037730931197,
-1.02151039621354));
#86170=CARTESIAN_POINT('Ctrl Pts',(-0.223778125585007,0.167793143528841,
-1.00565607581455));
#86171=CARTESIAN_POINT('Ctrl Pts',(-0.262474272421997,-0.096635629154999,
-0.98980175541557));
#86172=CARTESIAN_POINT('Ctrl Pts',(-0.0615485447722762,-0.27284238149907,
-0.973947435016587));
#86173=CARTESIAN_POINT('Ctrl Pts',(0.195566985916719,-0.199961852674703,
-0.9580931146176));
#86174=CARTESIAN_POINT('Ctrl Pts',(0.274142626502709,0.0554707926736992,
-0.942238794218616));
#86175=CARTESIAN_POINT('Ctrl Pts',(0.102443947121514,0.260262225848894,
-0.926384473819631));
#86176=CARTESIAN_POINT('Ctrl Pts',(-0.162779367693708,0.227451238640043,
-0.910530153420645));
#86177=CARTESIAN_POINT('Ctrl Pts',(-0.279395747228729,-0.0130078797716646,
-0.894675833021661));
#86178=CARTESIAN_POINT('Ctrl Pts',(-0.14094205053573,-0.241591653201093,
-0.878821512622675));
#86179=CARTESIAN_POINT('Ctrl Pts',(0.126182536571542,-0.249618020122797,
-0.86296719222369));
#86180=CARTESIAN_POINT('Ctrl Pts',(0.278110705905143,-0.0297594315570249,
-0.847112871824706));
#86181=CARTESIAN_POINT('Ctrl Pts',(0.17614195784229,0.217267575107605,-0.83125855142572));
#86182=CARTESIAN_POINT('Ctrl Pts',(-0.0866328978990892,0.26594347051067,
-0.815404231026735));
#86183=CARTESIAN_POINT('Ctrl Pts',(-0.270317573885926,0.071830340066582,
-0.79954991062775));
#86184=CARTESIAN_POINT('Ctrl Pts',(-0.207219953217366,-0.187859201249889,
-0.783695590228765));
#86185=CARTESIAN_POINT('Ctrl Pts',(0.0450559559089969,-0.27604555664379,
-0.767841269829779));
#86186=CARTESIAN_POINT('Ctrl Pts',(0.256198718871808,-0.112220341088851,
-0.751986949430795));
#86187=CARTESIAN_POINT('Ctrl Pts',(0.233448778025299,0.154054719318002,
-0.736132629031809));
#86188=CARTESIAN_POINT('Ctrl Pts',(-0.00242465591970453,0.279687878803005,
-0.720278308632825));
#86189=CARTESIAN_POINT('Ctrl Pts',(-0.236084537309237,0.149984265005156,
-0.704423988233839));
#86190=CARTESIAN_POINT('Ctrl Pts',(-0.254214649455628,-0.116645190675855,
-0.688569667834855));
#86191=CARTESIAN_POINT('Ctrl Pts',(-0.0402633836351476,-0.276785202718466,
-0.672715347435869));
#86192=CARTESIAN_POINT('Ctrl Pts',(0.210445722756922,-0.184238395235546,
-0.656861027036884));
#86193=CARTESIAN_POINT('Ctrl Pts',(0.26903162370334,0.0765060386714696,
-0.641006706637899));
#86194=CARTESIAN_POINT('Ctrl Pts',(0.082009216554843,0.26740545414354,-0.625152386238914));
#86195=CARTESIAN_POINT('Ctrl Pts',(-0.179882251148508,0.214181148160604,
-0.609298065839929));
#86196=CARTESIAN_POINT('Ctrl Pts',(-0.277552967578429,-0.0345765627857494,
-0.593443745440943));
#86197=CARTESIAN_POINT('Ctrl Pts',(-0.121835945290864,-0.251768129318864,
-0.577589425041959));
#86198=CARTESIAN_POINT('Ctrl Pts',(0.145109340708106,-0.239111831043317,
-0.561735104642973));
#86199=CARTESIAN_POINT('Ctrl Pts',(0.279579272436864,-0.00816204198919175,
-0.545880784243989));
#86200=CARTESIAN_POINT('Ctrl Pts',(0.158811581403771,0.230239158523389,
-0.530026463845003));
#86201=CARTESIAN_POINT('Ctrl Pts',(-0.106940715071558,0.25844703899546,
-0.514172143446019));
#86202=CARTESIAN_POINT('Ctrl Pts',(-0.275063120558711,0.0507096461718393,
-0.498317823047033));
#86203=CARTESIAN_POINT('Ctrl Pts',(-0.192070855097454,-0.203322342910778,
-0.482463502648048));
#86204=CARTESIAN_POINT('Ctrl Pts',(0.0662695612728291,-0.27173430728185,
-0.466609182249063));
#86205=CARTESIAN_POINT('Ctrl Pts',(0.264110194778236,-0.092070589900268,
-0.450754861850078));
#86206=CARTESIAN_POINT('Ctrl Pts',(0.2208354634581,0.171647565017942,-0.434900541451093));
#86207=CARTESIAN_POINT('Ctrl Pts',(-0.0240476281877313,0.278662699484875,
-0.419046221052108));
#86208=CARTESIAN_POINT('Ctrl Pts',(-0.246976805421383,0.131276982444985,
-0.403191900653123));
#86209=CARTESIAN_POINT('Ctrl Pts',(-0.244432283525357,-0.135956048828884,
-0.387337580254138));
#86210=CARTESIAN_POINT('Ctrl Pts',(-0.0187370455261411,-0.279070083761682,
-0.371483259855153));
#86211=CARTESIAN_POINT('Ctrl Pts',(0.224063892576015,-0.167411351878704,
-0.355628939456167));
#86212=CARTESIAN_POINT('Ctrl Pts',(0.262309123697625,0.0970830142990478,
-0.339774619057182));
#86213=CARTESIAN_POINT('Ctrl Pts',(0.0610832533620543,0.272946926970009,
-0.323920298658198));
#86214=CARTESIAN_POINT('Ctrl Pts',(-0.195907645116697,0.199628114784122,
-0.308065978259212));
#86215=CARTESIAN_POINT('Ctrl Pts',(-0.274047642829653,-0.0559381320668637,
-0.292211657860227));
#86216=CARTESIAN_POINT('Ctrl Pts',(-0.102000055593709,-0.260436518212721,
-0.276357337461242));
#86217=CARTESIAN_POINT('Ctrl Pts',(0.163166963467383,-0.227173362941872,
-0.260503017062257));
#86218=CARTESIAN_POINT('Ctrl Pts',(0.279373120447245,0.0134842345034367,
-0.244648696663271));
#86219=CARTESIAN_POINT('Ctrl Pts',(0.140530005448733,0.241831618920349,
-0.228794376264287));
#86220=CARTESIAN_POINT('Ctrl Pts',(-0.126608111552335,0.249402499476613,
-0.212940055865302));
#86221=CARTESIAN_POINT('Ctrl Pts',(-0.278160749939319,0.0292852273004961,
-0.197085735466316));
#86222=CARTESIAN_POINT('Ctrl Pts',(-0.17577181348236,-0.217567634271371,
-0.181231415067331));
#86223=CARTESIAN_POINT('Ctrl Pts',(0.0870872805517992,-0.265795280397715,
-0.165377094668346));
#86224=CARTESIAN_POINT('Ctrl Pts',(0.270437612831538,-0.0713695130114197,
-0.149522774269361));
#86225=CARTESIAN_POINT('Ctrl Pts',(0.206903247343454,0.188212580286055,
-0.133668453870376));
#86226=CARTESIAN_POINT('Ctrl Pts',(-0.0455340097501608,0.275967690647318,
-0.117814133471391));
#86227=CARTESIAN_POINT('Ctrl Pts',(-0.256375438305264,0.111784581355383,
-0.101959813072406));
#86228=CARTESIAN_POINT('Ctrl Pts',(-0.233213003869395,-0.154454880299785,
-0.0861054926734209));
#86229=CARTESIAN_POINT('Ctrl Pts',(0.00295361272834789,-0.279678854419679,
-0.0702511722744358));
#86230=CARTESIAN_POINT('Ctrl Pts',(0.236240033908498,-0.14959004476596,
-0.0543968518754509));
#86231=CARTESIAN_POINT('Ctrl Pts',(0.254209355375769,0.117094399321184,
-0.0385425314764656));
#86232=CARTESIAN_POINT('Ctrl Pts',(0.0393936381945584,0.27682614867795,
-0.0226882110774808));
#86233=CARTESIAN_POINT('Ctrl Pts',(-0.126717381518695,0.214885434336106,
-0.0121186641448238));
#86234=CARTESIAN_POINT('Ctrl Pts',(-0.178400367917765,0.155647215752429,
-0.00683389067849545));
#86235=CARTESIAN_POINT('Ctrl Pts',(0.133736061201431,0.262046381265468,
-1.5608));
#86236=CARTESIAN_POINT('Ctrl Pts',(0.132207210795712,0.262985442201215,
-1.5608));
#86237=CARTESIAN_POINT('Ctrl Pts',(0.130678360389994,0.263924503136962,
-1.5608));
#86238=CARTESIAN_POINT('Ctrl Pts',(0.129149509984275,0.264863564072709,
-1.5608));
#86239=CARTESIAN_POINT('Origin',(0.,0.,-0.04));
#86240=CARTESIAN_POINT('',(-0.3342,4.09276960275046E-17,0.));
#86241=CARTESIAN_POINT('Origin',(0.,0.,0.));
#86242=CARTESIAN_POINT('Origin',(-0.3342,-4.09276960275045E-17,-0.04));
#86243=CARTESIAN_POINT('Origin',(0.48,0.,0.));
#86244=CARTESIAN_POINT('',(-0.48,-5.8783046359073E-17,3.46944695195361E-18));
#86245=CARTESIAN_POINT('Origin',(0.,0.,0.));
#86246=CARTESIAN_POINT('Origin',(0.,0.,0.6066185719505));
#86247=CARTESIAN_POINT('',(-0.25,0.144337567297406,0.588452994616207));
#86248=CARTESIAN_POINT('',(-0.25,-5.3231743852413E-17,0.566123895246948));
#86249=CARTESIAN_POINT('Ctrl Pts',(-0.25,0.144337567297406,0.588452994616208));
#86250=CARTESIAN_POINT('Ctrl Pts',(-0.25,0.0669872981077805,0.566123895246948));
#86251=CARTESIAN_POINT('Ctrl Pts',(-0.25,-7.58473177261421E-17,0.566123895246948));
#86252=CARTESIAN_POINT('',(1.76762539787485E-17,0.288675134594813,0.588452994616207));
#86253=CARTESIAN_POINT('Ctrl Pts',(1.76762539787485E-17,0.288675134594813,
0.588452994616207));
#86254=CARTESIAN_POINT('Ctrl Pts',(-0.125,0.21650635094611,0.546786327949541));
#86255=CARTESIAN_POINT('Ctrl Pts',(-0.25,0.144337567297406,0.588452994616207));
#86256=CARTESIAN_POINT('',(0.25,0.144337567297406,0.588452994616207));
#86257=CARTESIAN_POINT('Ctrl Pts',(0.25,0.144337567297406,0.588452994616207));
#86258=CARTESIAN_POINT('Ctrl Pts',(0.125,0.21650635094611,0.546786327949541));
#86259=CARTESIAN_POINT('Ctrl Pts',(1.76762539787485E-17,0.288675134594813,
0.588452994616207));
#86260=CARTESIAN_POINT('',(0.25,-0.144337567297407,0.588452994616207));
#86261=CARTESIAN_POINT('Ctrl Pts',(0.25,-0.144337567297407,0.588452994616207));
#86262=CARTESIAN_POINT('Ctrl Pts',(0.25,-2.77555756156289E-17,0.546786327949541));
#86263=CARTESIAN_POINT('Ctrl Pts',(0.25,0.144337567297406,0.588452994616207));
#86264=CARTESIAN_POINT('',(-5.30287619362454E-17,-0.288675134594813,0.588452994616207));
#86265=CARTESIAN_POINT('Ctrl Pts',(-5.30287619362454E-17,-0.288675134594813,
0.588452994616207));
#86266=CARTESIAN_POINT('Ctrl Pts',(0.125,-0.21650635094611,0.546786327949541));
#86267=CARTESIAN_POINT('Ctrl Pts',(0.25,-0.144337567297407,0.588452994616207));
#86268=CARTESIAN_POINT('',(-0.25,-0.144337567297406,0.588452994616207));
#86269=CARTESIAN_POINT('Ctrl Pts',(-0.25,-0.144337567297406,0.588452994616207));
#86270=CARTESIAN_POINT('Ctrl Pts',(-0.125,-0.21650635094611,0.546786327949541));
#86271=CARTESIAN_POINT('Ctrl Pts',(-5.30287619362454E-17,-0.288675134594813,
0.588452994616207));
#86272=CARTESIAN_POINT('Ctrl Pts',(-0.25,-7.58473177261421E-17,0.566123895246948));
#86273=CARTESIAN_POINT('Ctrl Pts',(-0.25,-0.0669872981077807,0.566123895246948));
#86274=CARTESIAN_POINT('Ctrl Pts',(-0.25,-0.144337567297406,0.588452994616208));
#86275=CARTESIAN_POINT('',(-0.308675134594813,3.78018015557916E-17,0.6));
#86276=CARTESIAN_POINT('',(-0.320138837486628,-3.92057002610754E-17,0.6066185719505));
#86277=CARTESIAN_POINT('Origin',(0.,0.,0.6));
#86278=CARTESIAN_POINT('Origin',(-5.55111512312578E-17,-0.288675134594813,
0.6));
#86279=CARTESIAN_POINT('',(-5.55111512312578E-17,-0.288675134594813,0.25));
#86280=CARTESIAN_POINT('',(-5.30287619362453E-17,-0.288675134594813,0.6));
#86281=CARTESIAN_POINT('',(-0.25,-0.144337567297406,0.25));
#86282=CARTESIAN_POINT('',(-0.25,-0.144337567297406,0.25));
#86283=CARTESIAN_POINT('',(-0.25,-0.144337567297406,0.6));
#86284=CARTESIAN_POINT('Origin',(0.25,-0.144337567297407,0.6));
#86285=CARTESIAN_POINT('',(0.25,-0.144337567297407,0.25));
#86286=CARTESIAN_POINT('',(0.25,-0.144337567297407,0.6));
#86287=CARTESIAN_POINT('',(-5.30287619362453E-17,-0.288675134594813,0.25));
#86288=CARTESIAN_POINT('Origin',(0.25,0.144337567297406,0.6));
#86289=CARTESIAN_POINT('',(0.25,0.144337567297406,0.25));
#86290=CARTESIAN_POINT('',(0.25,0.144337567297406,0.6));
#86291=CARTESIAN_POINT('',(0.25,-0.144337567297407,0.25));
#86292=CARTESIAN_POINT('Origin',(0.,0.,0.176894574169124));
#86293=CARTESIAN_POINT('',(0.,0.,0.102789148338248));
#86294=CARTESIAN_POINT('',(-0.243346949651439,2.98014062972907E-17,0.25));
#86295=CARTESIAN_POINT('',(-0.1225,-1.50019232895551E-17,0.176894574169124));
#86296=CARTESIAN_POINT('Origin',(0.,0.,0.25));
#86297=CARTESIAN_POINT('Origin',(0.,0.288675134594813,0.6));
#86298=CARTESIAN_POINT('',(2.77555756156289E-17,0.288675134594813,0.25));
#86299=CARTESIAN_POINT('',(1.76762539787485E-17,0.288675134594813,0.6));
#86300=CARTESIAN_POINT('',(0.25,0.144337567297406,0.25));
#86301=CARTESIAN_POINT('Origin',(-0.25,0.144337567297406,0.6));
#86302=CARTESIAN_POINT('',(-0.25,0.144337567297406,0.25));
#86303=CARTESIAN_POINT('',(-0.25,0.144337567297406,0.6));
#86304=CARTESIAN_POINT('',(1.76762539787485E-17,0.288675134594813,0.25));
#86305=CARTESIAN_POINT('Origin',(-0.25,-0.144337567297406,0.6));
#86306=CARTESIAN_POINT('',(-0.25,0.144337567297406,0.25));
#86307=CARTESIAN_POINT('Origin',(0.,0.,0.25));
#86308=CARTESIAN_POINT('Origin',(0.,0.,0.54));
#86309=CARTESIAN_POINT('',(-0.44,-5.38844591624835E-17,0.6));
#86310=CARTESIAN_POINT('Origin',(0.,0.,0.6));
#86311=CARTESIAN_POINT('',(-0.5,-6.12323399573677E-17,0.54));
#86312=CARTESIAN_POINT('Origin',(-0.44,-5.38844591624835E-17,0.54));
#86313=CARTESIAN_POINT('Origin',(0.,0.,0.54));
#86314=CARTESIAN_POINT('Origin',(0.,0.,0.31));
#86315=CARTESIAN_POINT('',(-0.5,-6.12323399573677E-17,0.02));
#86316=CARTESIAN_POINT('',(-0.5,-6.12323399573677E-17,0.31));
#86317=CARTESIAN_POINT('Origin',(0.,0.,0.02));
#86318=CARTESIAN_POINT('Origin',(0.,0.,0.6));
#86319=CARTESIAN_POINT('Origin',(0.255,0.,-1.6));
#86320=CARTESIAN_POINT('',(-0.255,-3.12284933782575E-17,-1.6));
#86321=CARTESIAN_POINT('Origin',(0.,0.,-1.6));
#86322=CARTESIAN_POINT('Origin',(0.,0.,-1.5775));
#86323=CARTESIAN_POINT('',(-0.2775,-3.39839486763391E-17,-1.5775));
#86324=CARTESIAN_POINT('Origin',(0.,0.,0.01));
#86325=CARTESIAN_POINT('',(-0.49,-6.00076931582203E-17,0.01));
#86326=CARTESIAN_POINT('',(0.,0.,0.));
#86327=CARTESIAN_POINT('Origin',(0.,0.,-0.36));
#86328=CARTESIAN_POINT('',(-1.1,-1.34711147906209E-16,-0.8));
#86329=CARTESIAN_POINT('Origin',(0.,0.,-0.8));
#86330=CARTESIAN_POINT('',(-1.1,-1.34711147906209E-16,0.08));
#86331=CARTESIAN_POINT('',(-1.1,-1.34711147906209E-16,-0.36));
#86332=CARTESIAN_POINT('Origin',(0.,0.,0.08));
#86333=CARTESIAN_POINT('Origin',(1.21,0.,-0.8));
#86334=CARTESIAN_POINT('',(-1.21,-1.4818226269683E-16,-0.8));
#86335=CARTESIAN_POINT('Origin',(0.,0.,-0.8));
#86336=CARTESIAN_POINT('Origin',(0.,0.,-0.78));
#86337=CARTESIAN_POINT('',(-1.25,-1.53080849893419E-16,-0.76));
#86338=CARTESIAN_POINT('Origin',(0.,0.,-0.76));
#86339=CARTESIAN_POINT('',(-1.23,-1.50631556295124E-16,-0.78));
#86340=CARTESIAN_POINT('Origin',(0.,0.,-0.38));
#86341=CARTESIAN_POINT('',(-1.25,-1.53080849893419E-16,0.));
#86342=CARTESIAN_POINT('Origin',(0.,0.,0.));
#86343=CARTESIAN_POINT('',(-1.25,-1.53080849893419E-16,-0.38));
#86344=CARTESIAN_POINT('Origin',(1.55,0.,0.));
#86345=CARTESIAN_POINT('',(-1.55,-1.8982025386784E-16,-7.97972798949331E-17));
#86346=CARTESIAN_POINT('Origin',(0.,0.,0.));
#86347=CARTESIAN_POINT('Origin',(0.,0.,0.025));
#86348=CARTESIAN_POINT('',(-1.6,-1.95943487863577E-16,0.0499999999999999));
#86349=CARTESIAN_POINT('Origin',(0.,0.,0.05));
#86350=CARTESIAN_POINT('',(-1.575,-1.92881870865708E-16,0.025));
#86351=CARTESIAN_POINT('Origin',(0.,0.,0.105));
#86352=CARTESIAN_POINT('',(-1.6,-1.95943487863577E-16,0.16));
#86353=CARTESIAN_POINT('Origin',(0.,0.,0.16));
#86354=CARTESIAN_POINT('',(-1.6,-1.95943487863577E-16,0.105));
#86355=CARTESIAN_POINT('Origin',(0.,0.,0.18));
#86356=CARTESIAN_POINT('',(-1.56,-1.91044900666987E-16,0.2));
#86357=CARTESIAN_POINT('',(-1.58,1.93494194265282E-16,0.18));
#86358=CARTESIAN_POINT('Origin',(0.,0.,0.2));
#86359=CARTESIAN_POINT('Origin',(0.,0.,0.2));
#86360=CARTESIAN_POINT('Origin',(1.1,0.,0.08));
#86361=CARTESIAN_POINT('',(0.,0.,0.));
#86362=CARTESIAN_POINT('',(0.,0.,0.));
#86363=CARTESIAN_POINT('',(0.,0.,0.));
#86364=CARTESIAN_POINT('',(0.,0.,0.));
#86365=CARTESIAN_POINT('',(3.46944695195361E-18,0.,-6.93889390390723E-18));
#86366=CARTESIAN_POINT('',(0.,0.,-6.93889390390723E-18));
#86367=CARTESIAN_POINT('',(4.4,0.,13.5));
#86368=CARTESIAN_POINT('',(0.,3.2,7.2));
#86369=CARTESIAN_POINT('',(0.,4.8,7.2));
#86370=CARTESIAN_POINT('',(-6.35,0.,13.5));
#86371=CARTESIAN_POINT('',(6.57,0.,13.5));
#86372=CARTESIAN_POINT('',(5.705,0.,13.5));
#86373=CARTESIAN_POINT('',(-2.,0.,17.5));
#86374=CARTESIAN_POINT('',(-2.,0.,17.4));
#86375=CARTESIAN_POINT('',(-7.55,3.182,16.682));
#86376=CARTESIAN_POINT('',(6.,-4.95,8.));
#86377=CARTESIAN_POINT('',(1.11022302462516E-16,5.55,7.2));
#86378=CARTESIAN_POINT('',(-7.2,0.,13.5));
#86379=CARTESIAN_POINT('',(-4.4,0.,13.5));
#86380=CARTESIAN_POINT('',(0.,-3.2,7.2));
#86381=CARTESIAN_POINT('',(0.,-4.8,7.2));
#86382=CARTESIAN_POINT('',(-5.705,0.,13.5));
#86383=CARTESIAN_POINT('',(-7.55,-3.182,16.682));
#86384=CARTESIAN_POINT('',(-7.55,3.182,10.318));
#86385=CARTESIAN_POINT('',(-7.55,-3.182,10.318));
#86386=CARTESIAN_POINT('',(-6.,-4.95,8.));
#86387=CARTESIAN_POINT('',(4.,-4.95,2.6));
#86388=CARTESIAN_POINT('',(-4.,-4.95,2.6));
#86389=CARTESIAN_POINT('',(1.11022302462516E-16,-5.55,7.2));
#86390=UNCERTAINTY_MEASURE_WITH_UNIT(LENGTH_MEASURE(0.001),#86430,
'DISTANCE_ACCURACY_VALUE',
'Maximum model space distance between geometric entities at asserted c
onnectivities');
#86391=UNCERTAINTY_MEASURE_WITH_UNIT(LENGTH_MEASURE(0.001),#86430,
'DISTANCE_ACCURACY_VALUE',
'Maximum model space distance between geometric entities at asserted c
onnectivities');
#86392=UNCERTAINTY_MEASURE_WITH_UNIT(LENGTH_MEASURE(0.001),#86430,
'DISTANCE_ACCURACY_VALUE',
'Maximum model space distance between geometric entities at asserted c
onnectivities');
#86393=UNCERTAINTY_MEASURE_WITH_UNIT(LENGTH_MEASURE(0.001),#86430,
'DISTANCE_ACCURACY_VALUE',
'Maximum model space distance between geometric entities at asserted c
onnectivities');
#86394=UNCERTAINTY_MEASURE_WITH_UNIT(LENGTH_MEASURE(0.001),#86430,
'DISTANCE_ACCURACY_VALUE',
'Maximum model space distance between geometric entities at asserted c
onnectivities');
#86395=UNCERTAINTY_MEASURE_WITH_UNIT(LENGTH_MEASURE(0.001),#86430,
'DISTANCE_ACCURACY_VALUE',
'Maximum model space distance between geometric entities at asserted c
onnectivities');
#86396=UNCERTAINTY_MEASURE_WITH_UNIT(LENGTH_MEASURE(0.001),#86430,
'DISTANCE_ACCURACY_VALUE',
'Maximum model space distance between geometric entities at asserted c
onnectivities');
#86397=UNCERTAINTY_MEASURE_WITH_UNIT(LENGTH_MEASURE(0.001),#86430,
'DISTANCE_ACCURACY_VALUE',
'Maximum model space distance between geometric entities at asserted c
onnectivities');
#86398=UNCERTAINTY_MEASURE_WITH_UNIT(LENGTH_MEASURE(0.001),#86430,
'DISTANCE_ACCURACY_VALUE',
'Maximum model space distance between geometric entities at asserted c
onnectivities');
#86399=UNCERTAINTY_MEASURE_WITH_UNIT(LENGTH_MEASURE(0.001),#86430,
'DISTANCE_ACCURACY_VALUE',
'Maximum model space distance between geometric entities at asserted c
onnectivities');
#86400=UNCERTAINTY_MEASURE_WITH_UNIT(LENGTH_MEASURE(0.001),#86430,
'DISTANCE_ACCURACY_VALUE',
'Maximum model space distance between geometric entities at asserted c
onnectivities');
#86401=UNCERTAINTY_MEASURE_WITH_UNIT(LENGTH_MEASURE(0.001),#86430,
'DISTANCE_ACCURACY_VALUE',
'Maximum model space distance between geometric entities at asserted c
onnectivities');
#86402=UNCERTAINTY_MEASURE_WITH_UNIT(LENGTH_MEASURE(0.001),#86430,
'DISTANCE_ACCURACY_VALUE',
'Maximum model space distance between geometric entities at asserted c
onnectivities');
#86403=UNCERTAINTY_MEASURE_WITH_UNIT(LENGTH_MEASURE(0.001),#86430,
'DISTANCE_ACCURACY_VALUE',
'Maximum model space distance between geometric entities at asserted c
onnectivities');
#86404=UNCERTAINTY_MEASURE_WITH_UNIT(LENGTH_MEASURE(0.001),#86430,
'DISTANCE_ACCURACY_VALUE',
'Maximum model space distance between geometric entities at asserted c
onnectivities');
#86405=UNCERTAINTY_MEASURE_WITH_UNIT(LENGTH_MEASURE(0.001),#86430,
'DISTANCE_ACCURACY_VALUE',
'Maximum model space distance between geometric entities at asserted c
onnectivities');
#86406=UNCERTAINTY_MEASURE_WITH_UNIT(LENGTH_MEASURE(0.001),#86430,
'DISTANCE_ACCURACY_VALUE',
'Maximum model space distance between geometric entities at asserted c
onnectivities');
#86407=UNCERTAINTY_MEASURE_WITH_UNIT(LENGTH_MEASURE(0.001),#86430,
'DISTANCE_ACCURACY_VALUE',
'Maximum model space distance between geometric entities at asserted c
onnectivities');
#86408=UNCERTAINTY_MEASURE_WITH_UNIT(LENGTH_MEASURE(0.001),#86430,
'DISTANCE_ACCURACY_VALUE',
'Maximum model space distance between geometric entities at asserted c
onnectivities');
#86409=UNCERTAINTY_MEASURE_WITH_UNIT(LENGTH_MEASURE(0.001),#86430,
'DISTANCE_ACCURACY_VALUE',
'Maximum model space distance between geometric entities at asserted c
onnectivities');
#86410=(
GEOMETRIC_REPRESENTATION_CONTEXT(3)
GLOBAL_UNCERTAINTY_ASSIGNED_CONTEXT((#86390))
GLOBAL_UNIT_ASSIGNED_CONTEXT((#86430,#86432,#86433))
REPRESENTATION_CONTEXT('','3D')
);
#86411=(
GEOMETRIC_REPRESENTATION_CONTEXT(3)
GLOBAL_UNCERTAINTY_ASSIGNED_CONTEXT((#86391))
GLOBAL_UNIT_ASSIGNED_CONTEXT((#86430,#86432,#86433))
REPRESENTATION_CONTEXT('','3D')
);
#86412=(
GEOMETRIC_REPRESENTATION_CONTEXT(3)
GLOBAL_UNCERTAINTY_ASSIGNED_CONTEXT((#86392))
GLOBAL_UNIT_ASSIGNED_CONTEXT((#86430,#86432,#86433))
REPRESENTATION_CONTEXT('','3D')
);
#86413=(
GEOMETRIC_REPRESENTATION_CONTEXT(3)
GLOBAL_UNCERTAINTY_ASSIGNED_CONTEXT((#86393))
GLOBAL_UNIT_ASSIGNED_CONTEXT((#86430,#86432,#86433))
REPRESENTATION_CONTEXT('','3D')
);
#86414=(
GEOMETRIC_REPRESENTATION_CONTEXT(3)
GLOBAL_UNCERTAINTY_ASSIGNED_CONTEXT((#86394))
GLOBAL_UNIT_ASSIGNED_CONTEXT((#86430,#86432,#86433))
REPRESENTATION_CONTEXT('','3D')
);
#86415=(
GEOMETRIC_REPRESENTATION_CONTEXT(3)
GLOBAL_UNCERTAINTY_ASSIGNED_CONTEXT((#86395))
GLOBAL_UNIT_ASSIGNED_CONTEXT((#86430,#86432,#86433))
REPRESENTATION_CONTEXT('','3D')
);
#86416=(
GEOMETRIC_REPRESENTATION_CONTEXT(3)
GLOBAL_UNCERTAINTY_ASSIGNED_CONTEXT((#86396))
GLOBAL_UNIT_ASSIGNED_CONTEXT((#86430,#86432,#86433))
REPRESENTATION_CONTEXT('','3D')
);
#86417=(
GEOMETRIC_REPRESENTATION_CONTEXT(3)
GLOBAL_UNCERTAINTY_ASSIGNED_CONTEXT((#86397))
GLOBAL_UNIT_ASSIGNED_CONTEXT((#86430,#86432,#86433))
REPRESENTATION_CONTEXT('','3D')
);
#86418=(
GEOMETRIC_REPRESENTATION_CONTEXT(3)
GLOBAL_UNCERTAINTY_ASSIGNED_CONTEXT((#86398))
GLOBAL_UNIT_ASSIGNED_CONTEXT((#86430,#86432,#86433))
REPRESENTATION_CONTEXT('','3D')
);
#86419=(
GEOMETRIC_REPRESENTATION_CONTEXT(3)
GLOBAL_UNCERTAINTY_ASSIGNED_CONTEXT((#86399))
GLOBAL_UNIT_ASSIGNED_CONTEXT((#86430,#86432,#86433))
REPRESENTATION_CONTEXT('','3D')
);
#86420=(
GEOMETRIC_REPRESENTATION_CONTEXT(3)
GLOBAL_UNCERTAINTY_ASSIGNED_CONTEXT((#86400))
GLOBAL_UNIT_ASSIGNED_CONTEXT((#86430,#86432,#86433))
REPRESENTATION_CONTEXT('','3D')
);
#86421=(
GEOMETRIC_REPRESENTATION_CONTEXT(3)
GLOBAL_UNCERTAINTY_ASSIGNED_CONTEXT((#86401))
GLOBAL_UNIT_ASSIGNED_CONTEXT((#86430,#86432,#86433))
REPRESENTATION_CONTEXT('','3D')
);
#86422=(
GEOMETRIC_REPRESENTATION_CONTEXT(3)
GLOBAL_UNCERTAINTY_ASSIGNED_CONTEXT((#86402))
GLOBAL_UNIT_ASSIGNED_CONTEXT((#86430,#86432,#86433))
REPRESENTATION_CONTEXT('','3D')
);
#86423=(
GEOMETRIC_REPRESENTATION_CONTEXT(3)
GLOBAL_UNCERTAINTY_ASSIGNED_CONTEXT((#86403))
GLOBAL_UNIT_ASSIGNED_CONTEXT((#86430,#86432,#86433))
REPRESENTATION_CONTEXT('','3D')
);
#86424=(
GEOMETRIC_REPRESENTATION_CONTEXT(3)
GLOBAL_UNCERTAINTY_ASSIGNED_CONTEXT((#86404))
GLOBAL_UNIT_ASSIGNED_CONTEXT((#86430,#86432,#86433))
REPRESENTATION_CONTEXT('','3D')
);
#86425=(
GEOMETRIC_REPRESENTATION_CONTEXT(3)
GLOBAL_UNCERTAINTY_ASSIGNED_CONTEXT((#86405))
GLOBAL_UNIT_ASSIGNED_CONTEXT((#86430,#86432,#86433))
REPRESENTATION_CONTEXT('','3D')
);
#86426=(
GEOMETRIC_REPRESENTATION_CONTEXT(3)
GLOBAL_UNCERTAINTY_ASSIGNED_CONTEXT((#86406))
GLOBAL_UNIT_ASSIGNED_CONTEXT((#86430,#86432,#86433))
REPRESENTATION_CONTEXT('','3D')
);
#86427=(
GEOMETRIC_REPRESENTATION_CONTEXT(3)
GLOBAL_UNCERTAINTY_ASSIGNED_CONTEXT((#86407))
GLOBAL_UNIT_ASSIGNED_CONTEXT((#86430,#86432,#86433))
REPRESENTATION_CONTEXT('','3D')
);
#86428=(
GEOMETRIC_REPRESENTATION_CONTEXT(3)
GLOBAL_UNCERTAINTY_ASSIGNED_CONTEXT((#86408))
GLOBAL_UNIT_ASSIGNED_CONTEXT((#86430,#86432,#86433))
REPRESENTATION_CONTEXT('','3D')
);
#86429=(
GEOMETRIC_REPRESENTATION_CONTEXT(3)
GLOBAL_UNCERTAINTY_ASSIGNED_CONTEXT((#86409))
GLOBAL_UNIT_ASSIGNED_CONTEXT((#86430,#86432,#86433))
REPRESENTATION_CONTEXT('','3D')
);
#86430=(
LENGTH_UNIT()
NAMED_UNIT(*)
SI_UNIT(.CENTI.,.METRE.)
);
#86431=(
LENGTH_UNIT()
NAMED_UNIT(*)
SI_UNIT($,.METRE.)
);
#86432=(
NAMED_UNIT(*)
PLANE_ANGLE_UNIT()
SI_UNIT($,.RADIAN.)
);
#86433=(
NAMED_UNIT(*)
SI_UNIT($,.STERADIAN.)
SOLID_ANGLE_UNIT()
);
#86434=SHAPE_DEFINITION_REPRESENTATION(#86453,#86501);
#86435=SHAPE_DEFINITION_REPRESENTATION(#86454,#86502);
#86436=SHAPE_DEFINITION_REPRESENTATION(#86455,#86503);
#86437=SHAPE_DEFINITION_REPRESENTATION(#86456,#86504);
#86438=SHAPE_DEFINITION_REPRESENTATION(#86457,#86505);
#86439=SHAPE_DEFINITION_REPRESENTATION(#86458,#86506);
#86440=SHAPE_DEFINITION_REPRESENTATION(#86459,#86507);
#86441=SHAPE_DEFINITION_REPRESENTATION(#86460,#86508);
#86442=SHAPE_DEFINITION_REPRESENTATION(#86461,#86509);
#86443=SHAPE_DEFINITION_REPRESENTATION(#86462,#86510);
#86444=SHAPE_DEFINITION_REPRESENTATION(#86463,#86511);
#86445=SHAPE_DEFINITION_REPRESENTATION(#86464,#86512);
#86446=SHAPE_DEFINITION_REPRESENTATION(#86465,#86513);
#86447=SHAPE_DEFINITION_REPRESENTATION(#86466,#86514);
#86448=SHAPE_DEFINITION_REPRESENTATION(#86467,#86515);
#86449=SHAPE_DEFINITION_REPRESENTATION(#86468,#86516);
#86450=SHAPE_DEFINITION_REPRESENTATION(#86469,#86517);
#86451=SHAPE_DEFINITION_REPRESENTATION(#86470,#86518);
#86452=SHAPE_DEFINITION_REPRESENTATION(#86471,#86519);
#86453=PRODUCT_DEFINITION_SHAPE('',$,#86521);
#86454=PRODUCT_DEFINITION_SHAPE('',$,#86522);
#86455=PRODUCT_DEFINITION_SHAPE('',$,#86523);
#86456=PRODUCT_DEFINITION_SHAPE('',$,#86524);
#86457=PRODUCT_DEFINITION_SHAPE('',$,#86525);
#86458=PRODUCT_DEFINITION_SHAPE('',$,#86526);
#86459=PRODUCT_DEFINITION_SHAPE('',$,#86527);
#86460=PRODUCT_DEFINITION_SHAPE('',$,#86528);
#86461=PRODUCT_DEFINITION_SHAPE('',$,#86529);
#86462=PRODUCT_DEFINITION_SHAPE('',$,#86530);
#86463=PRODUCT_DEFINITION_SHAPE('',$,#86531);
#86464=PRODUCT_DEFINITION_SHAPE('',$,#86532);
#86465=PRODUCT_DEFINITION_SHAPE('',$,#86533);
#86466=PRODUCT_DEFINITION_SHAPE('',$,#86534);
#86467=PRODUCT_DEFINITION_SHAPE('',$,#86535);
#86468=PRODUCT_DEFINITION_SHAPE('',$,#86536);
#86469=PRODUCT_DEFINITION_SHAPE('',$,#86537);
#86470=PRODUCT_DEFINITION_SHAPE('',$,#86538);
#86471=PRODUCT_DEFINITION_SHAPE('',$,#86539);
#86472=PRODUCT_DEFINITION_SHAPE($,$,#98);
#86473=PRODUCT_DEFINITION_SHAPE($,$,#99);
#86474=PRODUCT_DEFINITION_SHAPE($,$,#100);
#86475=PRODUCT_DEFINITION_SHAPE($,$,#101);
#86476=PRODUCT_DEFINITION_SHAPE($,$,#102);
#86477=PRODUCT_DEFINITION_SHAPE($,$,#103);
#86478=PRODUCT_DEFINITION_SHAPE($,$,#104);
#86479=PRODUCT_DEFINITION_SHAPE($,$,#105);
#86480=PRODUCT_DEFINITION_SHAPE($,$,#106);
#86481=PRODUCT_DEFINITION_SHAPE($,$,#107);
#86482=PRODUCT_DEFINITION_SHAPE($,$,#108);
#86483=PRODUCT_DEFINITION_SHAPE($,$,#109);
#86484=PRODUCT_DEFINITION_SHAPE($,$,#110);
#86485=PRODUCT_DEFINITION_SHAPE($,$,#111);
#86486=PRODUCT_DEFINITION_SHAPE($,$,#112);
#86487=PRODUCT_DEFINITION_SHAPE($,$,#113);
#86488=PRODUCT_DEFINITION_SHAPE($,$,#114);
#86489=PRODUCT_DEFINITION_SHAPE($,$,#115);
#86490=PRODUCT_DEFINITION_SHAPE($,$,#116);
#86491=PRODUCT_DEFINITION_SHAPE($,$,#117);
#86492=PRODUCT_DEFINITION_SHAPE($,$,#118);
#86493=PRODUCT_DEFINITION_SHAPE($,$,#119);
#86494=PRODUCT_DEFINITION_SHAPE($,$,#120);
#86495=PRODUCT_DEFINITION_SHAPE($,$,#121);
#86496=PRODUCT_DEFINITION_SHAPE($,$,#122);
#86497=PRODUCT_DEFINITION_SHAPE($,$,#123);
#86498=PRODUCT_DEFINITION_SHAPE($,$,#124);
#86499=PRODUCT_DEFINITION_SHAPE($,$,#125);
#86500=PRODUCT_DEFINITION_SHAPE($,$,#126);
#86501=SHAPE_REPRESENTATION('',(#15830,#17257,#17258,#17259,#17260,#17261,
#17262,#17263,#17264,#17265,#17266,#17267,#17268,#17269,#17270,#17271,#17272,
#17273,#17274,#17275,#17276,#17277,#17278,#17279,#17280,#17281,#17282,#17283,
#17284,#17285),#86410);
#86502=SHAPE_REPRESENTATION('',(#15831),#86411);
#86503=SHAPE_REPRESENTATION('',(#16203),#86412);
#86504=SHAPE_REPRESENTATION('',(#16305),#86413);
#86505=SHAPE_REPRESENTATION('',(#16419),#86414);
#86506=SHAPE_REPRESENTATION('',(#16477),#86415);
#86507=SHAPE_REPRESENTATION('',(#16819),#86416);
#86508=SHAPE_REPRESENTATION('',(#16859),#86417);
#86509=SHAPE_REPRESENTATION('',(#16882),#86418);
#86510=SHAPE_REPRESENTATION('',(#16902),#86419);
#86511=SHAPE_REPRESENTATION('',(#16948),#86420);
#86512=SHAPE_REPRESENTATION('',(#16965),#86421);
#86513=SHAPE_REPRESENTATION('',(#16985),#86422);
#86514=SHAPE_REPRESENTATION('',(#17028),#86423);
#86515=SHAPE_REPRESENTATION('',(#17061),#86424);
#86516=SHAPE_REPRESENTATION('',(#17084),#86425);
#86517=SHAPE_REPRESENTATION('',(#17121),#86426);
#86518=SHAPE_REPRESENTATION('',(#17181),#86427);
#86519=SHAPE_REPRESENTATION('',(#17237),#86428);
#86520=PRODUCT_DEFINITION_CONTEXT('part definition',#86579,'design');
#86521=PRODUCT_DEFINITION('MAS-359',
'MAS-359',#86540,#86520);
#86522=PRODUCT_DEFINITION('Housing','Housing',#86541,#86520);
#86523=PRODUCT_DEFINITION('Output Side Cover','Output Side Cover',#86542,
#86520);
#86524=PRODUCT_DEFINITION('IEC71 B5 Input Motor Flange',
'IEC71 B5 Input Motor Flange',#86543,#86520);
#86525=PRODUCT_DEFINITION('Hardened Steel Worm Shaft m3 z1',
'Hardened Steel Worm Shaft m3 z1',#86544,#86520);
#86526=PRODUCT_DEFINITION('Bronze Worm Wheel Ring z30',
'Bronze Worm Wheel Ring z30',#86545,#86520);
#86527=PRODUCT_DEFINITION('Cast Iron Output Hollow Shaft Hub',
'Cast Iron Output Hollow Shaft Hub',#86546,#86520);
#86528=PRODUCT_DEFINITION('Oil Seal DIN3760 A 25x52x7 Viton',
'Oil Seal DIN3760 A 25x52x7 Viton',#86547,#86520);
#86529=PRODUCT_DEFINITION('Worm End Cap 52','Worm End Cap 52',#86548,#86520);
#86530=PRODUCT_DEFINITION('DIN908 M10x1 Hex Drive Plug',
'DIN908 M10x1 Hex Drive Plug',#86549,#86520);
#86531=PRODUCT_DEFINITION('DIN7603 A10x14x1 Copper Washer',
'DIN7603 A10x14x1 Copper Washer',#86550,#86520);
#86532=PRODUCT_DEFINITION('Input Bore Protective Plug 14',
'Input Bore Protective Plug 14',#86551,#86520);
#86533=PRODUCT_DEFINITION('Tapered Roller Bearing 30205',
'Tapered Roller Bearing 30205',#86552,#86520);
#86534=PRODUCT_DEFINITION('Deep Groove Ball Bearing 6009-2RS',
'Deep Groove Ball Bearing 6009-2RS',#86553,#86520);
#86535=PRODUCT_DEFINITION('Oil Seal DIN3760 A 45x62x8 Viton',
'Oil Seal DIN3760 A 45x62x8 Viton',#86554,#86520);
#86536=PRODUCT_DEFINITION('DIN472 52x2 Retaining Ring',
'DIN472 52x2 Retaining Ring',#86555,#86520);
#86537=PRODUCT_DEFINITION('ISO 4762 M6x20 A2 SHCS',
'ISO 4762 M6x20 A2 SHCS',#86556,#86520);
#86538=PRODUCT_DEFINITION('ISO 4762 M6x16 A2 SHCS',
'ISO 4762 M6x16 A2 SHCS',#86557,#86520);
#86539=PRODUCT_DEFINITION('Output Bore Protective Plug 25',
'Output Bore Protective Plug 25',#86558,#86520);
#86540=PRODUCT_DEFINITION_FORMATION('',$,#86581);
#86541=PRODUCT_DEFINITION_FORMATION('',$,#86582);
#86542=PRODUCT_DEFINITION_FORMATION('',$,#86583);
#86543=PRODUCT_DEFINITION_FORMATION('',$,#86584);
#86544=PRODUCT_DEFINITION_FORMATION('',$,#86585);
#86545=PRODUCT_DEFINITION_FORMATION('',$,#86586);
#86546=PRODUCT_DEFINITION_FORMATION('',$,#86587);
#86547=PRODUCT_DEFINITION_FORMATION('',$,#86588);
#86548=PRODUCT_DEFINITION_FORMATION('',$,#86589);
#86549=PRODUCT_DEFINITION_FORMATION('',$,#86590);
#86550=PRODUCT_DEFINITION_FORMATION('',$,#86591);
#86551=PRODUCT_DEFINITION_FORMATION('',$,#86592);
#86552=PRODUCT_DEFINITION_FORMATION('',$,#86593);
#86553=PRODUCT_DEFINITION_FORMATION('',$,#86594);
#86554=PRODUCT_DEFINITION_FORMATION('',$,#86595);
#86555=PRODUCT_DEFINITION_FORMATION('',$,#86596);
#86556=PRODUCT_DEFINITION_FORMATION('',$,#86597);
#86557=PRODUCT_DEFINITION_FORMATION('',$,#86598);
#86558=PRODUCT_DEFINITION_FORMATION('',$,#86599);
#86559=PRODUCT_RELATED_PRODUCT_CATEGORY('MAS-359',
'MAS-359',(#86581));
#86560=PRODUCT_RELATED_PRODUCT_CATEGORY('Housing','Housing',(#86582));
#86561=PRODUCT_RELATED_PRODUCT_CATEGORY('Output Side Cover',
'Output Side Cover',(#86583));
#86562=PRODUCT_RELATED_PRODUCT_CATEGORY('IEC71 B5 Input Motor Flange',
'IEC71 B5 Input Motor Flange',(#86584));
#86563=PRODUCT_RELATED_PRODUCT_CATEGORY(
'Hardened Steel Worm Shaft m3 z1','Hardened Steel Worm Shaft m3 z1',(#86585));
#86564=PRODUCT_RELATED_PRODUCT_CATEGORY('Bronze Worm Wheel Ring z30',
'Bronze Worm Wheel Ring z30',(#86586));
#86565=PRODUCT_RELATED_PRODUCT_CATEGORY(
'Cast Iron Output Hollow Shaft Hub','Cast Iron Output Hollow Shaft Hub',
(#86587));
#86566=PRODUCT_RELATED_PRODUCT_CATEGORY(
'Oil Seal DIN3760 A 25x52x7 Viton','Oil Seal DIN3760 A 25x52x7 Viton',(#86588));
#86567=PRODUCT_RELATED_PRODUCT_CATEGORY('Worm End Cap 52',
'Worm End Cap 52',(#86589));
#86568=PRODUCT_RELATED_PRODUCT_CATEGORY('DIN908 M10x1 Hex Drive Plug',
'DIN908 M10x1 Hex Drive Plug',(#86590));
#86569=PRODUCT_RELATED_PRODUCT_CATEGORY(
'DIN7603 A10x14x1 Copper Washer','DIN7603 A10x14x1 Copper Washer',(#86591));
#86570=PRODUCT_RELATED_PRODUCT_CATEGORY('Input Bore Protective Plug 14',
'Input Bore Protective Plug 14',(#86592));
#86571=PRODUCT_RELATED_PRODUCT_CATEGORY('Tapered Roller Bearing 30205',
'Tapered Roller Bearing 30205',(#86593));
#86572=PRODUCT_RELATED_PRODUCT_CATEGORY(
'Deep Groove Ball Bearing 6009-2RS','Deep Groove Ball Bearing 6009-2RS',
(#86594));
#86573=PRODUCT_RELATED_PRODUCT_CATEGORY(
'Oil Seal DIN3760 A 45x62x8 Viton','Oil Seal DIN3760 A 45x62x8 Viton',(#86595));
#86574=PRODUCT_RELATED_PRODUCT_CATEGORY('DIN472 52x2 Retaining Ring',
'DIN472 52x2 Retaining Ring',(#86596));
#86575=PRODUCT_RELATED_PRODUCT_CATEGORY('ISO 4762 M6x20 A2 SHCS',
'ISO 4762 M6x20 A2 SHCS',(#86597));
#86576=PRODUCT_RELATED_PRODUCT_CATEGORY('ISO 4762 M6x16 A2 SHCS',
'ISO 4762 M6x16 A2 SHCS',(#86598));
#86577=PRODUCT_RELATED_PRODUCT_CATEGORY(
'Output Bore Protective Plug 25','Output Bore Protective Plug 25',(#86599));
#86578=APPLICATION_PROTOCOL_DEFINITION('international standard',
'automotive_design',2009,#86579);
#86579=APPLICATION_CONTEXT(
'Core Data for Automotive Mechanical Design Process');
#86580=PRODUCT_CONTEXT('part definition',#86579,'mechanical');
#86581=PRODUCT('MAS-359','MAS-359',
$,(#86580));
#86582=PRODUCT('Housing','Housing',$,(#86580));
#86583=PRODUCT('Output Side Cover','Output Side Cover',$,(#86580));
#86584=PRODUCT('IEC71 B5 Input Motor Flange',
'IEC71 B5 Input Motor Flange',$,(#86580));
#86585=PRODUCT('Hardened Steel Worm Shaft m3 z1',
'Hardened Steel Worm Shaft m3 z1',$,(#86580));
#86586=PRODUCT('Bronze Worm Wheel Ring z30',
'Bronze Worm Wheel Ring z30',$,(#86580));
#86587=PRODUCT('Cast Iron Output Hollow Shaft Hub',
'Cast Iron Output Hollow Shaft Hub',$,(#86580));
#86588=PRODUCT('Oil Seal DIN3760 A 25x52x7 Viton',
'Oil Seal DIN3760 A 25x52x7 Viton',$,(#86580));
#86589=PRODUCT('Worm End Cap 52','Worm End Cap 52',$,(#86580));
#86590=PRODUCT('DIN908 M10x1 Hex Drive Plug',
'DIN908 M10x1 Hex Drive Plug',$,(#86580));
#86591=PRODUCT('DIN7603 A10x14x1 Copper Washer',
'DIN7603 A10x14x1 Copper Washer',$,(#86580));
#86592=PRODUCT('Input Bore Protective Plug 14',
'Input Bore Protective Plug 14',$,(#86580));
#86593=PRODUCT('Tapered Roller Bearing 30205',
'Tapered Roller Bearing 30205',$,(#86580));
#86594=PRODUCT('Deep Groove Ball Bearing 6009-2RS',
'Deep Groove Ball Bearing 6009-2RS',$,(#86580));
#86595=PRODUCT('Oil Seal DIN3760 A 45x62x8 Viton',
'Oil Seal DIN3760 A 45x62x8 Viton',$,(#86580));
#86596=PRODUCT('DIN472 52x2 Retaining Ring',
'DIN472 52x2 Retaining Ring',$,(#86580));
#86597=PRODUCT('ISO 4762 M6x20 A2 SHCS','ISO 4762 M6x20 A2 SHCS',$,(#86580));
#86598=PRODUCT('ISO 4762 M6x16 A2 SHCS','ISO 4762 M6x16 A2 SHCS',$,(#86580));
#86599=PRODUCT('Output Bore Protective Plug 25',
'Output Bore Protective Plug 25',$,(#86580));
#86600=PRESENTATION_STYLE_ASSIGNMENT((#86618));
#86601=PRESENTATION_STYLE_ASSIGNMENT((#86619));
#86602=PRESENTATION_STYLE_ASSIGNMENT((#86620));
#86603=PRESENTATION_STYLE_ASSIGNMENT((#86621));
#86604=PRESENTATION_STYLE_ASSIGNMENT((#86622));
#86605=PRESENTATION_STYLE_ASSIGNMENT((#86623));
#86606=PRESENTATION_STYLE_ASSIGNMENT((#86624));
#86607=PRESENTATION_STYLE_ASSIGNMENT((#86625));
#86608=PRESENTATION_STYLE_ASSIGNMENT((#86626));
#86609=PRESENTATION_STYLE_ASSIGNMENT((#86627));
#86610=PRESENTATION_STYLE_ASSIGNMENT((#86628));
#86611=PRESENTATION_STYLE_ASSIGNMENT((#86629));
#86612=PRESENTATION_STYLE_ASSIGNMENT((#86630));
#86613=PRESENTATION_STYLE_ASSIGNMENT((#86631));
#86614=PRESENTATION_STYLE_ASSIGNMENT((#86632));
#86615=PRESENTATION_STYLE_ASSIGNMENT((#86633));
#86616=PRESENTATION_STYLE_ASSIGNMENT((#86634));
#86617=PRESENTATION_STYLE_ASSIGNMENT((#86635));
#86618=SURFACE_STYLE_USAGE(.BOTH.,#86636);
#86619=SURFACE_STYLE_USAGE(.BOTH.,#86637);
#86620=SURFACE_STYLE_USAGE(.BOTH.,#86638);
#86621=SURFACE_STYLE_USAGE(.BOTH.,#86639);
#86622=SURFACE_STYLE_USAGE(.BOTH.,#86640);
#86623=SURFACE_STYLE_USAGE(.BOTH.,#86641);
#86624=SURFACE_STYLE_USAGE(.BOTH.,#86642);
#86625=SURFACE_STYLE_USAGE(.BOTH.,#86643);
#86626=SURFACE_STYLE_USAGE(.BOTH.,#86644);
#86627=SURFACE_STYLE_USAGE(.BOTH.,#86645);
#86628=SURFACE_STYLE_USAGE(.BOTH.,#86646);
#86629=SURFACE_STYLE_USAGE(.BOTH.,#86647);
#86630=SURFACE_STYLE_USAGE(.BOTH.,#86648);
#86631=SURFACE_STYLE_USAGE(.BOTH.,#86649);
#86632=SURFACE_STYLE_USAGE(.BOTH.,#86650);
#86633=SURFACE_STYLE_USAGE(.BOTH.,#86651);
#86634=SURFACE_STYLE_USAGE(.BOTH.,#86652);
#86635=SURFACE_STYLE_USAGE(.BOTH.,#86653);
#86636=SURFACE_SIDE_STYLE('',(#86654));
#86637=SURFACE_SIDE_STYLE('',(#86655));
#86638=SURFACE_SIDE_STYLE('',(#86656));
#86639=SURFACE_SIDE_STYLE('',(#86657));
#86640=SURFACE_SIDE_STYLE('',(#86658));
#86641=SURFACE_SIDE_STYLE('',(#86659));
#86642=SURFACE_SIDE_STYLE('',(#86660));
#86643=SURFACE_SIDE_STYLE('',(#86661));
#86644=SURFACE_SIDE_STYLE('',(#86662));
#86645=SURFACE_SIDE_STYLE('',(#86663));
#86646=SURFACE_SIDE_STYLE('',(#86664));
#86647=SURFACE_SIDE_STYLE('',(#86665));
#86648=SURFACE_SIDE_STYLE('',(#86666));
#86649=SURFACE_SIDE_STYLE('',(#86667));
#86650=SURFACE_SIDE_STYLE('',(#86668));
#86651=SURFACE_SIDE_STYLE('',(#86669));
#86652=SURFACE_SIDE_STYLE('',(#86670));
#86653=SURFACE_SIDE_STYLE('',(#86671));
#86654=SURFACE_STYLE_FILL_AREA(#86672);
#86655=SURFACE_STYLE_FILL_AREA(#86673);
#86656=SURFACE_STYLE_FILL_AREA(#86674);
#86657=SURFACE_STYLE_FILL_AREA(#86675);
#86658=SURFACE_STYLE_FILL_AREA(#86676);
#86659=SURFACE_STYLE_FILL_AREA(#86677);
#86660=SURFACE_STYLE_FILL_AREA(#86678);
#86661=SURFACE_STYLE_FILL_AREA(#86679);
#86662=SURFACE_STYLE_FILL_AREA(#86680);
#86663=SURFACE_STYLE_FILL_AREA(#86681);
#86664=SURFACE_STYLE_FILL_AREA(#86682);
#86665=SURFACE_STYLE_FILL_AREA(#86683);
#86666=SURFACE_STYLE_FILL_AREA(#86684);
#86667=SURFACE_STYLE_FILL_AREA(#86685);
#86668=SURFACE_STYLE_FILL_AREA(#86686);
#86669=SURFACE_STYLE_FILL_AREA(#86687);
#86670=SURFACE_STYLE_FILL_AREA(#86688);
#86671=SURFACE_STYLE_FILL_AREA(#86689);
#86672=FILL_AREA_STYLE('Steel - Satin',(#86690));
#86673=FILL_AREA_STYLE('Opaque(192,195,199)',(#86691));
#86674=FILL_AREA_STYLE('Opaque(184,188,192)',(#86692));
#86675=FILL_AREA_STYLE('Opaque(198,201,205)',(#86693));
#86676=FILL_AREA_STYLE('Opaque(212,215,220)',(#86694));
#86677=FILL_AREA_STYLE('Opaque(214,178,102)',(#86695));
#86678=FILL_AREA_STYLE('Opaque(128,131,135)',(#86696));
#86679=FILL_AREA_STYLE('Opaque(52,52,56)',(#86697));
#86680=FILL_AREA_STYLE('Opaque(205,208,212)',(#86698));
#86681=FILL_AREA_STYLE('Opaque(199,203,208)',(#86699));
#86682=FILL_AREA_STYLE('Opaque(200,128,82)',(#86700));
#86683=FILL_AREA_STYLE('Opaque(240,172,28)',(#86701));
#86684=FILL_AREA_STYLE('Opaque(218,221,226)',(#86702));
#86685=FILL_AREA_STYLE('Opaque(210,213,218)',(#86703));
#86686=FILL_AREA_STYLE('Opaque(48,48,52)',(#86704));
#86687=FILL_AREA_STYLE('Opaque(200,204,208)',(#86705));
#86688=FILL_AREA_STYLE('Opaque(198,202,208)',(#86706));
#86689=FILL_AREA_STYLE('Opaque(203,207,212)',(#86707));
#86690=FILL_AREA_STYLE_COLOUR('Steel - Satin',#86708);
#86691=FILL_AREA_STYLE_COLOUR('Opaque(192,195,199)',#86709);
#86692=FILL_AREA_STYLE_COLOUR('Opaque(184,188,192)',#86710);
#86693=FILL_AREA_STYLE_COLOUR('Opaque(198,201,205)',#86711);
#86694=FILL_AREA_STYLE_COLOUR('Opaque(212,215,220)',#86712);
#86695=FILL_AREA_STYLE_COLOUR('Opaque(214,178,102)',#86713);
#86696=FILL_AREA_STYLE_COLOUR('Opaque(128,131,135)',#86714);
#86697=FILL_AREA_STYLE_COLOUR('Opaque(52,52,56)',#86715);
#86698=FILL_AREA_STYLE_COLOUR('Opaque(205,208,212)',#86716);
#86699=FILL_AREA_STYLE_COLOUR('Opaque(199,203,208)',#86717);
#86700=FILL_AREA_STYLE_COLOUR('Opaque(200,128,82)',#86718);
#86701=FILL_AREA_STYLE_COLOUR('Opaque(240,172,28)',#86719);
#86702=FILL_AREA_STYLE_COLOUR('Opaque(218,221,226)',#86720);
#86703=FILL_AREA_STYLE_COLOUR('Opaque(210,213,218)',#86721);
#86704=FILL_AREA_STYLE_COLOUR('Opaque(48,48,52)',#86722);
#86705=FILL_AREA_STYLE_COLOUR('Opaque(200,204,208)',#86723);
#86706=FILL_AREA_STYLE_COLOUR('Opaque(198,202,208)',#86724);
#86707=FILL_AREA_STYLE_COLOUR('Opaque(203,207,212)',#86725);
#86708=COLOUR_RGB('Steel - Satin', 0.09019608, 0.27058824, 0.51372549);
#86709=COLOUR_RGB('Opaque(192,195,199)', 0.09019608, 0.27058824, 0.51372549);
#86710=COLOUR_RGB('Opaque(184,188,192)', 0.66274510, 0.83137255, 0.94901961);
#86711=COLOUR_RGB('Opaque(198,201,205)', 0.31764706, 0.68627451, 0.89019608);
#86712=COLOUR_RGB('Opaque(212,215,220)', 0.40784314, 0.44705882, 0.49803922);
#86713=COLOUR_RGB('Opaque(214,178,102)', 0.72549020, 0.75294118, 0.79215686);
#86714=COLOUR_RGB('Opaque(128,131,135)', 0.08235294, 0.09019608, 0.10196078);
#86715=COLOUR_RGB('Opaque(52,52,56)', 0.09019608, 0.27058824, 0.51372549);
#86716=COLOUR_RGB('Opaque(205,208,212)', 0.66274510, 0.83137255, 0.94901961);
#86717=COLOUR_RGB('Opaque(199,203,208)', 0.31764706, 0.68627451, 0.89019608);
#86718=COLOUR_RGB('Opaque(200,128,82)', 0.40784314, 0.44705882, 0.49803922);
#86719=COLOUR_RGB('Opaque(240,172,28)', 0.72549020, 0.75294118, 0.79215686);
#86720=COLOUR_RGB('Opaque(218,221,226)', 0.08235294, 0.09019608, 0.10196078);
#86721=COLOUR_RGB('Opaque(210,213,218)', 0.09019608, 0.27058824, 0.51372549);
#86722=COLOUR_RGB('Opaque(48,48,52)', 0.66274510, 0.83137255, 0.94901961);
#86723=COLOUR_RGB('Opaque(200,204,208)', 0.31764706, 0.68627451, 0.89019608);
#86724=COLOUR_RGB('Opaque(198,202,208)', 0.40784314, 0.44705882, 0.49803922);
#86725=COLOUR_RGB('Opaque(203,207,212)', 0.72549020, 0.75294118, 0.79215686);
ENDSEC;
END-ISO-10303-21;
